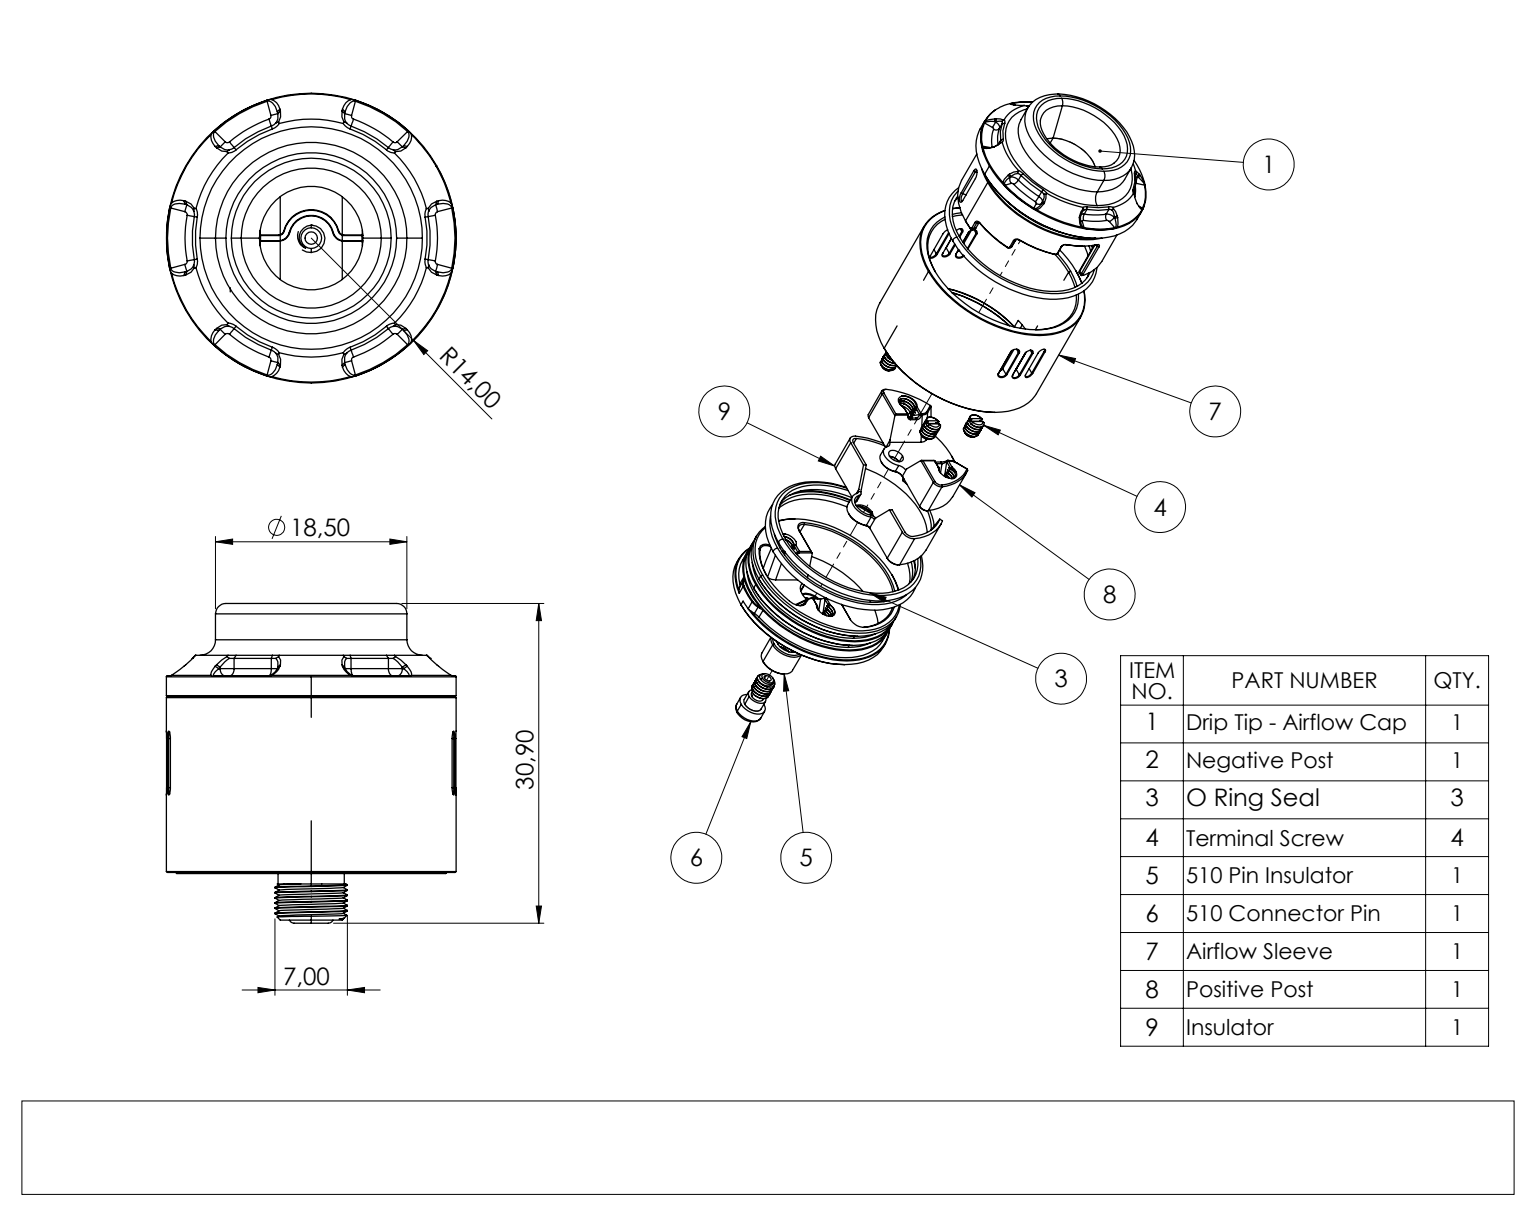
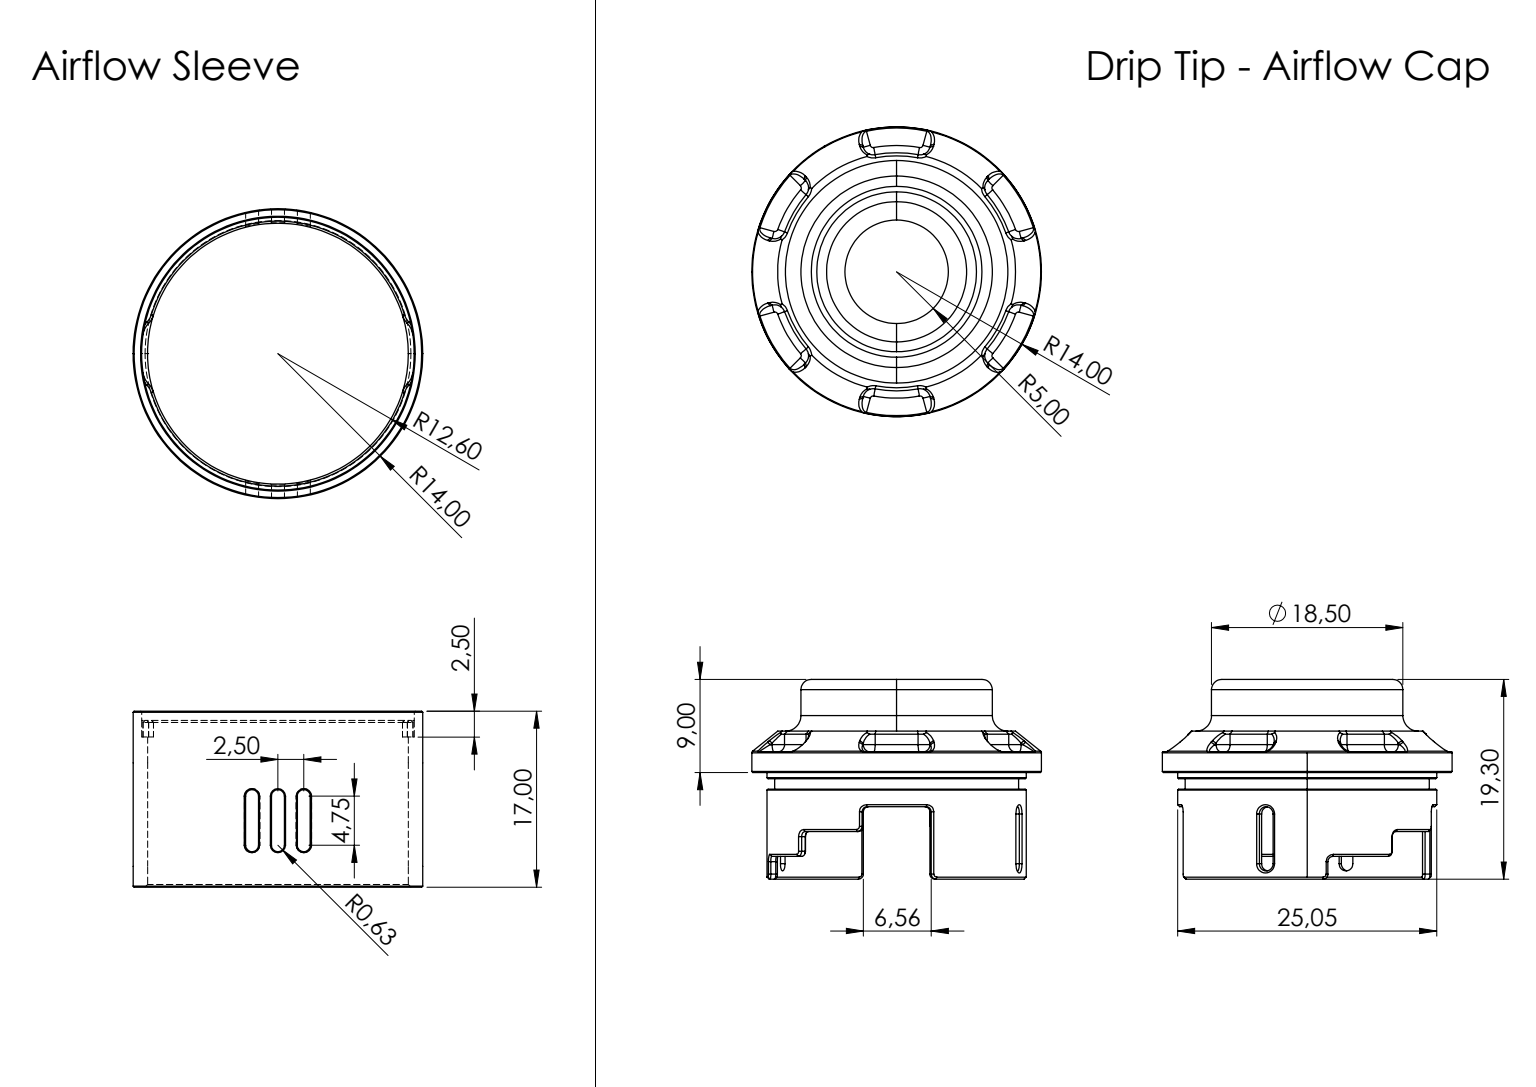
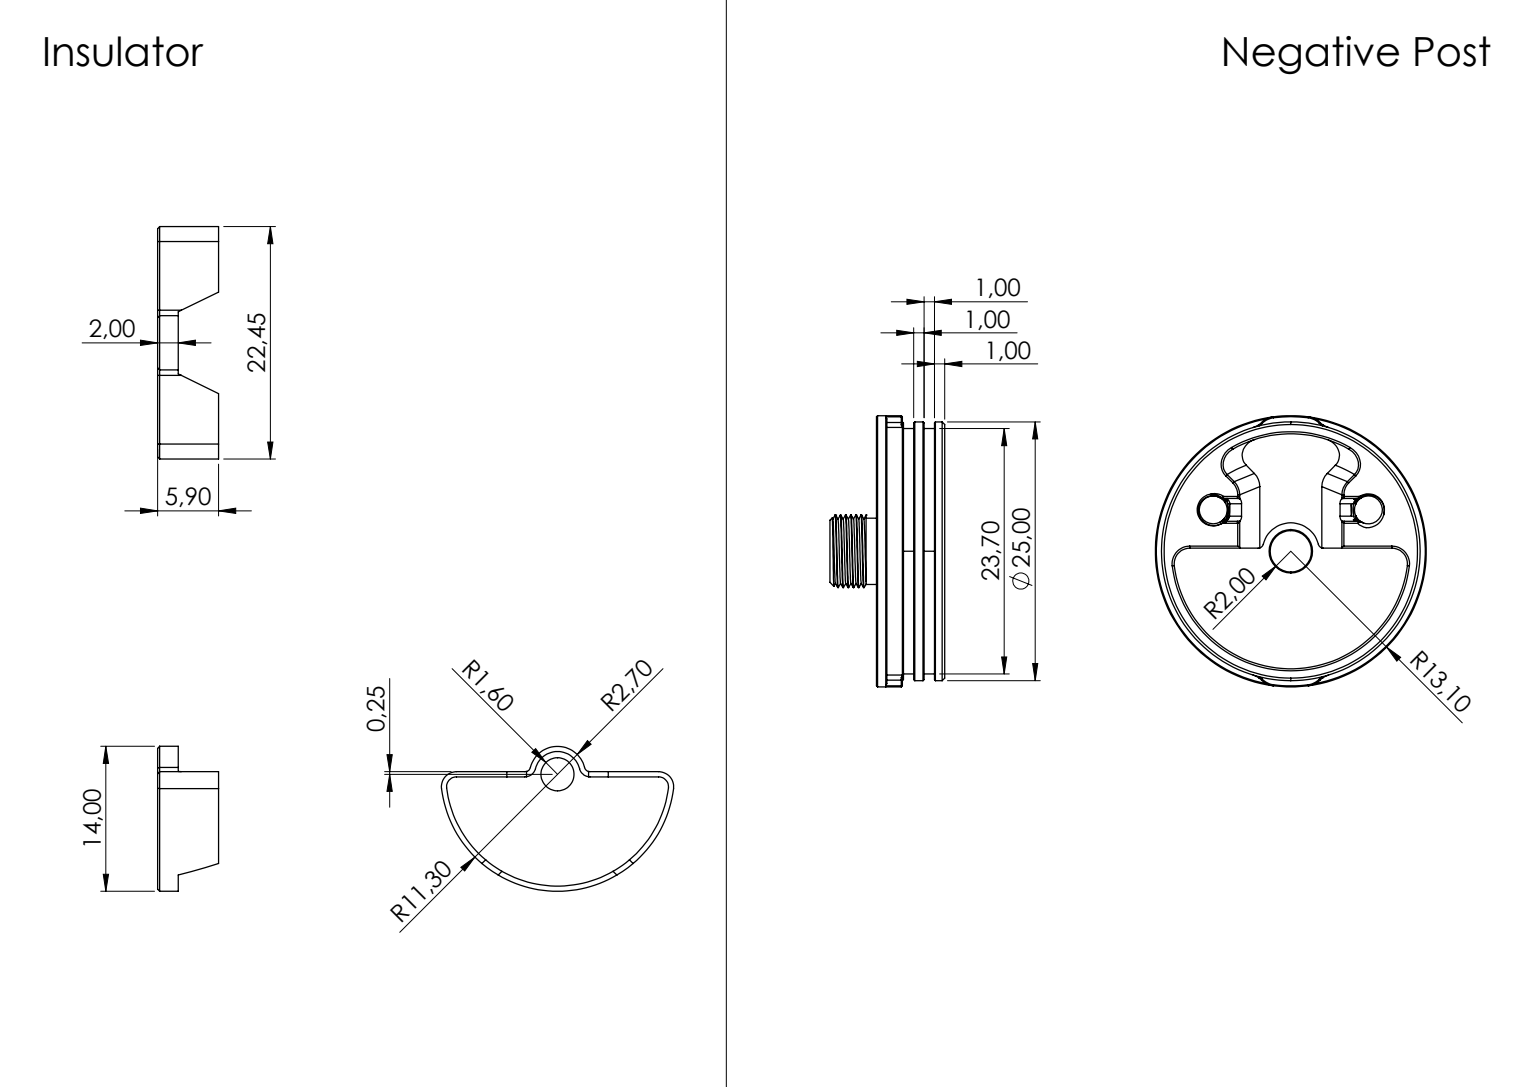
ISO-10303-21;
HEADER;
FILE_DESCRIPTION (('STEP AP214'),
    '1' );
FILE_NAME ('MAS-678',
    '2026-10-05T22:38:29',
    ( '' ),
    ( '' ),
    'SwSTEP 2.0',
    'SolidWorks 2020',
    '' );
FILE_SCHEMA (( 'AUTOMOTIVE_DESIGN' ));
ENDSEC;

DATA;
#1 = ORIENTED_EDGE ( 'NONE', *, *, #7882, .T. ) ;
#2 = CARTESIAN_POINT ( 'NONE',  ( 10.88210843320517007, 2.862311695598936723, 6.901605483505062644 ) ) ;
#3 = DIRECTION ( 'NONE',  ( 1.000000000000000000, 0.000000000000000000, 0.000000000000000000 ) ) ;
#4 = VERTEX_POINT ( 'NONE', #45504 ) ;
#5 = DIRECTION ( 'NONE',  ( 1.000000000000000000, 0.000000000000000000, 0.000000000000000000 ) ) ;
#6 = CARTESIAN_POINT ( 'NONE',  ( 11.11718313518939816, 3.377550038693600154, 6.712912394634500401 ) ) ;
#7 = CARTESIAN_POINT ( 'NONE',  ( 10.13049857835000012, 3.092060693447000297, 8.629378633793999498 ) ) ;
#8 = CARTESIAN_POINT ( 'NONE',  ( 10.70780830849999887, 5.157484706885999692, -6.267808298721999627 ) ) ;
#9 = CARTESIAN_POINT ( 'NONE',  ( 8.298061260823001106, 5.118905885020002877, 6.382684838875003486 ) ) ;
#10 = CARTESIAN_POINT ( 'NONE',  ( 9.778462793022999477, -5.743713977826000239, 7.748300060190000060 ) ) ;
#11 = CARTESIAN_POINT ( 'NONE',  ( 17.93538082550040613, 0.4959841406075952142, -12.68696163625449991 ) ) ;
#12 = CARTESIAN_POINT ( 'NONE',  ( 12.26368341514758420, 2.812488373142785214, -12.37327521544950670 ) ) ;
#13 = CARTESIAN_POINT ( 'NONE',  ( 11.38795122972049967, -3.601717549869600354, -6.578956058177199751 ) ) ;
#14 = CARTESIAN_POINT ( 'NONE',  ( 8.817635841231000526, 3.894644548817000285, 6.044465307984999924 ) ) ;
#15 = ORIENTED_EDGE ( 'NONE', *, *, #36574, .T. ) ;
#16 = ADVANCED_FACE ( 'NONE', ( #60887 ), #64896, .T. ) ;
#17 = FILL_AREA_STYLE_COLOUR ( '', #27665 ) ;
#18 = CARTESIAN_POINT ( 'NONE',  ( 11.09999999999999787, 2.363924005032890907, -6.981107664647397293 ) ) ;
#19 = CYLINDRICAL_SURFACE ( 'NONE', #27188, 3.500000000000000000 ) ;
#20 = CARTESIAN_POINT ( 'NONE',  ( 29.60000000000000142, 0.000000000000000000, 9.250000000000000000 ) ) ;
#21 = ADVANCED_FACE ( 'NONE', ( #67495 ), #4617, .T. ) ;
#22 = CARTESIAN_POINT ( 'NONE',  ( 18.07822721942927302, 2.978550302103497138, 12.24288824562991351 ) ) ;
#23 = CARTESIAN_POINT ( 'NONE',  ( 10.96871661479000082, 6.473054195915000086, 5.205103511516999681 ) ) ;
#24 = B_SPLINE_CURVE_WITH_KNOTS ( 'NONE', 3,
 ( #18393, #12452, #50546, #13155, #61715, #44967, #55102, #35164, #34485, #56132, #66271, #55449, #55796, #8240, #40068, #29927 ),
 .UNSPECIFIED., .F., .F.,
 ( 4, 2, 2, 1, 1, 2, 2, 2, 4 ),
 ( 0.000000000000000000, 0.2499999999999854561, 0.3749999999999792943, 0.4374999999999752420, 0.4687499999999756861, 0.4843749999999741873, 0.4999999999999726885, 0.7499999999999863443, 1.000000000000000000 ),
 .UNSPECIFIED. ) ;
#25 = CARTESIAN_POINT ( 'NONE',  ( 11.12426277055000057, 7.494722804685999940, 6.525523669353000322 ) ) ;
#26 = CARTESIAN_POINT ( 'NONE',  ( 9.239023565813489824, -2.669687318136871212, 7.269906695626100479 ) ) ;
#27 = CARTESIAN_POINT ( 'NONE',  ( 12.80505043854146940, -1.875000000000000444, 13.78631952119025605 ) ) ;
#28 = ORIENTED_EDGE ( 'NONE', *, *, #52791, .T. ) ;
#29 = FACE_OUTER_BOUND ( 'NONE', #10230, .T. ) ;
#30 = CARTESIAN_POINT ( 'NONE',  ( 10.08762143724499794, -3.241588663654300095, -6.646450532840099790 ) ) ;
#31 = CARTESIAN_POINT ( 'NONE',  ( 8.842811534616762614, 2.713269201112010087, -7.026666560124946947 ) ) ;
#32 = VECTOR ( 'NONE', #8697, 999.9999999999998863 ) ;
#33 = CARTESIAN_POINT ( 'NONE',  ( 8.330224159023998709, 2.898680183691999979, -6.607597200868999820 ) ) ;
#34 = CARTESIAN_POINT ( 'NONE',  ( 11.83872066707849946, -3.141388196630700236, 8.019361746728900897 ) ) ;
#35 = B_SPLINE_SURFACE_WITH_KNOTS ( 'NONE', 3, 3, ( 
 ( #2869, #65803, #50776, #34359 ),
 ( #29812, #34009, #40284, #7079 ),
 ( #23854, #61601, #66495, #55327 ),
 ( #7424, #28419, #39247, #8122 ),
 ( #61263, #39944, #28771, #60570 ),
 ( #24197, #50084, #1494, #45534 ),
 ( #13032, #2527, #23505, #44847 ),
 ( #22810, #49733, #13718, #17578 ),
 ( #55678, #56015, #66844, #65457 ),
 ( #50423, #38906, #18957, #35048 ),
 ( #1842, #60228, #7777, #56363 ),
 ( #23160, #12678, #66153, #18271 ) ),
 .UNSPECIFIED., .F., .F., .F.,
 ( 4, 1, 1, 1, 1, 1, 1, 1, 1, 4 ),
 ( 4, 4 ),
 ( 0.01095778183512000070, 0.05000000000000000278, 0.1000000000000000056, 0.1499999999999999944, 0.2000000000000000111, 0.2500000000000000000, 0.2999999999999999889, 0.3499999999999999778, 0.4000000000000000222, 0.4461465442842999507 ),
 ( -0.2706701497076000051, 1.270791666117000007 ),
 .UNSPECIFIED. ) ;
#36 = CARTESIAN_POINT ( 'NONE',  ( 10.55103166480599874, 2.999015536536000504, -7.570575893572789816 ) ) ;
#37 = CARTESIAN_POINT ( 'NONE',  ( 8.691343736187999269, 3.625767601089900261, 6.690658690097199823 ) ) ;
#38 = CARTESIAN_POINT ( 'NONE',  ( 11.59999999999999964, 3.116215992411100366, 7.174999999999999822 ) ) ;
#39 = CARTESIAN_POINT ( 'NONE',  ( 43.76123417800000226, 13.94845324556000143, -4.312847325879000770 ) ) ;
#40 = CARTESIAN_POINT ( 'NONE',  ( 12.29711362085063797, 1.966768764679983184, 12.44555721978031038 ) ) ;
#42 = CARTESIAN_POINT ( 'NONE',  ( 18.35676500243362952, -3.328522075972216498, -12.07468831868077963 ) ) ;
#41 = CARTESIAN_POINT ( 'NONE',  ( 9.125113844317997547, 4.288351516201100111, -6.395197822644999697 ) ) ;
#43 = CARTESIAN_POINT ( 'NONE',  ( 11.67918044953561996, 5.011483761127000669, -8.027436060358800418 ) ) ;
#44 = CARTESIAN_POINT ( 'NONE',  ( 7.733151861820001471, 2.920631402299000534, -6.523085346364998038 ) ) ;
#45 = CARTESIAN_POINT ( 'NONE',  ( 10.26693915877000052, 5.500023470133998948, -6.419501519420999891 ) ) ;
#46 = CARTESIAN_POINT ( 'NONE',  ( 8.568822372493999140, 3.671800173070400408, -8.573651380901999630 ) ) ;
#48 = CARTESIAN_POINT ( 'NONE',  ( 12.27854653041788957, 2.836954440259892962, 12.36664979425441580 ) ) ;
#47 = CARTESIAN_POINT ( 'NONE',  ( 15.36937411412500154, -8.827864207275998965, -7.821779713377999599 ) ) ;
#49 = CARTESIAN_POINT ( 'NONE',  ( 8.041787892231001322, 5.114458628598999468, -6.690862273930999748 ) ) ;
#50 = ORIENTED_EDGE ( 'NONE', *, *, #56829, .T. ) ;
#51 = CARTESIAN_POINT ( 'NONE',  ( 12.25734197670618641, 0.3012394090295977822, 12.69519438487549756 ) ) ;
#52 = DIRECTION ( 'NONE',  ( 0.000000000000000000, -1.000000000000000000, 0.000000000000000000 ) ) ;
#53 = DIRECTION ( 'NONE',  ( 1.000000000000000000, 0.000000000000000000, 0.000000000000000000 ) ) ;
#54 = CARTESIAN_POINT ( 'NONE',  ( 9.804975701332999449, 4.636077325177999420, 6.910836541441499392 ) ) ;
#55 = CARTESIAN_POINT ( 'NONE',  ( 12.37605701841387607, -2.954974367521621570, 13.56637846613975107 ) ) ;
#56 = CARTESIAN_POINT ( 'NONE',  ( 12.19373784185879472, 2.630112414937235688, 13.64494795218897671 ) ) ;
#57 = CARTESIAN_POINT ( 'NONE',  ( 8.674830025576039105, -2.649890579813208191, 7.499988935010342139 ) ) ;
#58 = ORIENTED_EDGE ( 'NONE', *, *, #5676, .F. ) ;
#59 = CARTESIAN_POINT ( 'NONE',  ( 4.808535432091000317, -0.4767679613171000308, 1.182990937922999919 ) ) ;
#60 = CARTESIAN_POINT ( 'NONE',  ( 9.554646554150998838, -3.380689388027600106, -8.619302797893999113 ) ) ;
#61 = CARTESIAN_POINT ( 'NONE',  ( 9.794101180193951706, -2.685368189354502721, -7.853409369710684373 ) ) ;
#62 = CYLINDRICAL_SURFACE ( 'NONE', #7615, 1.350000000000000089 ) ;
#63 = AXIS2_PLACEMENT_3D ( 'NONE', #33493, #16702, #6562 ) ;
#64 = CARTESIAN_POINT ( 'NONE',  ( 17.89568490471441820, 3.024116370425395939, -12.31388631808444600 ) ) ;
#65 = CARTESIAN_POINT ( 'NONE',  ( 9.833766445374623189, -5.249999999999997335, 7.659651991919251834 ) ) ;
#66 = DIRECTION ( 'NONE',  ( 0.000000000000000000, -1.000000000000000000, 0.000000000000000000 ) ) ;
#67 = CARTESIAN_POINT ( 'NONE',  ( 3.799999782336999754, 0.000000000000000000, -2.724999689663869962 ) ) ;
#68 = CARTESIAN_POINT ( 'NONE',  ( 24.30000000000000071, 8.810505093353000916, -8.810505093353000916 ) ) ;
#69 = CARTESIAN_POINT ( 'NONE',  ( 4.719609839682791907, -0.1963495408493605987, -1.500000000000000444 ) ) ;
#70 = B_SPLINE_CURVE_WITH_KNOTS ( 'NONE', 3,
 ( #4155, #68818, #63577, #63225, #63916, #25495, #46825, #36328, #9749, #31097, #4497, #25838, #47166, #15351, #10099, #27912 ),
 .UNSPECIFIED., .F., .F.,
 ( 4, 2, 2, 2, 2, 2, 2, 4 ),
 ( 0.000000000000000000, 0.06249999999999925060, 0.1249999999999985012, 0.2499999999999987232, 0.3749999999999989453, 0.4999999999999991118, 0.7499999999999995559, 1.000000000000000000 ),
 .UNSPECIFIED. ) ;
#71 = CARTESIAN_POINT ( 'NONE',  ( 11.09999763817999963, -1.407106875523000067, -11.46396985304999916 ) ) ;
#72 = CARTESIAN_POINT ( 'NONE',  ( 23.84129431493439455, 9.640979322668712825, -9.399448990175832463 ) ) ;
#73 = EDGE_CURVE ( 'NONE', #54965, #29508, #17176, .T. ) ;
#74 = CARTESIAN_POINT ( 'NONE',  ( 4.500000000000000000, -13.10000000000000142, 0.000000000000000000 ) ) ;
#75 = EDGE_CURVE ( 'NONE', #48923, #52150, #18017, .T. ) ;
#76 = CARTESIAN_POINT ( 'NONE',  ( 24.22109577643600176, 12.94658526084000094, -3.131939672619000081 ) ) ;
#77 = AXIS2_PLACEMENT_3D ( 'NONE', #39446, #28974, #49587 ) ;
#78 = B_SPLINE_CURVE_WITH_KNOTS ( 'NONE', 3,
 ( #47462, #68766, #250, #37651 ),
 .UNSPECIFIED., .F., .F.,
 ( 4, 4 ),
 ( 0.000000000000000000, 1.000000000000000000 ),
 .UNSPECIFIED. ) ;
#79 = VERTEX_POINT ( 'NONE', #50744 ) ;
#80 = CARTESIAN_POINT ( 'NONE',  ( 9.351420280414000530, 4.953415418491999844, -8.946479654552000227 ) ) ;
#81 = CARTESIAN_POINT ( 'NONE',  ( 11.88795122972049967, -3.601717549869600354, 8.421043941822800249 ) ) ;
#82 = ORIENTED_EDGE ( 'NONE', *, *, #59738, .T. ) ;
#83 = FACE_OUTER_BOUND ( 'NONE', #29738, .T. ) ;
#84 = CARTESIAN_POINT ( 'NONE',  ( 11.18687482311539938, -2.942322404451000128, -7.927326830586499007 ) ) ;
#85 = ORIENTED_EDGE ( 'NONE', *, *, #60976, .T. ) ;
#86 = CARTESIAN_POINT ( 'NONE',  ( 11.05435090131019926, 5.119447121461000449, 6.807613609764599616 ) ) ;
#87 = CARTESIAN_POINT ( 'NONE',  ( 23.84019513318622074, 3.320741495842120639, -13.05081507454588241 ) ) ;
#88 = CARTESIAN_POINT ( 'NONE',  ( 10.01835931248959888, -5.126777126172243015, -6.752018918849381102 ) ) ;
#89 = CARTESIAN_POINT ( 'NONE',  ( 14.46666666323366890, -9.471992681081616183, -8.194936219980965220 ) ) ;
#90 = CARTESIAN_POINT ( 'NONE',  ( 12.26246717640210626, 0.3103928943003824159, -13.89533876751735342 ) ) ;
#91 = CARTESIAN_POINT ( 'NONE',  ( 11.59999999999999964, -4.640264089079230381, -6.808168915892154338 ) ) ;
#92 = CARTESIAN_POINT ( 'NONE',  ( 13.73959992722299894, 11.36892293904000084, 2.362143082378000081 ) ) ;
#93 = VERTEX_POINT ( 'NONE', #24168 ) ;
#94 = CARTESIAN_POINT ( 'NONE',  ( 0.7000000000000000666, 0.000000000000000000, 0.000000000000000000 ) ) ;
#95 = VERTEX_POINT ( 'NONE', #41621 ) ;
#96 = CARTESIAN_POINT ( 'NONE',  ( 0.1199860357128856997, -1.197242505009922908, -2.894009422536151011 ) ) ;
#97 = EDGE_LOOP ( 'NONE', ( #29437, #64562 ) ) ;
#98 = CARTESIAN_POINT ( 'NONE',  ( 8.592138961223998450, 5.059894361919000438, 6.783753885003399375 ) ) ;
#99 = CARTESIAN_POINT ( 'NONE',  ( 18.17480529351248109, -2.583342416263718633, -12.43177882285068137 ) ) ;
#100 = EDGE_CURVE ( 'NONE', #6210, #57286, #54708, .T. ) ;
#101 = DIRECTION ( 'NONE',  ( 0.000000000000000000, 0.000000000000000000, -1.000000000000000000 ) ) ;
#102 = CARTESIAN_POINT ( 'NONE',  ( 20.10000000000000142, 11.84999999999999964, 0.000000000000000000 ) ) ;
#103 = CARTESIAN_POINT ( 'NONE',  ( 12.21303990359567848, -0.2014071429975183569, 13.89805485625563541 ) ) ;
#104 = EDGE_LOOP ( 'NONE', ( #11078, #29942, #13944, #17736 ) ) ;
#105 = CARTESIAN_POINT ( 'NONE',  ( 12.83944380997200163, 12.16696032571000075, -3.135189167188999537 ) ) ;
#106 = CARTESIAN_POINT ( 'NONE',  ( 18.29845715546600005, 11.81398323980999976, -3.695357857504999899 ) ) ;
#107 = B_SPLINE_CURVE_WITH_KNOTS ( 'NONE', 3,
 ( #46552, #47923, #10170, #41640 ),
 .UNSPECIFIED., .F., .F.,
 ( 4, 4 ),
 ( 0.000000000000000000, 1.000000000000000000 ),
 .UNSPECIFIED. ) ;
#108 = CARTESIAN_POINT ( 'NONE',  ( 9.860128811416625894, 4.869607263996035940, 7.403483289911290122 ) ) ;
#109 = CARTESIAN_POINT ( 'NONE',  ( 8.383148997457999130, -5.167567567567999731, 6.822293592207000934 ) ) ;
#110 = AXIS2_PLACEMENT_3D ( 'NONE', #3453, #51019, #35292 ) ;
#111 = CARTESIAN_POINT ( 'NONE',  ( 9.833904719592002408, 5.048004622677000341, -6.120508709481000231 ) ) ;
#112 = CARTESIAN_POINT ( 'NONE',  ( 18.47645006436894022, 11.77746884181073384, -4.263736182725015311 ) ) ;
#113 = CARTESIAN_POINT ( 'NONE',  ( 10.36950884864999978, -2.719121019997000399, -7.031782724641000293 ) ) ;
#114 = ORIENTED_EDGE ( 'NONE', *, *, #34124, .T. ) ;
#115 = VERTEX_POINT ( 'NONE', #31827 ) ;
#116 = AXIS2_PLACEMENT_3D ( 'NONE', #14745, #2874, #57380 ) ;
#117 = CARTESIAN_POINT ( 'NONE',  ( 10.17905590578999941, -2.899999999999999911, 6.571291218949999902 ) ) ;
#118 = LINE ( 'NONE', #6737, #27722 ) ;
#119 = CARTESIAN_POINT ( 'NONE',  ( 8.635274708161395196, -3.045105040003566632, -6.545565613752198253 ) ) ;
#120 = CARTESIAN_POINT ( 'NONE',  ( 12.27869449350093056, -2.837185661390559499, 13.59614283363490905 ) ) ;
#121 = CARTESIAN_POINT ( 'NONE',  ( 0.1499942179680000265, 2.749953718116143087, -0.3599680999394002101 ) ) ;
#122 = B_SPLINE_CURVE_WITH_KNOTS ( 'NONE', 3,
 ( #66091, #18210, #1783, #39886 ),
 .UNSPECIFIED., .F., .F.,
 ( 4, 4 ),
 ( 0.000000000000000000, 1.000000000000000000 ),
 .UNSPECIFIED. ) ;
#123 = B_SPLINE_CURVE_WITH_KNOTS ( 'NONE', 3,
 ( #913, #28170, #54387, #23268, #22568, #44612 ),
 .UNSPECIFIED., .F., .F.,
 ( 4, 2, 4 ),
 ( 0.000000000000000000, 0.5000000000000000000, 1.000000000000000000 ),
 .UNSPECIFIED. ) ;
#124 = CARTESIAN_POINT ( 'NONE',  ( 11.17901463001529905, 4.697110652903200290, -6.383488688482000128 ) ) ;
#125 = CARTESIAN_POINT ( 'NONE',  ( 8.927455549952998837, 4.674761969675400586, -6.955569812538500152 ) ) ;
#127 = CARTESIAN_POINT ( 'NONE',  ( 4.399793616306585164, -0.6172922141386431027, -0.9509182009922042544 ) ) ;
#126 = CARTESIAN_POINT ( 'NONE',  ( 9.549126402770998112, -2.931626221533000010, 7.902879529556599891 ) ) ;
#128 = DIRECTION ( 'NONE',  ( -0.3310054520069888873, 0.000000000000000000, -0.9436288416224086761 ) ) ;
#129 = VERTEX_POINT ( 'NONE', #36029 ) ;
#130 = CARTESIAN_POINT ( 'NONE',  ( 11.04749144726329924, -4.500836215462999945, -6.793273974143599681 ) ) ;
#131 = CIRCLE ( 'NONE', #66002, 11.65000000000000036 ) ;
#132 = CARTESIAN_POINT ( 'NONE',  ( 7.905017292225999803, -2.916160783733999562, 6.437838678341997856 ) ) ;
#133 = ADVANCED_FACE ( 'NONE', ( #9448 ), #52633, .T. ) ;
#134 = EDGE_CURVE ( 'NONE', #63154, #64134, #61396, .T. ) ;
#135 = CARTESIAN_POINT ( 'NONE',  ( 10.08963399569799790, 5.271405458160000279, 7.358888170452400068 ) ) ;
#136 = DIRECTION ( 'NONE',  ( 0.7071067617951957152, 0.000000000000000000, -0.7071068005778986532 ) ) ;
#137 = CARTESIAN_POINT ( 'NONE',  ( 9.215289122285998502, -4.861979632688999686, 8.938813901364000003 ) ) ;
#138 = CARTESIAN_POINT ( 'NONE',  ( 18.16648463825930548, 2.629536981073587132, -12.42046771373108172 ) ) ;
#139 = CARTESIAN_POINT ( 'NONE',  ( 16.13763077846600069, -3.625006537420000008, -11.03132468648999875 ) ) ;
#140 = CARTESIAN_POINT ( 'NONE',  ( 13.64331666222400052, -12.23490852752999913, -2.418322770048999981 ) ) ;
#141 = CARTESIAN_POINT ( 'NONE',  ( 7.083500347624626770, 5.272504913147756156, -6.972355927689905641 ) ) ;
#142 = CARTESIAN_POINT ( 'NONE',  ( 8.851468108405999402, -3.165798890946399879, -7.736255015838599647 ) ) ;
#143 = CARTESIAN_POINT ( 'NONE',  ( 5.807487603146999966, -1.101608967510000037, 0.4118716830840000176 ) ) ;
#144 = CARTESIAN_POINT ( 'NONE',  ( 15.39999999998900293, -9.471998555523999386, -8.194929586088999685 ) ) ;
#145 = CARTESIAN_POINT ( 'NONE',  ( 17.65093666542126272, 1.765655615500123954, 12.47567830514603671 ) ) ;
#146 = VERTEX_POINT ( 'NONE', #46530 ) ;
#147 = CARTESIAN_POINT ( 'NONE',  ( 12.18127380957210093, 0.04040257046694419041, -12.69991905489011685 ) ) ;
#148 = CARTESIAN_POINT ( 'NONE',  ( 10.87518447801629939, 4.865987311498500389, -7.480906371072489236 ) ) ;
#149 = CARTESIAN_POINT ( 'NONE',  ( 24.44496487975900223, 3.224879802562000464, -12.03535984693000138 ) ) ;
#150 = DIRECTION ( 'NONE',  ( -1.000000000000000000, 0.000000000000000000, 0.000000000000000000 ) ) ;
#151 = CARTESIAN_POINT ( 'NONE',  ( 10.13586576648993542, 5.314625264832240070, -7.853278872970742341 ) ) ;
#152 = EDGE_LOOP ( 'NONE', ( #38398, #58380, #48495, #62252 ) ) ;
#153 = CARTESIAN_POINT ( 'NONE',  ( 10.87751262143000019, 2.899999999999999911, 6.466455373849333554 ) ) ;
#154 = CONTEXT_DEPENDENT_SHAPE_REPRESENTATION ( #10108, #3848 ) ;
#155 = CARTESIAN_POINT ( 'NONE',  ( 10.85679632507500081, -3.509334349252600127, -8.409605917786398877 ) ) ;
#156 = EDGE_CURVE ( 'NONE', #45407, #3060, #52452, .T. ) ;
#157 = DIRECTION ( 'NONE',  ( 0.000000000000000000, -0.1333333333333049930, -0.9910712498212376209 ) ) ;
#158 = CYLINDRICAL_SURFACE ( 'NONE', #24280, 3.500000000000000000 ) ;
#159 = DIRECTION ( 'NONE',  ( 1.000000000000000000, -1.776356839337000228E-14, 0.000000000000000000 ) ) ;
#160 = CARTESIAN_POINT ( 'NONE',  ( 10.94501463001509833, 4.472480213525599879, -6.743262887067199784 ) ) ;
#161 = ORIENTED_EDGE ( 'NONE', *, *, #34361, .F. ) ;
#162 = EDGE_CURVE ( 'NONE', #21254, #36556, #58057, .T. ) ;
#163 = CARTESIAN_POINT ( 'NONE',  ( 10.00122642709000154, -2.274091010763000131, 7.851325450887000734 ) ) ;
#164 = CARTESIAN_POINT ( 'NONE',  ( 18.14041819333145966, 2.719953065120093161, -13.62436182279261132 ) ) ;
#165 = ORIENTED_EDGE ( 'NONE', *, *, #34097, .T. ) ;
#166 = DIRECTION ( 'NONE',  ( -1.000000000000000000, -0.000000000000000000, -0.000000000000000000 ) ) ;
#167 = CARTESIAN_POINT ( 'NONE',  ( 9.085769353209000698, -2.821866379289000193, 6.127148604720000336 ) ) ;
#168 = CARTESIAN_POINT ( 'NONE',  ( 10.32322128467999889, -3.399999874579999748, -4.621083553505000552 ) ) ;
#169 = ORIENTED_EDGE ( 'NONE', *, *, #59426, .T. ) ;
#170 = FACE_OUTER_BOUND ( 'NONE', #15935, .T. ) ;
#171 = CIRCLE ( 'NONE', #66048, 0.5000000000000000000 ) ;
#172 = CARTESIAN_POINT ( 'NONE',  ( 7.414760841225000121, 5.517512745430000365, -8.643112676966000052 ) ) ;
#173 = CARTESIAN_POINT ( 'NONE',  ( 9.593930206849998754, -2.750000000000000000, -7.500000000000000000 ) ) ;
#174 = CARTESIAN_POINT ( 'NONE',  ( 9.490131263588281740, 4.919273367466419522, 8.488493135541203216 ) ) ;
#175 = ORIENTED_EDGE ( 'NONE', *, *, #20604, .T. ) ;
#176 = CARTESIAN_POINT ( 'NONE',  ( 10.84168850528999961, -2.681008214828000114, 6.554752254946000889 ) ) ;
#177 = CARTESIAN_POINT ( 'NONE',  ( 25.19966795687700056, 11.70907786114999993, -2.905888020798000237 ) ) ;
#178 = CARTESIAN_POINT ( 'NONE',  ( 11.32299956498189886, 2.792989229543000107, -7.174999999999999822 ) ) ;
#179 = ORIENTED_EDGE ( 'NONE', *, *, #15611, .T. ) ;
#180 = CARTESIAN_POINT ( 'NONE',  ( 9.051300837857860770, 5.190117543293265356, -7.723566111296684689 ) ) ;
#181 = CARTESIAN_POINT ( 'NONE',  ( 10.65229194037999960, -4.944342461481999962, -8.478476072358999360 ) ) ;
#182 = ORIENTED_EDGE ( 'NONE', *, *, #30805, .F. ) ;
#183 = CARTESIAN_POINT ( 'NONE',  ( 10.90000000536000080, -2.899999999941999640, -5.157071284930999866 ) ) ;
#184 = CARTESIAN_POINT ( 'NONE',  ( 17.79602238657566105, -1.801771354310902185, -12.47051018296933833 ) ) ;
#185 = CARTESIAN_POINT ( 'NONE',  ( 4.658558767843999249, -0.5257635793736999963, -1.466092528140000129 ) ) ;
#186 = ADVANCED_FACE ( 'NONE', ( #41966 ), #57076, .T. ) ;
#187 = VECTOR ( 'NONE', #31580, 1000.000000000000000 ) ;
#188 = CARTESIAN_POINT ( 'NONE',  ( 11.59999999999999964, 4.695782097862117865, -6.595854147058993533 ) ) ;
#189 = CARTESIAN_POINT ( 'NONE',  ( 16.04647714749799903, 3.814092932148000159, 11.87318743920999964 ) ) ;
#190 = CARTESIAN_POINT ( 'NONE',  ( 7.117714276092232062, 5.069132632172260067, -8.338946761425976462 ) ) ;
#191 = CARTESIAN_POINT ( 'NONE',  ( 10.98768521492000083, -5.299565686336999981, -4.945211137252000455 ) ) ;
#192 = ORIENTED_EDGE ( 'NONE', *, *, #17294, .T. ) ;
#193 = CARTESIAN_POINT ( 'NONE',  ( 13.63045347340496072, -12.32568024774126414, -2.226002549929300134 ) ) ;
#194 = ORIENTED_EDGE ( 'NONE', *, *, #47268, .T. ) ;
#195 = CARTESIAN_POINT ( 'NONE',  ( 10.66951519566999806, 4.592673277375999952, 5.841403042559999648 ) ) ;
#196 = DIRECTION ( 'NONE',  ( 0.000000000000000000, -0.7577476854548028662, 0.6525476574074028369 ) ) ;
#197 = CARTESIAN_POINT ( 'NONE',  ( 25.60000000000000142, 2.258942858049999725, 12.29419282279000036 ) ) ;
#198 = CARTESIAN_POINT ( 'NONE',  ( 12.37517135966887061, 2.046199321548339611, -13.75929785978299158 ) ) ;
#199 = DIRECTION ( 'NONE',  ( 0.7071067811865462405, 0.7071067811865462405, -6.013987063531392487E-08 ) ) ;
#200 = CARTESIAN_POINT ( 'NONE',  ( 8.767881343006999728, -4.605543323398999966, -6.293427432547999523 ) ) ;
#201 = CARTESIAN_POINT ( 'NONE',  ( 17.81345962944524075, -0.5694488842926289651, 13.88429844810378277 ) ) ;
#202 = CARTESIAN_POINT ( 'NONE',  ( 9.492702081557240490, -3.384517283567192170, -9.168413593352800817 ) ) ;
#203 = ORIENTED_EDGE ( 'NONE', *, *, #51624, .T. ) ;
#204 = CARTESIAN_POINT ( 'NONE',  ( 4.599999999999999645, 0.7302158263239199032, -13.98094363220830871 ) ) ;
#205 = B_SPLINE_CURVE_WITH_KNOTS ( 'NONE', 3,
 ( #23649, #19782, #46008, #23996, #18761 ),
 .UNSPECIFIED., .F., .F.,
 ( 4, 1, 4 ),
 ( 0.8746094594482839435, 0.9935764648741313154, 1.000000000000000000 ),
 .UNSPECIFIED. ) ;
#206 = CARTESIAN_POINT ( 'NONE',  ( 11.21503032197930061, -3.256621462143499901, 8.539569492647999027 ) ) ;
#207 = CARTESIAN_POINT ( 'NONE',  ( 18.00676300522524897, -0.4321619634102875085, -13.89096157872279313 ) ) ;
#208 = CARTESIAN_POINT ( 'NONE',  ( 8.464254440379999522, -2.029110377978999846, 7.726994002375999315 ) ) ;
#210 = CARTESIAN_POINT ( 'NONE',  ( 11.09999999999999964, 4.000000000000000000, -7.500000000000000000 ) ) ;
#209 = CARTESIAN_POINT ( 'NONE',  ( 10.28314886242000092, 2.387776420306999992, 7.684265965147999644 ) ) ;
#211 = CARTESIAN_POINT ( 'NONE',  ( 10.47303166480599934, 2.862083839376000416, -7.580230465881790280 ) ) ;
#212 = VECTOR ( 'NONE', #46961, 1000.000000000000000 ) ;
#213 = CARTESIAN_POINT ( 'NONE',  ( 13.99999999379500082, -8.815218614167999789, -7.616697584347000394 ) ) ;
#214 = CARTESIAN_POINT ( 'NONE',  ( 9.577013376692997682, 3.227076647348800176, -7.107192877568799361 ) ) ;
#215 = ADVANCED_FACE ( 'NONE', ( #63962 ), #25886, .F. ) ;
#216 = EDGE_CURVE ( 'NONE', #67955, #28137, #42558, .T. ) ;
#217 = CARTESIAN_POINT ( 'NONE',  ( 18.17882706751078814, 0.04040257046694405857, 12.69991905489010442 ) ) ;
#218 = CARTESIAN_POINT ( 'NONE',  ( 6.627690453616000177, -1.117491691666000042, 0.8211442336051000268 ) ) ;
#219 = B_SPLINE_CURVE_WITH_KNOTS ( 'NONE', 3,
 ( #58732, #10838, #32180, #5585, #347, #21664, #49972, #33901, #17109, #28659 ),
 .UNSPECIFIED., .F., .F.,
 ( 4, 2, 2, 2, 4 ),
 ( 0.2126015446065814829, 0.4094511584549361261, 0.6063007723032907137, 0.8031503861516453568, 1.000000000000000000 ),
 .UNSPECIFIED. ) ;
#220 = CARTESIAN_POINT ( 'NONE',  ( 11.09999999999999964, -6.593648099371000271, -5.598803483715999896 ) ) ;
#221 = EDGE_LOOP ( 'NONE', ( #55907, #18470, #68764, #30688 ) ) ;
#222 = CARTESIAN_POINT ( 'NONE',  ( 8.764831853209999579, -5.808258301303999893, 7.446016267012000256 ) ) ;
#223 = CARTESIAN_POINT ( 'NONE',  ( 8.898558059623999483, -5.146736128384000075, 6.597417125647000447 ) ) ;
#224 = EDGE_CURVE ( 'NONE', #15130, #33857, #51488, .T. ) ;
#225 = CARTESIAN_POINT ( 'NONE',  ( 8.856851002545001350, 2.832432432432000269, -6.822293592207000934 ) ) ;
#226 = CARTESIAN_POINT ( 'NONE',  ( 0.7000000000000000666, 0.5773502691895999739, -1.000000000000000000 ) ) ;
#227 = VERTEX_POINT ( 'NONE', #53143 ) ;
#228 = AXIS2_PLACEMENT_3D ( 'NONE', #34366, #45196, #60235 ) ;
#229 = CARTESIAN_POINT ( 'NONE',  ( 0.9904415426042999515, 3.273731968234999901, -1.479853775367000246 ) ) ;
#230 = CARTESIAN_POINT ( 'NONE',  ( 10.29399293566599916, 4.546741702992100009, 6.829299525004299376 ) ) ;
#231 = AXIS2_PLACEMENT_3D ( 'NONE', #53437, #47852, #5532 ) ;
#232 = CARTESIAN_POINT ( 'NONE',  ( 10.95519834123000003, 3.860336562672999960, -6.147350406894000585 ) ) ;
#233 = EDGE_LOOP ( 'NONE', ( #37593, #40253, #39646, #55320, #24111 ) ) ;
#234 = CARTESIAN_POINT ( 'NONE',  ( 9.383499245234510511, 2.750003956825025853, -7.336369100805423038 ) ) ;
#235 = CARTESIAN_POINT ( 'NONE',  ( 9.928197172113101487, 5.125396288428318847, 6.749639981086157370 ) ) ;
#236 = CARTESIAN_POINT ( 'NONE',  ( 18.05312913029195698, 3.003720153666129100, -12.23674614497118718 ) ) ;
#237 = CARTESIAN_POINT ( 'NONE',  ( 2.300973465875999935, -3.500000000000000000, 0.000000000000000000 ) ) ;
#238 = CARTESIAN_POINT ( 'NONE',  ( 7.667607780408999929, 5.638704226117999596, 8.266404648244000342 ) ) ;
#239 = ORIENTED_EDGE ( 'NONE', *, *, #67496, .F. ) ;
#240 = CARTESIAN_POINT ( 'NONE',  ( 5.982073283530000118, -0.8842068839782000200, 1.351115652313999771 ) ) ;
#241 = CARTESIAN_POINT ( 'NONE',  ( 7.847520280408001092, 3.511256298105000173, -6.013302684100999329 ) ) ;
#242 = B_SPLINE_CURVE_WITH_KNOTS ( 'NONE', 3,
 ( #55856, #2711, #2367, #19824 ),
 .UNSPECIFIED., .F., .F.,
 ( 4, 4 ),
 ( 0.000000000000000000, 1.000000000000000000 ),
 .UNSPECIFIED. ) ;
#243 = CARTESIAN_POINT ( 'NONE',  ( 8.449835681852293945, -2.260412657429408334, 7.498936987450196767 ) ) ;
#244 = CARTESIAN_POINT ( 'NONE',  ( 11.79999999771000141, -12.39026187696000036, -1.832249219479999969 ) ) ;
#245 = ORIENTED_EDGE ( 'NONE', *, *, #68293, .F. ) ;
#246 = CARTESIAN_POINT ( 'NONE',  ( 2.959306799210166705, 3.058252359239905793, -1.762666431298143488 ) ) ;
#247 = CARTESIAN_POINT ( 'NONE',  ( 11.26443347348000046, 11.78677031080999882, 1.538950076482000107 ) ) ;
#248 = ORIENTED_EDGE ( 'NONE', *, *, #50052, .F. ) ;
#249 = DIRECTION ( 'NONE',  ( 1.000000000000000000, 0.000000000000000000, 0.000000000000000000 ) ) ;
#250 = CARTESIAN_POINT ( 'NONE',  ( 18.36662463489987474, -2.877217017167624125, 12.05304703251516507 ) ) ;
#251 = DIRECTION ( 'NONE',  ( 1.000000000000000000, 0.000000000000000000, 0.000000000000000000 ) ) ;
#252 = VERTEX_POINT ( 'NONE', #5244 ) ;
#253 = CARTESIAN_POINT ( 'NONE',  ( 15.71007343403957002, -8.769519461636603452, -7.669310999670508444 ) ) ;
#254 = CARTESIAN_POINT ( 'NONE',  ( 9.865041550948088656, -2.650034642413194419, -7.500002425457253707 ) ) ;
#255 = CARTESIAN_POINT ( 'NONE',  ( 10.94501463001509833, 4.472480213525599879, -6.743262887067199784 ) ) ;
#256 = CARTESIAN_POINT ( 'NONE',  ( 12.39106450428430328, 2.968342857027793880, -12.33004038639662525 ) ) ;
#257 = CARTESIAN_POINT ( 'NONE',  ( 10.64887885159599890, -2.730985436695000157, 7.651388779553199626 ) ) ;
#258 = ORIENTED_EDGE ( 'NONE', *, *, #890, .F. ) ;
#259 = CARTESIAN_POINT ( 'NONE',  ( 7.486426658771000220, 5.321913229613000063, 8.118244847118999630 ) ) ;
#260 = ORIENTED_EDGE ( 'NONE', *, *, #5436, .F. ) ;
#261 = CARTESIAN_POINT ( 'NONE',  ( 9.352250488097009651, -5.092274670905195144, -6.870455438679058169 ) ) ;
#262 = AXIS2_PLACEMENT_3D ( 'NONE', #53883, #16817, #11569 ) ;
#263 = CARTESIAN_POINT ( 'NONE',  ( 17.74546162999697074, 0.7003689475978067680, 12.58057160030229227 ) ) ;
#264 = CARTESIAN_POINT ( 'NONE',  ( 27.09999999999999787, 0.000000000000000000, 0.000000000000000000 ) ) ;
#265 = ORIENTED_EDGE ( 'NONE', *, *, #31744, .F. ) ;
#266 = CARTESIAN_POINT ( 'NONE',  ( 12.19523649643098295, -2.361571219431551238, -12.48275271858022073 ) ) ;
#267 = EDGE_CURVE ( 'NONE', #32166, #65266, #66403, .T. ) ;
#268 = CARTESIAN_POINT ( 'NONE',  ( 0.3804339246497162041, -3.380412643848677234, -0.4416305321314611398 ) ) ;
#269 = CARTESIAN_POINT ( 'NONE',  ( 23.56666365135700403, -9.069641144872004901, 7.556701426719000025 ) ) ;
#270 = CARTESIAN_POINT ( 'NONE',  ( 10.26685100253999927, 2.832432432432000269, 6.822293592207000934 ) ) ;
#271 = CARTESIAN_POINT ( 'NONE',  ( 12.33310466175879938, -1.963577280744732700, -13.86161695422964435 ) ) ;
#272 = ADVANCED_FACE ( 'NONE', ( #33201 ), #34811, .F. ) ;
#273 = CARTESIAN_POINT ( 'NONE',  ( 10.96949144726329806, -4.580206776679999869, -6.681274802424499448 ) ) ;
#274 = CARTESIAN_POINT ( 'NONE',  ( 18.22725926606490532, 3.461153921112412934, 12.03746648326613133 ) ) ;
#275 = CARTESIAN_POINT ( 'NONE',  ( 18.18412234634031677, -2.838955764657545178, 12.27602435542072001 ) ) ;
#276 = ORIENTED_EDGE ( 'NONE', *, *, #50855, .T. ) ;
#277 = CARTESIAN_POINT ( 'NONE',  ( 11.63611496860034933, -2.828587461987000395, -6.899705789500199415 ) ) ;
#278 = ORIENTED_EDGE ( 'NONE', *, *, #15421, .F. ) ;
#279 = CONICAL_SURFACE ( 'NONE', #19241, 5.886037960926999268, 0.3217505543965463732 ) ;
#280 = CARTESIAN_POINT ( 'NONE',  ( 11.44730853405000204, -12.38161968051000095, -1.492087993499999987 ) ) ;
#281 = CARTESIAN_POINT ( 'NONE',  ( 4.900006121741999898, 1.007237960741801164, 1.747572776708514297 ) ) ;
#282 = CARTESIAN_POINT ( 'NONE',  ( 10.98768521492000083, -5.299565686336999981, -4.945211137252000455 ) ) ;
#283 = LINE ( 'NONE', #64587, #6388 ) ;
#284 = CARTESIAN_POINT ( 'NONE',  ( 24.30000000000000071, 2.548720605937000006, 12.21654710926000220 ) ) ;
#285 = CARTESIAN_POINT ( 'NONE',  ( 24.02043810212400032, -12.55433174484000070, 3.484779853151999784 ) ) ;
#286 = CARTESIAN_POINT ( 'NONE',  ( 10.19255830160000009, 2.560287027313000063, 7.664549200117999561 ) ) ;
#287 = ORIENTED_EDGE ( 'NONE', *, *, #54615, .F. ) ;
#288 = LINE ( 'NONE', #16362, #21275 ) ;
#289 = CARTESIAN_POINT ( 'NONE',  ( 9.194604681486000075, 5.157771204918000230, 8.637848577075999401 ) ) ;
#290 = CARTESIAN_POINT ( 'NONE',  ( 2.071806799209333416, 3.408904368339104263, 0.9161175952574878156 ) ) ;
#291 = CARTESIAN_POINT ( 'NONE',  ( 11.06591429142999949, -3.980313504646230349, 8.533318907609000803 ) ) ;
#292 = CARTESIAN_POINT ( 'NONE',  ( 11.29999334531184552, -11.74553346643965490, -1.558194258341520699 ) ) ;
#293 = CARTESIAN_POINT ( 'NONE',  ( 11.14595257254739913, 3.168263696564200149, -7.741895249827200232 ) ) ;
#294 = CARTESIAN_POINT ( 'NONE',  ( 12.24435292127285457, -0.2761699508452415963, 12.69595998167824114 ) ) ;
#295 = CARTESIAN_POINT ( 'NONE',  ( 8.241841482360854343, 3.974357482335666436, -8.874747363613822770 ) ) ;
#296 = ADVANCED_FACE ( 'NONE', ( #16756 ), #38788, .T. ) ;
#297 = CARTESIAN_POINT ( 'NONE',  ( 9.814910518647794291, 2.650130971540564317, -7.499994893876710478 ) ) ;
#298 = B_SPLINE_SURFACE_WITH_KNOTS ( 'NONE', 1, 3, ( 
 ( #36914, #9639, #20138, #1143, #64749, #9988, #794, #31326, #57534, #6370, #16864, #59521, #32957, #54271, #27720, #57888, #22453, #65093, #20482, #63112, #9292, #51944, #4044, #25381, #52296, #62775, #14897, #4393, #15239, #52637, #4732, #26076, #47405, #68709, #1833, #12323, #28061, #7414, #23497, #39935, #7767, #45525, #50766, #66835, #61253, #28763, #39582, #7071, #28408, #13371, #17570, #39237, #38897, #60218, #33306, #59864, #8114, #17919, #23151, #49371, #23845, #50076, #49724, #34696, #11970, #18262, #44500, #1485, #60562, #33654, #18608, #56007, #65793, #24188, #18947, #29458, #12669, #2860, #33999, #54624, #55317, #6721, #2182, #22801, #65450, #44838, #54971, #44152, #66144, #60906 ),
 ( #29109, #13023, #34350, #55669, #50415, #2518, #45180, #66485, #25906, #31169, #47237, #41642, #61593, #9821, #57367, #30471, #51446, #52472, #29803, #67171, #13710, #15071, #51786, #19981, #25565, #35039, #4570, #62947, #20315, #4228, #51107, #8800, #61938, #3883, #35716, #8459, #14734, #14051, #68540, #36397, #40276, #67515, #41303, #57033, #19636, #46892, #56353, #3209, #24536, #3541, #46208, #62612, #40610, #30140, #45862, #57713, #19285, #35379, #36052, #9134, #14399, #46554, #56700, #9471, #24878, #40957, #62280, #25216, #67857, #30813, #68196, #52124, #20662, #41988, #52823, #26256, #53164, #64672, #63295, #53849, #54188, #15423, #5947, #5265, #36748, #31501, #714, #58069, #6287, #27634 ) ),
 .UNSPECIFIED., .F., .F., .F.,
 ( 2, 2 ),
 ( 4, 2, 2, 2, 2, 2, 2, 2, 2, 2, 2, 2, 2, 2, 2, 2, 2, 2, 2, 2, 2, 2, 2, 2, 2, 2, 2, 2, 2, 2, 2, 2, 2, 2, 2, 2, 2, 2, 2, 2, 2, 2, 2, 2, 4 ),
 ( 0.000000000000000000, 1.000000000000000000 ),
 ( 0.000000000000000000, 7.143002489358809843E-05, 0.0001428600497871761969, 0.0002142900746807642953, 0.0002857200995743523937, 0.0003214351120211464429, 0.0003571501244679404921, 0.0003928651369147345414, 0.0004285801493615285906, 0.0005000101742551166890, 0.0005357251867019107924, 0.0005714401991487047874, 0.0006071552115954987824, 0.0006428702240422928859, 0.0007143002489358809843, 0.0007857302738294690827, 0.0008214452862762631861, 0.0008571602987230571812, 0.0009285903236166452796, 0.001000020348510233378, 0.001071450373403821585, 0.001142880398297409575, 0.001214310423190997565, 0.001285740448084585772, 0.001321455460531379984, 0.001357170472978173979, 0.001428600497871761969, 0.001500030522765349959, 0.001535745535212143954, 0.001571460547658938165, 0.001607175560105732377, 0.001642890572552526372, 0.001714320597446114362, 0.001750035609892908357, 0.001785750622339702352, 0.001821465634786496347, 0.001857180647233290559, 0.001928610672126878766, 0.001964325684573672761, 0.002000040697020466756, 0.002035755709467261185, 0.002071470721914055180, 0.002142900746807643170, 0.002214330771701231160, 0.002285760796594819150 ),
 .UNSPECIFIED. ) ;
#299 = ORIENTED_EDGE ( 'NONE', *, *, #35075, .F. ) ;
#300 = FACE_OUTER_BOUND ( 'NONE', #44362, .T. ) ;
#301 = CARTESIAN_POINT ( 'NONE',  ( 6.928706320015000308, -0.2869491282519000541, -1.095445449434000018 ) ) ;
#302 = ADVANCED_FACE ( 'NONE', ( #33547 ), #22385, .T. ) ;
#303 = EDGE_CURVE ( 'NONE', #62021, #50139, #529, .T. ) ;
#304 = CARTESIAN_POINT ( 'NONE',  ( 18.12478797189196555, 2.757742546077707857, 13.61537068597721856 ) ) ;
#305 = APPLICATION_CONTEXT ( 'automotive_design' ) ;
#306 = CARTESIAN_POINT ( 'NONE',  ( 24.72544608131600086, 8.702416312035001766, -9.187185040898000921 ) ) ;
#307 = CARTESIAN_POINT ( 'NONE',  ( 10.94072200990529886, -5.077092948368999714, -7.124286150322599376 ) ) ;
#308 = ORIENTED_EDGE ( 'NONE', *, *, #5264, .T. ) ;
#309 = AXIS2_PLACEMENT_3D ( 'NONE', #43572, #37285, #64184 ) ;
#310 = DIRECTION ( 'NONE',  ( 1.000000000000000000, 0.000000000000000000, 0.000000000000000000 ) ) ;
#311 = CARTESIAN_POINT ( 'NONE',  ( 8.437857780412000963, 2.606995215518000286, 6.345762205468999717 ) ) ;
#314 = CARTESIAN_POINT ( 'NONE',  ( 17.55505043854144276, -0.6250000000000001110, -25.00000000000000000 ) ) ;
#313 = CARTESIAN_POINT ( 'NONE',  ( 9.152520280414000453, 4.102804347295999854, -5.770625657082999460 ) ) ;
#312 = PRODUCT_DEFINITION_CONTEXT ( 'detailed design', #15925, 'design' ) ;
#315 = DIRECTION ( 'NONE',  ( -1.000000000000000000, 0.000000000000000000, 0.000000000000000000 ) ) ;
#316 = ORIENTED_EDGE ( 'NONE', *, *, #45064, .F. ) ;
#317 = CARTESIAN_POINT ( 'NONE',  ( 9.444315208305999576, 2.927258006877999641, 8.897018628538001295 ) ) ;
#318 = CARTESIAN_POINT ( 'NONE',  ( 17.60327209889956279, -1.789008353514938809, -13.88522434179080101 ) ) ;
#319 = CARTESIAN_POINT ( 'NONE',  ( 10.29262282008599882, 4.451581486939200083, 6.771613406921599854 ) ) ;
#320 = CARTESIAN_POINT ( 'NONE',  ( 10.64872180584000105, -2.614778238704999591, 6.717279975758000177 ) ) ;
#321 = CARTESIAN_POINT ( 'NONE',  ( 7.127706853208000126, -4.698358408974000255, 8.789434435623999065 ) ) ;
#322 = ORIENTED_EDGE ( 'NONE', *, *, #42337, .T. ) ;
#323 = CARTESIAN_POINT ( 'NONE',  ( 8.829017219593000121, 5.290207928847999064, 8.768105151414001597 ) ) ;
#324 = EDGE_CURVE ( 'NONE', #49260, #51205, #2147, .T. ) ;
#326 = CARTESIAN_POINT ( 'NONE',  ( 10.41025564679000048, -4.690690303276999984, -6.142863315966000215 ) ) ;
#325 = CARTESIAN_POINT ( 'NONE',  ( 10.45222191436347714, 4.437430566769827500, -6.743201413565676816 ) ) ;
#327 = CARTESIAN_POINT ( 'NONE',  ( 7.869532996850215234, -3.050177706499410668, 8.968124616582409558 ) ) ;
#328 = VECTOR ( 'NONE', #55122, 1000.000000000000114 ) ;
#329 = CARTESIAN_POINT ( 'NONE',  ( 10.09196524370999981, -3.841385669346000231, 5.536421174581999338 ) ) ;
#330 = CARTESIAN_POINT ( 'NONE',  ( 24.15421034170099901, 3.593683958043000004, 12.72347868493999989 ) ) ;
#331 = ORIENTED_EDGE ( 'NONE', *, *, #21053, .T. ) ;
#332 = DIRECTION ( 'NONE',  ( 1.000000000000000000, 0.000000000000000000, 0.000000000000000000 ) ) ;
#333 = CARTESIAN_POINT ( 'NONE',  ( 10.87872469555899890, -3.497841151814999883, 8.368784980615899372 ) ) ;
#334 = CARTESIAN_POINT ( 'NONE',  ( 10.98579841651039857, 3.550031058388499972, 6.303820944768999901 ) ) ;
#335 = ORIENTED_EDGE ( 'NONE', *, *, #34880, .T. ) ;
#336 = CARTESIAN_POINT ( 'NONE',  ( 9.518314158773000244, 4.845406482350000488, -6.387189183984999907 ) ) ;
#337 = CARTESIAN_POINT ( 'NONE',  ( 12.50285324413422394, 1.826185914346435180, -12.46695919779662098 ) ) ;
#338 = CARTESIAN_POINT ( 'NONE',  ( 11.47124174884019965, -4.036194082918090231, 6.184229974648999928 ) ) ;
#339 = CARTESIAN_POINT ( 'NONE',  ( 7.951287431685589269, 4.953067615740292418, -6.432288716792883498 ) ) ;
#340 = CARTESIAN_POINT ( 'NONE',  ( 18.17508454104003945, 2.579277621789493047, -13.65633006993505205 ) ) ;
#341 = ORIENTED_EDGE ( 'NONE', *, *, #30199, .F. ) ;
#342 = CARTESIAN_POINT ( 'NONE',  ( 9.475279990687596410, 5.350441389720215213, 7.499985493516660107 ) ) ;
#343 = CARTESIAN_POINT ( 'NONE',  ( 5.752943173017458278, 1.199500263597271577, -0.9218200799623702535 ) ) ;
#344 = ORIENTED_EDGE ( 'NONE', *, *, #13743, .T. ) ;
#345 = CARTESIAN_POINT ( 'NONE',  ( 12.58137933218757887, -3.164643396295688138, -12.19610741112356678 ) ) ;
#346 = CARTESIAN_POINT ( 'NONE',  ( 10.74795391537419853, 4.830118059977199785, 6.936213817702099327 ) ) ;
#347 = CARTESIAN_POINT ( 'NONE',  ( 10.25036334590211773, 3.059888261081768590, -8.493457116339008905 ) ) ;
#348 = CARTESIAN_POINT ( 'NONE',  ( 11.05220172819000091, 2.768652217526999859, -4.974789451568000231 ) ) ;
#349 = CARTESIAN_POINT ( 'NONE',  ( 8.222961399606997901, 4.680050665548002087, 6.135920769709001021 ) ) ;
#350 = CARTESIAN_POINT ( 'NONE',  ( 10.92717634842000152, -5.023656093247000243, 8.718039182945998888 ) ) ;
#351 = CARTESIAN_POINT ( 'NONE',  ( 17.77734287254348544, -0.6847469513499682137, -12.58138041838080490 ) ) ;
#352 = B_SPLINE_CURVE_WITH_KNOTS ( 'NONE', 3,
 ( #56236, #18494, #65060, #55897 ),
 .UNSPECIFIED., .F., .F.,
 ( 4, 4 ),
 ( 0.000000000000000000, 0.5000000026798849806 ),
 .UNSPECIFIED. ) ;
#353 = EDGE_CURVE ( 'NONE', #93, #10401, #47217, .T. ) ;
#354 = CARTESIAN_POINT ( 'NONE',  ( 12.37651575364836098, 2.955073904862975720, -12.33383124654925567 ) ) ;
#355 = CARTESIAN_POINT ( 'NONE',  ( 10.55103166480599874, -5.000984463463999496, -7.570575893572789816 ) ) ;
#356 = CARTESIAN_POINT ( 'NONE',  ( 9.266948341230998309, 3.049618631524000367, 6.392542946894000266 ) ) ;
#357 = ORIENTED_EDGE ( 'NONE', *, *, #14220, .T. ) ;
#358 = CONICAL_SURFACE ( 'NONE', #32750, 12.71246950475999959, 0.8960553845711767273 ) ;
#359 = AXIS2_PLACEMENT_3D ( 'NONE', #39, #4584, #43386 ) ;
#360 =( LENGTH_UNIT ( ) NAMED_UNIT ( * ) SI_UNIT ( .MILLI., .METRE. ) );
#361 = DIRECTION ( 'NONE',  ( 0.000000000000000000, 1.000000000000000000, 0.000000000000000000 ) ) ;
#362 = DIRECTION ( 'NONE',  ( 0.000000000000000000, -1.000000000000000000, 0.000000000000000000 ) ) ;
#363 = CARTESIAN_POINT ( 'NONE',  ( 23.56665676678100141, -0.02078841289292433087, 13.98987519048835360 ) ) ;
#364 = PRODUCT_DEFINITION_SHAPE ( 'NONE', 'NONE',  #69206 ) ;
#365 = CARTESIAN_POINT ( 'NONE',  ( 18.17347573203822009, 2.104651709959050265, 12.42298141210392970 ) ) ;
#366 = DIRECTION ( 'NONE',  ( 0.000000000000000000, -0.7198977633594745296, 0.6940801180771755119 ) ) ;
#367 = CARTESIAN_POINT ( 'NONE',  ( 10.87889121877999976, 9.617170530054998778, 5.911408669357999912 ) ) ;
#368 = LINE ( 'NONE', #31851, #12349 ) ;
#369 = CARTESIAN_POINT ( 'NONE',  ( 10.08351354018237345, -2.750000000000000000, -7.663624617374468428 ) ) ;
#370 = ORIENTED_EDGE ( 'NONE', *, *, #4078, .T. ) ;
#371 = CARTESIAN_POINT ( 'NONE',  ( 12.27369669298503574, -2.970039040581493595, 12.24495604130071946 ) ) ;
#372 = CARTESIAN_POINT ( 'NONE',  ( 9.099784697134998268, -3.380386586585000241, -6.540930833646799947 ) ) ;
#373 = DIRECTION ( 'NONE',  ( 1.000000000000000000, 4.884985026250000111E-14, 0.000000000000000000 ) ) ;
#374 = CARTESIAN_POINT ( 'NONE',  ( 10.06844525594999951, -4.148609764890999863, 8.941457795715999524 ) ) ;
#375 = CARTESIAN_POINT ( 'NONE',  ( 11.19872335273220010, -3.650693637952500126, 6.559289673553299060 ) ) ;
#376 = CONICAL_SURFACE ( 'NONE', #56224, 0.9999998338055000602, 0.7853981908209605178 ) ;
#377 = CARTESIAN_POINT ( 'NONE',  ( 11.18687482311539938, 5.057677595549000316, -7.927326830586499007 ) ) ;
#378 = CARTESIAN_POINT ( 'NONE',  ( 12.61757266016683410, 0.6952251598378623720, 12.58080715426405938 ) ) ;
#379 = CARTESIAN_POINT ( 'NONE',  ( 8.717397846562217723, 3.754687009553119736, 6.659228100213050006 ) ) ;
#380 = CARTESIAN_POINT ( 'NONE',  ( 5.028782850970884510, 0.9602633891249825471, -0.7171280660100972648 ) ) ;
#381 = CARTESIAN_POINT ( 'NONE',  ( 12.58060354176263296, 1.796139714418076627, 12.47132288122299570 ) ) ;
#383 = PLANE ( 'NONE',  #54416 ) ;
#382 = CARTESIAN_POINT ( 'NONE',  ( 10.41690035061499842, 4.304339077956200299, -8.600505223349999895 ) ) ;
#384 = CARTESIAN_POINT ( 'NONE',  ( 10.84226088462129844, 4.002427228022017225, -6.359261544073000039 ) ) ;
#385 = CARTESIAN_POINT ( 'NONE',  ( 7.893560293058006216, 2.859109450078002546, -6.778905949012001386 ) ) ;
#386 = EDGE_CURVE ( 'NONE', #57373, #55782, #131, .T. ) ;
#387 = CARTESIAN_POINT ( 'NONE',  ( 17.60000000085000238, 12.11987927271999865, -3.159802730921999814 ) ) ;
#388 = CARTESIAN_POINT ( 'NONE',  ( 10.99999999997000089, 4.000000000000000000, 7.500000000000000000 ) ) ;
#390 = CARTESIAN_POINT ( 'NONE',  ( 18.16002653637816167, -0.1622975230824323101, 12.69869204565316601 ) ) ;
#389 = CARTESIAN_POINT ( 'NONE',  ( 7.826132327310000747, 5.086383815897999483, 6.522343373212003748 ) ) ;
#391 = FACE_OUTER_BOUND ( 'NONE', #34041, .T. ) ;
#392 = ORIENTED_EDGE ( 'NONE', *, *, #24053, .T. ) ;
#393 = CARTESIAN_POINT ( 'NONE',  ( 12.76469316422328859, 0.6249999999999994449, 12.67928922306548145 ) ) ;
#394 = DIRECTION ( 'NONE',  ( 0.000000000000000000, -0.7071067811865475727, -0.7071067811865475727 ) ) ;
#395 = CARTESIAN_POINT ( 'NONE',  ( 18.00086602808685754, -0.5750310236731011049, -12.58704914195511293 ) ) ;
#396 = CARTESIAN_POINT ( 'NONE',  ( 11.00000000000000000, 3.031410575668799900, 7.825000000000000178 ) ) ;
#397 = CARTESIAN_POINT ( 'NONE',  ( 12.21870270123690183, -2.283379404039359351, 13.71702370352176104 ) ) ;
#398 = CARTESIAN_POINT ( 'NONE',  ( 10.96083988456000036, 2.844674717313000034, 5.100114893396999527 ) ) ;
#399 = CARTESIAN_POINT ( 'NONE',  ( 10.99999975383417627, 2.937013229513552925, 7.633391978603163430 ) ) ;
#400 = EDGE_LOOP ( 'NONE', ( #33240, #49205, #31738, #46802 ) ) ;
#401 = ADVANCED_FACE ( 'NONE', ( #48505 ), #41881, .F. ) ;
#402 = CARTESIAN_POINT ( 'NONE',  ( 7.199141827028999963, 0.000000000000000000, 0.000000000000000000 ) ) ;
#403 = CARTESIAN_POINT ( 'NONE',  ( 11.16486084871730000, -2.792989229543000107, -7.174999999999999822 ) ) ;
#404 = VECTOR ( 'NONE', #30309, 1000.000000000000000 ) ;
#405 = CARTESIAN_POINT ( 'NONE',  ( 11.09999999999999964, 4.000000000000000000, 7.500000000000000000 ) ) ;
#406 = FACE_OUTER_BOUND ( 'NONE', #31055, .T. ) ;
#407 = ADVANCED_FACE ( 'NONE', ( #22962 ), #48160, .F. ) ;
#408 = CARTESIAN_POINT ( 'NONE',  ( 17.72806902343758040, 3.100663240735257897, -12.29112607895898890 ) ) ;
#409 = LINE ( 'NONE', #47627, #4203 ) ;
#410 = CARTESIAN_POINT ( 'NONE',  ( 11.04749144726329924, 3.499163784537000055, 8.206726025856399431 ) ) ;
#411 = B_SPLINE_CURVE_WITH_KNOTS ( 'NONE', 3,
 ( #32955, #65091, #6719, #11273 ),
 .UNSPECIFIED., .F., .F.,
 ( 4, 4 ),
 ( 0.000000000000000000, 1.000000000000000000 ),
 .UNSPECIFIED. ) ;
#412 = B_SPLINE_CURVE_WITH_KNOTS ( 'NONE', 3,
 ( #28021, #10975, #54929, #1442, #55625, #33954, #64101, #28714 ),
 .UNSPECIFIED., .F., .F.,
 ( 4, 1, 1, 1, 1, 4 ),
 ( 0.000000000000000000, 0.2000000000000000111, 0.4000000000000000222, 0.5999999999999999778, 0.8000000000000000444, 1.000000000000000000 ),
 .UNSPECIFIED. ) ;
#413 = CARTESIAN_POINT ( 'NONE',  ( 10.96029575260939204, -3.171266584307757874, 6.746534734305131842 ) ) ;
#414 = CARTESIAN_POINT ( 'NONE',  ( 10.10735564678999943, -4.293585439421999439, -8.994200998147999115 ) ) ;
#415 = CARTESIAN_POINT ( 'NONE',  ( 4.677943173015960632, -0.9218200799623716968, -1.199500263597270910 ) ) ;
#416 = CARTESIAN_POINT ( 'NONE',  ( 21.60000021221999944, -12.84999978760999895, -2.874109817690000262E-09 ) ) ;
#417 = DIRECTION ( 'NONE',  ( -0.000000000000000000, 0.6555644356537908557, 0.7551392392836745460 ) ) ;
#418 = DIRECTION ( 'NONE',  ( -1.000000000000000000, 0.000000000000000000, 0.000000000000000000 ) ) ;
#419 = ORIENTED_EDGE ( 'NONE', *, *, #22122, .T. ) ;
#420 = CARTESIAN_POINT ( 'NONE',  ( 9.401145280412999128, 3.927090956378999742, -9.230892435423001530 ) ) ;
#422 = CONICAL_SURFACE ( 'NONE', #39511, 13.04999999969999891, 0.7853981633972997312 ) ;
#421 = CARTESIAN_POINT ( 'NONE',  ( 10.80903300763299946, -3.402282662142699809, 6.873077781830399857 ) ) ;
#423 = EDGE_LOOP ( 'NONE', ( #35216, #41530, #64033, #16512, #37170, #10912, #48215, #947, #69122, #9098 ) ) ;
#424 = CARTESIAN_POINT ( 'NONE',  ( 17.57587793826700562, -3.124999446933518943, 13.52084426442465315 ) ) ;
#425 = CARTESIAN_POINT ( 'NONE',  ( 10.47303166480599934, -5.137916160623999140, -7.580230465881790280 ) ) ;
#426 = VERTEX_POINT ( 'NONE', #5845 ) ;
#427 = CARTESIAN_POINT ( 'NONE',  ( 10.43614141025499897, 4.549633050978300730, 6.521048559232099251 ) ) ;
#428 = CARTESIAN_POINT ( 'NONE',  ( 6.180771831090410728, 0.3343430079570269275, 1.082181004987261330 ) ) ;
#430 = DIRECTION ( 'NONE',  ( 0.9999999999999473754, 3.241492201312155981E-07, 2.435229255853115792E-09 ) ) ;
#429 = CIRCLE ( 'NONE', #68538, 2.000000000000001776 ) ;
#431 = CARTESIAN_POINT ( 'NONE',  ( 18.35295676019000055, -2.690485605734000085, 11.48482900035000043 ) ) ;
#432 = CARTESIAN_POINT ( 'NONE',  ( 11.27745123989519982, -3.589787500396900199, -8.292221125039500151 ) ) ;
#433 = CARTESIAN_POINT ( 'NONE',  ( 12.60522794377905775, 0.5937363472582638524, -13.88293910736286030 ) ) ;
#434 = CARTESIAN_POINT ( 'NONE',  ( 29.60000000000000142, 0.000000000000000000, 0.000000000000000000 ) ) ;
#435 = ADVANCED_FACE ( 'NONE', ( #64566 ), #48853, .T. ) ;
#436 = CARTESIAN_POINT ( 'NONE',  ( 10.52663358771999924, -4.933730002636999679, -6.506004698255999585 ) ) ;
#437 = CARTESIAN_POINT ( 'NONE',  ( 13.64504292973000332, 11.45087266113000091, 2.419799131125000002 ) ) ;
#438 = VERTEX_POINT ( 'NONE', #64909 ) ;
#439 = CARTESIAN_POINT ( 'NONE',  ( 7.614999999996999946, 5.349999999999999645, -7.500000000000000000 ) ) ;
#440 = ORIENTED_EDGE ( 'NONE', *, *, #23269, .T. ) ;
#441 = CARTESIAN_POINT ( 'NONE',  ( 9.934212804449000345, 5.120437537252000126, -8.883398686237999442 ) ) ;
#442 = ORIENTED_EDGE ( 'NONE', *, *, #23207, .F. ) ;
#443 = LINE ( 'NONE', #11611, #41449 ) ;
#444 = CARTESIAN_POINT ( 'NONE',  ( 18.09708155689165565, -2.811828937043457266, -12.37344130164188805 ) ) ;
#445 = CARTESIAN_POINT ( 'NONE',  ( 16.86666666157666583, 3.216308280197299752, 11.40341444503674850 ) ) ;
#446 = DIRECTION ( 'NONE',  ( 1.000000000000000000, 0.000000000000000000, 0.000000000000000000 ) ) ;
#447 = B_SPLINE_SURFACE_WITH_KNOTS ( 'NONE', 3, 3, ( 
 ( #68396, #63151, #9675, #42537, #51644, #8995, #69101, #31026, #41500, #35913, #63846, #15279, #3741, #52335, #46754, #36603, #4428, #15958, #9328 ),
 ( #51979, #4084, #31363, #47440, #68747, #16985, #54748, #5474, #65577, #11064, #16301, #38316, #32735, #38670, #42880, #54053, #58960, #32057, #53373 ),
 ( #32398, #6501, #53713, #576, #33085, #21887, #28183, #16646, #65227, #59644, #43222, #5808, #11742, #64527, #6847, #59293, #49499, #27150, #17340 ),
 ( #37972, #22926, #11397, #1609, #64874, #33431, #44277, #43574, #10710, #26810, #54399, #37289, #27846, #1265, #49153, #58608, #48123, #229, #43921 ) ),
 .UNSPECIFIED., .F., .F., .F.,
 ( 4, 4 ),
 ( 4, 1, 1, 1, 1, 1, 1, 1, 1, 1, 1, 1, 1, 1, 1, 1, 4 ),
 ( -0.1039370721279000015, 1.103937072127999963 ),
 ( 0.5600558712726999566, 0.5880915265348000132, 0.6161271817967999276, 0.6441628370587999530, 0.6721984923209000096, 0.7002341475828999240, 0.7282698028449000605, 0.7563054581070000060, 0.7843411133690000314, 0.8123767686310000569, 0.8404124238931000024, 0.8684480791551000278, 0.8964837344171000533, 0.9245193896790999677, 0.9525550449412000242, 0.9805907002032000497, 1.008626355465000124 ),
 .UNSPECIFIED. ) ;
#448 = CARTESIAN_POINT ( 'NONE',  ( 10.29378083128999855, -3.483628580733000302, 6.176326635498999629 ) ) ;
#449 = CARTESIAN_POINT ( 'NONE',  ( 12.18127378141864980, 0.04040202251154181162, 13.89992604541790477 ) ) ;
#450 = ORIENTED_EDGE ( 'NONE', *, *, #10251, .T. ) ;
#451 = CARTESIAN_POINT ( 'NONE',  ( 12.21268235885900033, 11.62758720635999765, -4.758865308234000224 ) ) ;
#452 = CARTESIAN_POINT ( 'NONE',  ( 18.19608105989800251, 11.86124369401000145, -3.532130569927999897 ) ) ;
#453 = CARTESIAN_POINT ( 'NONE',  ( 9.150912690312626552, 3.194792839887663938, 7.157693560935859622 ) ) ;
#454 = CARTESIAN_POINT ( 'NONE',  ( 4.446647932087000044, 1.441877299643999910, 0.3432711633658000472 ) ) ;
#455 = AXIS2_PLACEMENT_3D ( 'NONE', #28603, #17765, #7956 ) ;
#456 = CARTESIAN_POINT ( 'NONE',  ( 11.41486084871699802, 2.792989229543000107, 7.174999999999999822 ) ) ;
#457 = CARTESIAN_POINT ( 'NONE',  ( 17.98628609634500108, -3.388648274289000284, 11.90503202562999974 ) ) ;
#458 = CARTESIAN_POINT ( 'NONE',  ( 10.36629943602999937, -5.852732332139999549, -7.568014220767000033 ) ) ;
#459 = ORIENTED_EDGE ( 'NONE', *, *, #4248, .T. ) ;
#460 = ORIENTED_EDGE ( 'NONE', *, *, #48777, .T. ) ;
#461 = CARTESIAN_POINT ( 'NONE',  ( 8.821685841230998193, 2.633142096252999664, -7.791134854666999843 ) ) ;
#462 = CARTESIAN_POINT ( 'NONE',  ( 7.883148997456999929, 5.167567567567999731, 6.822293592207000934 ) ) ;
#463 = DIRECTION ( 'NONE',  ( -0.9486832980505238710, 8.389526310658208895E-10, -0.3162277660168079652 ) ) ;
#464 = CYLINDRICAL_SURFACE ( 'NONE', #11206, 1.500000000000000000 ) ;
#465 = CARTESIAN_POINT ( 'NONE',  ( 12.71012035425584763, 0.7146386402729469900, 12.57972080578532470 ) ) ;
#466 = EDGE_CURVE ( 'NONE', #45574, #28824, #50443, .T. ) ;
#467 = ADVANCED_FACE ( 'NONE', ( #50232 ), #38152, .T. ) ;
#468 = CARTESIAN_POINT ( 'NONE',  ( 11.63611496860034933, 5.171412538012999605, -6.899705789500199415 ) ) ;
#469 = CARTESIAN_POINT ( 'NONE',  ( 10.19190035061499877, 4.267716286314199969, -8.468075389605498771 ) ) ;
#471 = CARTESIAN_POINT ( 'NONE',  ( 23.60000000000000142, -9.305479840184000651, 8.315530346521999405 ) ) ;
#470 = CARTESIAN_POINT ( 'NONE',  ( 10.17832996542199986, -4.602191201513400109, 6.876242273533999416 ) ) ;
#472 = STYLED_ITEM ( 'NONE', ( #6780 ), #31992 ) ;
#473 = FACE_OUTER_BOUND ( 'NONE', #7500, .T. ) ;
#474 = ORIENTED_EDGE ( 'NONE', *, *, #22248, .F. ) ;
#475 = ADVANCED_FACE ( 'NONE', ( #66987 ), #44994, .T. ) ;
#476 = DIRECTION ( 'NONE',  ( 1.000000000000000000, 0.000000000000000000, 0.000000000000000000 ) ) ;
#477 = AXIS2_PLACEMENT_3D ( 'NONE', #56146, #39734, #50561 ) ;
#478 = CARTESIAN_POINT ( 'NONE',  ( 9.318721994369999706, -2.755032632138999737, 8.795122807847999269 ) ) ;
#479 = CARTESIAN_POINT ( 'NONE',  ( 9.758342523874999230, 2.871335344632000020, 7.672773098917999413 ) ) ;
#480 = CARTESIAN_POINT ( 'NONE',  ( 11.35394314717303388, -3.574441963229890717, 11.79291588350140252 ) ) ;
#481 = B_SPLINE_CURVE_WITH_KNOTS ( 'NONE', 3,
 ( #46917, #10879, #49, #58772, #15446 ),
 .UNSPECIFIED., .F., .F.,
 ( 4, 1, 4 ),
 ( 0.000000000000000000, 0.5000000000000000000, 1.000000000000000000 ),
 .UNSPECIFIED. ) ;
#482 = CARTESIAN_POINT ( 'NONE',  ( 9.504901164121001500, -3.934733502342999678, 5.704835336325999151 ) ) ;
#483 = CARTESIAN_POINT ( 'NONE',  ( 17.63847140754354470, 3.120744938278101177, -12.28504437646774328 ) ) ;
#484 = CARTESIAN_POINT ( 'NONE',  ( 9.780103651350286142, -2.899999999999999911, -6.453331515098025051 ) ) ;
#485 = EDGE_CURVE ( 'NONE', #31101, #42061, #40421, .T. ) ;
#486 = CARTESIAN_POINT ( 'NONE',  ( 10.16455864497999961, -3.101067942814400347, -8.204026508301600629 ) ) ;
#487 = B_SPLINE_CURVE_WITH_KNOTS ( 'NONE', 3,
 ( #56245, #40501, #34592, #24770, #50999, #23736, #61490, #8693, #13265, #40173, #7660, #28652, #18847, #3434, #19524, #62167 ),
 .UNSPECIFIED., .F., .F.,
 ( 4, 2, 2, 2, 2, 2, 2, 4 ),
 ( 0.000000000000000000, 0.2499999999999993339, 0.3749999999999994449, 0.4999999999999995559, 0.6249999999999996669, 0.7499999999999997780, 0.8749999999999998890, 1.000000000000000000 ),
 .UNSPECIFIED. ) ;
#488 = CARTESIAN_POINT ( 'NONE',  ( 5.375631947951000633, -0.1057711097905999903, -1.318062398728999884 ) ) ;
#489 = EDGE_CURVE ( 'NONE', #48158, #58325, #17998, .T. ) ;
#490 = CARTESIAN_POINT ( 'NONE',  ( 10.90299135172148226, -3.204747416617449218, 7.862853843651285146 ) ) ;
#491 = CARTESIAN_POINT ( 'NONE',  ( 11.49999672494999992, 5.885481364898664580, -10.12743717035875157 ) ) ;
#492 = EDGE_LOOP ( 'NONE', ( #43852, #65890, #15231, #61686 ) ) ;
#493 = CARTESIAN_POINT ( 'NONE',  ( 12.52804317529069955, 0.5603556898929429320, -12.68335562943301476 ) ) ;
#494 = CARTESIAN_POINT ( 'NONE',  ( 11.14595257254739913, 3.168263696564200149, -7.741895249827200232 ) ) ;
#495 = DIRECTION ( 'NONE',  ( 0.000000000000000000, -1.000000000000000000, 0.000000000000000000 ) ) ;
#496 = PLANE ( 'NONE',  #6664 ) ;
#497 = DIRECTION ( 'NONE',  ( 0.000000000000000000, -1.000000000000000000, 0.000000000000000000 ) ) ;
#498 = ORIENTED_EDGE ( 'NONE', *, *, #46740, .T. ) ;
#499 = CARTESIAN_POINT ( 'NONE',  ( 25.08881866225100410, -11.66016336090999950, -3.018804192941999975 ) ) ;
#500 = CARTESIAN_POINT ( 'NONE',  ( 11.10612378248509913, -4.482960757953799558, -6.586279795136899651 ) ) ;
#501 = CARTESIAN_POINT ( 'NONE',  ( 18.17180710799850374, 0.1030387083473175008, 12.69945707558845704 ) ) ;
#502 = DIRECTION ( 'NONE',  ( 0.000000000000000000, -1.000000000000000000, 0.000000000000000000 ) ) ;
#503 = CARTESIAN_POINT ( 'NONE',  ( 11.04664311227086415, 4.444039568019538144, -8.706333095531743282 ) ) ;
#504 = CARTESIAN_POINT ( 'NONE',  ( 10.56591429142999949, 4.019686495353769651, -6.466681092390999197 ) ) ;
#505 = ORIENTED_EDGE ( 'NONE', *, *, #36321, .F. ) ;
#506 = VECTOR ( 'NONE', #37555, 1000.000000000000000 ) ;
#507 = CARTESIAN_POINT ( 'NONE',  ( 10.18909467608999897, -5.907859813488999912, 7.801539220053999912 ) ) ;
#508 = CARTESIAN_POINT ( 'NONE',  ( 17.92121436125177070, 3.006915247989151219, -13.55278817016120740 ) ) ;
#509 = VERTEX_POINT ( 'NONE', #29617 ) ;
#510 = CARTESIAN_POINT ( 'NONE',  ( 4.599999999999999645, 1.875000000000000000, -13.78631952119025073 ) ) ;
#511 = DIRECTION ( 'NONE',  ( -0.7071052132515089905, -0.7071083491181088254, 2.836092545889034718E-08 ) ) ;
#512 = CARTESIAN_POINT ( 'NONE',  ( 15.35917414208899956, 8.811049802147000065, 7.563839685023999948 ) ) ;
#513 = ORIENTED_EDGE ( 'NONE', *, *, #37970, .T. ) ;
#514 = CARTESIAN_POINT ( 'NONE',  ( 10.90000000000000036, 0.2500000000000000000, 4.902439024389999567 ) ) ;
#515 = CARTESIAN_POINT ( 'NONE',  ( 7.762835841224000610, 4.574593532473000046, -5.689090339675999530 ) ) ;
#516 = CARTESIAN_POINT ( 'NONE',  ( 10.30226354018233437, -5.092232985442821658, -6.870476274536374994 ) ) ;
#517 = CARTESIAN_POINT ( 'NONE',  ( 7.198460030931516762, 4.679653997254563436, -8.679420697515526584 ) ) ;
#518 = VERTEX_POINT ( 'NONE', #61745 ) ;
#519 = CARTESIAN_POINT ( 'NONE',  ( 9.104016254283999743, -5.045864843302999780, 8.527867871227000407 ) ) ;
#520 = CARTESIAN_POINT ( 'NONE',  ( 24.48565841892600048, 12.12924569191000046, -3.164390090946999745 ) ) ;
#522 = CARTESIAN_POINT ( 'NONE',  ( 25.46372676430900128, 8.354609436172999892, -8.148458316574000548 ) ) ;
#521 = B_SPLINE_CURVE_WITH_KNOTS ( 'NONE', 3,
 ( #66809, #55639, #22770, #44121, #29079, #18920 ),
 .UNSPECIFIED., .F., .F.,
 ( 4, 2, 4 ),
 ( 0.000000000000000000, 0.5000000000000000000, 1.000000000000000000 ),
 .UNSPECIFIED. ) ;
#523 = VERTEX_POINT ( 'NONE', #44659 ) ;
#524 = AXIS2_PLACEMENT_3D ( 'NONE', #22459, #44507, #60569 ) ;
#525 = DIRECTION ( 'NONE',  ( 0.8987684456439055669, 0.000000000000000000, -0.4384236320214022764 ) ) ;
#526 = DIRECTION ( 'NONE',  ( 0.000000000000000000, 0.9553735099700838562, 0.2954005017724949944 ) ) ;
#527 = ORIENTED_EDGE ( 'NONE', *, *, #38514, .F. ) ;
#528 = CARTESIAN_POINT ( 'NONE',  ( 23.56664309646999911, -10.37807348783000094, 9.381504613656002078 ) ) ;
#529 = B_SPLINE_CURVE_WITH_KNOTS ( 'NONE', 3,
 ( #14964, #10403, #31745, #53061 ),
 .UNSPECIFIED., .F., .F.,
 ( 4, 4 ),
 ( 0.000000000000000000, 0.1253970409990855239 ),
 .UNSPECIFIED. ) ;
#530 = CARTESIAN_POINT ( 'NONE',  ( 17.97864539808068329, 0.4596704780454121120, -13.88977177191355139 ) ) ;
#531 = CARTESIAN_POINT ( 'NONE',  ( 5.332217238860999409, 0.4341136435772000035, 1.348325027692000022 ) ) ;
#532 = VECTOR ( 'NONE', #65504, 1000.000000000000114 ) ;
#533 = FACE_OUTER_BOUND ( 'NONE', #790, .T. ) ;
#534 = EDGE_CURVE ( 'NONE', #39090, #52961, #7578, .T. ) ;
#535 = CARTESIAN_POINT ( 'NONE',  ( 16.39944283128300029, 3.410739012457999930, 11.89826262991000050 ) ) ;
#536 = CARTESIAN_POINT ( 'NONE',  ( 7.243250223023721901, 3.136812440417415804, -8.580788443034522928 ) ) ;
#537 = CARTESIAN_POINT ( 'NONE',  ( 24.16219604515211117, 12.44497281315807413, 3.348778968579924520 ) ) ;
#538 = ADVANCED_FACE ( 'NONE', ( #39747 ), #65951, .T. ) ;
#539 = ORIENTED_EDGE ( 'NONE', *, *, #30229, .F. ) ;
#540 = CARTESIAN_POINT ( 'NONE',  ( 8.726787239609997471, 3.780467314030099946, -8.340498368324299250 ) ) ;
#541 = ORIENTED_EDGE ( 'NONE', *, *, #19877, .T. ) ;
#542 = CARTESIAN_POINT ( 'NONE',  ( 9.945533384955998812, 2.906048475816000121, 8.880389653997999844 ) ) ;
#543 = CARTESIAN_POINT ( 'NONE',  ( 4.587940964153251144, -1.500000000000001332, 0.3220548830679713093 ) ) ;
#544 = CIRCLE ( 'NONE', #61931, 0.5999999999999999778 ) ;
#545 = CARTESIAN_POINT ( 'NONE',  ( 18.38566024598074833, -11.99831085744367165, 3.595680291927078276 ) ) ;
#546 = CARTESIAN_POINT ( 'NONE',  ( 12.61254665343898651, 3.094705746550272529, -13.52917745889216228 ) ) ;
#547 = CARTESIAN_POINT ( 'NONE',  ( 11.09999999999999964, 4.000000000000000000, 7.500000000000000000 ) ) ;
#548 = CARTESIAN_POINT ( 'NONE',  ( 25.25778303248700141, 2.569631777580000165, 11.37091703377000051 ) ) ;
#549 = CARTESIAN_POINT ( 'NONE',  ( 17.65768761389442787, -0.6168528257048858654, 13.88157091029611045 ) ) ;
#550 = CARTESIAN_POINT ( 'NONE',  ( 10.90000000016000037, -2.832432432627000285, -6.822293591557000880 ) ) ;
#551 = B_SPLINE_CURVE_WITH_KNOTS ( 'NONE', 3,
 ( #46391, #63486, #3386, #19819 ),
 .UNSPECIFIED., .F., .F.,
 ( 4, 4 ),
 ( 0.000000000000000000, 1.000000000000000000 ),
 .UNSPECIFIED. ) ;
#552 = B_SPLINE_CURVE_WITH_KNOTS ( 'NONE', 3,
 ( #4825, #10765, #5523, #63558 ),
 .UNSPECIFIED., .F., .F.,
 ( 4, 4 ),
 ( 0.000000000000000000, 1.000000000000000000 ),
 .UNSPECIFIED. ) ;
#553 = ORIENTED_EDGE ( 'NONE', *, *, #2355, .F. ) ;
#554 = CARTESIAN_POINT ( 'NONE',  ( 12.53086501621864635, 0.5620205154750185228, 13.88470856849518675 ) ) ;
#555 = CARTESIAN_POINT ( 'NONE',  ( 11.23964560330029983, -3.608363763633400279, 8.716526793355999558 ) ) ;
#556 = PLANE ( 'NONE',  #3403 ) ;
#557 = CARTESIAN_POINT ( 'NONE',  ( 15.89994436294300151, 8.847904542234999781, 8.580301953175000662 ) ) ;
#558 = EDGE_CURVE ( 'NONE', #9109, #56864, #53026, .T. ) ;
#559 = ADVANCED_FACE ( 'NONE', ( #55130 ), #12482, .F. ) ;
#560 = CARTESIAN_POINT ( 'NONE',  ( 7.705394353206999725, -3.245532552444000185, 8.949627348471000943 ) ) ;
#562 = CARTESIAN_POINT ( 'NONE',  ( 7.851684996376999237, -4.710033951126000318, 6.351751497389999557 ) ) ;
#561 = CARTESIAN_POINT ( 'NONE',  ( 10.19255830160000009, 2.560287027313000063, 7.664549200117999561 ) ) ;
#563 = CARTESIAN_POINT ( 'NONE',  ( 10.49764694612699856, 2.940513484064000149, -7.922821994243300914 ) ) ;
#564 = EDGE_CURVE ( 'NONE', #28902, #67173, #57226, .T. ) ;
#565 = CARTESIAN_POINT ( 'NONE',  ( 24.60999195316300003, -8.752663949940000521, -9.057796881813999335 ) ) ;
#566 = PRODUCT_DEFINITION_FORMATION_WITH_SPECIFIED_SOURCE ( 'ANY', '', #18770, .NOT_KNOWN. ) ;
#567 = CARTESIAN_POINT ( 'NONE',  ( 8.969113844317998741, 4.218953675027299788, -6.661091642253600398 ) ) ;
#568 = CARTESIAN_POINT ( 'NONE',  ( 17.93538082550040613, -0.4959841406075954362, 12.68696163625449103 ) ) ;
#569 = CARTESIAN_POINT ( 'NONE',  ( 11.09999999999999787, -5.533462193136272411, 7.009885406647008210 ) ) ;
#570 = CARTESIAN_POINT ( 'NONE',  ( 17.97872601847819851, -3.578425380680470447, 12.00298730842247252 ) ) ;
#571 = ORIENTED_EDGE ( 'NONE', *, *, #6260, .F. ) ;
#572 = CARTESIAN_POINT ( 'NONE',  ( 9.406706853206999952, -3.705847642455000202, 9.096432253453999195 ) ) ;
#573 = CARTESIAN_POINT ( 'NONE',  ( 8.722714158775000115, 3.892978337449999771, -8.893414073324001023 ) ) ;
#574 = CARTESIAN_POINT ( 'NONE',  ( 8.599999952505998024, 4.000000000000000000, 7.500000000000000000 ) ) ;
#575 = CYLINDRICAL_SURFACE ( 'NONE', #60048, 0.5000000000000004441 ) ;
#576 = CARTESIAN_POINT ( 'NONE',  ( 0.3377116734105999885, 1.258511261458999941, -3.306246502378999974 ) ) ;
#577 = EDGE_CURVE ( 'NONE', #1541, #49491, #24675, .T. ) ;
#578 = AXIS2_PLACEMENT_3D ( 'NONE', #48457, #16634, #59282 ) ;
#579 = CARTESIAN_POINT ( 'NONE',  ( 10.40480513895999870, 4.779740423663599636, 7.933462475324499330 ) ) ;
#580 = CARTESIAN_POINT ( 'NONE',  ( 1.932518698273000046, 1.300495226975000085, -3.293006394410000315 ) ) ;
#581 = ORIENTED_EDGE ( 'NONE', *, *, #21347, .T. ) ;
#582 = CARTESIAN_POINT ( 'NONE',  ( 12.53842182639420244, -0.6689867242971878625, -12.58222862546947241 ) ) ;
#583 = CARTESIAN_POINT ( 'NONE',  ( 9.470944094206000585, -5.100000000000000533, 6.571291218949999902 ) ) ;
#584 = CARTESIAN_POINT ( 'NONE',  ( 17.81282484970910573, 3.152868460668829975, -12.19915726504404851 ) ) ;
#585 = CARTESIAN_POINT ( 'NONE',  ( 5.596495275685874127, 12.13697930370352296, 3.751366953416817029 ) ) ;
#586 = CARTESIAN_POINT ( 'NONE',  ( 8.026329719592000700, 5.601795057054999916, 7.176148573050999957 ) ) ;
#587 = ORIENTED_EDGE ( 'NONE', *, *, #5822, .F. ) ;
#588 = CARTESIAN_POINT ( 'NONE',  ( 5.629173046212000209, -1.056937757944000023, -1.220746830110999825 ) ) ;
#589 = CARTESIAN_POINT ( 'NONE',  ( 8.105004719587000750, 2.627120679234999923, -8.556648795244999661 ) ) ;
#590 = CARTESIAN_POINT ( 'NONE',  ( 8.432199894032919474, -2.299073235464944798, 7.876362923782135539 ) ) ;
#591 = CARTESIAN_POINT ( 'NONE',  ( 9.218784697134999817, -3.305825103746500293, 8.574479223074998657 ) ) ;
#592 = ORIENTED_EDGE ( 'NONE', *, *, #31679, .T. ) ;
#593 = CARTESIAN_POINT ( 'NONE',  ( 15.99022209853100129, -3.654801648850000362, -11.82543339652000114 ) ) ;
#594 = CARTESIAN_POINT ( 'NONE',  ( 11.71278712779700015, 11.72302084951000190, 1.966028253584000129 ) ) ;
#595 = ORIENTED_EDGE ( 'NONE', *, *, #47317, .T. ) ;
#596 = CARTESIAN_POINT ( 'NONE',  ( 11.10000000000000142, 2.402782103116360979, -8.046943094580276679 ) ) ;
#597 = CARTESIAN_POINT ( 'NONE',  ( 7.732053840042254045, -3.067861470021875814, 6.507875357840980257 ) ) ;
#598 = CARTESIAN_POINT ( 'NONE',  ( 17.81326568215976636, -0.5695321295966285779, -13.88429381145914299 ) ) ;
#599 = ORIENTED_EDGE ( 'NONE', *, *, #49645, .F. ) ;
#600 = CARTESIAN_POINT ( 'NONE',  ( 10.28566371494471632, -5.375939593780930892, -6.377587382198379728 ) ) ;
#601 = CARTESIAN_POINT ( 'NONE',  ( 9.079784991436001818, 7.881284392328999466, 5.316045437065000101 ) ) ;
#602 = CARTESIAN_POINT ( 'NONE',  ( 24.32158614469118518, -12.72716443521392016, 3.095238905934254880 ) ) ;
#603 = CARTESIAN_POINT ( 'NONE',  ( 9.004094043040858253, -2.621318921512024946, 6.376249635427098994 ) ) ;
#605 = AXIS2_PLACEMENT_3D ( 'NONE', #58152, #41390, #62024 ) ;
#604 = CARTESIAN_POINT ( 'NONE',  ( 11.19041504065829962, -2.975441626403999784, 8.263934892306599167 ) ) ;
#606 = VERTEX_POINT ( 'NONE', #23655 ) ;
#607 = CARTESIAN_POINT ( 'NONE',  ( 7.256079719589999755, 2.531201476950000195, 8.216704145297999418 ) ) ;
#608 = ORIENTED_EDGE ( 'NONE', *, *, #1012, .T. ) ;
#609 = CARTESIAN_POINT ( 'NONE',  ( 10.11094409420000062, 5.100000000000000533, -6.571291218949999902 ) ) ;
#610 = CARTESIAN_POINT ( 'NONE',  ( 15.39165415090800337, -9.395515400280999074, -8.199438574490999443 ) ) ;
#611 = CARTESIAN_POINT ( 'NONE',  ( 9.056630296855326279, -5.100000000000000533, 6.328714934328742103 ) ) ;
#612 = ORIENTED_EDGE ( 'NONE', *, *, #21132, .T. ) ;
#613 = B_SPLINE_SURFACE_WITH_KNOTS ( 'NONE', 3, 3, ( 
 ( #37486, #31912, #20724, #14796, #5326, #20038, #26668, #47984, #15137, #57429, #36115, #42052, #31566, #58467, #4984, #21069, #25628, #47300, #9888, #15820, #86, #25972, #51846, #42737, #36458, #9535, #25283, #4633, #64041, #41367, #47646, #16162, #46617, #58812, #4292 ),
 ( #30533, #3944, #30880, #26318, #52193, #36812, #46956, #68259, #41705, #63008, #57777, #31229, #52536, #68604, #63358, #15485, #58130, #10231, #54603, #43434, #6007, #17900, #33636, #38166, #48323, #49350, #65428, #49014, #11949, #59496, #54248, #27347, #32260, #53569, #427 ),
 ( #44483, #16844, #21743, #39217, #1121, #59843, #1812, #10916, #23132, #5664, #11594, #32593, #27005, #54952, #17551, #44130, #33288, #48669, #1465, #43075, #22780, #64382, #49703, #16503, #37830, #59153, #11255, #65774, #53907, #32938, #774, #22089, #22434, #64728, #6350 ),
 ( #27698, #43776, #6701, #65070, #38877, #17190, #60199, #38521, #28042, #12303, #7053, #28389, #50745, #23481, #14033, #50058, #56681, #35359, #45161, #18243, #44820, #2842, #61575, #19264, #13691, #51088, #55649, #8095, #39917, #24518, #8780, #55991, #12649, #3190, #66467 ) ),
 .UNSPECIFIED., .F., .F., .F.,
 ( 4, 4 ),
 ( 4, 1, 1, 1, 1, 1, 1, 1, 1, 1, 1, 1, 1, 1, 1, 1, 1, 1, 1, 1, 1, 1, 1, 1, 1, 1, 1, 1, 1, 1, 1, 1, 4 ),
 ( -0.02000000000000000042, 1.020000000000000018 ),
 ( 0.1633025096610999927, 0.1899619885200000136, 0.2166214673788000034, 0.2432809462376999965, 0.2699404250964999585, 0.2965999039553000038, 0.3232593828141999692, 0.3499188616730000145, 0.3765783405318000043, 0.4032378193906999697, 0.4298972982494999595, 0.4565567771083000048, 0.4832162559671999702, 0.5098757348260000155, 0.5365352136848999809, 0.5631946925437000262, 0.5898541714025000715, 0.6165136502614000369, 0.6431731291201999712, 0.6698326079790000165, 0.6964920868378999819, 0.7231515656967000272, 0.7498110445554999615, 0.7764705234143999268, 0.8031300022731999722, 0.8297894811320000175, 0.8564489599908999828, 0.8831084388497000282, 0.9097679177085999935, 0.9364273965674000388, 0.9630868754261999731, 0.9897463542851000495, 1.016405833144000015 ),
 .UNSPECIFIED. ) ;
#614 = CARTESIAN_POINT ( 'NONE',  ( 12.55381283423609418, -1.927626388171778116, -12.56664888159296112 ) ) ;
#615 = PRODUCT_DEFINITION_FORMATION_WITH_SPECIFIED_SOURCE ( 'ANY', '', #3696, .NOT_KNOWN. ) ;
#616 = LINE ( 'NONE', #53412, #60037 ) ;
#617 = FACE_OUTER_BOUND ( 'NONE', #1285, .T. ) ;
#618 = EDGE_CURVE ( 'NONE', #41936, #57550, #68288, .T. ) ;
#619 = CARTESIAN_POINT ( 'NONE',  ( 24.30001697352500045, -3.271769158411000245, -12.21048181092999840 ) ) ;
#620 = CARTESIAN_POINT ( 'NONE',  ( 12.15267534726965337, -2.198616041048526704, -13.82629894333309295 ) ) ;
#621 = ADVANCED_FACE ( 'NONE', ( #24348 ), #36555, .F. ) ;
#622 = CARTESIAN_POINT ( 'NONE',  ( 11.58071932425156980, -4.167269912168199753, -8.628410767520000135 ) ) ;
#623 = CARTESIAN_POINT ( 'NONE',  ( 10.40769129028899975, 3.110563525881361535, 6.586710612921465646 ) ) ;
#624 = CARTESIAN_POINT ( 'NONE',  ( 18.25535445515778576, -2.667446342172965501, 12.31441698789904393 ) ) ;
#625 = ORIENTED_EDGE ( 'NONE', *, *, #32487, .T. ) ;
#626 = CARTESIAN_POINT ( 'NONE',  ( 11.39189666366029918, -4.052152326617509459, -8.673729056199000809 ) ) ;
#627 = ORIENTED_EDGE ( 'NONE', *, *, #37110, .F. ) ;
#628 = CARTESIAN_POINT ( 'NONE',  ( 11.48828127163000268, -12.23964378314000001, -1.839251152677999990 ) ) ;
#629 = VECTOR ( 'NONE', #51467, 1000.000000000000000 ) ;
#630 = CARTESIAN_POINT ( 'NONE',  ( 11.97657389914466819, -4.648774973711785385, 6.404407512144051573 ) ) ;
#631 = B_SPLINE_CURVE_WITH_KNOTS ( 'NONE', 3,
 ( #60194, #12642, #28735, #50050, #49008, #43068, #64375, #6000, #44477, #65769, #33973, #59145, #27341, #22429, #767, #16838, #43428, #64722, #38160, #11587, #59837, #32931, #11942, #54241, #33282, #29083, #14027, #51081, #19609, #40929, #29778, #57008, #35013, #55983, #30117, #24162, #3184, #35692, #51758, #61911, #50393, #39910, #24512, #40585, #66117, #61569, #44814, #45833, #45154, #8432, #2493, #23475, #66812, #35352, #18237, #45498, #66461, #39558, #46181, #8775, #56675, #14373, #67488, #51420, #18583, #60882, #3515, #62251, #8089, #61229, #2836, #23817, #12998, #13345, #18923, #34322, #40248, #13684, #9108, #34670, #24853, #30446, #29432, #67145, #55642, #56328, #19258, #50738, #7741, #31476, #4202 ),
 .UNSPECIFIED., .F., .F.,
 ( 4, 1, 1, 1, 1, 1, 1, 1, 1, 1, 1, 1, 1, 1, 1, 1, 1, 1, 1, 1, 1, 1, 1, 1, 1, 1, 1, 1, 1, 1, 1, 1, 1, 1, 1, 1, 1, 1, 1, 1, 1, 1, 1, 1, 1, 1, 1, 1, 1, 1, 1, 1, 1, 1, 1, 1, 1, 1, 1, 1, 1, 1, 1, 1, 1, 1, 1, 1, 1, 1, 1, 1, 1, 1, 1, 1, 1, 1, 1, 1, 1, 1, 1, 1, 1, 1, 1, 1, 4 ),
 ( 0.000000000000000000, 0.004874450823355541522, 0.009661345194022003327, 0.01436103260279607101, 0.01897537103212419002, 0.02350775731914938119, 0.02796115294545339219, 0.03233656637161005237, 0.03663363768239984858, 0.04085119304253923694, 0.04498768735433079924, 0.04904154886712413369, 0.05301143935174792293, 0.05689644225696363633, 0.06069618962671503859, 0.06441093687713574101, 0.06804159303743011200, 0.07158970920874503652, 0.07498141635100204205, 0.08501006463908243604, 0.09841337508356413910, 0.1118176718332323377, 0.1187820131990808270, 0.1252437490255899066, 0.1404218166617251795, 0.1574035577456479040, 0.1761129495041070525, 0.1966414853897626713, 0.2019033837996370984, 0.2100638602301221347, 0.2234696548173721320, 0.2414626216399035907, 0.2502561337435587063, 0.2678629632046341524, 0.2752677410504689171, 0.2907998480710696776, 0.3002851497986598339, 0.3238876161481084592, 0.3442582269590512833, 0.3613588172231308460, 0.3751465592194264675, 0.3959010830434372408, 0.4196307664705191121, 0.4463514864640283908, 0.4514228443006744196, 0.4597736081350440318, 0.4670316664865736267, 0.4731994725281417624, 0.4907875272513019804, 0.4999891125105156986, 0.5206125037787298071, 0.5393828774126382397, 0.5563118703635043794, 0.5713334752878752587, 0.5782068158715422124, 0.5847575811334744245, 0.5906763917012011200, 0.5981799785644238421, 0.6175854672771887710, 0.6249630545279218907, 0.6409200020002955300, 0.6581577244971096308, 0.6766092828860079678, 0.6963689643179452604, 0.7014886240358610969, 0.7097912278688763843, 0.7168462699965328921, 0.7232171845259283138, 0.7405756818954355447, 0.7500085531557023621, 0.7700661893775517797, 0.7886464287371296455, 0.8057650030297832666, 0.8213545077432261587, 0.8410359930661466255, 0.8481241221261679453, 0.8668504199967879131, 0.8749138338875376286, 0.8911902668814143391, 0.9085325902296357281, 0.9268791062040830919, 0.9463236143299509351, 0.9513222611507794468, 0.9597458290560116900, 0.9666803444524524336, 0.9731718905766858496, 0.9852515542005497728, 0.9942041435450702513, 1.000000000000000000 ),
 .UNSPECIFIED. ) ;
#632 = CARTESIAN_POINT ( 'NONE',  ( 5.077371418665322267, -0.3835488334464972615, 1.315173458188629851 ) ) ;
#633 = CARTESIAN_POINT ( 'NONE',  ( 10.25166529434999951, -3.418639857622999934, -8.733652610425998830 ) ) ;
#634 = AXIS2_PLACEMENT_3D ( 'NONE', #59823, #28367, #23107 ) ;
#635 = CARTESIAN_POINT ( 'NONE',  ( 11.58810207955139937, -4.796537143354000499, 7.825000000000000178 ) ) ;
#636 = CARTESIAN_POINT ( 'NONE',  ( 23.86822025922500146, -13.28639123634000008, 3.449149526223000084 ) ) ;
#637 = CARTESIAN_POINT ( 'NONE',  ( 10.44079719460000000, 5.435719122931000236, 7.303631812894000319 ) ) ;
#638 = ORIENTED_EDGE ( 'NONE', *, *, #47754, .F. ) ;
#639 = CARTESIAN_POINT ( 'NONE',  ( 10.85646369190719973, -5.100000000000000533, 6.665341197380437066 ) ) ;
#640 = CARTESIAN_POINT ( 'NONE',  ( 10.93227693248999977, 2.539877577705000000, 6.453611809651000009 ) ) ;
#641 = PLANE ( 'NONE',  #30391 ) ;
#642 = CARTESIAN_POINT ( 'NONE',  ( 11.19057802013490033, -5.033226574983999946, 7.524052967375959966 ) ) ;
#643 = CARTESIAN_POINT ( 'NONE',  ( 17.60000001994400165, -11.53041320601000130, 4.891397783926000109 ) ) ;
#644 = CARTESIAN_POINT ( 'NONE',  ( 11.49056651104150006, 4.085456792591960706, -6.638028001068500217 ) ) ;
#645 = ADVANCED_FACE ( 'NONE', ( #36905 ), #41460, .T. ) ;
#646 = CARTESIAN_POINT ( 'NONE',  ( 7.100000000000154188, 5.265235852882342193, -6.934887023210864143 ) ) ;
#647 = FACE_OUTER_BOUND ( 'NONE', #28213, .T. ) ;
#648 = CARTESIAN_POINT ( 'NONE',  ( 23.52034043602500191, -10.38860555204000136, 9.575296714885999094 ) ) ;
#649 = ORIENTED_EDGE ( 'NONE', *, *, #42532, .T. ) ;
#650 = DIRECTION ( 'NONE',  ( 1.000000000000000000, 0.000000000000000000, -1.736057635220000058E-14 ) ) ;
#651 = CARTESIAN_POINT ( 'NONE',  ( 6.895498187670000334, -0.7063073661229000155, -0.8851390247125999755 ) ) ;
#652 = CARTESIAN_POINT ( 'NONE',  ( 18.08647318473500221, 2.829117779091812501, 13.59807435138920617 ) ) ;
#653 = CARTESIAN_POINT ( 'NONE',  ( 10.66922466734516739, 4.845815779105637766, 4.789865691387857893 ) ) ;
#654 = CARTESIAN_POINT ( 'NONE',  ( 10.34995525820099971, -4.107710726525199973, -6.364355462479999836 ) ) ;
#655 = ORIENTED_EDGE ( 'NONE', *, *, #20266, .T. ) ;
#656 =( GEOMETRIC_REPRESENTATION_CONTEXT ( 3 ) GLOBAL_UNCERTAINTY_ASSIGNED_CONTEXT ( ( #63933 ) ) GLOBAL_UNIT_ASSIGNED_CONTEXT ( ( #8267, #61410, #19098 ) ) REPRESENTATION_CONTEXT ( 'NONE', 'WORKASPACE' ) );
#657 = CARTESIAN_POINT ( 'NONE',  ( 9.099999886593998610, -3.819167204710999825E-14, 1.447156853930999928E-13 ) ) ;
#658 = CARTESIAN_POINT ( 'NONE',  ( 7.577017219590000074, 5.480308727866000318, 8.192324747680999053 ) ) ;
#659 = EDGE_CURVE ( 'NONE', #35912, #16031, #57879, .T. ) ;
#660 = VECTOR ( 'NONE', #36324, 1000.000000000000000 ) ;
#662 = CARTESIAN_POINT ( 'NONE',  ( 10.98937577273789046, -4.461177266722074819, -8.699885912910444219 ) ) ;
#661 = CARTESIAN_POINT ( 'NONE',  ( 9.608904719592000987, 4.946705552514000459, -6.253848946732999181 ) ) ;
#663 = CARTESIAN_POINT ( 'NONE',  ( 3.148789388360131447, -0.09951366136684100527, -3.256401652200602737 ) ) ;
#664 = VERTEX_POINT ( 'NONE', #9284 ) ;
#665 = CARTESIAN_POINT ( 'NONE',  ( 9.611387933856001098, 3.334846092635999959, 5.869117602953000556 ) ) ;
#666 = CARTESIAN_POINT ( 'NONE',  ( 18.27992102884633141, -2.544330805874861934, -13.76687901878135278 ) ) ;
#667 = CARTESIAN_POINT ( 'NONE',  ( 10.45257053952200010, 3.605640676136899980, 8.422730500489899796 ) ) ;
#668 = CARTESIAN_POINT ( 'NONE',  ( 10.98286725694000054, -3.998514182530999772, 9.091066422484001208 ) ) ;
#669 = CARTESIAN_POINT ( 'NONE',  ( 7.833769353207999941, -2.583664704444999849, 6.684748541034000624 ) ) ;
#670 = ORIENTED_EDGE ( 'NONE', *, *, #63025, .T. ) ;
#671 = CARTESIAN_POINT ( 'NONE',  ( 8.205992358809998777, -3.399999999999999911, 6.138278517058000538 ) ) ;
#673 = CARTESIAN_POINT ( 'NONE',  ( 10.29666814679000097, -2.755511079787000384, -6.622434938646999392 ) ) ;
#672 = CARTESIAN_POINT ( 'NONE',  ( 12.38412398422500083, -11.44428158143999852, 4.450268217599000486 ) ) ;
#674 = CARTESIAN_POINT ( 'NONE',  ( 7.771548168530000744, -5.066493862386956870, 8.873801325387214334 ) ) ;
#675 = CARTESIAN_POINT ( 'NONE',  ( 10.58844302970999962, -3.754658547780000521, 5.545362468768000319 ) ) ;
#677 = CARTESIAN_POINT ( 'NONE',  ( 11.46989666366029859, -4.058428102321880004, -8.814970315645998866 ) ) ;
#676 = CIRCLE ( 'NONE', #63137, 2.250000000000000000 ) ;
#678 = ORIENTED_EDGE ( 'NONE', *, *, #66237, .T. ) ;
#679 = CARTESIAN_POINT ( 'NONE',  ( 9.446013540182333301, 3.000416447002273834, -8.268183399968640046 ) ) ;
#680 = CARTESIAN_POINT ( 'NONE',  ( 11.34641504065830020, -3.195537720350400068, 8.099826052678000821 ) ) ;
#681 = VECTOR ( 'NONE', #12487, 1000.000000000000000 ) ;
#682 = CARTESIAN_POINT ( 'NONE',  ( 11.61759063708296047, 5.217265640542000149, 7.157757529645699890 ) ) ;
#683 = VERTEX_POINT ( 'NONE', #46710 ) ;
#684 = B_SPLINE_CURVE_WITH_KNOTS ( 'NONE', 3,
 ( #26074, #9986, #26422, #58569 ),
 .UNSPECIFIED., .F., .F.,
 ( 4, 4 ),
 ( 0.000000000000000000, 1.000000000000000000 ),
 .UNSPECIFIED. ) ;
#685 = CARTESIAN_POINT ( 'NONE',  ( 8.921614158776000281, 3.251172436837000301, -6.320036569851000152 ) ) ;
#686 = CARTESIAN_POINT ( 'NONE',  ( 12.15211780798802188, 2.166395227764201792, -12.41237995041120712 ) ) ;
#687 = CARTESIAN_POINT ( 'NONE',  ( 11.51790547754520055, -2.825704134258000266, 7.462730980357120458 ) ) ;
#688 = PLANE ( 'NONE',  #67510 ) ;
#689 = CARTESIAN_POINT ( 'NONE',  ( 18.07075314651731546, 2.853223032301765105, -13.59217294861458036 ) ) ;
#690 = ORIENTED_EDGE ( 'NONE', *, *, #61029, .F. ) ;
#691 = CARTESIAN_POINT ( 'NONE',  ( 8.946004440379999423, -5.458705123429999695, 7.456451825584000659 ) ) ;
#692 = CARTESIAN_POINT ( 'NONE',  ( 23.72390849569146454, 9.881471858020274723, 9.454770968183350277 ) ) ;
#693 = ORIENTED_EDGE ( 'NONE', *, *, #12418, .T. ) ;
#694 = CARTESIAN_POINT ( 'NONE',  ( 12.50326937753805190, -3.134539878383340472, -12.20388000700442355 ) ) ;
#695 = CARTESIAN_POINT ( 'NONE',  ( 11.31410538575739899, 4.975963290822400076, 7.733337754805098996 ) ) ;
#696 = CARTESIAN_POINT ( 'NONE',  ( 10.00637913184999839, 5.119263020957999899, 8.420380450036001108 ) ) ;
#697 = CARTESIAN_POINT ( 'NONE',  ( 10.01277517397999972, 3.440623091551000101, -9.267603345544999982 ) ) ;
#698 = EDGE_CURVE ( 'NONE', #53063, #51133, #31661, .T. ) ;
#699 = CARTESIAN_POINT ( 'NONE',  ( 9.140654977342494547, 5.049579698492543400, -6.802596805975135830 ) ) ;
#700 = CARTESIAN_POINT ( 'NONE',  ( 13.64731601457200050, 9.647116713587001513, 7.903424745186999445 ) ) ;
#701 = EDGE_CURVE ( 'NONE', #59694, #61758, #40523, .T. ) ;
#702 = CARTESIAN_POINT ( 'NONE',  ( 17.65049462686344128, -0.7131288892044901351, -12.57980326738671906 ) ) ;
#703 = LINE ( 'NONE', #27621, #24063 ) ;
#704 = CARTESIAN_POINT ( 'NONE',  ( 11.33456651104149948, -3.887457492043800311, -6.364824110469998963 ) ) ;
#705 = ADVANCED_FACE ( 'NONE', ( #26415 ), #52981, .T. ) ;
#706 = EDGE_CURVE ( 'NONE', #1057, #51230, #41392, .T. ) ;
#707 = CARTESIAN_POINT ( 'NONE',  ( 8.625073341231001223, 3.117378429069999957, 8.662179062556001341 ) ) ;
#708 = ORIENTED_EDGE ( 'NONE', *, *, #61590, .F. ) ;
#709 = CARTESIAN_POINT ( 'NONE',  ( 23.60205915885299888, -11.53346724329999873, 4.150849519444998137 ) ) ;
#710 = CARTESIAN_POINT ( 'NONE',  ( 9.266851002542999538, 2.832432432432000269, 6.822293592207000934 ) ) ;
#711 = CARTESIAN_POINT ( 'NONE',  ( 11.84785375340600133, 12.11644693747000012, 2.030267990277999868 ) ) ;
#712 = B_SPLINE_CURVE_WITH_KNOTS ( 'NONE', 3,
 ( #8653, #51640, #4081, #36251 ),
 .UNSPECIFIED., .F., .F.,
 ( 4, 4 ),
 ( 0.000000000000000000, 1.000000000000000000 ),
 .UNSPECIFIED. ) ;
#713 = CARTESIAN_POINT ( 'NONE',  ( 18.16391642019718944, 2.089583161048361060, 12.42552483951006614 ) ) ;
#714 = CARTESIAN_POINT ( 'NONE',  ( 12.70945613931266394, 1.793774045999471989, 13.88460948128834538 ) ) ;
#715 = CARTESIAN_POINT ( 'NONE',  ( 11.13250283087000092, 9.191281752207999034, 6.598833342203999308 ) ) ;
#716 = CARTESIAN_POINT ( 'NONE',  ( 10.46144540014562807, -3.652722274830687343, 8.303075619429563403 ) ) ;
#717 = CARTESIAN_POINT ( 'NONE',  ( 10.05226354018249779, -2.907767014557177898, -8.129523725463625894 ) ) ;
#718 = VERTEX_POINT ( 'NONE', #41118 ) ;
#719 = CARTESIAN_POINT ( 'NONE',  ( 12.63802361681261743, -3.180808137691513604, 12.19190235712762416 ) ) ;
#720 = CARTESIAN_POINT ( 'NONE',  ( 10.28824205624999877, -4.360201998293100623, -8.437601616732200327 ) ) ;
#721 = CARTESIAN_POINT ( 'NONE',  ( 9.959641781044998865, 5.406625910119999823, 7.700299649248999678 ) ) ;
#722 = EDGE_CURVE ( 'NONE', #61638, #23923, #32242, .T. ) ;
#723 = CARTESIAN_POINT ( 'NONE',  ( 10.31668414895000119, -3.819528725844000494, 6.062183754159999438 ) ) ;
#724 = AXIS2_PLACEMENT_3D ( 'NONE', #29766, #40575, #8080 ) ;
#725 = CARTESIAN_POINT ( 'NONE',  ( 11.06379841651039797, 3.598362324325699912, -8.567697191971999970 ) ) ;
#726 = CARTESIAN_POINT ( 'NONE',  ( 12.08617037725598031, 0.09400131084486976207, 12.59965472429368916 ) ) ;
#727 = CARTESIAN_POINT ( 'NONE',  ( 8.560885841230001958, 4.228291488957999888, 8.941375734143997889 ) ) ;
#728 = CARTESIAN_POINT ( 'NONE',  ( 4.759810628746807382, -0.7637421492518075006, 0.9236198983835054444 ) ) ;
#729 = CARTESIAN_POINT ( 'NONE',  ( 12.20420485406508782, 2.672372548754606836, 12.40973746665996025 ) ) ;
#730 = CARTESIAN_POINT ( 'NONE',  ( 18.15060209888356724, -3.510419631047395850, -12.02305644365783976 ) ) ;
#731 = CARTESIAN_POINT ( 'NONE',  ( 10.74379975933729980, 5.078682052940000524, -7.128873141726999485 ) ) ;
#732 = CARTESIAN_POINT ( 'NONE',  ( 12.21312755196900390, 11.61418968116140249, -4.689146002353034248 ) ) ;
#733 = CARTESIAN_POINT ( 'NONE',  ( 10.48598278040999965, 5.506034726153999692, -7.274787238512000265 ) ) ;
#734 = CARTESIAN_POINT ( 'NONE',  ( 17.55505043854143565, 1.875000000000000000, -13.78631952119025073 ) ) ;
#736 = CARTESIAN_POINT ( 'NONE',  ( 12.35392836371782188, 2.932699513109607192, 12.34015408322985863 ) ) ;
#735 = CARTESIAN_POINT ( 'NONE',  ( 7.948904172952001801, 4.897346594336003278, 6.290771953639007208 ) ) ;
#737 = DIRECTION ( 'NONE',  ( 0.8660254037844289376, 0.000000000000000000, -0.5000000000000169864 ) ) ;
#738 = ORIENTED_EDGE ( 'NONE', *, *, #19532, .T. ) ;
#739 = CARTESIAN_POINT ( 'NONE',  ( 12.38151466835624070, 0.4597251443544757565, 12.68880184500992137 ) ) ;
#740 = CARTESIAN_POINT ( 'NONE',  ( 8.765417767663000959, 5.029951493281999753, -6.097931603992000404 ) ) ;
#741 = EDGE_CURVE ( 'NONE', #62685, #5496, #3861, .T. ) ;
#742 = CARTESIAN_POINT ( 'NONE',  ( 12.25964841771344638, -11.59985379594602861, 4.724415456180611983 ) ) ;
#743 = CARTESIAN_POINT ( 'NONE',  ( 8.791809814040998816, 4.530359890157599878, 6.814123855771700100 ) ) ;
#744 = EDGE_CURVE ( 'NONE', #12348, #53120, #12170, .T. ) ;
#745 = CARTESIAN_POINT ( 'NONE',  ( 12.08613047971140020, -2.614761652440403150, 13.75367554324229680 ) ) ;
#746 = CARTESIAN_POINT ( 'NONE',  ( 11.13709883525000066, 2.663413669911999904, 5.177930968215000540 ) ) ;
#747 = CARTESIAN_POINT ( 'NONE',  ( 11.00000000000000000, 2.941427501403999667, 7.174999999999999822 ) ) ;
#748 = ORIENTED_EDGE ( 'NONE', *, *, #51140, .F. ) ;
#749 = CARTESIAN_POINT ( 'NONE',  ( 12.10000000004390586, 11.04996331189681946, -3.691231723793510167 ) ) ;
#750 = CARTESIAN_POINT ( 'NONE',  ( 11.37299956498129916, -5.207010770456999893, -7.174999999999999822 ) ) ;
#751 = VECTOR ( 'NONE', #15220, 1000.000000000000000 ) ;
#752 = CARTESIAN_POINT ( 'NONE',  ( 18.23980063401625173, -2.972525811573661692, 11.47315805793748389 ) ) ;
#753 = CARTESIAN_POINT ( 'NONE',  ( 10.14393020684899938, -2.750000000000000000, -7.500000000000000000 ) ) ;
#754 = CARTESIAN_POINT ( 'NONE',  ( 17.81575242098903544, 1.931873426913545355, -12.56596755615859884 ) ) ;
#755 = CARTESIAN_POINT ( 'NONE',  ( 10.45746213570999927, 5.100000000000000533, -6.571291218949999902 ) ) ;
#756 =( GEOMETRIC_REPRESENTATION_CONTEXT ( 3 ) GLOBAL_UNCERTAINTY_ASSIGNED_CONTEXT ( ( #28801 ) ) GLOBAL_UNIT_ASSIGNED_CONTEXT ( ( #13097, #2935, #24264 ) ) REPRESENTATION_CONTEXT ( 'NONE', 'WORKASPACE' ) );
#757 = CARTESIAN_POINT ( 'NONE',  ( 8.342859831669791504, 2.714084127472751629, -7.027014477893811950 ) ) ;
#758 = B_SPLINE_CURVE_WITH_KNOTS ( 'NONE', 3,
 ( #19058, #30584, #36168, #20089, #57480, #2978, #30932, #52242, #34810, #40383 ),
 .UNSPECIFIED., .F., .F.,
 ( 4, 2, 2, 2, 4 ),
 ( 0.1253179912170450105, 0.3126267435314338261, 0.4999354958458225862, 0.6872442481602113462, 0.8745530004746001618 ),
 .UNSPECIFIED. ) ;
#759 = CARTESIAN_POINT ( 'NONE',  ( 15.52628979459879588, 9.187490316955907232, 8.213190486479970076 ) ) ;
#760 = CARTESIAN_POINT ( 'NONE',  ( 10.09249435321000021, -2.841617206345000035, -8.724656239052000828 ) ) ;
#761 = AXIS2_PLACEMENT_3D ( 'NONE', #40490, #29334, #65681 ) ;
#762 = DIRECTION ( 'NONE',  ( -1.000000000000000000, 0.000000000000000000, 0.000000000000000000 ) ) ;
#763 = DIRECTION ( 'NONE',  ( -1.000000000000000000, 0.000000000000000000, 0.000000000000000000 ) ) ;
#764 = CARTESIAN_POINT ( 'NONE',  ( 24.14075320594848861, 9.153203792121958671, -9.127249519516993814 ) ) ;
#765 = DIRECTION ( 'NONE',  ( -0.7660444431190119863, -5.852582307674940185E-12, -0.6427876096864989508 ) ) ;
#766 = ORIENTED_EDGE ( 'NONE', *, *, #53572, .F. ) ;
#767 = CARTESIAN_POINT ( 'NONE',  ( 7.397780563817286215, 2.619533902629167965, 8.557926001834172069 ) ) ;
#768 = CARTESIAN_POINT ( 'NONE',  ( 11.69102897915239936, -3.743141152489600110, 6.529961657816500065 ) ) ;
#769 = ORIENTED_EDGE ( 'NONE', *, *, #2828, .T. ) ;
#770 = AXIS2_PLACEMENT_3D ( 'NONE', #37977, #27155, #33437 ) ;
#771 = CARTESIAN_POINT ( 'NONE',  ( 18.00577237252833385, -2.933105347812601238, 13.57200668515162434 ) ) ;
#772 = CARTESIAN_POINT ( 'NONE',  ( 10.71918447801630059, -2.859536135895000442, -7.474854604063350116 ) ) ;
#773 = ORIENTED_EDGE ( 'NONE', *, *, #61507, .T. ) ;
#774 = CARTESIAN_POINT ( 'NONE',  ( 10.48280513895999988, 4.903310631086600146, 8.002155910165599906 ) ) ;
#775 = CARTESIAN_POINT ( 'NONE',  ( 6.423150728792507813, -0.4364103388565075958, -1.045044225101665614 ) ) ;
#776 = CARTESIAN_POINT ( 'NONE',  ( 24.01910276523975796, 3.345607443898567457, -12.71185236705795418 ) ) ;
#777 = FACE_OUTER_BOUND ( 'NONE', #56163, .T. ) ;
#778 = FACE_OUTER_BOUND ( 'NONE', #54702, .T. ) ;
#779 = CARTESIAN_POINT ( 'NONE',  ( 9.841846873515665450, -4.999583552997724389, -6.731816600031354625 ) ) ;
#780 = CARTESIAN_POINT ( 'NONE',  ( 11.59999999999999964, -4.817420948848700313, -7.174999999999999822 ) ) ;
#781 = AXIS2_PLACEMENT_3D ( 'NONE', #36370, #52797, #57683 ) ;
#782 = CARTESIAN_POINT ( 'NONE',  ( 10.43283788151999936, -3.279327064383000145, -9.029275888523999427 ) ) ;
#783 = CYLINDRICAL_SURFACE ( 'NONE', #42949, 1.350000000000000533 ) ;
#784 = ORIENTED_EDGE ( 'NONE', *, *, #40961, .T. ) ;
#785 = ADVANCED_FACE ( 'NONE', ( #4383, #56855 ), #42154, .T. ) ;
#786 = EDGE_CURVE ( 'NONE', #29932, #48584, #62192, .T. ) ;
#787 = CARTESIAN_POINT ( 'NONE',  ( 8.830545280412000153, 3.207599814920999659, -6.150466394809999571 ) ) ;
#788 = ORIENTED_EDGE ( 'NONE', *, *, #41401, .T. ) ;
#789 = CARTESIAN_POINT ( 'NONE',  ( 15.90018573812399971, 8.493548356068000516, 8.263529029821000904 ) ) ;
#790 = EDGE_LOOP ( 'NONE', ( #8197, #43500, #53236, #46954 ) ) ;
#791 = CARTESIAN_POINT ( 'NONE',  ( 17.77739983953771841, -3.084473828682777974, -12.29598274197197760 ) ) ;
#792 = CARTESIAN_POINT ( 'NONE',  ( 25.09889915318881393, -8.522830760771270775, 8.212608576531337690 ) ) ;
#793 = DIRECTION ( 'NONE',  ( 0.000000000000000000, -0.7270098363383266094, 0.6866270442294852838 ) ) ;
#794 = CARTESIAN_POINT ( 'NONE',  ( 12.64146116164745060, 3.103558470340185504, 13.52669597090169695 ) ) ;
#795 = CARTESIAN_POINT ( 'NONE',  ( 9.423521818475000700, -4.993993578306000103, 8.578110568283999982 ) ) ;
#796 = CARTESIAN_POINT ( 'NONE',  ( 23.56666365135700403, -8.673757318230000735, -7.881093921673004488 ) ) ;
#797 = CARTESIAN_POINT ( 'NONE',  ( 12.30917092924265077, -0.3809766167652373636, 13.89298487834589402 ) ) ;
#798 = VERTEX_POINT ( 'NONE', #25717 ) ;
#799 = CARTESIAN_POINT ( 'NONE',  ( 6.886728317542999633, 3.037137096735000430, -6.379793420563999895 ) ) ;
#800 = CARTESIAN_POINT ( 'NONE',  ( 18.10540495109299997, 12.00990144118000025, -3.349639255392000248 ) ) ;
#801 = EDGE_CURVE ( 'NONE', #38352, #55375, #8952, .T. ) ;
#802 = CARTESIAN_POINT ( 'NONE',  ( 10.26539516633362759, 4.233208782175254647, 6.656705459454948404 ) ) ;
#803 = CARTESIAN_POINT ( 'NONE',  ( 4.686986683301000767, -0.8504805407472000311, 1.028515646795000071 ) ) ;
#804 = VECTOR ( 'NONE', #57381, 1000.000000000000000 ) ;
#805 = CARTESIAN_POINT ( 'NONE',  ( 9.155142860581458208, 2.899999999999999911, -6.163493177590811278 ) ) ;
#806 =( GEOMETRIC_REPRESENTATION_CONTEXT ( 3 ) GLOBAL_UNCERTAINTY_ASSIGNED_CONTEXT ( ( #18298 ) ) GLOBAL_UNIT_ASSIGNED_CONTEXT ( ( #13706, #60212, #45521 ) ) REPRESENTATION_CONTEXT ( 'NONE', 'WORKASPACE' ) );
#807 = CARTESIAN_POINT ( 'NONE',  ( 10.53706676393788300, 5.286158710546891015, -7.027080267280216397 ) ) ;
#808 = CARTESIAN_POINT ( 'NONE',  ( 10.19715077290999972, -4.982624057277000418, -6.124316828241999744 ) ) ;
#809 = ORIENTED_EDGE ( 'NONE', *, *, #32463, .T. ) ;
#810 = CARTESIAN_POINT ( 'NONE',  ( 30.60000000000000142, 0.000000000000000000, 0.000000000000000000 ) ) ;
#811 = CARTESIAN_POINT ( 'NONE',  ( 11.13729092125999998, 5.336331659174000208, -5.186744570729000969 ) ) ;
#812 = VECTOR ( 'NONE', #3122, 999.9999999999998863 ) ;
#813 = LINE ( 'NONE', #29124, #66788 ) ;
#814 = CARTESIAN_POINT ( 'NONE',  ( 17.55505043854147118, -3.248109929747637903, 13.61799478206225444 ) ) ;
#815 = FACE_OUTER_BOUND ( 'NONE', #8987, .T. ) ;
#816 = DIRECTION ( 'NONE',  ( -1.000000000000000000, 0.000000000000000000, 0.000000000000000000 ) ) ;
#817 = CARTESIAN_POINT ( 'NONE',  ( 11.14767835872009982, 3.125658946326500320, -6.948943352864199952 ) ) ;
#818 = CARTESIAN_POINT ( 'NONE',  ( 9.001430433046998303, 3.145249924879699677, -6.972511033848699746 ) ) ;
#820 = CARTESIAN_POINT ( 'NONE',  ( 4.399761055266754539, -0.1241639754006147178, -1.193569193835689379 ) ) ;
#819 = CARTESIAN_POINT ( 'NONE',  ( 9.621088727410999297, -4.863977618062000019, 7.427538838030949719 ) ) ;
#821 = DIRECTION ( 'NONE',  ( -0.4384236320214023319, 0.000000000000000000, -0.8987684456439056779 ) ) ;
#822 = ORIENTED_EDGE ( 'NONE', *, *, #22160, .T. ) ;
#823 = AXIS2_PLACEMENT_3D ( 'NONE', #45975, #56816, #14846 ) ;
#824 = CARTESIAN_POINT ( 'NONE',  ( 11.39700581613019992, 4.869652672166700391, 6.941573685175900010 ) ) ;
#825 = CARTESIAN_POINT ( 'NONE',  ( 10.02990552045999983, -2.506467134554999809, 6.215414506835998942 ) ) ;
#826 = CARTESIAN_POINT ( 'NONE',  ( 10.06229229006299875, 4.987433183662999703, 8.073332500201798823 ) ) ;
#827 = CARTESIAN_POINT ( 'NONE',  ( 5.568708401995168700, -12.91387459874235688, -2.616215378977960970 ) ) ;
#828 = AXIS2_PLACEMENT_3D ( 'NONE', #21507, #9987, #48429 ) ;
#829 = CARTESIAN_POINT ( 'NONE',  ( 9.442841440870999747, -2.691258483914000355, 6.269525829285999663 ) ) ;
#830 = EDGE_CURVE ( 'NONE', #13026, #36556, #49687, .T. ) ;
#831 = CARTESIAN_POINT ( 'NONE',  ( 23.56665657345700282, -13.31365812469000076, 4.296923216748999685 ) ) ;
#832 = CARTESIAN_POINT ( 'NONE',  ( 10.56059687351646481, 4.629523725463624118, 6.407767014557177454 ) ) ;
#833 = CARTESIAN_POINT ( 'NONE',  ( 9.128076168957999670, -4.509700402263200125, -8.365475476407400635 ) ) ;
#834 = B_SPLINE_CURVE_WITH_KNOTS ( 'NONE', 3,
 ( #1682, #43648, #12175, #38390, #60071, #63918 ),
 .UNSPECIFIED., .F., .F.,
 ( 4, 1, 1, 4 ),
 ( 0.000000000000000000, 0.1550125193758622177, 0.7488612380771151322, 1.000000000000000000 ),
 .UNSPECIFIED. ) ;
#835 = CARTESIAN_POINT ( 'NONE',  ( 6.686404257991999778, -0.8351886993729999986, 1.025064727650000007 ) ) ;
#836 = CARTESIAN_POINT ( 'NONE',  ( 10.95222191436348247, -3.562569433230172944, 8.256798586434323184 ) ) ;
#837 = CARTESIAN_POINT ( 'NONE',  ( 24.44496483130000186, -3.224879855413000040, 12.03535978074999946 ) ) ;
#838 = CARTESIAN_POINT ( 'NONE',  ( 12.66237550623657704, 0.6088395004560429591, -12.68034807294329980 ) ) ;
#839 = CARTESIAN_POINT ( 'NONE',  ( 23.59999999999999787, 11.54195020457962606, 7.798376075308690147 ) ) ;
#840 = CARTESIAN_POINT ( 'NONE',  ( 5.500000000000000000, 12.87590651766999983, 2.791353855799999728 ) ) ;
#841 = CARTESIAN_POINT ( 'NONE',  ( 8.331682176603999679, 5.101289360622999425, 6.607176324693000424 ) ) ;
#842 = DIRECTION ( 'NONE',  ( 1.000000000000000000, 0.000000000000000000, 0.000000000000000000 ) ) ;
#843 = EDGE_LOOP ( 'NONE', ( #8756, #37718, #39211, #61668 ) ) ;
#844 = CARTESIAN_POINT ( 'NONE',  ( 7.610826510211253115, -3.823093646280199653, 8.848653938445639966 ) ) ;
#845 = SHAPE_DEFINITION_REPRESENTATION ( #41120, #15732 ) ;
#846 = CARTESIAN_POINT ( 'NONE',  ( 10.98656920625009903, -3.967932847735990531, -6.608450613814399688 ) ) ;
#847 = CARTESIAN_POINT ( 'NONE',  ( 5.699999999836000697, -1.433333331105999919, -10.65401593570999950 ) ) ;
#848 = B_SPLINE_CURVE_WITH_KNOTS ( 'NONE', 3,
 ( #68295, #61336, #45608, #41038 ),
 .UNSPECIFIED., .F., .F.,
 ( 4, 4 ),
 ( 0.000000000000000000, 1.000000000000000000 ),
 .UNSPECIFIED. ) ;
#849 = CARTESIAN_POINT ( 'NONE',  ( 10.84920446231350155, -2.899999999999999911, -6.662590550579920112 ) ) ;
#850 = CYLINDRICAL_SURFACE ( 'NONE', #44076, 11.84999999999999964 ) ;
#851 = CARTESIAN_POINT ( 'NONE',  ( 10.44635971519499940, 4.459622816450200311, -6.735384833238199143 ) ) ;
#852 = VERTEX_POINT ( 'NONE', #14552 ) ;
#853 = CARTESIAN_POINT ( 'NONE',  ( 4.600001223043999943, 1.829647544581999737E-13, -13.09999975891967416 ) ) ;
#854 = CARTESIAN_POINT ( 'NONE',  ( 17.55505043854143565, 3.125000000000000000, -13.52084414783465505 ) ) ;
#855 = VERTEX_POINT ( 'NONE', #54700 ) ;
#856 = CARTESIAN_POINT ( 'NONE',  ( 8.087243290925727024, 5.285867343427418596, -7.027213786845273091 ) ) ;
#857 = LINE ( 'NONE', #11681, #59166 ) ;
#858 = CARTESIAN_POINT ( 'NONE',  ( 9.608904719592000987, 4.946705552514000459, -6.253848946732999181 ) ) ;
#859 = EDGE_LOOP ( 'NONE', ( #2403, #13429, #58338, #59065 ) ) ;
#860 = CARTESIAN_POINT ( 'NONE',  ( 23.60000648363190123, -13.25016151468667225, 4.189794345519016971 ) ) ;
#861 = CARTESIAN_POINT ( 'NONE',  ( 11.67766954483535891, -3.284117569315500251, -6.395429936871999566 ) ) ;
#862 = CARTESIAN_POINT ( 'NONE',  ( 18.11689826751305787, 0.2739464174175113564, -12.69602652205120208 ) ) ;
#863 = AXIS2_PLACEMENT_3D ( 'NONE', #9240, #47006, #61366 ) ;
#864 = CARTESIAN_POINT ( 'NONE',  ( 9.911640687501567015, -2.873222873816665413, -6.752018918868491149 ) ) ;
#865 = CARTESIAN_POINT ( 'NONE',  ( 7.136007566080033726, 5.350530049016002820, -7.853201045838831718 ) ) ;
#866 = VERTEX_POINT ( 'NONE', #6104 ) ;
#867 = CARTESIAN_POINT ( 'NONE',  ( 10.68904248846000016, -2.568964727443000307, 7.728094434513999467 ) ) ;
#868 = EDGE_CURVE ( 'NONE', #40899, #66838, #6329, .T. ) ;
#870 = EDGE_CURVE ( 'NONE', #57810, #22321, #17292, .T. ) ;
#869 = B_SPLINE_CURVE_WITH_KNOTS ( 'NONE', 3,
 ( #26263, #31, #15769, #62955 ),
 .UNSPECIFIED., .F., .F.,
 ( 4, 4 ),
 ( 0.000000000000000000, 0.1844766778621776404 ),
 .UNSPECIFIED. ) ;
#871 = CARTESIAN_POINT ( 'NONE',  ( 25.41802413019000184, 11.20519658595999957, -3.227494277392999766 ) ) ;
#872 =( LENGTH_UNIT ( ) NAMED_UNIT ( * ) SI_UNIT ( .MILLI., .METRE. ) );
#873 = VERTEX_POINT ( 'NONE', #6798 ) ;
#874 = AXIS2_PLACEMENT_3D ( 'NONE', #61387, #34827, #56139 ) ;
#875 = CARTESIAN_POINT ( 'NONE',  ( 27.64127793187000037, 13.87069231928999891, -4.225386915259999654 ) ) ;
#876 = FACE_OUTER_BOUND ( 'NONE', #24822, .T. ) ;
#877 = ORIENTED_EDGE ( 'NONE', *, *, #25501, .F. ) ;
#878 = CARTESIAN_POINT ( 'NONE',  ( 10.18988779216199880, 5.056118594996999782, 7.119137915499500480 ) ) ;
#879 = CARTESIAN_POINT ( 'NONE',  ( 18.13610176147147257, 0.2304125752724597853, -13.89743363615660776 ) ) ;
#880 = CARTESIAN_POINT ( 'NONE',  ( 4.795397656733999092, 1.527828479674999906, -0.3026462966785000153 ) ) ;
#881 = CARTESIAN_POINT ( 'NONE',  ( 7.841306432805004611, 5.081857837045995474, -6.476218562526999456 ) ) ;
#882 = B_SPLINE_CURVE_WITH_KNOTS ( 'NONE', 3,
 ( #55892, #6952, #65330, #54503, #12550, #23382, #29330, #18142, #17089, #17449, #39119, #1712, #11847, #33185, #6603, #65678, #27945, #28284, #60099, #12205, #17800, #33533, #60442, #54852, #49604, #23031, #55197, #7299, #28640, #49951, #2064 ),
 .UNSPECIFIED., .F., .F.,
 ( 4, 2, 2, 1, 1, 2, 2, 2, 1, 2, 2, 2, 2, 2, 2, 2, 4 ),
 ( 0.000000000000000000, 0.06250000000000358047, 0.09375000000000592582, 0.1093750000000056066, 0.1171875000000048711, 0.1210937500000059258, 0.1250000000000069666, 0.1875000000000131839, 0.2187500000000159872, 0.2343750000000168199, 0.2500000000000176525, 0.3750000000000245359, 0.4375000000000285882, 0.4687500000000288658, 0.5000000000000291989, 0.7500000000000146549, 1.000000000000000000 ),
 .UNSPECIFIED. ) ;
#883 = CARTESIAN_POINT ( 'NONE',  ( 24.81123823827553565, 11.68013870454559289, -3.194582531880967746 ) ) ;
#884 = DIRECTION ( 'NONE',  ( 0.000000000000000000, 0.000000000000000000, -1.000000000000000000 ) ) ;
#885 = B_SPLINE_SURFACE_WITH_KNOTS ( 'NONE', 3, 3, ( 
 ( #48955, #21008, #38108, #37089 ),
 ( #43015, #43373, #16440, #48609 ),
 ( #15762, #5600, #58404, #64319 ),
 ( #23, #59434, #21344, #37769 ),
 ( #42673, #59094, #32876, #11196 ),
 ( #32534, #28676, #23422, #13292 ),
 ( #23068, #34263, #17487, #44066 ),
 ( #44757, #8033, #12937, #50338 ),
 ( #49641, #66061, #43715, #65008 ) ),
 .UNSPECIFIED., .F., .F., .F.,
 ( 4, 1, 1, 1, 1, 1, 4 ),
 ( 4, 4 ),
 ( -0.01864526228370000024, 0.000000000000000000, 0.2500000000000000000, 0.5000000000000000000, 0.7500000000000000000, 1.000000000000000000, 1.019255357118999950 ),
 ( -0.2206650646280000072, 1.220665064628000174 ),
 .UNSPECIFIED. ) ;
#886 = CARTESIAN_POINT ( 'NONE',  ( 9.327383005933997495, -3.946161398296482048, 9.238824392371451921 ) ) ;
#887 = ORIENTED_EDGE ( 'NONE', *, *, #47584, .T. ) ;
#888 = CARTESIAN_POINT ( 'NONE',  ( 10.63461554336999981, 5.668731883089999535, 6.527253515312000154 ) ) ;
#889 = CARTESIAN_POINT ( 'NONE',  ( 9.900934992105000276, 4.883852641422000040, -9.070888919673000927 ) ) ;
#890 = EDGE_CURVE ( 'NONE', #26237, #27264, #13051, .T. ) ;
#891 = CARTESIAN_POINT ( 'NONE',  ( 18.47604564451473053, -11.77695503131875121, 4.265147058870558894 ) ) ;
#892 = CARTESIAN_POINT ( 'NONE',  ( 12.21987570834413006, 2.720459983100028012, -13.62424277487875024 ) ) ;
#893 = CARTESIAN_POINT ( 'NONE',  ( 9.972537864286000087, 2.899999999999999911, -6.571291218949999902 ) ) ;
#894 = EDGE_CURVE ( 'NONE', #28055, #27697, #3524, .T. ) ;
#895 = CARTESIAN_POINT ( 'NONE',  ( 9.305875415870998424, -4.945293979885000191, 9.077881967919999795 ) ) ;
#896 = CARTESIAN_POINT ( 'NONE',  ( 18.16408159376649323, -0.1418539764880170639, 13.89904537328360767 ) ) ;
#897 = CARTESIAN_POINT ( 'NONE',  ( 7.717206996518667594, -2.839603352907888123, 6.809939372030577864 ) ) ;
#898 = B_SPLINE_CURVE_WITH_KNOTS ( 'NONE', 3,
 ( #49158, #53718, #235, #33090 ),
 .UNSPECIFIED., .F., .F.,
 ( 4, 4 ),
 ( 0.000000000000000000, 1.000000000000000000 ),
 .UNSPECIFIED. ) ;
#899 = EDGE_LOOP ( 'NONE', ( #66916, #36286, #32294, #9509 ) ) ;
#900 = ORIENTED_EDGE ( 'NONE', *, *, #41275, .F. ) ;
#901 = CARTESIAN_POINT ( 'NONE',  ( 10.80168826891999956, 3.998196217194999846, 9.431555066626000183 ) ) ;
#902 = CARTESIAN_POINT ( 'NONE',  ( 12.24303834293817417, 0.2736100116213214806, 13.89637849652254609 ) ) ;
#903 = CARTESIAN_POINT ( 'NONE',  ( 12.32624190542397891, -0.4017285589307944549, -13.89218662323934339 ) ) ;
#904 = CARTESIAN_POINT ( 'NONE',  ( 9.199609130449999839, -2.551382302226000487, 7.536606162076999738 ) ) ;
#905 = CARTESIAN_POINT ( 'NONE',  ( 17.82908354277550700, -0.5620915422472464451, -13.88470483921558341 ) ) ;
#906 = CARTESIAN_POINT ( 'NONE',  ( 8.347269353210000631, -2.741638482234999952, 6.457327039244000311 ) ) ;
#907 = CARTESIAN_POINT ( 'NONE',  ( 5.100000000000000533, 0.1499999999999999944, 6.463315149415000072 ) ) ;
#909 = CARTESIAN_POINT ( 'NONE',  ( 12.09999922233642522, -11.66744139996562701, 3.971920075675145156 ) ) ;
#908 = CARTESIAN_POINT ( 'NONE',  ( 9.905747021776001304, -4.961496216383199709, 6.656252755052399550 ) ) ;
#910 = CARTESIAN_POINT ( 'NONE',  ( 10.56733863405299800, 4.788475529394700558, -8.505794571537999005 ) ) ;
#911 = CARTESIAN_POINT ( 'NONE',  ( 12.10000000000000142, -4.549997407263328242, 6.620235306175750623 ) ) ;
#912 = AXIS2_PLACEMENT_3D ( 'NONE', #56306, #8412, #34650 ) ;
#913 = CARTESIAN_POINT ( 'NONE',  ( 8.757697342472001267, 2.899999999999999911, -6.397101765418000241 ) ) ;
#914 = CARTESIAN_POINT ( 'NONE',  ( 18.17477462772146524, -0.08167875237853229609, 12.69965198491186342 ) ) ;
#915 = CARTESIAN_POINT ( 'NONE',  ( 11.07925595036916633, -5.279255950369167394, 6.503434303641999925 ) ) ;
#916 = MECHANICAL_DESIGN_GEOMETRIC_PRESENTATION_REPRESENTATION (  '', ( #29982 ), #21023 ) ;
#917 = CARTESIAN_POINT ( 'NONE',  ( 24.15346678657299861, 9.222906534045000271, 9.474494998088001552 ) ) ;
#918 = ORIENTED_EDGE ( 'NONE', *, *, #57966, .F. ) ;
#919 = FACE_OUTER_BOUND ( 'NONE', #48407, .T. ) ;
#920 = CARTESIAN_POINT ( 'NONE',  ( 8.834370559623998531, -4.141908960411000429, 6.047561724438000219 ) ) ;
#921 = DIRECTION ( 'NONE',  ( -1.000000000000000000, 0.000000000000000000, 0.000000000000000000 ) ) ;
#922 = CARTESIAN_POINT ( 'NONE',  ( 10.99328643597520738, 6.237225121672477002, 5.127881282518703898 ) ) ;
#923 = CONICAL_SURFACE ( 'NONE', #42201, 11.34994642770999818, 0.7853934433894341760 ) ;
#924 = CARTESIAN_POINT ( 'NONE',  ( 13.49980696792483137, -10.68794281923488931, -6.218617845733625416 ) ) ;
#925 = CARTESIAN_POINT ( 'NONE',  ( 11.44366954483529852, 4.485203148598100320, 8.248643701125299543 ) ) ;
#926 = CARTESIAN_POINT ( 'NONE',  ( 2.600065990445999731, 2.304586066898000052, 2.969387198930000249 ) ) ;
#927 = ORIENTED_EDGE ( 'NONE', *, *, #61621, .F. ) ;
#928 = ADVANCED_FACE ( 'NONE', ( #43869 ), #27800, .F. ) ;
#929 = CARTESIAN_POINT ( 'NONE',  ( 12.13954479299508904, 0.2856017019952032387, -12.59676745213710447 ) ) ;
#930 = CIRCLE ( 'NONE', #18804, 13.00000000000000178 ) ;
#931 = DIRECTION ( 'NONE',  ( -1.000000000000000000, 0.000000000000000000, 0.000000000000000000 ) ) ;
#932 = CARTESIAN_POINT ( 'NONE',  ( 10.19810941423799910, 4.946022705791000007, 8.359277272599898723 ) ) ;
#933 = CARTESIAN_POINT ( 'NONE',  ( 15.80279819343546599, -8.703657694420874336, -8.043987028914523663 ) ) ;
#934 = CARTESIAN_POINT ( 'NONE',  ( 9.053329719590999858, 5.618384167307999277, 7.727742442702000503 ) ) ;
#935 = ORIENTED_EDGE ( 'NONE', *, *, #21606, .T. ) ;
#936 = CARTESIAN_POINT ( 'NONE',  ( 5.751874906802000531, 1.422967556274000067, 0.3628923349178999613 ) ) ;
#937 = CARTESIAN_POINT ( 'NONE',  ( 7.110504719587999567, 2.557426065706999818, -8.459317650138999056 ) ) ;
#938 = CARTESIAN_POINT ( 'NONE',  ( 8.447423826815846581, -2.260942181570626541, 7.552185937853629127 ) ) ;
#939 = CARTESIAN_POINT ( 'NONE',  ( 10.99375810342578141, -3.998140074039970848, -6.625879789168364731 ) ) ;
#940 = ORIENTED_EDGE ( 'NONE', *, *, #36929, .F. ) ;
#941 = CYLINDRICAL_SURFACE ( 'NONE', #63297, 1.250000000000000222 ) ;
#942 = CARTESIAN_POINT ( 'NONE',  ( 6.115443173016667622, -1.500000000000000222, -0.1963495408493622085 ) ) ;
#943 = ORIENTED_EDGE ( 'NONE', *, *, #1738, .T. ) ;
#944 = CARTESIAN_POINT ( 'NONE',  ( 11.09999999999999964, 3.512324525112999751, -8.971282648301999174 ) ) ;
#945 = CARTESIAN_POINT ( 'NONE',  ( 12.80505043854146940, -3.166049082260463443, -13.55318600037536747 ) ) ;
#946 = CARTESIAN_POINT ( 'NONE',  ( 18.16373243908211776, -0.1422577892986764680, -13.89902525486550289 ) ) ;
#947 = ORIENTED_EDGE ( 'NONE', *, *, #10087, .F. ) ;
#948 = CARTESIAN_POINT ( 'NONE',  ( 10.77164068750950143, -2.873222873834234914, 6.752018918838221140 ) ) ;
#949 = CARTESIAN_POINT ( 'NONE',  ( 11.04783424078000031, -2.764605797469000148, 5.041477660832000218 ) ) ;
#950 = CARTESIAN_POINT ( 'NONE',  ( 10.98656920625009903, 4.032067152264009913, -6.608450613814399688 ) ) ;
#951 = DIRECTION ( 'NONE',  ( 0.000000000000000000, -1.000000000000000000, 0.000000000000000000 ) ) ;
#952 = CARTESIAN_POINT ( 'NONE',  ( 11.63349010443640097, -2.725546193138000284, 7.404690636538299842 ) ) ;
#953 = EDGE_LOOP ( 'NONE', ( #20511, #17436, #26609 ) ) ;
#954 = CARTESIAN_POINT ( 'NONE',  ( 7.769579719591000355, 2.431401017850999935, 7.958393275880999873 ) ) ;
#955 = EDGE_CURVE ( 'NONE', #66838, #16567, #68868, .T. ) ;
#956 = EDGE_CURVE ( 'NONE', #9091, #38701, #48076, .T. ) ;
#957 = CARTESIAN_POINT ( 'NONE',  ( 17.94049251029959535, -1.899108762321214394, 13.87060088084272458 ) ) ;
#958 = VERTEX_POINT ( 'NONE', #12051 ) ;
#959 = CARTESIAN_POINT ( 'NONE',  ( 9.196006702408608291, -3.000394487162607149, -6.731788826750699783 ) ) ;
#960 = EDGE_CURVE ( 'NONE', #28311, #4423, #4597, .T. ) ;
#961 = CARTESIAN_POINT ( 'NONE',  ( 11.59999999999999964, -4.000000000000000000, -7.500000000000000000 ) ) ;
#962 = CARTESIAN_POINT ( 'NONE',  ( 11.07126769815000067, 6.557511878246000236, -5.495874711259999934 ) ) ;
#963 = ORIENTED_EDGE ( 'NONE', *, *, #30747, .T. ) ;
#964 = CARTESIAN_POINT ( 'NONE',  ( 12.18778960455906635, -2.401422506651156752, -12.47398279053984282 ) ) ;
#965 = AXIS2_PLACEMENT_3D ( 'NONE', #37909, #1203, #48061 ) ;
#966 = CARTESIAN_POINT ( 'NONE',  ( 0.1423795961331161819, -1.074693865285089478, -3.000024710404201045 ) ) ;
#967 = CYLINDRICAL_SURFACE ( 'NONE', #19295, 1.350000000000000533 ) ;
#968 = FACE_OUTER_BOUND ( 'NONE', #9546, .T. ) ;
#969 = CARTESIAN_POINT ( 'NONE',  ( 12.30654613137385489, -1.987682873648405124, -13.85818111229402838 ) ) ;
#970 = CARTESIAN_POINT ( 'NONE',  ( 10.28026357027499849, -3.014700852776899698, -7.690095141806899903 ) ) ;
#971 = CARTESIAN_POINT ( 'NONE',  ( 5.846693173017501799, 1.310679582531385501, 0.7554284705563518720 ) ) ;
#972 = CARTESIAN_POINT ( 'NONE',  ( 17.81328364446397927, -1.807903055951888938, 12.46962321666120665 ) ) ;
#973 = ORIENTED_EDGE ( 'NONE', *, *, #67687, .F. ) ;
#974 = FACE_OUTER_BOUND ( 'NONE', #62452, .T. ) ;
#975 = EDGE_LOOP ( 'NONE', ( #66563, #2565, #7052, #21478 ) ) ;
#976 = CARTESIAN_POINT ( 'NONE',  ( 11.75750014570500035, -12.43407951582999971, -1.799970604841000021 ) ) ;
#977 = CARTESIAN_POINT ( 'NONE',  ( 9.436104719595000745, 5.619431609641999614, -8.115423117607999615 ) ) ;
#978 = CARTESIAN_POINT ( 'NONE',  ( 10.99480479316000014, 3.850613903518000036, -9.347963496621000345 ) ) ;
#979 = EDGE_CURVE ( 'NONE', #25079, #67571, #55510, .T. ) ;
#980 = CARTESIAN_POINT ( 'NONE',  ( 10.77434462036999818, -4.612888200890999713, -8.898797372219998891 ) ) ;
#981 = FACE_OUTER_BOUND ( 'NONE', #43868, .T. ) ;
#982 = CARTESIAN_POINT ( 'NONE',  ( 7.681993940831000067, 3.468925063633002903, -6.455929610676999886 ) ) ;
#983 = VECTOR ( 'NONE', #46111, 1000.000000000000227 ) ;
#984 = CARTESIAN_POINT ( 'NONE',  ( 18.00454058110402755, -1.908039605442538145, -12.45487753843153200 ) ) ;
#985 = ORIENTED_EDGE ( 'NONE', *, *, #39002, .F. ) ;
#986 = CARTESIAN_POINT ( 'NONE',  ( 1.977569202129666914, 2.124261041935755934, -2.802062795322278532 ) ) ;
#987 = CARTESIAN_POINT ( 'NONE',  ( 10.12550053024000007, 5.788811067708000024, 7.335561454339999621 ) ) ;
#988 = CARTESIAN_POINT ( 'NONE',  ( 23.60000000000000142, 9.305479840184000651, -8.315530346521999405 ) ) ;
#989 = CARTESIAN_POINT ( 'NONE',  ( 10.89969598649000027, -3.111999510220800236, 6.971269690999399415 ) ) ;
#990 = DIRECTION ( 'NONE',  ( 0.000000000000000000, 0.9835907196275001096, 0.1804142351995999538 ) ) ;
#991 = AXIS2_PLACEMENT_3D ( 'NONE', #2694, #50934, #24364 ) ;
#992 = CARTESIAN_POINT ( 'NONE',  ( 11.05286138047000222, 9.767097133436999812, -6.032307961834000309 ) ) ;
#993 = CARTESIAN_POINT ( 'NONE',  ( 11.09999999999999964, 2.649999999999999911, 7.500000000000000000 ) ) ;
#994 = CARTESIAN_POINT ( 'NONE',  ( 24.22107886057200332, -9.185649942997999418, -9.646111962386999750 ) ) ;
#995 = CARTESIAN_POINT ( 'NONE',  ( 11.48052502238429895, -2.954316262216015065, -7.824990984965952912 ) ) ;
#996 = DIRECTION ( 'NONE',  ( -0.7071067811865474617, -0.7071067811865474617, 1.013775886743067205E-08 ) ) ;
#997 = ORIENTED_EDGE ( 'NONE', *, *, #11789, .F. ) ;
#998 = FACE_OUTER_BOUND ( 'NONE', #6504, .T. ) ;
#999 = CARTESIAN_POINT ( 'NONE',  ( 7.327076482695999537, -0.8753148192162999441, 0.8932045635694000341 ) ) ;
#1000 = CARTESIAN_POINT ( 'NONE',  ( 18.18012160401607957, 2.482106737233722882, 13.67720576235794638 ) ) ;
#1001 = CARTESIAN_POINT ( 'NONE',  ( 10.59999999999999964, 4.599999999999999645, 4.756097560976000338 ) ) ;
#1002 = CARTESIAN_POINT ( 'NONE',  ( 11.33041235500449950, -4.942357465271699724, -6.636704692336500067 ) ) ;
#1003 = EDGE_LOOP ( 'NONE', ( #60883, #57791, #7358 ) ) ;
#1004 = CARTESIAN_POINT ( 'NONE',  ( 10.63789391302397647, -4.829717262113836895, -8.579596796881972409 ) ) ;
#1005 = CARTESIAN_POINT ( 'NONE',  ( 9.041948341230998665, 2.707986230053999854, 5.994446745591000436 ) ) ;
#1007 = CARTESIAN_POINT ( 'NONE',  ( 11.10391045180384140, -2.870950512581996961, -8.114538794791119614 ) ) ;
#1006 = CARTESIAN_POINT ( 'NONE',  ( 8.912754719595000097, 2.481540185810000132, -7.878707153279001396 ) ) ;
#1009 = B_SPLINE_CURVE_WITH_KNOTS ( 'NONE', 3,
 ( #13795, #60995, #55062, #45270 ),
 .UNSPECIFIED., .F., .F.,
 ( 4, 4 ),
 ( 0.000000000000000000, 1.000000000000000000 ),
 .UNSPECIFIED. ) ;
#1008 = CARTESIAN_POINT ( 'NONE',  ( 10.60689139207886988, 3.306467137587833172, 4.759459215648202957 ) ) ;
#1010 = ADVANCED_FACE ( 'NONE', ( #32688 ), #15657, .T. ) ;
#1011 = VERTEX_POINT ( 'NONE', #58142 ) ;
#1012 = EDGE_CURVE ( 'NONE', #60415, #6697, #5473, .T. ) ;
#1013 = CARTESIAN_POINT ( 'NONE',  ( 9.332933391271998502, 5.100349772922000646, 8.693467186193998941 ) ) ;
#1015 = CARTESIAN_POINT ( 'NONE',  ( 18.26357562437061688, -2.673039206754515007, -13.74245258260623714 ) ) ;
#1014 = VECTOR ( 'NONE', #43655, 1000.000000000000114 ) ;
#1016 = CARTESIAN_POINT ( 'NONE',  ( 11.43718179236249988, 3.790319673775199849, 8.481317998227099864 ) ) ;
#1017 = CARTESIAN_POINT ( 'NONE',  ( 10.18239901426000138, -2.607725299334000102, 7.783410967795999724 ) ) ;
#1018 = CARTESIAN_POINT ( 'NONE',  ( 8.770183059623999355, -3.049610585291000042, 6.392533570808999421 ) ) ;
#1019 = VERTEX_POINT ( 'NONE', #26331 ) ;
#1020 = DIRECTION ( 'NONE',  ( -1.000000000000000000, 0.000000000000000000, -3.472115270429000239E-14 ) ) ;
#1022 = CARTESIAN_POINT ( 'NONE',  ( 11.01605564679000082, -5.482859940357000639, -7.846409404949000077 ) ) ;
#1021 = CARTESIAN_POINT ( 'NONE',  ( 12.00339635128600158, -11.70009917314000170, 4.315816162729000816 ) ) ;
#1023 = CARTESIAN_POINT ( 'NONE',  ( 7.767789809242127141, -5.129599579532937881, 8.822844411293367273 ) ) ;
#1024 = DIRECTION ( 'NONE',  ( 0.8843050081471363066, -0.1786785918943075702, -0.4313683036160176343 ) ) ;
#1025 = CARTESIAN_POINT ( 'NONE',  ( 11.00284540370999942, 5.167376273215000815, 4.969475793453000279 ) ) ;
#1026 = ORIENTED_EDGE ( 'NONE', *, *, #43279, .F. ) ;
#1027 = CARTESIAN_POINT ( 'NONE',  ( 5.719609839683332808, -0.1963495408493605987, -1.500000000000000444 ) ) ;
#1028 = CARTESIAN_POINT ( 'NONE',  ( 12.19559063708295987, -2.913481137622000006, 7.194517870904999945 ) ) ;
#1029 = CARTESIAN_POINT ( 'NONE',  ( 17.92302462182508194, 1.881539600493004061, 13.87303898715941486 ) ) ;
#1030 = CARTESIAN_POINT ( 'NONE',  ( 11.10887482311539998, 5.184953745778000389, 7.021250586468399391 ) ) ;
#1031 = ORIENTED_EDGE ( 'NONE', *, *, #60303, .F. ) ;
#1032 = B_SPLINE_CURVE_WITH_KNOTS ( 'NONE', 3,
 ( #42511, #68372, #21179, #4744 ),
 .UNSPECIFIED., .F., .F.,
 ( 4, 4 ),
 ( 0.000000000000000000, 1.000000000000000000 ),
 .UNSPECIFIED. ) ;
#1033 = B_SPLINE_SURFACE_WITH_KNOTS ( 'NONE', 3, 3, ( 
 ( #27951, #38781, #17456, #33888 ),
 ( #10223, #42043, #25962, #54858 ),
 ( #17096, #52877, #23037, #44386 ),
 ( #20716, #60108, #58121, #4976 ),
 ( #38428, #49262, #12212, #10564 ),
 ( #43684, #47291, #63349, #28291 ),
 ( #59752, #31555, #33541, #39125 ),
 ( #6960, #47976, #26659, #49611 ),
 ( #21061, #65686, #1718, #76 ),
 ( #1372, #60450, #17809, #11854 ),
 ( #58458, #22690, #22347, #37141 ),
 ( #26309, #33193, #53216, #68594 ) ),
 .UNSPECIFIED., .F., .F., .F.,
 ( 4, 1, 1, 1, 1, 1, 1, 1, 1, 4 ),
 ( 4, 4 ),
 ( 0.5515699153562999557, 0.5999999999999999778, 0.6500000000000000222, 0.6999999999999999556, 0.7500000000000000000, 0.8000000000000000444, 0.8499999999999999778, 0.9000000000000000222, 0.9499999999999999556, 0.9893635532735000071 ),
 ( -0.2706691663378000268, 1.270787837442000079 ),
 .UNSPECIFIED. ) ;
#1034 = CARTESIAN_POINT ( 'NONE',  ( 9.418864158773999407, 3.210851187372000037, -6.346613542714999667 ) ) ;
#1035 = CARTESIAN_POINT ( 'NONE',  ( 12.80505043854143388, 1.874999999999999556, -12.57545641911172751 ) ) ;
#1036 = CARTESIAN_POINT ( 'NONE',  ( 12.05811496860034993, -2.954409148022000053, 8.035816473382100256 ) ) ;
#1037 = EDGE_CURVE ( 'NONE', #55115, #37404, #15830, .T. ) ;
#1038 = EDGE_LOOP ( 'NONE', ( #13976, #62077, #33921, #6620 ) ) ;
#1039 = FACE_OUTER_BOUND ( 'NONE', #39336, .T. ) ;
#1041 = EDGE_CURVE ( 'NONE', #38352, #51298, #47656, .T. ) ;
#1040 = DIRECTION ( 'NONE',  ( -0.7660444431190069903, 0.000000000000000000, -0.6427876096865049460 ) ) ;
#1042 = ORIENTED_EDGE ( 'NONE', *, *, #49334, .T. ) ;
#1043 = CARTESIAN_POINT ( 'NONE',  ( 9.395316940379000670, -5.146736128384000075, 6.597417125647000447 ) ) ;
#1044 = CARTESIAN_POINT ( 'NONE',  ( 23.71153137169101299, 9.910002971162056085, 9.457066138817401324 ) ) ;
#1045 = ORIENTED_EDGE ( 'NONE', *, *, #54865, .F. ) ;
#1046 = CARTESIAN_POINT ( 'NONE',  ( 10.00068357938802954, -3.239576832587917732, -9.078134629932138822 ) ) ;
#1047 = CARTESIAN_POINT ( 'NONE',  ( 11.01872200990539952, 3.052519557825900343, 7.830502140005199507 ) ) ;
#1048 = CARTESIAN_POINT ( 'NONE',  ( 23.56666365135700403, 2.009474831861002286, -11.63289034805000277 ) ) ;
#1049 = CARTESIAN_POINT ( 'NONE',  ( 11.13508722342999846, 2.662017522928000091, -5.085688471786000697 ) ) ;
#1050 = CARTESIAN_POINT ( 'NONE',  ( 8.361434368299004660, 5.126350915548002263, 6.365320234831002288 ) ) ;
#1051 = CARTESIAN_POINT ( 'NONE',  ( 12.79999999202000005, 11.41069016990000051, -4.623987642516999230 ) ) ;
#1052 = CARTESIAN_POINT ( 'NONE',  ( 11.09999233421999953, -1.199999999999999956, -11.47663049995799156 ) ) ;
#1053 = CARTESIAN_POINT ( 'NONE',  ( 17.95964167607823114, -0.4764818960106708690, -12.68796903437993606 ) ) ;
#1054 = SURFACE_STYLE_FILL_AREA ( #22016 ) ;
#1055 = CARTESIAN_POINT ( 'NONE',  ( 10.44841638348500013, -5.108333310975999630, -7.230023356477299323 ) ) ;
#1056 = CARTESIAN_POINT ( 'NONE',  ( 8.764829719592999169, 5.808262417891000062, 7.446016144116000213 ) ) ;
#1057 = VERTEX_POINT ( 'NONE', #21414 ) ;
#1058 = DIRECTION ( 'NONE',  ( -1.000000000000000000, 0.000000000000000000, 0.000000000000000000 ) ) ;
#1059 = B_SPLINE_CURVE_WITH_KNOTS ( 'NONE', 3,
 ( #43938, #50214, #65243, #60353 ),
 .UNSPECIFIED., .F., .F.,
 ( 4, 4 ),
 ( 0.000000000000000000, 1.000000000000000000 ),
 .UNSPECIFIED. ) ;
#1060 = CARTESIAN_POINT ( 'NONE',  ( 7.108390820783056618, 3.867390187372035548, 8.850036383993245437 ) ) ;
#1061 = CARTESIAN_POINT ( 'NONE',  ( 7.883148997456999929, 5.167567567567999731, 6.822293592207000934 ) ) ;
#1062 = EDGE_CURVE ( 'NONE', #36031, #28388, #27149, .T. ) ;
#1063 = CARTESIAN_POINT ( 'NONE',  ( 18.20581337561478108, 2.797825772877919004, 12.28545032770987078 ) ) ;
#1064 = LINE ( 'NONE', #22718, #65137 ) ;
#1065 = CARTESIAN_POINT ( 'NONE',  ( 10.99096914765000044, 9.108466108418001639, 6.431364469357999880 ) ) ;
#1066 = CARTESIAN_POINT ( 'NONE',  ( 9.752229279041625176, -3.908861085869333785, 6.629812682664218748 ) ) ;
#1067 = CARTESIAN_POINT ( 'NONE',  ( 4.574515983791000080E-07, 0.000000000000000000, 0.000000000000000000 ) ) ;
#1068 = EDGE_LOOP ( 'NONE', ( #44039, #31133, #6167, #22308 ) ) ;
#1069 = CARTESIAN_POINT ( 'NONE',  ( 12.15211780798805385, -2.166395227764209341, 12.41237995041120712 ) ) ;
#1070 = CARTESIAN_POINT ( 'NONE',  ( 8.897151519676997466, -3.975306837623020062, -8.641543873690000765 ) ) ;
#1071 = CARTESIAN_POINT ( 'NONE',  ( 0.2500098862125000321, 0.000000000000000000, -3.249989426617000188 ) ) ;
#1072 = CARTESIAN_POINT ( 'NONE',  ( 10.13050497920000126, -3.092053006542000215, 8.629388195475000245 ) ) ;
#1073 = CARTESIAN_POINT ( 'NONE',  ( 10.45257053952200010, 3.605640676136899980, -6.577269499510100204 ) ) ;
#1074 = CARTESIAN_POINT ( 'NONE',  ( 12.08961557973415779, -0.1170514037749869340, 12.59946170170351643 ) ) ;
#1075 = CARTESIAN_POINT ( 'NONE',  ( 9.304732780410999382, 5.284130523641000110, 6.489275570566000795 ) ) ;
#1076 = CARTESIAN_POINT ( 'NONE',  ( 9.285195242305000818, 5.269680202247999823, 8.747831873285999649 ) ) ;
#1077 = CARTESIAN_POINT ( 'NONE',  ( 12.18120961385783829, 2.543048387066358274, 12.44145101111442742 ) ) ;
#1078 = ORIENTED_EDGE ( 'NONE', *, *, #21219, .T. ) ;
#1079 = CARTESIAN_POINT ( 'NONE',  ( 21.10000000000000142, 12.35000000006999876, 0.000000000000000000 ) ) ;
#1080 = CARTESIAN_POINT ( 'NONE',  ( 11.70379573085659786, 5.106255642043000087, -7.691418046581699919 ) ) ;
#1081 = CARTESIAN_POINT ( 'NONE',  ( 18.22927867710214045, -0.2646961475753731308, 12.59722401988189411 ) ) ;
#1082 = DIRECTION ( 'NONE',  ( 0.000000000000000000, 1.000000000000000000, 0.000000000000000000 ) ) ;
#1084 = CARTESIAN_POINT ( 'NONE',  ( 17.69617877293821451, -0.6091736731909352942, 12.68032649603923545 ) ) ;
#1083 = PLANE ( 'NONE',  #43091 ) ;
#1085 = VECTOR ( 'NONE', #9254, 1000.000000000000000 ) ;
#1086 = CARTESIAN_POINT ( 'NONE',  ( 8.350387243830999395, 3.399999999999999911, 6.632262360512000576 ) ) ;
#1087 = EDGE_LOOP ( 'NONE', ( #13122, #64415, #41237, #26351 ) ) ;
#1088 = CARTESIAN_POINT ( 'NONE',  ( 1.882430528421999982, -0.1982148001128000159, 3.252998300308999724 ) ) ;
#1089 = CARTESIAN_POINT ( 'NONE',  ( 23.97709314544701442, -9.403781800835757210, -9.292205342148244895 ) ) ;
#1090 = CARTESIAN_POINT ( 'NONE',  ( 12.68562097720242576, -12.11848650044661291, 3.165127050490176064 ) ) ;
#1091 = CARTESIAN_POINT ( 'NONE',  ( 18.20209611037771325, 2.854851737536822753, -12.27307487513336959 ) ) ;
#1092 = EDGE_CURVE ( 'NONE', #65620, #63173, #16942, .T. ) ;
#1093 = EDGE_CURVE ( 'NONE', #17729, #50078, #52151, .T. ) ;
#1094 = B_SPLINE_CURVE_WITH_KNOTS ( 'NONE', 3,
 ( #11339, #860, #32680, #22177, #53993, #43517, #64815, #16925, #59583, #11684, #6438, #29526, #66895, #39303, #23909, #60282, #38965, #40334, #13436, #50143, #29171, #7139, #45590, #45246, #66552, #18670, #13086, #28477, #2581, #1548, #49793, #65861 ),
 .UNSPECIFIED., .F., .F.,
 ( 4, 2, 2, 2, 2, 2, 2, 2, 1, 2, 2, 2, 1, 1, 1, 2, 2, 4 ),
 ( 0.000000000000000000, 0.2499999999999824030, 0.3749999999999745759, 0.4374999999999704681, 0.4687499999999693578, 0.4999999999999682476, 0.6249999999999634737, 0.6874999999999632516, 0.7187499999999620304, 0.7343749999999621414, 0.7499999999999622524, 0.8124999999999668043, 0.8437499999999708011, 0.8593749999999727995, 0.8671874999999756861, 0.8710937499999781286, 0.8749999999999804601, 1.000000000000000000 ),
 .UNSPECIFIED. ) ;
#1095 = CARTESIAN_POINT ( 'NONE',  ( 12.21493840618619053, -2.942228658260931162, 13.68734401625692954 ) ) ;
#1096 = CARTESIAN_POINT ( 'NONE',  ( 11.03521345716899837, -3.075109701058799772, 6.659120737011199331 ) ) ;
#1097 = CARTESIAN_POINT ( 'NONE',  ( 24.63805276219900264, 3.694107246557000401, -12.29549514572999946 ) ) ;
#1098 = ORIENTED_EDGE ( 'NONE', *, *, #66211, .F. ) ;
#1099 = EDGE_CURVE ( 'NONE', #35088, #29684, #36309, .T. ) ;
#1100 = DIRECTION ( 'NONE',  ( 0.000000000000000000, 0.000000000000000000, -1.000000000000000000 ) ) ;
#1101 = CARTESIAN_POINT ( 'NONE',  ( 18.17745566902672394, -10.88889238843039209, 4.142628063310672459 ) ) ;
#1102 = CARTESIAN_POINT ( 'NONE',  ( 21.05000072320150295, 1.558041382508999773E-13, -6.372680161347999694E-14 ) ) ;
#1103 = CARTESIAN_POINT ( 'NONE',  ( 0.9374279487471000039, -2.315742118336999944, -2.746122198278999615 ) ) ;
#1104 = CARTESIAN_POINT ( 'NONE',  ( 18.50003594170800270, -2.686563649653999963, 11.33603604535000109 ) ) ;
#1105 = B_SPLINE_CURVE_WITH_KNOTS ( 'NONE', 3,
 ( #52305, #25741, #42173, #52649, #53688, #11036 ),
 .UNSPECIFIED., .F., .F.,
 ( 4, 2, 4 ),
 ( 0.000000000000000000, 0.5000000000000000000, 1.000000000000000000 ),
 .UNSPECIFIED. ) ;
#1106 = CARTESIAN_POINT ( 'NONE',  ( 18.00740283128405395, 2.068595914410284120, -12.54170588102538808 ) ) ;
#1107 = CARTESIAN_POINT ( 'NONE',  ( 9.841834235717474400, -4.999591705763746674, 8.268200207948643410 ) ) ;
#1108 = CARTESIAN_POINT ( 'NONE',  ( 10.60441638348510018, 3.158410350011299883, 7.705001100909899314 ) ) ;
#1109 = LINE ( 'NONE', #53890, #62457 ) ;
#1110 = CARTESIAN_POINT ( 'NONE',  ( 10.16821935321000048, -2.330398934821000356, -7.267462182607999921 ) ) ;
#1111 = CARTESIAN_POINT ( 'NONE',  ( 11.00000000000000000, -0.4000000000000000222, -7.331472342878999626 ) ) ;
#1112 = CARTESIAN_POINT ( 'NONE',  ( 6.587956561560666557, -1.500000000000001332, 0.3217608788839342315 ) ) ;
#1113 = CARTESIAN_POINT ( 'NONE',  ( 24.60320129348500018, 12.45517092796000114, 2.982541609212000289 ) ) ;
#1114 = DIRECTION ( 'NONE',  ( 0.4384236320214023319, 0.000000000000000000, -0.8987684456439056779 ) ) ;
#1115 = EDGE_LOOP ( 'NONE', ( #37361, #63353, #248, #26137, #18913 ) ) ;
#1116 = CARTESIAN_POINT ( 'NONE',  ( 9.292835841232999883, 5.200883864107000321, -6.027780766890000308 ) ) ;
#1117 = ORIENTED_EDGE ( 'NONE', *, *, #15075, .T. ) ;
#1118 = CARTESIAN_POINT ( 'NONE',  ( 17.84291783703838874, -3.054853729147657848, 13.53999333998545218 ) ) ;
#1119 = CARTESIAN_POINT ( 'NONE',  ( 10.09964828895399869, -2.878385131502000149, -8.112615456209400833 ) ) ;
#1120 = ORIENTED_EDGE ( 'NONE', *, *, #39328, .F. ) ;
#1121 = CARTESIAN_POINT ( 'NONE',  ( 11.56322412107030928, 4.054600656575539475, 8.532060764998998792 ) ) ;
#1122 = CARTESIAN_POINT ( 'NONE',  ( 6.229247610630833876, -0.3449401851437640110, 1.078764845586133392 ) ) ;
#1123 = CARTESIAN_POINT ( 'NONE',  ( 24.30000000000000071, -3.224868684338999980, 12.03537377768999939 ) ) ;
#1124 = CARTESIAN_POINT ( 'NONE',  ( 18.24051303026600124, -3.055556278716000218, 11.39470302754000031 ) ) ;
#1125 = CARTESIAN_POINT ( 'NONE',  ( 12.70654069053541768, -3.248070099070596850, -13.61800428248625572 ) ) ;
#1126 = DIRECTION ( 'NONE',  ( -1.000000000000000000, 0.000000000000000000, 0.000000000000000000 ) ) ;
#1127 = CARTESIAN_POINT ( 'NONE',  ( 13.99999999231800096, 8.833253877201999060, 7.896562762484000686 ) ) ;
#1128 = CARTESIAN_POINT ( 'NONE',  ( 10.98277446826000059, -2.518728855032000169, -8.314788219120000434 ) ) ;
#1129 = CARTESIAN_POINT ( 'NONE',  ( 11.73671932425159881, -4.127012898954600217, -8.356835045446798560 ) ) ;
#1130 = EDGE_LOOP ( 'NONE', ( #15241, #60982, #45864, #48062, #6883 ) ) ;
#1131 = CARTESIAN_POINT ( 'NONE',  ( 8.559020380274414919, 4.705862675926775651, 8.704770267039732445 ) ) ;
#1133 = ORIENTED_EDGE ( 'NONE', *, *, #68920, .T. ) ;
#1132 = B_SPLINE_CURVE_WITH_KNOTS ( 'NONE', 3,
 ( #7572, #7229, #2671, #65944 ),
 .UNSPECIFIED., .F., .F.,
 ( 4, 4 ),
 ( 0.000000000000000000, 1.000000000000000000 ),
 .UNSPECIFIED. ) ;
#1134 = VECTOR ( 'NONE', #25112, 1000.000000000000114 ) ;
#1135 = DIRECTION ( 'NONE',  ( 0.000000000000000000, 0.9048270524660052549, -0.4257792915651026910 ) ) ;
#1136 = ORIENTED_EDGE ( 'NONE', *, *, #47046, .F. ) ;
#1137 = CARTESIAN_POINT ( 'NONE',  ( 21.00000000000000000, 0.000000000000000000, 0.000000000000000000 ) ) ;
#1138 = CARTESIAN_POINT ( 'NONE',  ( 10.85067755245999876, -5.068636324353000155, 5.153848641568999689 ) ) ;
#1139 = ADVANCED_FACE ( 'NONE', ( #66480 ), #2857, .F. ) ;
#1140 = CARTESIAN_POINT ( 'NONE',  ( 10.55068303964747578, 3.428091289053144308, 8.161067340483363353 ) ) ;
#1141 = CARTESIAN_POINT ( 'NONE',  ( 10.26693802597399952, 3.334935831489500124, -6.407263051216999017 ) ) ;
#1142 = B_SPLINE_CURVE_WITH_KNOTS ( 'NONE', 3,
 ( #7494, #49808, #55750, #28491, #28141, #34774, #17656, #49454, #65874, #33737, #55052, #40018, #67853, #28849, #2261, #50495, #8191, #50158 ),
 .UNSPECIFIED., .F., .F.,
 ( 4, 2, 2, 2, 2, 2, 2, 2, 4 ),
 ( 0.000000000000000000, 0.1250000000000000000, 0.2500000000000000000, 0.3750000000000000000, 0.5000000000000000000, 0.6250000000000000000, 0.7500000000000000000, 0.8750000000000000000, 1.000000000000000000 ),
 .UNSPECIFIED. ) ;
#1143 = CARTESIAN_POINT ( 'NONE',  ( 12.72201428491563746, 3.119809216722633227, 13.52222099568140479 ) ) ;
#1144 = CARTESIAN_POINT ( 'NONE',  ( 17.57589479786111042, -1.875260891896569415, 12.57541370809468972 ) ) ;
#1145 = ADVANCED_FACE ( 'NONE', ( #44144 ), #38890, .T. ) ;
#1146 = CARTESIAN_POINT ( 'NONE',  ( 23.59999172348799945, -10.30759808834999980, 9.317726582648999667 ) ) ;
#1147 = CARTESIAN_POINT ( 'NONE',  ( 12.70241326318844877, 0.6168528257048850882, 13.88157091029611045 ) ) ;
#1148 = VERTEX_POINT ( 'NONE', #12661 ) ;
#1149 = CARTESIAN_POINT ( 'NONE',  ( 6.652728317542999648, 4.719833207100999850, -8.789699670502999496 ) ) ;
#1150 = DIRECTION ( 'NONE',  ( 1.000000000000000000, 0.000000000000000000, 0.000000000000000000 ) ) ;
#1151 = CARTESIAN_POINT ( 'NONE',  ( 10.01210369451062654, 3.801861024511436593, 8.352216648108843344 ) ) ;
#1152 = CARTESIAN_POINT ( 'NONE',  ( 4.740781127745999690, -1.306963758498000061, 0.2701982545766000166 ) ) ;
#1153 = CARTESIAN_POINT ( 'NONE',  ( 10.02394528041000044, 5.481267232667000222, -8.005061172455999241 ) ) ;
#1154 = DIRECTION ( 'NONE',  ( -1.000000000000000000, 0.000000000000000000, 0.000000000000000000 ) ) ;
#1155 = CARTESIAN_POINT ( 'NONE',  ( 9.973487588364999823, -4.344961837988999598, -9.321582626371998970 ) ) ;
#1156 = ORIENTED_EDGE ( 'NONE', *, *, #49731, .F. ) ;
#1157 = CARTESIAN_POINT ( 'NONE',  ( 11.09999965054999826, -2.398081733189999864E-14, 0.000000000000000000 ) ) ;
#1158 = CARTESIAN_POINT ( 'NONE',  ( 8.218666589540001510, -2.895314275791000203, 6.639800878566000542 ) ) ;
#1159 = CARTESIAN_POINT ( 'NONE',  ( 5.605026506349999771, -1.500000000000000000, 0.000000000000000000 ) ) ;
#1160 = DIRECTION ( 'NONE',  ( 0.000000000000000000, 0.000000000000000000, -1.000000000000000000 ) ) ;
#1161 = DIRECTION ( 'NONE',  ( 0.000000000000000000, -1.000000000000000000, 0.000000000000000000 ) ) ;
#1162 = CARTESIAN_POINT ( 'NONE',  ( 10.72702344389999851, 2.995605560827999891, -6.890449684422599752 ) ) ;
#1163 = CARTESIAN_POINT ( 'NONE',  ( 9.457355082327998375, 3.550486524676900402, -6.601790705997299114 ) ) ;
#1165 = CYLINDRICAL_SURFACE ( 'NONE', #35113, 3.500000000000000000 ) ;
#1164 = CARTESIAN_POINT ( 'NONE',  ( 10.65958376188599921, -4.731143729777899765, 7.034020612385399218 ) ) ;
#1166 = CARTESIAN_POINT ( 'NONE',  ( 11.25851354018298522, -3.836375382625526687, 8.749999999999996447 ) ) ;
#1167 = ORIENTED_EDGE ( 'NONE', *, *, #53745, .T. ) ;
#1168 = AXIS2_PLACEMENT_3D ( 'NONE', #5018, #52227, #25660 ) ;
#1169 = CARTESIAN_POINT ( 'NONE',  ( 10.85679632507500081, 4.490665650747399873, 6.590394082213600235 ) ) ;
#1170 = CARTESIAN_POINT ( 'NONE',  ( 9.967845797207999681, -2.034786297409000078, 7.636877353231999344 ) ) ;
#1171 = CARTESIAN_POINT ( 'NONE',  ( 9.429063610504998749, 4.468346739194200445, 6.458661544034999480 ) ) ;
#1172 = CARTESIAN_POINT ( 'NONE',  ( 5.700000000000001954, -13.02829083177932823, 1.966948496269156132 ) ) ;
#1173 = EDGE_CURVE ( 'NONE', #26310, #57892, #61331, .T. ) ;
#1174 = CARTESIAN_POINT ( 'NONE',  ( 11.02786767503999954, -5.596230239120999705, 7.209501483790000442 ) ) ;
#1175 = CARTESIAN_POINT ( 'NONE',  ( 12.80505043854146940, -1.787797342887047947, -13.88538010501570774 ) ) ;
#1176 = CARTESIAN_POINT ( 'NONE',  ( 11.53943995709000170, 3.847421095330999741, -11.95976051375000004 ) ) ;
#1177 = EDGE_CURVE ( 'NONE', #35879, #44670, #28401, .T. ) ;
#1178 = EDGE_CURVE ( 'NONE', #50051, #21433, #30369, .T. ) ;
#1179 = VECTOR ( 'NONE', #6236, 1000.000000000000000 ) ;
#1180 = CARTESIAN_POINT ( 'NONE',  ( 8.874784697134998623, -3.454948069423500190, -6.656340890368899643 ) ) ;
#1181 = B_SPLINE_CURVE_WITH_KNOTS ( 'NONE', 3,
 ( #36973, #31045, #4447, #15640 ),
 .UNSPECIFIED., .F., .F.,
 ( 4, 4 ),
 ( 0.000000000000000000, 1.000000000000000000 ),
 .UNSPECIFIED. ) ;
#1182 = DIRECTION ( 'NONE',  ( 0.000000000000000000, -1.000000000000000000, 0.000000000000000000 ) ) ;
#1183 = CARTESIAN_POINT ( 'NONE',  ( 6.506620200880000482, 0.8089969479913999839, 1.225571816066999942 ) ) ;
#1184 = B_SPLINE_SURFACE_WITH_KNOTS ( 'NONE', 3, 3, ( 
 ( #28833, #59584, #60627, #54337, #43518, #861, #38966, #1903, #55385, #22178, #33374, #50144, #59930, #39304, #64816, #1549, #33722, #44570, #11685, #65862, #7480, #2249, #23562, #12388, #16926, #44903, #27788, #18328, #33025, #6439, #12041, #49438, #22870, #44220, #65514 ),
 ( #17642, #60283, #24603, #7837, #56767, #8178, #40673, #34758, #55734, #29868, #24941, #29172, #56417, #29527, #14800, #9195, #41022, #19702, #8864, #50829, #35781, #67578, #51176, #45591, #25286, #50480, #2582, #13437, #30202, #62005, #62344, #3272, #51507, #23910, #66897 ),
 ( #2925, #24253, #66553, #56068, #18671, #30538, #14461, #45247, #57096, #67235, #3606, #40003, #8520, #45925, #19010, #61318, #51849, #40335, #3947, #46620, #61658, #67925, #13772, #35105, #19351, #14117, #46274, #20041, #41370, #62679, #35441, #52888, #15488, #31232, #4636 ),
 ( #25975, #58472, #42741, #36815, #27009, #21747, #68262, #58133, #37153, #432, #47304, #43080, #20383, #21073, #5668, #64386, #36119, #42057, #48327, #57434, #46960, #10576, #64045, #16165, #31916, #47987, #68608, #63011, #9892, #37490, #57780, #26674, #53230, #20728, #52539 ) ),
 .UNSPECIFIED., .F., .F., .F.,
 ( 4, 4 ),
 ( 4, 1, 1, 1, 1, 1, 1, 1, 1, 1, 1, 1, 1, 1, 1, 1, 1, 1, 1, 1, 1, 1, 1, 1, 1, 1, 1, 1, 1, 1, 1, 1, 4 ),
 ( -0.02000000000000000042, 1.020000000000000018 ),
 ( 0.1633025096610999927, 0.1899619885200000136, 0.2166214673788000034, 0.2432809462376999965, 0.2699404250964999585, 0.2965999039553000038, 0.3232593828141999692, 0.3499188616730000145, 0.3765783405318000043, 0.4032378193906999697, 0.4298972982494999595, 0.4565567771083000048, 0.4832162559671999702, 0.5098757348260000155, 0.5365352136848999809, 0.5631946925437000262, 0.5898541714025000715, 0.6165136502614000369, 0.6431731291201999712, 0.6698326079790000165, 0.6964920868378999819, 0.7231515656967000272, 0.7498110445554999615, 0.7764705234143999268, 0.8031300022731999722, 0.8297894811320000175, 0.8564489599908999828, 0.8831084388497000282, 0.9097679177085999935, 0.9364273965674000388, 0.9630868754261999731, 0.9897463542851000495, 1.016405833144000015 ),
 .UNSPECIFIED. ) ;
#1185 = CARTESIAN_POINT ( 'NONE',  ( 8.629721738021999045, -2.812225201737000635, -6.860033716225003353 ) ) ;
#1186 = DIRECTION ( 'NONE',  ( 0.000000000000000000, -1.000000000000000000, 0.000000000000000000 ) ) ;
#1187 = CARTESIAN_POINT ( 'NONE',  ( 11.89210538575740017, -3.157545584346100220, 7.701417844014099678 ) ) ;
#1188 = CARTESIAN_POINT ( 'NONE',  ( 11.02287616594229824, 3.738072157442200005, -6.674353346984900348 ) ) ;
#1189 = CARTESIAN_POINT ( 'NONE',  ( 12.72228957558485618, 1.874999999999999778, -13.78631905550013137 ) ) ;
#1190 = CARTESIAN_POINT ( 'NONE',  ( 25.27036502875199986, -8.566977734595999650, 7.889724197193000776 ) ) ;
#1191 = CARTESIAN_POINT ( 'NONE',  ( 5.568708408617618844, 12.91387460240243357, 2.616215362094806540 ) ) ;
#1192 = ORIENTED_EDGE ( 'NONE', *, *, #19050, .T. ) ;
#1193 = DIRECTION ( 'NONE',  ( 1.000000000000000000, 0.000000000000000000, 0.000000000000000000 ) ) ;
#1194 = APPLICATION_PROTOCOL_DEFINITION ( 'draft international standard', 'automotive_design', 1998, #54308 ) ;
#1195 = CARTESIAN_POINT ( 'NONE',  ( 10.29399293566599916, -3.453258297007899991, -8.170700474995699736 ) ) ;
#1196 = CARTESIAN_POINT ( 'NONE',  ( 18.09779212070452914, 0.3101159434603414367, 12.69490728026488569 ) ) ;
#1197 = EDGE_CURVE ( 'NONE', #5681, #47380, #25405, .T. ) ;
#1198 = CARTESIAN_POINT ( 'NONE',  ( 7.961731591766580074, -5.351349901897480166, 7.263035046629693348 ) ) ;
#1199 = CARTESIAN_POINT ( 'NONE',  ( 7.000000000000000888, 9.410344523941196471, 4.699947945108982061 ) ) ;
#1200 = CARTESIAN_POINT ( 'NONE',  ( 5.634824896760862067, 12.09997259267891678, -3.741298181620886343 ) ) ;
#1201 = VERTEX_POINT ( 'NONE', #39231 ) ;
#1202 = DIRECTION ( 'NONE',  ( -5.239392413525232509E-16, -0.6482718649732923666, -0.7614089499631913061 ) ) ;
#1203 = DIRECTION ( 'NONE',  ( -1.000000000000000000, 0.000000000000000000, 0.000000000000000000 ) ) ;
#1204 = ORIENTED_EDGE ( 'NONE', *, *, #33666, .T. ) ;
#1205 = CARTESIAN_POINT ( 'NONE',  ( 9.884624721933931824, -2.899999999999999911, 6.445686799102332110 ) ) ;
#1206 = CARTESIAN_POINT ( 'NONE',  ( 8.545870559624999530, -3.856773448568000084, 5.521258396339000285 ) ) ;
#1207 = CARTESIAN_POINT ( 'NONE',  ( 9.070789158774999805, 5.349936549139000519, -7.138437102151999447 ) ) ;
#1208 = DIRECTION ( 'NONE',  ( 0.000000000000000000, -0.1862490057674050514, -0.9825025739664263735 ) ) ;
#1209 = CARTESIAN_POINT ( 'NONE',  ( 8.771640687503264644, 2.873222873813474632, 6.752018918873988085 ) ) ;
#1210 = CARTESIAN_POINT ( 'NONE',  ( 6.826920280409000341, 5.346927244140000646, -8.589407719218000281 ) ) ;
#1211 = CARTESIAN_POINT ( 'NONE',  ( 16.39999999347100257, -3.345256695718999751, -11.86066175541999890 ) ) ;
#1212 = CARTESIAN_POINT ( 'NONE',  ( 4.877943173016666023, 0.9218200799623692543, 1.199500263597272687 ) ) ;
#1213 = ORIENTED_EDGE ( 'NONE', *, *, #58230, .F. ) ;
#1214 = CARTESIAN_POINT ( 'NONE',  ( 8.100000113405998903, 3.037570195374000164E-13, -12.39999890530004123 ) ) ;
#1215 = CARTESIAN_POINT ( 'NONE',  ( 17.71800267517521377, -3.104751769966808794, -13.52637079326617453 ) ) ;
#1216 = EDGE_LOOP ( 'NONE', ( #57811, #11201, #40238 ) ) ;
#1217 = CARTESIAN_POINT ( 'NONE',  ( 11.04752711762115780, 5.162390711389719833, 7.175009463222314032 ) ) ;
#1218 = CARTESIAN_POINT ( 'NONE',  ( 11.35905860703999970, -2.719090443614000208, -7.157642341559000698 ) ) ;
#1219 = VERTEX_POINT ( 'NONE', #59857 ) ;
#1220 = CARTESIAN_POINT ( 'NONE',  ( 9.229392757687000071, 4.677963304775400566, 6.758914271013199304 ) ) ;
#1221 = CARTESIAN_POINT ( 'NONE',  ( 18.10291897067260436, 0.3009486140249941211, -13.89561788111246621 ) ) ;
#1222 = CARTESIAN_POINT ( 'NONE',  ( 5.389233442565000587, -0.5479625777084999871, 1.274769677192999939 ) ) ;
#1223 = AXIS2_PLACEMENT_3D ( 'NONE', #19547, #14309, #13625 ) ;
#1224 = CARTESIAN_POINT ( 'NONE',  ( 11.60000000000000320, 4.988477031107066750, -6.852161599766356304 ) ) ;
#1225 = CARTESIAN_POINT ( 'NONE',  ( 16.29309513285500088, 3.300500509464999954, 11.83372189959999865 ) ) ;
#1226 = CARTESIAN_POINT ( 'NONE',  ( 7.297051343136737422, 2.650314471270581063, -7.803711873237447527 ) ) ;
#1227 = AXIS2_PLACEMENT_3D ( 'NONE', #62461, #20852, #62798 ) ;
#1228 = EDGE_CURVE ( 'NONE', #12996, #40006, #20300, .T. ) ;
#1229 = CARTESIAN_POINT ( 'NONE',  ( 9.535355082327999554, 3.611978631017199959, 8.275336934318801241 ) ) ;
#1230 = CARTESIAN_POINT ( 'NONE',  ( 12.80505043854144276, 0.6249999999999994449, 13.88107975066923316 ) ) ;
#1231 = VERTEX_POINT ( 'NONE', #55311 ) ;
#1232 = DIRECTION ( 'NONE',  ( 1.000000000000000000, 0.000000000000000000, 0.000000000000000000 ) ) ;
#1233 = CARTESIAN_POINT ( 'NONE',  ( 9.991525552923999243, 4.805950298207000593, -8.932431532051998246 ) ) ;
#1234 = CARTESIAN_POINT ( 'NONE',  ( 17.65734784985741967, -11.53038622195815144, 4.891402515914990090 ) ) ;
#1235 = CARTESIAN_POINT ( 'NONE',  ( 12.18088137079341671, 2.461818645006701445, -13.68150212747531214 ) ) ;
#1236 = CARTESIAN_POINT ( 'NONE',  ( 16.39999999485600313, -3.595156957901000094, -11.99794989424000136 ) ) ;
#1237 = CARTESIAN_POINT ( 'NONE',  ( 9.409308287954999628, -2.634700736117999931, 8.920302460802998823 ) ) ;
#1238 = CARTESIAN_POINT ( 'NONE',  ( 17.99694095195319221, -0.5793931417437904186, 13.98801390351337659 ) ) ;
#1239 = CARTESIAN_POINT ( 'NONE',  ( 17.89454199030562620, 0.5248377731126082635, 13.88666204734250620 ) ) ;
#1240 = EDGE_LOOP ( 'NONE', ( #37312, #27362, #1741, #18662 ) ) ;
#1241 = ORIENTED_EDGE ( 'NONE', *, *, #9940, .T. ) ;
#1242 = CARTESIAN_POINT ( 'NONE',  ( 24.30000000000000071, 8.756202924575998026, -7.455126447192999883 ) ) ;
#1243 = CARTESIAN_POINT ( 'NONE',  ( 12.76469414187607399, -0.6250000000000007772, 13.88107975724713761 ) ) ;
#1244 = CARTESIAN_POINT ( 'NONE',  ( 12.31443335387396054, -0.3873583148778746987, -13.89273910399192147 ) ) ;
#1245 = CARTESIAN_POINT ( 'NONE',  ( 24.30001696810800027, 12.21047201856000086, 3.271805692349999628 ) ) ;
#1246 = CARTESIAN_POINT ( 'NONE',  ( 17.72543224073729817, -0.6019432101965236370, -13.88245510388864012 ) ) ;
#1247 = CARTESIAN_POINT ( 'NONE',  ( 8.796581853210000190, -2.368260286481999710, 7.410200011629000549 ) ) ;
#1248 = DIRECTION ( 'NONE',  ( -1.000000000000000000, 0.000000000000000000, 0.000000000000000000 ) ) ;
#1250 = LINE ( 'NONE', #43208, #68567 ) ;
#1249 = CARTESIAN_POINT ( 'NONE',  ( 10.91891290906799838, -4.809406943772300380, 6.509421987543800192 ) ) ;
#1251 = PLANE ( 'NONE',  #9581 ) ;
#1252 = FACE_OUTER_BOUND ( 'NONE', #59376, .T. ) ;
#1253 = CARTESIAN_POINT ( 'NONE',  ( 1.850000260467999924, -1.625000260409000141, 4.909918417534999635E-10 ) ) ;
#1254 = CARTESIAN_POINT ( 'NONE',  ( 18.06292190248829499, -0.3644117276601269717, 12.69296657371243953 ) ) ;
#1255 = DIRECTION ( 'NONE',  ( -4.331025598861020273E-21, -3.276905820014099985E-06, 0.9999999999946310725 ) ) ;
#1256 = CARTESIAN_POINT ( 'NONE',  ( 17.59643454745107505, -3.124999999999999556, -12.28373095898681910 ) ) ;
#1257 = ORIENTED_EDGE ( 'NONE', *, *, #60141, .F. ) ;
#1259 = CARTESIAN_POINT ( 'NONE',  ( 17.74638838757299553, 10.78680295286436852, -4.401676307962380186 ) ) ;
#1258 = CARTESIAN_POINT ( 'NONE',  ( 8.353308059623998361, -2.800111029801999774, 9.079936276749000612 ) ) ;
#1260 = CARTESIAN_POINT ( 'NONE',  ( 9.003345280414000840, 2.319062457810000311, -7.919229449146000022 ) ) ;
#1261 = EDGE_CURVE ( 'NONE', #64636, #25798, #1264, .T. ) ;
#1262 = CARTESIAN_POINT ( 'NONE',  ( 44.24148000000000280, -11.77655473258999841, 4.190794510628000680 ) ) ;
#1263 = FACE_OUTER_BOUND ( 'NONE', #6963, .T. ) ;
#1264 = B_SPLINE_CURVE_WITH_KNOTS ( 'NONE', 3,
 ( #28756, #50411, #13017, #2177, #23492 ),
 .UNSPECIFIED., .F., .F.,
 ( 4, 1, 4 ),
 ( 0.000000000000000000, 0.5000000000000000000, 1.000000000000000000 ),
 .UNSPECIFIED. ) ;
#1265 = CARTESIAN_POINT ( 'NONE',  ( 0.8396236793818999677, -2.525007632204000263, -2.706826389191999915 ) ) ;
#1266 = CARTESIAN_POINT ( 'NONE',  ( 10.52946886766499901, 3.569835351907400423, 8.281567006984099422 ) ) ;
#1267 = CARTESIAN_POINT ( 'NONE',  ( 2.552384041004999826, 3.577765746644000266, 1.152375606624999937 ) ) ;
#1268 = VERTEX_POINT ( 'NONE', #2512 ) ;
#1269 = CARTESIAN_POINT ( 'NONE',  ( 12.13047558099394863, 0.2638285456865417933, -12.59724228039519822 ) ) ;
#1271 = CONICAL_SURFACE ( 'NONE', #33670, 2.100040596737999810, 0.7853981633972997312 ) ;
#1270 = CARTESIAN_POINT ( 'NONE',  ( 6.899999691988000450, 12.20988339176000004, -3.111064831549000154 ) ) ;
#1272 = CARTESIAN_POINT ( 'NONE',  ( 10.14887885159599890, 5.269014563305000287, 7.651388779553199626 ) ) ;
#1273 = DIRECTION ( 'NONE',  ( 0.000000000000000000, -1.000000000000000000, 0.000000000000000000 ) ) ;
#1274 = CARTESIAN_POINT ( 'NONE',  ( 8.373670280412000011, 2.202812441249000219, 7.706988150133999405 ) ) ;
#1275 = ORIENTED_EDGE ( 'NONE', *, *, #68206, .F. ) ;
#1276 = CARTESIAN_POINT ( 'NONE',  ( 6.284559201231999737, 1.526675769738000010, -0.5259243426933000176 ) ) ;
#1277 = CARTESIAN_POINT ( 'NONE',  ( 8.145870280407001118, 3.552539078410000162, -8.999639305067001160 ) ) ;
#1278 = EDGE_CURVE ( 'NONE', #11696, #53746, #2872, .T. ) ;
#1280 = CARTESIAN_POINT ( 'NONE',  ( 9.520797373037000355, 3.270552986600999912, 5.711478154812000163 ) ) ;
#1279 = CARTESIAN_POINT ( 'NONE',  ( 8.377276386243467599, -2.937594683383006888, 8.878994193280906444 ) ) ;
#1281 = CARTESIAN_POINT ( 'NONE',  ( 11.22056920625029974, 4.047312782235129802, -6.184582852561999466 ) ) ;
#1282 = VERTEX_POINT ( 'NONE', #24530 ) ;
#1283 = LINE ( 'NONE', #33448, #6506 ) ;
#1284 = CARTESIAN_POINT ( 'NONE',  ( 9.532671748231999587, -4.663050389319001177, 8.669823109968998409 ) ) ;
#1285 = EDGE_LOOP ( 'NONE', ( #36999, #35644, #17389, #40139 ) ) ;
#1286 = ADVANCED_FACE ( 'NONE', ( #29799 ), #3878, .T. ) ;
#1287 = CARTESIAN_POINT ( 'NONE',  ( 12.15658143857204898, 2.853298863252174744, -12.27345178217327160 ) ) ;
#1288 = CARTESIAN_POINT ( 'NONE',  ( 24.81126097005384779, -8.606648885476735344, -8.517984218207937275 ) ) ;
#1289 = CARTESIAN_POINT ( 'NONE',  ( 18.17902784157848473, -0.04113803725886195500, -13.89993798560270122 ) ) ;
#1290 = EDGE_LOOP ( 'NONE', ( #30271, #11363, #2119, #42884 ) ) ;
#1291 = CARTESIAN_POINT ( 'NONE',  ( 16.09586749610213374, -8.411110950737080927, -8.060864562931225663 ) ) ;
#1292 = FILL_AREA_STYLE ('',( #64556 ) ) ;
#1293 = CARTESIAN_POINT ( 'NONE',  ( 11.31900581613029821, 4.750686773407899466, -7.982035256002799173 ) ) ;
#1294 = CARTESIAN_POINT ( 'NONE',  ( 10.20000030442999872, 12.49999969551000056, -3.568568717444000015E-10 ) ) ;
#1295 = CARTESIAN_POINT ( 'NONE',  ( 11.70733594839949809, -3.159733897807000425, 8.462948211532999920 ) ) ;
#1296 = ORIENTED_EDGE ( 'NONE', *, *, #59364, .F. ) ;
#1297 = DIRECTION ( 'NONE',  ( -1.000000000000000000, 0.000000000000000000, 0.000000000000000000 ) ) ;
#1298 = CARTESIAN_POINT ( 'NONE',  ( 12.30950027206278818, -2.881007065227998876, -13.58518188446750230 ) ) ;
#1299 = CARTESIAN_POINT ( 'NONE',  ( 9.258504216683469679, -3.836370129433861020, -6.250027056024106464 ) ) ;
#1300 = CARTESIAN_POINT ( 'NONE',  ( 17.55505043854144631, 0.7192913403693005359, 12.57945229203838267 ) ) ;
#1301 = ORIENTED_EDGE ( 'NONE', *, *, #41104, .T. ) ;
#1302 = CARTESIAN_POINT ( 'NONE',  ( 12.61159012396490731, -1.905606515074950602, -12.57035430044310331 ) ) ;
#1303 = FACE_OUTER_BOUND ( 'NONE', #8010, .T. ) ;
#1304 = CARTESIAN_POINT ( 'NONE',  ( 8.404999999999999361, 5.190914425723000214, -8.768195054477999406 ) ) ;
#1305 = DIRECTION ( 'NONE',  ( 0.000000000000000000, 1.000000000000000000, 0.000000000000000000 ) ) ;
#1306 = DIRECTION ( 'NONE',  ( -1.000000000000000000, 0.000000000000000000, 0.000000000000000000 ) ) ;
#1307 = CARTESIAN_POINT ( 'NONE',  ( 10.37872469555899890, -3.497841151814999883, -6.631215019384099740 ) ) ;
#1308 = CARTESIAN_POINT ( 'NONE',  ( 12.80505043854146940, -3.199751711897561801, 12.18694338143115452 ) ) ;
#1309 = CARTESIAN_POINT ( 'NONE',  ( 17.75769270374273390, -3.091259753241552222, 12.29395838111495465 ) ) ;
#1310 = ORIENTED_EDGE ( 'NONE', *, *, #68127, .T. ) ;
#1311 = CARTESIAN_POINT ( 'NONE',  ( 10.59725056272499977, -2.683866746800999792, -7.519505747156228992 ) ) ;
#1312 = ORIENTED_EDGE ( 'NONE', *, *, #52096, .F. ) ;
#1313 = CARTESIAN_POINT ( 'NONE',  ( 11.53681706333000179, -12.46890164658000089, -1.535189833763999978 ) ) ;
#1314 = CARTESIAN_POINT ( 'NONE',  ( 10.01622971959000097, 4.325866256860000369, -9.125812605905000652 ) ) ;
#1315 = CARTESIAN_POINT ( 'NONE',  ( 3.418575286264000201, -1.583709913295999971, 2.797960796442000131 ) ) ;
#1316 = CARTESIAN_POINT ( 'NONE',  ( 10.65650106607000147, -5.448187878199999723, -7.015213573792999036 ) ) ;
#1317 = LINE ( 'NONE', #11119, #24965 ) ;
#1318 = CARTESIAN_POINT ( 'NONE',  ( 7.607791299150002295, 3.471796661068001999, -6.504286038290998384 ) ) ;
#1319 = DIRECTION ( 'NONE',  ( 1.000000000000000000, 0.000000000000000000, 0.000000000000000000 ) ) ;
#1320 = VECTOR ( 'NONE', #52571, 1000.000000000000000 ) ;
#1321 = ORIENTED_EDGE ( 'NONE', *, *, #14631, .T. ) ;
#1322 = DIRECTION ( 'NONE',  ( 0.4682208595142289265, -0.4682208595142289265, -0.7493586947727458591 ) ) ;
#1323 = CARTESIAN_POINT ( 'NONE',  ( 10.06344080699000010, 5.156228702401000952, 6.125219923432000613 ) ) ;
#1324 = FACE_BOUND ( 'NONE', #36148, .T. ) ;
#1325 = CARTESIAN_POINT ( 'NONE',  ( 9.615066448851507630, -5.349942704376990044, -7.499996115248991124 ) ) ;
#1326 = CARTESIAN_POINT ( 'NONE',  ( 18.49055856039300139, 2.949841519493000330, -11.23086453091999992 ) ) ;
#1327 = CARTESIAN_POINT ( 'NONE',  ( 10.33364828895399867, 4.760196147278000112, -7.915211961479200475 ) ) ;
#1328 = CARTESIAN_POINT ( 'NONE',  ( 10.12947109217999930, 5.100000000000000533, 6.152188490330000370 ) ) ;
#1329 = VECTOR ( 'NONE', #54963, 1000.000000000000000 ) ;
#1330 = CARTESIAN_POINT ( 'NONE',  ( 24.22093573973900149, -8.982850686176998778, -8.867479996275999810 ) ) ;
#1331 = CARTESIAN_POINT ( 'NONE',  ( 23.64072730899000163, -10.12004117118999957, 9.384740691128001799 ) ) ;
#1332 = CARTESIAN_POINT ( 'NONE',  ( 10.90000000000000036, -8.091320520030999219, -7.077643127633000297 ) ) ;
#1333 = ORIENTED_EDGE ( 'NONE', *, *, #47460, .F. ) ;
#1334 = CARTESIAN_POINT ( 'NONE',  ( 8.207504440379000954, -5.944572422272999646, 7.106845737860000511 ) ) ;
#1335 = CARTESIAN_POINT ( 'NONE',  ( 7.326949057234999785, 0.08117426202284000469, 1.366388098755000113 ) ) ;
#1336 = ADVANCED_FACE ( 'NONE', ( #69147 ), #52485, .F. ) ;
#1337 = ADVANCED_FACE ( 'NONE', ( #40605 ), #57360, .F. ) ;
#1338 = CARTESIAN_POINT ( 'NONE',  ( 17.94528078231815371, 2.988314720655957935, 13.55762497744564321 ) ) ;
#1339 = CYLINDRICAL_SURFACE ( 'NONE', #51118, 1.250000000000000222 ) ;
#1340 = CARTESIAN_POINT ( 'NONE',  ( 10.96118313518939935, -4.792748567750200195, -8.502430091786999711 ) ) ;
#1341 = B_SPLINE_CURVE_WITH_KNOTS ( 'NONE', 3,
 ( #64302, #54167, #38789, #32176, #38439, #5581, #1381, #6267, #54521, #59413, #16420, #37748, #26924, #343, #64988, #21660, #59761, #49619 ),
 .UNSPECIFIED., .F., .F.,
 ( 4, 2, 2, 2, 2, 2, 2, 2, 4 ),
 ( 0.000000000000000000, 0.1250000000000000000, 0.2500000000000000000, 0.3750000000000000000, 0.5000000000000000000, 0.6250000000000000000, 0.7500000000000000000, 0.8750000000000000000, 1.000000000000000000 ),
 .UNSPECIFIED. ) ;
#1342 = ORIENTED_EDGE ( 'NONE', *, *, #57044, .F. ) ;
#1343 = CARTESIAN_POINT ( 'NONE',  ( 24.85114803437500086, 3.384270252302000070, -11.84837700269999949 ) ) ;
#1344 = CARTESIAN_POINT ( 'NONE',  ( 9.208107780409999776, 5.057081813675999626, 8.967637988488998957 ) ) ;
#1346 = CARTESIAN_POINT ( 'NONE',  ( 10.67905590578999941, -2.899999999999999911, 6.571291218949999902 ) ) ;
#1345 = CARTESIAN_POINT ( 'NONE',  ( 9.807804719590000886, 3.988943694240999704, -8.966360307350999648 ) ) ;
#1347 = CARTESIAN_POINT ( 'NONE',  ( 2.897287607496109807, 0.1609468932050526768, 3.253943878959492331 ) ) ;
#1348 = ORIENTED_EDGE ( 'NONE', *, *, #39585, .T. ) ;
#1349 = CARTESIAN_POINT ( 'NONE',  ( 10.91307008594999850, 2.096286256021000050, 7.827189715349000210 ) ) ;
#1351 = CARTESIAN_POINT ( 'NONE',  ( 17.57920283571460374, -1.787797991197240366, -13.88537998700429910 ) ) ;
#1350 = B_SPLINE_CURVE_WITH_KNOTS ( 'NONE', 3,
 ( #42513, #41819, #30998, #32375, #5450, #42175 ),
 .UNSPECIFIED., .F., .F.,
 ( 4, 2, 4 ),
 ( 0.000000000000000000, 0.5000000000000000000, 1.000000000000000000 ),
 .UNSPECIFIED. ) ;
#1352 = CARTESIAN_POINT ( 'NONE',  ( 11.04333729122639873, 2.996877626170000308, 7.526388557597149642 ) ) ;
#1353 = CARTESIAN_POINT ( 'NONE',  ( 9.534903635507999908, -3.030945724184999968, 8.761987396837000119 ) ) ;
#1354 = CARTESIAN_POINT ( 'NONE',  ( 8.641808059624999316, -2.933824946949000090, 8.496487880080000110 ) ) ;
#1355 = ORIENTED_EDGE ( 'NONE', *, *, #39332, .T. ) ;
#1356 = CARTESIAN_POINT ( 'NONE',  ( 8.191498616105999275, -3.399962740672999750, 6.146646623957999545 ) ) ;
#1357 = DIRECTION ( 'NONE',  ( -1.000000000000000000, 0.000000000000000000, 0.000000000000000000 ) ) ;
#1359 = CARTESIAN_POINT ( 'NONE',  ( 10.62256935321000029, -2.471463903746000224, -8.210787855397999380 ) ) ;
#1358 = CARTESIAN_POINT ( 'NONE',  ( 12.83176788310500172, -11.93188535256000016, 3.261584788209999974 ) ) ;
#1360 = CARTESIAN_POINT ( 'NONE',  ( 7.755402176232501610, -5.324011115352642598, 8.627901512810892015 ) ) ;
#1361 = CARTESIAN_POINT ( 'NONE',  ( 9.967845797207999681, -2.034786297409000078, 7.636877353231999344 ) ) ;
#1362 = CARTESIAN_POINT ( 'NONE',  ( 11.55300581613033906, -2.892415530317000272, -8.211208432468300344 ) ) ;
#1363 = ORIENTED_EDGE ( 'NONE', *, *, #20264, .F. ) ;
#1365 = CARTESIAN_POINT ( 'NONE',  ( 24.72672761098415961, -11.76480477972923389, -3.190859381812851669 ) ) ;
#1364 = VECTOR ( 'NONE', #19089, 1000.000000000000114 ) ;
#1366 = CARTESIAN_POINT ( 'NONE',  ( 10.75149413291699929, -2.962184842772000337, 7.973529073237199505 ) ) ;
#1367 = EDGE_CURVE ( 'NONE', #27101, #12493, #24548, .T. ) ;
#1368 = CARTESIAN_POINT ( 'NONE',  ( 17.60000000532009423, 11.20144845259485678, -4.552734317499857575 ) ) ;
#1369 = CARTESIAN_POINT ( 'NONE',  ( 11.20733594839949809, 4.840266102192999575, 8.462948211532999920 ) ) ;
#1370 = ORIENTED_EDGE ( 'NONE', *, *, #801, .T. ) ;
#1371 = CARTESIAN_POINT ( 'NONE',  ( 9.161379719595000637, 5.511689883260999956, -7.095113581311000672 ) ) ;
#1372 = CARTESIAN_POINT ( 'NONE',  ( 24.13719010493599981, 12.33331563296999889, -3.394048515820999867 ) ) ;
#1373 = CARTESIAN_POINT ( 'NONE',  ( 12.54706542093073018, 3.153101027525006650, -12.19910009420586050 ) ) ;
#1374 = CARTESIAN_POINT ( 'NONE',  ( 10.98791429143000009, -3.983006558652820051, 8.391963954669400039 ) ) ;
#1375 = ORIENTED_EDGE ( 'NONE', *, *, #64062, .T. ) ;
#1376 = CARTESIAN_POINT ( 'NONE',  ( 8.158337970077000990E-06, 2.999989272562999965, 0.000000000000000000 ) ) ;
#1377 = AXIS2_PLACEMENT_3D ( 'NONE', #9487, #68209, #20329 ) ;
#1378 = CARTESIAN_POINT ( 'NONE',  ( 10.62309687351639020, 5.217465845835395299, -7.827184855449101697 ) ) ;
#1379 = VERTEX_POINT ( 'NONE', #56694 ) ;
#1380 = CARTESIAN_POINT ( 'NONE',  ( 9.517197013793715854, 5.205368702673863091, 8.206177812346076905 ) ) ;
#1381 = CARTESIAN_POINT ( 'NONE',  ( 5.638359839683665165, -0.7554284705563483193, -1.310679582531387721 ) ) ;
#1382 = ORIENTED_EDGE ( 'NONE', *, *, #4865, .F. ) ;
#1383 = DIRECTION ( 'NONE',  ( 0.000000000000000000, 0.6664713972124013397, -0.7455306007789014311 ) ) ;
#1384 = CARTESIAN_POINT ( 'NONE',  ( 10.92026088462129962, 4.002135146349410810, 8.503467136482999678 ) ) ;
#1385 = CONICAL_SURFACE ( 'NONE', #46000, 2.624999810206000372, 0.7853980665166908626 ) ;
#1386 = CARTESIAN_POINT ( 'NONE',  ( 23.89320776801300283, 3.288740538445000805, -12.20874841465999516 ) ) ;
#1387 = CARTESIAN_POINT ( 'NONE',  ( 10.28774346735000123, 5.077605961126000267, -5.991341245382999503 ) ) ;
#1388 = CARTESIAN_POINT ( 'NONE',  ( 18.48305742508500416, -12.00075408335000127, 3.715624526910999759 ) ) ;
#1389 = CARTESIAN_POINT ( 'NONE',  ( 8.736413463905998711, 4.084156314540369870, 6.617590440947399344 ) ) ;
#1390 = CARTESIAN_POINT ( 'NONE',  ( 7.982285464787000961, 4.608336336177999648, -6.267435635568999963 ) ) ;
#1391 = CARTESIAN_POINT ( 'NONE',  ( 18.17180462559269571, -0.1017072266180428924, -12.69945743039636099 ) ) ;
#1392 = CARTESIAN_POINT ( 'NONE',  ( 12.19259201841741813, 2.624586292379584851, -12.42169361725944832 ) ) ;
#1393 = CARTESIAN_POINT ( 'NONE',  ( 11.57656516821460890, -3.100463633631699967, -8.407828142327998577 ) ) ;
#1394 = CARTESIAN_POINT ( 'NONE',  ( 9.187739158772000536, 5.964723767581000757, 7.776480083716999836 ) ) ;
#1395 = EDGE_LOOP ( 'NONE', ( #37179, #57187, #32619, #49048, #36873 ) ) ;
#1396 = B_SPLINE_CURVE_WITH_KNOTS ( 'NONE', 3,
 ( #38125, #59801, #11903, #21699 ),
 .UNSPECIFIED., .F., .F.,
 ( 4, 4 ),
 ( 0.000000000000000000, 1.000000000000000000 ),
 .UNSPECIFIED. ) ;
#1397 = CARTESIAN_POINT ( 'NONE',  ( 9.114639751325487538, 5.184985712744430764, -7.959719964829115035 ) ) ;
#1398 = CARTESIAN_POINT ( 'NONE',  ( 8.475341021510232054, 5.350570349241480450, 7.499981640446101494 ) ) ;
#1399 = CARTESIAN_POINT ( 'NONE',  ( 11.31944011432000075, 12.15765269271000015, 1.759220518310000037 ) ) ;
#1400 = CARTESIAN_POINT ( 'NONE',  ( 18.20050923854813263, 2.808308534135711909, 12.28305809155435924 ) ) ;
#1401 = EDGE_CURVE ( 'NONE', #46460, #36450, #58715, .T. ) ;
#1402 = CARTESIAN_POINT ( 'NONE',  ( 9.475279990687596410, 5.350441389720215213, 7.499985493516660107 ) ) ;
#1403 = ADVANCED_FACE ( 'NONE', ( #48865 ), #37022, .F. ) ;
#1404 = CARTESIAN_POINT ( 'NONE',  ( 11.08492721656000057, 3.668390701878999849, 5.558148445539999649 ) ) ;
#1405 = CARTESIAN_POINT ( 'NONE',  ( 10.43611625296362710, -3.418844976054905782, 8.154057418782388211 ) ) ;
#1406 = CARTESIAN_POINT ( 'NONE',  ( 8.783078676347997771, 3.752732269140699906, 6.553315803938899897 ) ) ;
#1407 = ORIENTED_EDGE ( 'NONE', *, *, #43007, .F. ) ;
#1408 = CARTESIAN_POINT ( 'NONE',  ( 12.15953697780020093, -2.808329718129386254, 12.28305324893824313 ) ) ;
#1409 = CARTESIAN_POINT ( 'NONE',  ( 9.226430433046999724, -4.971677342931100085, -6.900352112302299723 ) ) ;
#1410 = DIRECTION ( 'NONE',  ( 0.7071090068939822615, 0.000000000000000000, -0.7071045554721071547 ) ) ;
#1411 = CARTESIAN_POINT ( 'NONE',  ( 9.289886373836322875, -3.999992178805580334, 6.560153657526066162 ) ) ;
#1412 = AXIS2_PLACEMENT_3D ( 'NONE', #13011, #55655, #7755 ) ;
#1413 = CARTESIAN_POINT ( 'NONE',  ( 10.52641638348499953, 3.025038519517300184, -7.262511127784999410 ) ) ;
#1414 = CARTESIAN_POINT ( 'NONE',  ( 12.08472055051101890, 0.08234928811776985602, 12.59973629603894096 ) ) ;
#1415 = CARTESIAN_POINT ( 'NONE',  ( 7.983198341228001205, 5.321913229613000063, 8.118244847118999630 ) ) ;
#1416 = B_SPLINE_CURVE_WITH_KNOTS ( 'NONE', 3,
 ( #37175, #68632, #53599, #456 ),
 .UNSPECIFIED., .F., .F.,
 ( 4, 4 ),
 ( 0.000000000000000000, 1.000000000000000000 ),
 .UNSPECIFIED. ) ;
#1417 = B_SPLINE_CURVE_WITH_KNOTS ( 'NONE', 3,
 ( #33485, #17394, #59349, #2010 ),
 .UNSPECIFIED., .F., .F.,
 ( 4, 4 ),
 ( 0.8745775486650082531, 1.000000000000000000 ),
 .UNSPECIFIED. ) ;
#1418 = CARTESIAN_POINT ( 'NONE',  ( 10.52638970730999901, 2.451081172664000274, 6.282749363171999946 ) ) ;
#1419 = CARTESIAN_POINT ( 'NONE',  ( 12.59749754106150554, 3.089553852145856983, 12.29445441479364831 ) ) ;
#1420 = ORIENTED_EDGE ( 'NONE', *, *, #9940, .F. ) ;
#1421 = CARTESIAN_POINT ( 'NONE',  ( 7.726448341228000061, 2.630487280353000390, 6.995957894972000268 ) ) ;
#1422 = CARTESIAN_POINT ( 'NONE',  ( 10.39918582084299992, 3.253651555277099927, -6.637298362509499228 ) ) ;
#1423 = ADVANCED_FACE ( 'NONE', ( #974 ), #63655, .F. ) ;
#1424 = CARTESIAN_POINT ( 'NONE',  ( 9.574741131514889148, 3.579783539280448679, 8.799459768377362323 ) ) ;
#1426 = CARTESIAN_POINT ( 'NONE',  ( 24.77780280611190378, 11.71374231672910504, 3.192708380903468868 ) ) ;
#1425 = CARTESIAN_POINT ( 'NONE',  ( 12.22262912535705937, 10.88886164601108675, -4.142707164787215568 ) ) ;
#1427 = CARTESIAN_POINT ( 'NONE',  ( 11.46595122972049907, -3.656201404350900130, -6.704952129760900270 ) ) ;
#1428 = CARTESIAN_POINT ( 'NONE',  ( 23.59999193302000364, -13.22318594659000013, 4.267778254689999606 ) ) ;
#1429 = ORIENTED_EDGE ( 'NONE', *, *, #56998, .F. ) ;
#1430 = CIRCLE ( 'NONE', #49428, 11.84999999999999964 ) ;
#1431 = EDGE_CURVE ( 'NONE', #59495, #14271, #42132, .T. ) ;
#1432 = CARTESIAN_POINT ( 'NONE',  ( 1.014608762361999927, 1.892658550137999995, 3.053125390820000007 ) ) ;
#1433 = CARTESIAN_POINT ( 'NONE',  ( 6.903516731156273067, -1.060941250248529810, 0.7957428194428121104 ) ) ;
#1434 = CARTESIAN_POINT ( 'NONE',  ( 17.92003806247919329, 0.6285461057906830407, -12.58436427553157166 ) ) ;
#1435 = CARTESIAN_POINT ( 'NONE',  ( 11.80000000000000071, -49.70447530208000586, -8.683202977359000485 ) ) ;
#1436 = CARTESIAN_POINT ( 'NONE',  ( 8.724507172011824352, 3.875764422069722492, -8.374507226493388856 ) ) ;
#1437 = CARTESIAN_POINT ( 'NONE',  ( 12.18685148345903890, -2.135865664097126526, 13.83612956354244083 ) ) ;
#1438 = CARTESIAN_POINT ( 'NONE',  ( 6.999999691988000095, 0.000000000000000000, 0.000000000000000000 ) ) ;
#1439 = CARTESIAN_POINT ( 'NONE',  ( 24.22079749817700289, 3.188112890658000076, -12.21338637798000093 ) ) ;
#1440 = CARTESIAN_POINT ( 'NONE',  ( 12.99403162610500040, -12.11619719077999946, -2.031914795679000019 ) ) ;
#1441 = VERTEX_POINT ( 'NONE', #57891 ) ;
#1442 = CARTESIAN_POINT ( 'NONE',  ( 8.370221971083998014, 8.037647819758998224, -4.982909524621000230 ) ) ;
#1443 = DIRECTION ( 'NONE',  ( 0.000000000000000000, 0.000000000000000000, -1.000000000000000000 ) ) ;
#1444 = CARTESIAN_POINT ( 'NONE',  ( 11.59999999999999964, -4.883784007588900522, -7.825000000000000178 ) ) ;
#1445 = CARTESIAN_POINT ( 'NONE',  ( 18.22968849645625511, -3.214251582956586528, -11.19784508593207484 ) ) ;
#1446 = CARTESIAN_POINT ( 'NONE',  ( 1.085247135132000107, 2.814509306356999918, 2.491368026013999870 ) ) ;
#1447 = CARTESIAN_POINT ( 'NONE',  ( 10.66714959199030410, 5.079709024444567511, -8.329714913667638498 ) ) ;
#1448 = B_SPLINE_CURVE_WITH_KNOTS ( 'NONE', 3,
 ( #31023, #3398, #41841, #19833, #40461, #62470, #46407, #52331, #35911, #61791 ),
 .UNSPECIFIED., .F., .F.,
 ( 4, 2, 2, 2, 4 ),
 ( 0.000000000000000000, 0.1250000000000001665, 0.2500000000000002776, 0.3750000000000004441, 0.5000000000000005551 ),
 .UNSPECIFIED. ) ;
#1449 = ADVANCED_FACE ( 'NONE', ( #9991 ), #58479, .F. ) ;
#1450 = CARTESIAN_POINT ( 'NONE',  ( 18.03475265876376810, 2.099231872491031936, -12.53598779768163318 ) ) ;
#1451 = CARTESIAN_POINT ( 'NONE',  ( 9.748087964304161801, -3.672831456759385382, 8.717422821756882101 ) ) ;
#1452 = CARTESIAN_POINT ( 'NONE',  ( 10.72749279009019929, 3.774717370312400178, 6.663611138821799784 ) ) ;
#1453 = CARTESIAN_POINT ( 'NONE',  ( 11.72005178064354780, -3.595543782890631146, 11.99782022136165871 ) ) ;
#1454 = CARTESIAN_POINT ( 'NONE',  ( 11.16750564679000135, -3.188702545307000147, -8.788667016604001958 ) ) ;
#1455 = DIRECTION ( 'NONE',  ( 0.000000000000000000, 0.000000000000000000, -1.000000000000000000 ) ) ;
#1456 = CARTESIAN_POINT ( 'NONE',  ( 24.46275371508600216, 12.39843049379000028, 3.098824767661999768 ) ) ;
#1457 = CARTESIAN_POINT ( 'NONE',  ( 9.408231868349719917, 5.323181814481385388, 7.228671914213086858 ) ) ;
#1458 = ORIENTED_EDGE ( 'NONE', *, *, #33084, .T. ) ;
#1459 = CARTESIAN_POINT ( 'NONE',  ( 8.994485841233000656, 3.854507394315999758, -9.394302886912999639 ) ) ;
#1460 = ORIENTED_EDGE ( 'NONE', *, *, #17637, .F. ) ;
#1461 = VECTOR ( 'NONE', #1082, 1000.000000000000000 ) ;
#1462 = CARTESIAN_POINT ( 'NONE',  ( 18.17918265292645685, -2.461360938835027934, 13.68159685767607137 ) ) ;
#1463 = CARTESIAN_POINT ( 'NONE',  ( 10.19810941423799910, -3.053977294209000437, -6.640722727400100389 ) ) ;
#1464 = EDGE_LOOP ( 'NONE', ( #38827, #63076, #36669, #30707 ) ) ;
#1465 = CARTESIAN_POINT ( 'NONE',  ( 10.98146005378009882, 4.911671201000399556, 7.986817550794899745 ) ) ;
#1466 = CARTESIAN_POINT ( 'NONE',  ( 27.64127793187000037, 2.399999999999999911, 6.571291218949999902 ) ) ;
#1467 = CARTESIAN_POINT ( 'NONE',  ( 8.396419424012371735, 5.286796060078585491, 7.027454876807467166 ) ) ;
#1468 = CARTESIAN_POINT ( 'NONE',  ( 10.83668832355999889, 4.288537082977999404, 9.448742031664000507 ) ) ;
#1469 = CARTESIAN_POINT ( 'NONE',  ( 24.30001694670299983, 8.938702829764999080, 8.938676122491999720 ) ) ;
#1470 = CARTESIAN_POINT ( 'NONE',  ( 11.09999999969000051, 8.475027130630000016, -6.745942718869000210 ) ) ;
#1471 = CARTESIAN_POINT ( 'NONE',  ( 11.31919037786000182, 3.456300244116000453, -11.37193521011000108 ) ) ;
#1472 = CARTESIAN_POINT ( 'NONE',  ( 11.15192313136999935, -2.359310578948000003, -6.636692315558000210 ) ) ;
#1473 = CARTESIAN_POINT ( 'NONE',  ( 11.49056651104150006, -3.914543207408039738, -6.638028001068500217 ) ) ;
#1474 = ORIENTED_EDGE ( 'NONE', *, *, #36051, .F. ) ;
#1475 = CYLINDRICAL_SURFACE ( 'NONE', #7670, 0.4999999999999998335 ) ;
#1476 = VERTEX_POINT ( 'NONE', #44240 ) ;
#1477 = VECTOR ( 'NONE', #32084, 1000.000000000000000 ) ;
#1478 = CARTESIAN_POINT ( 'NONE',  ( 8.857090631127384484, 4.619515535681817830, -6.695274228472994693 ) ) ;
#1479 = ORIENTED_EDGE ( 'NONE', *, *, #21563, .T. ) ;
#1480 = CARTESIAN_POINT ( 'NONE',  ( 17.79074592071068039, -3.210128306667220155, -13.62701119231860680 ) ) ;
#1481 = VECTOR ( 'NONE', #30903, 1000.000000000000000 ) ;
#1482 = CARTESIAN_POINT ( 'NONE',  ( 10.32769335537625111, -3.168316061382061566, 4.960153499376385611 ) ) ;
#1483 = CARTESIAN_POINT ( 'NONE',  ( 12.80505043854144276, 0.7192913403693015351, 12.57945229203838267 ) ) ;
#1484 = EDGE_CURVE ( 'NONE', #44214, #24573, #12032, .T. ) ;
#1485 = CARTESIAN_POINT ( 'NONE',  ( 12.39041931600610091, 2.032227219086496284, 13.76156428297225709 ) ) ;
#1486 = ADVANCED_FACE ( 'NONE', ( #33394 ), #6869, .T. ) ;
#1487 = CARTESIAN_POINT ( 'NONE',  ( 9.569799020577001158, -4.064052785562999759, 8.919253808370999792 ) ) ;
#1488 = CARTESIAN_POINT ( 'NONE',  ( 12.78475401282448942, 0.6249999999999995559, -12.67928921589118474 ) ) ;
#1489 = ADVANCED_FACE ( 'NONE', ( #54710 ), #63063, .F. ) ;
#1490 = CARTESIAN_POINT ( 'NONE',  ( 12.57146999070152837, 0.6916885356983997202, 13.98290438115173551 ) ) ;
#1491 = EDGE_LOOP ( 'NONE', ( #34098, #13524, #34844, #26152 ) ) ;
#1492 = CARTESIAN_POINT ( 'NONE',  ( 7.424590560819000373, 5.346164515353000191, -7.398308812559000636 ) ) ;
#1493 = DIRECTION ( 'NONE',  ( 0.000000000000000000, -0.8648648648648720183, 0.5020047465136825426 ) ) ;
#1494 = CARTESIAN_POINT ( 'NONE',  ( 23.85158989719599987, -3.519737302176999982, -13.16814931014999956 ) ) ;
#1495 = CARTESIAN_POINT ( 'NONE',  ( 4.550764323399000055, 1.072805779648999813, -0.5080389213338001309 ) ) ;
#1496 = B_SPLINE_CURVE_WITH_KNOTS ( 'NONE', 3,
 ( #53555, #757, #32921, #64363 ),
 .UNSPECIFIED., .F., .F.,
 ( 4, 4 ),
 ( 0.000000000000000000, 0.1253988501910747455 ),
 .UNSPECIFIED. ) ;
#1497 = CARTESIAN_POINT ( 'NONE',  ( 8.929995280412999392, 5.030502105212999453, -6.322203460290999999 ) ) ;
#1498 = CARTESIAN_POINT ( 'NONE',  ( 9.896013540183126622, 3.000416447002273834, -8.268183399968641822 ) ) ;
#1499 = CARTESIAN_POINT ( 'NONE',  ( 10.43283788151999936, -3.279327064383000145, -9.029275888523999427 ) ) ;
#1500 = DIRECTION ( 'NONE',  ( -1.000000000000000000, 0.000000000000000000, 0.000000000000000000 ) ) ;
#1501 = PLANE ( 'NONE',  #44912 ) ;
#1502 = LINE ( 'NONE', #17589, #63425 ) ;
#1503 = CARTESIAN_POINT ( 'NONE',  ( 5.000000000000000000, -0.2999999999999999889, -6.709430130811999682 ) ) ;
#1504 = FACE_OUTER_BOUND ( 'NONE', #31225, .T. ) ;
#1505 = FACE_OUTER_BOUND ( 'NONE', #35515, .T. ) ;
#1506 = CARTESIAN_POINT ( 'NONE',  ( 11.23078751119019891, 3.084247107206000038, -7.979095341142500075 ) ) ;
#1507 = CARTESIAN_POINT ( 'NONE',  ( 9.482684229509999341, 3.291972602441000095, -6.787581931282099745 ) ) ;
#1509 = CARTESIAN_POINT ( 'NONE',  ( 10.32941944301999904, -3.080527974829000204, 4.567383801607999949 ) ) ;
#1508 = CARTESIAN_POINT ( 'NONE',  ( 10.55826717315600050, -4.659895246859299789, 8.062357722167599050 ) ) ;
#1510 = CARTESIAN_POINT ( 'NONE',  ( 11.39393020684959978, -5.250000000000000000, 7.500000000000000000 ) ) ;
#1511 = ORIENTED_EDGE ( 'NONE', *, *, #59478, .F. ) ;
#1512 = CONICAL_SURFACE ( 'NONE', #11528, 11.34994642770999818, 0.7853934433896081480 ) ;
#1513 = CARTESIAN_POINT ( 'NONE',  ( 11.67403632436368888, 3.023821283238099955, 7.727966254184200245 ) ) ;
#1514 = CARTESIAN_POINT ( 'NONE',  ( 9.442841440870999747, -2.691258483914000355, 6.269525829285999663 ) ) ;
#1515 = CARTESIAN_POINT ( 'NONE',  ( 9.329759580229000093, 2.755835090116000696, 7.797385380423699885 ) ) ;
#1516 = CARTESIAN_POINT ( 'NONE',  ( 10.74809687351632448, -3.672815144550895194, -6.282534154164607365 ) ) ;
#1517 = CARTESIAN_POINT ( 'NONE',  ( 10.15903154954000165, -4.166415630773999901, 9.114167874391000623 ) ) ;
#1518 = CARTESIAN_POINT ( 'NONE',  ( 10.90453766415000025, -2.900310535872000273, -5.130381900875999435 ) ) ;
#1519 = CARTESIAN_POINT ( 'NONE',  ( 10.59184687351642751, 4.999583552997727054, 6.731816600031356401 ) ) ;
#1520 = ORIENTED_EDGE ( 'NONE', *, *, #12013, .F. ) ;
#1521 = CARTESIAN_POINT ( 'NONE',  ( 9.305380199233999505, -3.003429752324399793, -7.374740103075099640 ) ) ;
#1522 = CARTESIAN_POINT ( 'NONE',  ( 9.614763540183329127, -2.782534154164604256, -7.172815144550903632 ) ) ;
#1523 = CARTESIAN_POINT ( 'NONE',  ( 6.326836143768000298, 1.551976682437999910, -0.4457619964912000188 ) ) ;
#1524 = EDGE_CURVE ( 'NONE', #48385, #63935, #65393, .T. ) ;
#1525 = CARTESIAN_POINT ( 'NONE',  ( 8.666062080003996471, -2.822439486461001401, -6.845494810064998603 ) ) ;
#1526 = AXIS2_PLACEMENT_3D ( 'NONE', #10852, #31849, #11534 ) ;
#1527 = CARTESIAN_POINT ( 'NONE',  ( 25.59994555223599733, 8.527741194213000142, 7.260611644044000279 ) ) ;
#1528 = CARTESIAN_POINT ( 'NONE',  ( 11.84287482311539996, -3.196874704906699893, 7.175518335304800210 ) ) ;
#1529 = CARTESIAN_POINT ( 'NONE',  ( 10.48133997687999930, 4.184599793140999502, -6.653701289769800020 ) ) ;
#1530 = CARTESIAN_POINT ( 'NONE',  ( 6.899999691988000450, 12.43893545635000031, -2.828937028792000152 ) ) ;
#1531 = CARTESIAN_POINT ( 'NONE',  ( 24.87547543774200065, -8.587518678078000178, 8.379277945963000462 ) ) ;
#1532 = CARTESIAN_POINT ( 'NONE',  ( 12.80505043854143388, 1.760910691117811844, 12.47634535983622861 ) ) ;
#1533 = ORIENTED_EDGE ( 'NONE', *, *, #47663, .F. ) ;
#1534 = CARTESIAN_POINT ( 'NONE',  ( 7.548482128266483571, -4.828745666966125505, 8.579002673691162428 ) ) ;
#1535 = CARTESIAN_POINT ( 'NONE',  ( 12.12622056954395156, -0.2566959043864930345, -13.99765098363215365 ) ) ;
#1536 = CARTESIAN_POINT ( 'NONE',  ( 13.87289819560299975, -8.829573912736998764, -7.542332231507000273 ) ) ;
#1537 = CARTESIAN_POINT ( 'NONE',  ( 2.312398069789000310, -2.519008840803133698, -2.453290717214521077 ) ) ;
#1538 = CARTESIAN_POINT ( 'NONE',  ( 10.39393020684999946, -5.250000000000000000, -7.500000000000000000 ) ) ;
#1539 = DIRECTION ( 'NONE',  ( 0.000000000000000000, 0.000000000000000000, 1.000000000000000000 ) ) ;
#1540 = CARTESIAN_POINT ( 'NONE',  ( 10.26685100253999927, 2.832432432432000269, 6.822293592207000934 ) ) ;
#1541 = VERTEX_POINT ( 'NONE', #16267 ) ;
#1542 = CARTESIAN_POINT ( 'NONE',  ( 0.1274953728650994322, -0.5341933183653647665, -3.127475674304287967 ) ) ;
#1543 = CARTESIAN_POINT ( 'NONE',  ( 18.15689837892989544, 2.331154328543900700, -13.70782442673660384 ) ) ;
#1544 = ORIENTED_EDGE ( 'NONE', *, *, #22077, .T. ) ;
#1545 = FACE_OUTER_BOUND ( 'NONE', #6452, .T. ) ;
#1546 = CARTESIAN_POINT ( 'NONE',  ( 8.866808059624998961, -2.550589632307000088, 8.854674225901000284 ) ) ;
#1547 = CARTESIAN_POINT ( 'NONE',  ( 8.424364158774000799, 3.292387953886000140, -6.294868737226000377 ) ) ;
#1548 = CARTESIAN_POINT ( 'NONE',  ( 24.17206752463402708, -12.42860866793109231, 3.341570834813612390 ) ) ;
#1549 = CARTESIAN_POINT ( 'NONE',  ( 11.26212378248529866, -4.615095948180499619, -6.336291382830999908 ) ) ;
#1550 = CARTESIAN_POINT ( 'NONE',  ( 17.85612272126378031, 0.5477996803047007202, -12.68409554377638315 ) ) ;
#1551 = DIRECTION ( 'NONE',  ( -1.000000000000000000, 0.000000000000000000, 0.000000000000000000 ) ) ;
#1552 = ORIENTED_EDGE ( 'NONE', *, *, #16777, .F. ) ;
#1553 = CARTESIAN_POINT ( 'NONE',  ( 8.849204462305999996, 2.899999999999999911, -6.662590550603814776 ) ) ;
#1554 = AXIS2_PLACEMENT_3D ( 'NONE', #1589, #22905, #65555 ) ;
#1555 = CARTESIAN_POINT ( 'NONE',  ( 18.11165249910125752, -2.784436927218168378, -13.60895423192975073 ) ) ;
#1556 = CARTESIAN_POINT ( 'NONE',  ( 9.643864158774000828, 2.927176851028000293, -5.932007155957999878 ) ) ;
#1557 = VERTEX_POINT ( 'NONE', #58926 ) ;
#1558 = CARTESIAN_POINT ( 'NONE',  ( 10.64447074117000014, 5.073827170570999634, -8.340679549192000053 ) ) ;
#1559 = CARTESIAN_POINT ( 'NONE',  ( 9.284678295047999796, -4.000000000000000000, 7.500000000000000000 ) ) ;
#1560 = ORIENTED_EDGE ( 'NONE', *, *, #37783, .F. ) ;
#1561 = CARTESIAN_POINT ( 'NONE',  ( 9.406696787962999906, 4.172481380750499902, 8.489491017455099708 ) ) ;
#1562 = CARTESIAN_POINT ( 'NONE',  ( 17.95087979294698499, -3.083166700081136025, -12.21696069964854559 ) ) ;
#1563 = CARTESIAN_POINT ( 'NONE',  ( 23.50387503050299998, 3.769846058462999530E-06, -14.00000000000000000 ) ) ;
#1564 = CARTESIAN_POINT ( 'NONE',  ( 15.99022209853100129, 3.654801648850000362, 11.82543339652000114 ) ) ;
#1565 = CARTESIAN_POINT ( 'NONE',  ( 23.60205915885299888, 2.489696159930001595, 12.09604418630999945 ) ) ;
#1566 = EDGE_CURVE ( 'NONE', #852, #67663, #47083, .T. ) ;
#1567 = ADVANCED_FACE ( 'NONE', ( #23930 ), #45266, .F. ) ;
#1568 = CARTESIAN_POINT ( 'NONE',  ( 10.03992546752099990, 2.997990738918999920, 7.569424354486659290 ) ) ;
#1569 = ADVANCED_FACE ( 'NONE', ( #51195 ), #60302, .T. ) ;
#1570 = ADVANCED_FACE ( 'NONE', ( #39324 ), #59792, .F. ) ;
#1571 = CARTESIAN_POINT ( 'NONE',  ( 8.712501735000000025, 3.641148095589300304, -8.276078370613198842 ) ) ;
#1572 = ORIENTED_EDGE ( 'NONE', *, *, #63116, .F. ) ;
#1573 = CARTESIAN_POINT ( 'NONE',  ( 17.79999999998900151, -3.595165934733000057, -11.99793354950999991 ) ) ;
#1574 = CARTESIAN_POINT ( 'NONE',  ( 11.24323278040999874, 2.479734175328000223, -7.587230544849999703 ) ) ;
#1575 = CARTESIAN_POINT ( 'NONE',  ( 17.90362871669234579, -11.55108254360806264, 4.842339049571677378 ) ) ;
#1576 = CARTESIAN_POINT ( 'NONE',  ( 12.39110436774224588, 2.968713941934965295, -13.56281002627123122 ) ) ;
#1577 = CARTESIAN_POINT ( 'NONE',  ( 10.31759632033899976, -5.184381781355999586, -7.016653143730500197 ) ) ;
#1578 = CARTESIAN_POINT ( 'NONE',  ( 24.87547783684399860, 2.962907585147000145, 11.62664596340999879 ) ) ;
#1579 = CARTESIAN_POINT ( 'NONE',  ( 17.96724268330523344, 0.4699225802676941233, 13.88930950616752114 ) ) ;
#1580 = TOROIDAL_SURFACE ( 'NONE', #38402, 6.000000000000000000, 1.000000000000000000 ) ;
#1581 = CARTESIAN_POINT ( 'NONE',  ( 17.82908354283126329, 0.5620915422200578604, 13.88470483921787135 ) ) ;
#1582 = EDGE_LOOP ( 'NONE', ( #30528, #56779, #3834, #2096, #67818 ) ) ;
#1583 = ORIENTED_EDGE ( 'NONE', *, *, #45645, .F. ) ;
#1584 = CARTESIAN_POINT ( 'NONE',  ( 8.848264158775000610, 5.751585344281000545, -8.235867044345999588 ) ) ;
#1585 = CARTESIAN_POINT ( 'NONE',  ( 12.27345183621622837, -0.3288514424339070708, 13.89476819318031708 ) ) ;
#1586 = AXIS2_PLACEMENT_3D ( 'NONE', #15876, #57487, #64105 ) ;
#1587 = CARTESIAN_POINT ( 'NONE',  ( 12.70148458876750652, -0.6166668696418402540, -13.88158203759318887 ) ) ;
#1588 = CARTESIAN_POINT ( 'NONE',  ( 10.75110221171000013, -2.822135527917999820, 6.655890318096999714 ) ) ;
#1589 = CARTESIAN_POINT ( 'NONE',  ( 0.000000000000000000, 2.899999999999999911, 7.500000000000000000 ) ) ;
#1590 = EDGE_CURVE ( 'NONE', #12209, #11759, #18729, .T. ) ;
#1591 = DIRECTION ( 'NONE',  ( 1.000000000000000000, 0.000000000000000000, 0.000000000000000000 ) ) ;
#1592 = DIRECTION ( 'NONE',  ( 0.000000000000000000, -0.8350135785640888653, -0.5502293372890927348 ) ) ;
#1594 = CYLINDRICAL_SURFACE ( 'NONE', #31758, 0.6250000000000005551 ) ;
#1593 = CARTESIAN_POINT ( 'NONE',  ( 10.76693802597399952, -4.665064168510499876, 8.592736948783000983 ) ) ;
#1595 = CARTESIAN_POINT ( 'NONE',  ( 8.851049249631991245, -5.136676904523000076, -6.770570396461005558 ) ) ;
#1596 = CARTESIAN_POINT ( 'NONE',  ( 12.10000000000000142, -3.261098123302581531, 6.529275711103853297 ) ) ;
#1597 = CARTESIAN_POINT ( 'NONE',  ( 8.817138961223998095, 4.718363881473300658, -7.985449642667900250 ) ) ;
#1598 = CARTESIAN_POINT ( 'NONE',  ( 17.83205770179218774, 0.5603556898929425989, 12.68335562943300232 ) ) ;
#1599 = B_SPLINE_SURFACE_WITH_KNOTS ( 'NONE', 3, 3, ( 
 ( #37380, #15714, #30765, #37042, #58357, #20269, #42628, #36701, #58021, #26555, #46504, #9088, #52075, #57321, #10123, #4521, #10459, #14686, #25857, #4179, #3831, #25169, #9422, #25518, #47537, #46846, #41595, #41252, #62567, #68150, #19931, #31801, #31455, #15025, #62904, #52773, #36349, #47882, #31121, #69186, #57664, #53117, #21298, #4868, #5219, #63938, #9770, #26209, #16049, #30427, #15372, #51737, #67807, #68842, #36005, #20960, #42298, #63596, #52424, #47190, #68491, #20615, #41939, #63247, #54491, #319, #17433 ),
 ( #22669, #48563, #64277, #6592, #6936, #17788, #53465, #28271, #27933, #11834, #49591, #5897, #38061, #11152, #23018, #1016, #21635, #22324, #32826, #60087, #64963, #42970, #43666, #58702, #54142, #5558, #16394, #17076, #38762, #49242, #44366, #1352, #65665, #38409, #44012, #1698, #65317, #12193, #37721, #10805, #48908, #33521, #59733, #27582, #33174, #59385, #6240, #32149, #26900, #54840, #48212, #59050, #32486, #27239, #53800, #667, #21979, #43320, #64624, #16732, #11486, #56217, #49940, #55182, #24745, #3069, #28979 ),
 ( #13239, #50286, #8667, #23711, #18473, #61802, #7632, #45046, #61462, #45389, #46071, #67377, #29317, #7287, #24402, #39799, #2051, #66700, #28626, #23370, #66354, #55534, #56560, #13919, #34565, #18822, #61123, #44710, #34901, #55878, #30012, #24056, #18130, #51315, #60430, #39106, #35246, #7984, #40147, #50630, #3410, #12538, #33867, #66007, #2731, #2387, #39452, #45732, #13581, #60771, #8327, #29670, #50973, #67040, #12886, #19151, #34215, #40473, #47447, #30679, #53034, #47105, #68402, #36959, #56902, #47800, #62480 ),
 ( #20870, #26467, #5130, #9683, #9001, #4779, #20180, #51650, #25774, #35590, #30344, #25428, #35921, #58273, #63511, #14938, #20525, #41507, #3747, #15286, #4091, #10376, #4435, #67717, #31714, #40818, #19501, #15628, #57579, #41851, #46761, #62143, #14262, #25083, #46416, #68064, #51986, #19844, #52683, #31033, #41173, #62819, #9334, #63157, #36262, #14601, #26119, #57234, #68753, #42209, #52341, #36610, #57936, #10032, #31371, #37295, #29148, #42887, #48132, #932, #64535, #1272, #5480, #16652, #21551, #63852, #15965 ) ),
 .UNSPECIFIED., .F., .F., .F.,
 ( 4, 4 ),
 ( 4, 1, 1, 1, 1, 1, 1, 1, 1, 1, 1, 1, 1, 1, 1, 1, 1, 1, 1, 1, 1, 1, 1, 1, 1, 1, 1, 1, 1, 1, 1, 1, 1, 1, 1, 1, 1, 1, 1, 1, 1, 1, 1, 1, 1, 1, 1, 1, 1, 1, 1, 1, 1, 1, 1, 1, 1, 1, 1, 1, 1, 1, 1, 1, 4 ),
 ( -0.02000000000000000042, 1.020000000000000018 ),
 ( 0.008747244164287000176, 0.02453926110774999961, 0.04033127805120999970, 0.05612329499467000327, 0.07191531193812999989, 0.08770732888158999652, 0.1034993458251000087, 0.1192913627684999978, 0.1350833797120000179, 0.1508753966553999792, 0.1666674135988999994, 0.1824594305423999918, 0.1982514474858000086, 0.2140434644293000011, 0.2298354813727000179, 0.2456274983162000103, 0.2614195152596999749, 0.2772115322030999640, 0.2930035491465999842, 0.3087955660900000288, 0.3245875830334999934, 0.3403795999769999581, 0.3561716169204000026, 0.3719636338639000228, 0.3877556508073999875, 0.4035476677507999765, 0.4193396846942999967, 0.4351317016376999858, 0.4509237185811999504, 0.4667157355247000261, 0.4825077524681000152, 0.4982997694115999798, 0.5140917863550000799, 0.5298838032985000446, 0.5456758202420000092, 0.5614678371854000538, 0.5772598541289000185, 0.5930518710723000630, 0.6088438880158000277, 0.6246359049592999924, 0.6404279219027000369, 0.6562199388462000016, 0.6720119557896999662, 0.6878039727331000108, 0.7035959896765999755, 0.7193880066200000201, 0.7351800235634999847, 0.7509720405069999494, 0.7667640574504001050, 0.7825560743939000696, 0.7983480913373000032, 0.8141401082808000789, 0.8299321252243000435, 0.8457241421676999771, 0.8615161591112000528, 0.8773081760545999863, 0.8931001929981000620, 0.9088922099416000266, 0.9246842268849999602, 0.9404762438285000359, 0.9562682607720000005, 0.9720602777153999341, 0.9878522946589000098, 1.003644311601999961, 1.019436328545999970 ),
 .UNSPECIFIED. ) ;
#1600 = CARTESIAN_POINT ( 'NONE',  ( 10.31498017945871126, -2.650031506806249659, -7.499998780888571304 ) ) ;
#1601 = CARTESIAN_POINT ( 'NONE',  ( 18.16712151970202882, -2.626596269781440007, -12.42116978061999433 ) ) ;
#1602 = VERTEX_POINT ( 'NONE', #47322 ) ;
#1604 = CARTESIAN_POINT ( 'NONE',  ( 7.961495038489999843, 3.389986099490999827, -6.279439026173999849 ) ) ;
#1603 = CARTESIAN_POINT ( 'NONE',  ( 11.73627509987185746, -4.272452942476324012, 8.750000000000000000 ) ) ;
#1605 = CARTESIAN_POINT ( 'NONE',  ( 8.704995280412999747, 5.140767546012999567, -6.196177269779999719 ) ) ;
#1606 = CARTESIAN_POINT ( 'NONE',  ( 12.70155625791299947, -1.883284863834662648, 13.78507964965113963 ) ) ;
#1607 = CARTESIAN_POINT ( 'NONE',  ( 23.56665676678199972, -7.629452625224000015E-13, 2.908784324518000003E-13 ) ) ;
#1608 = VECTOR ( 'NONE', #56881, 1000.000000000000000 ) ;
#1609 = CARTESIAN_POINT ( 'NONE',  ( 0.4283022342298000162, 1.316872153397000034, -3.459566938009000392 ) ) ;
#1610 = B_SPLINE_SURFACE_WITH_KNOTS ( 'NONE', 3, 3, ( 
 ( #57043, #37102, #43030, #58760 ),
 ( #10864, #36760, #21357, #9833 ),
 ( #21694, #5276, #58081, #42355 ),
 ( #32210, #31860, #68551, #37 ) ),
 .UNSPECIFIED., .F., .F., .F.,
 ( 4, 4 ),
 ( 4, 4 ),
 ( -0.01349945606786999951, 0.08053609420915000539 ),
 ( -0.0005287450254680999126, 0.02696599629895000266 ),
 .UNSPECIFIED. ) ;
#1611 = EDGE_CURVE ( 'NONE', #23725, #4046, #18063, .T. ) ;
#1612 = CARTESIAN_POINT ( 'NONE',  ( 9.374036292344317900, 2.996224904950563150, 8.935525811917834460 ) ) ;
#1613 = CARTESIAN_POINT ( 'NONE',  ( 2.399791516557000293, -2.527095471400999660, 2.312705381146000327 ) ) ;
#1614 = ORIENTED_EDGE ( 'NONE', *, *, #62391, .F. ) ;
#1615 = CARTESIAN_POINT ( 'NONE',  ( 12.08146954708834997, 0.04649795050485474451, -12.59991969135870526 ) ) ;
#1616 = CARTESIAN_POINT ( 'NONE',  ( 11.00000000000000000, -2.920245322398999921, -7.825000000000000178 ) ) ;
#1617 = EDGE_CURVE ( 'NONE', #31379, #59008, #56247, .T. ) ;
#1618 = CARTESIAN_POINT ( 'NONE',  ( 23.79452366329859458, -13.02995649425213465, -3.714610742098415130 ) ) ;
#1619 = CARTESIAN_POINT ( 'NONE',  ( 7.705392219590000202, 3.245534453799999941, 8.949623695221001540 ) ) ;
#1620 = ORIENTED_EDGE ( 'NONE', *, *, #65212, .F. ) ;
#1621 = CARTESIAN_POINT ( 'NONE',  ( 6.435802160082999990, 0.003195320017092000316, 1.614721372341000105 ) ) ;
#1622 = CARTESIAN_POINT ( 'NONE',  ( 8.584535841227999953, 5.395910762051999932, -7.432402852051000153 ) ) ;
#1624 = DIRECTION ( 'NONE',  ( 1.000000000000000000, 0.000000000000000000, 0.000000000000000000 ) ) ;
#1623 = CARTESIAN_POINT ( 'NONE',  ( 23.56664676942400050, 2.935522432666999748, 13.67843419499999946 ) ) ;
#1625 =( GEOMETRIC_REPRESENTATION_CONTEXT ( 3 ) GLOBAL_UNCERTAINTY_ASSIGNED_CONTEXT ( ( #23190 ) ) GLOBAL_UNIT_ASSIGNED_CONTEXT ( ( #12731, #28118, #7829 ) ) REPRESENTATION_CONTEXT ( 'NONE', 'WORKASPACE' ) );
#1626 = CARTESIAN_POINT ( 'NONE',  ( 10.35376078907947495, -3.141705924399422312, -7.665591875800525479 ) ) ;
#1627 = ORIENTED_EDGE ( 'NONE', *, *, #25480, .F. ) ;
#1628 = CARTESIAN_POINT ( 'NONE',  ( 16.43164332880499856, -3.528999066054999467, -11.96046905204000055 ) ) ;
#1629 = FILL_AREA_STYLE_COLOUR ( '', #4910 ) ;
#1630 = ORIENTED_EDGE ( 'NONE', *, *, #46199, .T. ) ;
#1631 = CARTESIAN_POINT ( 'NONE',  ( 9.769471092180999960, -5.100000000000000533, -6.152188490330000370 ) ) ;
#1632 = CARTESIAN_POINT ( 'NONE',  ( 12.80505043854146763, -3.248147246781390329, -13.61798588129781074 ) ) ;
#1633 = CIRCLE ( 'NONE', #34034, 5.000000000000000000 ) ;
#1634 = CARTESIAN_POINT ( 'NONE',  ( 18.06311169547815254, -0.3645810575750400573, -13.89357890581303501 ) ) ;
#1635 = EDGE_LOOP ( 'NONE', ( #49943, #30620, #39046, #66215, #5952, #10313 ) ) ;
#1636 = CARTESIAN_POINT ( 'NONE',  ( 12.80505043854143388, 2.499999999999999556, -25.00000000000000000 ) ) ;
#1637 = CARTESIAN_POINT ( 'NONE',  ( 25.49996575949806044, -2.042068214647287938, -11.11386275109044774 ) ) ;
#1638 = CARTESIAN_POINT ( 'NONE',  ( 10.10434687351666661, -2.749999999999998224, 7.663624617374462211 ) ) ;
#1639 = DIRECTION ( 'NONE',  ( -0.9999999999999997780, 1.340566441529999910E-09, -2.196397022486999685E-08 ) ) ;
#1640 = LINE ( 'NONE', #12475, #26186 ) ;
#1641 = VERTEX_POINT ( 'NONE', #10250 ) ;
#1642 = CARTESIAN_POINT ( 'NONE',  ( 7.000002934099999408, 1.243449787579999883E-13, -12.49999584805017250 ) ) ;
#1643 = CARTESIAN_POINT ( 'NONE',  ( 12.60065541204594908, -3.091968277195503489, -13.52988132686527756 ) ) ;
#1644 = AXIS2_PLACEMENT_3D ( 'NONE', #1722, #44391, #17814 ) ;
#1645 = CARTESIAN_POINT ( 'NONE',  ( 9.927263540183332680, -4.629523725463626782, 6.407767014557179230 ) ) ;
#1646 = CARTESIAN_POINT ( 'NONE',  ( 18.27990737420073586, -0.1887961029072405539, 12.59999260960568535 ) ) ;
#1647 = ORIENTED_EDGE ( 'NONE', *, *, #46056, .F. ) ;
#1648 = PLANE ( 'NONE',  #5957 ) ;
#1649 = CARTESIAN_POINT ( 'NONE',  ( 10.83351354018309820, 2.750000000000000000, -7.336375382625529795 ) ) ;
#1650 = CARTESIAN_POINT ( 'NONE',  ( 8.087797165043788539, 2.143741258173240460, -7.557751568339210024 ) ) ;
#1651 = CARTESIAN_POINT ( 'NONE',  ( 5.000030787343000327, 1.679270695423619619, 1.290525307673962674 ) ) ;
#1652 = CARTESIAN_POINT ( 'NONE',  ( 25.59997125372800042, -2.856414944279999979, 11.13959160109000024 ) ) ;
#1653 = CARTESIAN_POINT ( 'NONE',  ( 10.37581074856900187, 2.827416853083249748, 6.999756549658378901 ) ) ;
#1654 = EDGE_CURVE ( 'NONE', #56837, #65371, #36476, .T. ) ;
#1656 = EDGE_CURVE ( 'NONE', #4626, #15819, #9908, .T. ) ;
#1655 = CARTESIAN_POINT ( 'NONE',  ( 17.67525416028805552, -1.770698066894643041, 12.47496018400917173 ) ) ;
#1657 = ORIENTED_EDGE ( 'NONE', *, *, #17610, .F. ) ;
#1658 = CARTESIAN_POINT ( 'NONE',  ( 11.17901463001529905, -3.302889347096799710, -6.383488688482000128 ) ) ;
#1659 = ORIENTED_EDGE ( 'NONE', *, *, #37399, .T. ) ;
#1660 = AXIS2_PLACEMENT_3D ( 'NONE', #51724, #24478, #3819 ) ;
#1661 = CARTESIAN_POINT ( 'NONE',  ( 11.80877518040099972, -12.11591042788000117, -2.033719807695000270 ) ) ;
#1662 = CARTESIAN_POINT ( 'NONE',  ( 9.643864158774000828, 2.927176851028000293, -5.932007155957999878 ) ) ;
#1663 = CARTESIAN_POINT ( 'NONE',  ( 3.341497993174000314, 3.378630897718999826, -0.07134658118214000366 ) ) ;
#1664 = CARTESIAN_POINT ( 'NONE',  ( 10.85290698989999925, -3.170384785323999921, -8.782188229854000383 ) ) ;
#1665 = CARTESIAN_POINT ( 'NONE',  ( 6.691040091391770694, -0.7154887884274937493, -1.338493503189307487 ) ) ;
#1666 = PRODUCT_DEFINITION_FORMATION_WITH_SPECIFIED_SOURCE ( 'ANY', '', #8728, .NOT_KNOWN. ) ;
#1667 = CARTESIAN_POINT ( 'NONE',  ( 24.51038902278400045, 12.36384862481999924, 3.075095933055000064 ) ) ;
#1668 = CARTESIAN_POINT ( 'NONE',  ( 11.36486084871759950, 2.792989229543000107, 7.174999999999999822 ) ) ;
#1669 = ORIENTED_EDGE ( 'NONE', *, *, #30622, .T. ) ;
#1670 = CARTESIAN_POINT ( 'NONE',  ( 1.954534975661666785, 1.236092914997090064, -3.291825510064176896 ) ) ;
#1671 = CARTESIAN_POINT ( 'NONE',  ( 11.02641638348499953, -4.974961480482700260, 7.737488872214999702 ) ) ;
#1672 = CARTESIAN_POINT ( 'NONE',  ( 10.71256887705999894, 5.951815279772000089, 7.233043586354999555 ) ) ;
#1673 = CARTESIAN_POINT ( 'NONE',  ( 18.50003594167399967, -2.686563651857999613, -11.33603604486000016 ) ) ;
#1674 = EDGE_CURVE ( 'NONE', #28639, #10089, #68734, .T. ) ;
#1675 = CARTESIAN_POINT ( 'NONE',  ( 12.09999999999999964, -4.000000000000000000, 7.500000000000000000 ) ) ;
#1676 = CARTESIAN_POINT ( 'NONE',  ( 9.180263857702785302, 2.858372283262407887, 8.226552109004314772 ) ) ;
#1677 = CARTESIAN_POINT ( 'NONE',  ( 10.70287750876920008, 3.530799696887600092, -8.228113772635300194 ) ) ;
#1678 = CARTESIAN_POINT ( 'NONE',  ( 11.01895424672824397, 5.424779607850673813, 7.028465765783779240 ) ) ;
#1679 = CARTESIAN_POINT ( 'NONE',  ( 9.277088727410998104, 2.862182806015999947, -7.595427884080399927 ) ) ;
#1680 = CARTESIAN_POINT ( 'NONE',  ( 24.38582845604300076, -8.886027874258999759, -8.989742048622000326 ) ) ;
#1681 = CARTESIAN_POINT ( 'NONE',  ( 23.73390405283800320, -9.844988621918998817, 9.786411380388001291 ) ) ;
#1682 = CARTESIAN_POINT ( 'NONE',  ( 24.53429011008099891, 3.614318944477000084, -12.31267538233000103 ) ) ;
#1683 = VERTEX_POINT ( 'NONE', #31586 ) ;
#1684 = CARTESIAN_POINT ( 'NONE',  ( 7.886566940378000545, -3.084082018960999871, 9.259837032825000591 ) ) ;
#1685 = CARTESIAN_POINT ( 'NONE',  ( 9.754318513071000396, -2.462132291381999849, -7.373611177161000008 ) ) ;
#1686 = CARTESIAN_POINT ( 'NONE',  ( 17.81289281796187751, 1.835117743393749334, 13.87920855489149297 ) ) ;
#1687 = CARTESIAN_POINT ( 'NONE',  ( 23.56666365135700403, -2.920993777334001340, 11.72568747145000145 ) ) ;
#1688 = CARTESIAN_POINT ( 'NONE',  ( 10.73964560330029983, -3.608363763633400279, -6.283473206644000442 ) ) ;
#1689 = ORIENTED_EDGE ( 'NONE', *, *, #47994, .F. ) ;
#1690 = CARTESIAN_POINT ( 'NONE',  ( 10.58580560302255336, -5.314991280552569641, -7.853445763305400007 ) ) ;
#1691 = CARTESIAN_POINT ( 'NONE',  ( 7.282482780409000434, 3.448180532882000104, 9.222462917385000125 ) ) ;
#1693 = CARTESIAN_POINT ( 'NONE',  ( 11.30367835872029936, 2.886444435522000251, 8.201822467543799178 ) ) ;
#1692 = CARTESIAN_POINT ( 'NONE',  ( 8.895035841232999729, 5.751585344281000545, -8.235867044345999588 ) ) ;
#1694 = LINE ( 'NONE', #40142, #5609 ) ;
#1695 = ORIENTED_EDGE ( 'NONE', *, *, #30611, .F. ) ;
#1696 = DIRECTION ( 'NONE',  ( 0.000000000000000000, 0.000000000000000000, -1.000000000000000000 ) ) ;
#1697 = CARTESIAN_POINT ( 'NONE',  ( 18.25518009351767645, -2.707823354518777759, -13.73564093574334422 ) ) ;
#1698 = CARTESIAN_POINT ( 'NONE',  ( 10.94487616594229884, 3.696562859151900415, 8.456491899811199531 ) ) ;
#1699 = EDGE_CURVE ( 'NONE', #35262, #29277, #52901, .T. ) ;
#1700 = CARTESIAN_POINT ( 'NONE',  ( 11.09424907396999949, -2.431867116603999790, 7.769513708858000633 ) ) ;
#1701 = CARTESIAN_POINT ( 'NONE',  ( 7.832795987768000678, 2.851255020980998811, 6.795938453665997692 ) ) ;
#1702 = EDGE_LOOP ( 'NONE', ( #43272, #25436, #49295, #17211 ) ) ;
#1703 = CARTESIAN_POINT ( 'NONE',  ( 24.36809152945900081, 12.06003563633000120, -3.271087558346000179 ) ) ;
#1705 = CARTESIAN_POINT ( 'NONE',  ( 10.09249435321000021, -2.841617206345000035, -8.724656239052000828 ) ) ;
#1704 = CARTESIAN_POINT ( 'NONE',  ( 12.13343030045100157, -11.60886806805999960, 4.031065632098000506 ) ) ;
#1706 = CARTESIAN_POINT ( 'NONE',  ( 8.093175425641877752, -4.412936408959972745, 5.810561453377049546 ) ) ;
#1707 = AXIS2_PLACEMENT_3D ( 'NONE', #13473, #45284, #49829 ) ;
#1708 = CARTESIAN_POINT ( 'NONE',  ( 24.60115016793161757, 12.20856116708383965, 3.061105478265555568 ) ) ;
#1709 = CARTESIAN_POINT ( 'NONE',  ( -15.86200481174999943, 5.599999999999999645, 6.571291218949999902 ) ) ;
#1710 = CARTESIAN_POINT ( 'NONE',  ( 9.324126402770998467, -3.060189502158800146, 7.854398824525599565 ) ) ;
#1711 = ORIENTED_EDGE ( 'NONE', *, *, #29031, .F. ) ;
#1712 = CARTESIAN_POINT ( 'NONE',  ( 24.11212158815197526, -9.194244891325380920, 9.158718484554565720 ) ) ;
#1713 = CARTESIAN_POINT ( 'NONE',  ( 11.02226222744799955, -4.880489021643899861, 6.774721295617600170 ) ) ;
#1714 = ORIENTED_EDGE ( 'NONE', *, *, #11784, .T. ) ;
#1715 = CARTESIAN_POINT ( 'NONE',  ( 17.92207321737432579, 3.154877352444517058, 13.63994794764266238 ) ) ;
#1716 = VERTEX_POINT ( 'NONE', #14133 ) ;
#1717 = CARTESIAN_POINT ( 'NONE',  ( 9.889535841229999846, 5.798263352390999437, -8.113145944980999502 ) ) ;
#1718 = CARTESIAN_POINT ( 'NONE',  ( 24.15441789255899963, 12.81544408666000123, -3.249376310703999682 ) ) ;
#1719 = CARTESIAN_POINT ( 'NONE',  ( 12.75668783919146954, 3.198551280946738018, -12.18725874734144021 ) ) ;
#1720 = CARTESIAN_POINT ( 'NONE',  ( 11.14902344389989963, -4.883530143601199747, 8.036199780531900316 ) ) ;
#1721 =( BOUNDED_SURFACE ( )  B_SPLINE_SURFACE ( 3, 3, ( 
 ( #15410, #32518, #53151, #43000, #4903, #48245, #43358, #63632, #22011 ),
 ( #1050, #47572, #9, #16081, #53834, #5931, #27273, #64659, #16763 ),
 ( #37413, #63280, #32862, #32182, #54175, #6273, #27614, #53497, #36736 ),
 ( #58734, #349, #68877, #20994, #42330, #15749, #60122, #45084, #23051 ) ),
 .UNSPECIFIED., .F., .F., .T. ) 
 B_SPLINE_SURFACE_WITH_KNOTS ( ( 4, 4 ),
 ( 4, 1, 1, 1, 1, 1, 4 ),
 ( 0.000000000000000000, 1.000000000000000000 ),
 ( -0.004644144098274999473, 0.000000000000000000, 0.03269534097185999855, 0.06255479614191999937, 0.08986301827557000022, 0.1148786485006000058, 0.1342276000085000087 ),
 .UNSPECIFIED. ) 
 GEOMETRIC_REPRESENTATION_ITEM ( )  RATIONAL_B_SPLINE_SURFACE ( (
 ( 1.157365337832999996, 1.157365337832999996, 1.157365337832999996, 1.157365337832999996, 1.157365337832999996, 1.157365337832999996, 1.157365337832999996, 1.157365337832999996, 1.157365337832999996),
 ( 0.9475448873890999213, 0.9475448873890999213, 0.9475448873890999213, 0.9475448873890999213, 0.9475448873890999213, 0.9475448873890999213, 0.9475448873890999213, 0.9475448873890999213, 0.9475448873890999213),
 ( 0.9475448873890999213, 0.9475448873890999213, 0.9475448873890999213, 0.9475448873890999213, 0.9475448873890999213, 0.9475448873890999213, 0.9475448873890999213, 0.9475448873890999213, 0.9475448873890999213),
 ( 1.157365337832999996, 1.157365337832999996, 1.157365337832999996, 1.157365337832999996, 1.157365337832999996, 1.157365337832999996, 1.157365337832999996, 1.157365337832999996, 1.157365337832999996) ) ) 
 REPRESENTATION_ITEM ( '' )  SURFACE ( )  );
#1722 = CARTESIAN_POINT ( 'NONE',  ( 11.09999965054999826, -3.730349362740999292E-14, -9.259260025373999922E-14 ) ) ;
#1723 = ORIENTED_EDGE ( 'NONE', *, *, #16134, .F. ) ;
#1724 = CARTESIAN_POINT ( 'NONE',  ( 27.64127793187000037, -2.399999999999999911, -6.571291218949999902 ) ) ;
#1725 = DIRECTION ( 'NONE',  ( -0.000000000000000000, 0.4815106998111243208, 0.8764402124317445253 ) ) ;
#1726 = ORIENTED_EDGE ( 'NONE', *, *, #31675, .F. ) ;
#1727 = CARTESIAN_POINT ( 'NONE',  ( 12.58710648703388912, -3.166459836794174088, -12.19563591444343054 ) ) ;
#1729 = CARTESIAN_POINT ( 'NONE',  ( 11.16225954179439839, 4.877394611789299894, 6.770980925167799036 ) ) ;
#1728 = AXIS2_PLACEMENT_3D ( 'NONE', #29476, #67188, #24555 ) ;
#1730 = CARTESIAN_POINT ( 'NONE',  ( 11.06205805961999999, -2.154403720901000518, -7.605897512385999981 ) ) ;
#1731 = CARTESIAN_POINT ( 'NONE',  ( 10.95203274796000059, 2.845888289962000162, -5.182718820692000961 ) ) ;
#1732 = CARTESIAN_POINT ( 'NONE',  ( 18.35381692023100086, -11.68079677495000013, 4.101394359672999812 ) ) ;
#1733 = DIRECTION ( 'NONE',  ( 1.000000000000000000, 0.000000000000000000, 0.000000000000000000 ) ) ;
#1734 = CARTESIAN_POINT ( 'NONE',  ( 12.76344776297779227, -3.123961325724114779, -13.52107359494106475 ) ) ;
#1735 = CARTESIAN_POINT ( 'NONE',  ( 18.15003166281171332, 0.1916424759571789538, -12.69805926625132919 ) ) ;
#1736 = PLANE ( 'NONE',  #51995 ) ;
#1737 = CARTESIAN_POINT ( 'NONE',  ( 10.30072469555899950, -3.429147315060100176, -6.512367818249299667 ) ) ;
#1738 = EDGE_CURVE ( 'NONE', #38790, #21989, #49551, .T. ) ;
#1740 = EDGE_CURVE ( 'NONE', #11416, #1441, #13785, .T. ) ;
#1739 = CARTESIAN_POINT ( 'NONE',  ( 7.930392219590000735, 3.164805384346000228, 9.104735843897000080 ) ) ;
#1741 = ORIENTED_EDGE ( 'NONE', *, *, #35469, .F. ) ;
#1742 = CARTESIAN_POINT ( 'NONE',  ( 23.60205915885299888, -11.56239291744999065, 3.974820703413998846 ) ) ;
#1743 = CARTESIAN_POINT ( 'NONE',  ( 7.139655177822382015, 3.361094247794269574, 8.696675791344738116 ) ) ;
#1744 = DIRECTION ( 'NONE',  ( -1.000000000000000000, 7.105427357347999651E-14, -1.243449787536000124E-13 ) ) ;
#1745 = CARTESIAN_POINT ( 'NONE',  ( 23.74333388532700084, -3.207902546252999976, 13.21027681470999937 ) ) ;
#1746 = CARTESIAN_POINT ( 'NONE',  ( 17.78706641053893378, 1.919568985577240872, 12.56801103569107703 ) ) ;
#1747 = B_SPLINE_CURVE_WITH_KNOTS ( 'NONE', 3,
 ( #45743, #46770, #56573, #68073, #51662, #20190, #14948, #8677, #30024, #5490, #15296, #21224, #5140, #64548, #246, #52350, #42897, #63861 ),
 .UNSPECIFIED., .F., .F.,
 ( 4, 2, 2, 2, 2, 2, 2, 2, 4 ),
 ( 0.000000000000000000, 0.1250000000000000278, 0.2500000000000000555, 0.3749999999999999445, 0.4999999999999999445, 0.6249999999999998890, 0.7499999999999998890, 0.8750000000000000000, 1.000000000000000000 ),
 .UNSPECIFIED. ) ;
#1748 = LINE ( 'NONE', #49993, #6009 ) ;
#1749 = CARTESIAN_POINT ( 'NONE',  ( 9.409314688805999083, 2.634692233435000031, 8.920311306029999443 ) ) ;
#1750 = CARTESIAN_POINT ( 'NONE',  ( 10.80371347217102773, -3.410708369063951029, 6.869346568680468224 ) ) ;
#1751 = CARTESIAN_POINT ( 'NONE',  ( 2.175038703101999982, 1.745712609554999961, -2.581970805235000110 ) ) ;
#1752 = ORIENTED_EDGE ( 'NONE', *, *, #5266, .T. ) ;
#1753 = CARTESIAN_POINT ( 'NONE',  ( 12.13935791461259583, -2.765884558748030742, 12.29268093925658079 ) ) ;
#1754 = CARTESIAN_POINT ( 'NONE',  ( 9.353076168957999315, -4.579425901182000658, -8.483869947211399420 ) ) ;
#1755 = CARTESIAN_POINT ( 'NONE',  ( 24.60320129348500018, -3.644628662557000354, -12.27776523668999786 ) ) ;
#1756 = ADVANCED_FACE ( 'NONE', ( #59868 ), #10064, .T. ) ;
#1757 = CARTESIAN_POINT ( 'NONE',  ( 9.323602683899247623, 2.780955253993290022, 7.819247029363189050 ) ) ;
#1758 = CIRCLE ( 'NONE', #38577, 6.772075922005999615 ) ;
#1759 = B_SPLINE_SURFACE_WITH_KNOTS ( 'NONE', 3, 3, ( 
 ( #46830, #36334, #57649, #20946, #35315, #31103, #8736, #51381, #35657, #3480, #40892, #56971, #30410, #51722, #3817, #25154, #67793, #19914, #10443 ),
 ( #6226, #32134, #69172, #11472, #1335, #27566, #53787, #38046, #33160, #49228, #22310, #32472, #54477, #21620, #54127, #48894, #17062, #26884, #21282 ),
 ( #5883, #43303, #999, #64610, #32812, #37363, #59034, #42955, #43651, #38394, #37708, #63582, #64947, #48199, #26539, #37028, #16378, #59719, #31783 ),
 ( #11819, #58340, #6578, #16033, #27918, #27222, #42279, #11137, #53447, #48547, #15697, #63922, #301, #651, #53101, #5199, #47865, #42612, #21964 ) ),
 .UNSPECIFIED., .F., .F., .F.,
 ( 4, 4 ),
 ( 4, 1, 1, 1, 1, 1, 1, 1, 1, 1, 1, 1, 1, 1, 1, 1, 4 ),
 ( 0.1425182627899000132, 1.026369452518000047 ),
 ( 0.6640607743075999103, 0.6854686661408999626, 0.7068765579742000149, 0.7282844498075999873, 0.7496923416409000396, 0.7711002334743000119, 0.7925081253075999532, 0.8139160171409000055, 0.8353239089742999779, 0.8567318008076000302, 0.8781396926410000026, 0.8995475844743000549, 0.9209554763077000272, 0.9423633681409999685, 0.9637712599743000208, 0.9851791518076999932, 1.006587043640999823 ),
 .UNSPECIFIED. ) ;
#1760 = EDGE_CURVE ( 'NONE', #63538, #8271, #19600, .T. ) ;
#1761 = CARTESIAN_POINT ( 'NONE',  ( 11.15810538575740019, 5.242981041160000188, -7.202822423614300362 ) ) ;
#1762 = ORIENTED_EDGE ( 'NONE', *, *, #66570, .T. ) ;
#1763 = CARTESIAN_POINT ( 'NONE',  ( 12.16000645811907255, -0.3284204639250598023, 12.59572022474404562 ) ) ;
#1764 = VECTOR ( 'NONE', #32559, 1000.000000000000000 ) ;
#1765 = CARTESIAN_POINT ( 'NONE',  ( 8.047385841228999581, 4.468366666325000125, 8.882140983065999862 ) ) ;
#1766 = CARTESIAN_POINT ( 'NONE',  ( 9.305881816721999655, 4.945299866898000829, 9.077891794505999812 ) ) ;
#1767 = CARTESIAN_POINT ( 'NONE',  ( 12.27327344217065175, 2.829024202110181907, 12.36880877243790700 ) ) ;
#1768 = ORIENTED_EDGE ( 'NONE', *, *, #64540, .F. ) ;
#1769 = CARTESIAN_POINT ( 'NONE',  ( 9.345514158774999913, 5.775964236216999836, -8.174909295649001706 ) ) ;
#1770 = CARTESIAN_POINT ( 'NONE',  ( 10.39503166480599994, 2.725152142215999884, -7.589885038193400213 ) ) ;
#1771 = DIRECTION ( 'NONE',  ( 0.000000000000000000, 0.000000000000000000, -1.000000000000000000 ) ) ;
#1773 = CARTESIAN_POINT ( 'NONE',  ( 10.39393020684999946, 2.750000000000000000, -7.500000000000000000 ) ) ;
#1772 = CARTESIAN_POINT ( 'NONE',  ( 7.621422090919002912, 4.588776658069999570, 6.481258258681996232 ) ) ;
#1774 = CARTESIAN_POINT ( 'NONE',  ( 9.579430433046999482, -4.737822807309499673, 7.955330044604899342 ) ) ;
#1775 = CARTESIAN_POINT ( 'NONE',  ( 11.21979841651039855, -4.304975143798100312, -8.310733465454200442 ) ) ;
#1776 = ORIENTED_EDGE ( 'NONE', *, *, #618, .T. ) ;
#1777 = CIRCLE ( 'NONE', #55376, 12.79999953825000070 ) ;
#1778 = CARTESIAN_POINT ( 'NONE',  ( 1.925339139801000021, 1.756325177964999984, 2.941112093452000309 ) ) ;
#1779 = CARTESIAN_POINT ( 'NONE',  ( 24.30001682246400208, -8.938702682732001747, -8.938676171235998780 ) ) ;
#1780 = VECTOR ( 'NONE', #63109, 1000.000000000000000 ) ;
#1781 = CARTESIAN_POINT ( 'NONE',  ( 12.79999998712400178, -11.53033693765999779, 4.891431908114999949 ) ) ;
#1782 = CARTESIAN_POINT ( 'NONE',  ( 17.92356899887492006, 1.853474162671549852, -12.46298541230188128 ) ) ;
#1783 = CARTESIAN_POINT ( 'NONE',  ( 16.86666666253433533, 3.351256455363717190, 11.15757949424526352 ) ) ;
#1784 = CARTESIAN_POINT ( 'NONE',  ( 12.78422499708368321, -3.124999410541265732, 13.52084427634422603 ) ) ;
#1785 = CARTESIAN_POINT ( 'NONE',  ( 11.04471440339000132, 2.754763222384000176, 5.184237568466999235 ) ) ;
#1786 = LINE ( 'NONE', #50719, #5342 ) ;
#1787 = CARTESIAN_POINT ( 'NONE',  ( 13.73682146000800053, -12.29517900649999973, -2.580790095973999776 ) ) ;
#1788 = EDGE_LOOP ( 'NONE', ( #20717, #67196, #12483, #48430, #46677, #49089, #64017, #27105, #14391, #50804, #27207, #17189, #26426, #33045, #29344, #30815, #67646, #42917, #24260, #20176, #39518, #17278, #7910, #28187, #35313, #8859 ) ) ;
#1789 = CARTESIAN_POINT ( 'NONE',  ( 7.614999999996999946, 5.349999999999999645, -7.500000000000000000 ) ) ;
#1790 = CARTESIAN_POINT ( 'NONE',  ( 9.643930206848999376, 5.250000000000000000, -7.500000000000000000 ) ) ;
#1791 = CARTESIAN_POINT ( 'NONE',  ( 11.25158531382729876, -3.727547057523674212, -6.249999999999998224 ) ) ;
#1792 = CARTESIAN_POINT ( 'NONE',  ( 9.721802827886399712, 2.874603711570469677, 6.749639981088244589 ) ) ;
#1793 = CARTESIAN_POINT ( 'NONE',  ( 1.609748578980999989, 1.927138280259999892, 3.227152792068999965 ) ) ;
#1794 = ORIENTED_EDGE ( 'NONE', *, *, #42391, .F. ) ;
#1795 = CARTESIAN_POINT ( 'NONE',  ( 10.76087777166980075, 3.646736399438096132, -8.814656132371421648 ) ) ;
#1796 = DIRECTION ( 'NONE',  ( 0.8987684456439055669, 0.000000000000000000, 0.4384236320214022764 ) ) ;
#1797 = CARTESIAN_POINT ( 'NONE',  ( 10.62793268324000096, 3.100586971929999880, 8.599896650316999569 ) ) ;
#1798 = CARTESIAN_POINT ( 'NONE',  ( 11.07210672858429845, 3.307795442047700263, 8.020722037455799480 ) ) ;
#1799 = EDGE_CURVE ( 'NONE', #57590, #42732, #8805, .T. ) ;
#1800 = ADVANCED_FACE ( 'NONE', ( #14738 ), #53780, .T. ) ;
#1801 = CARTESIAN_POINT ( 'NONE',  ( 7.115095033390245405, 5.350161709276040511, -7.499994210608702083 ) ) ;
#1802 = CARTESIAN_POINT ( 'NONE',  ( 11.01605564679000082, -5.482859940357000639, -7.846409404949000077 ) ) ;
#1803 = CARTESIAN_POINT ( 'NONE',  ( 11.29998658800000122, 3.824194713071000340, -11.71675648045999907 ) ) ;
#1804 = CARTESIAN_POINT ( 'NONE',  ( 12.48079089692552479, -10.80976533111302729, 4.345114765590690986 ) ) ;
#1805 = CARTESIAN_POINT ( 'NONE',  ( 12.54534433730547782, -3.068834427903050610, 12.30067458026101157 ) ) ;
#1806 = ORIENTED_EDGE ( 'NONE', *, *, #5814, .T. ) ;
#1807 = CARTESIAN_POINT ( 'NONE',  ( 9.392285841233000809, 5.775964236216999836, -8.174909295649001706 ) ) ;
#1808 = VERTEX_POINT ( 'NONE', #19640 ) ;
#1809 = CARTESIAN_POINT ( 'NONE',  ( 17.81506173200510190, -3.068442049787682979, 13.53632421860061008 ) ) ;
#1810 = CYLINDRICAL_SURFACE ( 'NONE', #28570, 1.050000000000000044 ) ;
#1811 = EDGE_LOOP ( 'NONE', ( #40604, #36803, #47897, #42745, #14625 ) ) ;
#1812 = CARTESIAN_POINT ( 'NONE',  ( 11.48011496860029901, 4.919769165942200040, 7.971338736265699332 ) ) ;
#1813 = CARTESIAN_POINT ( 'NONE',  ( 6.600895253773083837, 1.094225353004803170, 0.2934724196684175279 ) ) ;
#1814 = LINE ( 'NONE', #8440, #31130 ) ;
#1815 = VECTOR ( 'NONE', #20909, 1000.000000000000000 ) ;
#1816 = CARTESIAN_POINT ( 'NONE',  ( 10.77462860031000069, 5.575476001419000127, 8.682676628339999425 ) ) ;
#1817 = CARTESIAN_POINT ( 'NONE',  ( 12.70934146430499290, -1.792598170651241052, -13.88476440023862324 ) ) ;
#1818 = CARTESIAN_POINT ( 'NONE',  ( 10.72726354018266548, -3.370476274536371442, 8.592232985442818105 ) ) ;
#1819 = CARTESIAN_POINT ( 'NONE',  ( 17.78803358707871851, 0.6812425322175482689, -12.58157083403807341 ) ) ;
#1820 = CARTESIAN_POINT ( 'NONE',  ( 10.58996262057999971, -2.876743158681999812, -6.236533224899999617 ) ) ;
#1821 = CARTESIAN_POINT ( 'NONE',  ( 11.66287348028854964, -4.761955701524100526, -7.911973420841600380 ) ) ;
#1822 = EDGE_CURVE ( 'NONE', #61003, #58602, #36057, .T. ) ;
#1823 = EDGE_CURVE ( 'NONE', #15006, #18158, #54635, .T. ) ;
#1824 = ORIENTED_EDGE ( 'NONE', *, *, #13802, .T. ) ;
#1825 = B_SPLINE_CURVE_WITH_KNOTS ( 'NONE', 3,
 ( #51317, #24748, #46073, #67379 ),
 .UNSPECIFIED., .F., .F.,
 ( 4, 4 ),
 ( 0.000000000000000000, 1.000000000000000000 ),
 .UNSPECIFIED. ) ;
#1826 = DIRECTION ( 'NONE',  ( 1.000000000000000000, 0.000000000000000000, 0.000000000000000000 ) ) ;
#1827 = EDGE_CURVE ( 'NONE', #35905, #30122, #41502, .T. ) ;
#1828 = EDGE_LOOP ( 'NONE', ( #1310, #33184, #16721, #22187 ) ) ;
#1829 = CARTESIAN_POINT ( 'NONE',  ( 10.79967784386921359, 3.012248194717311645, -4.853501387253247756 ) ) ;
#1830 = CARTESIAN_POINT ( 'NONE',  ( 10.42019978113000001, -4.954695572289999461, 4.899689062414000595 ) ) ;
#1831 = CARTESIAN_POINT ( 'NONE',  ( 25.02478208083906708, -8.536665412330339819, 8.299458527514417483 ) ) ;
#1832 = CARTESIAN_POINT ( 'NONE',  ( 10.16562143724499911, 4.849675135054999586, -6.543738240676099771 ) ) ;
#1833 = CARTESIAN_POINT ( 'NONE',  ( 12.23130451870204460, 2.748081639521271935, 13.61765624098743821 ) ) ;
#1834 = CARTESIAN_POINT ( 'NONE',  ( 10.25888544622000076, -4.512389816463000081, 5.993697694029000544 ) ) ;
#1835 = ORIENTED_EDGE ( 'NONE', *, *, #52244, .T. ) ;
#1836 = B_SPLINE_CURVE_WITH_KNOTS ( 'NONE', 3,
 ( #53669, #27444, #27801, #5761 ),
 .UNSPECIFIED., .F., .F.,
 ( 4, 4 ),
 ( 0.000000000000000000, 1.000000000000000000 ),
 .UNSPECIFIED. ) ;
#1837 = CARTESIAN_POINT ( 'NONE',  ( 23.89320776801300283, -8.283889223751996767, -7.778387372934005839 ) ) ;
#1838 = CARTESIAN_POINT ( 'NONE',  ( 12.08961512266909999, 0.1188263301541283151, 13.99950072926553446 ) ) ;
#1839 = VERTEX_POINT ( 'NONE', #27292 ) ;
#1840 = CARTESIAN_POINT ( 'NONE',  ( 7.430271682458000626, 3.037137096735000430, -6.379793420563999895 ) ) ;
#1841 = CARTESIAN_POINT ( 'NONE',  ( 17.60677072361600182, 12.04986663410999981, -3.196654394853999825 ) ) ;
#1842 = CARTESIAN_POINT ( 'NONE',  ( 23.61707933771300105, -2.917569334758999933, -13.53508108455999981 ) ) ;
#1843 = CARTESIAN_POINT ( 'NONE',  ( 5.171136683305999071, -0.5839666677625000579, 1.090217988517000025 ) ) ;
#1844 = B_SPLINE_CURVE_WITH_KNOTS ( 'NONE', 3,
 ( #61692, #56452, #8558, #29905, #16201, #31264 ),
 .UNSPECIFIED., .F., .F.,
 ( 4, 2, 4 ),
 ( 0.000000000000000000, 0.5000000000000000000, 1.000000000000000000 ),
 .UNSPECIFIED. ) ;
#1845 = EDGE_CURVE ( 'NONE', #23021, #64952, #17865, .T. ) ;
#1846 = CARTESIAN_POINT ( 'NONE',  ( 9.485829719593997567, 4.953415418491999844, -8.946479654552000227 ) ) ;
#1847 = CARTESIAN_POINT ( 'NONE',  ( 4.099967492754000631, -2.049969825927307809, -8.734266014444028751E-09 ) ) ;
#1848 = CARTESIAN_POINT ( 'NONE',  ( 10.90421209872000041, -3.863781031729999871, -9.185081053980001187 ) ) ;
#1849 = DIRECTION ( 'NONE',  ( 0.000000000000000000, -1.000000000000000000, 0.000000000000000000 ) ) ;
#1850 = CARTESIAN_POINT ( 'NONE',  ( 23.66004879239100234, 3.393653897912999984, 13.50507458845999942 ) ) ;
#1851 = CARTESIAN_POINT ( 'NONE',  ( 4.529188755291665203, -1.439555872821473681, 0.4868043516139976545 ) ) ;
#1852 = CARTESIAN_POINT ( 'NONE',  ( 9.614739029020999084, -5.020908168068000776, -6.342951604057000203 ) ) ;
#1853 = CARTESIAN_POINT ( 'NONE',  ( 11.34287482311539996, 4.803125295093300551, -7.824481664695199790 ) ) ;
#1854 = CARTESIAN_POINT ( 'NONE',  ( 1.105140132542249631, 0.9161175952574701631, 3.408904368339106927 ) ) ;
#1855 = CARTESIAN_POINT ( 'NONE',  ( 10.35814141025499957, 4.483492689244800822, -8.361148840840000318 ) ) ;
#1856 = CARTESIAN_POINT ( 'NONE',  ( 9.584000818238999742, 3.111278474435999808, -7.967991827203400490 ) ) ;
#1858 = CARTESIAN_POINT ( 'NONE',  ( 7.000000000000000000, -9.735955015381000166, -5.735955015381000166 ) ) ;
#1857 = CARTESIAN_POINT ( 'NONE',  ( 10.35563399569799969, -3.138280386550500012, 7.404358731173799946 ) ) ;
#1859 = CARTESIAN_POINT ( 'NONE',  ( 11.37309687351627296, -5.217465845835394411, 7.827184855449101697 ) ) ;
#1860 = ORIENTED_EDGE ( 'NONE', *, *, #13240, .F. ) ;
#1861 = VECTOR ( 'NONE', #37919, 1000.000000000000000 ) ;
#1862 = CARTESIAN_POINT ( 'NONE',  ( 11.47500581613029880, 4.988618570924500339, 6.865182626353099948 ) ) ;
#1863 = CIRCLE ( 'NONE', #3003, 1.500000000000001332 ) ;
#1864 = CARTESIAN_POINT ( 'NONE',  ( 10.15402496696000156, -5.267980706381999667, 5.992344456606999437 ) ) ;
#1865 = CARTESIAN_POINT ( 'NONE',  ( 9.733013376692998264, 2.982096917914000223, 8.017308190024898806 ) ) ;
#1866 = CARTESIAN_POINT ( 'NONE',  ( 9.480191603681626944, 4.150249255682260774, -6.638050216028796413 ) ) ;
#1867 = CARTESIAN_POINT ( 'NONE',  ( 9.447848023450999833, -5.447470167531999863, 7.431328114251999573 ) ) ;
#1868 = CIRCLE ( 'NONE', #42088, 1.549999999999999156 ) ;
#1869 = DIRECTION ( 'NONE',  ( 0.000000000000000000, 1.000000000000000000, 0.000000000000000000 ) ) ;
#1870 = CARTESIAN_POINT ( 'NONE',  ( 5.477523075960999854, -12.82224764859999766, -2.276049205301000189 ) ) ;
#1871 = VERTEX_POINT ( 'NONE', #31504 ) ;
#1872 = B_SPLINE_CURVE_WITH_KNOTS ( 'NONE', 3,
 ( #57319, #67460, #19585, #62227 ),
 .UNSPECIFIED., .F., .F.,
 ( 4, 4 ),
 ( 0.000000000000000000, 1.000000000000000000 ),
 .UNSPECIFIED. ) ;
#1873 = CARTESIAN_POINT ( 'NONE',  ( 8.672151519676999598, -3.978278301382419890, -8.504175633905001419 ) ) ;
#1874 = CIRCLE ( 'NONE', #65486, 2.725000000000000089 ) ;
#1875 = CARTESIAN_POINT ( 'NONE',  ( 8.792630737453640322, 5.083486636429016770, -6.186355545360274100 ) ) ;
#1876 = CARTESIAN_POINT ( 'NONE',  ( 5.095019251604999688, -0.7389799844016000652, 1.268943043503000023 ) ) ;
#1877 = CARTESIAN_POINT ( 'NONE',  ( 7.000000000000000000, 10.29642145254486785, -4.279174610942646950 ) ) ;
#1878 = CARTESIAN_POINT ( 'NONE',  ( 24.46225079000999969, -3.515716880278999756, 12.28737560831000053 ) ) ;
#1879 = ADVANCED_FACE ( 'NONE', ( #43376 ), #33736, .F. ) ;
#1880 = EDGE_CURVE ( 'NONE', #56864, #16266, #33714, .T. ) ;
#1881 = CARTESIAN_POINT ( 'NONE',  ( 11.57210672858429845, -4.692204557952299737, 8.020722037455799480 ) ) ;
#1882 = CARTESIAN_POINT ( 'NONE',  ( 10.53057053952199951, 3.659587858614300249, -6.703496287302799672 ) ) ;
#1883 = CARTESIAN_POINT ( 'NONE',  ( 5.700000000000000178, 0.000000000000000000, 0.000000000000000000 ) ) ;
#1884 = CARTESIAN_POINT ( 'NONE',  ( 24.56666016946500264, -8.743959839545999202, 8.863853254959998651 ) ) ;
#1885 = CARTESIAN_POINT ( 'NONE',  ( 10.70271159698171992, 5.100000000000000533, 6.305985889763628727 ) ) ;
#1886 = ORIENTED_EDGE ( 'NONE', *, *, #26542, .T. ) ;
#1887 = CARTESIAN_POINT ( 'NONE',  ( 17.55505043854143565, 3.248109929747637903, -13.61799478206225444 ) ) ;
#1888 = CARTESIAN_POINT ( 'NONE',  ( 12.08146951720330087, -0.04720351400547519866, -13.99992551180917211 ) ) ;
#1889 = CARTESIAN_POINT ( 'NONE',  ( 21.00000012402669824, 12.42499880353999941, 0.000000000000000000 ) ) ;
#1890 = CARTESIAN_POINT ( 'NONE',  ( 25.25797159228700295, -8.562781201510999196, -7.910473564811001168 ) ) ;
#1891 = CARTESIAN_POINT ( 'NONE',  ( 13.00000000001300116, -11.52577654661000039, -1.696746661728000038 ) ) ;
#1892 = DIRECTION ( 'NONE',  ( 0.000000000000000000, 0.000000000000000000, -1.000000000000000000 ) ) ;
#1893 = CARTESIAN_POINT ( 'NONE',  ( 13.26944243593800010, 12.10482456369999937, 2.110592202804000284 ) ) ;
#1894 = ORIENTED_EDGE ( 'NONE', *, *, #26066, .T. ) ;
#1895 = CARTESIAN_POINT ( 'NONE',  ( 23.56666365135700403, 9.069641144917994779, 7.556701426681005529 ) ) ;
#1896 = CARTESIAN_POINT ( 'NONE',  ( 17.79021264935886748, 3.209040350003987463, -13.62725621160039324 ) ) ;
#1897 = ORIENTED_EDGE ( 'NONE', *, *, #20825, .T. ) ;
#1898 = CARTESIAN_POINT ( 'NONE',  ( 24.67921430886200085, -8.727631620858000261, -9.158313288899000426 ) ) ;
#1899 = CARTESIAN_POINT ( 'NONE',  ( 24.99831752671624585, 8.543272426953288701, -8.328706555083702057 ) ) ;
#1900 = CARTESIAN_POINT ( 'NONE',  ( 8.216604719590000272, 5.331510020787000315, -8.114341808290998159 ) ) ;
#1901 = CARTESIAN_POINT ( 'NONE',  ( 9.114639751325487538, 5.184985712744429875, 7.040280035170889406 ) ) ;
#1902 = B_SPLINE_CURVE_WITH_KNOTS ( 'NONE', 3,
 ( #39343, #11723, #23602, #6134, #59973, #44261 ),
 .UNSPECIFIED., .F., .F.,
 ( 4, 1, 1, 4 ),
 ( 0.000000000000000000, 0.3333333333333000081, 0.6666666666667000474, 1.000000000000000000 ),
 .UNSPECIFIED. ) ;
#1903 = CARTESIAN_POINT ( 'NONE',  ( 11.59456039236534330, -2.685288321999000249, -7.563984187103470092 ) ) ;
#1904 = FACE_OUTER_BOUND ( 'NONE', #31398, .T. ) ;
#1905 = CARTESIAN_POINT ( 'NONE',  ( 10.14393020684900115, -2.750000000000000000, 7.500000000000000000 ) ) ;
#1906 = EDGE_LOOP ( 'NONE', ( #68804, #41397, #34788, #67548, #39477, #23973, #37921, #1572, #51184, #50832 ) ) ;
#1907 = CARTESIAN_POINT ( 'NONE',  ( 9.820206362952999868, -3.883324525498000224, 6.055606607331999847 ) ) ;
#1908 = DIRECTION ( 'NONE',  ( 1.000000000000000000, 0.000000000000000000, 0.000000000000000000 ) ) ;
#1909 = CARTESIAN_POINT ( 'NONE',  ( 18.08703349542470917, -2.171337119009642436, 13.73770667395803358 ) ) ;
#1910 = VERTEX_POINT ( 'NONE', #11537 ) ;
#1911 = CIRCLE ( 'NONE', #8592, 14.00000000000000000 ) ;
#1912 = CARTESIAN_POINT ( 'NONE',  ( 10.57793656291999973, 4.393379542724999531, -6.024362243994999311 ) ) ;
#1913 = SURFACE_SIDE_STYLE ('',( #29879 ) ) ;
#1914 = EDGE_CURVE ( 'NONE', #57987, #6055, #56083, .T. ) ;
#1915 = ORIENTED_EDGE ( 'NONE', *, *, #46236, .F. ) ;
#1916 = CARTESIAN_POINT ( 'NONE',  ( 9.102747021775998704, 3.245052836381700168, 6.837506920432799618 ) ) ;
#1917 = CARTESIAN_POINT ( 'NONE',  ( 18.14595306053284318, -2.897894011715727025, -12.26224306838060585 ) ) ;
#1918 = CARTESIAN_POINT ( 'NONE',  ( 9.099999931440999390, 5.246365646610000155, 7.595250590283559866 ) ) ;
#1919 = CARTESIAN_POINT ( 'NONE',  ( 24.53429015151300163, -3.614318902553999902, -12.31267542782000035 ) ) ;
#1920 = CARTESIAN_POINT ( 'NONE',  ( 24.35365242081699932, 1.906711579079999552, 11.36048031428999572 ) ) ;
#1921 = COLOUR_RGB ( '', 0.08235294, 0.09019608, 0.10196078) ;
#1922 = CARTESIAN_POINT ( 'NONE',  ( 9.206076168957999073, 3.560025096655699883, 6.752918994396699404 ) ) ;
#1923 = CARTESIAN_POINT ( 'NONE',  ( 9.456118062523774626, -2.255366135290077345, 7.362790452840693334 ) ) ;
#1924 = ORIENTED_EDGE ( 'NONE', *, *, #13803, .F. ) ;
#1925 = CARTESIAN_POINT ( 'NONE',  ( 10.52323372634000087, 3.325642821414999784, 5.689987891230000372 ) ) ;
#1926 = CARTESIAN_POINT ( 'NONE',  ( 11.03905471959000018, 3.855072614532999875, -9.179480010827999692 ) ) ;
#1927 = CARTESIAN_POINT ( 'NONE',  ( 12.80505043854143388, 3.124999999999999556, -13.52084414783465505 ) ) ;
#1928 = CIRCLE ( 'NONE', #20935, 2.750000000000000000 ) ;
#1929 = CARTESIAN_POINT ( 'NONE',  ( 12.19536857401206831, 2.360987227094834218, -13.70197821715308706 ) ) ;
#1930 = CARTESIAN_POINT ( 'NONE',  ( 17.33333333161133538, -3.595161661652010565, -11.99793472338498646 ) ) ;
#1931 = CARTESIAN_POINT ( 'NONE',  ( 24.37846962615400059, 3.167532807711999965, 12.03742776834999972 ) ) ;
#1932 = EDGE_CURVE ( 'NONE', #26882, #57519, #6915, .T. ) ;
#1933 = CARTESIAN_POINT ( 'NONE',  ( 17.98979471028674126, 0.4491394412341184750, 13.89023495843590439 ) ) ;
#1934 = CARTESIAN_POINT ( 'NONE',  ( 17.92176811213217036, 0.5062908249625720503, 13.88759084002720989 ) ) ;
#1935 = ORIENTED_EDGE ( 'NONE', *, *, #53847, .F. ) ;
#1936 = ORIENTED_EDGE ( 'NONE', *, *, #20827, .T. ) ;
#1937 = CIRCLE ( 'NONE', #20890, 10.75000000000000533 ) ;
#1938 = CARTESIAN_POINT ( 'NONE',  ( 9.088029719595001055, 2.881930053949999682, -8.823338183322999129 ) ) ;
#1939 = CARTESIAN_POINT ( 'NONE',  ( 6.999999691988000095, -12.11716380430000051, -3.069905306952999791 ) ) ;
#1940 = CARTESIAN_POINT ( 'NONE',  ( 10.55041772631200026, -3.450375740502100275, 6.368647051112000135 ) ) ;
#1941 = CARTESIAN_POINT ( 'NONE',  ( 10.06844525594999951, -4.148609764890999863, 8.941457795715999524 ) ) ;
#1942 = CARTESIAN_POINT ( 'NONE',  ( 23.66004879239100234, 3.393652551760000247, -13.50507492672999987 ) ) ;
#1943 = CARTESIAN_POINT ( 'NONE',  ( 8.192495559623999668, -2.550228841911000188, 7.666975032000999946 ) ) ;
#1944 = CARTESIAN_POINT ( 'NONE',  ( 12.09999999999999964, -4.000000000000000000, 7.500000000000000000 ) ) ;
#1946 = CARTESIAN_POINT ( 'NONE',  ( 12.80505043854143388, 2.499999999999999556, -25.00000000000000000 ) ) ;
#1945 = CARTESIAN_POINT ( 'NONE',  ( 8.725348536223823004, 2.649439212887079620, 7.500023728975156345 ) ) ;
#1947 = CARTESIAN_POINT ( 'NONE',  ( 9.264867054676999558, -5.097279491198996482, -6.598518734304002820 ) ) ;
#1948 = LINE ( 'NONE', #66253, #10161 ) ;
#1949 = CARTESIAN_POINT ( 'NONE',  ( 8.724265421554999733, 3.837285628664199866, -8.341695632489900092 ) ) ;
#1950 = CARTESIAN_POINT ( 'NONE',  ( 17.56537431432192164, 0.6249999662751106744, 12.67928921590351798 ) ) ;
#1951 = CARTESIAN_POINT ( 'NONE',  ( 11.09999999999999964, -5.489445176276809057, 6.853104147731436946 ) ) ;
#1952 = CARTESIAN_POINT ( 'NONE',  ( 18.06413707771143606, -2.862722769407199053, -12.35962335206856544 ) ) ;
#1953 = ORIENTED_EDGE ( 'NONE', *, *, #35446, .T. ) ;
#1955 = CARTESIAN_POINT ( 'NONE',  ( 12.08078742596668675, -2.670354628853650603, -12.31525682383281506 ) ) ;
#1954 = LINE ( 'NONE', #50195, #11797 ) ;
#1956 = CARTESIAN_POINT ( 'NONE',  ( 8.506095280410999493, 2.305580295895999665, -7.860904109308999743 ) ) ;
#1957 = B_SPLINE_CURVE_WITH_KNOTS ( 'NONE', 3,
 ( #15570, #36898, #45511, #49442 ),
 .UNSPECIFIED., .F., .F.,
 ( 4, 4 ),
 ( 0.000000000000000000, 1.000000000000000000 ),
 .UNSPECIFIED. ) ;
#1958 = CARTESIAN_POINT ( 'NONE',  ( 11.09999999999999964, 4.000000000000000000, -7.500000000000000000 ) ) ;
#1959 = CARTESIAN_POINT ( 'NONE',  ( 18.18005043799233178, 2.500000011518615395, -12.45159158845316405 ) ) ;
#1960 = FACE_OUTER_BOUND ( 'NONE', #9425, .T. ) ;
#1961 = CARTESIAN_POINT ( 'NONE',  ( 18.29995268966800026, -2.861739928647000220, -11.98821236628000086 ) ) ;
#1962 = CARTESIAN_POINT ( 'NONE',  ( 2.304427617675000040, 1.234641978838000087, 3.195386953671000008 ) ) ;
#1963 = VERTEX_POINT ( 'NONE', #42677 ) ;
#1964 = ADVANCED_FACE ( 'NONE', ( #22378 ), #22582, .T. ) ;
#1965 = EDGE_CURVE ( 'NONE', #26060, #24715, #65012, .T. ) ;
#1966 = CARTESIAN_POINT ( 'NONE',  ( 12.23004733766516949, -0.4382646521645954252, -12.59237917444261434 ) ) ;
#1967 = CARTESIAN_POINT ( 'NONE',  ( 12.63917144501162326, -1.891830949829975461, -12.57269938248998642 ) ) ;
#1968 = DIRECTION ( 'NONE',  ( 0.000000000000000000, -0.9466492601157000530, 0.3222656952305000266 ) ) ;
#1970 = CARTESIAN_POINT ( 'NONE',  ( 7.924357780410000274, 2.432118421226999949, 6.597517552098000060 ) ) ;
#1969 = VECTOR ( 'NONE', #19314, 1000.000000000000114 ) ;
#1971 = VERTEX_POINT ( 'NONE', #17131 ) ;
#1972 = CARTESIAN_POINT ( 'NONE',  ( 5.846035669131000034, -1.131660731475000015, -0.3201946116248999830 ) ) ;
#1973 = EDGE_CURVE ( 'NONE', #57705, #2412, #32110, .T. ) ;
#1974 = EDGE_CURVE ( 'NONE', #63863, #13607, #32628, .T. ) ;
#1975 = CARTESIAN_POINT ( 'NONE',  ( 7.440860841227999956, 3.609683333014999995, -6.158094852492999927 ) ) ;
#1977 = CARTESIAN_POINT ( 'NONE',  ( 7.851683310611999644, 4.710036428759999616, 6.351753055261999847 ) ) ;
#1976 = CARTESIAN_POINT ( 'NONE',  ( 11.09999999999999964, -4.000000000000000000, 7.500000000000000000 ) ) ;
#1978 = CARTESIAN_POINT ( 'NONE',  ( 10.59991360228957191, -4.849288934224095904, -7.293123446196289272 ) ) ;
#1979 = ORIENTED_EDGE ( 'NONE', *, *, #63681, .F. ) ;
#1980 = CARTESIAN_POINT ( 'NONE',  ( 8.227533346876342080, 4.737976145808172390, 6.141445531819171855 ) ) ;
#1981 = ORIENTED_EDGE ( 'NONE', *, *, #34379, .F. ) ;
#1982 = CARTESIAN_POINT ( 'NONE',  ( 9.487500104632182740, -4.950335429809691767, 8.458601829922910653 ) ) ;
#1983 = CARTESIAN_POINT ( 'NONE',  ( 24.30001680106099826, 12.21047197645999915, -3.271805488357999891 ) ) ;
#1984 = CARTESIAN_POINT ( 'NONE',  ( 17.94354858665103336, -0.4896942981276207196, -13.88839019180475809 ) ) ;
#1985 = ORIENTED_EDGE ( 'NONE', *, *, #955, .T. ) ;
#1986 = CARTESIAN_POINT ( 'NONE',  ( 10.97494570512294132, 8.502725158598858357, -6.546417107134506530 ) ) ;
#1987 = CARTESIAN_POINT ( 'NONE',  ( 8.316694475082000437, 2.898380349184999982, 6.611503672649000407 ) ) ;
#1988 = LINE ( 'NONE', #3350, #1364 ) ;
#1989 = CARTESIAN_POINT ( 'NONE',  ( 8.769549439917666334, -5.100000000000000533, 6.459823844766666490 ) ) ;
#1990 = CARTESIAN_POINT ( 'NONE',  ( 18.16257472060389233, -2.647071732840386549, 12.41611113220489138 ) ) ;
#1991 = ORIENTED_EDGE ( 'NONE', *, *, #5864, .T. ) ;
#1992 = CARTESIAN_POINT ( 'NONE',  ( 8.513426658773999733, 5.040787533781999841, 8.522957620707000359 ) ) ;
#1993 = CARTESIAN_POINT ( 'NONE',  ( 24.22085262432600317, -12.94683699972000035, -3.132093620313999960 ) ) ;
#1994 = FACE_OUTER_BOUND ( 'NONE', #41081, .T. ) ;
#1995 = DIRECTION ( 'NONE',  ( -0.5000000000000150990, 0.08222066253632250021, -0.8621135439442261239 ) ) ;
#1996 = ORIENTED_EDGE ( 'NONE', *, *, #50585, .F. ) ;
#1997 = CARTESIAN_POINT ( 'NONE',  ( 10.67500447327561908, -2.650284540010996004, 7.500001951671615430 ) ) ;
#1998 = CARTESIAN_POINT ( 'NONE',  ( -2.444943969992999916E-05, -2.899969545325999931, 0.000000000000000000 ) ) ;
#1999 = CARTESIAN_POINT ( 'NONE',  ( 7.491097165042828188, 3.407826859982625578, -9.260216617036411080 ) ) ;
#2000 = CARTESIAN_POINT ( 'NONE',  ( 7.204898016025000018, -0.2500000000000000000, 3.099950251719000072 ) ) ;
#2001 = CARTESIAN_POINT ( 'NONE',  ( 24.34832162669904321, 8.810502600456597833, 8.810502600456597833 ) ) ;
#2002 = CARTESIAN_POINT ( 'NONE',  ( 8.205992358813000820, 3.399999999999999911, 6.138278517057000450 ) ) ;
#2003 = AXIS2_PLACEMENT_3D ( 'NONE', #35024, #19268, #45510 ) ;
#2004 = CARTESIAN_POINT ( 'NONE',  ( 17.60337015074825828, -1.762344248314565931, 12.47614295832086206 ) ) ;
#2005 = VERTEX_POINT ( 'NONE', #26607 ) ;
#2006 = CARTESIAN_POINT ( 'NONE',  ( 11.44366954483529852, -3.514796851401900124, -6.751356298874699569 ) ) ;
#2007 = B_SPLINE_CURVE_WITH_KNOTS ( 'NONE', 3,
 ( #39401, #49889, #44661, #18079 ),
 .UNSPECIFIED., .F., .F.,
 ( 4, 4 ),
 ( 0.000000000000000000, 1.000000000000000000 ),
 .UNSPECIFIED. ) ;
#2008 = EDGE_LOOP ( 'NONE', ( #58991, #6494, #23721, #13922 ) ) ;
#2009 = CARTESIAN_POINT ( 'NONE',  ( 0.1499942179679999987, -2.750000000000000000, 0.000000000000000000 ) ) ;
#2010 = CARTESIAN_POINT ( 'NONE',  ( 8.766851002546001581, -2.832432432432000269, 6.822293592207000934 ) ) ;
#2011 = CARTESIAN_POINT ( 'NONE',  ( 2.622152980194000005, -0.2193973046792999926, -3.207556849382000141 ) ) ;
#2012 = CARTESIAN_POINT ( 'NONE',  ( 9.870877370727999534, -2.904359058094999835, -8.563874348197000330 ) ) ;
#2013 = ADVANCED_FACE ( 'NONE', ( #10856 ), #5603, .T. ) ;
#2014 = AXIS2_PLACEMENT_3D ( 'NONE', #36960, #10377, #32406 ) ;
#2015 = CARTESIAN_POINT ( 'NONE',  ( 10.72422653164066730, 2.899999999999999911, -6.304440313833583609 ) ) ;
#2016 = CARTESIAN_POINT ( 'NONE',  ( 0.1500001228197999914, -2.250000122783999856, 5.253497258719000289E-10 ) ) ;
#2017 = DIRECTION ( 'NONE',  ( -1.000000000000000000, 0.000000000000000000, 0.000000000000000000 ) ) ;
#2018 = ORIENTED_EDGE ( 'NONE', *, *, #830, .T. ) ;
#2019 = EDGE_CURVE ( 'NONE', #25814, #56658, #66265, .T. ) ;
#2020 = COLOUR_RGB ( '', 0.66274510, 0.83137255, 0.94901961) ;
#2021 = CARTESIAN_POINT ( 'NONE',  ( 10.26537527815838580, 5.100000000000000533, 6.445686799303629755 ) ) ;
#2022 = CARTESIAN_POINT ( 'NONE',  ( 10.83364828895399867, -3.239803852721999888, 7.084788038520800413 ) ) ;
#2023 = CARTESIAN_POINT ( 'NONE',  ( 9.786671076420999427, 2.381202181614999525, 7.612749448318000489 ) ) ;
#2024 = CARTESIAN_POINT ( 'NONE',  ( 10.82336322479176083, -2.820284244472506252, -8.179952785015981220 ) ) ;
#2025 = DIRECTION ( 'NONE',  ( 0.8660254001570034665, -4.588230081904017516E-12, -0.5000000062829018654 ) ) ;
#2026 = CARTESIAN_POINT ( 'NONE',  ( 11.08333333333437842, 2.470076941866840237, 7.228155005602348915 ) ) ;
#2027 = AXIS2_PLACEMENT_3D ( 'NONE', #65321, #17437, #66358 ) ;
#2028 = CARTESIAN_POINT ( 'NONE',  ( 11.11718313518939816, 3.377550038693600154, -8.287087605365499599 ) ) ;
#2029 = CARTESIAN_POINT ( 'NONE',  ( 10.52052890781999928, 2.899999999999999911, 6.152188490330000370 ) ) ;
#2030 = CARTESIAN_POINT ( 'NONE',  ( 9.657025935145998830, 3.834207658792500251, -6.370288821165999593 ) ) ;
#2031 = B_SPLINE_CURVE_WITH_KNOTS ( 'NONE', 3,
 ( #28093, #50111, #59898, #43487, #23532, #22837, #23188, #12006, #49067, #44183, #44534, #7107, #66178, #11310, #28444, #32647, #53959, #22488, #43831, #60595, #6062, #65482, #17606, #65130 ),
 .UNSPECIFIED., .F., .F.,
 ( 4, 2, 2, 2, 2, 2, 2, 2, 2, 2, 2, 4 ),
 ( 0.000000000000000000, 0.06250000000000027756, 0.1250000000000005551, 0.1875000000000008327, 0.2500000000000011102, 0.3750000000000009992, 0.5000000000000008882, 0.6250000000000007772, 0.7500000000000006661, 0.8750000000000005551, 0.9375000000000002220, 1.000000000000000000 ),
 .UNSPECIFIED. ) ;
#2032 = CARTESIAN_POINT ( 'NONE',  ( 23.74223885472600060, -9.839017400655999168, 9.383841620339000045 ) ) ;
#2033 = CARTESIAN_POINT ( 'NONE',  ( 8.130886538030239308, 4.885509777356301875, -6.278165256758011736 ) ) ;
#2034 = CARTESIAN_POINT ( 'NONE',  ( 11.35906500789999996, 2.719101288111000159, -7.157645240044000268 ) ) ;
#2035 = ORIENTED_EDGE ( 'NONE', *, *, #57349, .F. ) ;
#2036 = CARTESIAN_POINT ( 'NONE',  ( 7.346668146792000087, -2.374041291348000016, 8.293390875797999939 ) ) ;
#2037 = CARTESIAN_POINT ( 'NONE',  ( 10.09166489801000033, -4.565692099013000771, -8.879633571423999783 ) ) ;
#2038 = CARTESIAN_POINT ( 'NONE',  ( 18.07920178076626883, 2.013390639430577167, 13.85446980737596157 ) ) ;
#2039 = CARTESIAN_POINT ( 'NONE',  ( 15.90000000000314451, -3.738168175168965046, -11.41174933108808176 ) ) ;
#2040 = CARTESIAN_POINT ( 'NONE',  ( 10.83810672858429847, -5.021298157087000114, -6.731711997412900494 ) ) ;
#2041 = VERTEX_POINT ( 'NONE', #60140 ) ;
#2042 = CARTESIAN_POINT ( 'NONE',  ( 24.78226642313899930, 3.612166370762999623, -12.07973911291999869 ) ) ;
#2043 = CARTESIAN_POINT ( 'NONE',  ( 17.76385332268500150, 3.526697956045000026, 11.96114712952999959 ) ) ;
#2045 = CARTESIAN_POINT ( 'NONE',  ( 11.17901463001529905, 4.697110652903200290, 8.616511311517999872 ) ) ;
#2044 = CARTESIAN_POINT ( 'NONE',  ( 10.33744474310099903, -3.228742141949900279, -7.874284411628199365 ) ) ;
#2046 = DIRECTION ( 'NONE',  ( 0.000000000000000000, -1.000000000000000000, 0.000000000000000000 ) ) ;
#2047 = ORIENTED_EDGE ( 'NONE', *, *, #59211, .T. ) ;
#2048 = EDGE_CURVE ( 'NONE', #14563, #36985, #42657, .T. ) ;
#2049 = CARTESIAN_POINT ( 'NONE',  ( 11.09647882763000126, 3.099775370665000196, 6.097099813297999660 ) ) ;
#2050 = CARTESIAN_POINT ( 'NONE',  ( 25.27001783331474627, 3.169702853053691260, -11.48327890507672144 ) ) ;
#2051 = CARTESIAN_POINT ( 'NONE',  ( 11.33456651104149948, 4.112542507956200133, 8.635175889530000148 ) ) ;
#2052 = CARTESIAN_POINT ( 'NONE',  ( 9.555699158955999195, -2.440755924888999839, 6.680881588809999272 ) ) ;
#2053 = CARTESIAN_POINT ( 'NONE',  ( 8.016657426769000949, 2.906672751340000804, 6.403732826568004910 ) ) ;
#2054 = VERTEX_POINT ( 'NONE', #61175 ) ;
#2055 = CARTESIAN_POINT ( 'NONE',  ( 8.455992358796999397, 2.899999999999999911, -6.571291218954000257 ) ) ;
#2056 = ADVANCED_FACE ( 'NONE', ( #29033 ), #38009, .F. ) ;
#2057 = EDGE_CURVE ( 'NONE', #28231, #31293, #31531, .T. ) ;
#2058 = CARTESIAN_POINT ( 'NONE',  ( 10.22094314679000071, -2.563075248996000255, -8.004105227364998854 ) ) ;
#2059 = CARTESIAN_POINT ( 'NONE',  ( 8.059803797423384708, -3.670685108766681193, 5.791771361350072311 ) ) ;
#2060 = CARTESIAN_POINT ( 'NONE',  ( 10.77962878203999963, -2.397503436487000261, 7.755423856053000442 ) ) ;
#2061 = CARTESIAN_POINT ( 'NONE',  ( 11.07745841296999778, 5.274854172210999614, 5.088889326835999150 ) ) ;
#2062 = CARTESIAN_POINT ( 'NONE',  ( 9.879355082327998971, -4.511005581663400044, 8.521081653687000212 ) ) ;
#2063 = ORIENTED_EDGE ( 'NONE', *, *, #25484, .T. ) ;
#2064 = CARTESIAN_POINT ( 'NONE',  ( 23.59999172348799945, -10.30759808834999980, 9.317726582648999667 ) ) ;
#2065 = CARTESIAN_POINT ( 'NONE',  ( 11.41610672858429965, -4.911600290708499905, 8.185766014210599906 ) ) ;
#2066 = ORIENTED_EDGE ( 'NONE', *, *, #34743, .F. ) ;
#2067 = DIRECTION ( 'NONE',  ( 2.801582883299285241E-16, -0.3352635608502960163, 0.9421243786071880066 ) ) ;
#2068 = VERTEX_POINT ( 'NONE', #44069 ) ;
#2069 = CARTESIAN_POINT ( 'NONE',  ( 9.102795280413999990, 3.071719032003000116, -6.037263251225000182 ) ) ;
#2070 = AXIS2_PLACEMENT_3D ( 'NONE', #15851, #52921, #10265 ) ;
#2071 = CARTESIAN_POINT ( 'NONE',  ( 8.188938565157450000, -2.652235273545322070, 7.263344527950025942 ) ) ;
#2072 = CARTESIAN_POINT ( 'NONE',  ( 24.30000000000000071, 8.756202924575998026, 7.455126447192999883 ) ) ;
#2073 = CARTESIAN_POINT ( 'NONE',  ( 12.61213290433100553, 1.905496177770260591, -12.57041190218061288 ) ) ;
#2074 = CARTESIAN_POINT ( 'NONE',  ( 11.61718313518939993, -4.622449961306399402, 6.712912394634500401 ) ) ;
#2075 = CARTESIAN_POINT ( 'NONE',  ( 11.81389666366019853, -4.045876550911099656, 6.467512203247999913 ) ) ;
#2076 = ADVANCED_FACE ( 'NONE', ( #17491 ), #1385, .T. ) ;
#2077 = ORIENTED_EDGE ( 'NONE', *, *, #61893, .T. ) ;
#2078 = DIRECTION ( 'NONE',  ( 1.000000000000000000, 0.000000000000000000, 0.000000000000000000 ) ) ;
#2079 = VECTOR ( 'NONE', #48036, 1000.000000000000114 ) ;
#2080 = VERTEX_POINT ( 'NONE', #23072 ) ;
#2081 = CARTESIAN_POINT ( 'NONE',  ( 7.464688980125999684, -4.351670788182000038, 8.977200644264000218 ) ) ;
#2082 = CARTESIAN_POINT ( 'NONE',  ( 17.65273365043483977, -0.7301396911442770143, 13.98094760870049136 ) ) ;
#2083 = ORIENTED_EDGE ( 'NONE', *, *, #54861, .T. ) ;
#2084 = CARTESIAN_POINT ( 'NONE',  ( 12.25620353052270595, -2.010025970016508623, -12.43864443381842833 ) ) ;
#2085 = CARTESIAN_POINT ( 'NONE',  ( 10.76841504065829902, 4.914510326623699576, 8.181880472491098288 ) ) ;
#2086 = CARTESIAN_POINT ( 'NONE',  ( 10.56984555961999916, -2.152868447761999704, -7.425101130468999777 ) ) ;
#2087 = CARTESIAN_POINT ( 'NONE',  ( 13.99999999379500082, 8.815218614167999789, 7.616697584347000394 ) ) ;
#2088 = AXIS2_PLACEMENT_3D ( 'NONE', #24785, #24101, #40861 ) ;
#2089 = CARTESIAN_POINT ( 'NONE',  ( 17.57251690949600231, -11.38899788448000017, 4.574196188622000392 ) ) ;
#2090 = CARTESIAN_POINT ( 'NONE',  ( 9.181310023244000362, 4.573021367100345458, -6.377665258770703005 ) ) ;
#2091 = CARTESIAN_POINT ( 'NONE',  ( 12.78422293702846524, -3.124999446934218383, -13.52078617650838943 ) ) ;
#2092 = CARTESIAN_POINT ( 'NONE',  ( 18.00459872918310822, -0.4343244881883122632, -12.69000555157927934 ) ) ;
#2093 = CARTESIAN_POINT ( 'NONE',  ( 12.18033843151448181, 2.521515055313179321, -12.44655896212864121 ) ) ;
#2094 = CARTESIAN_POINT ( 'NONE',  ( 10.32533997688000049, -3.756890902898200046, -6.385465081946999355 ) ) ;
#2095 = CARTESIAN_POINT ( 'NONE',  ( 8.251329719592000345, 5.773189794777000117, 7.141495931231999883 ) ) ;
#2096 = ORIENTED_EDGE ( 'NONE', *, *, #52477, .F. ) ;
#2097 = B_SPLINE_CURVE_WITH_KNOTS ( 'NONE', 3,
 ( #6932, #61798, #61458, #19147 ),
 .UNSPECIFIED., .F., .F.,
 ( 4, 4 ),
 ( 0.000000000000000000, 1.000000000000000000 ),
 .UNSPECIFIED. ) ;
#2098 = AXIS2_PLACEMENT_3D ( 'NONE', #41474, #4399, #42170 ) ;
#2099 = SHAPE_DEFINITION_REPRESENTATION ( #14325, #10823 ) ;
#2100 = CARTESIAN_POINT ( 'NONE',  ( 23.89320776801300283, -10.75689324691000337, 4.023240149132002230 ) ) ;
#2101 = CARTESIAN_POINT ( 'NONE',  ( 8.204580816340586225, 2.648164948733333635, 7.853008025112000468 ) ) ;
#2102 = CARTESIAN_POINT ( 'NONE',  ( 10.44806481732999792, 3.684980864017000091, -6.173120265414000052 ) ) ;
#2103 = CARTESIAN_POINT ( 'NONE',  ( 17.84319482158666048, 1.945290144093657192, 12.56363827966045932 ) ) ;
#2104 = CARTESIAN_POINT ( 'NONE',  ( 18.53493609108600282, 3.035043098171999798, -12.19104765307000093 ) ) ;
#2105 = CARTESIAN_POINT ( 'NONE',  ( 9.753142190738998352, 4.104977339646000090, 9.293283246364000050 ) ) ;
#2106 = ADVANCED_FACE ( 'NONE', ( #12247 ), #47478, .F. ) ;
#2107 = CARTESIAN_POINT ( 'NONE',  ( 10.00552075086462622, -4.127043264527912925, 8.365674464137100586 ) ) ;
#2108 = DIRECTION ( 'NONE',  ( 1.000000000000000000, 0.000000000000000000, 0.000000000000000000 ) ) ;
#2109 = VERTEX_POINT ( 'NONE', #10683 ) ;
#2110 = CARTESIAN_POINT ( 'NONE',  ( 12.60227161487513747, -1.908786995848724022, 12.56986146204938137 ) ) ;
#2111 = CARTESIAN_POINT ( 'NONE',  ( 9.097772138681998300, -4.373757805842100055, -6.567719246739500250 ) ) ;
#2112 = CARTESIAN_POINT ( 'NONE',  ( 9.514114512910998300, 4.887632373702999189, 8.462748516415999234 ) ) ;
#2113 = DIRECTION ( 'NONE',  ( 0.000000000000000000, 1.000000000000000000, 0.000000000000000000 ) ) ;
#2114 = CARTESIAN_POINT ( 'NONE',  ( 10.69456919669529960, 5.093991349577000172, -7.823222900359999343 ) ) ;
#2115 = CARTESIAN_POINT ( 'NONE',  ( 12.45211143562937650, -0.6284163952874709524, 12.58432055988358123 ) ) ;
#2116 = CARTESIAN_POINT ( 'NONE',  ( 8.625073341231001223, 3.117378429069999957, 8.662179062556001341 ) ) ;
#2117 = CARTESIAN_POINT ( 'NONE',  ( 9.781673028307999118, 5.464749740720999505, 8.817329433105999925 ) ) ;
#2118 = CARTESIAN_POINT ( 'NONE',  ( 12.39760546513563533, 2.025954772141363769, 12.54945441499613068 ) ) ;
#2119 = ORIENTED_EDGE ( 'NONE', *, *, #25190, .F. ) ;
#2120 = CARTESIAN_POINT ( 'NONE',  ( 25.41800012423099986, 8.397683232140998655, 8.090286078321000218 ) ) ;
#2121 = CARTESIAN_POINT ( 'NONE',  ( 10.34580110216399973, 2.909301855364999856, -6.833896451085399448 ) ) ;
#2122 = DIRECTION ( 'NONE',  ( 0.000000000000000000, 0.000000000000000000, -1.000000000000000000 ) ) ;
#2124 = CARTESIAN_POINT ( 'NONE',  ( 17.96217742534082618, -0.4744044027482017256, 12.68807559256817008 ) ) ;
#2123 = CARTESIAN_POINT ( 'NONE',  ( 8.753441940380000119, -2.876278577719999952, 6.568889245344999850 ) ) ;
#2125 = CARTESIAN_POINT ( 'NONE',  ( 10.48926717315599966, -4.764472860199700399, 8.151477970733999712 ) ) ;
#2126 = CARTESIAN_POINT ( 'NONE',  ( 11.53979707368350027, -4.430269712815499972, -6.748224392138099326 ) ) ;
#2127 = ORIENTED_EDGE ( 'NONE', *, *, #18147, .T. ) ;
#2128 = CARTESIAN_POINT ( 'NONE',  ( 1.310247135131999974, 2.440310627160000134, 2.160132089918000098 ) ) ;
#2129 = CARTESIAN_POINT ( 'NONE',  ( 24.12728729028544450, -9.172538159014450798, -9.141953683885004622 ) ) ;
#2130 = CARTESIAN_POINT ( 'NONE',  ( 11.09393020684900044, -2.750000000000000000, 7.500000000000000000 ) ) ;
#2131 = CARTESIAN_POINT ( 'NONE',  ( 18.10276869593483440, -2.801190086625830133, 13.60495303825237023 ) ) ;
#2132 = CARTESIAN_POINT ( 'NONE',  ( 7.720433623367209286, 2.879779284299745168, 6.726083774559347361 ) ) ;
#2133 = CARTESIAN_POINT ( 'NONE',  ( 12.09915596617140920, -2.684647274610782119, 13.74018952919733572 ) ) ;
#2134 = FACE_BOUND ( 'NONE', #12463, .T. ) ;
#2135 = DIRECTION ( 'NONE',  ( 0.7071067811865473507, 0.7071067811865473507, -2.044918114706133567E-08 ) ) ;
#2136 = CARTESIAN_POINT ( 'NONE',  ( 24.44496356232399847, -3.224881240379999792, -12.03535804424000055 ) ) ;
#2137 = ORIENTED_EDGE ( 'NONE', *, *, #3463, .T. ) ;
#2138 = CARTESIAN_POINT ( 'NONE',  ( 7.500416666664126097, 4.176714586764424197, -6.150000000000000355 ) ) ;
#2139 = EDGE_CURVE ( 'NONE', #67987, #8310, #21178, .T. ) ;
#2140 = EDGE_CURVE ( 'NONE', #22158, #29897, #58322, .T. ) ;
#2141 = DIRECTION ( 'NONE',  ( 0.000000000000000000, 0.9772984074130801613, 0.2118674653358960658 ) ) ;
#2142 = CARTESIAN_POINT ( 'NONE',  ( 17.63765675162811419, 1.874999999999999778, -13.78631904427533428 ) ) ;
#2143 = CARTESIAN_POINT ( 'NONE',  ( 18.30003129334700063, -2.732683817159999862, 11.53064095410000078 ) ) ;
#2144 = CARTESIAN_POINT ( 'NONE',  ( 1.657430528421999893, -0.2286091751511999948, 3.751814989407999956 ) ) ;
#2145 = ORIENTED_EDGE ( 'NONE', *, *, #32579, .T. ) ;
#2146 = DIRECTION ( 'NONE',  ( -1.000000000000000000, 0.000000000000000000, 0.000000000000000000 ) ) ;
#2147 = B_SPLINE_CURVE_WITH_KNOTS ( 'NONE', 3,
 ( #68432, #35946, #15315, #41878, #21242, #36639, #57260, #42570, #63185, #9360 ),
 .UNSPECIFIED., .F., .F.,
 ( 4, 2, 2, 2, 4 ),
 ( 0.000000000000000000, 0.2500000000000004441, 0.5000000000000008882, 0.7500000000000004441, 1.000000000000000000 ),
 .UNSPECIFIED. ) ;
#2148 = CARTESIAN_POINT ( 'NONE',  ( 21.59999953993000332, 7.283063041541000399E-14, -6.705747068735999778E-14 ) ) ;
#2149 = DIRECTION ( 'NONE',  ( 0.000000000000000000, -0.9466492601157001641, 0.3222656952305000266 ) ) ;
#2150 = CARTESIAN_POINT ( 'NONE',  ( 10.82179975933729921, 4.948878321068100661, 7.826467126457498757 ) ) ;
#2151 = B_SPLINE_CURVE_WITH_KNOTS ( 'NONE', 3,
 ( #29955, #3013, #8264, #35529 ),
 .UNSPECIFIED., .F., .F.,
 ( 4, 4 ),
 ( 0.000000000000000000, 1.000000000000000000 ),
 .UNSPECIFIED. ) ;
#2152 = CARTESIAN_POINT ( 'NONE',  ( 9.662398456552571346, -2.649938674317672049, 7.712117850346626113 ) ) ;
#2153 = CARTESIAN_POINT ( 'NONE',  ( 10.17270027370999941, -4.650151116117000605, -8.655526539784000661 ) ) ;
#2154 = CARTESIAN_POINT ( 'NONE',  ( 10.99385884816407888, -6.138431480138868856, 5.072166845528967016 ) ) ;
#2155 = CARTESIAN_POINT ( 'NONE',  ( 8.132072785282833394, 10.58563748539984850, 4.156721893235244103 ) ) ;
#2156 = CARTESIAN_POINT ( 'NONE',  ( 12.19483627255733893, -2.635236895375446586, 12.41905446230203758 ) ) ;
#2157 = EDGE_CURVE ( 'NONE', #61768, #27955, #21192, .T. ) ;
#2158 = VERTEX_POINT ( 'NONE', #53344 ) ;
#2159 = CARTESIAN_POINT ( 'NONE',  ( 9.342560841233000346, 5.835196551504000517, -7.008466539623000813 ) ) ;
#2160 = ORIENTED_EDGE ( 'NONE', *, *, #46879, .T. ) ;
#2161 = CARTESIAN_POINT ( 'NONE',  ( 18.07092639204462259, -2.147008627175521767, 13.74201915664823659 ) ) ;
#2162 = CARTESIAN_POINT ( 'NONE',  ( 11.23195122972050086, -3.492749840905900349, -6.326963915009999440 ) ) ;
#2163 = EDGE_LOOP ( 'NONE', ( #31496, #56603, #67810, #61087 ) ) ;
#2164 = ORIENTED_EDGE ( 'NONE', *, *, #36441, .F. ) ;
#2165 = ADVANCED_FACE ( 'NONE', ( #21860 ), #41558, .F. ) ;
#2166 = CARTESIAN_POINT ( 'NONE',  ( 24.97036958156635578, -2.963721569976427439, -11.58470578805197526 ) ) ;
#2167 = CARTESIAN_POINT ( 'NONE',  ( 5.000000000000000000, 0.6769230769231000533, -2.665384615385000266 ) ) ;
#2168 = CARTESIAN_POINT ( 'NONE',  ( 10.98768491210000064, -8.067891622241001315, 6.818837029638999958 ) ) ;
#2169 = CARTESIAN_POINT ( 'NONE',  ( 11.09999999999999964, -4.000000000000000000, -7.500000000000000000 ) ) ;
#2170 = CARTESIAN_POINT ( 'NONE',  ( 24.39664890157733268, -12.09373467336017960, 3.240506439202065270 ) ) ;
#2171 = DIRECTION ( 'NONE',  ( 1.000000000000000000, 0.000000000000000000, 0.000000000000000000 ) ) ;
#2172 = CARTESIAN_POINT ( 'NONE',  ( 0.7509734658760000015, -3.500000000000000000, 0.000000000000000000 ) ) ;
#2173 = CARTESIAN_POINT ( 'NONE',  ( 11.11264194660999927, -2.146089039267000231, -7.517188649391000510 ) ) ;
#2174 = DIRECTION ( 'NONE',  ( -0.7071067811865474617, 0.7071067811865474617, 1.196435574830078999E-09 ) ) ;
#2175 = CARTESIAN_POINT ( 'NONE',  ( 10.69836233406524606, -2.942435227297377498, -5.063088263990971782 ) ) ;
#2176 = ORIENTED_EDGE ( 'NONE', *, *, #18228, .F. ) ;
#2177 = CARTESIAN_POINT ( 'NONE',  ( 10.99828335019000214, -2.710349843344999954, -4.962170859942000689 ) ) ;
#2178 = CARTESIAN_POINT ( 'NONE',  ( 1.775000508673000077, 0.000000000000000000, -1.700000581162000035 ) ) ;
#2179 = CARTESIAN_POINT ( 'NONE',  ( 10.27122572358000063, -4.578406546873999616, 4.846540991051999647 ) ) ;
#2180 = DIRECTION ( 'NONE',  ( 0.000000000000000000, -0.8648648648648720183, -0.5020047465136826537 ) ) ;
#2181 = CARTESIAN_POINT ( 'NONE',  ( 10.31759632033899976, 2.815618218644000414, -7.016653143730500197 ) ) ;
#2182 = CARTESIAN_POINT ( 'NONE',  ( 12.61244651655885640, 1.905326457160023690, 13.78169738549997092 ) ) ;
#2183 = B_SPLINE_SURFACE_WITH_KNOTS ( 'NONE', 3, 3, ( 
 ( #41366, #56413, #51503, #3267, #66892, #19004, #51172, #24599, #51845, #67231, #35437, #30532, #56763, #30879, #8860, #62675, #14457, #30197, #19346, #57091, #3600, #9534, #24936, #46955, #46270, #14795, #24249, #67573, #3943, #45586, #57428, #25282, #40331, #61654, #46616, #8516, #29864, #67921, #13768, #35101, #19698, #41018, #62340, #35777, #49665, #24129, #12964, #17510, #13316, #28348, #45464, #1774, #66778, #33594, #3148, #12265, #18894, #50706, #54911, #29050, #65739, #38836, #39525, #24479, #60162, #34979, #7014 ),
 ( #55610, #60849, #66081, #44782, #2803, #34288, #23092, #50016, #7711, #28701, #29397, #18202, #2125, #50362, #40219, #34638, #45801, #56296, #2461, #60501, #61536, #13651, #23785, #33941, #8399, #44441, #45121, #17862, #39178, #66428, #12610, #29744, #51047, #23444, #55262, #7356, #18549, #55950, #61195, #39878, #8055, #44719, #28282, #18484, #50640, #44378, #56227, #34225, #54850, #55544, #66016, #24066, #28990, #6949, #7642, #55890, #49602, #50298, #1710, #2396, #2740, #39810, #8336, #61132, #29680, #23720, #34574 ),
 ( #34912, #39117, #66363, #50983, #7994, #45056, #18831, #40157, #13249, #65328, #17447, #29327, #61473, #45401, #66710, #13592, #22681, #44025, #23029, #38773, #18139, #60097, #12203, #33531, #65676, #17798, #60440, #12547, #33878, #55195, #7297, #28638, #49949, #2062, #23380, #39462, #60782, #12896, #24413, #20534, #61811, #9343, #10039, #57943, #62487, #40484, #57586, #3755, #35255, #41180, #52348, #30687, #56571, #19509, #41859, #47112, #67727, #51996, #25094, #8675, #68071, #4442, #13928, #19160, #14611, #4100, #40827 ),
 ( #51659, #30022, #3419, #45741, #3080, #63165, #30352, #35598, #51324, #25435, #35929, #46425, #19851, #57241, #9694, #46768, #24754, #56912, #20188, #14270, #14946, #41516, #9011, #62827, #36271, #31040, #31378, #15294, #25781, #46079, #68411, #36619, #67387, #67051, #62152, #5826, #11758, #22252, #53727, #5138, #58975, #63859, #26475, #32753, #43590, #37302, #11077, #53043, #42216, #64889, #16660, #53387, #48485, #43239, #54067, #32412, #591, #21900, #64545, #16316, #47808, #5488, #59311, #42551, #63521, #27163, #26823 ) ),
 .UNSPECIFIED., .F., .F., .F.,
 ( 4, 4 ),
 ( 4, 1, 1, 1, 1, 1, 1, 1, 1, 1, 1, 1, 1, 1, 1, 1, 1, 1, 1, 1, 1, 1, 1, 1, 1, 1, 1, 1, 1, 1, 1, 1, 1, 1, 1, 1, 1, 1, 1, 1, 1, 1, 1, 1, 1, 1, 1, 1, 1, 1, 1, 1, 1, 1, 1, 1, 1, 1, 1, 1, 1, 1, 1, 1, 4 ),
 ( -0.02000000000000000042, 1.020000000000000018 ),
 ( -0.02000000000000000042, -0.003749999999999999861, 0.01250000000000000069, 0.02875000000000000125, 0.04499999999999999833, 0.06124999999999999889, 0.07749999999999999944, 0.09375000000000000000, 0.1100000000000000006, 0.1262500000000000011, 0.1424999999999999878, 0.1587500000000000022, 0.1749999999999999889, 0.1912500000000000033, 0.2074999999999999900, 0.2237500000000000044, 0.2399999999999999911, 0.2562499999999999778, 0.2725000000000000200, 0.2887500000000000067, 0.3049999999999999933, 0.3212499999999999800, 0.3375000000000000222, 0.3537500000000000089, 0.3699999999999999956, 0.3862499999999999822, 0.4025000000000000244, 0.4187500000000000111, 0.4349999999999999978, 0.4512499999999999845, 0.4675000000000000266, 0.4837500000000000133, 0.5000000000000000000, 0.5162499999999999867, 0.5324999999999999734, 0.5487499999999999600, 0.5649999999999999467, 0.5812500000000000444, 0.5975000000000000311, 0.6137500000000000178, 0.6300000000000000044, 0.6462499999999999911, 0.6624999999999999778, 0.6787499999999999645, 0.6949999999999999512, 0.7112500000000000488, 0.7275000000000000355, 0.7437500000000000222, 0.7600000000000000089, 0.7762499999999999956, 0.7924999999999999822, 0.8087499999999999689, 0.8249999999999999556, 0.8412500000000000533, 0.8575000000000000400, 0.8737500000000000266, 0.8900000000000000133, 0.9062500000000000000, 0.9224999999999999867, 0.9387499999999999734, 0.9549999999999999600, 0.9712499999999999467, 0.9875000000000000444, 1.003749999999999920, 1.020000000000000018 ),
 .UNSPECIFIED. ) ;
#2184 = CARTESIAN_POINT ( 'NONE',  ( 10.64872180584000105, -2.614778238704999591, 6.717279975758000177 ) ) ;
#2185 = ORIENTED_EDGE ( 'NONE', *, *, #42796, .F. ) ;
#2186 = CARTESIAN_POINT ( 'NONE',  ( 23.60205915885299888, -9.230633470673003771, -8.204162215335996322 ) ) ;
#2187 = CARTESIAN_POINT ( 'NONE',  ( 12.57519714614618778, -0.5812901181791702010, 13.88363587338390381 ) ) ;
#2188 = ORIENTED_EDGE ( 'NONE', *, *, #14440, .T. ) ;
#2189 = CARTESIAN_POINT ( 'NONE',  ( 6.950909439180999350, 2.788803157567000035, -8.345558963038001821 ) ) ;
#2190 = CARTESIAN_POINT ( 'NONE',  ( 10.60689139212527898, 4.693532862563775332, -4.759459215670841736 ) ) ;
#2191 = AXIS2_PLACEMENT_3D ( 'NONE', #67985, #150, #5047 ) ;
#2192 = CARTESIAN_POINT ( 'NONE',  ( 8.751496707488000126, 4.081676005979390176, 6.643597378104299622 ) ) ;
#2193 = CARTESIAN_POINT ( 'NONE',  ( 4.170446217910000364, -0.9708739270978999913, -1.205883038339000235 ) ) ;
#2194 = B_SPLINE_CURVE_WITH_KNOTS ( 'NONE', 3,
 ( #31715, #22243, #53035, #49160, #15629, #43581, #54060, #26468, #27157, #21214 ),
 .UNSPECIFIED., .F., .F.,
 ( 4, 2, 2, 2, 4 ),
 ( 0.000000000000000000, 0.08334174874897928853, 0.1666834974979585771, 0.2500252462469378933, 0.3333669949959171541 ),
 .UNSPECIFIED. ) ;
#2195 = B_SPLINE_SURFACE_WITH_KNOTS ( 'NONE', 3, 3, ( 
 ( #6315, #53193, #52850, #4947, #37117, #26634, #58431, #10536, #47952, #42704, #37453, #23448, #12969, #39181, #2128, #49669, #44444, #44785, #18553, #17155, #59810, #34291, #11913, #38842, #22745, #55613, #1088, #17514, #50020, #65394, #50365, #61199, #12613, #38488, #55953 ),
 ( #13319, #22402, #34643, #43743, #66086, #29054, #60506, #33944, #44095, #29401, #54916, #18206, #12271, #33598, #7019, #60167, #33253, #7359, #55266, #39882, #7714, #8060, #28354, #2465, #23789, #1778, #23095, #28704, #65742, #65039, #39529, #54571, #6668, #17866, #60852 ),
 ( #45124, #49317, #28008, #66431, #1432, #30088, #14679, #14340, #2806, #56978, #3823, #25507, #35323, #8403, #13655, #50709, #8743, #40553, #9081, #51050, #18897, #24133, #30757, #51729, #62221, #29748, #68142, #20259, #46495, #66782, #67800, #30418, #56299, #40223, #9761 ),
 ( #40901, #19580, #3151, #45467, #56640, #25162, #61881, #13997, #51393, #24483, #61539, #19920, #35663, #41586, #57312, #62896, #67117, #52066, #62557, #3487, #24824, #41245, #46150, #15015, #35997, #34983, #45805, #67455, #19227, #9413, #4171, #46836, #36341, #57656, #21289 ) ),
 .UNSPECIFIED., .F., .F., .F.,
 ( 4, 4 ),
 ( 4, 1, 1, 1, 1, 1, 1, 1, 1, 1, 1, 1, 1, 1, 1, 1, 1, 1, 1, 1, 1, 1, 1, 1, 1, 1, 1, 1, 1, 1, 1, 1, 4 ),
 ( -0.1039370721279000015, 1.103937072127999963 ),
 ( -0.01999999999996000116, 0.01250000000003000100, 0.04500000000002999517, 0.07750000000003000322, 0.1100000000000000006, 0.1424999999999999878, 0.1749999999999999889, 0.2074999999999999900, 0.2399999999999999911, 0.2725000000000000200, 0.3049999999999999933, 0.3375000000000000222, 0.3699999999999999956, 0.4025000000000000244, 0.4349999999999999978, 0.4675000000000000266, 0.5000000000000000000, 0.5324999999999999734, 0.5649999999999999467, 0.5975000000000000311, 0.6300000000000000044, 0.6624999999999999778, 0.6949999999999999512, 0.7275000000000000355, 0.7600000000000000089, 0.7924999999999999822, 0.8249999999999999556, 0.8575000000000000400, 0.8900000000000000133, 0.9224999999999999867, 0.9549999999999999600, 0.9875000000000000444, 1.020000000000000018 ),
 .UNSPECIFIED. ) ;
#2196 = CARTESIAN_POINT ( 'NONE',  ( 9.079170280414000871, 4.815598936798999752, -8.835641302565999666 ) ) ;
#2197 = CARTESIAN_POINT ( 'NONE',  ( 17.76910169249500271, -3.411882384414000047, 11.89794055422999897 ) ) ;
#2198 = CARTESIAN_POINT ( 'NONE',  ( 25.59994555223600088, 10.09686240769173793, 5.033199831112243672 ) ) ;
#2199 = PRODUCT_DEFINITION ( 'UNKNOWN', '', #31816, #58350 ) ;
#2200 = DIRECTION ( 'NONE',  ( 0.000000000000000000, -1.000000000000000000, 0.000000000000000000 ) ) ;
#2201 = CARTESIAN_POINT ( 'NONE',  ( 0.000000000000000000, -2.899999999999999911, 7.500000000000000000 ) ) ;
#2202 = DIRECTION ( 'NONE',  ( 0.7071058580589949516, -0.7071077043128949358, 4.007459190705968920E-09 ) ) ;
#2203 = CARTESIAN_POINT ( 'NONE',  ( 9.658740731405000446, -5.476443305113000370, -7.051545409824000465 ) ) ;
#2204 = CARTESIAN_POINT ( 'NONE',  ( 10.40749413291699987, 4.788043169210699723, -7.140435631538599281 ) ) ;
#2205 = LINE ( 'NONE', #59883, #62835 ) ;
#2206 = CARTESIAN_POINT ( 'NONE',  ( 10.64391429142989765, 4.022379549362480766, -6.325326139450999641 ) ) ;
#2207 = CARTESIAN_POINT ( 'NONE',  ( 9.455342523874998406, 2.871335344632000020, -7.327226901081999699 ) ) ;
#2209 = DIRECTION ( 'NONE',  ( 0.000000000000000000, -1.000000000000000000, 0.000000000000000000 ) ) ;
#2208 = CARTESIAN_POINT ( 'NONE',  ( 15.48018231457700189, -8.819832297131000587, -7.692419064155999742 ) ) ;
#2210 = DIRECTION ( 'NONE',  ( 0.000000000000000000, 2.692747180787898834E-07, -0.9999999999999638067 ) ) ;
#2211 = ORIENTED_EDGE ( 'NONE', *, *, #64933, .T. ) ;
#2212 = CARTESIAN_POINT ( 'NONE',  ( 11.56322412107030928, 4.054600656575539475, 8.532060764998998792 ) ) ;
#2213 = CARTESIAN_POINT ( 'NONE',  ( 11.15982711745999900, -5.578228817597000955, 8.067792329320999656 ) ) ;
#2214 = CARTESIAN_POINT ( 'NONE',  ( 9.175772138681999479, 3.575113238066399912, 8.559813987224998755 ) ) ;
#2215 = CARTESIAN_POINT ( 'NONE',  ( 9.378875014952626543, 4.868116531169106587, -7.390885577342253931 ) ) ;
#2216 = CARTESIAN_POINT ( 'NONE',  ( 9.124702828701000357, -4.778665285493000070, 8.799745834808000211 ) ) ;
#2217 = CARTESIAN_POINT ( 'NONE',  ( 11.09999999999999964, 0.000000000000000000, 0.000000000000000000 ) ) ;
#2218 = UNCERTAINTY_MEASURE_WITH_UNIT (LENGTH_MEASURE( 1.000000000000000082E-05 ), #30891, 'distance_accuracy_value', 'NONE');
#2219 = ORIENTED_EDGE ( 'NONE', *, *, #66522, .T. ) ;
#2220 = EDGE_CURVE ( 'NONE', #22693, #7406, #5340, .T. ) ;
#2221 = EDGE_CURVE ( 'NONE', #8563, #48552, #29298, .T. ) ;
#2222 = CARTESIAN_POINT ( 'NONE',  ( 8.746126402770999064, -2.931626221533000010, -7.097120470443400109 ) ) ;
#2223 = DIRECTION ( 'NONE',  ( 0.000000000000000000, 1.000000000000000000, 0.000000000000000000 ) ) ;
#2224 = CARTESIAN_POINT ( 'NONE',  ( 6.002477004709999342, 0.8716839254852999375, 1.181818379215999970 ) ) ;
#2225 = CARTESIAN_POINT ( 'NONE',  ( 7.000000000000000000, 7.526486366024999874, 3.526486366024999874 ) ) ;
#2226 = DIRECTION ( 'NONE',  ( -1.000000000000000000, 0.000000000000000000, 0.000000000000000000 ) ) ;
#2227 = CARTESIAN_POINT ( 'NONE',  ( 11.78179573085659904, 4.973133828855400118, -7.668383662421899061 ) ) ;
#2228 = DIRECTION ( 'NONE',  ( 0.000000000000000000, 0.9565994702956989171, -0.2914059941558995170 ) ) ;
#2229 = CARTESIAN_POINT ( 'NONE',  ( 9.568154437819998748, -5.318469253323000245, -7.099528416287999910 ) ) ;
#2230 = CARTESIAN_POINT ( 'NONE',  ( 10.15293113568789352, -5.100000000000000533, -6.444141223401128826 ) ) ;
#2231 = VERTEX_POINT ( 'NONE', #10343 ) ;
#2232 = CARTESIAN_POINT ( 'NONE',  ( 7.400000000000000355, 0.000000000000000000, 0.000000000000000000 ) ) ;
#2233 = CARTESIAN_POINT ( 'NONE',  ( 12.63955452181609296, -0.7113363331415235580, -13.98191770012930135 ) ) ;
#2234 = CARTESIAN_POINT ( 'NONE',  ( 9.179055905797000037, -2.899999999999999911, 6.571291218949999902 ) ) ;
#2235 = CARTESIAN_POINT ( 'NONE',  ( 24.85106292538000261, -8.568916185850000033, -8.855133745165000292 ) ) ;
#2236 = VECTOR ( 'NONE', #24250, 999.9999999999998863 ) ;
#2237 = CARTESIAN_POINT ( 'NONE',  ( 4.900006121741999010, 1.007237960741798055, -1.747572776708516296 ) ) ;
#2238 = CARTESIAN_POINT ( 'NONE',  ( 7.000000000000000000, 10.24590114424279363, 4.325272293848827054 ) ) ;
#2239 = CARTESIAN_POINT ( 'NONE',  ( 13.36350100824700071, 12.09092425779999935, 2.196870506499999820 ) ) ;
#2240 = ORIENTED_EDGE ( 'NONE', *, *, #41188, .T. ) ;
#2241 = DIRECTION ( 'NONE',  ( 0.000000000000000000, 0.000000000000000000, -1.000000000000000000 ) ) ;
#2242 = CARTESIAN_POINT ( 'NONE',  ( 18.10320344748333454, 2.199570933858661981, -13.73260621368703660 ) ) ;
#2243 = VERTEX_POINT ( 'NONE', #15931 ) ;
#2244 = ADVANCED_FACE ( 'NONE', ( #5446 ), #32707, .F. ) ;
#2245 = CARTESIAN_POINT ( 'NONE',  ( 8.466090690305668076, 5.179931350395810874, 8.180989497825182255 ) ) ;
#2246 = CARTESIAN_POINT ( 'NONE',  ( 2.759306799211165728, -3.058252359239909346, 1.762666431298136605 ) ) ;
#2247 = CARTESIAN_POINT ( 'NONE',  ( 9.988985841228000595, 3.986577607995999806, -9.280166295424001177 ) ) ;
#2248 = CARTESIAN_POINT ( 'NONE',  ( 13.73886390325583484, -9.223149073484993465, -8.172668166918892751 ) ) ;
#2249 = CARTESIAN_POINT ( 'NONE',  ( 11.01279632507519857, -3.375091146194399983, -8.658468685623999406 ) ) ;
#2250 = CARTESIAN_POINT ( 'NONE',  ( 17.88362877544205176, 0.5317665474480599563, -12.68501283761906251 ) ) ;
#2251 = PLANE ( 'NONE',  #36256 ) ;
#2252 = ORIENTED_EDGE ( 'NONE', *, *, #59755, .T. ) ;
#2253 = LINE ( 'NONE', #23567, #59966 ) ;
#2254 = CARTESIAN_POINT ( 'NONE',  ( 18.05135021981381982, -2.880031268720636195, -13.58542674995411126 ) ) ;
#2255 = CARTESIAN_POINT ( 'NONE',  ( 17.72013721777323880, -1.891648809703187606, 13.78386988244476008 ) ) ;
#2256 = ORIENTED_EDGE ( 'NONE', *, *, #58583, .F. ) ;
#2257 = CARTESIAN_POINT ( 'NONE',  ( 10.02799997617999850, 3.452028386838999818, -6.074524158096999749 ) ) ;
#2258 = ORIENTED_EDGE ( 'NONE', *, *, #786, .F. ) ;
#2259 = CARTESIAN_POINT ( 'NONE',  ( 9.001430433046998303, 3.145249924879699677, 8.027488966151301142 ) ) ;
#2260 = CARTESIAN_POINT ( 'NONE',  ( 18.03534466112218482, -3.019381283786360282, -12.23288205540259099 ) ) ;
#2261 = CARTESIAN_POINT ( 'NONE',  ( 9.435596873515667227, 2.907767014557176566, 6.870476274536375882 ) ) ;
#2262 = CARTESIAN_POINT ( 'NONE',  ( 20.75138802851920161, 5.760487483753345295, -0.05108123232907756106 ) ) ;
#2263 = CARTESIAN_POINT ( 'NONE',  ( 11.06697824072435488, 2.733021759275644946, 6.467485083951054925 ) ) ;
#2264 = CARTESIAN_POINT ( 'NONE',  ( 8.978113844317999082, 4.218953675027299788, 8.338908357746399602 ) ) ;
#2265 = CARTESIAN_POINT ( 'NONE',  ( 7.642630378808000557, -9.064121401021999702, -5.575735562471000328 ) ) ;
#2266 = EDGE_LOOP ( 'NONE', ( #53785, #31479 ) ) ;
#2267 = CARTESIAN_POINT ( 'NONE',  ( 8.237893718522188991, -4.937145962667132792, 6.269524514844754037 ) ) ;
#2268 = CARTESIAN_POINT ( 'NONE',  ( 10.66042971959000063, 2.315663237570999566, -7.431702255173999738 ) ) ;
#2269 = CARTESIAN_POINT ( 'NONE',  ( 18.18005044388383240, -2.499999700414728743, -12.45156116530568902 ) ) ;
#2270 = CARTESIAN_POINT ( 'NONE',  ( 12.37945077454910781, 1.926407208811268257, -13.86683589633374147 ) ) ;
#2271 = CARTESIAN_POINT ( 'NONE',  ( 11.11476354018240364, -2.782534154164604256, 7.827184855449092815 ) ) ;
#2272 = CARTESIAN_POINT ( 'NONE',  ( 24.95408850090100117, 3.532265432305000008, 11.87004585020000036 ) ) ;
#2273 = CARTESIAN_POINT ( 'NONE',  ( 17.55505043854144276, 0.6250000000000001110, 13.88107975066923316 ) ) ;
#2274 = CARTESIAN_POINT ( 'NONE',  ( 25.34046477980565726, -8.480592698500919013, 7.990868443695373635 ) ) ;
#2275 = EDGE_CURVE ( 'NONE', #10113, #8792, #3596, .T. ) ;
#2276 = EDGE_CURVE ( 'NONE', #59370, #20699, #35967, .T. ) ;
#2277 = ORIENTED_EDGE ( 'NONE', *, *, #19880, .F. ) ;
#2278 = EDGE_LOOP ( 'NONE', ( #10024, #47177, #239, #5015 ) ) ;
#2279 = CARTESIAN_POINT ( 'NONE',  ( 9.386379719595000282, 5.673443217382001080, -7.051790060464000476 ) ) ;
#2280 = CARTESIAN_POINT ( 'NONE',  ( 12.41737190950597736, -0.4903666733423311941, 13.88835870178277965 ) ) ;
#2281 = CARTESIAN_POINT ( 'NONE',  ( 12.19329716804611508, -2.371658047293454530, 13.69984404025631441 ) ) ;
#2282 = DIRECTION ( 'NONE',  ( 0.8660254037844288266, -2.732564487855089756E-14, 0.5000000000000169864 ) ) ;
#2283 = CARTESIAN_POINT ( 'NONE',  ( 7.743183059623000020, -2.735207418315000361, 6.771977475428999860 ) ) ;
#2284 = CARTESIAN_POINT ( 'NONE',  ( 8.470944094208999076, -5.100000000000000533, 6.571291218949999902 ) ) ;
#2286 = LINE ( 'NONE', #22909, #50725 ) ;
#2285 = CARTESIAN_POINT ( 'NONE',  ( 10.74160887879199855, -4.289688213680199702, 8.745979585038000437 ) ) ;
#2287 = CARTESIAN_POINT ( 'NONE',  ( 10.19810941423799910, 4.946022705791000007, -6.640722727400100389 ) ) ;
#2288 = ORIENTED_EDGE ( 'NONE', *, *, #68127, .F. ) ;
#2289 = LINE ( 'NONE', #29911, #35859 ) ;
#2290 = CARTESIAN_POINT ( 'NONE',  ( 5.200000000000000178, 0.8000000000000000444, -3.149999999999999911 ) ) ;
#2291 = CARTESIAN_POINT ( 'NONE',  ( 11.09999999999999787, 5.503163505825636292, 6.850128801896341102 ) ) ;
#2292 = CARTESIAN_POINT ( 'NONE',  ( 12.33488707410255714, -0.4118223544696936744, 12.69101228723419261 ) ) ;
#2293 = CARTESIAN_POINT ( 'NONE',  ( 18.15140653325676467, -2.687261711676918630, -12.40596587103102522 ) ) ;
#2294 = EDGE_LOOP ( 'NONE', ( #17746, #39052 ) ) ;
#2296 = CARTESIAN_POINT ( 'NONE',  ( 10.89393020684959978, 2.750000000000000000, 7.500000000000000000 ) ) ;
#2295 = CARTESIAN_POINT ( 'NONE',  ( 8.160745559622998968, -5.944572422272999646, 7.106845737860000511 ) ) ;
#2297 = CARTESIAN_POINT ( 'NONE',  ( 9.450870280412999591, 2.928319778732999978, -8.861178115809998701 ) ) ;
#2298 = EDGE_CURVE ( 'NONE', #1148, #1871, #54939, .T. ) ;
#2299 = CARTESIAN_POINT ( 'NONE',  ( 25.29987667925500361, 10.83443035398000021, 3.855530949778000149 ) ) ;
#2300 = CARTESIAN_POINT ( 'NONE',  ( 10.59195391537400077, 5.057233422790000432, 6.781965272201699868 ) ) ;
#2301 = ADVANCED_FACE ( 'NONE', ( #64843 ), #49383, .T. ) ;
#2302 = PLANE ( 'NONE',  #6545 ) ;
#2303 = CARTESIAN_POINT ( 'NONE',  ( 8.198728570659000070, 3.399995396149000371, 6.142472185125999573 ) ) ;
#2304 = CARTESIAN_POINT ( 'NONE',  ( 3.453567742316999922, -1.715169620629000136, -3.156336854149000448 ) ) ;
#2305 = ORIENTED_EDGE ( 'NONE', *, *, #61446, .T. ) ;
#2306 = CARTESIAN_POINT ( 'NONE',  ( 12.33591545429644398, -0.5485298171727041039, -12.58805670501782004 ) ) ;
#2307 = CARTESIAN_POINT ( 'NONE',  ( 12.30490414479101524, -2.123060221858890095, -12.53148904351019866 ) ) ;
#2308 = CARTESIAN_POINT ( 'NONE',  ( 24.11240964069585146, -12.52839750956255571, -3.382904902698306682 ) ) ;
#2309 = CARTESIAN_POINT ( 'NONE',  ( 24.36809152945900081, 3.197172894633000251, -12.07984101077999917 ) ) ;
#2310 = ORIENTED_EDGE ( 'NONE', *, *, #13063, .T. ) ;
#2311 = CARTESIAN_POINT ( 'NONE',  ( 6.148521586833000541, 0.6981053669911999604, 0.9464826977047000600 ) ) ;
#2312 = CARTESIAN_POINT ( 'NONE',  ( 8.667410841228999629, 4.727211190310000255, -8.622645617656999661 ) ) ;
#2314 = CARTESIAN_POINT ( 'NONE',  ( 6.999998782146999332, -11.95749337870000062, 3.642574926947999892 ) ) ;
#2313 = CYLINDRICAL_SURFACE ( 'NONE', #26337, 1.000000000000000444 ) ;
#2315 = CARTESIAN_POINT ( 'NONE',  ( 10.68035971519489813, 4.678140486081599825, -6.371865185335000348 ) ) ;
#2316 = EDGE_LOOP ( 'NONE', ( #27031, #25592, #43397, #31222 ) ) ;
#2317 = CARTESIAN_POINT ( 'NONE',  ( 8.228368194308000483, 4.806758213781000322, 6.177034601037000527 ) ) ;
#2318 = ORIENTED_EDGE ( 'NONE', *, *, #22954, .F. ) ;
#2319 = EDGE_CURVE ( 'NONE', #52012, #63702, #47413, .T. ) ;
#2320 = CARTESIAN_POINT ( 'NONE',  ( 11.09999233421999953, 0.5000002011213999786, -9.776630298829998011 ) ) ;
#2322 = CARTESIAN_POINT ( 'NONE',  ( 16.20679720086500097, 3.450734216086000394, 11.08786462205999968 ) ) ;
#2321 = CIRCLE ( 'NONE', #7914, 11.84999999999999964 ) ;
#2323 = CARTESIAN_POINT ( 'NONE',  ( 17.99694095195319576, 0.5793931417437954146, -13.98801390351337837 ) ) ;
#2324 = VERTEX_POINT ( 'NONE', #20838 ) ;
#2325 = CARTESIAN_POINT ( 'NONE',  ( 10.95501454684088749, 9.026663460494706470, -6.403348769895080395 ) ) ;
#2326 = DIRECTION ( 'NONE',  ( 0.000000000000000000, -1.000000000000000000, -4.343197676503993465E-12 ) ) ;
#2327 = VECTOR ( 'NONE', #35567, 1000.000000000000114 ) ;
#2328 = CARTESIAN_POINT ( 'NONE',  ( 7.739689158769000876, 3.600418141940000094, -8.839175402873999943 ) ) ;
#2329 = CARTESIAN_POINT ( 'NONE',  ( 10.10478570706233370, 5.131706358131709500, 6.886599490775120458 ) ) ;
#2330 = CARTESIAN_POINT ( 'NONE',  ( 18.19991693152162426, -3.160411602603943049, 11.91446363486502413 ) ) ;
#2331 = VERTEX_POINT ( 'NONE', #64162 ) ;
#2332 = CARTESIAN_POINT ( 'NONE',  ( 24.67921580188599862, 3.567514645466999923, -12.13750897870000145 ) ) ;
#2333 = CARTESIAN_POINT ( 'NONE',  ( 24.56914242134000048, -12.57279260814000033, -2.966897477730999544 ) ) ;
#2335 = CONICAL_SURFACE ( 'NONE', #44768, 12.47499939740000130, 0.7853981102588313279 ) ;
#2334 = B_SPLINE_CURVE_WITH_KNOTS ( 'NONE', 3,
 ( #28072, #11982, #33320, #49046, #1498, #44164, #54985, #44850, #7082, #17932, #12681, #28776, #66157, #34363, #39596, #46905, #19993, #9146 ),
 .UNSPECIFIED., .F., .F.,
 ( 4, 2, 2, 2, 2, 2, 2, 2, 4 ),
 ( 0.000000000000000000, 0.1250000000000000000, 0.2500000000000000000, 0.3750000000000000000, 0.5000000000000000000, 0.6250000000000000000, 0.7500000000000000000, 0.8750000000000000000, 1.000000000000000000 ),
 .UNSPECIFIED. ) ;
#2336 = DIRECTION ( 'NONE',  ( 0.000000000000000000, -0.2437104726400046162, 0.9698480321811173699 ) ) ;
#2337 = CARTESIAN_POINT ( 'NONE',  ( 12.80505043854146940, -1.787816316115923287, 13.88537766212463076 ) ) ;
#2338 = ORIENTED_EDGE ( 'NONE', *, *, #27193, .F. ) ;
#2339 = DIRECTION ( 'NONE',  ( -1.000000000000000000, 0.000000000000000000, 0.000000000000000000 ) ) ;
#2340 = CARTESIAN_POINT ( 'NONE',  ( 8.896714042595458949, -4.136150106425177775, -6.453285899984953389 ) ) ;
#2341 = CARTESIAN_POINT ( 'NONE',  ( 4.699998537092440642, 13.17499999999999893, 0.000000000000000000 ) ) ;
#2342 = CARTESIAN_POINT ( 'NONE',  ( 10.02052890782000105, -2.899999999999999911, 6.152188490330000370 ) ) ;
#2343 = CARTESIAN_POINT ( 'NONE',  ( 24.44496488009700030, 8.810487470433001178, 8.810507756548000557 ) ) ;
#2344 = CARTESIAN_POINT ( 'NONE',  ( 12.27392385059252966, -0.3300666952397324216, -13.89473968862477449 ) ) ;
#2345 = CARTESIAN_POINT ( 'NONE',  ( 17.74784205817680061, -3.094544633123687660, 12.29297002796977800 ) ) ;
#2346 = ORIENTED_EDGE ( 'NONE', *, *, #26547, .T. ) ;
#2347 = CARTESIAN_POINT ( 'NONE',  ( 10.68546886766499959, -4.566506264294200257, -6.470713638631999665 ) ) ;
#2348 = ORIENTED_EDGE ( 'NONE', *, *, #9941, .T. ) ;
#2349 = DIRECTION ( 'NONE',  ( 0.000000000000000000, 0.2588190451024934835, 0.9659258262890757507 ) ) ;
#2350 = CARTESIAN_POINT ( 'NONE',  ( 9.476970280414001024, 5.511689883260999956, -7.095113581311000672 ) ) ;
#2351 = CARTESIAN_POINT ( 'NONE',  ( 2.957488688014000111, -2.712413859928999749, 1.726084346459000107 ) ) ;
#2352 = CARTESIAN_POINT ( 'NONE',  ( 10.98277446826000059, -2.518728855032000169, -8.314788219120000434 ) ) ;
#2353 = CARTESIAN_POINT ( 'NONE',  ( 6.764778664328501279, 0.6406565617180175476, -1.375763741981867794 ) ) ;
#2354 = DIRECTION ( 'NONE',  ( 1.000000000000000000, 0.000000000000000000, 0.000000000000000000 ) ) ;
#2355 = EDGE_CURVE ( 'NONE', #20484, #34155, #69072, .T. ) ;
#2357 = EDGE_CURVE ( 'NONE', #37496, #5290, #28185, .T. ) ;
#2356 = FACE_OUTER_BOUND ( 'NONE', #13486, .T. ) ;
#2358 = VERTEX_POINT ( 'NONE', #55760 ) ;
#2359 = CARTESIAN_POINT ( 'NONE',  ( 15.90000000000000036, 0.000000000000000000, 0.000000000000000000 ) ) ;
#2360 = EDGE_CURVE ( 'NONE', #41699, #50813, #19462, .T. ) ;
#2361 = CARTESIAN_POINT ( 'NONE',  ( 11.46949144726329983, -4.580206776679999869, 8.318725197575499664 ) ) ;
#2362 = CARTESIAN_POINT ( 'NONE',  ( 10.97864812944000157, 5.273131703456000352, 7.958028903907000462 ) ) ;
#2363 = DIRECTION ( 'NONE',  ( -1.000000000000000000, 0.000000000000000000, 0.000000000000000000 ) ) ;
#2364 = DIRECTION ( 'NONE',  ( 0.000000000000000000, 1.000000000000000000, 0.000000000000000000 ) ) ;
#2365 = CARTESIAN_POINT ( 'NONE',  ( 9.198965353459591654, 2.717767460002217916, 7.940252943362748894 ) ) ;
#2366 = CARTESIAN_POINT ( 'NONE',  ( 11.04749144726329924, 3.499163784537000055, -6.793273974143599681 ) ) ;
#2367 = CARTESIAN_POINT ( 'NONE',  ( 25.39409677104811891, -11.19592564009993474, -3.259886264983261839 ) ) ;
#2368 = CARTESIAN_POINT ( 'NONE',  ( 9.503038493598998215, 4.726907342723099426, -6.806856425099999441 ) ) ;
#2369 = CARTESIAN_POINT ( 'NONE',  ( 17.87583791501560526, -0.6451567829544473387, 12.58347320810647929 ) ) ;
#2370 = CARTESIAN_POINT ( 'NONE',  ( 24.25375554908000097, 3.234179890672000290, 12.21792844062999883 ) ) ;
#2371 = VECTOR ( 'NONE', #50412, 1000.000000000000114 ) ;
#2372 = CARTESIAN_POINT ( 'NONE',  ( 0.7962103212659377149, -2.967632330001188201, -1.897762364885174913 ) ) ;
#2373 = CARTESIAN_POINT ( 'NONE',  ( 10.91733584123000078, 3.256275267152000108, -6.361562334135999919 ) ) ;
#2374 = ORIENTED_EDGE ( 'NONE', *, *, #4327, .T. ) ;
#2375 = CARTESIAN_POINT ( 'NONE',  ( 8.335879440378999305, -4.310353212080000773, 9.459493062793997709 ) ) ;
#2376 = CARTESIAN_POINT ( 'NONE',  ( 18.21591247723851481, 2.819087736749464224, 13.71325046847544016 ) ) ;
#2377 = CARTESIAN_POINT ( 'NONE',  ( 23.66004879239100234, 3.393653897912999984, 13.50507458845999942 ) ) ;
#2378 = CARTESIAN_POINT ( 'NONE',  ( 10.20226357027499908, -2.879914860223000250, -7.716099591766099053 ) ) ;
#2379 = VERTEX_POINT ( 'NONE', #66236 ) ;
#2380 = CARTESIAN_POINT ( 'NONE',  ( 8.283079719592000956, 2.376526778640999815, 7.686980884243000745 ) ) ;
#2382 = CARTESIAN_POINT ( 'NONE',  ( 5.500000000000000000, 0.5415384615384001288, -2.132307692307999769 ) ) ;
#2381 = CARTESIAN_POINT ( 'NONE',  ( 8.497235841230001085, 3.789127741898000057, -9.388182174781999123 ) ) ;
#2383 = CARTESIAN_POINT ( 'NONE',  ( 16.32027728221806484, 3.351613101376117232, 11.15747237328652730 ) ) ;
#2384 = ORIENTED_EDGE ( 'NONE', *, *, #51224, .F. ) ;
#2385 = CARTESIAN_POINT ( 'NONE',  ( 10.89227882974000039, 3.998355201738000630, 9.261308739708001170 ) ) ;
#2386 = CARTESIAN_POINT ( 'NONE',  ( 18.08585342091144099, -3.015868411947693950, -13.67131429327874947 ) ) ;
#2387 = CARTESIAN_POINT ( 'NONE',  ( 10.62072335273219892, 4.397090433355999473, 6.430603299050000388 ) ) ;
#2388 = CARTESIAN_POINT ( 'NONE',  ( 10.78089914631999946, -5.735295708369000600, 7.801561210335000496 ) ) ;
#2389 = CARTESIAN_POINT ( 'NONE',  ( 7.939460911587998382, 2.865023798136999922, 6.766038833998996971 ) ) ;
#2390 = ORIENTED_EDGE ( 'NONE', *, *, #8541, .T. ) ;
#2391 = CARTESIAN_POINT ( 'NONE',  ( 11.44792571093000255, -3.801678398496999733, 11.87711516161999903 ) ) ;
#2392 = CARTESIAN_POINT ( 'NONE',  ( 1.480140132540750386, 3.408904368339106927, -0.9161175952574746040 ) ) ;
#2393 = CARTESIAN_POINT ( 'NONE',  ( 7.911796541810308447, -2.452069608993371119, 8.293693421916961128 ) ) ;
#2394 = CARTESIAN_POINT ( 'NONE',  ( 9.910792656537999790, -3.869344906782000049, 5.882544796414999944 ) ) ;
#2395 = CARTESIAN_POINT ( 'NONE',  ( 11.64122412107036908, -3.937930136014310190, -6.326756392227999015 ) ) ;
#2396 = CARTESIAN_POINT ( 'NONE',  ( 9.298797255587999189, -2.996487526130999779, 7.542485555928790220 ) ) ;
#2397 = ORIENTED_EDGE ( 'NONE', *, *, #34906, .F. ) ;
#2398 = DIRECTION ( 'NONE',  ( 0.000000000000000000, 1.000000000000000000, 0.000000000000000000 ) ) ;
#2399 = CARTESIAN_POINT ( 'NONE',  ( 12.07656516821461068, -3.100463633631699967, 6.592171857671999646 ) ) ;
#2400 = ORIENTED_EDGE ( 'NONE', *, *, #29004, .T. ) ;
#2401 = EDGE_CURVE ( 'NONE', #25841, #51664, #33749, .T. ) ;
#2402 = CARTESIAN_POINT ( 'NONE',  ( 6.999999691988000095, -11.00717859340000082, -1.432487142323000118 ) ) ;
#2403 = ORIENTED_EDGE ( 'NONE', *, *, #65572, .T. ) ;
#2404 = CARTESIAN_POINT ( 'NONE',  ( 9.751735624253999646, -3.361793157411000266, -5.915550373431999631 ) ) ;
#2405 = CARTESIAN_POINT ( 'NONE',  ( 8.555820280412000045, 2.414630869937000046, -6.801495146585999407 ) ) ;
#2406 = EDGE_CURVE ( 'NONE', #38892, #23870, #46951, .T. ) ;
#2407 = CARTESIAN_POINT ( 'NONE',  ( 9.406851002546000373, -2.832432432432000269, -6.822293592207000934 ) ) ;
#2408 = CYLINDRICAL_SURFACE ( 'NONE', #68991, 1.500000000000000000 ) ;
#2409 = CARTESIAN_POINT ( 'NONE',  ( 12.17614882354824068, 2.839252809666478861, -12.27595571488803650 ) ) ;
#2410 = CARTESIAN_POINT ( 'NONE',  ( 11.46949144726329983, -4.580206776679999869, 8.318725197575499664 ) ) ;
#2411 = CARTESIAN_POINT ( 'NONE',  ( 12.02166954483529970, -3.437903757373499847, 8.367285821793199574 ) ) ;
#2412 = VERTEX_POINT ( 'NONE', #50508 ) ;
#2413 = CYLINDRICAL_SURFACE ( 'NONE', #46311, 3.500000000000000000 ) ;
#2414 = ORIENTED_EDGE ( 'NONE', *, *, #57925, .F. ) ;
#2415 = CARTESIAN_POINT ( 'NONE',  ( 9.240543146793999796, -4.158911960977000000, 5.873536005760000123 ) ) ;
#2416 = CARTESIAN_POINT ( 'NONE',  ( 24.13791493634210994, 9.157217056292619617, 9.130314356011920651 ) ) ;
#2417 = EDGE_LOOP ( 'NONE', ( #49117, #33023, #2657, #42134 ) ) ;
#2418 = CARTESIAN_POINT ( 'NONE',  ( 12.33234491188480320, -1.934664193338951899, -12.45058764867823164 ) ) ;
#2419 = CARTESIAN_POINT ( 'NONE',  ( 11.38379707368349969, 3.433355370490100533, 8.490052513816499058 ) ) ;
#2420 = CARTESIAN_POINT ( 'NONE',  ( 10.19122055961999962, -3.990707710465999813, -5.651373900265999950 ) ) ;
#2421 = CARTESIAN_POINT ( 'NONE',  ( 6.513359839683332098, -1.310679582531389276, 0.7554284705563443225 ) ) ;
#2422 = CARTESIAN_POINT ( 'NONE',  ( 18.01908732848200145, -11.78185846591000008, 3.459210216787000025 ) ) ;
#2423 = CARTESIAN_POINT ( 'NONE',  ( 7.474316494907240482, -3.999963201012326053, 8.979508826873761507 ) ) ;
#2424 = CARTESIAN_POINT ( 'NONE',  ( 5.000000000000000000, 0.000000000000000000, 0.000000000000000000 ) ) ;
#2425 = CARTESIAN_POINT ( 'NONE',  ( 18.13994946422174337, 0.2205037192104047084, -12.69742880170240085 ) ) ;
#2426 = B_SPLINE_CURVE_WITH_KNOTS ( 'NONE', 3,
 ( #61022, #4256, #60674, #7885, #19054, #34468, #41669, #31196, #50876, #7527, #25934, #25594, #29219, #52501, #12788, #4598, #34117, #41330, #68223, #29574, #2973, #44953, #45640, #14762, #62975, #50531, #66943, #2292, #46919, #47263, #30841, #15100, #45294, #36424, #66257, #28882, #66601, #57739, #9850, #34805, #18719, #50192, #36080, #18378, #39700, #13484, #40053, #56115, #13139, #61364, #15786, #27662, #43399, #10882, #22052, #43044, #32561, #58774, #21710, #51, #64010, #10198, #37798, #21035, #64348, #53874, #59121, #48981, #11224, #26284, #58095, #42019, #739, #16466, #32228, #68919, #38134, #59462, #5974, #36773, #27314, #20690, #32903, #63321, #48639, #64698, #53540, #5631, #42368, #15449, #5293, #393, #31876 ),
 .UNSPECIFIED., .F., .F.,
 ( 4, 2, 2, 2, 2, 2, 2, 2, 2, 1, 1, 2, 2, 2, 2, 2, 2, 2, 2, 2, 2, 2, 2, 2, 2, 2, 2, 2, 2, 2, 2, 2, 2, 1, 1, 2, 2, 2, 2, 1, 2, 2, 2, 2, 2, 2, 2, 2, 4 ),
 ( 0.000000000000000000, 0.03124999999999071576, 0.06249999999998143152, 0.09374999999997214728, 0.1093749999999674982, 0.1249999999999628630, 0.1562499999999562850, 0.1718749999999529821, 0.1874999999999496791, 0.2031249999999463762, 0.2109374999999447109, 0.2148437499999447942, 0.2187499999999448774, 0.2499999999999507061, 0.2656249999999529265, 0.2734374999999541478, 0.2812499999999553135, 0.2968749999999561462, 0.3124999999999569789, 0.3437499999999587552, 0.3593749999999590883, 0.3749999999999593658, 0.4062499999999609757, 0.4374999999999625300, 0.4999999999999656941, 0.5312499999999672484, 0.5624999999999689138, 0.5937499999999704681, 0.6093749999999715783, 0.6249999999999726885, 0.6562499999999740208, 0.6718749999999746869, 0.6874999999999753530, 0.7031249999999760192, 0.7109374999999763522, 0.7148437499999772404, 0.7187499999999782396, 0.7499999999999861222, 0.7656249999999907851, 0.7734374999999930056, 0.7773437499999942268, 0.7812499999999953371, 0.7968749999999964473, 0.8124999999999974465, 0.8437499999999995559, 0.8593750000000005551, 0.8750000000000015543, 0.9375000000000007772, 1.000000000000000000 ),
 .UNSPECIFIED. ) ;
#2427 = AXIS2_PLACEMENT_3D ( 'NONE', #6372, #7417, #38191 ) ;
#2428 = DIRECTION ( 'NONE',  ( -1.000000000000000000, 0.000000000000000000, 0.000000000000000000 ) ) ;
#2429 = CARTESIAN_POINT ( 'NONE',  ( 7.775614158771000817, 4.636729845879000500, 9.378977473003999421 ) ) ;
#2430 = ORIENTED_EDGE ( 'NONE', *, *, #48721, .F. ) ;
#2431 = CARTESIAN_POINT ( 'NONE',  ( 8.099999999999999645, 0.000000000000000000, 0.000000000000000000 ) ) ;
#2432 = CYLINDRICAL_SURFACE ( 'NONE', #23842, 13.17499999999999893 ) ;
#2433 = CARTESIAN_POINT ( 'NONE',  ( 23.99192513437000329, -3.573328852826999746, 12.95691943739999985 ) ) ;
#2434 = CARTESIAN_POINT ( 'NONE',  ( 17.55505043854143565, 3.199698446519374073, 12.18695736643652516 ) ) ;
#2435 = AXIS2_PLACEMENT_3D ( 'NONE', #58659, #5519, #26859 ) ;
#2436 = CARTESIAN_POINT ( 'NONE',  ( 18.48724299199999876, 3.206939682244000167, -12.14698705996000072 ) ) ;
#2438 = EDGE_CURVE ( 'NONE', #59495, #227, #18014, .T. ) ;
#2437 = CARTESIAN_POINT ( 'NONE',  ( 9.815201913989998417, 2.813632032385000148, 8.848857341496000117 ) ) ;
#2439 = CARTESIAN_POINT ( 'NONE',  ( 5.500000000000000000, 0.000000000000000000, 0.000000000000000000 ) ) ;
#2440 = ADVANCED_FACE ( 'NONE', ( #49466 ), #64224, .F. ) ;
#2441 = CARTESIAN_POINT ( 'NONE',  ( 8.734997988989999129, 3.937347817007940343, 6.633566614602599998 ) ) ;
#2442 = EDGE_CURVE ( 'NONE', #19263, #35108, #66140, .T. ) ;
#2443 = EDGE_LOOP ( 'NONE', ( #13712, #30939, #31368, #19628 ) ) ;
#2444 = CARTESIAN_POINT ( 'NONE',  ( 12.30671156051923809, -2.122656121997153367, 12.53154589464477731 ) ) ;
#2445 = CARTESIAN_POINT ( 'NONE',  ( 9.956950584426998319, -3.655872208659600275, -6.704208565179699875 ) ) ;
#2446 = CARTESIAN_POINT ( 'NONE',  ( 10.51655086620999846, 4.930662802525000110, 8.573584269714999095 ) ) ;
#2447 = DIRECTION ( 'NONE',  ( 0.000000000000000000, -1.000000000000000000, 0.000000000000000000 ) ) ;
#2448 = B_SPLINE_CURVE_WITH_KNOTS ( 'NONE', 3,
 ( #68583, #16486, #37467, #47282 ),
 .UNSPECIFIED., .F., .F.,
 ( 4, 4 ),
 ( 0.000000000000000000, 0.1494581667962512628 ),
 .UNSPECIFIED. ) ;
#2449 = CARTESIAN_POINT ( 'NONE',  ( 10.52226222744799955, 3.119510978356100139, -8.225278704382400718 ) ) ;
#2450 = CARTESIAN_POINT ( 'NONE',  ( 12.76392908090536515, 0.6239794389693666954, 12.67935706666152740 ) ) ;
#2451 = CARTESIAN_POINT ( 'NONE',  ( 7.262114158771001193, 4.847807297114000491, 9.065373753110998578 ) ) ;
#2452 = CARTESIAN_POINT ( 'NONE',  ( 10.96080777006000062, 2.054568739078000306, 7.810084630238000258 ) ) ;
#2453 = CARTESIAN_POINT ( 'NONE',  ( 12.21847001913369191, 2.284010606415769029, 12.49926433191011377 ) ) ;
#2454 = ORIENTED_EDGE ( 'NONE', *, *, #55405, .T. ) ;
#2455 = CARTESIAN_POINT ( 'NONE',  ( 9.684729719592999331, 2.370176859044999862, -6.912649125838000508 ) ) ;
#2456 = CARTESIAN_POINT ( 'NONE',  ( 10.15303300763299887, 4.787165141710600480, -8.325626572044798834 ) ) ;
#2457 = EDGE_CURVE ( 'NONE', #40201, #63789, #28641, .T. ) ;
#2458 = CARTESIAN_POINT ( 'NONE',  ( 13.50000000000000178, 11.75776087185409402, 2.440894935389088527 ) ) ;
#2460 = CARTESIAN_POINT ( 'NONE',  ( 24.92848013445852828, 11.55907645929356775, 3.214033862752819992 ) ) ;
#2459 = CARTESIAN_POINT ( 'NONE',  ( 9.587879440377001572, -3.762710033898000184, 8.787827024292999667 ) ) ;
#2461 = CARTESIAN_POINT ( 'NONE',  ( 10.33729229006299910, -3.131390070940299974, 8.004340253666999416 ) ) ;
#2462 = CARTESIAN_POINT ( 'NONE',  ( 11.41672066707849886, -3.258843737379200078, -7.051685395375099752 ) ) ;
#2463 = ORIENTED_EDGE ( 'NONE', *, *, #6826, .F. ) ;
#2464 = AXIS2_PLACEMENT_3D ( 'NONE', #38344, #48498, #43251 ) ;
#2465 = CARTESIAN_POINT ( 'NONE',  ( 1.829975240918999990, 3.378571531507999826, -0.5657499728117999505 ) ) ;
#2466 = CARTESIAN_POINT ( 'NONE',  ( 18.04063798913343675, -0.3934994367753943956, -12.69179478357233748 ) ) ;
#2467 = CARTESIAN_POINT ( 'NONE',  ( 20.75138802851920161, -5.760713961201000544, 0.000000000000000000 ) ) ;
#2468 = CARTESIAN_POINT ( 'NONE',  ( 17.59634971247464819, -3.125000000000000444, 13.52084437902333391 ) ) ;
#2469 = CARTESIAN_POINT ( 'NONE',  ( 24.60999195273300089, -12.22061417745999989, 3.051130890667999918 ) ) ;
#2470 = CARTESIAN_POINT ( 'NONE',  ( 17.59662294266148663, -1.876036575741765189, -13.78611707749648119 ) ) ;
#2471 = LINE ( 'NONE', #35333, #23027 ) ;
#2472 = FACE_OUTER_BOUND ( 'NONE', #39066, .T. ) ;
#2473 = CARTESIAN_POINT ( 'NONE',  ( 10.06489140842196406, 5.349900232312646331, -7.500006335289779003 ) ) ;
#2474 = ORIENTED_EDGE ( 'NONE', *, *, #38115, .F. ) ;
#2475 = CARTESIAN_POINT ( 'NONE',  ( 9.587885841227999251, 3.762712042852999872, 8.787816121229999666 ) ) ;
#2476 = DIRECTION ( 'NONE',  ( 1.000000000000000000, -2.772811999483000412E-10, 2.750922296957000062E-11 ) ) ;
#2477 = LINE ( 'NONE', #56654, #64243 ) ;
#2478 = CONICAL_SURFACE ( 'NONE', #39314, 11.45000430352999921, 0.7853991313766258697 ) ;
#2479 = CARTESIAN_POINT ( 'NONE',  ( 7.800894438721999613, -3.218815632501999868, 6.398977300879999497 ) ) ;
#2480 = CARTESIAN_POINT ( 'NONE',  ( 0.7467001509839000795, -0.1589293563100999951, 3.588678346333000313 ) ) ;
#2481 = ORIENTED_EDGE ( 'NONE', *, *, #29770, .T. ) ;
#2482 = CARTESIAN_POINT ( 'NONE',  ( 17.60000000085000238, 12.11987927271999865, -3.159802730921999814 ) ) ;
#2483 = CARTESIAN_POINT ( 'NONE',  ( 10.79325778752896525, -5.089851028638672226, 5.099140771708407627 ) ) ;
#2484 = CARTESIAN_POINT ( 'NONE',  ( 10.07102359808000003, 4.042170458878000083, 8.920189456109998360 ) ) ;
#2485 = EDGE_CURVE ( 'NONE', #16376, #32335, #50301, .T. ) ;
#2486 = CARTESIAN_POINT ( 'NONE',  ( 10.60026222744819790, 3.225465054973100099, 6.861998062869400172 ) ) ;
#2487 = CARTESIAN_POINT ( 'NONE',  ( 7.100000000000000533, 5.326087788487999575, -7.247035225330000330 ) ) ;
#2488 = CARTESIAN_POINT ( 'NONE',  ( 10.87946694038000039, -2.817416132545000007, -6.828662897514999663 ) ) ;
#2489 = EDGE_CURVE ( 'NONE', #62373, #67945, #62785, .T. ) ;
#2490 = DIRECTION ( 'NONE',  ( 0.000000000000000000, -1.000000000000000000, 0.000000000000000000 ) ) ;
#2491 = CARTESIAN_POINT ( 'NONE',  ( 24.50549018585800098, 12.34681877080999968, 3.084981659446000002 ) ) ;
#2492 = CARTESIAN_POINT ( 'NONE',  ( 12.18009334795439003, -2.513081858656105450, 12.44854102044225463 ) ) ;
#2493 = CARTESIAN_POINT ( 'NONE',  ( 7.973714672046428475, 2.314332798270127167, 7.004429797696275273 ) ) ;
#2494 = VERTEX_POINT ( 'NONE', #37694 ) ;
#2495 = CARTESIAN_POINT ( 'NONE',  ( 18.22053876895019542, -2.807780685761766204, 13.71555663160087057 ) ) ;
#2496 = CARTESIAN_POINT ( 'NONE',  ( 11.13349010443639919, -2.725546193138000284, -7.595309363461700158 ) ) ;
#2497 = ORIENTED_EDGE ( 'NONE', *, *, #38767, .F. ) ;
#2498 = VERTEX_POINT ( 'NONE', #6564 ) ;
#2499 = CARTESIAN_POINT ( 'NONE',  ( 25.26127586260790281, -2.660441985988178715, -11.37584977663462205 ) ) ;
#2500 = CARTESIAN_POINT ( 'NONE',  ( 4.149992563291999836, 0.2617923565147994291, -1.999946284944287722 ) ) ;
#2501 = DIRECTION ( 'NONE',  ( 0.000000000000000000, 0.7158784314710772145, 0.6982249432342778617 ) ) ;
#2502 = CARTESIAN_POINT ( 'NONE',  ( 9.533434135307000901, 2.564753581125000181, 6.150586364588000343 ) ) ;
#2503 = B_SPLINE_CURVE_WITH_KNOTS ( 'NONE', 3,
 ( #58616, #12108, #11748, #54406 ),
 .UNSPECIFIED., .F., .F.,
 ( 4, 4 ),
 ( 0.000000000000000000, 1.000000000000000000 ),
 .UNSPECIFIED. ) ;
#2504 = CARTESIAN_POINT ( 'NONE',  ( 10.68375192593000023, 4.547306763790999184, -8.749120576764999768 ) ) ;
#2505 = CARTESIAN_POINT ( 'NONE',  ( 7.000000000000000000, -9.370210309074998634, -5.370210309075000410 ) ) ;
#2506 = CARTESIAN_POINT ( 'NONE',  ( 11.09999999999999964, 7.281355511280001025, -6.286510895624999762 ) ) ;
#2507 = CARTESIAN_POINT ( 'NONE',  ( 17.60275121352128025, 0.7181168112306527407, -12.57951960855069551 ) ) ;
#2508 = CARTESIAN_POINT ( 'NONE',  ( 10.09133114265999964, -2.216726401468000152, -8.007130485478999304 ) ) ;
#2509 = CARTESIAN_POINT ( 'NONE',  ( 10.98688827724838113, 5.367975154760830314, -6.994477628651915246 ) ) ;
#2510 = DIRECTION ( 'NONE',  ( -1.000000000000000000, 0.000000000000000000, 0.000000000000000000 ) ) ;
#2511 = VERTEX_POINT ( 'NONE', #988 ) ;
#2512 = CARTESIAN_POINT ( 'NONE',  ( 7.364999999998000035, 2.649999999999999911, -7.500000000000000000 ) ) ;
#2513 = VECTOR ( 'NONE', #53549, 1000.000000000000227 ) ;
#2514 =( NAMED_UNIT ( * ) SI_UNIT ( $, .STERADIAN. ) SOLID_ANGLE_UNIT ( ) );
#2515 = FACE_OUTER_BOUND ( 'NONE', #56149, .T. ) ;
#2516 = DIRECTION ( 'NONE',  ( 1.000000000000000000, 0.000000000000000000, 0.000000000000000000 ) ) ;
#2517 = CARTESIAN_POINT ( 'NONE',  ( 10.49490035061499782, 4.340961869598300105, -8.732935057095000175 ) ) ;
#2518 = CARTESIAN_POINT ( 'NONE',  ( 12.63832872341678204, 3.228981699441171305, 13.62254385108541754 ) ) ;
#2519 = CARTESIAN_POINT ( 'NONE',  ( 10.98286725694000054, -3.998514182530999772, 9.091066422484001208 ) ) ;
#2520 = VERTEX_POINT ( 'NONE', #59359 ) ;
#2521 = CARTESIAN_POINT ( 'NONE',  ( 12.60485626873164300, 0.5921620643864188294, -12.68141136813213166 ) ) ;
#2522 = CARTESIAN_POINT ( 'NONE',  ( 12.76393046405280174, -0.6239795106976188110, 13.88114172264461210 ) ) ;
#2523 = ADVANCED_FACE ( 'NONE', ( #26872, #11808 ), #641, .F. ) ;
#2524 = ORIENTED_EDGE ( 'NONE', *, *, #11348, .F. ) ;
#2525 = FACE_OUTER_BOUND ( 'NONE', #20210, .T. ) ;
#2526 = CARTESIAN_POINT ( 'NONE',  ( 13.50018479229300006, -11.60142623882999935, -2.415183939829000259 ) ) ;
#2527 = CARTESIAN_POINT ( 'NONE',  ( 23.73943898212699821, -3.322335461309999793, -13.28161925880999839 ) ) ;
#2528 = FACE_OUTER_BOUND ( 'NONE', #28917, .T. ) ;
#2529 = CARTESIAN_POINT ( 'NONE',  ( 8.383148997457999130, -5.167567567567999731, 6.822293592207000934 ) ) ;
#2530 = CARTESIAN_POINT ( 'NONE',  ( 11.07076166751999935, 7.299647376920999520, -6.238566460401999691 ) ) ;
#2531 = CARTESIAN_POINT ( 'NONE',  ( 0.3923104132283999901, -3.376221432737999795, -1.056438743269999980 ) ) ;
#2532 = FACE_OUTER_BOUND ( 'NONE', #25345, .T. ) ;
#2533 = CARTESIAN_POINT ( 'NONE',  ( 12.65065493613386138, 3.183300664725533746, 12.19125106909030798 ) ) ;
#2534 = CARTESIAN_POINT ( 'NONE',  ( 9.881332132140999036, -4.333399685216000385, -9.088699530815999239 ) ) ;
#2535 = CARTESIAN_POINT ( 'NONE',  ( 11.66287348028854964, 3.238044298475899918, -7.911973420841600380 ) ) ;
#2536 = FACE_OUTER_BOUND ( 'NONE', #1087, .T. ) ;
#2537 = CARTESIAN_POINT ( 'NONE',  ( 11.52677869730533011, 3.596497913043499750, -6.704332466833498927 ) ) ;
#2538 = EDGE_CURVE ( 'NONE', #56515, #56175, #27023, .T. ) ;
#2539 = CARTESIAN_POINT ( 'NONE',  ( 9.581988259785999773, 3.850604015305000072, -8.631996151823999597 ) ) ;
#2541 = CARTESIAN_POINT ( 'NONE',  ( 10.25832334068999963, -3.359820126011999974, 4.530776491823000462 ) ) ;
#2540 = CARTESIAN_POINT ( 'NONE',  ( 9.317138961223998095, -3.281636118526699786, 7.014550357332099750 ) ) ;
#2542 = CARTESIAN_POINT ( 'NONE',  ( 23.59299099590867499, -13.38589721419561407, 4.028864339703104314 ) ) ;
#2543 = VERTEX_POINT ( 'NONE', #33149 ) ;
#2544 = EDGE_CURVE ( 'NONE', #23293, #2626, #5810, .T. ) ;
#2545 = CARTESIAN_POINT ( 'NONE',  ( 18.29999330150736014, -11.02846243710336616, 3.754394858745019103 ) ) ;
#2546 = CARTESIAN_POINT ( 'NONE',  ( 11.11845396862999991, -5.767021056207999763, 7.178419201465000121 ) ) ;
#2547 = CARTESIAN_POINT ( 'NONE',  ( 9.806988259785999418, 3.868581654116200141, 6.504223158184999853 ) ) ;
#2548 = CARTESIAN_POINT ( 'NONE',  ( 10.16407857760462718, 3.262163830883630489, -7.970244675898661590 ) ) ;
#2549 = CARTESIAN_POINT ( 'NONE',  ( 23.56666365135700403, 11.07911597677999360, -4.076188921367005058 ) ) ;
#2550 = CYLINDRICAL_SURFACE ( 'NONE', #39808, 0.6250000000000005551 ) ;
#2551 = VERTEX_POINT ( 'NONE', #11127 ) ;
#2552 = CARTESIAN_POINT ( 'NONE',  ( 10.11188779216199940, -2.816792857868000155, -7.926693309523199282 ) ) ;
#2553 = AXIS2_PLACEMENT_3D ( 'NONE', #7891, #67894, #51816 ) ;
#2554 = DIRECTION ( 'NONE',  ( 1.000000000000000000, 0.000000000000000000, 0.000000000000000000 ) ) ;
#2555 = CARTESIAN_POINT ( 'NONE',  ( 5.044604931988000196, 0.1454693244516999939, 1.365796648849999961 ) ) ;
#2556 = PRODUCT_DEFINITION_SHAPE ( 'NONE', 'NONE',  #35119 ) ;
#2557 = CARTESIAN_POINT ( 'NONE',  ( 17.65148079338494824, 1.767134912084544318, -12.47546541983269286 ) ) ;
#2558 = CARTESIAN_POINT ( 'NONE',  ( 10.44728840309080020, 2.899999999999999911, 6.305985889617041984 ) ) ;
#2559 = DIRECTION ( 'NONE',  ( 0.000000000000000000, -1.000000000000000000, 0.000000000000000000 ) ) ;
#2560 = CARTESIAN_POINT ( 'NONE',  ( 10.55518582084299872, 3.433275964779900047, -6.844925608615599621 ) ) ;
#2561 = CARTESIAN_POINT ( 'NONE',  ( 3.500000000000000000, 0.000000000000000000, 0.000000000000000000 ) ) ;
#2562 = CARTESIAN_POINT ( 'NONE',  ( 9.612156140204000110, -5.332339947063000629, -7.851654145788001138 ) ) ;
#2563 = CARTESIAN_POINT ( 'NONE',  ( 25.47111570701200023, 11.11941859758999840, 3.299547261379999874 ) ) ;
#2564 = EDGE_CURVE ( 'NONE', #20189, #34088, #61198, .T. ) ;
#2565 = ORIENTED_EDGE ( 'NONE', *, *, #37644, .F. ) ;
#2566 = DIRECTION ( 'NONE',  ( 0.000000000000000000, 1.000000000000000000, 0.000000000000000000 ) ) ;
#2567 = CARTESIAN_POINT ( 'NONE',  ( 12.44165070291072261, -0.6323113780857178012, -13.98571806661953332 ) ) ;
#2568 = CARTESIAN_POINT ( 'NONE',  ( 8.241912900173000267, 4.599999999999999645, 6.117539782833000928 ) ) ;
#2569 = CARTESIAN_POINT ( 'NONE',  ( 25.20464492906199894, -8.548379336130999206, -7.995593105742999640 ) ) ;
#2570 = CARTESIAN_POINT ( 'NONE',  ( 13.09269116698435909, -11.52576810756808356, -1.696811579065486741 ) ) ;
#2571 = CARTESIAN_POINT ( 'NONE',  ( 23.59999445750599989, -13.22316420035999940, -4.267800004853000040 ) ) ;
#2573 = AXIS2_PLACEMENT_3D ( 'NONE', #66289, #18414, #39739 ) ;
#2572 = CARTESIAN_POINT ( 'NONE',  ( 4.599999999999999645, -1.760910691117812954, -12.47634535983622861 ) ) ;
#2574 = ORIENTED_EDGE ( 'NONE', *, *, #7850, .F. ) ;
#2575 = DIRECTION ( 'NONE',  ( 1.000000000000000000, 0.000000000000000000, 0.000000000000000000 ) ) ;
#2576 = CARTESIAN_POINT ( 'NONE',  ( 18.14815926393670154, 2.301857555364728913, -13.71350736626465405 ) ) ;
#2577 = ORIENTED_EDGE ( 'NONE', *, *, #23518, .T. ) ;
#2578 = CARTESIAN_POINT ( 'NONE',  ( 0.2500098862125000321, 0.000000000000000000, 0.000000000000000000 ) ) ;
#2579 = CARTESIAN_POINT ( 'NONE',  ( 24.74120093721589342, 3.111623860952520193, 11.77170576849003147 ) ) ;
#2580 = CARTESIAN_POINT ( 'NONE',  ( 9.061929719594999710, 4.092867382745001059, -5.937785237406000505 ) ) ;
#2581 = CARTESIAN_POINT ( 'NONE',  ( 24.13791496213264409, -12.48569266960873136, 3.365225404910305418 ) ) ;
#2582 = CARTESIAN_POINT ( 'NONE',  ( 10.72702344389999851, -5.004394439171999664, -6.890449684422599752 ) ) ;
#2583 = FACE_OUTER_BOUND ( 'NONE', #6984, .T. ) ;
#2584 = CARTESIAN_POINT ( 'NONE',  ( 10.91666666666863073, -5.385217356302812952, 7.523132604489776831 ) ) ;
#2585 = ORIENTED_EDGE ( 'NONE', *, *, #6064, .F. ) ;
#2586 = CARTESIAN_POINT ( 'NONE',  ( 8.642077642326000841, -2.899999999999999911, 6.463854830420999953 ) ) ;
#2587 = CARTESIAN_POINT ( 'NONE',  ( 5.600000001140999828, 0.000000000000000000, 0.000000000000000000 ) ) ;
#2588 = CARTESIAN_POINT ( 'NONE',  ( 9.544414158773999901, 2.173570076733999823, -8.023168429484000441 ) ) ;
#2589 = ORIENTED_EDGE ( 'NONE', *, *, #20575, .F. ) ;
#2590 = CARTESIAN_POINT ( 'NONE',  ( 10.72303311070000120, 3.890114357827999747, -8.859327677199999584 ) ) ;
#2591 = CARTESIAN_POINT ( 'NONE',  ( 25.39991778581708814, 10.74016754877895430, 3.821986718425039786 ) ) ;
#2592 = ORIENTED_EDGE ( 'NONE', *, *, #2620, .T. ) ;
#2593 = CARTESIAN_POINT ( 'NONE',  ( 9.126063610504999701, 4.468346739194200445, 6.458661544034999480 ) ) ;
#2594 = CARTESIAN_POINT ( 'NONE',  ( 18.27407156835994684, -2.576234207239483709, -12.33383912514346648 ) ) ;
#2595 = CARTESIAN_POINT ( 'NONE',  ( 10.98960529797957797, 5.570865012723525744, -4.946148922830412964 ) ) ;
#2596 = DIRECTION ( 'NONE',  ( 0.000000000000000000, 0.000000000000000000, -1.000000000000000000 ) ) ;
#2597 = FACE_OUTER_BOUND ( 'NONE', #58221, .T. ) ;
#2598 = CARTESIAN_POINT ( 'NONE',  ( 10.26788779216199821, 4.929030047862200448, 7.164969140522200242 ) ) ;
#2599 = EDGE_CURVE ( 'NONE', #35905, #43884, #68338, .T. ) ;
#2600 = CARTESIAN_POINT ( 'NONE',  ( 9.407593387382531702, -2.496308800233906222, 8.374379778997440127 ) ) ;
#2602 = EDGE_CURVE ( 'NONE', #12398, #46125, #32801, .T. ) ;
#2601 = B_SPLINE_CURVE_WITH_KNOTS ( 'NONE', 3,
 ( #29683, #67054, #20883, #26826 ),
 .UNSPECIFIED., .F., .F.,
 ( 4, 4 ),
 ( 0.000000000000000000, 1.000000000000000000 ),
 .UNSPECIFIED. ) ;
#2603 = ORIENTED_EDGE ( 'NONE', *, *, #7566, .T. ) ;
#2604 = CARTESIAN_POINT ( 'NONE',  ( 11.44571737393083133, 2.988799872700407700, 6.726238946114240669 ) ) ;
#2605 = CARTESIAN_POINT ( 'NONE',  ( 11.26847444708000090, 2.565620268983000329, -7.116623294300999270 ) ) ;
#2606 = CARTESIAN_POINT ( 'NONE',  ( 10.95262606961999907, -5.154900359228999918, -5.178689578204999755 ) ) ;
#2607 = CARTESIAN_POINT ( 'NONE',  ( 12.25852519399115614, 2.998253127629454617, -13.67519035003951267 ) ) ;
#2608 = CIRCLE ( 'NONE', #35015, 12.60000000000000142 ) ;
#2609 = CARTESIAN_POINT ( 'NONE',  ( 10.49490035061499782, -3.659038130401700339, -8.732935057095000175 ) ) ;
#2610 = CARTESIAN_POINT ( 'NONE',  ( 9.629020610622001541, -5.794331084664000819, 7.414872097535999629 ) ) ;
#2611 = CARTESIAN_POINT ( 'NONE',  ( 18.18333308066189247, -0.3651687365794509810, 13.99525266148724256 ) ) ;
#2612 = CARTESIAN_POINT ( 'NONE',  ( 18.17891623994083616, -2.457256301358912154, 12.46146663849685865 ) ) ;
#2613 = EDGE_LOOP ( 'NONE', ( #63715, #59921, #49367 ) ) ;
#2614 = ORIENTED_EDGE ( 'NONE', *, *, #19176, .T. ) ;
#2615 = CARTESIAN_POINT ( 'NONE',  ( 9.983079719591000156, 5.002683760508999988, -8.912673867568997821 ) ) ;
#2616 = CARTESIAN_POINT ( 'NONE',  ( 5.500000000000000000, 12.43893545635000031, 2.828937028792000152 ) ) ;
#2617 = CARTESIAN_POINT ( 'NONE',  ( 12.18408897593004347, -2.571470745484657261, 13.65804488218840618 ) ) ;
#2618 = DIRECTION ( 'NONE',  ( 0.7071074108314172602, 0.7071061515411172227, -4.731322706660111483E-09 ) ) ;
#2619 = CARTESIAN_POINT ( 'NONE',  ( 23.51521487668100008, 10.46906073003999893, -9.496281516038997950 ) ) ;
#2620 = EDGE_CURVE ( 'NONE', #53074, #40500, #38204, .T. ) ;
#2621 = CARTESIAN_POINT ( 'NONE',  ( 18.26242637978999994, -2.744390477411999818, -11.56740641610000075 ) ) ;
#2623 = CARTESIAN_POINT ( 'NONE',  ( 10.96256856629999987, -6.761408932091000246, 5.456131228213999762 ) ) ;
#2622 = CARTESIAN_POINT ( 'NONE',  ( 9.853076168957999315, -4.579425901182000658, 6.516130052788599691 ) ) ;
#2624 =( GEOMETRIC_REPRESENTATION_CONTEXT ( 3 ) GLOBAL_UNCERTAINTY_ASSIGNED_CONTEXT ( ( #31116 ) ) GLOBAL_UNIT_ASSIGNED_CONTEXT ( ( #41969, #4210, #20298 ) ) REPRESENTATION_CONTEXT ( 'NONE', 'WORKASPACE' ) );
#2625 = CARTESIAN_POINT ( 'NONE',  ( 12.09213512191444195, -4.803449168604846164, 7.825049263296810054 ) ) ;
#2626 = VERTEX_POINT ( 'NONE', #43639 ) ;
#2627 = ADVANCED_FACE ( 'NONE', ( #54464, #1324, #48188, #65291 ), #53088, .T. ) ;
#2628 = CARTESIAN_POINT ( 'NONE',  ( 10.89610713867999969, -2.705901429593000174, 4.900545273262999935 ) ) ;
#2629 = VECTOR ( 'NONE', #3454, 1000.000000000000000 ) ;
#2630 = DIRECTION ( 'NONE',  ( 1.000000000000000000, 0.000000000000000000, 0.000000000000000000 ) ) ;
#2631 = B_SPLINE_CURVE_WITH_KNOTS ( 'NONE', 3,
 ( #3979, #24641, #39692, #14155 ),
 .UNSPECIFIED., .F., .F.,
 ( 4, 4 ),
 ( 0.000000000000000000, 1.000000000000000000 ),
 .UNSPECIFIED. ) ;
#2632 = CARTESIAN_POINT ( 'NONE',  ( 17.66769993992418364, 0.6148490057825420907, 12.67995724530759816 ) ) ;
#2633 = DIRECTION ( 'NONE',  ( 0.000000000000000000, 1.000000000000000000, 0.000000000000000000 ) ) ;
#2634 = CARTESIAN_POINT ( 'NONE',  ( 4.149992563291999836, -1.999946284944288388, 0.2617923565147958764 ) ) ;
#2635 = ORIENTED_EDGE ( 'NONE', *, *, #64371, .T. ) ;
#2637 = CARTESIAN_POINT ( 'NONE',  ( 12.70687399449098365, -1.760978113263731881, -12.47633584387829941 ) ) ;
#2636 = CARTESIAN_POINT ( 'NONE',  ( 10.95375739185000086, -5.155102718910000270, 5.173734077849999835 ) ) ;
#2638 = CARTESIAN_POINT ( 'NONE',  ( 9.401145280412999128, 3.927090956378999742, -9.230892435423001530 ) ) ;
#2639 = CARTESIAN_POINT ( 'NONE',  ( 4.000000000000000000, -2.750000000000000000, 0.000000000000000000 ) ) ;
#2640 = CARTESIAN_POINT ( 'NONE',  ( 10.54272335273199879, 4.444874504667400750, 6.301916924546999255 ) ) ;
#2641 = CARTESIAN_POINT ( 'NONE',  ( 10.31905590579000176, 2.899999999999999911, -6.571291218949999902 ) ) ;
#2642 = CARTESIAN_POINT ( 'NONE',  ( 18.23777342769881926, -3.105166803968429257, -11.92942855515249967 ) ) ;
#2643 = CARTESIAN_POINT ( 'NONE',  ( 2.209063718793000231, 3.425644328890999901, 0.01271980431870000164 ) ) ;
#2644 = ORIENTED_EDGE ( 'NONE', *, *, #42100, .T. ) ;
#2645 = CARTESIAN_POINT ( 'NONE',  ( 12.38211335778635558, 0.5846869236304474970, -12.58643362292763612 ) ) ;
#2646 = CARTESIAN_POINT ( 'NONE',  ( 10.98768472639999949, 2.860900986606000007, -4.945212061661000469 ) ) ;
#2647 = CARTESIAN_POINT ( 'NONE',  ( 11.04968150330033438, -2.750318496699665438, -6.534572094925334085 ) ) ;
#2648 = CARTESIAN_POINT ( 'NONE',  ( 24.41456973790700147, 3.182129207855000086, -12.02370739584000070 ) ) ;
#2649 = SURFACE_STYLE_USAGE ( .BOTH. , #56826 ) ;
#2650 = ORIENTED_EDGE ( 'NONE', *, *, #12277, .F. ) ;
#2651 = CARTESIAN_POINT ( 'NONE',  ( 6.731620200880000127, 0.7284491026353999699, 1.103547660897999938 ) ) ;
#2652 = CARTESIAN_POINT ( 'NONE',  ( 10.90000004630000063, 9.856474695503001371, 5.627825000517000298 ) ) ;
#2654 = CARTESIAN_POINT ( 'NONE',  ( 10.56498513754044311, 5.349957030113837497, -7.500000808964303545 ) ) ;
#2653 = CARTESIAN_POINT ( 'NONE',  ( 8.574101921698924045, -3.981802517092035476, 5.760066862916072949 ) ) ;
#2655 = CARTESIAN_POINT ( 'NONE',  ( 7.804619354695629063, 2.996383457933911032, 6.547394516041353363 ) ) ;
#2656 = DIRECTION ( 'NONE',  ( 0.000000000000000000, 1.000000000000000000, 0.000000000000000000 ) ) ;
#2657 = ORIENTED_EDGE ( 'NONE', *, *, #16478, .F. ) ;
#2658 = AXIS2_PLACEMENT_3D ( 'NONE', #67437, #41568, #62877 ) ;
#2659 = DIRECTION ( 'NONE',  ( 0.000000000000000000, 0.8765967884314782577, -0.4812255921203881792 ) ) ;
#2660 = ORIENTED_EDGE ( 'NONE', *, *, #2599, .F. ) ;
#2661 = FACE_OUTER_BOUND ( 'NONE', #54085, .T. ) ;
#2662 = CARTESIAN_POINT ( 'NONE',  ( 7.464688980125999684, -4.351670788182000038, 8.977200644264000218 ) ) ;
#2663 = CARTESIAN_POINT ( 'NONE',  ( 18.14440149583523620, -0.4259565731506483321, -13.99353270933016979 ) ) ;
#2664 = EDGE_CURVE ( 'NONE', #64650, #54437, #48242, .T. ) ;
#2665 = EDGE_CURVE ( 'NONE', #30301, #35342, #42003, .T. ) ;
#2666 = ORIENTED_EDGE ( 'NONE', *, *, #6462, .F. ) ;
#2667 = CARTESIAN_POINT ( 'NONE',  ( 10.92122291580152371, 9.608538131000051052, -5.970078283598937219 ) ) ;
#2668 = CARTESIAN_POINT ( 'NONE',  ( 11.09999999999999964, -5.299999999999999822, 6.469505845987999493 ) ) ;
#2669 = CARTESIAN_POINT ( 'NONE',  ( 10.90000000000000036, 5.283926297003000094, 7.082827057608000132 ) ) ;
#2670 = DIRECTION ( 'NONE',  ( 0.000000000000000000, -1.000000000000000000, 0.000000000000000000 ) ) ;
#2671 = CARTESIAN_POINT ( 'NONE',  ( 8.609967445932001695, -4.707159105298062585, 5.915074581558068978 ) ) ;
#2672 = ORIENTED_EDGE ( 'NONE', *, *, #65261, .F. ) ;
#2673 = CARTESIAN_POINT ( 'NONE',  ( 9.524624721938954153, 2.899999999999999911, -6.445686799096955966 ) ) ;
#2674 = CARTESIAN_POINT ( 'NONE',  ( 23.74313545907000389, -13.04470672865000047, -3.827358778968999786 ) ) ;
#2675 = FACE_OUTER_BOUND ( 'NONE', #19705, .T. ) ;
#2676 = SURFACE_STYLE_USAGE ( .BOTH. , #55825 ) ;
#2677 = MECHANICAL_DESIGN_GEOMETRIC_PRESENTATION_REPRESENTATION (  '', ( #6002 ), #38399 ) ;
#2678 = CARTESIAN_POINT ( 'NONE',  ( 9.817462135711998883, -5.100000000000000533, 6.571291218949999902 ) ) ;
#2679 = ORIENTED_EDGE ( 'NONE', *, *, #61365, .T. ) ;
#2680 = CARTESIAN_POINT ( 'NONE',  ( 10.07314899745999881, -5.167567567567999731, -6.822293592207000934 ) ) ;
#2681 = AXIS2_PLACEMENT_3D ( 'NONE', #41221, #24456, #29722 ) ;
#2682 = CARTESIAN_POINT ( 'NONE',  ( 11.09999999999999964, 4.000000000000000000, -7.500000000000000000 ) ) ;
#2683 = CARTESIAN_POINT ( 'NONE',  ( 3.500000000000000444, 1.332139861897094546, 3.064909822328984568 ) ) ;
#2684 = CARTESIAN_POINT ( 'NONE',  ( 10.11094409420000062, 5.100000000000000533, -6.571291218949999902 ) ) ;
#2685 = CARTESIAN_POINT ( 'NONE',  ( 24.34833239419533513, 3.256146798601845749, 12.15210528928062494 ) ) ;
#2686 = AXIS2_PLACEMENT_3D ( 'NONE', #68665, #26379, #63067 ) ;
#2687 = CARTESIAN_POINT ( 'NONE',  ( 12.18006450918421812, 0.02080959496298997666, -13.89999914846831075 ) ) ;
#2688 = CARTESIAN_POINT ( 'NONE',  ( 17.98541303540595493, -2.046657644932490250, 12.54573712159721133 ) ) ;
#2689 = ORIENTED_EDGE ( 'NONE', *, *, #5232, .T. ) ;
#2690 = EDGE_CURVE ( 'NONE', #4735, #21492, #57171, .T. ) ;
#2691 = CARTESIAN_POINT ( 'NONE',  ( 11.39700581613019992, -3.130347327833300053, -8.058426314824099990 ) ) ;
#2692 = EDGE_CURVE ( 'NONE', #1683, #16661, #7828, .T. ) ;
#2693 = VERTEX_POINT ( 'NONE', #7952 ) ;
#2694 = CARTESIAN_POINT ( 'NONE',  ( 23.58333425412700279, 1.475264355121999897E-12, 7.429612480791998923E-13 ) ) ;
#2695 = CARTESIAN_POINT ( 'NONE',  ( 8.548770280408998445, 5.203550244299999683, -8.391678825488000371 ) ) ;
#2696 = ADVANCED_FACE ( 'NONE', ( #56190 ), #62753, .T. ) ;
#2697 = CARTESIAN_POINT ( 'NONE',  ( 2.922328358399999715, 1.841131904257000018, 2.833808463758999974 ) ) ;
#2698 = CARTESIAN_POINT ( 'NONE',  ( 10.43283788151999936, -3.279327064383000145, -9.029275888523999427 ) ) ;
#2699 = CARTESIAN_POINT ( 'NONE',  ( 13.00000000009400303, -11.69118001589999878, -1.923222888683999932 ) ) ;
#2700 = CARTESIAN_POINT ( 'NONE',  ( 9.061840010887420860, -4.635352338266921279, 8.712813424890676117 ) ) ;
#2701 = ORIENTED_EDGE ( 'NONE', *, *, #68552, .T. ) ;
#2702 = CARTESIAN_POINT ( 'NONE',  ( 11.93302763632549990, -5.035790660926999784, 7.977941233841399971 ) ) ;
#2703 = CARTESIAN_POINT ( 'NONE',  ( 10.22108913916999917, 2.983268757921999637, 8.764704075288999974 ) ) ;
#2704 = CARTESIAN_POINT ( 'NONE',  ( 10.68797807636034847, -4.829546767829381970, -8.579382731881592505 ) ) ;
#2705 = DIRECTION ( 'NONE',  ( -1.000000000000000000, 0.000000000000000000, 0.000000000000000000 ) ) ;
#2707 = CARTESIAN_POINT ( 'NONE',  ( 10.90000000000000036, 5.283926297003000094, 7.082827057608000132 ) ) ;
#2706 = CARTESIAN_POINT ( 'NONE',  ( 9.566963020987998334, 5.215925787220999865, 6.177726425586999248 ) ) ;
#2708 = VECTOR ( 'NONE', #49482, 1000.000000000000000 ) ;
#2709 = CARTESIAN_POINT ( 'NONE',  ( 10.48133997687999930, 4.184599793140999502, -6.653701289769800020 ) ) ;
#2710 = ADVANCED_FACE ( 'NONE', ( #39773 ), #24848, .T. ) ;
#2711 = CARTESIAN_POINT ( 'NONE',  ( 25.34046054230887179, -11.16058825301069746, -3.348982524390977655 ) ) ;
#2712 = CARTESIAN_POINT ( 'NONE',  ( 9.756329965421999262, 3.302375896175799852, -8.222608407156599242 ) ) ;
#2713 = CARTESIAN_POINT ( 'NONE',  ( 18.26375634269466275, -0.1521017209118873392, 12.59908727444663867 ) ) ;
#2714 = DIRECTION ( 'NONE',  ( 0.000000000000000000, 0.000000000000000000, -1.000000000000000000 ) ) ;
#2715 = DIRECTION ( 'NONE',  ( 0.000000000000000000, 0.000000000000000000, 1.000000000000000000 ) ) ;
#2716 = CARTESIAN_POINT ( 'NONE',  ( 10.84161084123000052, 2.641275823976000137, -7.444905437480000110 ) ) ;
#2717 = ORIENTED_EDGE ( 'NONE', *, *, #10477, .F. ) ;
#2718 = CARTESIAN_POINT ( 'NONE',  ( 7.373066940378000034, -3.394845988290999816, 9.388942682504000103 ) ) ;
#2719 = CARTESIAN_POINT ( 'NONE',  ( 18.26096953105663800, 2.684662952176594786, 13.74018646639511942 ) ) ;
#2720 = CARTESIAN_POINT ( 'NONE',  ( 12.09999999999999964, -4.000000000000000000, 7.500000000000000000 ) ) ;
#2721 = CARTESIAN_POINT ( 'NONE',  ( 10.24733997687999931, -3.727636250918499705, -6.251346978035999591 ) ) ;
#2722 = ORIENTED_EDGE ( 'NONE', *, *, #61872, .T. ) ;
#2723 = AXIS2_PLACEMENT_3D ( 'NONE', #2810, #24140, #45471 ) ;
#2724 = CARTESIAN_POINT ( 'NONE',  ( 7.550614158771000284, 4.468366666325000125, 8.882140983065999862 ) ) ;
#2726 = CARTESIAN_POINT ( 'NONE',  ( 0.6825985948785217028, -0.3204594736343227002, 3.524357824565985897 ) ) ;
#2725 = CARTESIAN_POINT ( 'NONE',  ( 9.442010841233001273, 5.045571591548999812, -9.086294919530001124 ) ) ;
#2727 = CARTESIAN_POINT ( 'NONE',  ( 10.30480165877000154, 5.828331171948000211, -7.226590957700000928 ) ) ;
#2728 = ORIENTED_EDGE ( 'NONE', *, *, #23207, .T. ) ;
#2729 = CARTESIAN_POINT ( 'NONE',  ( 11.02445190299000011, 3.404087387974999768, 5.822483872269000216 ) ) ;
#2730 = CARTESIAN_POINT ( 'NONE',  ( 18.20591985607871521, -2.840417715854227421, -13.70884684492145134 ) ) ;
#2731 = CARTESIAN_POINT ( 'NONE',  ( 10.64533863405319991, 4.703785194191100416, 6.602238051205399749 ) ) ;
#2732 = CARTESIAN_POINT ( 'NONE',  ( 10.66951732929000052, -4.592671928130000580, 5.841406818427000047 ) ) ;
#2733 = CARTESIAN_POINT ( 'NONE',  ( 17.60000000024299993, 11.86189249994999884, -3.298671769835999967 ) ) ;
#2734 = ORIENTED_EDGE ( 'NONE', *, *, #50915, .F. ) ;
#2735 = DIRECTION ( 'NONE',  ( 0.000000000000000000, -0.7071067811865475727, 0.7071067811865475727 ) ) ;
#2736 = CARTESIAN_POINT ( 'NONE',  ( 1.428056799207624739, 2.150913519912206695, -2.798833948393627313 ) ) ;
#2737 = CARTESIAN_POINT ( 'NONE',  ( 7.967003474473192348, -2.304381480019767725, 7.113056951929115357 ) ) ;
#2738 = CARTESIAN_POINT ( 'NONE',  ( 10.62197618263000010, -5.779779175739000685, 7.256573549370999743 ) ) ;
#2739 = CARTESIAN_POINT ( 'NONE',  ( 10.63880513895979973, -2.849548954067000039, -6.860457220153399760 ) ) ;
#2740 = CARTESIAN_POINT ( 'NONE',  ( 9.273468108405999999, -3.033597967472499768, 7.226304214866999587 ) ) ;
#2741 = ORIENTED_EDGE ( 'NONE', *, *, #67162, .T. ) ;
#2742 = CARTESIAN_POINT ( 'NONE',  ( 10.34612086457000046, -4.749262201179999643, -4.718566242310000547 ) ) ;
#2743 = CARTESIAN_POINT ( 'NONE',  ( 11.70733594839949809, -3.159733897807000425, 8.462948211532999920 ) ) ;
#2744 = ORIENTED_EDGE ( 'NONE', *, *, #13110, .T. ) ;
#2745 = DIRECTION ( 'NONE',  ( -1.000000000000000000, 0.000000000000000000, 0.000000000000000000 ) ) ;
#2746 = ORIENTED_EDGE ( 'NONE', *, *, #66997, .F. ) ;
#2747 = EDGE_CURVE ( 'NONE', #34308, #25967, #67870, .T. ) ;
#2748 = EDGE_CURVE ( 'NONE', #44042, #28231, #31973, .T. ) ;
#2749 = CARTESIAN_POINT ( 'NONE',  ( 11.09999999999999964, 3.512324525112999751, -8.971282648301999174 ) ) ;
#2750 = CARTESIAN_POINT ( 'NONE',  ( 8.506095280410999493, 2.305580295895999665, -7.860904109308999743 ) ) ;
#2751 = CARTESIAN_POINT ( 'NONE',  ( 23.58334011193800350, 0.000000000000000000, -3.819167204710999951E-13 ) ) ;
#2752 = DIRECTION ( 'NONE',  ( -1.000000000000000000, 0.000000000000000000, 0.000000000000000000 ) ) ;
#2753 = CARTESIAN_POINT ( 'NONE',  ( 12.21314472040064913, 2.700933736278044339, -12.40250870093142410 ) ) ;
#2754 = CARTESIAN_POINT ( 'NONE',  ( 11.49410672858429905, -4.801902424331299990, 8.103244025831999764 ) ) ;
#2755 = CARTESIAN_POINT ( 'NONE',  ( 11.11257802013489915, -4.891884252872400474, 7.520762592984879369 ) ) ;
#2756 = VERTEX_POINT ( 'NONE', #22990 ) ;
#2757 = CARTESIAN_POINT ( 'NONE',  ( 0.000000000000000000, 0.000000000000000000, 0.000000000000000000 ) ) ;
#2758 = CONICAL_SURFACE ( 'NONE', #6086, 12.71246950475999959, 0.8960553845711767273 ) ;
#2759 = ORIENTED_EDGE ( 'NONE', *, *, #62223, .F. ) ;
#2760 = CARTESIAN_POINT ( 'NONE',  ( 8.534480646793999981, -3.011617647609999615, 8.801438026873999121 ) ) ;
#2761 = CARTESIAN_POINT ( 'NONE',  ( 7.474999999999999645, -5.349999999999999645, 7.500000000000000000 ) ) ;
#2762 = ORIENTED_EDGE ( 'NONE', *, *, #33583, .T. ) ;
#2763 = B_SPLINE_SURFACE_WITH_KNOTS ( 'NONE', 3, 3, ( 
 ( #60568, #59870, #27726, #49376, #1840, #59526, #12676, #38904, #53931, #17576, #37856 ),
 ( #1492, #16872, #60226, #22458, #27372, #32962, #54276, #23158, #48699, #33314, #59181 ),
 ( #11975, #54630, #12329, #7421, #50082, #54979, #2189, #7077, #6377, #44506, #23503 ),
 ( #49040, #17222, #65800, #64754, #799, #11280, #66150, #6726, #1149, #32620, #22116 ) ),
 .UNSPECIFIED., .F., .F., .F.,
 ( 4, 4 ),
 ( 4, 1, 1, 1, 1, 1, 1, 1, 4 ),
 ( -0.1039370721279000015, 1.103937072127999963 ),
 ( 0.6999999999992999600, 0.7382352941170999827, 0.7764705882347999744, 0.8147058823525000770, 0.8529411764702999887, 0.8911764705879999804, 0.9294117647057000831, 0.9676470588234999948, 1.005882352940999924 ),
 .UNSPECIFIED. ) ;
#2764 = CARTESIAN_POINT ( 'NONE',  ( 12.08005347077625835, -2.506700685333587586, -12.34815832536655833 ) ) ;
#2765 = CARTESIAN_POINT ( 'NONE',  ( 11.30995122972050027, 4.452766304612699955, 8.547040013405998948 ) ) ;
#2766 = CARTESIAN_POINT ( 'NONE',  ( 10.69829435321000055, -2.534030585780999711, -6.667788699001999220 ) ) ;
#2767 = CARTESIAN_POINT ( 'NONE',  ( 6.724999999999962341, 5.339057002848987210, -8.130112396048081891 ) ) ;
#2768 = CARTESIAN_POINT ( 'NONE',  ( 18.35500032369700207, -2.879010252073999521, -12.03969535450000095 ) ) ;
#2769 = CARTESIAN_POINT ( 'NONE',  ( 24.46729256497600247, -8.826997888156999039, 8.952499470947000049 ) ) ;
#2770 = CARTESIAN_POINT ( 'NONE',  ( 12.80505043854146763, -3.125000000000000444, -13.52078605991414761 ) ) ;
#2771 = CARTESIAN_POINT ( 'NONE',  ( 5.342753212293000153, 1.434852097279999850, 0.6058508543602000307 ) ) ;
#2772 = CARTESIAN_POINT ( 'NONE',  ( 11.53979707368350027, -4.430269712815499972, -6.748224392138099326 ) ) ;
#2773 = CARTESIAN_POINT ( 'NONE',  ( 10.24733997687999931, -3.727636250918499705, -6.251346978035999591 ) ) ;
#2774 = DIRECTION ( 'NONE',  ( -1.000000000000000000, 0.000000000000000000, 0.000000000000000000 ) ) ;
#2775 = ORIENTED_EDGE ( 'NONE', *, *, #15396, .F. ) ;
#2776 = DIRECTION ( 'NONE',  ( 0.000000000000000000, 1.000000000000000000, 0.000000000000000000 ) ) ;
#2777 = CARTESIAN_POINT ( 'NONE',  ( 17.71800267521794936, 3.104751769958197016, 13.52637079326926539 ) ) ;
#2778 = EDGE_CURVE ( 'NONE', #26398, #63101, #12858, .T. ) ;
#2779 = CARTESIAN_POINT ( 'NONE',  ( 23.64145649527500126, -3.069298110642999955, 13.45466198155999926 ) ) ;
#2780 = AXIS2_PLACEMENT_3D ( 'NONE', #15144, #3275, #8180 ) ;
#2781 = CARTESIAN_POINT ( 'NONE',  ( 17.74512657133769622, 3.174942931788175216, 12.19343219266723821 ) ) ;
#2782 = DIRECTION ( 'NONE',  ( 1.000000000000000000, 0.000000000000000000, 0.000000000000000000 ) ) ;
#2783 = CARTESIAN_POINT ( 'NONE',  ( 11.13459739833729856, 3.176841881612200158, -7.825000000000000178 ) ) ;
#2784 = CARTESIAN_POINT ( 'NONE',  ( 9.650912690312628328, -4.805207160112336950, 7.157693560935859622 ) ) ;
#2785 = ORIENTED_EDGE ( 'NONE', *, *, #25253, .T. ) ;
#2786 = CARTESIAN_POINT ( 'NONE',  ( 12.17998194132763423, -2.482033040872618113, 12.45578191469033413 ) ) ;
#2787 = CARTESIAN_POINT ( 'NONE',  ( 10.33688779216199904, -3.198058499272899979, -7.789199634454999632 ) ) ;
#2788 = CARTESIAN_POINT ( 'NONE',  ( 11.12915085989000019, 3.083869275439000024, 8.585995236726001067 ) ) ;
#2789 = CONICAL_SURFACE ( 'NONE', #21735, 13.94999929345000211, 0.7853981072369679017 ) ;
#2790 = CARTESIAN_POINT ( 'NONE',  ( 12.17766954483535891, -3.284117569315500251, 8.604570063127999546 ) ) ;
#2791 = CARTESIAN_POINT ( 'NONE',  ( 11.50271932425157040, 3.812601581225100400, -8.764198628556998827 ) ) ;
#2792 = EDGE_CURVE ( 'NONE', #49108, #68077, #61771, .T. ) ;
#2793 = CARTESIAN_POINT ( 'NONE',  ( 12.23161381921988422, 0.2487950381773037789, 12.69672507751632118 ) ) ;
#2794 = CARTESIAN_POINT ( 'NONE',  ( 9.214142219592000416, 5.421534627450999899, 6.381126373995999579 ) ) ;
#2795 = CARTESIAN_POINT ( 'NONE',  ( 9.199602729599000384, 2.551394566582000145, 7.536605852160000119 ) ) ;
#2796 = CARTESIAN_POINT ( 'NONE',  ( 12.18110988575100251, 2.462234709496985197, 12.46028276222759068 ) ) ;
#2797 = ORIENTED_EDGE ( 'NONE', *, *, #54179, .F. ) ;
#2798 = CARTESIAN_POINT ( 'NONE',  ( 9.395239158775000377, 5.045571591548999812, -9.086294919530001124 ) ) ;
#2799 = CARTESIAN_POINT ( 'NONE',  ( 11.50271932425157040, 3.812601581225100400, -8.764198628556998827 ) ) ;
#2800 = CARTESIAN_POINT ( 'NONE',  ( 5.329623228227332810, 1.445318020077273724, 0.4634605740919916506 ) ) ;
#2802 = PLANE ( 'NONE',  #40727 ) ;
#2801 = CARTESIAN_POINT ( 'NONE',  ( 7.443293146792999693, -4.698358408974000255, 8.789434435623999065 ) ) ;
#2803 = CARTESIAN_POINT ( 'NONE',  ( 10.69190035061499877, -3.732283713685800031, 6.531924610394499453 ) ) ;
#2804 = CARTESIAN_POINT ( 'NONE',  ( 11.14179841651039915, -4.353306409735099969, -8.439215328713499886 ) ) ;
#2805 = ORIENTED_EDGE ( 'NONE', *, *, #68468, .T. ) ;
#2806 = CARTESIAN_POINT ( 'NONE',  ( 1.205336560124999901, -3.461062994654999780, -0.9617132324576000979 ) ) ;
#2807 = CARTESIAN_POINT ( 'NONE',  ( 17.91195086072671572, -0.5131995813064865741, -12.68604179104344531 ) ) ;
#2808 = CARTESIAN_POINT ( 'NONE',  ( 12.79999999824001122, 12.03389405692475300, -3.206111686008664918 ) ) ;
#2809 = CARTESIAN_POINT ( 'NONE',  ( 18.12459608108212805, -2.757432806210013521, 13.61548201701218197 ) ) ;
#2810 = CARTESIAN_POINT ( 'NONE',  ( 7.000000000000000000, 0.000000000000000000, 0.000000000000000000 ) ) ;
#2811 = CARTESIAN_POINT ( 'NONE',  ( 12.70947385406810604, -3.242135136469473267, 13.61941870117945186 ) ) ;
#2812 = CARTESIAN_POINT ( 'NONE',  ( 11.70596535229475776, -4.908912176279685013, 7.175015064079871330 ) ) ;
#2813 = CARTESIAN_POINT ( 'NONE',  ( 9.520528907821001141, 2.899999999999999911, 6.152188490330000370 ) ) ;
#2814 = CARTESIAN_POINT ( 'NONE',  ( 7.822379440378000481, -4.636725880537000855, 9.378965771357000492 ) ) ;
#2815 = ORIENTED_EDGE ( 'NONE', *, *, #35366, .F. ) ;
#2816 = CARTESIAN_POINT ( 'NONE',  ( 8.213545280409999094, 3.608525622520999843, 5.913376237674000002 ) ) ;
#2817 = CARTESIAN_POINT ( 'NONE',  ( 10.91620964606000044, 2.818413279081999789, -6.814156272943999504 ) ) ;
#2818 = CARTESIAN_POINT ( 'NONE',  ( 7.449893704810870432, -2.260907433923616150, 7.482160321753426935 ) ) ;
#2819 = LINE ( 'NONE', #30103, #37991 ) ;
#2820 = CARTESIAN_POINT ( 'NONE',  ( 1.700339139801000155, 1.841731729107999982, 3.084132442762999915 ) ) ;
#2821 = ORIENTED_EDGE ( 'NONE', *, *, #65016, .F. ) ;
#2822 = DIRECTION ( 'NONE',  ( 0.8660254038003750710, -1.114487574551968024E-07, -0.4999999999723849786 ) ) ;
#2823 = CARTESIAN_POINT ( 'NONE',  ( 11.08613868670750335, -2.236165381191161039, -7.580675004253683902 ) ) ;
#2824 = CARTESIAN_POINT ( 'NONE',  ( 9.479214860607999782, 4.071727169861000029, 9.089299483126000112 ) ) ;
#2825 = CIRCLE ( 'NONE', #13967, 0.5500000000000001554 ) ;
#2826 = CARTESIAN_POINT ( 'NONE',  ( 10.47718582084299932, 3.343463760027599818, 8.258888014436699621 ) ) ;
#2827 = EDGE_CURVE ( 'NONE', #12746, #20439, #6973, .T. ) ;
#2828 = EDGE_CURVE ( 'NONE', #56347, #4626, #55851, .T. ) ;
#2829 = CARTESIAN_POINT ( 'NONE',  ( 18.50001572531400029, -1.956586047027013553, 12.40985500578818090 ) ) ;
#2830 = CARTESIAN_POINT ( 'NONE',  ( 10.38725444037999956, -2.888666857901000196, -6.716331201355000502 ) ) ;
#2831 = CARTESIAN_POINT ( 'NONE',  ( 11.79999999684100054, 3.345264396959000130, -11.86064773189999855 ) ) ;
#2832 = EDGE_CURVE ( 'NONE', #60315, #18158, #48686, .T. ) ;
#2833 = EDGE_CURVE ( 'NONE', #17467, #8257, #41138, .T. ) ;
#2834 = CARTESIAN_POINT ( 'NONE',  ( 8.737760194560388882, -4.066145789045418013, -8.370465981241705933 ) ) ;
#2835 = CARTESIAN_POINT ( 'NONE',  ( 12.27931543957927119, -2.838108479055812872, 12.36635919027515307 ) ) ;
#2836 = CARTESIAN_POINT ( 'NONE',  ( 8.294817490939964344, 4.669395409018583187, 9.123971829385043364 ) ) ;
#2837 = ORIENTED_EDGE ( 'NONE', *, *, #6291, .T. ) ;
#2838 = CARTESIAN_POINT ( 'NONE',  ( 17.92019487611651485, -3.148838011673614101, 13.64129243465967356 ) ) ;
#2839 = CARTESIAN_POINT ( 'NONE',  ( 10.31746213571000048, -5.100000000000000533, 6.571291218949999902 ) ) ;
#2840 = ORIENTED_EDGE ( 'NONE', *, *, #46005, .T. ) ;
#2841 = ORIENTED_EDGE ( 'NONE', *, *, #64153, .F. ) ;
#2842 = CARTESIAN_POINT ( 'NONE',  ( 10.77879632507499785, 4.423544049216699747, 6.714825466131699727 ) ) ;
#2843 = CARTESIAN_POINT ( 'NONE',  ( 24.67921321731900264, -3.567517257907000250, -12.13750614118000115 ) ) ;
#2844 = CARTESIAN_POINT ( 'NONE',  ( 12.80505043854143388, 3.174834474598374090, -12.21921104873077013 ) ) ;
#2845 = CARTESIAN_POINT ( 'NONE',  ( 9.967852198058999136, 2.034774058634999605, 7.636878205663998997 ) ) ;
#2846 = CARTESIAN_POINT ( 'NONE',  ( 9.819565861057999001, 2.688248842995000221, -7.873038103423000145 ) ) ;
#2847 = CARTESIAN_POINT ( 'NONE',  ( 8.814947692958833514, 2.650138447187985413, -7.499997389691697158 ) ) ;
#2848 = CARTESIAN_POINT ( 'NONE',  ( 10.76010362286999822, -4.535387425205000156, 6.001717576299999024 ) ) ;
#2849 = CARTESIAN_POINT ( 'NONE',  ( 11.35562122949000141, 3.716778816705999855, -11.19591510979999960 ) ) ;
#2850 = DIRECTION ( 'NONE',  ( 0.000000000000000000, -0.9835907196275001096, -0.1804142351995999538 ) ) ;
#2851 = CARTESIAN_POINT ( 'NONE',  ( 10.28441772631199846, -3.627481539113199815, -8.266796319406900295 ) ) ;
#2852 = VECTOR ( 'NONE', #33316, 1000.000000000000000 ) ;
#2853 = DIRECTION ( 'NONE',  ( 1.000000000000000000, 0.000000000000000000, 0.000000000000000000 ) ) ;
#2854 = VERTEX_POINT ( 'NONE', #18794 ) ;
#2855 = EDGE_CURVE ( 'NONE', #16623, #2498, #14513, .T. ) ;
#2856 = VECTOR ( 'NONE', #61927, 1000.000000000000000 ) ;
#2857 = CYLINDRICAL_SURFACE ( 'NONE', #45952, 1.350000000000000533 ) ;
#2858 = DIRECTION ( 'NONE',  ( 0.000000000000000000, 0.7198977633594747516, -0.6940801180771756229 ) ) ;
#2859 = CARTESIAN_POINT ( 'NONE',  ( 9.177784697135001224, 4.694174896253500151, -6.425520776924999566 ) ) ;
#2860 = CARTESIAN_POINT ( 'NONE',  ( 12.54499921992989719, 1.931577877770959573, 13.77766407476416077 ) ) ;
#2861 = CARTESIAN_POINT ( 'NONE',  ( 10.53733998880999856, -2.992814141720000265, 8.731692578598000409 ) ) ;
#2862 = VERTEX_POINT ( 'NONE', #40446 ) ;
#2863 = CARTESIAN_POINT ( 'NONE',  ( 12.20957360716226248, -0.1900975198226042273, -12.69808960362384553 ) ) ;
#2864 = CARTESIAN_POINT ( 'NONE',  ( 12.75722769875344476, 0.7290248443971270031, 13.98100598729141097 ) ) ;
#2865 = ORIENTED_EDGE ( 'NONE', *, *, #21607, .T. ) ;
#2866 = DIRECTION ( 'NONE',  ( -1.000000000000000000, 0.000000000000000000, 0.000000000000000000 ) ) ;
#2867 = B_SPLINE_CURVE_WITH_KNOTS ( 'NONE', 3,
 ( #254, #27516, #31732, #58987, #63532, #53052, #16327, #11088 ),
 .UNSPECIFIED., .F., .F.,
 ( 4, 1, 1, 1, 1, 4 ),
 ( 0.2125974459517032678, 0.3245965717578418452, 0.5241428039294082630, 0.7236890361001979688, 0.9232352682709885627, 1.000000000000000000 ),
 .UNSPECIFIED. ) ;
#2868 = CARTESIAN_POINT ( 'NONE',  ( 10.52052890781999928, -2.899999999999999911, 6.152188490330000370 ) ) ;
#2869 = CARTESIAN_POINT ( 'NONE',  ( 24.25865791894600321, -3.167027296516999879, -12.13989236613999978 ) ) ;
#2870 = CARTESIAN_POINT ( 'NONE',  ( 23.59999443371599881, 2.915558930973999985, 13.58549620949000136 ) ) ;
#2871 = CIRCLE ( 'NONE', #17393, 1.699994593733000547 ) ;
#2872 = B_SPLINE_CURVE_WITH_KNOTS ( 'NONE', 3,
 ( #23840, #13365, #37335, #48172, #25211 ),
 .UNSPECIFIED., .F., .F.,
 ( 4, 1, 4 ),
 ( 0.000000000000000000, 0.3670466485305822757, 1.000000000000000000 ),
 .UNSPECIFIED. ) ;
#2873 = ADVANCED_FACE ( 'NONE', ( #41483 ), #46734, .F. ) ;
#2874 = DIRECTION ( 'NONE',  ( 1.000000000000000000, 0.000000000000000000, 0.000000000000000000 ) ) ;
#2875 = CARTESIAN_POINT ( 'NONE',  ( 24.67921580255100267, 8.727633792449999817, 9.158312800479000870 ) ) ;
#2876 = CARTESIAN_POINT ( 'NONE',  ( 25.55282635881618347, 11.13089659500204753, -3.116549873335771714 ) ) ;
#2877 = FACE_OUTER_BOUND ( 'NONE', #61126, .T. ) ;
#2878 = ADVANCED_FACE ( 'NONE', ( #51962 ), #15259, .F. ) ;
#2879 = CARTESIAN_POINT ( 'NONE',  ( 12.34734069910707710, 3.038294257956348776, 12.22819623478419260 ) ) ;
#2880 = CARTESIAN_POINT ( 'NONE',  ( 9.086718600414000591, -4.531444417037000072, -6.133284059228000018 ) ) ;
#2881 = CARTESIAN_POINT ( 'NONE',  ( 11.53979707368350027, 3.569730287184500472, -6.748224392138099326 ) ) ;
#2882 = LINE ( 'NONE', #8478, #57051 ) ;
#2883 = CARTESIAN_POINT ( 'NONE',  ( 10.32169598648999909, 4.766524664146899681, -7.956401575444799867 ) ) ;
#2884 = CARTESIAN_POINT ( 'NONE',  ( 9.860608878791998322, 3.741427262966100287, -6.387851364408000165 ) ) ;
#2886 = CARTESIAN_POINT ( 'NONE',  ( 9.290860954912000480, -3.902433532469449684, 6.578106533244199916 ) ) ;
#2885 = CARTESIAN_POINT ( 'NONE',  ( 9.443784697134999462, -3.529509552262100058, 8.228249052908999772 ) ) ;
#2887 = CARTESIAN_POINT ( 'NONE',  ( 23.56665657345700282, -13.31365812469000076, 4.296923216748999685 ) ) ;
#2888 = ORIENTED_EDGE ( 'NONE', *, *, #40786, .T. ) ;
#2889 = CARTESIAN_POINT ( 'NONE',  ( 1.700000000000000178, 0.000000000000000000, 0.000000000000000000 ) ) ;
#2890 = CARTESIAN_POINT ( 'NONE',  ( 10.80815535238000002, -2.937528991339000140, 8.948455587554001056 ) ) ;
#2891 = CARTESIAN_POINT ( 'NONE',  ( 9.477709346417000802, 4.907312911337299965, 7.930842873041400232 ) ) ;
#2892 = CARTESIAN_POINT ( 'NONE',  ( 9.657495633957626779, 3.225830943932614048, -7.907669647568630111 ) ) ;
#2893 = B_SPLINE_CURVE_WITH_KNOTS ( 'NONE', 3,
 ( #28176, #34120, #44272, #34472 ),
 .UNSPECIFIED., .F., .F.,
 ( 4, 4 ),
 ( 0.000000000000000000, 1.000000000000000000 ),
 .UNSPECIFIED. ) ;
#2894 = DIRECTION ( 'NONE',  ( 1.000000000000000000, 0.000000000000000000, 0.000000000000000000 ) ) ;
#2895 = CARTESIAN_POINT ( 'NONE',  ( 23.89320776801300283, 8.283889223723997830, -7.778387373039001851 ) ) ;
#2896 = ORIENTED_EDGE ( 'NONE', *, *, #27471, .T. ) ;
#2897 = CARTESIAN_POINT ( 'NONE',  ( 9.506000818238998562, -5.010295986746999830, -8.032011717116800398 ) ) ;
#2898 = CARTESIAN_POINT ( 'NONE',  ( 4.550000802215999229, 1.829647544581999737E-13, -13.04999934368000147 ) ) ;
#2899 = CARTESIAN_POINT ( 'NONE',  ( 18.28003019995797018, 2.460172313524571663, -12.35749544995779559 ) ) ;
#2900 = CARTESIAN_POINT ( 'NONE',  ( 10.96459579918999871, -2.848437942114999899, 5.071485159340999971 ) ) ;
#2901 = CIRCLE ( 'NONE', #48672, 13.98989063586000370 ) ;
#2902 = CARTESIAN_POINT ( 'NONE',  ( 5.440293061358000060, 12.88483958404999896, 2.133988467672999878 ) ) ;
#2903 = CARTESIAN_POINT ( 'NONE',  ( 6.055026506350000837, -1.500000000000000000, 0.000000000000000000 ) ) ;
#2904 = CARTESIAN_POINT ( 'NONE',  ( 9.883915020958999875, -5.811247906278000031, -7.978055797018001272 ) ) ;
#2905 = CARTESIAN_POINT ( 'NONE',  ( 8.150000662387999029, 3.037570195374000164E-13, -12.44999944941003989 ) ) ;
#2906 = VERTEX_POINT ( 'NONE', #36582 ) ;
#2907 = CARTESIAN_POINT ( 'NONE',  ( 24.48513962453899850, -12.12976302882999846, -3.164527203478999962 ) ) ;
#2908 = ADVANCED_FACE ( 'NONE', ( #9657 ), #54785, .F. ) ;
#2909 = CARTESIAN_POINT ( 'NONE',  ( 12.25919481816069734, -0.4811670829680815276, -13.99174107639406373 ) ) ;
#2910 = EDGE_CURVE ( 'NONE', #10029, #50859, #62792, .T. ) ;
#2911 = CARTESIAN_POINT ( 'NONE',  ( 13.99956681845000084, -8.827069132150999309, -7.822720559936999329 ) ) ;
#2912 = CARTESIAN_POINT ( 'NONE',  ( 21.72233714749290101, 4.999803429358669504, -0.04433585200820212152 ) ) ;
#2913 = CARTESIAN_POINT ( 'NONE',  ( 25.37646317443000044, -8.494765284640999781, -7.922174285211998956 ) ) ;
#2914 = CARTESIAN_POINT ( 'NONE',  ( 23.60000000000000497, -10.96673476284452775, -8.588459421149421402 ) ) ;
#2915 = CARTESIAN_POINT ( 'NONE',  ( 6.899999438051000133, 0.5526611926744998682, 1.394476821647000042 ) ) ;
#2916 = ORIENTED_EDGE ( 'NONE', *, *, #57098, .T. ) ;
#2917 = DIRECTION ( 'NONE',  ( -0.000000000000000000, 1.000000000000000000, 0.000000000000000000 ) ) ;
#2918 = CARTESIAN_POINT ( 'NONE',  ( 17.55505043854143565, 1.875000000000000000, -13.78631952119025250 ) ) ;
#2919 = VERTEX_POINT ( 'NONE', #41146 ) ;
#2920 = CARTESIAN_POINT ( 'NONE',  ( 10.90000000000000036, 0.000000000000000000, 0.000000000000000000 ) ) ;
#2921 = LINE ( 'NONE', #24600, #2236 ) ;
#2922 = CONICAL_SURFACE ( 'NONE', #52019, 13.94999929345000211, 0.7853981072369679017 ) ;
#2923 = CARTESIAN_POINT ( 'NONE',  ( 8.465229719592999302, 2.567871051582000241, -6.869011921437000012 ) ) ;
#2924 = CARTESIAN_POINT ( 'NONE',  ( 9.457462135716001583, 5.100000000000000533, -6.571291218949999902 ) ) ;
#2925 = CARTESIAN_POINT ( 'NONE',  ( 11.68788784977535933, -4.985985832792199979, -7.443657794094239222 ) ) ;
#2926 = CARTESIAN_POINT ( 'NONE',  ( 17.77470270344264947, 0.5852243768386650169, -12.68184418015340142 ) ) ;
#2927 = CARTESIAN_POINT ( 'NONE',  ( 11.07928131834999874, -7.977359646417001571, 6.935621157201000031 ) ) ;
#2928 = VERTEX_POINT ( 'NONE', #36235 ) ;
#2929 = CARTESIAN_POINT ( 'NONE',  ( 7.821752845075590876, 2.830873829569032107, -8.205201578233504378 ) ) ;
#2930 = CARTESIAN_POINT ( 'NONE',  ( 10.69809687351567362, -3.672815144550895639, 8.717465845835397076 ) ) ;
#2931 = CARTESIAN_POINT ( 'NONE',  ( 18.16451541384049051, -2.360124911643264323, 13.70214797745214241 ) ) ;
#2932 = ORIENTED_EDGE ( 'NONE', *, *, #1367, .F. ) ;
#2933 = ADVANCED_FACE ( 'NONE', ( #31003 ), #4409, .T. ) ;
#2934 = CARTESIAN_POINT ( 'NONE',  ( 10.22440590001000160, 5.317411003666999925, -8.272452263128000638 ) ) ;
#2935 =( NAMED_UNIT ( * ) PLANE_ANGLE_UNIT ( ) SI_UNIT ( $, .RADIAN. ) );
#2936 = ORIENTED_EDGE ( 'NONE', *, *, #2544, .T. ) ;
#2937 = CARTESIAN_POINT ( 'NONE',  ( 9.708633995697999453, 5.134843509922999871, 7.374045024026299799 ) ) ;
#2938 = CARTESIAN_POINT ( 'NONE',  ( 18.27884988594220772, -2.529462001843207464, -12.34351620764206814 ) ) ;
#2939 = CARTESIAN_POINT ( 'NONE',  ( 10.99328643597795896, 6.034724004534248287, -5.044002573406743295 ) ) ;
#2940 = CARTESIAN_POINT ( 'NONE',  ( 23.89320776801300283, 3.226867021103002831, 11.46303308828999867 ) ) ;
#2941 = CARTESIAN_POINT ( 'NONE',  ( 5.500000000000000000, 0.000000000000000000, 0.000000000000000000 ) ) ;
#2942 = CARTESIAN_POINT ( 'NONE',  ( 9.382165295667087790, -2.854056800879049671, 8.808963309177558543 ) ) ;
#2943 = ORIENTED_EDGE ( 'NONE', *, *, #46367, .F. ) ;
#2944 = CARTESIAN_POINT ( 'NONE',  ( 24.37808886069849379, 3.385972254890575961, -12.24452376059983827 ) ) ;
#2945 = CARTESIAN_POINT ( 'NONE',  ( 8.737804660583998739, 4.491756428607999396, -5.831236541471000123 ) ) ;
#2946 = CARTESIAN_POINT ( 'NONE',  ( 9.947724669985010593, -5.285954009497336514, 7.027653896126389022 ) ) ;
#2947 = CARTESIAN_POINT ( 'NONE',  ( 12.51458961313711171, 3.187047769811530706, -13.63241538057482671 ) ) ;
#2948 = CONICAL_SURFACE ( 'NONE', #63219, 11.74991359182999950, 0.7853990805437361944 ) ;
#2949 = CARTESIAN_POINT ( 'NONE',  ( 10.49288779216199785, -2.943881405003000218, -7.880862084500499520 ) ) ;
#2950 = CARTESIAN_POINT ( 'NONE',  ( 10.62197618263000010, -5.779779175739000685, 7.256573549370999743 ) ) ;
#2951 = CARTESIAN_POINT ( 'NONE',  ( 18.08442884140762175, 0.4994936913945440815, 13.99109680828866153 ) ) ;
#2952 = AXIS2_PLACEMENT_3D ( 'NONE', #21154, #64468, #1208 ) ;
#2953 = CARTESIAN_POINT ( 'NONE',  ( 7.100000000000000533, 0.000000000000000000, 0.000000000000000000 ) ) ;
#2954 = ORIENTED_EDGE ( 'NONE', *, *, #53131, .T. ) ;
#2955 = ORIENTED_EDGE ( 'NONE', *, *, #65162, .F. ) ;
#2956 = B_SPLINE_CURVE_WITH_KNOTS ( 'NONE', 3,
 ( #65821, #38217, #59546, #65120 ),
 .UNSPECIFIED., .F., .F.,
 ( 4, 4 ),
 ( 0.000000000000000000, 1.000000000000000000 ),
 .UNSPECIFIED. ) ;
#2957 = CARTESIAN_POINT ( 'NONE',  ( 10.01622971959000097, 4.325866256860000369, -9.125812605905000652 ) ) ;
#2958 = ADVANCED_FACE ( 'NONE', ( #38297 ), #52907, .T. ) ;
#2959 = CARTESIAN_POINT ( 'NONE',  ( 9.144252007565954798, 5.327746249399065270, 6.363126469476570790 ) ) ;
#2960 = CARTESIAN_POINT ( 'NONE',  ( 10.47253786429000044, 2.899999999999999911, -6.571291218949999902 ) ) ;
#2961 = LINE ( 'NONE', #55424, #17164 ) ;
#2963 = CARTESIAN_POINT ( 'NONE',  ( 23.58699436501100166, 10.27243565008999937, -9.419031392528999902 ) ) ;
#2962 =( REPRESENTATION_RELATIONSHIP ('NONE','NONE', #10823, #60729 ) REPRESENTATION_RELATIONSHIP_WITH_TRANSFORMATION ( #26389 )SHAPE_REPRESENTATION_RELATIONSHIP( ) );
#2964 = CARTESIAN_POINT ( 'NONE',  ( 17.96012107570599881, -3.168891391480999520, -11.45723209283999999 ) ) ;
#2966 = CARTESIAN_POINT ( 'NONE',  ( 11.07074860546000039, -5.433615603927000492, 5.078288009826000149 ) ) ;
#2965 = CARTESIAN_POINT ( 'NONE',  ( 10.48630484851599931, -2.961576783819000358, 7.025224608805800131 ) ) ;
#2967 = CARTESIAN_POINT ( 'NONE',  ( 9.082867883171827472, 4.782673203840020371, -8.474986547786114599 ) ) ;
#2968 = ORIENTED_EDGE ( 'NONE', *, *, #31098, .F. ) ;
#2969 = AXIS2_PLACEMENT_3D ( 'NONE', #1958, #39709, #33429 ) ;
#2970 = CARTESIAN_POINT ( 'NONE',  ( 12.43999839839561794, -0.6380582630144968626, 13.98550026811445157 ) ) ;
#2971 = CARTESIAN_POINT ( 'NONE',  ( 10.73883163666999963, -2.873420258502000113, -5.007713218437999991 ) ) ;
#2972 = CARTESIAN_POINT ( 'NONE',  ( 17.89428234746476676, 0.5250240499537031091, 12.68539034781188413 ) ) ;
#2973 = CARTESIAN_POINT ( 'NONE',  ( 12.41699802712859224, -0.4899468514546045372, 12.68727699266409203 ) ) ;
#2974 = DIRECTION ( 'NONE',  ( 1.000000000000000000, 0.000000000000000000, 0.000000000000000000 ) ) ;
#2975 = ORIENTED_EDGE ( 'NONE', *, *, #16779, .T. ) ;
#2977 = LINE ( 'NONE', #7889, #44094 ) ;
#2976 = CARTESIAN_POINT ( 'NONE',  ( 10.95899882946999959, -5.155721817611999214, 5.124270346052999692 ) ) ;
#2978 = CARTESIAN_POINT ( 'NONE',  ( 10.07963755961372776, 4.353097593134667598, 8.851823023821664194 ) ) ;
#2979 = CARTESIAN_POINT ( 'NONE',  ( 7.750036073563001615, -5.085252754069001568, 6.546627699621002883 ) ) ;
#2980 = DIRECTION ( 'NONE',  ( 0.000000000000000000, 0.7071067811865475727, -0.7071067811865475727 ) ) ;
#2981 = CARTESIAN_POINT ( 'NONE',  ( 0.3606221729291086975, -3.272802759155408747, 0.8804288485544362608 ) ) ;
#2982 = CARTESIAN_POINT ( 'NONE',  ( 3.501249691757999827, 0.3639092243019000361, -3.573579329690000250 ) ) ;
#2983 = VERTEX_POINT ( 'NONE', #15602 ) ;
#2984 = CARTESIAN_POINT ( 'NONE',  ( 12.50535913667519239, 0.6550687562476287251, -12.58296113213902423 ) ) ;
#2985 = CARTESIAN_POINT ( 'NONE',  ( 11.91544519387736578, -3.267573604823260869, 7.982107551664254785 ) ) ;
#2986 = CARTESIAN_POINT ( 'NONE',  ( 16.09997386696500143, 7.697446472043785626, 8.794756076490960695 ) ) ;
#2987 = CARTESIAN_POINT ( 'NONE',  ( 24.55996189763800075, 3.658601031398000192, -12.32999353876000015 ) ) ;
#2988 = CARTESIAN_POINT ( 'NONE',  ( 17.55505043854143565, 3.125000000000000000, 13.52078605991414939 ) ) ;
#2989 = ORIENTED_EDGE ( 'NONE', *, *, #56853, .T. ) ;
#2990 = CARTESIAN_POINT ( 'NONE',  ( 6.249350226066000324, -0.6943539861719999484, 0.9492381903959000722 ) ) ;
#2991 = EDGE_CURVE ( 'NONE', #64727, #56117, #39528, .T. ) ;
#2992 = EDGE_CURVE ( 'NONE', #5259, #36190, #47323, .T. ) ;
#2993 = CARTESIAN_POINT ( 'NONE',  ( 8.236460841226000085, 3.600418141940000094, -8.839175402873999943 ) ) ;
#2994 = CARTESIAN_POINT ( 'NONE',  ( 7.866260132094000213, 4.690793098693000651, 6.339956846641999988 ) ) ;
#2995 = CARTESIAN_POINT ( 'NONE',  ( 7.806090764269955962, 3.007686321021738607, 6.534914955162395955 ) ) ;
#2996 = CARTESIAN_POINT ( 'NONE',  ( 11.43345123989529810, 4.540230239159599890, -8.543317325199000223 ) ) ;
#2997 = ORIENTED_EDGE ( 'NONE', *, *, #61726, .F. ) ;
#2998 = AXIS2_PLACEMENT_3D ( 'NONE', #30155, #14412, #14748 ) ;
#2999 = CARTESIAN_POINT ( 'NONE',  ( 9.611390067472999732, -3.334847606888000193, 5.869121315726000709 ) ) ;
#3000 = EDGE_LOOP ( 'NONE', ( #68141, #29600, #65568, #23670, #1333 ) ) ;
#3001 = CARTESIAN_POINT ( 'NONE',  ( 16.03350391962053578, -3.653603504000225932, -11.13263026093549790 ) ) ;
#3002 = CARTESIAN_POINT ( 'NONE',  ( 8.534480646793999981, -3.011617647609999615, 8.801438026873999121 ) ) ;
#3003 = AXIS2_PLACEMENT_3D ( 'NONE', #26242, #5251, #11516 ) ;
#3004 = CARTESIAN_POINT ( 'NONE',  ( 17.99626221348004407, -0.5795518042670582126, -13.98800095993140857 ) ) ;
#3005 = VERTEX_POINT ( 'NONE', #21868 ) ;
#3006 = CARTESIAN_POINT ( 'NONE',  ( 6.831155956914999550, -9.270367636368000319, 5.219306890235999141 ) ) ;
#3007 = CARTESIAN_POINT ( 'NONE',  ( 23.73952317692686975, -9.827649483940422925, -9.725500440716153605 ) ) ;
#3008 = DIRECTION ( 'NONE',  ( 0.000000000000000000, -1.000000000000000000, 0.000000000000000000 ) ) ;
#3009 = CIRCLE ( 'NONE', #67719, 0.2999999999999999334 ) ;
#3010 = LINE ( 'NONE', #3352, #52098 ) ;
#3011 = CARTESIAN_POINT ( 'NONE',  ( 24.66807826193639031, 3.571100427759083651, 12.15100773348912178 ) ) ;
#3012 = ORIENTED_EDGE ( 'NONE', *, *, #50136, .F. ) ;
#3013 = CARTESIAN_POINT ( 'NONE',  ( 8.721802827889566956, -2.874603711571219744, 6.749639981086952290 ) ) ;
#3014 = CARTESIAN_POINT ( 'NONE',  ( 11.59999999999999964, 4.935123867447915202, 8.208828950335220753 ) ) ;
#3015 = CARTESIAN_POINT ( 'NONE',  ( 11.09999999999999964, -6.075667615221999718, -5.238593909383999048 ) ) ;
#3016 = EDGE_CURVE ( 'NONE', #38787, #35474, #57837, .T. ) ;
#3017 = CARTESIAN_POINT ( 'NONE',  ( 9.873096873515667227, 2.782534154164606921, 7.827184855449101697 ) ) ;
#3018 = AXIS2_PLACEMENT_3D ( 'NONE', #63932, #10799, #5892 ) ;
#3019 = DIRECTION ( 'NONE',  ( 0.000000000000000000, -1.000000000000000000, 0.000000000000000000 ) ) ;
#3020 = EDGE_LOOP ( 'NONE', ( #11322, #30908, #55815, #10074 ) ) ;
#3021 = CARTESIAN_POINT ( 'NONE',  ( 23.60000336012799593, 13.25014977213286471, -4.189788727593960260 ) ) ;
#3022 = ADVANCED_FACE ( 'NONE', ( #10691 ), #33063, .F. ) ;
#3023 = CARTESIAN_POINT ( 'NONE',  ( 0.09997256829956271962, -2.799974420760032334, -1.315021563105355128E-09 ) ) ;
#3024 = CARTESIAN_POINT ( 'NONE',  ( 7.043572165045040911, 2.453565085646790767, -8.528385632692831564 ) ) ;
#3025 = CARTESIAN_POINT ( 'NONE',  ( 24.14062753054661314, -3.327835720320030166, -12.49067376861903433 ) ) ;
#3026 = CARTESIAN_POINT ( 'NONE',  ( 11.09999999999999964, -1.300000000000000044, -9.662944685757000940 ) ) ;
#3027 = CARTESIAN_POINT ( 'NONE',  ( 12.70241326318844877, -0.6168528257048864205, -13.88157091029610157 ) ) ;
#3028 = CARTESIAN_POINT ( 'NONE',  ( 18.16584637247986933, -2.632875908479945348, 12.41964751440798409 ) ) ;
#3029 = ORIENTED_EDGE ( 'NONE', *, *, #2832, .F. ) ;
#3030 = CARTESIAN_POINT ( 'NONE',  ( 10.69057802013490033, -5.033226574983999946, -7.475947032624040034 ) ) ;
#3031 = ORIENTED_EDGE ( 'NONE', *, *, #23349, .F. ) ;
#3032 = CARTESIAN_POINT ( 'NONE',  ( 10.31457848836000046, 5.362142879234999882, 6.677781064327999339 ) ) ;
#3033 = CARTESIAN_POINT ( 'NONE',  ( 0.1499942179679999987, 1.384928887584813584, 2.402872127494069421 ) ) ;
#3034 = CARTESIAN_POINT ( 'NONE',  ( 10.11453584122999949, 5.322769172805999816, -7.951018786192998178 ) ) ;
#3035 = CARTESIAN_POINT ( 'NONE',  ( 2.977758589606999795, 3.090212625808999913, -2.049442917693999888 ) ) ;
#3036 = CARTESIAN_POINT ( 'NONE',  ( 9.922182479546000522, -3.489927462211000364, -9.111803974470001677 ) ) ;
#3037 = CARTESIAN_POINT ( 'NONE',  ( 24.30000000000000071, -8.756202924575998026, -7.455126447192999883 ) ) ;
#3038 = CARTESIAN_POINT ( 'NONE',  ( 23.58461259684199973, 13.39492983452999830, 4.041214499598000387 ) ) ;
#3039 = VERTEX_POINT ( 'NONE', #48107 ) ;
#3040 = CARTESIAN_POINT ( 'NONE',  ( 10.99764694612700033, -5.059486515935999407, 7.077178005756699974 ) ) ;
#3041 = CARTESIAN_POINT ( 'NONE',  ( 11.02786554143000153, 5.596226216413000110, 7.209502215883999199 ) ) ;
#3042 = CARTESIAN_POINT ( 'NONE',  ( 24.39664835772133600, -8.853227849050998799, -8.853227849050998799 ) ) ;
#3043 = CARTESIAN_POINT ( 'NONE',  ( 10.17500046684965120, 2.650307855385062972, 7.500001770945063484 ) ) ;
#3045 = CARTESIAN_POINT ( 'NONE',  ( 9.162715019320227583, 3.042330479684312472, 8.452182092981665562 ) ) ;
#3044 = CARTESIAN_POINT ( 'NONE',  ( 9.848730799670999403, 2.769737997918999994, 6.441853401936000090 ) ) ;
#3046 = CARTESIAN_POINT ( 'NONE',  ( 10.82179975933729921, 4.948878321068100661, -7.173532873542499466 ) ) ;
#3047 = CIRCLE ( 'NONE', #46627, 0.5000000000000004441 ) ;
#3048 = CARTESIAN_POINT ( 'NONE',  ( 24.30000000000000071, -2.524919604596999712, 12.12772056298999956 ) ) ;
#3049 = COLOUR_RGB ( '', 0.08235294, 0.09019608, 0.10196078) ;
#3050 = CARTESIAN_POINT ( 'NONE',  ( 9.300405316139999101, 3.786750623988900166, -8.481512610189300361 ) ) ;
#3051 = CARTESIAN_POINT ( 'NONE',  ( 17.81057016328025000, -0.6732419856523113033, 12.58200148172923960 ) ) ;
#3052 = CARTESIAN_POINT ( 'NONE',  ( 7.272653897099000453, -0.7925871808662000584, 0.8087861320687000921 ) ) ;
#3053 = CARTESIAN_POINT ( 'NONE',  ( 0.9681103717476999826, 3.205765437135000173, -1.404659375816999844 ) ) ;
#3054 = CARTESIAN_POINT ( 'NONE',  ( 23.61277708754100146, 10.15828648011000190, 9.482376091975998733 ) ) ;
#3055 = ORIENTED_EDGE ( 'NONE', *, *, #6336, .T. ) ;
#3056 = CARTESIAN_POINT ( 'NONE',  ( 7.550620559621999739, -4.468370631666999770, 8.882152684713000568 ) ) ;
#3057 = CARTESIAN_POINT ( 'NONE',  ( 18.27399547846086136, 2.614774648920893174, 13.75367307402544270 ) ) ;
#3058 = CARTESIAN_POINT ( 'NONE',  ( 8.550900948453382000, 5.350547267263451090, -7.263495630725214092 ) ) ;
#3059 = CARTESIAN_POINT ( 'NONE',  ( 10.01660887879199890, 3.803658216258800184, 8.344486736701099971 ) ) ;
#3060 = VERTEX_POINT ( 'NONE', #58939 ) ;
#3061 = AXIS2_PLACEMENT_3D ( 'NONE', #55633, #23467, #64713 ) ;
#3062 = CARTESIAN_POINT ( 'NONE',  ( 8.539829719592999524, 5.633477595780999714, 7.451234169193000412 ) ) ;
#3064 = CARTESIAN_POINT ( 'NONE',  ( 0.6708157676188386542, 0.2100481489804951751, 3.532047167415213629 ) ) ;
#3063 = CARTESIAN_POINT ( 'NONE',  ( 9.143660841233000269, 2.235961884443999459, -6.794506518623999902 ) ) ;
#3065 = CARTESIAN_POINT ( 'NONE',  ( 11.15264221959000146, 2.317063201199000222, -7.596564358366999947 ) ) ;
#3066 = ORIENTED_EDGE ( 'NONE', *, *, #64730, .F. ) ;
#3067 = CARTESIAN_POINT ( 'NONE',  ( 5.221693173016666023, 0.7554284705563509839, -1.310679582531386167 ) ) ;
#3068 = CARTESIAN_POINT ( 'NONE',  ( 17.78978190923680458, -3.208919636066283498, -13.62728338959921537 ) ) ;
#3069 = CARTESIAN_POINT ( 'NONE',  ( 10.21462282008599942, 4.523146351753199568, 6.656181553372300108 ) ) ;
#3070 = CARTESIAN_POINT ( 'NONE',  ( 9.743567407955000093, -5.287392049455999832, 8.939957179821000466 ) ) ;
#3071 = DIRECTION ( 'NONE',  ( -0.1522489054329967118, -0.9525130356996803771, -0.2637028396066944946 ) ) ;
#3072 = VERTEX_POINT ( 'NONE', #48451 ) ;
#3073 = CARTESIAN_POINT ( 'NONE',  ( 11.72754826524499983, -3.413272067235999963, 11.89753034518999897 ) ) ;
#3074 = EDGE_CURVE ( 'NONE', #42736, #40281, #29519, .T. ) ;
#3075 = ADVANCED_FACE ( 'NONE', ( #34106 ), #50517, .T. ) ;
#3076 = CARTESIAN_POINT ( 'NONE',  ( 11.10664194037999941, -5.324199331986000594, -7.809344861333999965 ) ) ;
#3077 = CARTESIAN_POINT ( 'NONE',  ( 7.966914046381088355, -2.303960697091592014, 7.114913321231458809 ) ) ;
#3078 = CARTESIAN_POINT ( 'NONE',  ( 9.848732933287999813, -2.769734897491000325, 6.441850735262000249 ) ) ;
#3079 = CARTESIAN_POINT ( 'NONE',  ( 11.72433327354039889, -4.983220429128399687, -6.856888818507299810 ) ) ;
#3080 = CARTESIAN_POINT ( 'NONE',  ( 10.53590035061499997, -3.659038130401700339, 6.267064942904999825 ) ) ;
#3081 = EDGE_LOOP ( 'NONE', ( #7939, #42566, #1511, #24982 ) ) ;
#3082 = CARTESIAN_POINT ( 'NONE',  ( 10.35353477906000030, -4.571505382416000351, -4.862086577461999681 ) ) ;
#3083 = CARTESIAN_POINT ( 'NONE',  ( 10.62426357027499968, -2.745128867668000350, 7.257895958275299542 ) ) ;
#3084 = EDGE_LOOP ( 'NONE', ( #18436, #5800, #47000, #44840, #64223 ) ) ;
#3085 = LINE ( 'NONE', #28995, #10507 ) ;
#3086 = ORIENTED_EDGE ( 'NONE', *, *, #37007, .F. ) ;
#3087 = CARTESIAN_POINT ( 'NONE',  ( 9.397139116365000433, -4.993413662858000812, -9.088148847710000311 ) ) ;
#3088 = CARTESIAN_POINT ( 'NONE',  ( 8.406645280410000254, 3.807713920470999991, -9.221758713517999695 ) ) ;
#3089 = B_SPLINE_CURVE_WITH_KNOTS ( 'NONE', 3,
 ( #30741, #29472, #50781, #62541 ),
 .UNSPECIFIED., .F., .F.,
 ( 4, 4 ),
 ( 0.000000000000000000, 1.000000000000000000 ),
 .UNSPECIFIED. ) ;
#3090 = FACE_OUTER_BOUND ( 'NONE', #60427, .T. ) ;
#3091 = DIRECTION ( 'NONE',  ( 1.000000000000000000, 0.000000000000000000, 0.000000000000000000 ) ) ;
#3092 = CARTESIAN_POINT ( 'NONE',  ( 12.32688384993702080, 2.902596799746486322, -12.34862005174977462 ) ) ;
#3093 = VECTOR ( 'NONE', #51941, 1000.000000000000227 ) ;
#3094 = CARTESIAN_POINT ( 'NONE',  ( 10.71462282008599942, -3.476853648246800432, 6.656181553372300108 ) ) ;
#3095 = CARTESIAN_POINT ( 'NONE',  ( 8.335885841230000537, 4.310355144869000732, 9.459505265942000918 ) ) ;
#3096 = ORIENTED_EDGE ( 'NONE', *, *, #37727, .T. ) ;
#3097 = CARTESIAN_POINT ( 'NONE',  ( 5.002606837613999602, -0.4199405305951999789, 1.440017343911000003 ) ) ;
#3098 = AXIS2_PLACEMENT_3D ( 'NONE', #5641, #36435, #58447 ) ;
#3099 = CARTESIAN_POINT ( 'NONE',  ( 9.176355646795000709, -2.935738482289000029, 6.259841087764999479 ) ) ;
#3100 = CARTESIAN_POINT ( 'NONE',  ( 17.92038287127229523, -0.6379138416578085113, 13.98550699733554303 ) ) ;
#3101 = ORIENTED_EDGE ( 'NONE', *, *, #20313, .T. ) ;
#3102 = CARTESIAN_POINT ( 'NONE',  ( 12.14402373937352841, -2.776896049134141009, -12.29021278449864774 ) ) ;
#3103 = EDGE_CURVE ( 'NONE', #64627, #19590, #12079, .T. ) ;
#3104 = CARTESIAN_POINT ( 'NONE',  ( 10.39918582084299992, 3.253651555277099927, 8.362701637490498996 ) ) ;
#3105 =( GEOMETRIC_REPRESENTATION_CONTEXT ( 3 ) GLOBAL_UNCERTAINTY_ASSIGNED_CONTEXT ( ( #34387 ) ) GLOBAL_UNIT_ASSIGNED_CONTEXT ( ( #25560, #9466, #41637 ) ) REPRESENTATION_CONTEXT ( 'NONE', 'WORKASPACE' ) );
#3106 = CARTESIAN_POINT ( 'NONE',  ( 11.09178064679000109, -4.578543110806999827, -8.908602356389000221 ) ) ;
#3107 = CARTESIAN_POINT ( 'NONE',  ( 6.440443173016666911, -0.1963495408493673156, 1.499999999999999556 ) ) ;
#3108 = CARTESIAN_POINT ( 'NONE',  ( 18.35168611684299833, -2.962034070680999776, -12.02052262816000017 ) ) ;
#3109 = CARTESIAN_POINT ( 'NONE',  ( 24.40777907856499951, -8.879621479695998687, 9.005112135669000040 ) ) ;
#3110 = DIRECTION ( 'NONE',  ( 0.000000000000000000, -1.000000000000000000, 0.000000000000000000 ) ) ;
#3111 = DIRECTION ( 'NONE',  ( -1.000000000000000000, 0.000000000000000000, 0.000000000000000000 ) ) ;
#3112 = VECTOR ( 'NONE', #42024, 1000.000000000000227 ) ;
#3113 = CARTESIAN_POINT ( 'NONE',  ( 11.63825819896753977, -4.851203879749700576, -7.660469764776300039 ) ) ;
#3114 = CARTESIAN_POINT ( 'NONE',  ( 11.10887482311539998, -2.815046254222000055, -7.978749413531599721 ) ) ;
#3115 = CARTESIAN_POINT ( 'NONE',  ( 8.560832189570803052, -5.056892070296432173, 6.275968648838331276 ) ) ;
#3116 = ORIENTED_EDGE ( 'NONE', *, *, #69052, .F. ) ;
#3117 = ORIENTED_EDGE ( 'NONE', *, *, #28669, .T. ) ;
#3118 = VECTOR ( 'NONE', #55368, 1000.000000000000227 ) ;
#3119 = CARTESIAN_POINT ( 'NONE',  ( 12.10000000004390408, -11.04996331180911717, 3.691231724050993979 ) ) ;
#3120 = CARTESIAN_POINT ( 'NONE',  ( 17.96842299895978101, 2.968890910958777773, 13.56270300417350860 ) ) ;
#3121 = CARTESIAN_POINT ( 'NONE',  ( 24.23279320724300234, -3.402312112046000259, 12.43077114457000043 ) ) ;
#3122 = DIRECTION ( 'NONE',  ( -0.9999999999999987788, -4.835299792554983623E-08, 1.472960222966996186E-08 ) ) ;
#3123 = CARTESIAN_POINT ( 'NONE',  ( 17.87877696946767614, 3.124133162484063586, 12.20654824865394517 ) ) ;
#3124 = CARTESIAN_POINT ( 'NONE',  ( 6.899999691988000450, 12.99045401563999924, -1.690592933733000125 ) ) ;
#3125 = CARTESIAN_POINT ( 'NONE',  ( 10.53138775541999905, 5.607751175212000838, 7.280102404048999887 ) ) ;
#3126 = AXIS2_PLACEMENT_3D ( 'NONE', #24427, #2752, #45413 ) ;
#3127 = CARTESIAN_POINT ( 'NONE',  ( 24.67921321731900264, -3.567517257907000250, -12.13750614118000115 ) ) ;
#3128 = ORIENTED_EDGE ( 'NONE', *, *, #16611, .F. ) ;
#3129 = CARTESIAN_POINT ( 'NONE',  ( 12.47240630447280907, -1.970775872724743749, 12.55927287175691731 ) ) ;
#3130 = CARTESIAN_POINT ( 'NONE',  ( 8.920468108405998464, -3.033597967472499768, -7.773695785133000413 ) ) ;
#3131 = B_SPLINE_CURVE_WITH_KNOTS ( 'NONE', 3,
 ( #49086, #43849, #1198, #27080 ),
 .UNSPECIFIED., .F., .F.,
 ( 4, 4 ),
 ( 0.000000000000000000, 0.1255288163819863745 ),
 .UNSPECIFIED. ) ;
#3132 = CARTESIAN_POINT ( 'NONE',  ( 9.423523952092001110, 4.993991073313000406, 8.578107851305000864 ) ) ;
#3133 = CARTESIAN_POINT ( 'NONE',  ( 11.68412378248529926, -4.549028353065900809, 8.538714411016998795 ) ) ;
#3134 = PRODUCT ( 'Terminal Screw 3', 'Terminal Screw 3', '', ( #25347 ) ) ;
#3135 = CARTESIAN_POINT ( 'NONE',  ( 10.27610941423800028, 4.844410192686099847, -6.733017893878099791 ) ) ;
#3136 = CARTESIAN_POINT ( 'NONE',  ( 12.18832871607760460, 0.1019009512359494996, 12.69945530929771493 ) ) ;
#3137 = EDGE_CURVE ( 'NONE', #26116, #66034, #2961, .T. ) ;
#3138 = EDGE_CURVE ( 'NONE', #57343, #27955, #66246, .T. ) ;
#3139 = CARTESIAN_POINT ( 'NONE',  ( 8.572267219592999865, 2.606995215518000286, 6.345762205468999717 ) ) ;
#3140 = CARTESIAN_POINT ( 'NONE',  ( 10.40726830891999910, 3.797905842462999892, 5.889914049998000500 ) ) ;
#3141 = CARTESIAN_POINT ( 'NONE',  ( 12.79462099885201454, 1.875000035136120236, 12.57541665307954837 ) ) ;
#3142 = ORIENTED_EDGE ( 'NONE', *, *, #54835, .T. ) ;
#3143 = CARTESIAN_POINT ( 'NONE',  ( 8.549914158773001205, 2.141799395716999843, -7.895788736628000848 ) ) ;
#3144 = CARTESIAN_POINT ( 'NONE',  ( 10.91195257254739914, 2.772832764353999835, -7.856899084262298771 ) ) ;
#3145 = CARTESIAN_POINT ( 'NONE',  ( 24.30000000000000071, -2.204728229456999866, 11.99913219504999873 ) ) ;
#3147 = DIRECTION ( 'NONE',  ( 0.000000000000000000, -0.7071067811865475727, -0.7071067811865475727 ) ) ;
#3146 = CARTESIAN_POINT ( 'NONE',  ( 7.764230646791999924, -4.628942671846000501, 5.991663889842000046 ) ) ;
#3148 = CARTESIAN_POINT ( 'NONE',  ( 9.503442991500000048, -4.054579081944059915, 8.365291319916600798 ) ) ;
#3149 = CARTESIAN_POINT ( 'NONE',  ( 11.01872200990539952, -4.947480442174099657, -7.169497859994799605 ) ) ;
#3150 = VERTEX_POINT ( 'NONE', #61011 ) ;
#3151 = CARTESIAN_POINT ( 'NONE',  ( 1.009835424300000062, 3.696170276785000208, -0.6823948523853999859 ) ) ;
#3152 = CARTESIAN_POINT ( 'NONE',  ( 12.09999922233642344, 11.66744139996707119, -3.971920075670921424 ) ) ;
#3154 = CARTESIAN_POINT ( 'NONE',  ( 11.42397234076999979, 3.432581932914000156, -11.79497283202000091 ) ) ;
#3153 = CARTESIAN_POINT ( 'NONE',  ( 11.07213888212999997, -2.731532893235999904, -5.080375744811999716 ) ) ;
#3155 = PLANE ( 'NONE',  #42507 ) ;
#3156 = B_SPLINE_CURVE_WITH_KNOTS ( 'NONE', 3,
 ( #43988, #42944, #22301, #16707, #42602, #11462 ),
 .UNSPECIFIED., .F., .F.,
 ( 4, 1, 1, 4 ),
 ( 0.000000000000000000, 0.3333333333333000081, 0.6666666666667000474, 1.000000000000000000 ),
 .UNSPECIFIED. ) ;
#3157 = B_SPLINE_CURVE_WITH_KNOTS ( 'NONE', 3,
 ( #38807, #33913, #39846, #50334 ),
 .UNSPECIFIED., .F., .F.,
 ( 4, 4 ),
 ( 0.8719585443747394082, 1.000000000000000000 ),
 .UNSPECIFIED. ) ;
#3158 = CARTESIAN_POINT ( 'NONE',  ( 5.699999999554000496, -0.3000000004460000036, 9.662944681662999358 ) ) ;
#3159 = FACE_OUTER_BOUND ( 'NONE', #12491, .T. ) ;
#3160 = DIRECTION ( 'NONE',  ( 0.000000000000000000, 1.000000000000000000, 0.000000000000000000 ) ) ;
#3161 = CARTESIAN_POINT ( 'NONE',  ( 18.49993212792200126, -2.908182645667999999, -12.18276646858999968 ) ) ;
#3162 = CARTESIAN_POINT ( 'NONE',  ( 9.298691940377999288, -5.159251056493999954, 9.109488373271000583 ) ) ;
#3163 = ORIENTED_EDGE ( 'NONE', *, *, #38453, .T. ) ;
#3164 = CARTESIAN_POINT ( 'NONE',  ( 9.523698341228998387, 4.852728889087999598, 8.683917172082999514 ) ) ;
#3165 = EDGE_CURVE ( 'NONE', #21223, #852, #54504, .T. ) ;
#3166 = CARTESIAN_POINT ( 'NONE',  ( 7.100000000000000533, 12.50865771883999855, 2.924687089724999911 ) ) ;
#3167 = CARTESIAN_POINT ( 'NONE',  ( 7.446475209053147637, -2.261386354369964824, 7.556112484256551909 ) ) ;
#3168 = CONICAL_SURFACE ( 'NONE', #51185, 12.44999944941000081, 0.7853981146832407223 ) ;
#3169 = CARTESIAN_POINT ( 'NONE',  ( 11.41486084871699802, 2.792989229543000107, -7.825000000000000178 ) ) ;
#3170 = CARTESIAN_POINT ( 'NONE',  ( 1.361792155651999847, -1.181558911493999942, 3.215390670984000554 ) ) ;
#3171 = VERTEX_POINT ( 'NONE', #23950 ) ;
#3172 = CARTESIAN_POINT ( 'NONE',  ( 1.858550344655261810, 1.693358345689038202, 2.835668913445299477 ) ) ;
#3173 = EDGE_CURVE ( 'NONE', #12996, #16254, #43901, .T. ) ;
#3174 = CARTESIAN_POINT ( 'NONE',  ( 12.35159063708299954, -3.174974693948799942, 7.268038553423699533 ) ) ;
#3175 = CYLINDRICAL_SURFACE ( 'NONE', #64330, 0.5000000000000000000 ) ;
#3176 = CARTESIAN_POINT ( 'NONE',  ( 9.757669403192000601, 4.489270656625000022, 5.986034819543999852 ) ) ;
#3177 = CARTESIAN_POINT ( 'NONE',  ( 11.09256785386839894, 3.167490253789400523, 6.939751505745099358 ) ) ;
#3178 = AXIS2_PLACEMENT_3D ( 'NONE', #56692, #19974, #15064 ) ;
#3179 = CARTESIAN_POINT ( 'NONE',  ( 9.612308556531111492, -3.034755127823582921, 8.468084591988906951 ) ) ;
#3180 = DIRECTION ( 'NONE',  ( 0.000000000000000000, -0.2461538461537955691, -0.9692307692307821076 ) ) ;
#3181 = CARTESIAN_POINT ( 'NONE',  ( 7.816481737960005560, -3.426408505174418195, 6.252170097456407838 ) ) ;
#3182 = CARTESIAN_POINT ( 'NONE',  ( 11.40010796094000334, -6.616929226765999876E-14, -1.143529715363999905E-14 ) ) ;
#3183 = CARTESIAN_POINT ( 'NONE',  ( 12.36790781771545689, -2.946786910879655608, 12.33618673617669970 ) ) ;
#3184 = CARTESIAN_POINT ( 'NONE',  ( 7.696932380987085764, 5.748606536197243599, 7.412610333444322741 ) ) ;
#3185 = ORIENTED_EDGE ( 'NONE', *, *, #62808, .T. ) ;
#3186 = CARTESIAN_POINT ( 'NONE',  ( 17.65136412466926075, -3.242045876614692013, 13.61943996000380430 ) ) ;
#3187 = DIRECTION ( 'NONE',  ( -1.000000000000000000, 0.000000000000000000, 0.000000000000000000 ) ) ;
#3188 = ORIENTED_EDGE ( 'NONE', *, *, #15214, .T. ) ;
#3189 = ORIENTED_EDGE ( 'NONE', *, *, #34206, .T. ) ;
#3190 = CARTESIAN_POINT ( 'NONE',  ( 10.29399293566599916, 4.546741702992100009, 6.829299525004299376 ) ) ;
#3191 = CARTESIAN_POINT ( 'NONE',  ( 9.729346873516670158, 3.836375382625535124, -6.249999999999999112 ) ) ;
#3192 = ADVANCED_FACE ( 'NONE', ( #7181 ), #6830, .T. ) ;
#3193 = FACE_OUTER_BOUND ( 'NONE', #20944, .T. ) ;
#3194 = CARTESIAN_POINT ( 'NONE',  ( 10.71756692516999898, 3.040224182812999665, 8.808452309630000698 ) ) ;
#3195 = CARTESIAN_POINT ( 'NONE',  ( 10.85290485628999946, 3.170386876061999537, -8.782184998573001167 ) ) ;
#3196 = CARTESIAN_POINT ( 'NONE',  ( 10.24006601915162484, -4.042412777185713679, -8.373918476712228554 ) ) ;
#3197 = CARTESIAN_POINT ( 'NONE',  ( 9.479212726990999371, -4.071727350623000063, 9.089303488377000306 ) ) ;
#3198 = CARTESIAN_POINT ( 'NONE',  ( 18.26841343935702255, 0.1288995356414767979, -12.59934597632939735 ) ) ;
#3199 = CARTESIAN_POINT ( 'NONE',  ( 10.68054891417000007, -2.768175152062000155, -6.114413274984999980 ) ) ;
#3200 = CARTESIAN_POINT ( 'NONE',  ( 10.80133863405319872, -3.465595476214000215, -8.181696703306599261 ) ) ;
#3201 = DIRECTION ( 'NONE',  ( 0.000000000000000000, 1.000000000000000000, 0.000000000000000000 ) ) ;
#3202 = ORIENTED_EDGE ( 'NONE', *, *, #10334, .T. ) ;
#3203 = CARTESIAN_POINT ( 'NONE',  ( 11.12486991174999851, -5.426792458777999428, -5.164830891052999640 ) ) ;
#3204 = SHAPE_REPRESENTATION_RELATIONSHIP ( 'NONE' , 'NONE' ,  #12958, #43565 ) ;
#3205 = CARTESIAN_POINT ( 'NONE',  ( 24.71768044457226665, 8.650200248279249493, 8.600992414847871359 ) ) ;
#3206 = AXIS2_PLACEMENT_3D ( 'NONE', #47649, #30883, #58815 ) ;
#3207 = CARTESIAN_POINT ( 'NONE',  ( 9.099999931440999390, 5.246365646610000155, 7.595250590283559866 ) ) ;
#3208 = CARTESIAN_POINT ( 'NONE',  ( 9.025809814041000578, 4.782507962695600412, -8.511961036725999463 ) ) ;
#3209 = CARTESIAN_POINT ( 'NONE',  ( 12.09560501594671500, 2.367229839359596522, 13.79841893036761213 ) ) ;
#3210 = CARTESIAN_POINT ( 'NONE',  ( 9.687876499438001332, -5.912252057206999645, 7.772299417761000306 ) ) ;
#3211 = ORIENTED_EDGE ( 'NONE', *, *, #45064, .T. ) ;
#3212 = AXIS2_PLACEMENT_3D ( 'NONE', #68224, #20342, #15102 ) ;
#3213 = CARTESIAN_POINT ( 'NONE',  ( 12.64392860536586127, 0.6042188441601874516, -12.68064732209416867 ) ) ;
#3214 = DIRECTION ( 'NONE',  ( -1.000000000000000000, 0.000000000000000000, 0.000000000000000000 ) ) ;
#3215 = B_SPLINE_CURVE_WITH_KNOTS ( 'NONE', 3,
 ( #63658, #48274, #21696, #43032 ),
 .UNSPECIFIED., .F., .F.,
 ( 4, 4 ),
 ( 0.000000000000000000, 1.000000000000000000 ),
 .UNSPECIFIED. ) ;
#3216 = ORIENTED_EDGE ( 'NONE', *, *, #19477, .F. ) ;
#3217 = CARTESIAN_POINT ( 'NONE',  ( 11.28192504596561996, -3.091022006579346115, -7.825000185715046186 ) ) ;
#3218 = CARTESIAN_POINT ( 'NONE',  ( 12.80505043854144276, -0.6878608935795337276, 12.61273126665598276 ) ) ;
#3219 = CARTESIAN_POINT ( 'NONE',  ( 10.61476354018240187, -2.782534154164604256, -7.172815144550903632 ) ) ;
#3220 = CARTESIAN_POINT ( 'NONE',  ( 4.582870291988999867, -1.595997307511999752, 0.3299522913273999492 ) ) ;
#3221 = CARTESIAN_POINT ( 'NONE',  ( 8.698544349573893442, 4.680090960897770103, -8.679957510353851546 ) ) ;
#3222 = ADVANCED_FACE ( 'NONE', ( #65205 ), #40779, .F. ) ;
#3223 = EDGE_CURVE ( 'NONE', #52567, #7034, #44259, .T. ) ;
#3224 = CARTESIAN_POINT ( 'NONE',  ( 0.09605912983313999454, 2.413895893032000028, 2.806361486493000434 ) ) ;
#3225 = DIRECTION ( 'NONE',  ( -2.154007395656495261E-21, 3.276905819395100166E-06, -0.9999999999946310725 ) ) ;
#3226 = DIRECTION ( 'NONE',  ( 0.000000000000000000, -0.2588190451024934835, -0.9659258262890757507 ) ) ;
#3227 = CARTESIAN_POINT ( 'NONE',  ( 9.174722005181999762, -5.536248950452999473, -7.355084988757000453 ) ) ;
#3228 = EDGE_CURVE ( 'NONE', #2494, #12730, #63524, .T. ) ;
#3229 = CARTESIAN_POINT ( 'NONE',  ( 11.24441369783139777, 3.956299011112040187, -8.365094684940499903 ) ) ;
#3230 = CARTESIAN_POINT ( 'NONE',  ( 8.493376396436000064, 2.902501347630999984, -6.607668289109998483 ) ) ;
#3231 = CARTESIAN_POINT ( 'NONE',  ( 10.79701415876999882, 5.792870175253000298, -7.049262931951000510 ) ) ;
#3232 = CARTESIAN_POINT ( 'NONE',  ( 9.404684229509999938, 3.195116560491999991, -6.690125258578699885 ) ) ;
#3234 = CARTESIAN_POINT ( 'NONE',  ( 9.241501215035999195, -4.228777700933000538, 6.624106355763400344 ) ) ;
#3233 = CARTESIAN_POINT ( 'NONE',  ( 15.72922381500400313, -8.763625284509998892, -7.896085856502000233 ) ) ;
#3235 = DIRECTION ( 'NONE',  ( 0.000000000000000000, -1.000000000000000000, 0.000000000000000000 ) ) ;
#3236 = ORIENTED_EDGE ( 'NONE', *, *, #33621, .T. ) ;
#3237 = B_SPLINE_CURVE_WITH_KNOTS ( 'NONE', 3,
 ( #26257, #2783, #44067, #65368, #17488, #33571 ),
 .UNSPECIFIED., .F., .F.,
 ( 4, 1, 1, 4 ),
 ( 0.000000000000000000, 0.3333333333333000081, 0.6666666666667000474, 1.000000000000000000 ),
 .UNSPECIFIED. ) ;
#3238 = CARTESIAN_POINT ( 'NONE',  ( 10.98656920625009903, 4.032067152264009913, 8.391549386185598536 ) ) ;
#3239 = CARTESIAN_POINT ( 'NONE',  ( 9.166075977534999808, -4.023333687735000552, 9.122281080215000060 ) ) ;
#3240 = CARTESIAN_POINT ( 'NONE',  ( 9.251759580228998914, 2.889471124893000287, 7.765443149353999708 ) ) ;
#3241 = CARTESIAN_POINT ( 'NONE',  ( 9.100254395947628083, 3.149024541069663563, -7.296596368717002790 ) ) ;
#3242 = CARTESIAN_POINT ( 'NONE',  ( 9.615066448851507630, -5.349942704376990044, -7.499996115248991124 ) ) ;
#3243 = DIRECTION ( 'NONE',  ( 1.000000000000000000, 0.000000000000000000, 0.000000000000000000 ) ) ;
#3244 = CARTESIAN_POINT ( 'NONE',  ( 23.56666365135700403, 8.694246338465996260, -8.392498551259993889 ) ) ;
#3245 = VERTEX_POINT ( 'NONE', #50865 ) ;
#3246 = CARTESIAN_POINT ( 'NONE',  ( 9.126063610504999701, -3.531653260805799999, -8.541338455964998744 ) ) ;
#3247 = CARTESIAN_POINT ( 'NONE',  ( 10.68287132187968602, -5.051222535738905783, -5.058047779293387336 ) ) ;
#3248 = CARTESIAN_POINT ( 'NONE',  ( 11.06080513895999928, -2.973119161490000106, 8.070849345005600028 ) ) ;
#3249 = CARTESIAN_POINT ( 'NONE',  ( 17.87931509819275888, 1.836668601340711193, -12.46541920085824451 ) ) ;
#3250 = CARTESIAN_POINT ( 'NONE',  ( 2.709306799209334038, -3.058252359239909790, 1.762666431298136382 ) ) ;
#3251 = DIRECTION ( 'NONE',  ( 0.000000000000000000, -0.1218274111675002047, 0.9925512993736015366 ) ) ;
#3252 = CARTESIAN_POINT ( 'NONE',  ( 12.18026105735517461, 2.480641341450430026, -13.67754910896964660 ) ) ;
#3253 = CARTESIAN_POINT ( 'NONE',  ( 8.996132306828998892, -4.474581801608000120, -6.279517683005999551 ) ) ;
#3254 = CARTESIAN_POINT ( 'NONE',  ( 9.036851812263130057, 5.286388725631042895, -7.027200320027173319 ) ) ;
#3255 = EDGE_LOOP ( 'NONE', ( #27597, #8885, #11706, #56447 ) ) ;
#3256 = CARTESIAN_POINT ( 'NONE',  ( 24.77999265559800079, -12.27030725872999817, -2.912406685646000248 ) ) ;
#3257 = CARTESIAN_POINT ( 'NONE',  ( 12.30932141792787604, 0.5329747956505024309, -13.98985355243729423 ) ) ;
#3258 = CARTESIAN_POINT ( 'NONE',  ( 10.73912476063878607, 2.651371201321757187, 7.263709536580951642 ) ) ;
#3259 = CARTESIAN_POINT ( 'NONE',  ( 10.03695705046682818, -5.286467410629250629, -7.027033154920563796 ) ) ;
#3260 = CARTESIAN_POINT ( 'NONE',  ( 18.18005044388380043, 2.499999700417821380, 12.45156116530496604 ) ) ;
#3261 = CARTESIAN_POINT ( 'NONE',  ( 23.60000000000000497, -12.52449491606653709, -6.096403221384886884 ) ) ;
#3262 = CARTESIAN_POINT ( 'NONE',  ( 11.89210538575740017, -3.157545584346100220, 7.701417844014099678 ) ) ;
#3263 = ORIENTED_EDGE ( 'NONE', *, *, #15874, .F. ) ;
#3264 = CARTESIAN_POINT ( 'NONE',  ( 4.000000000000000888, -2.149963194831999935, 0.2827069376517963306 ) ) ;
#3265 = CARTESIAN_POINT ( 'NONE',  ( 18.05244152647595257, 3.049274110449839092, -13.66389386579125897 ) ) ;
#3266 = ORIENTED_EDGE ( 'NONE', *, *, #45588, .F. ) ;
#3267 = CARTESIAN_POINT ( 'NONE',  ( 10.79522949779699914, -3.519000825516800379, 6.778648208007999720 ) ) ;
#3268 = CARTESIAN_POINT ( 'NONE',  ( 24.73253374366442969, 3.116078331550232505, 11.77909370293319036 ) ) ;
#3269 = ADVANCED_FACE ( 'NONE', ( #38647 ), #39001, .T. ) ;
#3270 = CARTESIAN_POINT ( 'NONE',  ( 8.233179719589999834, 5.203550244299999683, -8.391678825488000371 ) ) ;
#3271 = CARTESIAN_POINT ( 'NONE',  ( 10.06805547886711594, 2.257110507042949799, -7.995645982437191712 ) ) ;
#3272 = CARTESIAN_POINT ( 'NONE',  ( 10.51925056272499859, -2.825232917634000085, -7.517410630436119234 ) ) ;
#3273 = CARTESIAN_POINT ( 'NONE',  ( 13.63315305048521964, -12.20113081363247076, -2.519319003639654220 ) ) ;
#3274 = EDGE_CURVE ( 'NONE', #12955, #37266, #55075, .T. ) ;
#3275 = DIRECTION ( 'NONE',  ( 1.000000000000000000, 0.000000000000000000, 0.000000000000000000 ) ) ;
#3276 = ORIENTED_EDGE ( 'NONE', *, *, #54353, .F. ) ;
#3277 = CARTESIAN_POINT ( 'NONE',  ( 7.882561745187770974, 2.667458184526113829, -7.203446184243078143 ) ) ;
#3278 = CARTESIAN_POINT ( 'NONE',  ( 10.64601354018233081, -3.000416447002271170, 8.268183399968638270 ) ) ;
#3279 = CARTESIAN_POINT ( 'NONE',  ( 9.029445280412998542, 5.442817578555000146, -8.106149115450000053 ) ) ;
#3280 = ORIENTED_EDGE ( 'NONE', *, *, #41131, .T. ) ;
#3281 = CARTESIAN_POINT ( 'NONE',  ( 9.753031682810998859, 4.922927894835999574, -8.639534507509999628 ) ) ;
#3282 =( NAMED_UNIT ( * ) PLANE_ANGLE_UNIT ( ) SI_UNIT ( $, .RADIAN. ) );
#3283 = ORIENTED_EDGE ( 'NONE', *, *, #22917, .F. ) ;
#3284 = CARTESIAN_POINT ( 'NONE',  ( 9.759292290062999697, 4.987433183662999703, 8.073332500201798823 ) ) ;
#3285 = CARTESIAN_POINT ( 'NONE',  ( 17.63760627221314081, -1.880133632725761172, -12.57457483776005525 ) ) ;
#3286 = DIRECTION ( 'NONE',  ( -1.000000000000000000, 0.000000000000000000, 0.000000000000000000 ) ) ;
#3287 = CARTESIAN_POINT ( 'NONE',  ( 24.60320129348500018, -12.45517092796000114, -2.982541609212000289 ) ) ;
#3288 = DIRECTION ( 'NONE',  ( 0.000000000000000000, -0.6884191022827257367, 0.7253131321107084695 ) ) ;
#3289 = ORIENTED_EDGE ( 'NONE', *, *, #33539, .T. ) ;
#3290 = CARTESIAN_POINT ( 'NONE',  ( 11.59999999999999964, 3.801977891258315534, 6.428664210949555979 ) ) ;
#3291 = CARTESIAN_POINT ( 'NONE',  ( 5.500000000000000000, -11.00717859340000082, 1.432487142323000118 ) ) ;
#3292 = CARTESIAN_POINT ( 'NONE',  ( 9.099999931440999390, -4.000000000000000000, -7.500000000000000000 ) ) ;
#3293 = CARTESIAN_POINT ( 'NONE',  ( 12.36183802548525179, 3.095880799707793063, -13.65340897264974451 ) ) ;
#3294 = CARTESIAN_POINT ( 'NONE',  ( 9.405747021775999528, -4.961496216383199709, -8.343747244947598674 ) ) ;
#3295 = CARTESIAN_POINT ( 'NONE',  ( 18.23380192947725575, 0.2577288767859139962, 13.99764474128114600 ) ) ;
#3296 = DIRECTION ( 'NONE',  ( 1.000000000000000000, 0.000000000000000000, -6.069219200923000182E-14 ) ) ;
#3297 = EDGE_CURVE ( 'NONE', #44223, #44911, #24975, .T. ) ;
#3298 = ORIENTED_EDGE ( 'NONE', *, *, #16906, .F. ) ;
#3299 = ORIENTED_EDGE ( 'NONE', *, *, #45108, .T. ) ;
#3300 = CARTESIAN_POINT ( 'NONE',  ( 9.219485841232998524, 3.892978337449999771, -8.893414073324001023 ) ) ;
#3301 = CARTESIAN_POINT ( 'NONE',  ( 10.60113158428548097, 5.349785647439726510, -7.263300972600675642 ) ) ;
#3302 = EDGE_CURVE ( 'NONE', #35662, #64677, #11035, .T. ) ;
#3303 = ADVANCED_FACE ( 'NONE', ( #35813 ), #53629, .F. ) ;
#3304 = CARTESIAN_POINT ( 'NONE',  ( 7.465326089856205272, -5.349750919053078313, 7.322903698185732502 ) ) ;
#3305 = CARTESIAN_POINT ( 'NONE',  ( 24.08742125846098503, 3.338819417450129112, 12.58660453514891309 ) ) ;
#3306 = CARTESIAN_POINT ( 'NONE',  ( 23.62017846084600237, 10.21547452202000095, -9.339924903530999245 ) ) ;
#3307 = CARTESIAN_POINT ( 'NONE',  ( 17.76937411412500367, -3.251867979506000150, -11.33740618442000070 ) ) ;
#3309 = CARTESIAN_POINT ( 'NONE',  ( 8.953746459558937332, 2.251940015626868519, 7.420647187261359079 ) ) ;
#3308 = CARTESIAN_POINT ( 'NONE',  ( 10.84091290906799898, -4.722468360609500593, 6.615820196229499572 ) ) ;
#3310 = CARTESIAN_POINT ( 'NONE',  ( 9.065735834902588053, 4.411345979885467727, -8.662764376609992212 ) ) ;
#3311 = EDGE_LOOP ( 'NONE', ( #16784, #34463 ) ) ;
#3312 = DIRECTION ( 'NONE',  ( -1.000000000000000000, 0.000000000000000000, 0.000000000000000000 ) ) ;
#3313 = CARTESIAN_POINT ( 'NONE',  ( 24.35365242081700288, -10.90899669677000006, -3.315896191878997978 ) ) ;
#3314 = CARTESIAN_POINT ( 'NONE',  ( 9.888906509039999904, -2.890602650755999647, -6.682694598879999504 ) ) ;
#3315 = CARTESIAN_POINT ( 'NONE',  ( 12.80505043854143210, 3.248147246781388553, 13.61798588129781251 ) ) ;
#3316 = LINE ( 'NONE', #25674, #15394 ) ;
#3317 = CARTESIAN_POINT ( 'NONE',  ( 21.60000000000000142, -12.52500000000000036, 0.000000000000000000 ) ) ;
#3318 = CARTESIAN_POINT ( 'NONE',  ( 9.243110841233001196, 4.112741311853999271, -5.603466076760000192 ) ) ;
#3319 = EDGE_CURVE ( 'NONE', #37580, #53410, #13840, .T. ) ;
#3321 = VECTOR ( 'NONE', #68066, 999.9999999999998863 ) ;
#3320 = B_SPLINE_CURVE_WITH_KNOTS ( 'NONE', 3,
 ( #36846, #3976, #67958, #58164 ),
 .UNSPECIFIED., .F., .F.,
 ( 4, 4 ),
 ( 0.000000000000000000, 1.000000000000000000 ),
 .UNSPECIFIED. ) ;
#3322 = CARTESIAN_POINT ( 'NONE',  ( 10.51810807141099779, 4.059045408506610109, 6.223352037434000117 ) ) ;
#3323 = DIRECTION ( 'NONE',  ( 0.7071067388045961799, 0.7071068235684964121, -1.176037761303994353E-10 ) ) ;
#3324 = B_SPLINE_SURFACE_WITH_KNOTS ( 'NONE', 3, 3, ( 
 ( #31250, #5353, #53595, #20750 ),
 ( #37511, #37857, #52910, #26692 ),
 ( #15508, #47326, #53247, #68629 ),
 ( #5691, #5007, #9911, #26343 ),
 ( #59182, #10595, #47669, #68981 ),
 ( #10943, #48346, #42421, #21095 ),
 ( #27033, #16531, #63728, #52559 ),
 ( #15840, #64068, #37172, #58491 ),
 ( #48700, #42760, #31937, #48007 ),
 ( #58835, #21770, #106, #11282 ),
 ( #32621, #64407, #452, #21423 ),
 ( #43105, #800, #22117, #25995 ),
 ( #53932, #43462, #6035, #27373 ),
 ( #15159, #36479, #4655, #60227 ),
 ( #12330, #1841, #13031, #65801 ),
 ( #11976, #17928, #54980, #11623 ) ),
 .UNSPECIFIED., .F., .F., .F.,
 ( 4, 1, 1, 1, 1, 1, 1, 1, 1, 1, 1, 1, 1, 4 ),
 ( 4, 4 ),
 ( 0.01677647950063999860, 0.07692307692307999434, 0.1538461538461999845, 0.2307692307692000011, 0.3076923076922999933, 0.3846153846154000133, 0.4615384615385000333, 0.5384615384614999112, 0.6153846153845999867, 0.6923076923076999512, 0.7692307692308000266, 0.8461538461537999600, 0.9230769230769000355, 0.9705716827899999455 ),
 ( -0.1835260008786999963, 1.183623993927000129 ),
 .UNSPECIFIED. ) ;
#3325 = CARTESIAN_POINT ( 'NONE',  ( 0.2681673312783822150, 1.646699379977375699, 2.855331343420156376 ) ) ;
#3326 = CARTESIAN_POINT ( 'NONE',  ( 2.490382077375999703, -2.404207915413000052, 2.200243182853999890 ) ) ;
#3327 = EDGE_LOOP ( 'NONE', ( #15740, #25312, #25715, #3984 ) ) ;
#3328 = CARTESIAN_POINT ( 'NONE',  ( 12.70960625021945134, 0.7131288892044854721, -12.57980326738671906 ) ) ;
#3329 = DIRECTION ( 'NONE',  ( 1.000000000000000000, 0.000000000000000000, 0.000000000000000000 ) ) ;
#3330 = FACE_OUTER_BOUND ( 'NONE', #63610, .T. ) ;
#3331 = CARTESIAN_POINT ( 'NONE',  ( 8.770176658772999900, 3.049618631524000367, 6.392542946894000266 ) ) ;
#3332 = CARTESIAN_POINT ( 'NONE',  ( 18.06247470437139313, -3.164801830692922202, -11.41978211458705594 ) ) ;
#3333 = ORIENTED_EDGE ( 'NONE', *, *, #20575, .T. ) ;
#3334 = CARTESIAN_POINT ( 'NONE',  ( 6.479548602795000889, -0.7569293636342000475, -1.084220404132000048 ) ) ;
#3335 = APPLICATION_PROTOCOL_DEFINITION ( 'draft international standard', 'automotive_design', 1998, #37366 ) ;
#3336 = CARTESIAN_POINT ( 'NONE',  ( 0.6152921912379571978, 0.4809088339291435754, 3.497386196961711491 ) ) ;
#3337 = CARTESIAN_POINT ( 'NONE',  ( 8.745593092018999926, 5.100000000000000533, 6.404090157675000228 ) ) ;
#3338 = CARTESIAN_POINT ( 'NONE',  ( 10.32118582084299874, 3.163839350524900063, 8.466515260542900378 ) ) ;
#3339 = CARTESIAN_POINT ( 'NONE',  ( 10.81524174883999834, 3.971581146373189597, -8.533115712456000423 ) ) ;
#3340 = ORIENTED_EDGE ( 'NONE', *, *, #61926, .T. ) ;
#3341 = CARTESIAN_POINT ( 'NONE',  ( 9.534903635507999908, -3.030945724184999968, 8.761987396837000119 ) ) ;
#3342 = ORIENTED_EDGE ( 'NONE', *, *, #53039, .F. ) ;
#3343 = FACE_BOUND ( 'NONE', #40249, .T. ) ;
#3344 = CARTESIAN_POINT ( 'NONE',  ( 8.304129440378000382, -3.650411072918999800, 6.083135626079000602 ) ) ;
#3345 = CARTESIAN_POINT ( 'NONE',  ( 18.18884185737635661, -0.3547769576528466695, -13.99550803169339730 ) ) ;
#3346 = B_SPLINE_CURVE_WITH_KNOTS ( 'NONE', 3,
 ( #42390, #25618, #19689, #14449, #62332, #20369, #31220, #9183, #35429, #30523, #47636, #68250 ),
 .UNSPECIFIED., .F., .F.,
 ( 4, 1, 1, 1, 1, 1, 1, 1, 1, 4 ),
 ( 0.000000000000000000, 0.1111111114150000051, 0.2222222219940999943, 0.3333333325730999941, 0.4444444431521000216, 0.5555555537312000247, 0.6666666643101999412, 0.7777777748892999998, 0.8888888854682999163, 1.000000000000000000 ),
 .UNSPECIFIED. ) ;
#3347 = ORIENTED_EDGE ( 'NONE', *, *, #56436, .F. ) ;
#3348 = CARTESIAN_POINT ( 'NONE',  ( 10.95238143012640109, 9.081849699400036613, -6.376793985733890224 ) ) ;
#3349 = PLANE ( 'NONE',  #50592 ) ;
#3350 = CARTESIAN_POINT ( 'NONE',  ( 11.09999422944000003, -1.406550927767000081, 10.45582307705999980 ) ) ;
#3351 = EDGE_CURVE ( 'NONE', #51171, #61050, #53944, .T. ) ;
#3352 = CARTESIAN_POINT ( 'NONE',  ( 7.550000000000000711, 4.000000000000000000, 8.849999999999999645 ) ) ;
#3353 = CARTESIAN_POINT ( 'NONE',  ( 12.80505043854146940, -3.207073286498425269, 13.58561123731972131 ) ) ;
#3354 = EDGE_LOOP ( 'NONE', ( #67265, #60278, #29681, #40410 ) ) ;
#3355 = CARTESIAN_POINT ( 'NONE',  ( 10.89874164595999950, -2.834836218627000193, 9.088455567997000273 ) ) ;
#3356 = CARTESIAN_POINT ( 'NONE',  ( 12.19373784164274532, -2.630112413918074932, -13.64494795241839675 ) ) ;
#3357 = CARTESIAN_POINT ( 'NONE',  ( 11.09999999999999964, -5.556657014908000569, -5.124965748850000224 ) ) ;
#3358 = CARTESIAN_POINT ( 'NONE',  ( 10.99548912979983939, 5.205161879957274529, 6.659293853268957619 ) ) ;
#3359 = CARTESIAN_POINT ( 'NONE',  ( 12.43708913301322028, -1.881554942479412018, 13.87303690248389643 ) ) ;
#3360 = ORIENTED_EDGE ( 'NONE', *, *, #61566, .F. ) ;
#3361 = CARTESIAN_POINT ( 'NONE',  ( 17.91802112630374211, 0.5089014841412820012, -13.88746088749277874 ) ) ;
#3362 = CARTESIAN_POINT ( 'NONE',  ( 11.02452225494999993, -2.775477745048999800, -6.571291218949999902 ) ) ;
#3363 = CARTESIAN_POINT ( 'NONE',  ( 23.59999172237900211, -2.915589696762999949, -13.58550518520000061 ) ) ;
#3364 = CYLINDRICAL_SURFACE ( 'NONE', #9751, 2.250000000000000000 ) ;
#3365 = CARTESIAN_POINT ( 'NONE',  ( 12.18528724423033616, -0.08139021474669536071, -13.89968437038779925 ) ) ;
#3366 = CARTESIAN_POINT ( 'NONE',  ( 18.13036722553557567, -2.255582932783688488, 12.50519018731260878 ) ) ;
#3367 = ORIENTED_EDGE ( 'NONE', *, *, #57684, .T. ) ;
#3368 = CARTESIAN_POINT ( 'NONE',  ( 10.60235971519489873, -3.394698737128500010, -6.493038401303000029 ) ) ;
#3369 = EDGE_LOOP ( 'NONE', ( #61943, #44800, #6576, #9043 ) ) ;
#3370 = CARTESIAN_POINT ( 'NONE',  ( 9.625496329943999285, 3.134638325776999856, 8.626949804392001653 ) ) ;
#3371 = AXIS2_PLACEMENT_3D ( 'NONE', #67151, #13004, #45839 ) ;
#3372 = DIRECTION ( 'NONE',  ( 1.000000000000000000, 0.000000000000000000, 0.000000000000000000 ) ) ;
#3373 = CARTESIAN_POINT ( 'NONE',  ( 8.681370280410998674, 2.949305648881000330, -8.659807625323999503 ) ) ;
#3374 = CARTESIAN_POINT ( 'NONE',  ( 3.355011260902999837, -1.961156070315999811, -3.146982238240999763 ) ) ;
#3375 = CARTESIAN_POINT ( 'NONE',  ( 9.973487588364999823, -4.344961837988999598, -9.321582626371998970 ) ) ;
#3376 = CARTESIAN_POINT ( 'NONE',  ( -0.2999999999999999889, 0.5773502691895999739, 1.000000000000000000 ) ) ;
#3377 = CARTESIAN_POINT ( 'NONE',  ( 23.66465205395200044, 13.24762218775999933, 3.909563642290999397 ) ) ;
#3378 = ORIENTED_EDGE ( 'NONE', *, *, #63757, .T. ) ;
#3379 = ADVANCED_FACE ( 'NONE', ( #68995 ), #26706, .T. ) ;
#3380 = CARTESIAN_POINT ( 'NONE',  ( 10.92380110216399913, -4.973546009874400653, 8.094557215852098864 ) ) ;
#3381 = CARTESIAN_POINT ( 'NONE',  ( 9.385781899350000401, 4.980865465981000106, 6.433345686594999613 ) ) ;
#3382 = ADVANCED_FACE ( 'NONE', ( #21782 ), #32300, .T. ) ;
#3383 = CARTESIAN_POINT ( 'NONE',  ( 15.58628609634500073, 9.247881098673000011, 8.227358011109998870 ) ) ;
#3384 = FACE_OUTER_BOUND ( 'NONE', #65595, .T. ) ;
#3386 = CARTESIAN_POINT ( 'NONE',  ( 13.56663763856171734, 9.565814837444753138, 7.877123307579370071 ) ) ;
#3385 = CARTESIAN_POINT ( 'NONE',  ( 10.58844943056000076, 3.754657019866000311, 5.545350295858999523 ) ) ;
#3387 = CARTESIAN_POINT ( 'NONE',  ( 10.32949413291699869, 4.912929163218899831, -7.083453279150199400 ) ) ;
#3388 = CARTESIAN_POINT ( 'NONE',  ( 24.37899130486400168, -12.00803297839000017, 3.275428646162999780 ) ) ;
#3389 = CARTESIAN_POINT ( 'NONE',  ( 10.00962143724499853, 4.667147537636399335, -6.749162825004299648 ) ) ;
#3390 = CARTESIAN_POINT ( 'NONE',  ( 17.91761838490637615, -0.6233258800551685352, 12.58457734799055139 ) ) ;
#3391 = CARTESIAN_POINT ( 'NONE',  ( 24.41555930013399944, 3.181808913646000381, 12.02251225967000003 ) ) ;
#3392 = DIRECTION ( 'NONE',  ( 1.000000000000000000, 0.000000000000000000, 0.000000000000000000 ) ) ;
#3393 = CARTESIAN_POINT ( 'NONE',  ( 25.29989727901499919, -2.078227429405999693, -11.31065739696999906 ) ) ;
#3394 = ORIENTED_EDGE ( 'NONE', *, *, #26841, .F. ) ;
#3395 = CARTESIAN_POINT ( 'NONE',  ( 7.897956853208000005, -3.608524635952000459, 5.913372239166000632 ) ) ;
#3396 = DIRECTION ( 'NONE',  ( -1.000000000000000000, 0.000000000000000000, 0.000000000000000000 ) ) ;
#3397 = EDGE_CURVE ( 'NONE', #47471, #13866, #67900, .T. ) ;
#3398 = CARTESIAN_POINT ( 'NONE',  ( 5.000030787343001215, -2.099962892531005210, -0.2748844998327738542 ) ) ;
#3399 = DIRECTION ( 'NONE',  ( -1.000000000000000000, 0.000000000000000000, 0.000000000000000000 ) ) ;
#3400 = ORIENTED_EDGE ( 'NONE', *, *, #28809, .T. ) ;
#3401 = EDGE_CURVE ( 'NONE', #24359, #44723, #27760, .T. ) ;
#3402 = CARTESIAN_POINT ( 'NONE',  ( 17.77415039705200073, 3.297056071606000227, 11.83473721697999892 ) ) ;
#3403 = AXIS2_PLACEMENT_3D ( 'NONE', #49133, #21867, #43204 ) ;
#3405 = CARTESIAN_POINT ( 'NONE',  ( 11.14767835872009982, 3.125658946326500320, 8.051056647135798272 ) ) ;
#3404 = CARTESIAN_POINT ( 'NONE',  ( 8.775480666858998191, -3.710922827228400056, -8.317400147935998689 ) ) ;
#3406 = CARTESIAN_POINT ( 'NONE',  ( 11.00119221959000093, 4.640446572790000168, -9.059321223816999336 ) ) ;
#3407 = ORIENTED_EDGE ( 'NONE', *, *, #61529, .T. ) ;
#3408 = CARTESIAN_POINT ( 'NONE',  ( 1.405140132540666942, -0.9161175952574773795, -3.408904368339105595 ) ) ;
#3409 = CARTESIAN_POINT ( 'NONE',  ( 17.67416556365687441, -3.238622530711267267, -13.62025504818856270 ) ) ;
#3410 = CARTESIAN_POINT ( 'NONE',  ( 10.74379975933729980, 5.078682052940000524, 7.871126858273000515 ) ) ;
#3411 = LINE ( 'NONE', #67718, #6488 ) ;
#3412 = CARTESIAN_POINT ( 'NONE',  ( 10.90000004630000063, 9.856474695503001371, 5.627825000517000298 ) ) ;
#3413 = VERTEX_POINT ( 'NONE', #38212 ) ;
#3414 = CARTESIAN_POINT ( 'NONE',  ( 11.35641146476999985, -3.755935701663000170, 11.79446980948000068 ) ) ;
#3415 = DIRECTION ( 'NONE',  ( -1.000000000000000000, 0.000000000000000000, 0.000000000000000000 ) ) ;
#3416 = AXIS2_PLACEMENT_3D ( 'NONE', #21781, #49744, #64421 ) ;
#3417 = CARTESIAN_POINT ( 'NONE',  ( 8.227919288421315258, -5.628404604175369030, 8.112053306693633559 ) ) ;
#3418 = CARTESIAN_POINT ( 'NONE',  ( 10.51925056272499859, -2.825232917634000085, -7.517410630436119234 ) ) ;
#3419 = CARTESIAN_POINT ( 'NONE',  ( 10.58655864498000021, -2.992894514506000192, 6.711254117843599154 ) ) ;
#3420 = VERTEX_POINT ( 'NONE', #58850 ) ;
#3421 = CARTESIAN_POINT ( 'NONE',  ( 10.38053123589000037, -4.707947451838999875, -5.013008711266000006 ) ) ;
#3422 = FACE_OUTER_BOUND ( 'NONE', #52917, .T. ) ;
#3423 = ORIENTED_EDGE ( 'NONE', *, *, #38032, .T. ) ;
#3424 = CARTESIAN_POINT ( 'NONE',  ( 9.946013540182333301, -4.999583552997726166, 6.731816600031359066 ) ) ;
#3425 = ORIENTED_EDGE ( 'NONE', *, *, #46204, .T. ) ;
#3426 = FACE_OUTER_BOUND ( 'NONE', #12221, .T. ) ;
#3427 = FACE_OUTER_BOUND ( 'NONE', #47908, .T. ) ;
#3428 = CARTESIAN_POINT ( 'NONE',  ( 11.84388784977539899, 2.744254309011999737, -7.428242901739219306 ) ) ;
#3429 = CARTESIAN_POINT ( 'NONE',  ( 8.228673390747101024, 4.831902665061588387, 6.190044796983404041 ) ) ;
#3430 = CARTESIAN_POINT ( 'NONE',  ( 12.21993702172673757, 2.719929609653445546, -12.39763114037443970 ) ) ;
#3431 = CARTESIAN_POINT ( 'NONE',  ( 11.66225954179439839, -3.122605388210700106, 6.770980925167799036 ) ) ;
#3432 = CARTESIAN_POINT ( 'NONE',  ( 8.464260841230998977, 2.029098103856999735, 7.726995416028000108 ) ) ;
#3433 = ORIENTED_EDGE ( 'NONE', *, *, #13109, .T. ) ;
#3434 = CARTESIAN_POINT ( 'NONE',  ( 7.500005746562851350, 5.303016073863008550, 7.913359363012708592 ) ) ;
#3435 = CARTESIAN_POINT ( 'NONE',  ( 8.855418146794999501, -5.633481712366999794, 7.451234046297000368 ) ) ;
#3436 = CARTESIAN_POINT ( 'NONE',  ( 10.07309687351575178, 5.217465845835396188, 7.172815144550900968 ) ) ;
#3437 = ORIENTED_EDGE ( 'NONE', *, *, #43227, .T. ) ;
#3438 = CARTESIAN_POINT ( 'NONE',  ( 12.12868457208163520, -2.220738826795313869, -12.40275942113248142 ) ) ;
#3439 = CARTESIAN_POINT ( 'NONE',  ( 11.18272066707849888, 5.093522884867000222, 8.161456030935699602 ) ) ;
#3440 = CARTESIAN_POINT ( 'NONE',  ( 10.56170564679000101, -5.057490041178001050, -8.595713413570999606 ) ) ;
#3441 = CARTESIAN_POINT ( 'NONE',  ( 8.475341021510246264, -5.350570349241358770, 7.499981640446112152 ) ) ;
#3442 = CARTESIAN_POINT ( 'NONE',  ( 18.53936233968600078, -2.923364741758000207, -12.21823820824000073 ) ) ;
#3443 = CARTESIAN_POINT ( 'NONE',  ( 24.26733150070300127, -8.951944080097000267, 8.897842723392001218 ) ) ;
#3444 = CARTESIAN_POINT ( 'NONE',  ( 12.42225061842106903, -2.005837741177418199, -13.76588300560132438 ) ) ;
#3445 = CARTESIAN_POINT ( 'NONE',  ( 9.356851002546999752, 2.832432432432000269, -6.822293592207000934 ) ) ;
#3446 = CARTESIAN_POINT ( 'NONE',  ( 10.34580110216399973, -5.090698144635000588, -6.833896451085399448 ) ) ;
#3447 = AXIS2_PLACEMENT_3D ( 'NONE', #3901, #56025, #56722 ) ;
#3448 = CARTESIAN_POINT ( 'NONE',  ( 8.614144221484336228, -4.937690759611556679, 6.045737820659460304 ) ) ;
#3449 = ORIENTED_EDGE ( 'NONE', *, *, #51146, .T. ) ;
#3450 = ORIENTED_EDGE ( 'NONE', *, *, #39707, .T. ) ;
#3451 = CARTESIAN_POINT ( 'NONE',  ( 10.27669459503999860, -4.581840238100999940, 5.003918118598999598 ) ) ;
#3452 = PRESENTATION_STYLE_ASSIGNMENT (( #51695 ) ) ;
#3453 = CARTESIAN_POINT ( 'NONE',  ( 15.20000000000000107, -11.99088163391999906, 3.229229350024999778 ) ) ;
#3454 = DIRECTION ( 'NONE',  ( 1.000000000000000000, 0.000000000000000000, 0.000000000000000000 ) ) ;
#3455 = CARTESIAN_POINT ( 'NONE',  ( 10.69578011722000177, 5.505003832924999507, -7.759263776825999770 ) ) ;
#3456 = AXIS2_PLACEMENT_3D ( 'NONE', #4224, #16435, #15067 ) ;
#3457 = PLANE ( 'NONE',  #41636 ) ;
#3458 = CARTESIAN_POINT ( 'NONE',  ( 17.84326074309960575, 3.054675730970588532, 12.30486402137391977 ) ) ;
#3459 = CARTESIAN_POINT ( 'NONE',  ( 25.59997821859199973, 2.856411258734000036, -11.13959759756999901 ) ) ;
#3460 = CARTESIAN_POINT ( 'NONE',  ( 10.84168637167000071, 2.681011538858999899, 6.554754637093000547 ) ) ;
#3461 = AXIS2_PLACEMENT_3D ( 'NONE', #63406, #62717, #36854 ) ;
#3462 = CARTESIAN_POINT ( 'NONE',  ( 11.33810207955129812, 4.796537143354000499, 7.174999999999999822 ) ) ;
#3463 = EDGE_CURVE ( 'NONE', #7451, #11759, #19904, .T. ) ;
#3464 = EDGE_LOOP ( 'NONE', ( #48545, #53593, #31926, #6711 ) ) ;
#3465 = CARTESIAN_POINT ( 'NONE',  ( 12.57303446153997406, -1.919568987556539152, 12.56805043247348941 ) ) ;
#3466 = EDGE_CURVE ( 'NONE', #56100, #38413, #51889, .T. ) ;
#3467 = B_SPLINE_CURVE_WITH_KNOTS ( 'NONE', 3,
 ( #7363, #50023, #51052, #8406, #29056, #66434 ),
 .UNSPECIFIED., .F., .F.,
 ( 4, 2, 4 ),
 ( 0.000000000000000000, 0.5000000000000000000, 1.000000000000000000 ),
 .UNSPECIFIED. ) ;
#3468 = CARTESIAN_POINT ( 'NONE',  ( 23.63877154019659343, -10.04588656656894408, -9.676553435357190480 ) ) ;
#3469 = CARTESIAN_POINT ( 'NONE',  ( 10.64872393945999995, 2.614781729644000130, 6.717281948314999696 ) ) ;
#3470 = CARTESIAN_POINT ( 'NONE',  ( 10.94999293566599974, -3.279967330949900450, 6.616719557880299085 ) ) ;
#3471 = CARTESIAN_POINT ( 'NONE',  ( 8.441604719589999917, 5.473983809665999622, -8.180077404516000072 ) ) ;
#3472 = CARTESIAN_POINT ( 'NONE',  ( 10.76426088462129904, 4.002719309691810778, -6.221990224628999755 ) ) ;
#3473 = CARTESIAN_POINT ( 'NONE',  ( 12.19601995205470502, -0.1418569258565868241, 12.69895512164409368 ) ) ;
#3474 = CLOSED_SHELL ( 'NONE', ( #28195, #17438, #68773, #19112, #26004, #23320, #22416, #45394, #47214, #46509, #33819, #65301, #62948, #8663, #61282, #19216, #21792, #7686, #34104, #11873, #31846, #60807, #30869, #19196, #40315, #7528, #66177, #45704, #37950, #7274, #37336, #51691, #68046, #42924, #46259, #37998, #4392, #62477, #41735, #1286, #10192, #3075, #8153, #26939, #60158, #32528, #16986, #51991, #5002, #31962, #62475, #32851, #4389, #705, #29629, #2696, #5033, #19055, #47007, #9517, #44482, #37639, #5438, #49841, #34185, #14878, #37872, #1964, #42276, #4958, #41741, #6971, #47662, #1449, #56238, #64684, #68248, #25729, #39874, #20513, #22999, #66381, #12726, #35288, #36862, #48965, #22577, #67823, #61981, #58308, #36891, #10721, #13970, #32198, #22521, #56187, #66404, #61200, #56518, #61839, #16108, #13933, #66134, #48631, #30784, #1567, #17259, #48352, #302, #31888, #8607, #62503, #56292, #61239, #20149, #51905, #50451, #14528, #51147, #43049, #15659, #31407, #32284, #18974, #65905, #19736, #16479, #44457, #29627, #48218, #29286, #46735, #62228, #32526, #12533, #50756, #1570, #60692, #38053, #1336, #35669, #13339, #11957, #39272, #30332, #59835, #4556, #35587, #17858, #34417, #33337, #46180, #16356, #51270, #61749, #58614, #10519, #7575, #22722, #21936, #10866, #296, #28976, #38746, #69003, #67771, #18932, #16390, #62369, #65956, #6713, #50272, #19277, #66566, #12394, #61108, #16525, #50130, #52221, #55966 ) ) ;
#3475 = CARTESIAN_POINT ( 'NONE',  ( 8.636454719592999041, 3.869396554003000421, 5.695652484872999466 ) ) ;
#3476 = CARTESIAN_POINT ( 'NONE',  ( 11.05639637898999972, 5.030226177531999632, 6.028288223959999748 ) ) ;
#3477 = CARTESIAN_POINT ( 'NONE',  ( 12.73227166903752128, 1.879164230820285608, 12.57473389636349026 ) ) ;
#3478 = VERTEX_POINT ( 'NONE', #58504 ) ;
#3479 = CARTESIAN_POINT ( 'NONE',  ( 9.915635841230999503, 3.210851187372000037, -6.346613542714999667 ) ) ;
#3480 = CARTESIAN_POINT ( 'NONE',  ( 7.227197234740000198, 1.247817563501999905, -0.8087676081403000206 ) ) ;
#3481 = CARTESIAN_POINT ( 'NONE',  ( 10.64079374716282800, -5.301110017552429277, 6.316741276523229587 ) ) ;
#3483 = CARTESIAN_POINT ( 'NONE',  ( 9.593930206849998754, -2.750000000000000000, -7.500000000000000000 ) ) ;
#3482 = CARTESIAN_POINT ( 'NONE',  ( 7.464688980125999684, -4.351670788182000038, 8.977200644264000218 ) ) ;
#3484 = CARTESIAN_POINT ( 'NONE',  ( 12.09999999999999964, -4.672781865721786332, 8.148846660984084167 ) ) ;
#3485 = CARTESIAN_POINT ( 'NONE',  ( 10.99410672858429905, -4.801902424331299990, -6.896755974168000236 ) ) ;
#3486 = ORIENTED_EDGE ( 'NONE', *, *, #16665, .T. ) ;
#3487 = CARTESIAN_POINT ( 'NONE',  ( 1.820428564792999859, -3.146289470026999879, -2.056511572473000093 ) ) ;
#3488 = EDGE_CURVE ( 'NONE', #23313, #22584, #53266, .T. ) ;
#3489 = CARTESIAN_POINT ( 'NONE',  ( 18.01651533331883570, -0.4224082581076209486, -12.69056396411460774 ) ) ;
#3491 = CARTESIAN_POINT ( 'NONE',  ( 13.78326532032400031, -9.295717737520000412, -8.172239456948000580 ) ) ;
#3490 = CARTESIAN_POINT ( 'NONE',  ( 8.324914158772999784, 2.633142096252999664, -7.791134854666999843 ) ) ;
#3492 = CARTESIAN_POINT ( 'NONE',  ( 17.92097848891127398, -3.007049802558098062, 13.55275178750181020 ) ) ;
#3493 = CARTESIAN_POINT ( 'NONE',  ( 25.50731327284336558, -8.309743679583657894, 8.116427603517399447 ) ) ;
#3494 = CARTESIAN_POINT ( 'NONE',  ( 11.49978667957999967, -12.43119799159999950, -1.530013559959999991 ) ) ;
#3495 = DIRECTION ( 'NONE',  ( 0.000000000000000000, -0.9693731749023103417, 0.2455924424322025734 ) ) ;
#3496 = DIRECTION ( 'NONE',  ( 1.000000000000000000, 0.000000000000000000, 0.000000000000000000 ) ) ;
#3497 = CARTESIAN_POINT ( 'NONE',  ( 8.592629440379999650, -3.856773448568000084, 5.521258396339000285 ) ) ;
#3498 = EDGE_LOOP ( 'NONE', ( #1257, #5484, #49726, #46063, #29954 ) ) ;
#3499 = CARTESIAN_POINT ( 'NONE',  ( 9.433107780409999421, 4.954905351382000944, 8.825777580285999235 ) ) ;
#3500 = CARTESIAN_POINT ( 'NONE',  ( 13.50018479229300006, -11.60142623882999935, -2.415183939829000259 ) ) ;
#3501 = CARTESIAN_POINT ( 'NONE',  ( 7.441574459899483962, -2.267067028809165219, 7.663462709907783221 ) ) ;
#3502 = DIRECTION ( 'NONE',  ( 0.4384236320213994453, 0.6355252626312996034, 0.6355252626312994924 ) ) ;
#3503 = CARTESIAN_POINT ( 'NONE',  ( 1.314110206211000165, 0.8376700968564000371, 3.321615185007000370 ) ) ;
#3504 = ORIENTED_EDGE ( 'NONE', *, *, #66051, .F. ) ;
#3505 = CARTESIAN_POINT ( 'NONE',  ( 1.620140597451261044, -1.263880145926562948, -3.051407509797793516 ) ) ;
#3506 = CARTESIAN_POINT ( 'NONE',  ( 10.88287885159599888, -3.139900861731399928, 7.602606670248799325 ) ) ;
#3507 = DIRECTION ( 'NONE',  ( -0.8660254037844288266, 0.000000000000000000, 0.5000000000000169864 ) ) ;
#3508 = CARTESIAN_POINT ( 'NONE',  ( 10.92717848204000042, 5.023653513500000223, 8.718036113327999104 ) ) ;
#3509 = CARTESIAN_POINT ( 'NONE',  ( 11.58487348028854846, 3.117292544139400157, 7.022738645480499642 ) ) ;
#3510 = VECTOR ( 'NONE', #19141, 1000.000000000000000 ) ;
#3511 = CARTESIAN_POINT ( 'NONE',  ( 23.84019000122944831, -3.320739317830645021, 13.05082518065574426 ) ) ;
#3512 = CARTESIAN_POINT ( 'NONE',  ( 18.05145975767274891, 0.3802875570022087870, -13.89301034115781874 ) ) ;
#3513 = CARTESIAN_POINT ( 'NONE',  ( 8.576923877145999242, -3.399999999999999911, 5.924121105096999962 ) ) ;
#3514 = LINE ( 'NONE', #20635, #47695 ) ;
#3515 = CARTESIAN_POINT ( 'NONE',  ( 8.237473783029317431, 5.556797505346596999, 8.286080926133671198 ) ) ;
#3516 = ORIENTED_EDGE ( 'NONE', *, *, #30043, .T. ) ;
#3517 = CARTESIAN_POINT ( 'NONE',  ( 17.88894803995539817, -3.166162608671032608, 13.63728156593011498 ) ) ;
#3518 = PLANE ( 'NONE',  #29431 ) ;
#3519 = ORIENTED_EDGE ( 'NONE', *, *, #38934, .F. ) ;
#3520 = DIRECTION ( 'NONE',  ( 0.000000000000000000, 0.000000000000000000, -1.000000000000000000 ) ) ;
#3521 = CARTESIAN_POINT ( 'NONE',  ( 24.57710018668033669, -3.191964740936587663, -11.91258045713028224 ) ) ;
#3522 = CARTESIAN_POINT ( 'NONE',  ( 9.833513540183332680, 2.750000000000000000, -7.336375382625529795 ) ) ;
#3523 = FACE_OUTER_BOUND ( 'NONE', #68930, .T. ) ;
#3524 = CIRCLE ( 'NONE', #30339, 11.55000237494000537 ) ;
#3525 = EDGE_CURVE ( 'NONE', #60760, #68619, #6817, .T. ) ;
#3526 = CARTESIAN_POINT ( 'NONE',  ( 10.15902941591999920, 4.166415211384999040, 9.114163806478000396 ) ) ;
#3527 = EDGE_CURVE ( 'NONE', #51133, #46559, #29127, .T. ) ;
#3528 = CARTESIAN_POINT ( 'NONE',  ( 10.40878363256000050, 3.093886843363999883, -6.480781753756000185 ) ) ;
#3529 = CARTESIAN_POINT ( 'NONE',  ( 9.530849898046625412, -4.391573077584247642, -6.717566108970133953 ) ) ;
#3530 = CARTESIAN_POINT ( 'NONE',  ( 10.12670810574000058, -3.117521507207000386, 8.613544937223998943 ) ) ;
#3531 = CARTESIAN_POINT ( 'NONE',  ( 18.03319509584025937, 0.5408165383911073265, -12.58839068838662278 ) ) ;
#3532 = CARTESIAN_POINT ( 'NONE',  ( 25.50737144172638438, 11.18383546498688297, 3.138211644118512833 ) ) ;
#3533 = CARTESIAN_POINT ( 'NONE',  ( 10.92441504065829960, -3.305585767322499979, -6.982228367137699898 ) ) ;
#3534 = CARTESIAN_POINT ( 'NONE',  ( 7.726448341228000061, 2.630487280353000390, 6.995957894972000268 ) ) ;
#3535 = ORIENTED_EDGE ( 'NONE', *, *, #485, .F. ) ;
#3536 = CARTESIAN_POINT ( 'NONE',  ( 10.96504121510999852, -6.670435863508999752, -5.365570440722000178 ) ) ;
#3537 =( NAMED_UNIT ( * ) PLANE_ANGLE_UNIT ( ) SI_UNIT ( $, .RADIAN. ) );
#3538 = CARTESIAN_POINT ( 'NONE',  ( 11.27769289846838241, -5.045673698156681652, -7.824982657629016458 ) ) ;
#3539 = CARTESIAN_POINT ( 'NONE',  ( 17.60324462842604376, 1.762109595560071851, 12.47617631420775197 ) ) ;
#3540 = CARTESIAN_POINT ( 'NONE',  ( 9.684367640780997988, 4.603017491986999943, -6.371835875489000323 ) ) ;
#3541 = CARTESIAN_POINT ( 'NONE',  ( 12.10383213726155560, 2.332238815612523553, 13.80437617213671331 ) ) ;
#3542 = CARTESIAN_POINT ( 'NONE',  ( 11.09999999999999964, -4.000000000000000000, 7.500000000000000000 ) ) ;
#3543 = ORIENTED_EDGE ( 'NONE', *, *, #65361, .F. ) ;
#3544 = CARTESIAN_POINT ( 'NONE',  ( 12.29147016624624733, 0.3563519072876710769, -12.69327554148065573 ) ) ;
#3545 = CARTESIAN_POINT ( 'NONE',  ( 25.44994642811700203, 0.000000000000000000, 2.140509991476999645E-13 ) ) ;
#3546 = EDGE_CURVE ( 'NONE', #37562, #19987, #34446, .T. ) ;
#3547 = ORIENTED_EDGE ( 'NONE', *, *, #57600, .T. ) ;
#3548 = DIRECTION ( 'NONE',  ( -1.000000000000000000, 0.000000000000000000, 0.000000000000000000 ) ) ;
#3549 = ADVANCED_FACE ( 'NONE', ( #45201 ), #8157, .T. ) ;
#3550 = DIRECTION ( 'NONE',  ( 1.000000000000000000, 0.000000000000000000, 0.000000000000000000 ) ) ;
#3551 = CARTESIAN_POINT ( 'NONE',  ( 10.98768472625999948, -5.449702614167000192, -4.945212061590999575 ) ) ;
#3552 = CARTESIAN_POINT ( 'NONE',  ( 11.05518582084300050, -4.566724035220099509, 8.155074391384399490 ) ) ;
#3553 = AXIS2_PLACEMENT_3D ( 'NONE', #52541, #30884, #4638 ) ;
#3554 = EDGE_CURVE ( 'NONE', #16603, #54112, #7094, .T. ) ;
#3555 = CARTESIAN_POINT ( 'NONE',  ( 10.09393020685000053, -2.750000000000000000, 7.500000000000000000 ) ) ;
#3556 = CARTESIAN_POINT ( 'NONE',  ( 0.3017198524092000178, -3.532786812989999969, -1.105428934477000080 ) ) ;
#3557 = CARTESIAN_POINT ( 'NONE',  ( 11.11486084871780022, 5.207010770456999893, 7.825000000000000178 ) ) ;
#3558 = CARTESIAN_POINT ( 'NONE',  ( 12.68571266918094764, 3.190282694684578590, 12.18942654693561600 ) ) ;
#3559 = CARTESIAN_POINT ( 'NONE',  ( 8.571413182547999554, 4.599999999999999645, 5.927302706106000407 ) ) ;
#3560 = CARTESIAN_POINT ( 'NONE',  ( 11.56025819896753859, 3.013900664291200293, -7.685900384398899554 ) ) ;
#3561 = DIRECTION ( 'NONE',  ( 0.000000000000000000, 0.7577476854548028662, -0.6525476574074028369 ) ) ;
#3562 = CARTESIAN_POINT ( 'NONE',  ( 10.28014141025500017, 4.417352327511700594, -8.243346240911998635 ) ) ;
#3563 = CARTESIAN_POINT ( 'NONE',  ( 9.784621437244998887, 4.758411336345700349, -6.646450532840099790 ) ) ;
#3565 = CARTESIAN_POINT ( 'NONE',  ( 12.18582115250623055, 2.585797660597818570, 12.43116941330281300 ) ) ;
#3564 = CARTESIAN_POINT ( 'NONE',  ( 16.04382898362900178, -8.457859886528000359, -8.090718092504999959 ) ) ;
#3566 = CARTESIAN_POINT ( 'NONE',  ( 10.97807333593999957, -5.235090452703000885, -6.783100406990000053 ) ) ;
#3567 = EDGE_LOOP ( 'NONE', ( #50420, #59717, #47929, #9347, #26491 ) ) ;
#3568 = ADVANCED_FACE ( 'NONE', ( #22476, #1505 ), #50433, .F. ) ;
#3569 = DIRECTION ( 'NONE',  ( -1.000000000000000000, 0.000000000000000000, 0.000000000000000000 ) ) ;
#3570 = VECTOR ( 'NONE', #55413, 1000.000000000000000 ) ;
#3571 = CARTESIAN_POINT ( 'NONE',  ( 9.481330364773148389, 3.644056349852950127, -9.240156464735864716 ) ) ;
#3572 = CARTESIAN_POINT ( 'NONE',  ( 9.150442991499998513, 3.928121959910110483, 8.639547276484998761 ) ) ;
#3573 = DIRECTION ( 'NONE',  ( 0.000000000000000000, 1.000000000000000000, 0.000000000000000000 ) ) ;
#3574 = CARTESIAN_POINT ( 'NONE',  ( 24.35365242081699932, 10.79182034089001796, -4.028979492054000744 ) ) ;
#3575 = FACE_OUTER_BOUND ( 'NONE', #55151, .T. ) ;
#3576 = CARTESIAN_POINT ( 'NONE',  ( 7.077542425583873253, -1.465994342824544899E-06, -1.322443989608400816 ) ) ;
#3577 = VERTEX_POINT ( 'NONE', #50096 ) ;
#3578 = CARTESIAN_POINT ( 'NONE',  ( 9.202051052051999136, -2.879444846832000415, -7.719295683256799379 ) ) ;
#3579 = DIRECTION ( 'NONE',  ( 0.7071067811865712205, 0.1740570408699930738, -0.6853496527492721757 ) ) ;
#3580 = CARTESIAN_POINT ( 'NONE',  ( 11.77234208742519961, -4.554746427620499638, 6.627995351445298944 ) ) ;
#3581 = CARTESIAN_POINT ( 'NONE',  ( 18.23147373744589927, 2.220711592698080494, -12.40276429823313897 ) ) ;
#3582 = CARTESIAN_POINT ( 'NONE',  ( 8.887782330080007398, -3.105205165878999196, -6.157731156825001051 ) ) ;
#3583 = DIRECTION ( 'NONE',  ( -1.000000000000000000, 0.000000000000000000, 0.000000000000000000 ) ) ;
#3584 = CARTESIAN_POINT ( 'NONE',  ( 8.186785374738994037, 2.888678623336002005, 6.695956381329003726 ) ) ;
#3585 = CARTESIAN_POINT ( 'NONE',  ( 9.353311703536000721, -4.905858243509999106, -8.948175900338000588 ) ) ;
#3586 = FACE_OUTER_BOUND ( 'NONE', #23902, .T. ) ;
#3587 = DIRECTION ( 'NONE',  ( 1.000000000000000000, 0.000000000000000000, 0.000000000000000000 ) ) ;
#3588 = PLANE ( 'NONE',  #56553 ) ;
#3589 = CARTESIAN_POINT ( 'NONE',  ( 10.26195629121000152, -4.600000265269999389, 4.591198190832999515 ) ) ;
#3590 = FACE_OUTER_BOUND ( 'NONE', #60039, .T. ) ;
#3591 = CARTESIAN_POINT ( 'NONE',  ( 2.821806799211333594, -3.408904368339104263, -0.9161175952574813763 ) ) ;
#3592 = CARTESIAN_POINT ( 'NONE',  ( 9.717214158771000143, 3.990126737362999609, -8.809457313313998839 ) ) ;
#3593 = CARTESIAN_POINT ( 'NONE',  ( 12.08902763632552002, -4.786505910413500153, 7.862914650060299770 ) ) ;
#3594 = ORIENTED_EDGE ( 'NONE', *, *, #41270, .F. ) ;
#3595 = CIRCLE ( 'NONE', #19280, 0.9999999999999993339 ) ;
#3596 = B_SPLINE_CURVE_WITH_KNOTS ( 'NONE', 3,
 ( #68718, #31678, #16274, #893 ),
 .UNSPECIFIED., .F., .F.,
 ( 4, 4 ),
 ( 0.000000000000000000, 1.000000000000000000 ),
 .UNSPECIFIED. ) ;
#3597 = CARTESIAN_POINT ( 'NONE',  ( 9.156713723001384864, -5.179807657556271927, -8.179981299039964071 ) ) ;
#3598 = CARTESIAN_POINT ( 'NONE',  ( 18.15341532599038032, 2.105586285009647174, -13.84075898842493935 ) ) ;
#3599 = ORIENTED_EDGE ( 'NONE', *, *, #11468, .T. ) ;
#3600 = CARTESIAN_POINT ( 'NONE',  ( 10.36463399569800004, -3.138280386550500012, 7.404358731173799946 ) ) ;
#3601 = FACE_OUTER_BOUND ( 'NONE', #56676, .T. ) ;
#3602 = DIRECTION ( 'NONE',  ( 0.000000000000000000, 1.000000000000000000, 0.000000000000000000 ) ) ;
#3603 = ADVANCED_FACE ( 'NONE', ( #2536 ), #18284, .F. ) ;
#3604 = CARTESIAN_POINT ( 'NONE',  ( 9.733247726267846289, 4.120954015165996687, -8.873126350618022684 ) ) ;
#3605 = EDGE_CURVE ( 'NONE', #46374, #38378, #22664, .T. ) ;
#3606 = CARTESIAN_POINT ( 'NONE',  ( 11.31389666366019853, -4.045876550911099656, -8.532487796751999198 ) ) ;
#3607 = CARTESIAN_POINT ( 'NONE',  ( 11.59999999999999787, -3.165084187357963597, -6.701316188976606192 ) ) ;
#3608 = EDGE_CURVE ( 'NONE', #46752, #65197, #2205, .T. ) ;
#3609 = CARTESIAN_POINT ( 'NONE',  ( 8.905196823546312146, -3.391797362091467427, -8.372486832488423403 ) ) ;
#3610 = ORIENTED_EDGE ( 'NONE', *, *, #5918, .F. ) ;
#3611 = CARTESIAN_POINT ( 'NONE',  ( 21.60000012424471194, 13.89999856298999958, 0.000000000000000000 ) ) ;
#3612 = CARTESIAN_POINT ( 'NONE',  ( 7.744301850232000461, 3.130385018321999890, 6.467396599055999395 ) ) ;
#3613 = CARTESIAN_POINT ( 'NONE',  ( 10.02394528041000044, 5.481267232667000222, -8.005061172455999241 ) ) ;
#3614 = ORIENTED_EDGE ( 'NONE', *, *, #58389, .F. ) ;
#3615 = VECTOR ( 'NONE', #842, 1000.000000000000000 ) ;
#3616 = CARTESIAN_POINT ( 'NONE',  ( 10.58996475420000039, 2.876740601533999797, -6.236530348556999392 ) ) ;
#3617 = ORIENTED_EDGE ( 'NONE', *, *, #3525, .T. ) ;
#3618 = CARTESIAN_POINT ( 'NONE',  ( 8.577265421554999492, 3.785712956512099936, 6.391527115138999626 ) ) ;
#3619 = CARTESIAN_POINT ( 'NONE',  ( 17.84610786052058984, -3.139226446220204636, -12.20267444563224224 ) ) ;
#3620 = CARTESIAN_POINT ( 'NONE',  ( 17.79999999998900151, -3.595165934733000057, 11.99793354950999991 ) ) ;
#3621 = B_SPLINE_CURVE_WITH_KNOTS ( 'NONE', 3,
 ( #19156, #55540, #18480, #39804 ),
 .UNSPECIFIED., .F., .F.,
 ( 4, 4 ),
 ( 0.000000000000000000, 1.000000000000000000 ),
 .UNSPECIFIED. ) ;
#3622 = DIRECTION ( 'NONE',  ( 0.000000000000000000, 0.8648648648648720183, 0.5020047465136825426 ) ) ;
#3623 = CARTESIAN_POINT ( 'NONE',  ( 13.50007192468514106, -9.074936576711701619, -7.617865797329282707 ) ) ;
#3624 = EDGE_LOOP ( 'NONE', ( #5415, #61793, #18763, #56843 ) ) ;
#3625 = CARTESIAN_POINT ( 'NONE',  ( 11.09999999999999964, 2.649999999999999911, 7.500000000000000000 ) ) ;
#3626 = CARTESIAN_POINT ( 'NONE',  ( 11.18237334122999904, 4.516636732814999888, -8.757876389238999693 ) ) ;
#3627 = DIRECTION ( 'NONE',  ( -0.000000000000000000, -0.000000000000000000, 1.000000000000000000 ) ) ;
#3628 = CARTESIAN_POINT ( 'NONE',  ( 12.18865279333483720, 2.902449960337685653, -13.69583488376822800 ) ) ;
#3629 = EDGE_CURVE ( 'NONE', #15208, #67674, #35195, .T. ) ;
#3630 = CARTESIAN_POINT ( 'NONE',  ( 18.27886422513980591, 0.04806343339259133707, 13.99993753789458850 ) ) ;
#3631 = DIRECTION ( 'NONE',  ( 1.000000000000000000, -2.025400574418000070E-14, -2.893429392025000534E-14 ) ) ;
#3632 = CARTESIAN_POINT ( 'NONE',  ( 10.64447714202000128, -5.073836261934999925, -8.340686666652999293 ) ) ;
#3633 = EDGE_LOOP ( 'NONE', ( #18086, #32343, #38437, #61367, #66252, #67432, #51642, #5520, #4334, #36983, #15639, #15704, #18460, #55837, #60774 ) ) ;
#3634 = ORIENTED_EDGE ( 'NONE', *, *, #890, .T. ) ;
#3635 = CARTESIAN_POINT ( 'NONE',  ( 9.576420280414000175, 4.861259245430999520, -8.806664389576001284 ) ) ;
#3636 = CARTESIAN_POINT ( 'NONE',  ( 6.899999691988000450, 12.43893545635000031, 2.828937028792000152 ) ) ;
#3637 = CARTESIAN_POINT ( 'NONE',  ( 7.434063311431996723, -5.180700782550064609, 6.820069141833377202 ) ) ;
#3638 = CARTESIAN_POINT ( 'NONE',  ( 24.11240984803955456, 3.334517130192976353, 12.54136258879263544 ) ) ;
#3639 = CARTESIAN_POINT ( 'NONE',  ( 23.85292159917500143, 9.641972580453998631, -9.631818861864001491 ) ) ;
#3640 = CARTESIAN_POINT ( 'NONE',  ( 18.16715644869600155, -3.024463723863999753, -11.49930835314999911 ) ) ;
#3642 = CARTESIAN_POINT ( 'NONE',  ( 8.886504504762845258, 2.780594424960459499, 8.755326434349345988 ) ) ;
#3641 = CARTESIAN_POINT ( 'NONE',  ( 10.03038019923399915, -2.867101906753999785, 7.642395078236999595 ) ) ;
#3643 = CARTESIAN_POINT ( 'NONE',  ( 8.344928245395999866, -4.790498497136999489, -6.523246444533000954 ) ) ;
#3644 = ORIENTED_EDGE ( 'NONE', *, *, #64240, .T. ) ;
#3645 = AXIS2_PLACEMENT_3D ( 'NONE', #3145, #44779, #24476 ) ;
#3646 = CARTESIAN_POINT ( 'NONE',  ( 10.64393020684969926, 5.250000000000000000, 7.500000000000000000 ) ) ;
#3647 = EDGE_CURVE ( 'NONE', #3577, #11746, #24416, .T. ) ;
#3648 = CARTESIAN_POINT ( 'NONE',  ( 10.61390167354000091, -2.793204138329999697, -4.716480657362000173 ) ) ;
#3649 = CARTESIAN_POINT ( 'NONE',  ( 10.01832872737000102, -5.491975933468000726, -7.893788029530999673 ) ) ;
#3650 = LINE ( 'NONE', #24987, #6790 ) ;
#3651 = CARTESIAN_POINT ( 'NONE',  ( 9.884778143176074394, -2.675332436538061742, -7.165830604257146241 ) ) ;
#3652 = DIRECTION ( 'NONE',  ( -1.000000000000000000, 0.000000000000000000, 1.554312234491000161E-14 ) ) ;
#3653 = CARTESIAN_POINT ( 'NONE',  ( 6.999999691988000095, -12.36734761319999798, 2.759114534468000368 ) ) ;
#3654 = CARTESIAN_POINT ( 'NONE',  ( 7.966947972481352558, 2.969119817116051330, -6.520715660824929927 ) ) ;
#3655 = AXIS2_PLACEMENT_3D ( 'NONE', #56151, #12128, #54772 ) ;
#3656 = CARTESIAN_POINT ( 'NONE',  ( 6.210802160082999457, 0.002327316029692000007, 1.176084684120999979 ) ) ;
#3657 = DIRECTION ( 'NONE',  ( 0.000000000000000000, -1.000000000000000000, 0.000000000000000000 ) ) ;
#3658 = CARTESIAN_POINT ( 'NONE',  ( 3.067338808729000110, -0.7022537682570999529, -3.352858224555000266 ) ) ;
#3659 = VERTEX_POINT ( 'NONE', #8132 ) ;
#3660 = CARTESIAN_POINT ( 'NONE',  ( 12.76392908090536338, -0.6239794389693680277, -12.67935706666153450 ) ) ;
#3661 = CARTESIAN_POINT ( 'NONE',  ( 12.20324964192238326, -2.330992520672867219, -12.48933099340478492 ) ) ;
#3662 = CARTESIAN_POINT ( 'NONE',  ( 16.09997386696500143, 8.350085070477001992, 8.123950967096998710 ) ) ;
#3663 = CARTESIAN_POINT ( 'NONE',  ( 8.449239158774000558, 5.458692773671000253, 7.456452194274000078 ) ) ;
#3664 = PRESENTATION_STYLE_ASSIGNMENT (( #2649 ) ) ;
#3665 = ORIENTED_EDGE ( 'NONE', *, *, #53282, .T. ) ;
#3666 = LINE ( 'NONE', #63773, #40012 ) ;
#3667 = CARTESIAN_POINT ( 'NONE',  ( 0.000000000000000000, 0.000000000000000000, 0.000000000000000000 ) ) ;
#3668 = CARTESIAN_POINT ( 'NONE',  ( 10.99014425376339688, 7.742518842553854697, 6.423560035353997222 ) ) ;
#3669 = CARTESIAN_POINT ( 'NONE',  ( 13.25609597789999938, -11.48890257311000163, -1.688129671228999928 ) ) ;
#3670 = CARTESIAN_POINT ( 'NONE',  ( 7.795984407058476506, 2.673910249782932347, -7.823565946277482475 ) ) ;
#3671 = CARTESIAN_POINT ( 'NONE',  ( 11.26723293495529887, 2.826061044294000180, -7.452807962566580180 ) ) ;
#3672 = EDGE_LOOP ( 'NONE', ( #15756, #21183, #46185, #55962 ) ) ;
#3673 = CARTESIAN_POINT ( 'NONE',  ( 10.64872180584000105, -2.614778238704999591, 6.717279975758000177 ) ) ;
#3674 = ORIENTED_EDGE ( 'NONE', *, *, #7441, .T. ) ;
#3675 = CARTESIAN_POINT ( 'NONE',  ( -15.86200481174999943, -2.399999999999999911, 6.571291218949999902 ) ) ;
#3676 = CARTESIAN_POINT ( 'NONE',  ( 15.95266668291200141, 3.685671355860000276, 11.20570641515999988 ) ) ;
#3677 = CARTESIAN_POINT ( 'NONE',  ( 18.27538073532130980, -0.08359636179364166031, -13.99975542440154541 ) ) ;
#3678 = ADVANCED_FACE ( 'NONE', ( #18967 ), #62629, .F. ) ;
#3679 = ORIENTED_EDGE ( 'NONE', *, *, #46178, .T. ) ;
#3680 = CARTESIAN_POINT ( 'NONE',  ( 23.58602290021012493, 10.21078611479860854, 9.552280232028873996 ) ) ;
#3681 = ADVANCED_FACE ( 'NONE', ( #9152 ), #55156, .F. ) ;
#3682 = CARTESIAN_POINT ( 'NONE',  ( 5.200000000000000178, -1.376649746192999846, 11.21582968292000082 ) ) ;
#3683 = CARTESIAN_POINT ( 'NONE',  ( 7.283304719589999365, 4.462983737834999687, -8.994919855354998717 ) ) ;
#3684 = CARTESIAN_POINT ( 'NONE',  ( 18.29995268966800026, -2.861739928647000220, -11.98821236628000086 ) ) ;
#3685 = EDGE_CURVE ( 'NONE', #17499, #67326, #5208, .T. ) ;
#3686 = CARTESIAN_POINT ( 'NONE',  ( 17.75789140674246980, -3.091531401859648476, 12.29387995131532918 ) ) ;
#3687 = ORIENTED_EDGE ( 'NONE', *, *, #12236, .F. ) ;
#3688 = CARTESIAN_POINT ( 'NONE',  ( 11.20904026220999938, -5.937811873294999820, 7.147336919140999001 ) ) ;
#3689 = EDGE_CURVE ( 'NONE', #5290, #13996, #62965, .T. ) ;
#3690 = CARTESIAN_POINT ( 'NONE',  ( 11.59999999999999964, 4.420828903570659385, 8.516100029838437280 ) ) ;
#3691 = CYLINDRICAL_SURFACE ( 'NONE', #37238, 1.350000000000000533 ) ;
#3692 = CARTESIAN_POINT ( 'NONE',  ( 10.17310292480999934, -4.709171320598000143, -8.664883863910000983 ) ) ;
#3693 = CIRCLE ( 'NONE', #51712, 1.249999999999999778 ) ;
#3694 = CARTESIAN_POINT ( 'NONE',  ( -15.86200481174999943, 13.87069231928999891, 4.225386915259999654 ) ) ;
#3695 = EDGE_LOOP ( 'NONE', ( #8253, #34860, #29460, #42476 ) ) ;
#3696 = PRODUCT ( 'MAS-678', 'MAS-678', '', ( #41982 ) ) ;
#3697 = CARTESIAN_POINT ( 'NONE',  ( 24.01908949132420545, 12.68161222272001609, -3.458556830167235585 ) ) ;
#3698 = CARTESIAN_POINT ( 'NONE',  ( 5.188359839683666763, -0.7554284705563480973, -1.310679582531387277 ) ) ;
#3699 = CARTESIAN_POINT ( 'NONE',  ( 10.46166951222632591, -5.351570712698000776, 7.263306442112493322 ) ) ;
#3700 = DIRECTION ( 'NONE',  ( 0.000000000000000000, 1.000000000000000000, 0.000000000000000000 ) ) ;
#3701 = CARTESIAN_POINT ( 'NONE',  ( 12.19409625758322235, 0.1321590433901056461, -13.89915950722680016 ) ) ;
#3702 = CARTESIAN_POINT ( 'NONE',  ( 18.05208962242105741, -2.879457400869560146, 12.35505085550156501 ) ) ;
#3703 = ORIENTED_EDGE ( 'NONE', *, *, #25818, .T. ) ;
#3704 = CARTESIAN_POINT ( 'NONE',  ( 8.185765847591000011, -4.942196905450001232, 6.196983455206997782 ) ) ;
#3705 = ORIENTED_EDGE ( 'NONE', *, *, #23301, .T. ) ;
#3706 = CARTESIAN_POINT ( 'NONE',  ( 10.70441484796999987, 3.444517850837000239, 6.009055070331999815 ) ) ;
#3707 = EDGE_CURVE ( 'NONE', #65107, #43577, #17735, .T. ) ;
#3708 = AXIS2_PLACEMENT_3D ( 'NONE', #39749, #7581, #28930 ) ;
#3709 = CARTESIAN_POINT ( 'NONE',  ( 11.33810207955129812, -3.203462856645999945, -7.825000000000000178 ) ) ;
#3710 = CARTESIAN_POINT ( 'NONE',  ( 8.590779719591999708, 2.836879604150999601, -8.783908972046001296 ) ) ;
#3711 = CARTESIAN_POINT ( 'NONE',  ( 3.432088553994000257, 3.542926904065000215, -0.07481602154510001712 ) ) ;
#3712 = CARTESIAN_POINT ( 'NONE',  ( 10.51140025105000042, -2.326718149302000160, -7.741209600718000239 ) ) ;
#3713 = LINE ( 'NONE', #67343, #35066 ) ;
#3714 = AXIS2_PLACEMENT_3D ( 'NONE', #55751, #2596, #362 ) ;
#3715 = CARTESIAN_POINT ( 'NONE',  ( 9.001479836347179742, -5.278236052291213731, 7.933966972496419245 ) ) ;
#3716 = ORIENTED_EDGE ( 'NONE', *, *, #29201, .F. ) ;
#3717 = CARTESIAN_POINT ( 'NONE',  ( 12.03148876160955005, -4.790673964186999534, 6.677731919207799294 ) ) ;
#3718 = CYLINDRICAL_SURFACE ( 'NONE', #40984, 1.350000000000000533 ) ;
#3719 = CARTESIAN_POINT ( 'NONE',  ( 16.04495723965300158, 8.927588545536998765, 8.707532029612000457 ) ) ;
#3720 = B_SPLINE_CURVE_WITH_KNOTS ( 'NONE', 3,
 ( #27770, #59567, #37898, #32662, #65144, #11664, #43499, #16909, #17265, #60955, #56748, #13753, #40318, #34738, #13419, #29154, #8502, #29849 ),
 .UNSPECIFIED., .F., .F.,
 ( 4, 2, 2, 2, 2, 2, 2, 2, 4 ),
 ( 0.000000000000000000, 0.1250000000000000000, 0.2500000000000000000, 0.3750000000000000000, 0.5000000000000000000, 0.6250000000000000000, 0.7500000000000000000, 0.8750000000000000000, 1.000000000000000000 ),
 .UNSPECIFIED. ) ;
#3721 = CARTESIAN_POINT ( 'NONE',  ( 7.565629440376999248, -3.206365290996999740, 5.681739161071000410 ) ) ;
#3723 = LINE ( 'NONE', #41828, #11626 ) ;
#3722 = CARTESIAN_POINT ( 'NONE',  ( 9.662551629919999385, 4.094830335839000135, 9.119946295870999364 ) ) ;
#3724 = CARTESIAN_POINT ( 'NONE',  ( 10.79718447801629999, 5.003225587801999552, -7.477880487566260115 ) ) ;
#3725 = CARTESIAN_POINT ( 'NONE',  ( 24.63781072324900023, -11.77741428486000075, 3.228729438162000420 ) ) ;
#3726 = EDGE_CURVE ( 'NONE', #34076, #27484, #30245, .T. ) ;
#3727 = B_SPLINE_CURVE_WITH_KNOTS ( 'NONE', 3,
 ( #56755, #9876, #3933, #15475 ),
 .UNSPECIFIED., .F., .F.,
 ( 4, 4 ),
 ( 0.000000000000000000, 1.000000000000000000 ),
 .UNSPECIFIED. ) ;
#3728 = CARTESIAN_POINT ( 'NONE',  ( 9.021784697134998865, 4.545051930576500254, -6.656340890368899643 ) ) ;
#3729 = CARTESIAN_POINT ( 'NONE',  ( 18.25578817174763202, 0.1860047152749647326, 12.59864695008082336 ) ) ;
#3730 = DIRECTION ( 'NONE',  ( 0.000000000000000000, 0.7071067811865475727, 0.7071067811865475727 ) ) ;
#3731 = CARTESIAN_POINT ( 'NONE',  ( 4.574515983791000080E-07, 0.000000000000000000, 0.000000000000000000 ) ) ;
#3732 = EDGE_CURVE ( 'NONE', #41793, #8371, #52143, .T. ) ;
#3733 = CARTESIAN_POINT ( 'NONE',  ( 23.73689480596400259, 9.842602752810000410, 9.652213948273999478 ) ) ;
#3734 = ORIENTED_EDGE ( 'NONE', *, *, #1611, .T. ) ;
#3735 = CARTESIAN_POINT ( 'NONE',  ( 7.320269353207000229, -2.466384407480000096, 6.935560677555000275 ) ) ;
#3736 = CARTESIAN_POINT ( 'NONE',  ( 20.10000000000000142, 0.000000000000000000, 0.000000000000000000 ) ) ;
#3737 = CARTESIAN_POINT ( 'NONE',  ( 9.082867883171827472, 4.782673203840020371, 6.525013452213887177 ) ) ;
#3738 = CARTESIAN_POINT ( 'NONE',  ( 10.19810941423799910, -3.053977294209000437, -6.640722727400100389 ) ) ;
#3739 = ORIENTED_EDGE ( 'NONE', *, *, #36867, .F. ) ;
#3740 = CIRCLE ( 'NONE', #62925, 10.75000000000000533 ) ;
#3741 = CARTESIAN_POINT ( 'NONE',  ( 0.5267198524092000511, -3.063090672237000156, -0.9584583608479999572 ) ) ;
#3742 = CARTESIAN_POINT ( 'NONE',  ( 10.72702344389999851, 2.995605560827999891, 8.109550315577399360 ) ) ;
#3743 = CARTESIAN_POINT ( 'NONE',  ( 10.39539221959000059, 5.667182949051000840, -7.250689098107000241 ) ) ;
#3744 = ORIENTED_EDGE ( 'NONE', *, *, #65897, .T. ) ;
#3745 = CARTESIAN_POINT ( 'NONE',  ( 11.79999999550100220, 3.351258778187000242, -11.15757272551999968 ) ) ;
#3746 = CARTESIAN_POINT ( 'NONE',  ( 21.59999987243000064, 1.172395514003999961E-13, -2.486899575159999765E-14 ) ) ;
#3747 = CARTESIAN_POINT ( 'NONE',  ( 11.20733594839949809, 4.840266102192999575, 8.462948211532999920 ) ) ;
#3748 = CARTESIAN_POINT ( 'NONE',  ( 15.40000000001299973, 8.815237407733999220, 7.616696375847999967 ) ) ;
#3749 = FACE_OUTER_BOUND ( 'NONE', #51580, .T. ) ;
#3750 = VERTEX_POINT ( 'NONE', #19655 ) ;
#3751 = CARTESIAN_POINT ( 'NONE',  ( 11.60578299225600141, -3.447612089971000326, 11.88742905964999963 ) ) ;
#3752 = CARTESIAN_POINT ( 'NONE',  ( 8.353629719588999691, 5.354408404900999230, -6.419792067946000103 ) ) ;
#3753 = CARTESIAN_POINT ( 'NONE',  ( 8.119297623376104056, -4.926355840723960711, 6.024311677146462429 ) ) ;
#3754 = CIRCLE ( 'NONE', #50694, 0.2999999999999999334 ) ;
#3755 = CARTESIAN_POINT ( 'NONE',  ( 9.524747021775999301, -4.858221690000700477, 6.746879837742599584 ) ) ;
#3756 = ORIENTED_EDGE ( 'NONE', *, *, #27217, .T. ) ;
#3757 = CARTESIAN_POINT ( 'NONE',  ( 10.42469759965999998, -4.813117804065999650, -5.025876989183999832 ) ) ;
#3758 = CARTESIAN_POINT ( 'NONE',  ( 10.91964694612699915, -5.186980343482999523, 7.026297514493899499 ) ) ;
#3759 = ORIENTED_EDGE ( 'NONE', *, *, #23060, .T. ) ;
#3760 = CARTESIAN_POINT ( 'NONE',  ( 9.977263540182335078, -4.629523725463626782, 6.407767014557177454 ) ) ;
#3761 = CONICAL_SURFACE ( 'NONE', #55134, 1.949999999913999860, 0.7853981633972997312 ) ;
#3762 = ORIENTED_EDGE ( 'NONE', *, *, #58697, .T. ) ;
#3763 = LINE ( 'NONE', #37313, #50964 ) ;
#3764 = DIRECTION ( 'NONE',  ( -1.000000000000000000, 0.000000000000000000, 0.000000000000000000 ) ) ;
#3765 = CARTESIAN_POINT ( 'NONE',  ( 11.52166954483529793, 4.562096242626500597, -6.632714178206799538 ) ) ;
#3766 = CARTESIAN_POINT ( 'NONE',  ( 11.47124174884019965, -4.036194082918090231, 6.184229974648999928 ) ) ;
#3767 = CARTESIAN_POINT ( 'NONE',  ( 12.28024293382672028, 2.160546425968631556, -12.52422939561507675 ) ) ;
#3768 = EDGE_CURVE ( 'NONE', #35849, #24800, #24896, .T. ) ;
#3769 = CARTESIAN_POINT ( 'NONE',  ( 11.14533863405319991, -3.296214805808900028, 6.602238051205399749 ) ) ;
#3770 = CARTESIAN_POINT ( 'NONE',  ( 7.886573341228999112, 3.084076314893000159, 9.259847992573000397 ) ) ;
#3771 = ADVANCED_FACE ( 'NONE', ( #35396 ), #8817, .F. ) ;
#3772 = ORIENTED_EDGE ( 'NONE', *, *, #2221, .F. ) ;
#3773 = CARTESIAN_POINT ( 'NONE',  ( 11.09999999999999964, 2.649999999999999911, -7.500000000000000000 ) ) ;
#3774 = B_SPLINE_CURVE_WITH_KNOTS ( 'NONE', 3,
 ( #41596, #67463, #15373, #30766 ),
 .UNSPECIFIED., .F., .F.,
 ( 4, 4 ),
 ( 0.000000000000000000, 1.000000000000000000 ),
 .UNSPECIFIED. ) ;
#3775 = CARTESIAN_POINT ( 'NONE',  ( 7.968183059622999664, -2.280579276705999803, 6.510290672242000198 ) ) ;
#3776 = CARTESIAN_POINT ( 'NONE',  ( 15.89994436294300151, -8.847904542234999781, -8.580301953175000662 ) ) ;
#3777 = ORIENTED_EDGE ( 'NONE', *, *, #17925, .F. ) ;
#3778 = CARTESIAN_POINT ( 'NONE',  ( 12.41053097114618708, -2.984774150185583785, -12.32529705072536963 ) ) ;
#3779 = CARTESIAN_POINT ( 'NONE',  ( 10.47303166480599934, 2.862083839376000416, 7.419769534118209720 ) ) ;
#3780 = CARTESIAN_POINT ( 'NONE',  ( 10.33453064679000200, -3.295701412239999684, -6.149875347297999895 ) ) ;
#3781 = CARTESIAN_POINT ( 'NONE',  ( 6.981311842138000934, 10.82753206518999534, -3.400792444267003667 ) ) ;
#3782 = CARTESIAN_POINT ( 'NONE',  ( 17.61613042390700201, -12.05009377076000021, 3.195812565461000343 ) ) ;
#3783 = FACE_OUTER_BOUND ( 'NONE', #40083, .T. ) ;
#3784 = CARTESIAN_POINT ( 'NONE',  ( 12.41408225146707522, -2.012274740545227480, -13.76483611190084133 ) ) ;
#3785 = CARTESIAN_POINT ( 'NONE',  ( 11.58902763632552002, -4.786505910413500153, -7.137085349939700230 ) ) ;
#3786 = CARTESIAN_POINT ( 'NONE',  ( 11.20733594839949809, -3.159733897807000425, -6.537051788466999191 ) ) ;
#3787 = CARTESIAN_POINT ( 'NONE',  ( 11.09999999999999964, 4.000000000000000000, 7.500000000000000000 ) ) ;
#3788 = ORIENTED_EDGE ( 'NONE', *, *, #28518, .T. ) ;
#3789 = EDGE_LOOP ( 'NONE', ( #67150, #61530, #29888, #3276 ) ) ;
#3790 = DIRECTION ( 'NONE',  ( 0.7071062208423759543, -0.7071073415302749909, 1.056388098201964040E-09 ) ) ;
#3791 = EDGE_CURVE ( 'NONE', #45267, #47657, #2882, .T. ) ;
#3792 = AXIS2_PLACEMENT_3D ( 'NONE', #63666, #64345, #21368 ) ;
#3793 = CARTESIAN_POINT ( 'NONE',  ( 23.60001133530950668, -1.983597864821140026E-14, -13.89477126879791058 ) ) ;
#3794 = CARTESIAN_POINT ( 'NONE',  ( 18.17228756840857073, 2.598712620722948508, 13.65197972919175484 ) ) ;
#3795 = CARTESIAN_POINT ( 'NONE',  ( 10.06728116094000036, 4.192860729918999496, -5.985054792427000336 ) ) ;
#3796 = CARTESIAN_POINT ( 'NONE',  ( 5.500000000000000000, 0.000000000000000000, 0.000000000000000000 ) ) ;
#3797 = CARTESIAN_POINT ( 'NONE',  ( 18.00599872992918549, 2.932869382066923603, 12.34010572687589757 ) ) ;
#3798 = CARTESIAN_POINT ( 'NONE',  ( 17.79290994143500271, 3.413161104324000217, -11.89755508104000015 ) ) ;
#3799 = CARTESIAN_POINT ( 'NONE',  ( 9.013423559847998590, 4.933953210258000155, 8.417881984655998906 ) ) ;
#3800 = CARTESIAN_POINT ( 'NONE',  ( 10.13586576648898330, -5.314625264832349316, -7.853278872971151792 ) ) ;
#3801 = VERTEX_POINT ( 'NONE', #34713 ) ;
#3802 = CARTESIAN_POINT ( 'NONE',  ( 9.905792474809000936, 2.698958900805999761, 8.979236532123000103 ) ) ;
#3803 = CARTESIAN_POINT ( 'NONE',  ( 8.943784697134999462, -3.529509552262100058, -6.771750947090999340 ) ) ;
#3804 = CARTESIAN_POINT ( 'NONE',  ( 9.534905769125000319, 3.030948166328000237, 8.761984216465000586 ) ) ;
#3805 = CARTESIAN_POINT ( 'NONE',  ( 12.26588784977539959, -5.120865761890000201, 7.564049652083489228 ) ) ;
#3806 = CARTESIAN_POINT ( 'NONE',  ( 7.156776345353000224, 1.243223188895000053, 2.274921040069000118E-10 ) ) ;
#3807 = CARTESIAN_POINT ( 'NONE',  ( 24.87965768662300192, 8.586235434208999706, 8.375234271308000800 ) ) ;
#3808 = CARTESIAN_POINT ( 'NONE',  ( 12.18407639872240189, 0.07155418421575378274, 12.69973420405192144 ) ) ;
#3809 = CIRCLE ( 'NONE', #30631, 10.75000000000000000 ) ;
#3810 = CARTESIAN_POINT ( 'NONE',  ( 8.289114158772999730, 4.310355144869000732, 9.459505265942000918 ) ) ;
#3811 = CARTESIAN_POINT ( 'NONE',  ( 10.22108913916999917, 2.983268757921999637, 8.764704075288999974 ) ) ;
#3812 = DIRECTION ( 'NONE',  ( 0.000000000000000000, 1.000000000000000000, 0.000000000000000000 ) ) ;
#3813 = ADVANCED_FACE ( 'NONE', ( #24205 ), #40976, .T. ) ;
#3814 = VERTEX_POINT ( 'NONE', #45548 ) ;
#3815 = CIRCLE ( 'NONE', #47352, 0.7499999936418002555 ) ;
#3816 = CARTESIAN_POINT ( 'NONE',  ( 9.427245280414000561, 4.989193221215000307, -6.287302145481000082 ) ) ;
#3817 = CARTESIAN_POINT ( 'NONE',  ( 7.061156573014000237, -1.318960494382000137, -0.6866539737626000672 ) ) ;
#3818 = CARTESIAN_POINT ( 'NONE',  ( 17.81540764135917243, 1.931433452195108869, 13.77768866547343407 ) ) ;
#3819 = DIRECTION ( 'NONE',  ( 1.000000000000000000, 0.000000000000000000, 0.000000000000000000 ) ) ;
#3820 = DIRECTION ( 'NONE',  ( 0.000000000000000000, 1.000000000000000000, 0.000000000000000000 ) ) ;
#3821 = CARTESIAN_POINT ( 'NONE',  ( 10.96949144726329806, -4.580206776679999869, -6.681274802424499448 ) ) ;
#3822 = ORIENTED_EDGE ( 'NONE', *, *, #9776, .T. ) ;
#3823 = CARTESIAN_POINT ( 'NONE',  ( 1.300700459006000065, -0.3635854775007999473, -3.573745162754999871 ) ) ;
#3824 = CARTESIAN_POINT ( 'NONE',  ( 12.18965064077888627, 11.77436608085541536, -3.633175706307454345 ) ) ;
#3827 = UNCERTAINTY_MEASURE_WITH_UNIT (LENGTH_MEASURE( 1.000000000000000082E-05 ), #61246, 'distance_accuracy_value', 'NONE');
#3826 = FACE_OUTER_BOUND ( 'NONE', #14473, .T. ) ;
#3825 = CARTESIAN_POINT ( 'NONE',  ( 8.275189158773001097, 3.061731693614000438, -8.535706278603999664 ) ) ;
#3828 = CARTESIAN_POINT ( 'NONE',  ( 15.89979320884932967, 7.372865056442157616, 9.926947018133178702 ) ) ;
#3829 = CARTESIAN_POINT ( 'NONE',  ( 9.514114512910998300, 4.887632373702999189, 8.462748516415999234 ) ) ;
#3830 = CARTESIAN_POINT ( 'NONE',  ( 17.96975113184320350, -2.032288328865629268, -13.76155421333986340 ) ) ;
#3831 = CARTESIAN_POINT ( 'NONE',  ( 11.39210538575740017, 4.842454415653899780, 7.701417844014099678 ) ) ;
#3832 = CARTESIAN_POINT ( 'NONE',  ( 24.81129275592842021, -11.68008348722340273, 3.194587719868046349 ) ) ;
#3833 = CARTESIAN_POINT ( 'NONE',  ( 7.694004440376999376, -5.850279024084999335, 6.784181137144999596 ) ) ;
#3834 = ORIENTED_EDGE ( 'NONE', *, *, #49027, .F. ) ;
#3835 = CARTESIAN_POINT ( 'NONE',  ( 7.673642219589999591, 4.696238830159999544, 5.830273622963999536 ) ) ;
#3837 = CARTESIAN_POINT ( 'NONE',  ( 10.45625805961999966, -3.661873208228000109, -9.317463915629002003 ) ) ;
#3836 = CARTESIAN_POINT ( 'NONE',  ( 6.562102968646999379, -1.381912473529000041, 0.6877288610791999490 ) ) ;
#3838 = CARTESIAN_POINT ( 'NONE',  ( 7.458084730951140884, -2.267780973363890062, 7.308742852188579775 ) ) ;
#3839 = AXIS2_PLACEMENT_3D ( 'NONE', #61094, #50949, #67017 ) ;
#3840 = CARTESIAN_POINT ( 'NONE',  ( 17.95596346641302077, -0.4795055877513557108, 13.88886709645684547 ) ) ;
#3841 = CARTESIAN_POINT ( 'NONE',  ( 1.552519953415999909, -1.310877008326999826, -3.164872840607000359 ) ) ;
#3842 = VERTEX_POINT ( 'NONE', #67879 ) ;
#3843 = CARTESIAN_POINT ( 'NONE',  ( 2.001596192978043476, -3.143789697970717167, 1.012455472687556313 ) ) ;
#3844 = CARTESIAN_POINT ( 'NONE',  ( 11.05518582084300050, -4.566724035220099509, 8.155074391384399490 ) ) ;
#3845 = CARTESIAN_POINT ( 'NONE',  ( 11.07236672166249924, -2.278048615010975553, -7.888876361990175390 ) ) ;
#3846 = CARTESIAN_POINT ( 'NONE',  ( 10.50244247011999832, 2.268911387573000038, 7.824865741583000300 ) ) ;
#3847 = CARTESIAN_POINT ( 'NONE',  ( 11.30995122972050027, 4.452766304612699955, 8.547040013405998948 ) ) ;
#3848 = PRODUCT_DEFINITION_SHAPE ( 'NONE', 'NONE',  #69204 ) ;
#3849 = CARTESIAN_POINT ( 'NONE',  ( 9.629471092178999214, 5.100000000000000533, 6.152188490330000370 ) ) ;
#3850 = CARTESIAN_POINT ( 'NONE',  ( 9.709999999999999076, 4.496968146123999865, -8.755198255949000696 ) ) ;
#3851 = EDGE_CURVE ( 'NONE', #36962, #18749, #68215, .T. ) ;
#3852 = CARTESIAN_POINT ( 'NONE',  ( 24.14474107922869806, -3.678932646489693870, -12.80134524014008690 ) ) ;
#3853 = ADVANCED_FACE ( 'NONE', ( #66853 ), #49495, .F. ) ;
#3854 = CARTESIAN_POINT ( 'NONE',  ( 24.37847033660100138, -3.167532588666000404, -12.03742754479999988 ) ) ;
#3855 = CIRCLE ( 'NONE', #524, 1.799999999999999156 ) ;
#3856 = ORIENTED_EDGE ( 'NONE', *, *, #26270, .T. ) ;
#3857 = CARTESIAN_POINT ( 'NONE',  ( 17.78669369145618973, -1.919420387948956419, 13.77958849407365349 ) ) ;
#3858 = CARTESIAN_POINT ( 'NONE',  ( 8.737804660583998739, 4.491756428607999396, -5.831236541471000123 ) ) ;
#3859 = ORIENTED_EDGE ( 'NONE', *, *, #40205, .T. ) ;
#3860 = CARTESIAN_POINT ( 'NONE',  ( 8.941938785621264429, -5.237454815711724443, 6.943328879398332099 ) ) ;
#3861 = B_SPLINE_CURVE_WITH_KNOTS ( 'NONE', 3,
 ( #30628, #63103, #19791, #47051 ),
 .UNSPECIFIED., .F., .F.,
 ( 4, 4 ),
 ( 0.000000000000000000, 1.000000000000000000 ),
 .UNSPECIFIED. ) ;
#3862 = CARTESIAN_POINT ( 'NONE',  ( 23.58888753768338375, 10.33110938381009980, -9.338951014280834073 ) ) ;
#3863 = ORIENTED_EDGE ( 'NONE', *, *, #13383, .F. ) ;
#3864 = CARTESIAN_POINT ( 'NONE',  ( 10.56690934386000080, -5.170965040585000061, 4.739956486541999858 ) ) ;
#3866 = CARTESIAN_POINT ( 'NONE',  ( 11.29364426047339975, 4.466097552695299733, 6.769896129503799820 ) ) ;
#3865 = VECTOR ( 'NONE', #26408, 1000.000000000000000 ) ;
#3867 = CARTESIAN_POINT ( 'NONE',  ( 10.00138108374000012, 3.855364958793999985, 5.709478909302000638 ) ) ;
#3868 = CARTESIAN_POINT ( 'NONE',  ( 10.88015784977000067, 2.793131772868000073, -6.864962922767000819 ) ) ;
#3869 = CARTESIAN_POINT ( 'NONE',  ( 10.13874943042162613, -4.847937002157847175, -7.715719979441764131 ) ) ;
#3870 = CARTESIAN_POINT ( 'NONE',  ( 10.73930809942999964, -2.762991917822000154, 6.801028165221000066 ) ) ;
#3871 = CARTESIAN_POINT ( 'NONE',  ( 18.00565376249823046, 0.5635217852606941857, -12.58739276154098086 ) ) ;
#3872 = CARTESIAN_POINT ( 'NONE',  ( 18.49993212792200126, 2.908182645667999999, 12.18276646858999968 ) ) ;
#3873 = CARTESIAN_POINT ( 'NONE',  ( 10.53057053952199951, -4.340412141385700195, -6.703496287302799672 ) ) ;
#3874 = CARTESIAN_POINT ( 'NONE',  ( 8.330260465798849268, 5.101896243649416185, -8.673380106616962237 ) ) ;
#3875 = ORIENTED_EDGE ( 'NONE', *, *, #52731, .T. ) ;
#3876 = EDGE_CURVE ( 'NONE', #7451, #8271, #61935, .T. ) ;
#3877 = CIRCLE ( 'NONE', #40712, 11.84999999999999964 ) ;
#3878 = CYLINDRICAL_SURFACE ( 'NONE', #2435, 1.000000000000000000 ) ;
#3879 = CYLINDRICAL_SURFACE ( 'NONE', #33885, 1.350000000000000533 ) ;
#3880 = CARTESIAN_POINT ( 'NONE',  ( 23.59999468372399889, -2.915558691838999739, 13.58549495651999983 ) ) ;
#3881 = EDGE_CURVE ( 'NONE', #48209, #5914, #7697, .T. ) ;
#3882 = CARTESIAN_POINT ( 'NONE',  ( 7.557540957726994968, 10.72894448916999544, 3.699722378877996931 ) ) ;
#3883 = CARTESIAN_POINT ( 'NONE',  ( 12.14431428438022564, 2.818682143830020248, 13.71332026632872747 ) ) ;
#3884 = CARTESIAN_POINT ( 'NONE',  ( 10.52324012719000024, -3.325647021086999722, 5.689999163383999026 ) ) ;
#3885 = ORIENTED_EDGE ( 'NONE', *, *, #23279, .T. ) ;
#3886 = CARTESIAN_POINT ( 'NONE',  ( 12.53084372997124163, 0.5620101267580669413, -12.68326259364286202 ) ) ;
#3887 = CARTESIAN_POINT ( 'NONE',  ( 12.08965255773060221, -0.1190513140356090627, 13.99949878896183719 ) ) ;
#3888 = ORIENTED_EDGE ( 'NONE', *, *, #31740, .F. ) ;
#3889 = DIRECTION ( 'NONE',  ( 0.000000000000000000, 0.9999503185633161761, 0.009967968956736161443 ) ) ;
#3890 = CARTESIAN_POINT ( 'NONE',  ( 10.88269270164825997, 5.042464834414079888, -4.893996439828388390 ) ) ;
#3891 = CARTESIAN_POINT ( 'NONE',  ( 10.83351354018309998, -5.249999999999999112, -7.336375382625531572 ) ) ;
#3892 = DIRECTION ( 'NONE',  ( 1.000000000000000000, 0.000000000000000000, 0.000000000000000000 ) ) ;
#3893 = B_SPLINE_SURFACE_WITH_KNOTS ( 'NONE', 3, 3, ( 
 ( #27765, #3174, #45824, #27410, #33001, #54315, #59215, #33697, #23197, #6415, #12016, #17964, #16904, #33352, #38234, #17618, #59563, #49416, #12367, #56317, #1187, #7118, #1528, #32658, #65491, #11317, #28456, #65840, #60604, #11660, #6073, #39283, #49770, #1881, #43839, #48736, #12715, #8422, #29765, #9100, #30439, #19601, #62916, #41265, #47203, #4880, #4533, #15387, #14361, #68505, #9785, #67820, #51750, #36017, #3844, #58036, #52089, #14015, #67135, #56999, #68162, #3506, #62579, #40920, #35685, #62243, #41610 ),
 ( #30777, #19246, #4193, #20282, #41952, #25182, #24844, #30108, #40574, #46517, #19944, #25530, #67479, #15037, #9435, #36715, #25869, #20627, #14700, #31467, #52786, #8766, #57333, #46859, #26223, #36363, #63260, #57676, #31135, #10135, #46171, #52437, #61901, #35344, #56660, #51410, #48575, #64976, #63951, #680, #37737, #63612, #32499, #47551, #16745, #6254, #22340, #21312, #20974, #54155, #16406, #59062, #16062, #11499, #15728, #42982, #68854, #42310, #333, #64289, #5912, #43678, #17090, #53814, #21991, #26912, #11164 ),
 ( #37392, #1028, #48227, #32843, #37055, #58716, #27253, #43334, #27594, #64639, #53477, #58370, #26569, #21647, #6604, #38422, #10472, #59747, #31813, #38073, #48920, #59400, #11848, #33186, #32162, #54505, #53132, #5231, #47894, #59795, #42642, #10820, #5571, #2065, #17450, #66366, #44722, #23724, #55893, #49605, #61476, #28285, #13252, #50302, #55547, #49952, #39813, #34916, #39120, #1713, #7997, #17801, #56230, #44028, #60443, #23032, #45059, #12551, #18489, #65331, #1366, #33882, #44381, #27946, #50643, #18143, #29331 ),
 ( #24069, #45406, #34228, #2399, #7300, #39465, #12206, #55198, #54853, #61135, #28642, #34577, #33534, #38776, #49257, #22684, #66714, #65679, #2743, #60786, #23383, #66020, #18834, #40161, #7645, #6954, #60100, #12899, #13595, #28993, #67730, #46771, #13931, #14614, #9346, #31043, #46083, #19854, #40488, #35258, #61814, #46428, #56574, #40831, #25438, #8678, #50986, #24757, #25784, #52351, #3758, #67390, #19512, #62155, #4103, #41519, #36623, #62830, #25097, #68074, #9697, #30025, #3083, #9014, #51327, #14274, #24417 ) ),
 .UNSPECIFIED., .F., .F., .F.,
 ( 4, 4 ),
 ( 4, 1, 1, 1, 1, 1, 1, 1, 1, 1, 1, 1, 1, 1, 1, 1, 1, 1, 1, 1, 1, 1, 1, 1, 1, 1, 1, 1, 1, 1, 1, 1, 1, 1, 1, 1, 1, 1, 1, 1, 1, 1, 1, 1, 1, 1, 1, 1, 1, 1, 1, 1, 1, 1, 1, 1, 1, 1, 1, 1, 1, 1, 1, 1, 4 ),
 ( -0.02000000000000000042, 1.020000000000000018 ),
 ( 0.008747244164287000176, 0.02453926110774999961, 0.04033127805120999970, 0.05612329499467000327, 0.07191531193812999989, 0.08770732888158999652, 0.1034993458251000087, 0.1192913627684999978, 0.1350833797120000179, 0.1508753966553999792, 0.1666674135988999994, 0.1824594305423999918, 0.1982514474858000086, 0.2140434644293000011, 0.2298354813727000179, 0.2456274983162000103, 0.2614195152596999749, 0.2772115322030999640, 0.2930035491465999842, 0.3087955660900000288, 0.3245875830334999934, 0.3403795999769999581, 0.3561716169204000026, 0.3719636338639000228, 0.3877556508073999875, 0.4035476677507999765, 0.4193396846942999967, 0.4351317016376999858, 0.4509237185811999504, 0.4667157355247000261, 0.4825077524681000152, 0.4982997694115999798, 0.5140917863550000799, 0.5298838032985000446, 0.5456758202420000092, 0.5614678371854000538, 0.5772598541289000185, 0.5930518710723000630, 0.6088438880158000277, 0.6246359049592999924, 0.6404279219027000369, 0.6562199388462000016, 0.6720119557896999662, 0.6878039727331000108, 0.7035959896765999755, 0.7193880066200000201, 0.7351800235634999847, 0.7509720405069999494, 0.7667640574504001050, 0.7825560743939000696, 0.7983480913373000032, 0.8141401082808000789, 0.8299321252243000435, 0.8457241421676999771, 0.8615161591112000528, 0.8773081760545999863, 0.8931001929981000620, 0.9088922099416000266, 0.9246842268849999602, 0.9404762438285000359, 0.9562682607720000005, 0.9720602777153999341, 0.9878522946589000098, 1.003644311601999961, 1.019436328545999970 ),
 .UNSPECIFIED. ) ;
#3894 = CARTESIAN_POINT ( 'NONE',  ( 27.64127793187000037, -2.399999999999999911, -6.571291218949999902 ) ) ;
#3895 = PRODUCT_DEFINITION_FORMATION_WITH_SPECIFIED_SOURCE ( 'ANY', '', #50578, .NOT_KNOWN. ) ;
#3896 = DIRECTION ( 'NONE',  ( -1.000000000000000000, 0.000000000000000000, 0.000000000000000000 ) ) ;
#3897 = CARTESIAN_POINT ( 'NONE',  ( 11.00301147230000076, 2.832304442428000169, 4.969741576018000373 ) ) ;
#3898 = CARTESIAN_POINT ( 'NONE',  ( 12.08013217067790990, 2.460179751193587006, 12.35749396829501023 ) ) ;
#3899 = CARTESIAN_POINT ( 'NONE',  ( 9.957251191599000961, -4.686746084135999801, -9.174865097765998456 ) ) ;
#3900 = CARTESIAN_POINT ( 'NONE',  ( 11.53564291764652872, 3.004110626587600308, -7.376893506359599506 ) ) ;
#3901 = CARTESIAN_POINT ( 'NONE',  ( 11.09999999999999964, 4.000000000000000000, -7.500000000000000000 ) ) ;
#3902 = CARTESIAN_POINT ( 'NONE',  ( 10.52946886766499901, 3.569835351907400423, -6.718432993015899690 ) ) ;
#3903 = CARTESIAN_POINT ( 'NONE',  ( 8.972076168957999087, 3.350848599899200142, -8.602264418015000302 ) ) ;
#3905 = FACE_OUTER_BOUND ( 'NONE', #1582, .T. ) ;
#3904 = DIRECTION ( 'NONE',  ( 1.000000000000000000, 0.000000000000000000, 0.000000000000000000 ) ) ;
#3906 = CARTESIAN_POINT ( 'NONE',  ( 23.57471769411892737, -13.35750757171955527, 4.149007248513409074 ) ) ;
#3907 = ORIENTED_EDGE ( 'NONE', *, *, #62563, .F. ) ;
#3908 = CARTESIAN_POINT ( 'NONE',  ( 18.30000000000000071, -7.694584455362999620, 1.879999999999999893 ) ) ;
#3909 = AXIS2_PLACEMENT_3D ( 'NONE', #14813, #62691, #29884 ) ;
#3910 = DIRECTION ( 'NONE',  ( 1.000000000000000000, 0.000000000000000000, 0.000000000000000000 ) ) ;
#3911 = CARTESIAN_POINT ( 'NONE',  ( 9.501025935145998247, 3.874109063559000088, 8.357822485499299958 ) ) ;
#3912 = CARTESIAN_POINT ( 'NONE',  ( 8.998937807218627682, 3.944921334759000420, -6.626788336335921237 ) ) ;
#3913 = DIRECTION ( 'NONE',  ( 0.000000000000000000, 1.000000000000000000, 0.000000000000000000 ) ) ;
#3914 = CARTESIAN_POINT ( 'NONE',  ( 12.76347793713369505, -1.876036575608651447, 13.78616487348348052 ) ) ;
#3915 = CARTESIAN_POINT ( 'NONE',  ( 12.64199182499262619, 3.104696382830980372, 13.52638422211090408 ) ) ;
#3916 = CARTESIAN_POINT ( 'NONE',  ( 23.61813871572700307, 2.884258943580999990, -13.53885632044999987 ) ) ;
#3917 = ORIENTED_EDGE ( 'NONE', *, *, #27223, .T. ) ;
#3918 = CARTESIAN_POINT ( 'NONE',  ( 4.592741125323000162, 1.103414028882999887, 0.2634071631652999956 ) ) ;
#3919 = CARTESIAN_POINT ( 'NONE',  ( 9.909254614703000286, -5.239722547583999912, -7.815392442832299835 ) ) ;
#3920 = CARTESIAN_POINT ( 'NONE',  ( 8.856793857978997764, 5.100000000000000533, -6.339888365514000590 ) ) ;
#3921 = CARTESIAN_POINT ( 'NONE',  ( 11.48656920625009903, -3.967932847735990531, 8.391549386185598536 ) ) ;
#3922 = CARTESIAN_POINT ( 'NONE',  ( 18.00033872679588498, 1.911966235111669743, -12.45410047071287174 ) ) ;
#3923 = CARTESIAN_POINT ( 'NONE',  ( 10.86169145887000020, -2.934707142245000178, 5.180212859994000496 ) ) ;
#3924 = CARTESIAN_POINT ( 'NONE',  ( 18.07102077504459814, 2.852831731484589906, 12.36232801722215235 ) ) ;
#3925 = CARTESIAN_POINT ( 'NONE',  ( 12.18001976712812073, 2.492954602445635715, -13.67495394283574228 ) ) ;
#3926 = CARTESIAN_POINT ( 'NONE',  ( 10.96990540416000037, -2.852123108999999879, -5.029685703292000376 ) ) ;
#3927 = CARTESIAN_POINT ( 'NONE',  ( 10.64557055961999943, -2.988935764546999607, -5.952339209104000162 ) ) ;
#3928 = CARTESIAN_POINT ( 'NONE',  ( 8.911640687508834091, 2.873222873817929734, -6.752018918866312447 ) ) ;
#3929 = VECTOR ( 'NONE', #14484, 1000.000000000000227 ) ;
#3930 = CARTESIAN_POINT ( 'NONE',  ( 12.50552075632584170, 0.6654101994098731154, -13.98418081573738903 ) ) ;
#3931 = CARTESIAN_POINT ( 'NONE',  ( 9.073148997461000675, 5.167567567567999731, -6.822293592207000934 ) ) ;
#3932 = EDGE_CURVE ( 'NONE', #20142, #47790, #68600, .T. ) ;
#3933 = CARTESIAN_POINT ( 'NONE',  ( 24.34832118755700137, -8.810502277406902394, 8.810502277406998317 ) ) ;
#3934 = EDGE_CURVE ( 'NONE', #66816, #59953, #13552, .T. ) ;
#3935 = CARTESIAN_POINT ( 'NONE',  ( 2.998890132544666631, 2.798833948393634419, -2.150913519912196925 ) ) ;
#3936 = CARTESIAN_POINT ( 'NONE',  ( 9.608904719592000987, 4.946705552514000459, -6.253848946732999181 ) ) ;
#3937 = CARTESIAN_POINT ( 'NONE',  ( 6.569697510850818212, -1.499768286218591706, -0.2711207260315494083 ) ) ;
#3938 = ORIENTED_EDGE ( 'NONE', *, *, #63566, .F. ) ;
#3939 = ADVANCED_FACE ( 'NONE', ( #34546 ), #59289, .T. ) ;
#3940 = CARTESIAN_POINT ( 'NONE',  ( 9.135881449927612863, -5.314639390875580460, -7.853423517146890909 ) ) ;
#3941 = CARTESIAN_POINT ( 'NONE',  ( 18.06104743845536831, 3.040966990778155132, -13.66574534766771798 ) ) ;
#3942 = ORIENTED_EDGE ( 'NONE', *, *, #64210, .T. ) ;
#3943 = CARTESIAN_POINT ( 'NONE',  ( 10.16200081823899914, -4.767147064380999666, 7.096028062709999418 ) ) ;
#3944 = CARTESIAN_POINT ( 'NONE',  ( 11.75203632436369894, 2.890282938442000127, 7.759151359668400083 ) ) ;
#3945 = CARTESIAN_POINT ( 'NONE',  ( 8.944760841233000193, 4.990139824845000405, -9.121472988377998803 ) ) ;
#3946 = CARTESIAN_POINT ( 'NONE',  ( 13.86901036581968860, 9.187486520156699754, 8.213234632844541139 ) ) ;
#3947 = CARTESIAN_POINT ( 'NONE',  ( 10.98146005378009882, -3.088328798999600000, -7.013182449205100255 ) ) ;
#3948 = DIRECTION ( 'NONE',  ( -0.000000000000000000, -0.000000000000000000, 1.000000000000000000 ) ) ;
#3949 = CARTESIAN_POINT ( 'NONE',  ( 9.716851002543000604, -2.832432432432000269, 6.822293592207000934 ) ) ;
#3950 = EDGE_LOOP ( 'NONE', ( #15795, #10678, #37059, #68015, #13253, #23913, #23584, #30978, #63029, #47219, #26395, #50303, #62739, #26387, #67509 ) ) ;
#3951 = CARTESIAN_POINT ( 'NONE',  ( 25.29987261392200182, 8.756202924575998026, -7.455126447192999883 ) ) ;
#3952 =( BOUNDED_SURFACE ( )  B_SPLINE_SURFACE ( 3, 3, ( 
 ( #65004, #2100, #59089, #709 ),
 ( #28672, #33564, #43710, #1742 ),
 ( #16772, #32871, #17832, #54184 ),
 ( #54883, #17123, #6282, #66056 ) ),
 .UNSPECIFIED., .F., .F., .T. ) 
 B_SPLINE_SURFACE_WITH_KNOTS ( ( 4, 4 ),
 ( 4, 4 ),
 ( 0.000000000000000000, 1.000000000000000000 ),
 ( 0.000000000000000000, 1.000000000000000000 ),
 .UNSPECIFIED. ) 
 GEOMETRIC_REPRESENTATION_ITEM ( )  RATIONAL_B_SPLINE_SURFACE ( (
 ( 1.512182578520000042, 1.160176301760999840, 1.160176301760999840, 1.512182578520000042),
 ( 1.111288591041000196, 0.8526025270081000196, 0.8526025270081000196, 1.111288591041000196),
 ( 1.111288591041000196, 0.8526025270081000196, 0.8526025270081000196, 1.111288591041000196),
 ( 1.512182578520000042, 1.160176301760999840, 1.160176301760999840, 1.512182578520000042) ) ) 
 REPRESENTATION_ITEM ( '' )  SURFACE ( )  );
#3953 = CARTESIAN_POINT ( 'NONE',  ( 8.400739158770999637, 4.933589693325000525, -9.154576215408999573 ) ) ;
#3954 = ORIENTED_EDGE ( 'NONE', *, *, #53660, .F. ) ;
#3955 = CARTESIAN_POINT ( 'NONE',  ( 11.07336716268999943, 2.375546981533999791, -8.393546861057000541 ) ) ;
#3956 = ORIENTED_EDGE ( 'NONE', *, *, #56717, .F. ) ;
#3957 = CARTESIAN_POINT ( 'NONE',  ( 9.607317406968999052, 4.212364169857599983, 6.378110563671000044 ) ) ;
#3958 = CARTESIAN_POINT ( 'NONE',  ( 17.59659105803586954, -1.876041592512284195, -12.57524627323323863 ) ) ;
#3959 = EDGE_CURVE ( 'NONE', #16603, #11416, #48553, .T. ) ;
#3960 = CIRCLE ( 'NONE', #63140, 1.000000000000000222 ) ;
#3961 = CARTESIAN_POINT ( 'NONE',  ( 12.79999999202000005, 11.41069016990000051, -4.623987642516999230 ) ) ;
#3962 = FACE_OUTER_BOUND ( 'NONE', #7902, .T. ) ;
#3963 = CARTESIAN_POINT ( 'NONE',  ( 11.80671024775549682, -3.379344054882541304, 6.880623181275072220 ) ) ;
#3964 = VERTEX_POINT ( 'NONE', #38127 ) ;
#3965 = DIRECTION ( 'NONE',  ( 1.000000000000000000, -4.332706595949694629E-15, 1.401268137124204108E-14 ) ) ;
#3966 = CARTESIAN_POINT ( 'NONE',  ( 10.27367334122999942, 3.065551304793999510, -8.487910413489000661 ) ) ;
#3967 = CARTESIAN_POINT ( 'NONE',  ( 8.433148997460000018, -5.167567567567999731, 6.822293592207000934 ) ) ;
#3968 = FACE_OUTER_BOUND ( 'NONE', #68952, .T. ) ;
#3969 = CARTESIAN_POINT ( 'NONE',  ( 17.82168025737886197, 0.6791475903683997783, 13.98351814429473094 ) ) ;
#3970 = CARTESIAN_POINT ( 'NONE',  ( 10.31746213571000048, 5.100000000000000533, 6.571291218949999902 ) ) ;
#3971 = CARTESIAN_POINT ( 'NONE',  ( 9.831596185961002377, -3.539228349258999984, -8.956015611440999891 ) ) ;
#3972 = ORIENTED_EDGE ( 'NONE', *, *, #6609, .F. ) ;
#3973 = ORIENTED_EDGE ( 'NONE', *, *, #10138, .T. ) ;
#3974 = CARTESIAN_POINT ( 'NONE',  ( 9.725595280412999699, 2.495531372253999791, -7.930944806125000746 ) ) ;
#3975 = CARTESIAN_POINT ( 'NONE',  ( 21.00000012402669824, 1.558133232118999877E-13, -6.372680161347999694E-14 ) ) ;
#3976 = CARTESIAN_POINT ( 'NONE',  ( 1.433329478674677082, -2.750000000000000000, 3.881562544924731475E-10 ) ) ;
#3977 = CARTESIAN_POINT ( 'NONE',  ( 25.25776035775700024, 8.562683428954001030, -7.910855114518000164 ) ) ;
#3978 = CARTESIAN_POINT ( 'NONE',  ( 23.58549012003300049, 10.19447453086000088, -9.580977173348999898 ) ) ;
#3979 = CARTESIAN_POINT ( 'NONE',  ( 11.50001496185000249, 12.52500000000000036, 0.000000000000000000 ) ) ;
#3981 = CARTESIAN_POINT ( 'NONE',  ( 8.836073038665773538, 3.765130766121813188, 9.264018223852634293 ) ) ;
#3980 = CARTESIAN_POINT ( 'NONE',  ( 10.58762143724499971, -3.241588663654300095, 8.353549467159899322 ) ) ;
#3983 = PRESENTATION_LAYER_ASSIGNMENT (  '', '', ( #8453 ) ) ;
#3982 = DIRECTION ( 'NONE',  ( 0.000000000000000000, 0.000000000000000000, -1.000000000000000000 ) ) ;
#3984 = ORIENTED_EDGE ( 'NONE', *, *, #36802, .T. ) ;
#3985 = CARTESIAN_POINT ( 'NONE',  ( 9.696013540182335078, 4.999583552997727054, -6.731816600031361730 ) ) ;
#3986 = AXIS2_PLACEMENT_3D ( 'NONE', #21445, #47689, #31268 ) ;
#3987 = CARTESIAN_POINT ( 'NONE',  ( 7.722414202460995192, -2.834216095980001349, 6.826613447391997269 ) ) ;
#3988 = ADVANCED_FACE ( 'NONE', ( #19130 ), #49193, .T. ) ;
#3989 = EDGE_CURVE ( 'NONE', #42529, #68830, #33579, .T. ) ;
#3990 = CARTESIAN_POINT ( 'NONE',  ( 9.756901401888999459, -3.283392111224999965, -8.676955243274001361 ) ) ;
#3991 = CARTESIAN_POINT ( 'NONE',  ( 7.949325904507976936, 5.068739420852621080, 6.584571070534249948 ) ) ;
#3992 = CARTESIAN_POINT ( 'NONE',  ( 9.906851002540999929, -2.832432432432000269, -6.822293592207000934 ) ) ;
#3993 = CARTESIAN_POINT ( 'NONE',  ( 11.04626556088000022, -5.245434002695000153, 5.120146859325999777 ) ) ;
#3994 = CARTESIAN_POINT ( 'NONE',  ( 8.944760841233000193, 4.990139824845000405, -9.121472988377998803 ) ) ;
#3995 = CARTESIAN_POINT ( 'NONE',  ( 13.60249209530700121, 8.943624754334001281, 7.827978252961999672 ) ) ;
#3996 = CARTESIAN_POINT ( 'NONE',  ( 7.921841810112000282, 2.875629839593000003, -6.725486766668000271 ) ) ;
#3997 = VECTOR ( 'NONE', #8481, 1000.000000000000000 ) ;
#3998 = CARTESIAN_POINT ( 'NONE',  ( 6.311630799317000218, -1.121550593885000113, 0.3539842735925000095 ) ) ;
#3999 = VECTOR ( 'NONE', #69141, 1000.000000000000000 ) ;
#4000 = CARTESIAN_POINT ( 'NONE',  ( 18.50003594170800270, 2.686563649653999963, -11.33603604535000109 ) ) ;
#4001 = CARTESIAN_POINT ( 'NONE',  ( 18.50003594167399967, -2.686563651857999613, -11.33603604486000016 ) ) ;
#4002 = EDGE_LOOP ( 'NONE', ( #25993, #15744, #58189, #1192, #7301, #38673, #11330, #41577, #68191, #58539 ) ) ;
#4003 = CARTESIAN_POINT ( 'NONE',  ( 12.37030581721858447, -0.4491390935506887616, -12.68931154995402188 ) ) ;
#4004 = CARTESIAN_POINT ( 'NONE',  ( 12.42192081635679912, -3.001194947154673276, -12.32076077294284566 ) ) ;
#4005 = DIRECTION ( 'NONE',  ( 0.000000000000000000, 0.7455306007789014311, 0.6664713972124013397 ) ) ;
#4006 = DIRECTION ( 'NONE',  ( -1.000000000000000000, 0.000000000000000000, 0.000000000000000000 ) ) ;
#4007 = ORIENTED_EDGE ( 'NONE', *, *, #18487, .T. ) ;
#4008 = CARTESIAN_POINT ( 'NONE',  ( 5.745207029897000162, -0.6440133831468000114, 0.9840870706126000345 ) ) ;
#4009 = PRODUCT_CONTEXT ( 'NONE', #8793, 'mechanical' ) ;
#4010 = EDGE_CURVE ( 'NONE', #23656, #36822, #11896, .T. ) ;
#4011 = CARTESIAN_POINT ( 'NONE',  ( 10.90000000000000036, 2.778483479159999714, -6.925197956411000000 ) ) ;
#4012 = CARTESIAN_POINT ( 'NONE',  ( 9.610944094206999466, -5.100000000000000533, -6.571291218949999902 ) ) ;
#4013 = CARTESIAN_POINT ( 'NONE',  ( 7.806713606405746297, 3.013404723643958061, 6.528857899631486106 ) ) ;
#4014 = CARTESIAN_POINT ( 'NONE',  ( 11.23078751119019891, 3.084247107206000038, -7.979095341142500075 ) ) ;
#4015 = ORIENTED_EDGE ( 'NONE', *, *, #62507, .F. ) ;
#4016 = EDGE_CURVE ( 'NONE', #56617, #36930, #20191, .T. ) ;
#4017 = CARTESIAN_POINT ( 'NONE',  ( 10.70441271436000008, -3.444516450945999786, 6.009051312948000323 ) ) ;
#4018 = ORIENTED_EDGE ( 'NONE', *, *, #20354, .T. ) ;
#4019 = CARTESIAN_POINT ( 'NONE',  ( 9.432978986056474113, -5.350301812018463110, 7.637514618902952357 ) ) ;
#4020 = CARTESIAN_POINT ( 'NONE',  ( 8.085168146793000332, -2.431397064767999439, 7.958394431095000776 ) ) ;
#4021 = CARTESIAN_POINT ( 'NONE',  ( 16.13959992722299930, 8.325816698831998153, 8.094004264449001340 ) ) ;
#4022 = ORIENTED_EDGE ( 'NONE', *, *, #59036, .T. ) ;
#4023 = CARTESIAN_POINT ( 'NONE',  ( 8.613580616166148118, 2.319743054166865992, -6.990328426993228206 ) ) ;
#4024 = CARTESIAN_POINT ( 'NONE',  ( 8.199995020667000034, 2.894508905068999827, 6.645190348705000360 ) ) ;
#4025 = CARTESIAN_POINT ( 'NONE',  ( 7.920870280406000496, 3.504660014889999786, -9.160103207264000957 ) ) ;
#4026 = DIRECTION ( 'NONE',  ( -1.000000000000000000, 0.000000000000000000, 0.000000000000000000 ) ) ;
#4027 = CARTESIAN_POINT ( 'NONE',  ( 12.80505043854146940, -3.248109929747638347, 13.61799478206225444 ) ) ;
#4028 = VERTEX_POINT ( 'NONE', #61363 ) ;
#4029 = CARTESIAN_POINT ( 'NONE',  ( 2.136390132540208597, -0.4581489286485235790, 3.499999999999998224 ) ) ;
#4030 = CARTESIAN_POINT ( 'NONE',  ( 12.18521525456901777, -2.580824918023420622, -13.65593716523674317 ) ) ;
#4031 = CARTESIAN_POINT ( 'NONE',  ( 9.599999931441001166, -2.753634353389999845, 7.595250590283559866 ) ) ;
#4032 = ORIENTED_EDGE ( 'NONE', *, *, #5456, .T. ) ;
#4033 = CARTESIAN_POINT ( 'NONE',  ( 10.21238410957999854, -4.072568653311000375, -8.861841462475000597 ) ) ;
#4034 = CARTESIAN_POINT ( 'NONE',  ( 11.00000000000000000, 5.079754677601000523, 7.174999999999999822 ) ) ;
#4035 = B_SPLINE_CURVE_WITH_KNOTS ( 'NONE', 3,
 ( #6762, #33349, #34046, #28454, #55710, #38582, #49767, #28101, #43837, #65136 ),
 .UNSPECIFIED., .F., .F.,
 ( 4, 2, 2, 2, 4 ),
 ( 0.000000000000000000, 0.2500000000000000000, 0.5000000000000000000, 0.7500000000000000000, 1.000000000000000000 ),
 .UNSPECIFIED. ) ;
#4036 = B_SPLINE_CURVE_WITH_KNOTS ( 'NONE', 3,
 ( #34101, #13470, #2959, #55768, #57127, #50515, #35811, #14150, #51207, #8554, #61689, #40368, #67607, #29902 ),
 .UNSPECIFIED., .F., .F.,
 ( 4, 2, 2, 2, 2, 2, 4 ),
 ( 0.000000000000000000, 0.1249999999999998057, 0.2499999999999996114, 0.4999999999999991673, 0.7499999999999993339, 0.8749999999999997780, 1.000000000000000000 ),
 .UNSPECIFIED. ) ;
#4037 = ORIENTED_EDGE ( 'NONE', *, *, #60012, .F. ) ;
#4038 = CARTESIAN_POINT ( 'NONE',  ( 10.78969997251173929, 4.768152166674551218, 9.097113251175899862 ) ) ;
#4039 = EDGE_CURVE ( 'NONE', #64156, #1476, #52603, .T. ) ;
#4040 = CONICAL_SURFACE ( 'NONE', #35309, 3.186893810805000005, 0.7853950157668545540 ) ;
#4041 = CARTESIAN_POINT ( 'NONE',  ( 5.334193173017583334, 1.460959015002474048, -0.3926218265389178064 ) ) ;
#4042 = CARTESIAN_POINT ( 'NONE',  ( 11.50001258332000020, 11.56502147876000031, 1.404302031979000054 ) ) ;
#4043 = CARTESIAN_POINT ( 'NONE',  ( 5.000000000000000000, -1.199999999999999956, -9.776630298829998011 ) ) ;
#4044 = CARTESIAN_POINT ( 'NONE',  ( 12.36880880067034738, 2.947687262017097964, 13.56819815501604509 ) ) ;
#4045 = CARTESIAN_POINT ( 'NONE',  ( 17.97023714413482764, -2.032719534845758069, 12.54827100236067494 ) ) ;
#4046 = VERTEX_POINT ( 'NONE', #20085 ) ;
#4047 = CARTESIAN_POINT ( 'NONE',  ( 10.90346005378009941, -3.213042707518099839, -7.079777642108599167 ) ) ;
#4048 = ORIENTED_EDGE ( 'NONE', *, *, #54921, .F. ) ;
#4049 = CARTESIAN_POINT ( 'NONE',  ( 9.423523952092001110, 4.993991073313000406, 8.578107851305000864 ) ) ;
#4050 = B_SPLINE_CURVE_WITH_KNOTS ( 'NONE', 3,
 ( #57284, #986, #64932, #1670, #28241, #55152, #49558, #17405, #65289, #38730, #64593, #33146, #17759, #43982, #48186, #48879, #6211, #42940 ),
 .UNSPECIFIED., .F., .F.,
 ( 4, 2, 2, 2, 2, 2, 2, 2, 4 ),
 ( 0.000000000000000000, 0.1250000000000000000, 0.2500000000000000000, 0.3750000000000000000, 0.5000000000000000000, 0.6250000000000000000, 0.7500000000000000000, 0.8750000000000000000, 1.000000000000000000 ),
 .UNSPECIFIED. ) ;
#4051 = CARTESIAN_POINT ( 'NONE',  ( 11.16544712921906957, -4.732401051283384952, -7.982093405445620959 ) ) ;
#4052 = AXIS2_PLACEMENT_3D ( 'NONE', #52385, #30389, #51699 ) ;
#4053 = CARTESIAN_POINT ( 'NONE',  ( 12.64132288496826639, 1.896477787946245774, -13.78309086827116658 ) ) ;
#4054 = CARTESIAN_POINT ( 'NONE',  ( 2.426081430536000116, 3.527224658283000025, -0.3417833995711000439 ) ) ;
#4055 = CARTESIAN_POINT ( 'NONE',  ( 10.19715077290999972, -4.982624057277000418, -6.124316828241999744 ) ) ;
#4056 = CARTESIAN_POINT ( 'NONE',  ( 15.89994436294300151, -8.847904542234999781, -8.580301953175000662 ) ) ;
#4057 = CARTESIAN_POINT ( 'NONE',  ( 9.039803704978325527, -4.929474118734117560, 8.478877421443728579 ) ) ;
#4058 = ORIENTED_EDGE ( 'NONE', *, *, #39003, .T. ) ;
#4059 = CARTESIAN_POINT ( 'NONE',  ( 11.61302897915239818, -3.708003626182200030, 6.397263297997000109 ) ) ;
#4060 = CARTESIAN_POINT ( 'NONE',  ( 3.061390132544625775, 3.499999999999999112, 0.4581489286485193602 ) ) ;
#4061 = B_SPLINE_CURVE_WITH_KNOTS ( 'NONE', 3,
 ( #22470, #49388, #49741, #1158, #17234 ),
 .UNSPECIFIED., .F., .F.,
 ( 4, 1, 4 ),
 ( 0.000000000000000000, 0.5000000000000000000, 1.000000000000000000 ),
 .UNSPECIFIED. ) ;
#4062 = B_SPLINE_CURVE_WITH_KNOTS ( 'NONE', 3,
 ( #43964, #60033, #18082, #48511 ),
 .UNSPECIFIED., .F., .F.,
 ( 4, 4 ),
 ( 0.000000000000000000, 1.000000000000000000 ),
 .UNSPECIFIED. ) ;
#4063 = CARTESIAN_POINT ( 'NONE',  ( 15.95309301929700219, 8.865091978629999758, 8.639514276306002216 ) ) ;
#4064 = CARTESIAN_POINT ( 'NONE',  ( 18.29983863915590447, 1.925365965127968426, -12.21183828433472307 ) ) ;
#4066 = CARTESIAN_POINT ( 'NONE',  ( 23.56666365135700403, -2.920993777382001166, -11.72568747150000412 ) ) ;
#4065 = CARTESIAN_POINT ( 'NONE',  ( 10.83668832355999889, 4.288537082977999404, 9.448742031664000507 ) ) ;
#4067 = CARTESIAN_POINT ( 'NONE',  ( 11.38379707368349969, 3.433355370490100533, -6.509947486183500054 ) ) ;
#4068 = CARTESIAN_POINT ( 'NONE',  ( 10.76947109217999810, -5.100000000000000533, -6.152188490330000370 ) ) ;
#4069 = CARTESIAN_POINT ( 'NONE',  ( 10.26090035061499961, 4.231093494672100164, -8.335645555860798694 ) ) ;
#4070 = EDGE_CURVE ( 'NONE', #44229, #51258, #40720, .T. ) ;
#4071 = EDGE_CURVE ( 'NONE', #59692, #48385, #36506, .T. ) ;
#4072 = CARTESIAN_POINT ( 'NONE',  ( 17.99694387276892371, 0.5707228546306919448, 12.58707662888204304 ) ) ;
#4073 = CARTESIAN_POINT ( 'NONE',  ( 7.027657817496000270, 1.230545047785000179, 0.3267465519018999953 ) ) ;
#4074 = CARTESIAN_POINT ( 'NONE',  ( 11.76077869730539938, 3.404661623424200201, 8.673950353177000139 ) ) ;
#4075 = DIRECTION ( 'NONE',  ( 1.000000000000000000, 0.000000000000000000, 0.000000000000000000 ) ) ;
#4076 = ORIENTED_EDGE ( 'NONE', *, *, #57743, .T. ) ;
#4077 = CARTESIAN_POINT ( 'NONE',  ( 7.871558059623000148, -4.780993534312999671, 6.267212032957000467 ) ) ;
#4078 = EDGE_CURVE ( 'NONE', #45774, #15974, #26889, .T. ) ;
#4079 = EDGE_CURVE ( 'NONE', #56837, #129, #30249, .T. ) ;
#4080 = CARTESIAN_POINT ( 'NONE',  ( 17.72083032727074681, 3.229203862303413608, 13.62249117442681978 ) ) ;
#4081 = CARTESIAN_POINT ( 'NONE',  ( 8.666729817973333638, 2.899999999999999911, 6.535479089440332956 ) ) ;
#4082 = ORIENTED_EDGE ( 'NONE', *, *, #11426, .T. ) ;
#4083 = AXIS2_PLACEMENT_3D ( 'NONE', #52972, #46702, #5069 ) ;
#4084 = CARTESIAN_POINT ( 'NONE',  ( 0.1785675383994000109, -1.568133397559999809, -2.874292603119999789 ) ) ;
#4085 = AXIS2_PLACEMENT_3D ( 'NONE', #36814, #15140, #63010 ) ;
#4086 = CARTESIAN_POINT ( 'NONE',  ( 10.76346886766499900, 3.365322927604099679, 8.653146038559000885 ) ) ;
#4087 = CARTESIAN_POINT ( 'NONE',  ( 10.13035471959000056, 2.409325917207000511, -8.058043919563999680 ) ) ;
#4088 = ORIENTED_EDGE ( 'NONE', *, *, #51445, .F. ) ;
#4089 = CARTESIAN_POINT ( 'NONE',  ( 1.311390132540666498, -3.500000000000000888, -0.4581489286485119217 ) ) ;
#4090 = CARTESIAN_POINT ( 'NONE',  ( 9.210982939512550871, -5.015527360726283135, -6.211259001266990154 ) ) ;
#4091 = CARTESIAN_POINT ( 'NONE',  ( 11.15810538575740019, 5.242981041160000188, 7.797177576385699638 ) ) ;
#4092 = CARTESIAN_POINT ( 'NONE',  ( 7.954503319898948988, -5.004866943022359571, 6.489198313767416515 ) ) ;
#4094 = CARTESIAN_POINT ( 'NONE',  ( 10.90000000042000039, -0.3000000004212000082, -9.662944680462999258 ) ) ;
#4093 = AXIS2_PLACEMENT_3D ( 'NONE', #7811, #34049, #2228 ) ;
#4095 = ORIENTED_EDGE ( 'NONE', *, *, #40021, .T. ) ;
#4096 = CARTESIAN_POINT ( 'NONE',  ( 11.44731512799000228, -3.899625435828999898, 11.84583327264999930 ) ) ;
#4097 = CARTESIAN_POINT ( 'NONE',  ( 15.83979990366733048, 8.664995957719213493, 8.086229679809639137 ) ) ;
#4098 = CARTESIAN_POINT ( 'NONE',  ( 8.218406721992218777, -5.687944966856361972, 7.919044992995649679 ) ) ;
#4099 = AXIS2_PLACEMENT_3D ( 'NONE', #53786, #37027, #42954 ) ;
#4100 = CARTESIAN_POINT ( 'NONE',  ( 9.077265421554999492, -4.214287043487900064, 6.391527115138999626 ) ) ;
#4101 = ORIENTED_EDGE ( 'NONE', *, *, #32928, .T. ) ;
#4102 = CARTESIAN_POINT ( 'NONE',  ( 9.225602416349406809, -4.497379437544680947, 9.030677449726647765 ) ) ;
#4103 = CARTESIAN_POINT ( 'NONE',  ( 10.82118582084300051, -4.836160649475099937, 8.466515260542900378 ) ) ;
#4104 = VERTEX_POINT ( 'NONE', #35824 ) ;
#4105 = DIRECTION ( 'NONE',  ( 0.000000000000000000, 1.000000000000000000, 0.000000000000000000 ) ) ;
#4106 = ORIENTED_EDGE ( 'NONE', *, *, #23832, .F. ) ;
#4107 = CARTESIAN_POINT ( 'NONE',  ( 0.1869138731963999878, 0.000000000000000000, 0.000000000000000000 ) ) ;
#4108 = CARTESIAN_POINT ( 'NONE',  ( 9.269471092183000138, 5.100000000000000533, -6.152188490330000370 ) ) ;
#4109 = CARTESIAN_POINT ( 'NONE',  ( 10.60235971519489873, 4.605301262871499546, -6.493038401303000029 ) ) ;
#4110 = CARTESIAN_POINT ( 'NONE',  ( 12.14122412107036908, -3.937930136014310190, 8.673243607771999208 ) ) ;
#4111 = CARTESIAN_POINT ( 'NONE',  ( 12.19547854351943705, 2.361608046327442700, -12.48276200957625548 ) ) ;
#4112 = CARTESIAN_POINT ( 'NONE',  ( 11.56379841651039975, -4.401637675674300532, 6.432302808027999141 ) ) ;
#4113 = CARTESIAN_POINT ( 'NONE',  ( 7.731795280408999993, 4.580608786027000612, 9.213365309690999538 ) ) ;
#4114 = ORIENTED_EDGE ( 'NONE', *, *, #706, .T. ) ;
#4115 = CARTESIAN_POINT ( 'NONE',  ( 10.82894633243952498, 2.649868422364484388, -7.263390030261542840 ) ) ;
#4116 = CARTESIAN_POINT ( 'NONE',  ( 17.74278939942546174, -0.6963438834338713246, 12.58074676375308165 ) ) ;
#4117 = DIRECTION ( 'NONE',  ( 0.000000000000000000, 1.000000000000000000, 1.181194577550999990E-14 ) ) ;
#4118 = EDGE_LOOP ( 'NONE', ( #34580, #19431, #37509 ) ) ;
#4119 = CARTESIAN_POINT ( 'NONE',  ( 12.57326805540222914, -3.080523641713202476, -12.29716358636311213 ) ) ;
#4120 = CARTESIAN_POINT ( 'NONE',  ( 10.27610941423800028, 4.844410192686099847, 8.266982106121901097 ) ) ;
#4121 = EDGE_CURVE ( 'NONE', #54494, #17499, #32708, .T. ) ;
#4122 = CARTESIAN_POINT ( 'NONE',  ( 10.82674314678999927, -3.167157901876000103, -6.225148200207000215 ) ) ;
#4123 = CARTESIAN_POINT ( 'NONE',  ( 9.365000000002998704, -2.649999999999999911, -7.500000000000000000 ) ) ;
#4124 = CARTESIAN_POINT ( 'NONE',  ( 18.26122879894100137, -2.828234032943000020, -11.95647652451000020 ) ) ;
#4125 = CARTESIAN_POINT ( 'NONE',  ( 23.66004879239100234, -13.39256464007999980, -3.813546745462999876 ) ) ;
#4126 = CARTESIAN_POINT ( 'NONE',  ( 12.48178274919588482, -3.171647819517037892, -13.63600670097294021 ) ) ;
#4127 = ADVANCED_FACE ( 'NONE', ( #46666 ), #62627, .T. ) ;
#4128 = CARTESIAN_POINT ( 'NONE',  ( 10.38287885159599888, -3.139900861731399928, -7.397393329751199786 ) ) ;
#4129 = CARTESIAN_POINT ( 'NONE',  ( 11.09999999999999964, -0.5000000000000000000, -5.124965750789000296 ) ) ;
#4130 = CARTESIAN_POINT ( 'NONE',  ( 8.542969685731069518, -5.075224516770981076, 6.339907061512210618 ) ) ;
#4131 = ORIENTED_EDGE ( 'NONE', *, *, #59428, .T. ) ;
#4132 = ORIENTED_EDGE ( 'NONE', *, *, #55235, .F. ) ;
#4133 = CARTESIAN_POINT ( 'NONE',  ( 12.70736722663045448, -0.7301396911442795679, -13.98094760870049491 ) ) ;
#4134 = VECTOR ( 'NONE', #15601, 1000.000000000000000 ) ;
#4135 = CARTESIAN_POINT ( 'NONE',  ( 8.099999999999999645, 0.000000000000000000, 0.000000000000000000 ) ) ;
#4136 = CARTESIAN_POINT ( 'NONE',  ( 17.81484293442183997, 3.068795199393538287, 13.53617370486282923 ) ) ;
#4137 = CARTESIAN_POINT ( 'NONE',  ( 10.66852712374000056, 4.435471808682999395, -5.866466547508000673 ) ) ;
#4138 = CARTESIAN_POINT ( 'NONE',  ( 8.678237328909947479, 5.064959164704544214, 6.230262016040554407 ) ) ;
#4139 = STYLED_ITEM ( 'NONE', ( #51441 ), #43565 ) ;
#4140 = CARTESIAN_POINT ( 'NONE',  ( 18.17480529351244201, 2.583342416263719077, 12.43177882285067781 ) ) ;
#4141 = CARTESIAN_POINT ( 'NONE',  ( 18.23043922992600230, 3.518658233831999826, -12.06062508533999988 ) ) ;
#4142 = CARTESIAN_POINT ( 'NONE',  ( 9.385781899350000401, 4.980865465981000106, 6.433345686594999613 ) ) ;
#4143 = ORIENTED_EDGE ( 'NONE', *, *, #11505, .T. ) ;
#4144 = CIRCLE ( 'NONE', #37634, 12.50000000000000178 ) ;
#4145 = CARTESIAN_POINT ( 'NONE',  ( 9.045397103852565124, 2.494519796715142235, -8.441659411582618233 ) ) ;
#4146 = EDGE_LOOP ( 'NONE', ( #22610, #46769, #68896, #11093 ) ) ;
#4147 = CARTESIAN_POINT ( 'NONE',  ( 12.54002611783806387, -3.066051210233500690, 12.30150130090889427 ) ) ;
#4148 = CARTESIAN_POINT ( 'NONE',  ( 9.425038493598998812, -3.372531419565699906, -6.901676404381399621 ) ) ;
#4149 = CARTESIAN_POINT ( 'NONE',  ( 10.13339736671999880, 5.653645990693000556, 6.501823474484000442 ) ) ;
#4150 = CARTESIAN_POINT ( 'NONE',  ( 11.96989666366029859, -4.058428102321880004, 6.185029684353999357 ) ) ;
#4151 = CARTESIAN_POINT ( 'NONE',  ( 7.178932123752673533, 1.128209471082204374, 0.5373459335455109676 ) ) ;
#4152 = CARTESIAN_POINT ( 'NONE',  ( 10.96261281413999988, 7.423575154918000685, -6.118088960612000804 ) ) ;
#4153 = CARTESIAN_POINT ( 'NONE',  ( 10.81349144726329925, 3.261052100888700345, -6.457276458983999490 ) ) ;
#4154 = CARTESIAN_POINT ( 'NONE',  ( 12.75354487906747991, -0.6229596466635322072, 12.67942438339646571 ) ) ;
#4155 = CARTESIAN_POINT ( 'NONE',  ( 11.59999999999999964, 3.116215992411100366, -7.825000000000000178 ) ) ;
#4156 = EDGE_CURVE ( 'NONE', #62789, #21338, #9935, .T. ) ;
#4157 = CARTESIAN_POINT ( 'NONE',  ( 11.02786554143000153, 5.596226216413000110, 7.209502215883999199 ) ) ;
#4158 = AXIS2_PLACEMENT_3D ( 'NONE', #8165, #60009, #18995 ) ;
#4159 = CARTESIAN_POINT ( 'NONE',  ( 9.225036374688860619, -2.649952446100997339, 7.500002253091946791 ) ) ;
#4160 = VERTEX_POINT ( 'NONE', #42103 ) ;
#4161 = CARTESIAN_POINT ( 'NONE',  ( 8.780820280412001466, 2.567871051582000241, -6.869011921437000012 ) ) ;
#4162 = CARTESIAN_POINT ( 'NONE',  ( 10.98768491210000064, -8.067891622241001315, 6.818837029638999958 ) ) ;
#4163 = EDGE_CURVE ( 'NONE', #63599, #49185, #68654, .T. ) ;
#4164 = ADVANCED_FACE ( 'NONE', ( #56465 ), #15532, .T. ) ;
#4165 = DIRECTION ( 'NONE',  ( 0.000000000000000000, 1.000000000000000000, 0.000000000000000000 ) ) ;
#4166 = CARTESIAN_POINT ( 'NONE',  ( 17.55505043854143565, 1.760845406083394682, -12.47635457398814829 ) ) ;
#4167 = CARTESIAN_POINT ( 'NONE',  ( 5.555026506349999948, -1.500000000000000000, 0.000000000000000000 ) ) ;
#4168 = CARTESIAN_POINT ( 'NONE',  ( 10.74795391537419853, -3.169881940022800215, -8.063786182297898009 ) ) ;
#4169 = ORIENTED_EDGE ( 'NONE', *, *, #52791, .F. ) ;
#4170 = B_SPLINE_CURVE_WITH_KNOTS ( 'NONE', 3,
 ( #39781, #45374, #66334, #28608, #40132, #67024, #55164, #60414, #55860, #56542, #65647, #39089, #19133, #7966, #66681, #50268, #12519, #49920, #2033, #18114, #23351, #35230, #61445 ),
 .UNSPECIFIED., .F., .F.,
 ( 4, 2, 2, 2, 1, 2, 2, 2, 2, 2, 2, 4 ),
 ( 0.000000000000000000, 0.1250000000000140721, 0.1875000000000225653, 0.2187500000000262845, 0.2343750000000250355, 0.2421875000000237033, 0.2500000000000223710, 0.3750000000000177636, 0.4375000000000164313, 0.5000000000000150990, 0.7500000000000075495, 1.000000000000000000 ),
 .UNSPECIFIED. ) ;
#4171 = CARTESIAN_POINT ( 'NONE',  ( 2.344930008642999830, -2.375092696518000146, -2.913277015014000160 ) ) ;
#4172 = CARTESIAN_POINT ( 'NONE',  ( 7.373073341229000377, 3.394842219570000097, 9.388954446285000088 ) ) ;
#4174 = DIRECTION ( 'NONE',  ( -1.000000000000000000, 0.000000000000000000, 3.552713678903000467E-14 ) ) ;
#4173 = CARTESIAN_POINT ( 'NONE',  ( 8.225464158772000545, 3.844886277615000125, -8.888911790991000927 ) ) ;
#4175 = CARTESIAN_POINT ( 'NONE',  ( 18.13153191400934716, -2.741475808281053972, 13.61927240699122876 ) ) ;
#4176 = ORIENTED_EDGE ( 'NONE', *, *, #2665, .F. ) ;
#4177 = CARTESIAN_POINT ( 'NONE',  ( 0.7000000000000000666, 1.154700538379000108, 0.000000000000000000 ) ) ;
#4178 = CARTESIAN_POINT ( 'NONE',  ( 17.84240044433953543, -3.055120806185296800, -13.53986419860029322 ) ) ;
#4179 = CARTESIAN_POINT ( 'NONE',  ( 11.41672066707849886, 4.741156262620799922, 7.948314604624900248 ) ) ;
#4180 = CARTESIAN_POINT ( 'NONE',  ( 24.65661251414474009, -11.83370281768760002, 3.192273988792572403 ) ) ;
#4181 = CARTESIAN_POINT ( 'NONE',  ( 7.565629440376999248, -3.206365290996999740, 5.681739161071000410 ) ) ;
#4182 = VERTEX_POINT ( 'NONE', #30580 ) ;
#4183 = CARTESIAN_POINT ( 'NONE',  ( 8.545864158774001851, 3.856772556595000179, 5.521246073317000125 ) ) ;
#4184 = EDGE_CURVE ( 'NONE', #7152, #18020, #29174, .T. ) ;
#4186 = CARTESIAN_POINT ( 'NONE',  ( 24.63002439619599926, 0.000000000000000000, 0.000000000000000000 ) ) ;
#4185 = CARTESIAN_POINT ( 'NONE',  ( 10.52606775832647656, 3.656473597603909553, -6.696209471835564919 ) ) ;
#4187 = B_SPLINE_CURVE_WITH_KNOTS ( 'NONE', 3,
 ( #62360, #24274, #35797, #25644, #30550, #8883, #14479, #57447, #4310, #46637, #56784, #8536 ),
 .UNSPECIFIED., .F., .F.,
 ( 4, 2, 2, 2, 2, 4 ),
 ( 0.000000000000000000, 0.2500000000000000555, 0.3750000000000001110, 0.5000000000000001110, 0.7500000000000000000, 1.000000000000000000 ),
 .UNSPECIFIED. ) ;
#4188 = CARTESIAN_POINT ( 'NONE',  ( 7.526976851188666551, -3.029433660751889690, 6.048151158366446900 ) ) ;
#4189 = FACE_OUTER_BOUND ( 'NONE', #4146, .T. ) ;
#4190 = CARTESIAN_POINT ( 'NONE',  ( 1.414247443154999839, -3.006852806188000216, -1.965371480138999871 ) ) ;
#4191 = ORIENTED_EDGE ( 'NONE', *, *, #67942, .T. ) ;
#4192 = CARTESIAN_POINT ( 'NONE',  ( 2.049278142419042936, -3.167119488121065807, -0.9369383795961846451 ) ) ;
#4193 = CARTESIAN_POINT ( 'NONE',  ( 12.25718044953559982, -3.110233631466100324, 7.036033215662999218 ) ) ;
#4194 = CARTESIAN_POINT ( 'NONE',  ( 11.50962052873067520, 3.830320465062102109, 8.360247930805771333 ) ) ;
#4195 = CARTESIAN_POINT ( 'NONE',  ( 10.69030645188999884, 5.903031974240000146, 7.830710565751001440 ) ) ;
#4196 = PRESENTATION_LAYER_ASSIGNMENT (  '', '', ( #34362 ) ) ;
#4197 = CARTESIAN_POINT ( 'NONE',  ( 10.37872469555899890, 4.502158848185001006, 8.368784980615899372 ) ) ;
#4198 = CARTESIAN_POINT ( 'NONE',  ( 24.13557959378723794, -3.329020217945502846, 12.49973103956492082 ) ) ;
#4199 = AXIS2_PLACEMENT_3D ( 'NONE', #14506, #41415, #14844 ) ;
#4200 = CARTESIAN_POINT ( 'NONE',  ( 24.30000000000000071, 12.03537377768999939, -3.224868684338999980 ) ) ;
#4201 = CARTESIAN_POINT ( 'NONE',  ( 11.18220574173929904, 5.136173005413447790, -6.911917091190550089 ) ) ;
#4202 = CARTESIAN_POINT ( 'NONE',  ( 8.610875063856999745, 4.757997781751000410, 5.934102420827000124 ) ) ;
#4203 = VECTOR ( 'NONE', #68937, 1000.000000000000227 ) ;
#4204 = CARTESIAN_POINT ( 'NONE',  ( 24.63626627244600087, -12.49727471743999985, -2.949030056809999856 ) ) ;
#4205 = CARTESIAN_POINT ( 'NONE',  ( 17.55505043854144276, 0.6250000000000001110, 12.67928921589117586 ) ) ;
#4206 = ORIENTED_EDGE ( 'NONE', *, *, #24704, .T. ) ;
#4207 = CARTESIAN_POINT ( 'NONE',  ( 15.44552286930127494, -9.471974105402734878, -8.194957690431824204 ) ) ;
#4208 = DIRECTION ( 'NONE',  ( 1.000000000000000000, 0.000000000000000000, 0.000000000000000000 ) ) ;
#4209 = EDGE_LOOP ( 'NONE', ( #39408, #68302, #28412, #30210 ) ) ;
#4210 =( NAMED_UNIT ( * ) PLANE_ANGLE_UNIT ( ) SI_UNIT ( $, .RADIAN. ) );
#4211 = CARTESIAN_POINT ( 'NONE',  ( 10.70287750876920008, 3.530799696887600092, 6.771886227364699806 ) ) ;
#4212 = CARTESIAN_POINT ( 'NONE',  ( 9.290193290418001126, 2.377818438998999806, 7.540992072119000689 ) ) ;
#4213 = CARTESIAN_POINT ( 'NONE',  ( 9.988718791410999387, 2.842026940133999702, -6.504333051298999635 ) ) ;
#4214 = CARTESIAN_POINT ( 'NONE',  ( 10.16407857760462718, -4.737836169116369511, -7.970244675898661590 ) ) ;
#4215 = CARTESIAN_POINT ( 'NONE',  ( 9.532671748231999587, -4.663050389319001177, 8.669823109968998409 ) ) ;
#4216 = CARTESIAN_POINT ( 'NONE',  ( 18.25212943717077252, 0.1980440493285416381, -12.59844852634975254 ) ) ;
#4217 = CIRCLE ( 'NONE', #52224, 1.250000000000000000 ) ;
#4218 = EDGE_CURVE ( 'NONE', #44139, #60354, #12645, .T. ) ;
#4219 = CARTESIAN_POINT ( 'NONE',  ( 9.016029693782781962, 5.181541736818266131, 8.155019048524399849 ) ) ;
#4220 = CARTESIAN_POINT ( 'NONE',  ( 11.75718044953559804, -3.110233631466100324, -7.963966784336999005 ) ) ;
#4221 = CARTESIAN_POINT ( 'NONE',  ( 7.062379262093081422, 0.1858842090091465671, 1.343634368969766957 ) ) ;
#4222 = ORIENTED_EDGE ( 'NONE', *, *, #60750, .F. ) ;
#4223 = DIRECTION ( 'NONE',  ( 0.000000000000000000, -0.9659258262890756397, 0.2588190451024934280 ) ) ;
#4224 = CARTESIAN_POINT ( 'NONE',  ( 11.09999999999999964, -4.000000000000000000, -7.500000000000000000 ) ) ;
#4225 = CARTESIAN_POINT ( 'NONE',  ( 5.399999746777999654, 0.000000000000000000, 0.000000000000000000 ) ) ;
#4226 = CARTESIAN_POINT ( 'NONE',  ( 10.25851354018279160, -3.836375382625526687, -6.250000000000000888 ) ) ;
#4227 = CARTESIAN_POINT ( 'NONE',  ( 17.94097423839751926, 1.871151600931000081, 12.46029012432409289 ) ) ;
#4228 = CARTESIAN_POINT ( 'NONE',  ( 12.18844676753244727, 2.902714632704711750, 13.69578956119810442 ) ) ;
#4229 = CARTESIAN_POINT ( 'NONE',  ( 11.00366278039000001, -2.264082614160999984, 7.798350693290999835 ) ) ;
#4230 = ORIENTED_EDGE ( 'NONE', *, *, #43970, .T. ) ;
#4231 = CARTESIAN_POINT ( 'NONE',  ( 9.266851002542999538, -2.832432432432000269, 6.822293592207000934 ) ) ;
#4232 = CARTESIAN_POINT ( 'NONE',  ( 12.27567203567527621, -0.4994936913945440815, 13.99109680828866509 ) ) ;
#4233 = ORIENTED_EDGE ( 'NONE', *, *, #31453, .T. ) ;
#4234 = CARTESIAN_POINT ( 'NONE',  ( 24.44916829770000177, 8.894890565782000991, 9.199951775352998240 ) ) ;
#4235 = CARTESIAN_POINT ( 'NONE',  ( 24.30000000000000071, 50.50083396221999976, 14.25635100356000073 ) ) ;
#4236 = CARTESIAN_POINT ( 'NONE',  ( 9.910792656537999790, -3.869344906782000049, 5.882544796414999944 ) ) ;
#4237 = CARTESIAN_POINT ( 'NONE',  ( 9.307788144226000426, -3.909067355573210278, 6.546538158064899804 ) ) ;
#4238 = CARTESIAN_POINT ( 'NONE',  ( 11.86749010443640096, -3.136214309321499805, 7.435402237490909449 ) ) ;
#4239 = CARTESIAN_POINT ( 'NONE',  ( 24.34832116925733203, -12.03536991270508061, -3.224867648718668267 ) ) ;
#4240 = CARTESIAN_POINT ( 'NONE',  ( 0.4089629568059000020, 0.6171034757514999303, 3.149659041885999766 ) ) ;
#4241 = CARTESIAN_POINT ( 'NONE',  ( 9.599999931441001166, -2.753634353389999845, 7.595250590283559866 ) ) ;
#4242 = AXIS2_PLACEMENT_3D ( 'NONE', #44518, #28428, #48710 ) ;
#4243 = CARTESIAN_POINT ( 'NONE',  ( 12.11673986888014376, 2.253747544392081803, 12.39680392560332045 ) ) ;
#4244 = CARTESIAN_POINT ( 'NONE',  ( 11.09999999999999964, 2.700230688341999752, -5.136744347299999625 ) ) ;
#4245 = CARTESIAN_POINT ( 'NONE',  ( 11.43718179236249988, 3.790319673775199849, -6.518682001772900136 ) ) ;
#4246 = CARTESIAN_POINT ( 'NONE',  ( 17.55505043854144276, -0.6250000000000001110, 13.88107975066923494 ) ) ;
#4247 = EDGE_CURVE ( 'NONE', #10847, #13445, #3650, .T. ) ;
#4248 = EDGE_CURVE ( 'NONE', #11948, #21230, #53509, .T. ) ;
#4249 = CARTESIAN_POINT ( 'NONE',  ( 10.92546721959000067, 5.641524285727999910, -7.883474821562000301 ) ) ;
#4250 = CARTESIAN_POINT ( 'NONE',  ( 8.693455549952998851, 4.995562869655000071, -6.696732323226999739 ) ) ;
#4252 = CARTESIAN_POINT ( 'NONE',  ( 12.33152592722388796, 2.090072125033849204, 12.53771354783954983 ) ) ;
#4251 = CARTESIAN_POINT ( 'NONE',  ( 18.30000103245939158, -11.66744832144745203, 3.971921730545766138 ) ) ;
#4253 = CARTESIAN_POINT ( 'NONE',  ( 11.30000000000000071, -12.07633875558669345, -1.479860865542806714 ) ) ;
#4254 = ORIENTED_EDGE ( 'NONE', *, *, #58869, .F. ) ;
#4255 = AXIS2_PLACEMENT_3D ( 'NONE', #46942, #3587, #4279 ) ;
#4256 = CARTESIAN_POINT ( 'NONE',  ( 12.78475401288254432, -0.6250000000000006661, 12.67928921589117408 ) ) ;
#4257 = CARTESIAN_POINT ( 'NONE',  ( 9.129428851719998406, 5.099284414202999827, 6.151604790022999758 ) ) ;
#4258 = LINE ( 'NONE', #15104, #40753 ) ;
#4259 = CARTESIAN_POINT ( 'NONE',  ( 9.224417874593999755, 3.075647715286899953, 7.107043063332000088 ) ) ;
#4260 = CARTESIAN_POINT ( 'NONE',  ( 8.751496707488000126, 4.081676005979390176, -8.356402621895700378 ) ) ;
#4261 = CIRCLE ( 'NONE', #48889, 12.52500000000000036 ) ;
#4262 = CARTESIAN_POINT ( 'NONE',  ( 11.36663360327350070, 3.844887449686455572, -11.78015558627826920 ) ) ;
#4263 = CARTESIAN_POINT ( 'NONE',  ( 12.66212950609382126, -3.108785237067038576, 13.52531707329824684 ) ) ;
#4264 = CARTESIAN_POINT ( 'NONE',  ( 12.23606299695415878, 2.758663578173562669, 13.61513466668993466 ) ) ;
#4265 = CARTESIAN_POINT ( 'NONE',  ( 23.64080852780499953, 3.067619660802999970, -13.45636821867999977 ) ) ;
#4266 = VERTEX_POINT ( 'NONE', #67971 ) ;
#4267 = EDGE_CURVE ( 'NONE', #45407, #63209, #33449, .T. ) ;
#4268 = CARTESIAN_POINT ( 'NONE',  ( 5.116422932093001030, 1.142727098684000131, -0.5665245414306999683 ) ) ;
#4269 = CARTESIAN_POINT ( 'NONE',  ( 9.073392757686999488, -3.136549968260000210, -8.443842375698499936 ) ) ;
#4270 = CARTESIAN_POINT ( 'NONE',  ( 10.55878694030978338, -4.980312522622296179, -5.017513730241772052 ) ) ;
#4271 = CARTESIAN_POINT ( 'NONE',  ( 11.52812378248509795, -4.416893162838900544, 8.288725998710999576 ) ) ;
#4272 = ADVANCED_FACE ( 'NONE', ( #63753 ), #34760, .F. ) ;
#4273 = CARTESIAN_POINT ( 'NONE',  ( 18.17639191339633697, 2.431702999347771676, -12.46724561074273296 ) ) ;
#4274 = CARTESIAN_POINT ( 'NONE',  ( 2.678056799209334482, -2.150913519912214245, 2.798833948393621984 ) ) ;
#4275 = CARTESIAN_POINT ( 'NONE',  ( 18.13163533202872557, 2.741228481653361637, 12.39208274281023847 ) ) ;
#4276 = CARTESIAN_POINT ( 'NONE',  ( 12.72306420252682280, 3.125000000000000000, -13.52084465375510014 ) ) ;
#4277 = CARTESIAN_POINT ( 'NONE',  ( 4.600000207916445483, 2.033928581112999763E-13, 13.27499874715509698 ) ) ;
#4278 = CARTESIAN_POINT ( 'NONE',  ( 10.45625805961999966, -3.661873208228000109, -9.317463915629002003 ) ) ;
#4279 = DIRECTION ( 'NONE',  ( 0.000000000000000000, 1.000000000000000000, 0.000000000000000000 ) ) ;
#4280 = B_SPLINE_CURVE_WITH_KNOTS ( 'NONE', 3,
 ( #51771, #57698, #9808, #25203, #3196, #14721, #68527, #4214, #3869, #56340, #46538, #67503, #67844, #62597, #52459, #62263, #19620, #25895, #19966, #9121, #40942, #24523, #61580, #14384, #51432, #36036, #20303, #31157, #52111, #57352, #41629, #62935, #3529, #47224, #20649, #45848, #8785, #30129, #13696, #9456, #68185, #30459, #30798, #15059, #14038, #51093, #25552, #19269, #46877, #24864, #36382, #40598, #4554, #61923, #56686, #35704, #57021, #26244, #58055, #5253, #37077, #21666, #26591, #10158, #58388 ),
 .UNSPECIFIED., .F., .F.,
 ( 4, 1, 1, 1, 1, 1, 1, 1, 1, 1, 1, 1, 1, 1, 1, 1, 1, 1, 1, 1, 1, 1, 1, 1, 1, 1, 1, 1, 1, 1, 1, 1, 1, 1, 1, 1, 1, 1, 1, 1, 1, 1, 1, 1, 1, 1, 1, 1, 1, 1, 1, 1, 1, 1, 1, 1, 1, 1, 1, 1, 1, 1, 4 ),
 ( 0.000000000000000000, 0.01249986222369742044, 0.02874986775682986107, 0.04499987328996229996, 0.06124987882309473886, 0.07749988435622719163, 0.09374988988935963052, 0.1099998954224920694, 0.1262499009556244944, 0.1424999064887569333, 0.1587499120218893722, 0.1749999175550218111, 0.1912499230881542500, 0.2074999286212866889, 0.2237499341544191278, 0.2399999396875515667, 0.2562499452206840056, 0.2724999507538165000, 0.2887499562869489389, 0.3049999618200813778, 0.3212499673532137612, 0.3374999728863462556, 0.3537499784194786945, 0.3699999839526111334, 0.3862499894857435723, 0.4024999950188760112, 0.4187500005520084501, 0.4350000060851408890, 0.4512500116182733279, 0.4675000171514058223, 0.4837500226845382056, 0.5000000282176706445, 0.5162500337508030279, 0.5325000392839354113, 0.5487500448170679057, 0.5650000503502002891, 0.5812500558833328945, 0.5975000614164652779, 0.6137500669495976613, 0.6300000724827301557, 0.6462500780158625391, 0.6625000835489949225, 0.6787500890821274169, 0.6950000946152598003, 0.7112501001483924057, 0.7275001056815247891, 0.7437501112146571725, 0.7600001167477896669, 0.7762501222809220502, 0.7925001278140545447, 0.8087501333471869280, 0.8250001388803193114, 0.8412501444134519168, 0.8575001499465843002, 0.8737501554797167946, 0.8900001610128491780, 0.9062501665459815614, 0.9225001720791140558, 0.9387501776122464392, 0.9550001831453789336, 0.9712501886785113170, 0.9875001942116438114, 1.000000000000000000 ),
 .UNSPECIFIED. ) ;
#4281 = CARTESIAN_POINT ( 'NONE',  ( 12.17125901970652180, 0.3547769576528396196, -13.99550803169339908 ) ) ;
#4282 = CARTESIAN_POINT ( 'NONE',  ( 13.64750315638899991, -9.067203425066999500, -7.400836607049000371 ) ) ;
#4283 = CARTESIAN_POINT ( 'NONE',  ( 7.800894438721999613, -3.218815632501999868, 6.398977300879999497 ) ) ;
#4284 = CARTESIAN_POINT ( 'NONE',  ( 2.915556799211332706, -0.4581489286485083134, -3.500000000000000888 ) ) ;
#4285 = CARTESIAN_POINT ( 'NONE',  ( 8.216604719590000272, 5.331510020787000315, -8.114341808290998159 ) ) ;
#4286 = CARTESIAN_POINT ( 'NONE',  ( 12.18333460557258974, -3.837988184179999873, 6.509695444280099608 ) ) ;
#4287 = ORIENTED_EDGE ( 'NONE', *, *, #55091, .F. ) ;
#4288 = FACE_OUTER_BOUND ( 'NONE', #49751, .T. ) ;
#4289 = CARTESIAN_POINT ( 'NONE',  ( 18.17163261364642324, 2.902690589304655955, -13.69579465584391365 ) ) ;
#4290 = ORIENTED_EDGE ( 'NONE', *, *, #48322, .T. ) ;
#4291 = CARTESIAN_POINT ( 'NONE',  ( 8.674830025576062198, 2.649890579813255709, 7.499988935010339475 ) ) ;
#4292 = CARTESIAN_POINT ( 'NONE',  ( 10.51414141025500015, 4.615773412711500434, 6.403245959303999868 ) ) ;
#4293 = CARTESIAN_POINT ( 'NONE',  ( 4.149992563291999836, -0.2617923565147979859, -1.999946284944288166 ) ) ;
#4294 = VECTOR ( 'NONE', #38728, 1000.000000000000000 ) ;
#4295 = CARTESIAN_POINT ( 'NONE',  ( 11.01053724730969918, 3.051574408741400291, 7.825000000000000178 ) ) ;
#4296 = DIRECTION ( 'NONE',  ( 0.000000000000000000, 0.000000000000000000, -1.000000000000000000 ) ) ;
#4297 = LINE ( 'NONE', #19353, #52711 ) ;
#4298 = VECTOR ( 'NONE', #50442, 999.9999999999998863 ) ;
#4299 = CARTESIAN_POINT ( 'NONE',  ( 21.70000133425200062, 0.000000000000000000, 0.000000000000000000 ) ) ;
#4300 = ORIENTED_EDGE ( 'NONE', *, *, #20293, .T. ) ;
#4301 = CYLINDRICAL_SURFACE ( 'NONE', #15353, 1.999999999999999556 ) ;
#4302 = CARTESIAN_POINT ( 'NONE',  ( 9.377520280414000098, 4.092867382745001059, -5.937785237406000505 ) ) ;
#4303 = ORIENTED_EDGE ( 'NONE', *, *, #42774, .F. ) ;
#4304 = CIRCLE ( 'NONE', #63436, 0.9999997023190999590 ) ;
#4305 = CARTESIAN_POINT ( 'NONE',  ( 9.766125411066999717, 4.735428155407000794, -8.791393655830999521 ) ) ;
#4306 = ORIENTED_EDGE ( 'NONE', *, *, #2748, .F. ) ;
#4307 = CARTESIAN_POINT ( 'NONE',  ( 8.541480666858999982, 4.426512626096299918, 6.293984733123999753 ) ) ;
#4308 = CARTESIAN_POINT ( 'NONE',  ( 18.09858302120876772, -2.191289104517299080, -12.51814558466705840 ) ) ;
#4309 = DIRECTION ( 'NONE',  ( -1.000000000000000000, 0.000000000000000000, 0.000000000000000000 ) ) ;
#4310 = CARTESIAN_POINT ( 'NONE',  ( 4.400028935372505501, -1.270524258233924453, 0.06756676468397571078 ) ) ;
#4311 = CARTESIAN_POINT ( 'NONE',  ( 11.75962254157670017, -3.830327337663943510, 6.639751609450683212 ) ) ;
#4312 = ORIENTED_EDGE ( 'NONE', *, *, #36299, .F. ) ;
#4313 = CARTESIAN_POINT ( 'NONE',  ( 11.59999999999999964, 5.064318446328999634, 6.844464917182299324 ) ) ;
#4314 = CARTESIAN_POINT ( 'NONE',  ( 9.879728264518837122, -5.547209490050214242, -8.349578818441225181 ) ) ;
#4315 = AXIS2_PLACEMENT_3D ( 'NONE', #30724, #15330, #36658 ) ;
#4316 = CARTESIAN_POINT ( 'NONE',  ( 7.966460921982604582, -5.180256874905444064, 8.180071673469297977 ) ) ;
#4317 = LINE ( 'NONE', #9563, #1481 ) ;
#4318 = CARTESIAN_POINT ( 'NONE',  ( 17.99626221348004051, 0.5795518042670492198, 13.98800095993141390 ) ) ;
#4319 = CARTESIAN_POINT ( 'NONE',  ( 17.75917414208900169, 3.376094807733999836, 11.11072694497999969 ) ) ;
#4320 = CARTESIAN_POINT ( 'NONE',  ( 10.97075054419999951, -2.648517896406999750, -6.788869136079999755 ) ) ;
#4321 = ORIENTED_EDGE ( 'NONE', *, *, #19656, .T. ) ;
#4322 = VERTEX_POINT ( 'NONE', #5029 ) ;
#4323 = CARTESIAN_POINT ( 'NONE',  ( 8.548770280408998445, 5.203550244299999683, -8.391678825488000371 ) ) ;
#4324 = CARTESIAN_POINT ( 'NONE',  ( 10.47253786429000044, 2.899999999999999911, -6.571291218949999902 ) ) ;
#4325 = CARTESIAN_POINT ( 'NONE',  ( 12.24837323140831202, -2.784344744657781590, 13.60903177735235836 ) ) ;
#4326 = CARTESIAN_POINT ( 'NONE',  ( 23.81723299462928622, 3.309383924426469559, 13.09646026573576272 ) ) ;
#4327 = EDGE_CURVE ( 'NONE', #51766, #15157, #10279, .T. ) ;
#4328 = ADVANCED_FACE ( 'NONE', ( #21796 ), #64782, .T. ) ;
#4329 = CARTESIAN_POINT ( 'NONE',  ( 10.76346886766499900, 3.365322927604099679, -6.346853961441000003 ) ) ;
#4330 = CARTESIAN_POINT ( 'NONE',  ( 9.940621437244999470, 4.575883738927100097, -6.851875117168399143 ) ) ;
#4332 = DIRECTION ( 'NONE',  ( 1.000000000000000000, 0.000000000000000000, 0.000000000000000000 ) ) ;
#4331 = CARTESIAN_POINT ( 'NONE',  ( 10.18034252387499983, -4.992846242613000030, 7.651982363644999730 ) ) ;
#4333 = CARTESIAN_POINT ( 'NONE',  ( 4.659193173016666911, -0.3926218265389189721, -1.460959015002473604 ) ) ;
#4334 = ORIENTED_EDGE ( 'NONE', *, *, #47404, .T. ) ;
#4335 = CARTESIAN_POINT ( 'NONE',  ( 11.07245484343000008, -2.731907627704000419, 5.080881421444000345 ) ) ;
#4336 = B_SPLINE_CURVE_WITH_KNOTS ( 'NONE', 3,
 ( #5777, #1234, #6468, #11366, #48436, #17664, #1575, #32704, #32029, #12067, #22893, #891, #49120, #22204, #64841, #545, #53342, #16272, #44244, #26781, #65190, #37597, #17309, #58930, #11032, #21858 ),
 .UNSPECIFIED., .F., .F.,
 ( 4, 2, 2, 2, 2, 2, 2, 2, 2, 2, 2, 2, 4 ),
 ( 0.000000000000000000, 0.06250000000000215106, 0.09375000000000133227, 0.1250000000000005274, 0.2500000000000011102, 0.3750000000000016653, 0.5000000000000022204, 0.6250000000000028866, 0.7500000000000033307, 0.8125000000000039968, 0.8437500000000027756, 0.8750000000000014433, 1.000000000000000000 ),
 .UNSPECIFIED. ) ;
#4337 = CARTESIAN_POINT ( 'NONE',  ( 10.38593211929999960, -3.066808974315999858, -4.600377780681998985 ) ) ;
#4338 = CARTESIAN_POINT ( 'NONE',  ( 9.760355082327999199, 3.427502311996299955, 8.643954013369999245 ) ) ;
#4339 = CARTESIAN_POINT ( 'NONE',  ( 6.899999691988000450, -12.20988339176000004, -3.111064831550000243 ) ) ;
#4340 = AXIS2_PLACEMENT_3D ( 'NONE', #5806, #6148, #16983 ) ;
#4341 = PLANE ( 'NONE',  #4199 ) ;
#4342 = LINE ( 'NONE', #26720, #38599 ) ;
#4343 = CARTESIAN_POINT ( 'NONE',  ( 9.939260841229000221, 5.099602161831000124, -9.049221499261999924 ) ) ;
#4344 = DIRECTION ( 'NONE',  ( 0.000000000000000000, 1.000000000000000000, 0.000000000000000000 ) ) ;
#4345 = CARTESIAN_POINT ( 'NONE',  ( 7.961495038489999843, 3.389986099490999827, -6.279439026173999849 ) ) ;
#4346 = CARTESIAN_POINT ( 'NONE',  ( 6.513288077784000762, 0.7188269793800999841, -0.9308427218166001049 ) ) ;
#4347 = EDGE_CURVE ( 'NONE', #20297, #67708, #9285, .T. ) ;
#4348 = CARTESIAN_POINT ( 'NONE',  ( 11.58810207955139937, -4.796537143354000499, 7.825000000000000178 ) ) ;
#4349 = CARTESIAN_POINT ( 'NONE',  ( 17.92307254474012623, 3.107335109280919383, 12.21089239123578984 ) ) ;
#4350 = CARTESIAN_POINT ( 'NONE',  ( 3.444021066193000191, -0.7970639432754000886, 3.160059308709000092 ) ) ;
#4351 = ORIENTED_EDGE ( 'NONE', *, *, #17205, .F. ) ;
#4352 = CARTESIAN_POINT ( 'NONE',  ( 12.30864223534303648, 0.3802890292809097961, -12.69234946364261241 ) ) ;
#4353 = CARTESIAN_POINT ( 'NONE',  ( 12.23610050202371369, -2.758887154262256391, -12.38747357484177947 ) ) ;
#4354 = DIRECTION ( 'NONE',  ( 0.000000000000000000, 1.000000000000000000, 0.000000000000000000 ) ) ;
#4355 = CARTESIAN_POINT ( 'NONE',  ( 3.499644761404835158, -1.843447052673009123, -2.761503345702634782 ) ) ;
#4356 = CARTESIAN_POINT ( 'NONE',  ( 1.686390132541208509, -0.4581489286485234680, 3.499999999999998668 ) ) ;
#4357 = ORIENTED_EDGE ( 'NONE', *, *, #57711, .T. ) ;
#4358 = CARTESIAN_POINT ( 'NONE',  ( 5.241063833726999910, -0.5918267827669999592, 1.016258213757999851 ) ) ;
#4359 = SHAPE_DEFINITION_REPRESENTATION ( #39978, #55423 ) ;
#4360 = CARTESIAN_POINT ( 'NONE',  ( 17.98740632563133346, 0.4515327045973433484, 12.68919950483489067 ) ) ;
#4361 = CARTESIAN_POINT ( 'NONE',  ( 13.73712493497300180, -11.35980872612999804, -2.405726353896999736 ) ) ;
#4362 = DIRECTION ( 'NONE',  ( -0.000000000000000000, 0.9624505444715651947, 0.2714570858282905341 ) ) ;
#4363 = CARTESIAN_POINT ( 'NONE',  ( 11.60477869730532774, 3.532552483170099844, -6.578238193496799724 ) ) ;
#4364 = ORIENTED_EDGE ( 'NONE', *, *, #51382, .F. ) ;
#4365 = CARTESIAN_POINT ( 'NONE',  ( 9.351499161061999743, -4.821938821912000073, 8.950150764319998231 ) ) ;
#4366 = ORIENTED_EDGE ( 'NONE', *, *, #18176, .F. ) ;
#4367 = CARTESIAN_POINT ( 'NONE',  ( 11.89043504475232815, -5.070797187771876047, 6.797261353019674601 ) ) ;
#4368 = CARTESIAN_POINT ( 'NONE',  ( 8.251331853209000755, -5.773185758034999893, 7.141496747382000798 ) ) ;
#4369 = DIRECTION ( 'NONE',  ( 1.000000000000000000, 0.000000000000000000, 0.000000000000000000 ) ) ;
#4370 = ORIENTED_EDGE ( 'NONE', *, *, #11007, .T. ) ;
#4371 = CARTESIAN_POINT ( 'NONE',  ( 23.61227780979461954, 10.11764914276287541, 9.630145176663825524 ) ) ;
#4372 = LINE ( 'NONE', #19433, #56176 ) ;
#4373 = CARTESIAN_POINT ( 'NONE',  ( 6.612589158770999731, 5.292420046468999217, -7.844702366751000966 ) ) ;
#4374 = LINE ( 'NONE', #64132, #751 ) ;
#4375 = FACE_OUTER_BOUND ( 'NONE', #16806, .T. ) ;
#4376 = VERTEX_POINT ( 'NONE', #37533 ) ;
#4377 = CARTESIAN_POINT ( 'NONE',  ( 9.305875415870998424, -4.945293979885000191, 9.077881967919999795 ) ) ;
#4378 = CARTESIAN_POINT ( 'NONE',  ( 12.18808187647154817, -2.399650199032397069, -13.69418124938799330 ) ) ;
#4379 = CARTESIAN_POINT ( 'NONE',  ( 12.62563329236251519, 11.41733447966572434, -4.609296053777672597 ) ) ;
#4380 = EDGE_LOOP ( 'NONE', ( #66659, #68072 ) ) ;
#4381 = CARTESIAN_POINT ( 'NONE',  ( 10.77434462036999818, -4.612888200890999713, -8.898797372219998891 ) ) ;
#4382 = B_SPLINE_CURVE_WITH_KNOTS ( 'NONE', 3,
 ( #22265, #27874, #22609, #43952 ),
 .UNSPECIFIED., .F., .F.,
 ( 4, 4 ),
 ( 0.000000000000000000, 1.000000000000000000 ),
 .UNSPECIFIED. ) ;
#4383 = FACE_BOUND ( 'NONE', #9653, .T. ) ;
#4384 = ORIENTED_EDGE ( 'NONE', *, *, #8853, .T. ) ;
#4385 = CARTESIAN_POINT ( 'NONE',  ( 23.57382309776751583, -10.27665349734288291, 9.488812925140930332 ) ) ;
#4386 = CARTESIAN_POINT ( 'NONE',  ( 24.17201630339561902, 12.42869476374950821, -3.341605307461719576 ) ) ;
#4387 = LINE ( 'NONE', #68705, #43834 ) ;
#4388 = DIRECTION ( 'NONE',  ( 0.000000000000000000, -0.9999606858717338120, 0.008867170401640298016 ) ) ;
#4389 = ADVANCED_FACE ( 'NONE', ( #32309 ), #33609, .T. ) ;
#4390 = LINE ( 'NONE', #25724, #1780 ) ;
#4391 = CARTESIAN_POINT ( 'NONE',  ( 11.53159663546301417, 3.486713160384601107, -11.11613240504657796 ) ) ;
#4392 = ADVANCED_FACE ( 'NONE', ( #31612 ), #4587, .F. ) ;
#4393 = CARTESIAN_POINT ( 'NONE',  ( 12.30785086506343795, 2.879247442421004166, 13.58563033715520341 ) ) ;
#4394 = CARTESIAN_POINT ( 'NONE',  ( 5.200000000000000178, 1.600000000000000089, 0.000000000000000000 ) ) ;
#4395 = ORIENTED_EDGE ( 'NONE', *, *, #15057, .T. ) ;
#4396 = CARTESIAN_POINT ( 'NONE',  ( 3.401913944286333980, -1.050734239995861019, -3.384364968950117625 ) ) ;
#4397 = ORIENTED_EDGE ( 'NONE', *, *, #33873, .T. ) ;
#4398 = CARTESIAN_POINT ( 'NONE',  ( 11.12915085989000019, 3.083869275439000024, 8.585995236726001067 ) ) ;
#4399 = DIRECTION ( 'NONE',  ( 0.8480635683784220058, 0.000000000000000000, -0.5298945026977139872 ) ) ;
#4400 = CARTESIAN_POINT ( 'NONE',  ( 12.24277986057914980, 2.226901448799673666, -13.72760233995392731 ) ) ;
#4401 = CARTESIAN_POINT ( 'NONE',  ( 2.845251065309999827, 1.568303745132999749, -3.177790406895000253 ) ) ;
#4402 = CYLINDRICAL_SURFACE ( 'NONE', #23168, 1.350000000000000533 ) ;
#4403 = DIRECTION ( 'NONE',  ( 0.000000000000000000, 0.8648648648648717963, -0.5020047465136829867 ) ) ;
#4404 = CARTESIAN_POINT ( 'NONE',  ( 18.18005043824477696, -1.062925945863725942E-10, 13.90000000153292881 ) ) ;
#4405 = ORIENTED_EDGE ( 'NONE', *, *, #23795, .T. ) ;
#4406 = CARTESIAN_POINT ( 'NONE',  ( 24.30000000000000071, 8.810505093353000916, -8.810505093353000916 ) ) ;
#4407 = CARTESIAN_POINT ( 'NONE',  ( 11.43656785386840014, -5.060279460151999587, 6.786470850652599474 ) ) ;
#4408 = FACE_OUTER_BOUND ( 'NONE', #39180, .T. ) ;
#4409 = PLANE ( 'NONE',  #33782 ) ;
#4410 = EDGE_CURVE ( 'NONE', #46362, #27235, #21791, .T. ) ;
#4411 = CARTESIAN_POINT ( 'NONE',  ( 7.308879440377999970, -4.847802017252000439, 9.065364004483999594 ) ) ;
#4412 = VECTOR ( 'NONE', #32580, 1000.000000000000000 ) ;
#4414 = CARTESIAN_POINT ( 'NONE',  ( 11.09999999999999964, 5.299999999999999822, 6.469505845987999493 ) ) ;
#4413 = CARTESIAN_POINT ( 'NONE',  ( 10.77962664842000073, 2.397507474987000009, 7.755423212350999407 ) ) ;
#4415 = CARTESIAN_POINT ( 'NONE',  ( 11.45348876160960039, 3.114179898019400206, -8.421216112044099589 ) ) ;
#4416 = EDGE_CURVE ( 'NONE', #12823, #40899, #65123, .T. ) ;
#4417 = CARTESIAN_POINT ( 'NONE',  ( 14.93333333127366735, -8.815235367372471487, -7.616700428521845367 ) ) ;
#4418 = CARTESIAN_POINT ( 'NONE',  ( 8.844480666858999030, 4.334888990546500231, -8.446938520915798776 ) ) ;
#4419 = CARTESIAN_POINT ( 'NONE',  ( 17.63863136176617274, 0.7145943380091432928, 12.57972004139935152 ) ) ;
#4420 = CARTESIAN_POINT ( 'NONE',  ( 6.782661737893000087, -0.3582968336244000129, -1.367819579490999971 ) ) ;
#4421 = DIRECTION ( 'NONE',  ( 0.000000000000000000, 0.6482718649732923666, -0.7614089499631913061 ) ) ;
#4422 = CARTESIAN_POINT ( 'NONE',  ( 0.4021888528303215748, 2.957367267881657824, -1.739788196031706757 ) ) ;
#4423 = VERTEX_POINT ( 'NONE', #21118 ) ;
#4424 = CARTESIAN_POINT ( 'NONE',  ( 7.512831853207000421, -5.524126964933000927, 6.910359834012999691 ) ) ;
#4425 = CARTESIAN_POINT ( 'NONE',  ( 18.08585342091140546, 3.015868411947682404, 13.67131429327875125 ) ) ;
#4426 = LINE ( 'NONE', #19140, #27824 ) ;
#4427 = EDGE_LOOP ( 'NONE', ( #55944, #27432, #8692, #55742, #47714 ) ) ;
#4428 = CARTESIAN_POINT ( 'NONE',  ( 0.6912484304700000637, 2.302377811826000098, -2.236047032684999714 ) ) ;
#4429 = EDGE_CURVE ( 'NONE', #44304, #5638, #42444, .T. ) ;
#4430 = CARTESIAN_POINT ( 'NONE',  ( 11.05946005378019947, 5.036385109519999403, 8.053412743695298914 ) ) ;
#4431 = CARTESIAN_POINT ( 'NONE',  ( 10.50897971959000010, 4.485029564998000318, -9.114435267298000909 ) ) ;
#4432 = ORIENTED_EDGE ( 'NONE', *, *, #25440, .T. ) ;
#4433 = CARTESIAN_POINT ( 'NONE',  ( 1.478056799207333460, 2.150913519912206695, -2.798833948393626869 ) ) ;
#4434 = DIRECTION ( 'NONE',  ( 0.7071067811865475727, 0.7071067811865475727, 0.000000000000000000 ) ) ;
#4435 = CARTESIAN_POINT ( 'NONE',  ( 11.10887482311539998, 5.184953745778000389, 7.021250586468399391 ) ) ;
#4436 = CARTESIAN_POINT ( 'NONE',  ( 24.57937622057101379, 8.815984698512634665, -9.246564900184520042 ) ) ;
#4437 = CARTESIAN_POINT ( 'NONE',  ( 9.170323341230000480, 5.558938731259999599, 6.272977177425000050 ) ) ;
#4438 = ORIENTED_EDGE ( 'NONE', *, *, #8103, .F. ) ;
#4439 = CARTESIAN_POINT ( 'NONE',  ( 10.16000000000000014, 4.496968146123999865, -8.755198255949000696 ) ) ;
#4440 = CARTESIAN_POINT ( 'NONE',  ( 8.362489158770998188, 5.592690705327999723, -8.535639167491000379 ) ) ;
#4441 = CARTESIAN_POINT ( 'NONE',  ( 8.283766169413352642, -4.844672635244611669, 9.020389543242568919 ) ) ;
#4442 = CARTESIAN_POINT ( 'NONE',  ( 9.170138961223999630, -3.053949131563199693, 6.860686042446299204 ) ) ;
#4443 = VERTEX_POINT ( 'NONE', #21450 ) ;
#4444 = LINE ( 'NONE', #36621, #57812 ) ;
#4445 = CARTESIAN_POINT ( 'NONE',  ( 7.000000000000000000, -0.2392304845412999981, -3.000000000000000000 ) ) ;
#4446 = VERTEX_POINT ( 'NONE', #43129 ) ;
#4447 = CARTESIAN_POINT ( 'NONE',  ( 11.00009108335970609, 5.118893581675404647, -7.597657431955929574 ) ) ;
#4448 = CARTESIAN_POINT ( 'NONE',  ( 16.39999999308669842, -3.302282894619416265, -11.70823727156336425 ) ) ;
#4449 = ORIENTED_EDGE ( 'NONE', *, *, #19883, .F. ) ;
#4450 = DIRECTION ( 'NONE',  ( -1.000000000000000000, 0.000000000000000000, 0.000000000000000000 ) ) ;
#4451 = DIRECTION ( 'NONE',  ( 0.000000000000000000, -1.000000000000000000, 0.000000000000000000 ) ) ;
#4452 = CARTESIAN_POINT ( 'NONE',  ( 10.81013259637009938, 2.968328969579000276, -8.062151801142800167 ) ) ;
#4453 = CARTESIAN_POINT ( 'NONE',  ( 11.85034208742530026, -4.630634088820300143, 6.508707709313799050 ) ) ;
#4454 = CYLINDRICAL_SURFACE ( 'NONE', #8545, 1.250000000000000000 ) ;
#4455 = CARTESIAN_POINT ( 'NONE',  ( 12.12579573085663043, -2.760622544769000264, 7.285547569258399747 ) ) ;
#4456 = CARTESIAN_POINT ( 'NONE',  ( 7.373073341229000377, 3.394842219570000097, 9.388954446285000088 ) ) ;
#4457 = EDGE_LOOP ( 'NONE', ( #48790, #48754, #16300, #52974 ) ) ;
#4458 = CIRCLE ( 'NONE', #17911, 0.6999999999999992895 ) ;
#4459 = CARTESIAN_POINT ( 'NONE',  ( 6.899999438051000133, 0.5526611926744998682, 1.394476821647000042 ) ) ;
#4460 = CARTESIAN_POINT ( 'NONE',  ( 7.711433059622000208, -5.797088532631000213, 8.340479314546998424 ) ) ;
#4461 = CARTESIAN_POINT ( 'NONE',  ( 10.02101354018262569, 4.768183399968643599, 6.500416447002272946 ) ) ;
#4462 = ORIENTED_EDGE ( 'NONE', *, *, #55425, .T. ) ;
#4463 = CARTESIAN_POINT ( 'NONE',  ( 12.79295051314563203, -1.760910731560545450, -12.47634535177225068 ) ) ;
#4464 = CARTESIAN_POINT ( 'NONE',  ( 6.611566299282000791, 8.335736774492993106, -4.065895807218002034 ) ) ;
#4465 = CARTESIAN_POINT ( 'NONE',  ( 12.09999999999999964, -4.883784007588900522, 7.174999999999999822 ) ) ;
#4466 = EDGE_CURVE ( 'NONE', #36754, #29376, #5078, .T. ) ;
#4467 = CARTESIAN_POINT ( 'NONE',  ( 23.63971702668698072, -13.40694874527435410, -3.855832365366145265 ) ) ;
#4468 = CARTESIAN_POINT ( 'NONE',  ( 12.70873338277719711, -3.242082958893204303, -13.61943113270052486 ) ) ;
#4469 = EDGE_CURVE ( 'NONE', #24854, #47095, #59314, .T. ) ;
#4470 = CARTESIAN_POINT ( 'NONE',  ( 11.14179841651039915, -4.353306409735099969, -8.439215328713499886 ) ) ;
#4471 = ADVANCED_FACE ( 'NONE', ( #55349 ), #38929, .F. ) ;
#4472 = CARTESIAN_POINT ( 'NONE',  ( 11.41544519387737289, 4.732426395176744016, -7.017892448335746103 ) ) ;
#4473 = CARTESIAN_POINT ( 'NONE',  ( 18.27597346048322535, -2.401680171065127212, 12.36899652916222436 ) ) ;
#4474 = ORIENTED_EDGE ( 'NONE', *, *, #29547, .F. ) ;
#4475 = VERTEX_POINT ( 'NONE', #17604 ) ;
#4476 = FILL_AREA_STYLE_COLOUR ( '', #41883 ) ;
#4477 = CARTESIAN_POINT ( 'NONE',  ( 11.58810207955109917, -4.796537143354000499, -7.174999999999999822 ) ) ;
#4478 = DIRECTION ( 'NONE',  ( 1.000000000000000000, 0.000000000000000000, 0.000000000000000000 ) ) ;
#4479 = CARTESIAN_POINT ( 'NONE',  ( 9.701722306758000514, 4.253749110891999585, -8.839930742927998963 ) ) ;
#4480 = DIRECTION ( 'NONE',  ( 0.000000000000000000, 1.000000000000000000, 0.000000000000000000 ) ) ;
#4481 = CARTESIAN_POINT ( 'NONE',  ( 18.05239999627272951, 2.879049404332129747, 12.35514073459315476 ) ) ;
#4482 = CARTESIAN_POINT ( 'NONE',  ( 24.57010863793600208, -12.57173122536999976, 2.966538848022999719 ) ) ;
#4483 = CARTESIAN_POINT ( 'NONE',  ( 10.09696969267000100, 5.253376380222999131, 8.530663119653999260 ) ) ;
#4484 = B_SPLINE_CURVE_WITH_KNOTS ( 'NONE', 3,
 ( #60677, #22231, #49147, #60335, #12441, #19749 ),
 .UNSPECIFIED., .F., .F.,
 ( 4, 2, 4 ),
 ( 0.000000000000000000, 0.5000000000000000000, 1.000000000000000000 ),
 .UNSPECIFIED. ) ;
#4485 = ORIENTED_EDGE ( 'NONE', *, *, #67630, .T. ) ;
#4486 = CARTESIAN_POINT ( 'NONE',  ( 8.625477980836398828, -4.987582323328632938, -6.571819886621350193 ) ) ;
#4487 = EDGE_LOOP ( 'NONE', ( #36704, #63668, #24026, #18587 ) ) ;
#4488 = CARTESIAN_POINT ( 'NONE',  ( 9.285195242305000818, 5.269680202247999823, 8.747831873285999649 ) ) ;
#4489 = CARTESIAN_POINT ( 'NONE',  ( 9.627671671056999614, -4.855035690642299784, -7.643603315539799326 ) ) ;
#4490 = CARTESIAN_POINT ( 'NONE',  ( 10.83658792121999959, 5.133186143592999962, 8.848368005200001107 ) ) ;
#4491 = CARTESIAN_POINT ( 'NONE',  ( 10.97769598648999967, -2.990523684589000197, 6.898940957443399746 ) ) ;
#4492 = CARTESIAN_POINT ( 'NONE',  ( 8.722235841230000730, 3.844886277615000125, -8.888911790991000927 ) ) ;
#4493 = CARTESIAN_POINT ( 'NONE',  ( 11.01762739314999884, 7.862581927908000701, -6.520239972965000241 ) ) ;
#4494 = CARTESIAN_POINT ( 'NONE',  ( 10.27195525820100031, 3.879327850572200198, -6.227697122196000024 ) ) ;
#4495 = CIRCLE ( 'NONE', #68128, 11.50000000000000533 ) ;
#4496 = CARTESIAN_POINT ( 'NONE',  ( 10.87969287004431784, 5.549552169302327975, -8.346468143089040836 ) ) ;
#4497 = CARTESIAN_POINT ( 'NONE',  ( 11.59999999999999964, 3.801977891258315978, -8.571335789050444021 ) ) ;
#4498 = CARTESIAN_POINT ( 'NONE',  ( 9.509901345851000443, 5.077442745148000647, 8.469003100811999474 ) ) ;
#4499 = CARTESIAN_POINT ( 'NONE',  ( 9.208690252286228173, -2.678874286390015680, 7.777716411846479438 ) ) ;
#4500 = ORIENTED_EDGE ( 'NONE', *, *, #42230, .T. ) ;
#4501 = CARTESIAN_POINT ( 'NONE',  ( 8.929995280412999392, 5.030502105212999453, -6.322203460290999999 ) ) ;
#4502 = CARTESIAN_POINT ( 'NONE',  ( 18.18005043824377154, 1.329526366183796371E-10, 12.70000000088145420 ) ) ;
#4503 = CARTESIAN_POINT ( 'NONE',  ( 9.132625033077289345, 2.794592352500905541, 8.206332652464679356 ) ) ;
#4504 = CARTESIAN_POINT ( 'NONE',  ( 12.70917152008051154, -3.194951439751541944, -12.18820651941599387 ) ) ;
#4505 = CARTESIAN_POINT ( 'NONE',  ( 10.20851354018233437, 4.163624617374472869, -6.250000000000001776 ) ) ;
#4506 = AXIS2_PLACEMENT_3D ( 'NONE', #67448, #62887, #9755 ) ;
#4507 = CARTESIAN_POINT ( 'NONE',  ( 10.74379975933729980, -2.921317947059999920, -7.128873141726999485 ) ) ;
#4508 = ORIENTED_EDGE ( 'NONE', *, *, #44117, .T. ) ;
#4509 = B_SPLINE_CURVE_WITH_KNOTS ( 'NONE', 3,
 ( #36276, #9348, #56917, #41521 ),
 .UNSPECIFIED., .F., .F.,
 ( 4, 4 ),
 ( 0.000000000000000000, 1.000000000000000000 ),
 .UNSPECIFIED. ) ;
#4510 = DIRECTION ( 'NONE',  ( 0.000000000000000000, 0.8514543052404082157, -0.5244287998266055073 ) ) ;
#4511 = CARTESIAN_POINT ( 'NONE',  ( 7.886573341228999112, 3.084076314893000159, 9.259847992573000397 ) ) ;
#4512 = EDGE_CURVE ( 'NONE', #22792, #3413, #17600, .T. ) ;
#4515 = CARTESIAN_POINT ( 'NONE',  ( 10.90000053908999966, 0.000000000000000000, 0.000000000000000000 ) ) ;
#4514 = CARTESIAN_POINT ( 'NONE',  ( 9.667489158770999680, 4.808846957865000604, -8.639578604182998944 ) ) ;
#4513 = UNCERTAINTY_MEASURE_WITH_UNIT (LENGTH_MEASURE( 1.000000000000000082E-05 ), #12748, 'distance_accuracy_value', 'NONE');
#4516 = CARTESIAN_POINT ( 'NONE',  ( 17.79999999998900151, 3.595165934733000057, -11.99793354950999991 ) ) ;
#4517 = VERTEX_POINT ( 'NONE', #57064 ) ;
#4518 = CARTESIAN_POINT ( 'NONE',  ( 9.625496329943999285, 3.134638325776999856, 8.626949804392001653 ) ) ;
#4519 = EDGE_CURVE ( 'NONE', #51180, #39230, #15117, .T. ) ;
#4520 = CARTESIAN_POINT ( 'NONE',  ( 18.04548494004250969, -2.887558854919742846, -13.58353091070611107 ) ) ;
#4521 = CARTESIAN_POINT ( 'NONE',  ( 11.51518179236248862, 3.819003318705799899, 8.347076615013298451 ) ) ;
#4522 = CARTESIAN_POINT ( 'NONE',  ( 11.01895424672924584, -5.424779607849700369, 7.028465765784092767 ) ) ;
#4523 = CARTESIAN_POINT ( 'NONE',  ( 7.448644353207000357, -4.628942671846000501, 5.991663889842000046 ) ) ;
#4524 = EDGE_LOOP ( 'NONE', ( #54508, #68012, #15369, #18504 ) ) ;
#4525 = CARTESIAN_POINT ( 'NONE',  ( 8.058767219590999176, 2.432118421226999949, 6.597517552098000060 ) ) ;
#4527 = CARTESIAN_POINT ( 'NONE',  ( 10.64557055961999943, -2.988935764546999607, -5.952339209104000162 ) ) ;
#4526 = CARTESIAN_POINT ( 'NONE',  ( 10.12125395348325441, -3.646954034496651786, 8.849054885471268506 ) ) ;
#4528 = CARTESIAN_POINT ( 'NONE',  ( 7.594155103570124687, -4.422461687346440407, 5.812547095734072577 ) ) ;
#4529 = CARTESIAN_POINT ( 'NONE',  ( 18.17906596529827823, -0.04061643729585483892, 13.89993966956888372 ) ) ;
#4530 = CARTESIAN_POINT ( 'NONE',  ( 24.22025250524800200, 3.188360109827999889, 12.21446149360000000 ) ) ;
#4531 = ORIENTED_EDGE ( 'NONE', *, *, #25878, .F. ) ;
#4532 = CARTESIAN_POINT ( 'NONE',  ( 10.27427156480999848, -4.600000212792999754, 4.944156960788000710 ) ) ;
#4533 = CARTESIAN_POINT ( 'NONE',  ( 11.25210807141120029, -3.959980833595939664, 6.634727177901499573 ) ) ;
#4534 = CARTESIAN_POINT ( 'NONE',  ( 11.43114108301961629, 4.620688244309836712, 8.119401481368297979 ) ) ;
#4535 = CARTESIAN_POINT ( 'NONE',  ( 10.41103858098833790, 5.348820511807942601, 7.263526229479707830 ) ) ;
#4536 = CARTESIAN_POINT ( 'NONE',  ( 10.57149279008999798, 3.703313553258400059, 6.398515879103999993 ) ) ;
#4537 = VERTEX_POINT ( 'NONE', #51139 ) ;
#4538 = CARTESIAN_POINT ( 'NONE',  ( 24.30001680216799897, -3.271769318036999774, 12.21048166890999909 ) ) ;
#4539 = CARTESIAN_POINT ( 'NONE',  ( 12.08085380679222531, 2.436412096897879298, -12.36221874022169764 ) ) ;
#4540 = CARTESIAN_POINT ( 'NONE',  ( 10.98041052569057285, -5.205274417407212084, 6.713913193645853816 ) ) ;
#4542 = CARTESIAN_POINT ( 'NONE',  ( 24.34833250136633609, -8.895958538877664523, 8.895958538877664523 ) ) ;
#4541 = B_SPLINE_CURVE_WITH_KNOTS ( 'NONE', 3,
 ( #4001, #25338, #32915, #6326, #26031, #33613, #47706, #17529, #1445, #59472, #21129, #33958, #49683, #17168 ),
 .UNSPECIFIED., .F., .F.,
 ( 4, 2, 2, 2, 2, 2, 4 ),
 ( 0.000000000000000000, 0.1249999999999998890, 0.2499999999999997780, 0.4999999999999995559, 0.6249999999999994449, 0.7499999999999993339, 1.000000000000000000 ),
 .UNSPECIFIED. ) ;
#4543 = CARTESIAN_POINT ( 'NONE',  ( 17.84579744522524436, -1.849003904486296701, 13.87736309738764184 ) ) ;
#4544 = CARTESIAN_POINT ( 'NONE',  ( 18.16264250269799163, 2.646798803964871549, -13.64122832052404988 ) ) ;
#4545 = VERTEX_POINT ( 'NONE', #67544 ) ;
#4546 = DIRECTION ( 'NONE',  ( 0.000000000000000000, 0.000000000000000000, -1.000000000000000000 ) ) ;
#4547 = CARTESIAN_POINT ( 'NONE',  ( 9.110163692916374956, -2.765799910565780895, -7.245561603203542589 ) ) ;
#4549 = EDGE_LOOP ( 'NONE', ( #10593, #27962, #51852, #13002, #6695, #65973, #10325, #21314, #35450, #2497 ) ) ;
#4548 = AXIS2_PLACEMENT_3D ( 'NONE', #18686, #23239, #18345 ) ;
#4550 = DIRECTION ( 'NONE',  ( 0.7071060865237062121, -0.7071074758487063683, -8.142070991701072997E-10 ) ) ;
#4551 = CARTESIAN_POINT ( 'NONE',  ( 11.85159063708299954, 4.825025306051200502, 7.268038553423699533 ) ) ;
#4552 = CARTESIAN_POINT ( 'NONE',  ( 10.59344747867000081, 5.297752619853000944, 8.474195539311001113 ) ) ;
#4553 = CARTESIAN_POINT ( 'NONE',  ( 11.19121071698999970, 3.005389011699000079, -6.023544385387999966 ) ) ;
#4554 = CARTESIAN_POINT ( 'NONE',  ( 9.024266954400625096, -4.325581995510845879, -6.687886317613946474 ) ) ;
#4555 = CARTESIAN_POINT ( 'NONE',  ( 10.13340376756999994, -5.653635692335999607, 6.501829690795999817 ) ) ;
#4556 = ADVANCED_FACE ( 'NONE', ( #24568 ), #14640, .F. ) ;
#4557 = CARTESIAN_POINT ( 'NONE',  ( 18.24150829797650530, 0.2316996085786106607, -12.59787430930301433 ) ) ;
#4559 = AXIS2_PLACEMENT_3D ( 'NONE', #55432, #34800, #23267 ) ;
#4558 = B_SPLINE_CURVE_WITH_KNOTS ( 'NONE', 3,
 ( #26656, #37820, #20713, #36798 ),
 .UNSPECIFIED., .F., .F.,
 ( 4, 4 ),
 ( 0.000000000000000000, 1.000000000000000000 ),
 .UNSPECIFIED. ) ;
#4560 = CARTESIAN_POINT ( 'NONE',  ( 12.52707377838018132, 3.060156797977223508, -12.30326077405661778 ) ) ;
#4561 = CARTESIAN_POINT ( 'NONE',  ( 11.50687348028854906, -5.003459210197000573, -8.042549288197099244 ) ) ;
#4562 = ADVANCED_FACE ( 'NONE', ( #25598 ), #46924, .F. ) ;
#4563 = EDGE_CURVE ( 'NONE', #15006, #27711, #23564, .T. ) ;
#4564 = CARTESIAN_POINT ( 'NONE',  ( 7.555281674562000838, 4.314040636970999820, 8.819134391732999845 ) ) ;
#4565 = ORIENTED_EDGE ( 'NONE', *, *, #40188, .F. ) ;
#4566 = CARTESIAN_POINT ( 'NONE',  ( 24.71426445414105544, -3.125270931515957695, 11.79471460629179624 ) ) ;
#4567 = CARTESIAN_POINT ( 'NONE',  ( 11.03667431141999877, 5.223173388369999337, -5.023616880107000249 ) ) ;
#4568 = DIRECTION ( 'NONE',  ( 0.8843050095428930391, 0.1786786001429985227, 0.4313682973379965868 ) ) ;
#4569 = CARTESIAN_POINT ( 'NONE',  ( 8.008552228053002153, 8.952106511966999136, 5.726245348430995641 ) ) ;
#4570 = CARTESIAN_POINT ( 'NONE',  ( 12.25061842917684451, 2.988573241473608366, 13.67729937646034521 ) ) ;
#4571 = CARTESIAN_POINT ( 'NONE',  ( 10.80169466977000070, -3.998196228428999355, 9.431543037543999475 ) ) ;
#4572 = CARTESIAN_POINT ( 'NONE',  ( 12.80505043854144276, -0.6250000000000001110, -12.67928921589118652 ) ) ;
#4573 = CARTESIAN_POINT ( 'NONE',  ( 12.44248702983405153, -0.6327954766588973490, 13.98569611075749108 ) ) ;
#4574 = ORIENTED_EDGE ( 'NONE', *, *, #59530, .F. ) ;
#4575 = CARTESIAN_POINT ( 'NONE',  ( 12.56977253056427557, -1.799738463188393256, 12.47080370841241326 ) ) ;
#4576 = CARTESIAN_POINT ( 'NONE',  ( 10.23959632033899858, -5.057167065956000407, -7.068569539041399175 ) ) ;
#4577 = CARTESIAN_POINT ( 'NONE',  ( 5.500000000000000000, -12.78667792605000031, -2.345384795463000049 ) ) ;
#4578 = ADVANCED_FACE ( 'NONE', ( #46239 ), #11782, .F. ) ;
#4579 = CARTESIAN_POINT ( 'NONE',  ( 10.15903154954000165, -4.166415630773999901, 9.114167874391000623 ) ) ;
#4580 = CARTESIAN_POINT ( 'NONE',  ( 18.18005043824477696, -1.062925945863725942E-10, 13.90000000153292881 ) ) ;
#4581 = CARTESIAN_POINT ( 'NONE',  ( 12.18748876160954886, -4.600381688599499697, 6.875627981711399883 ) ) ;
#4582 = CARTESIAN_POINT ( 'NONE',  ( 12.16008153508536083, 0.3287229608534073533, 12.59571550161850695 ) ) ;
#4583 = CARTESIAN_POINT ( 'NONE',  ( 7.598073341229000022, 3.554857159507999853, 8.889479859586000288 ) ) ;
#4584 = DIRECTION ( 'NONE',  ( -1.000000000000000000, 0.000000000000000000, 0.000000000000000000 ) ) ;
#4585 = CARTESIAN_POINT ( 'NONE',  ( 12.30575661439779900, 1.958493781132642386, 12.44686177741867006 ) ) ;
#4586 = CARTESIAN_POINT ( 'NONE',  ( 9.795911616191999016, -5.239375073306999475, -6.095351682555999240 ) ) ;
#4587 = CONICAL_SURFACE ( 'NONE', #20220, 1.199999999294000030, 0.7853981633972997312 ) ;
#4588 = CARTESIAN_POINT ( 'NONE',  ( 10.42795525820099911, 3.905250696375530239, -6.501013802764199490 ) ) ;
#4589 = CARTESIAN_POINT ( 'NONE',  ( 7.802644552000999489, 3.157760251094000825, -6.317964942532003469 ) ) ;
#4590 = B_SPLINE_CURVE_WITH_KNOTS ( 'NONE', 3,
 ( #9352, #8683, #24762, #46776, #68081, #4797, #26140, #46088, #19517, #40837 ),
 .UNSPECIFIED., .F., .F.,
 ( 4, 1, 1, 1, 1, 1, 1, 4 ),
 ( 0.000000000000000000, 0.03621323782862000129, 0.1968444277449999946, 0.3574756176613000380, 0.5181068075775999704, 0.6787379974939999894, 0.8393691874102999773, 1.000000000000000000 ),
 .UNSPECIFIED. ) ;
#4591 = CARTESIAN_POINT ( 'NONE',  ( 10.94033278040999946, 5.142729166069000435, -6.493505370358000128 ) ) ;
#4592 = CARTESIAN_POINT ( 'NONE',  ( 9.048063610504998522, 4.524705472883399970, -8.666648427848999248 ) ) ;
#4594 = CARTESIAN_POINT ( 'NONE',  ( 12.42192081640602019, 3.001194947204297581, 12.32076077293008076 ) ) ;
#4593 = CARTESIAN_POINT ( 'NONE',  ( 15.46873602477000276, -8.828190495471000432, -7.821444125541998638 ) ) ;
#4595 = CARTESIAN_POINT ( 'NONE',  ( 11.04782425406999913, -5.235403588978999601, 5.041461677707999911 ) ) ;
#4596 = ORIENTED_EDGE ( 'NONE', *, *, #61266, .T. ) ;
#4597 = B_SPLINE_CURVE_WITH_KNOTS ( 'NONE', 3,
 ( #48767, #22530, #180, #33034, #21497, #37578, #22190, #42831, #37926, #49106 ),
 .UNSPECIFIED., .F., .F.,
 ( 4, 2, 2, 2, 4 ),
 ( 0.000000000000000000, 0.2500000000000000000, 0.5000000000000000000, 0.7500000000000000000, 1.000000000000000000 ),
 .UNSPECIFIED. ) ;
#4598 = CARTESIAN_POINT ( 'NONE',  ( 12.47604026688563117, -0.5315006617180365600, 12.68502792337811336 ) ) ;
#4599 = CARTESIAN_POINT ( 'NONE',  ( 24.30000000000000071, 9.517611874540000017, -8.103398312166000039 ) ) ;
#4600 = ADVANCED_FACE ( 'NONE', ( #34614 ), #54197, .T. ) ;
#4601 = CARTESIAN_POINT ( 'NONE',  ( 9.385788300200999856, -4.980873770300999759, 6.433336655958999728 ) ) ;
#4602 = CARTESIAN_POINT ( 'NONE',  ( 10.26090035061499961, 4.231093494672100164, 6.664354444139199529 ) ) ;
#4603 = AXIS2_PLACEMENT_3D ( 'NONE', #56350, #44834, #35035 ) ;
#4604 = DIRECTION ( 'NONE',  ( 1.000000000000000000, 0.000000000000000000, 0.000000000000000000 ) ) ;
#4605 = EDGE_CURVE ( 'NONE', #12182, #47849, #46821, .T. ) ;
#4606 = CARTESIAN_POINT ( 'NONE',  ( 12.30652006878824700, -2.122495540605185749, 13.74632343115108490 ) ) ;
#4607 = CARTESIAN_POINT ( 'NONE',  ( 12.80505043854143388, 1.875000000000000000, 13.78627172894481667 ) ) ;
#4608 = CARTESIAN_POINT ( 'NONE',  ( 24.30001683570900184, 3.271769286791000209, 12.21048169671000139 ) ) ;
#4609 = ORIENTED_EDGE ( 'NONE', *, *, #62889, .F. ) ;
#4610 = CARTESIAN_POINT ( 'NONE',  ( 4.763789736435000144, -0.8239865257563000478, 0.7797128048906999398 ) ) ;
#4611 = CARTESIAN_POINT ( 'NONE',  ( 9.326684229509998758, -4.901739481456999670, -6.592668585875199661 ) ) ;
#4612 = CARTESIAN_POINT ( 'NONE',  ( 9.804518107930274340, -2.650217341019555306, -7.676659142575331884 ) ) ;
#4613 = CARTESIAN_POINT ( 'NONE',  ( 11.48146005378009882, -3.088328798999600000, 7.986817550794899745 ) ) ;
#4614 = CARTESIAN_POINT ( 'NONE',  ( 18.17988829291487818, 2.482516021556980590, -12.45565317647434611 ) ) ;
#4615 = DIRECTION ( 'NONE',  ( -1.000000000000000000, 0.000000000000000000, 0.000000000000000000 ) ) ;
#4616 = CARTESIAN_POINT ( 'NONE',  ( 5.200000000000000178, 0.6646153846154000400, -2.616923076922999858 ) ) ;
#4617 = CONICAL_SURFACE ( 'NONE', #49237, 0.9346783463124002100, 0.7853981908209605178 ) ;
#4618 = CARTESIAN_POINT ( 'NONE',  ( 7.656866975822993915, 3.528150633380001899, 6.493493947281997691 ) ) ;
#4619 = CARTESIAN_POINT ( 'NONE',  ( 9.282558421712998609, -4.950980172046000050, -5.959730545597000884 ) ) ;
#4620 = CARTESIAN_POINT ( 'NONE',  ( 11.11478185320999934, -2.548220588762000194, -8.356740464335999263 ) ) ;
#4621 = CARTESIAN_POINT ( 'NONE',  ( 23.85399064179406281, 3.593187972531236341, -13.20264717798629306 ) ) ;
#4622 = CARTESIAN_POINT ( 'NONE',  ( 12.80505043854144276, 0.7302158263239216796, -13.98094363220831049 ) ) ;
#4623 = CARTESIAN_POINT ( 'NONE',  ( 10.76685100253999927, 2.832432432432000269, 6.822293592207000934 ) ) ;
#4624 = DIRECTION ( 'NONE',  ( 0.000000000000000000, 0.9905022095861402143, 0.1374968101629056305 ) ) ;
#4625 = CARTESIAN_POINT ( 'NONE',  ( 25.59997239626699894, -8.218962899087999929, 8.043524294852000267 ) ) ;
#4626 = VERTEX_POINT ( 'NONE', #32450 ) ;
#4627 = CARTESIAN_POINT ( 'NONE',  ( 9.102795280413999990, 3.071719032003000116, -6.037263251225000182 ) ) ;
#4628 = CARTESIAN_POINT ( 'NONE',  ( 11.07980110216399972, -4.739241740354600552, 7.951464549725199227 ) ) ;
#4629 = ORIENTED_EDGE ( 'NONE', *, *, #2275, .T. ) ;
#4630 = CARTESIAN_POINT ( 'NONE',  ( 18.40015514469800095, -2.331468351713000075E-14, -1.065814103639999827E-13 ) ) ;
#4631 = CARTESIAN_POINT ( 'NONE',  ( 17.92014050163761496, 1.886715056483305952, -13.87229028472749981 ) ) ;
#4632 = ORIENTED_EDGE ( 'NONE', *, *, #15141, .F. ) ;
#4633 = CARTESIAN_POINT ( 'NONE',  ( 10.76346886766499900, 3.365322927604099679, 8.653146038559000885 ) ) ;
#4634 = CARTESIAN_POINT ( 'NONE',  ( 9.342560841233000346, 5.835196551504000517, -7.008466539623000813 ) ) ;
#4635 = CARTESIAN_POINT ( 'NONE',  ( 6.999998782146999332, 1.243449787579999883E-13, -12.50000000000276756 ) ) ;
#4636 = CARTESIAN_POINT ( 'NONE',  ( 10.35814141025499957, -3.516507310755200066, -8.361148840840000318 ) ) ;
#4637 = CARTESIAN_POINT ( 'NONE',  ( 12.21279768068213656, 0.1999278272693495451, -13.89806912752725232 ) ) ;
#4638 = DIRECTION ( 'NONE',  ( 0.000000000000000000, -0.9772984074130801613, -0.2118674653358960658 ) ) ;
#4639 = DIRECTION ( 'NONE',  ( 1.000000000000000000, 0.000000000000000000, 0.000000000000000000 ) ) ;
#4640 = VERTEX_POINT ( 'NONE', #53766 ) ;
#4641 = CARTESIAN_POINT ( 'NONE',  ( 13.91137892731300063, 9.265832517555999459, 8.206449300197000696 ) ) ;
#4642 = EDGE_CURVE ( 'NONE', #7462, #146, #55985, .T. ) ;
#4643 = CARTESIAN_POINT ( 'NONE',  ( 9.336654719594999818, 5.095038542659000136, -6.157541456184000062 ) ) ;
#4644 = ORIENTED_EDGE ( 'NONE', *, *, #30786, .F. ) ;
#4645 = CARTESIAN_POINT ( 'NONE',  ( 10.94349541711000029, 3.081616890687000065, -8.919380927961000793 ) ) ;
#4646 = VERTEX_POINT ( 'NONE', #282 ) ;
#4647 = CARTESIAN_POINT ( 'NONE',  ( 9.428000818238999159, 2.868129552070000088, 6.903968392969799694 ) ) ;
#4648 = CARTESIAN_POINT ( 'NONE',  ( 18.14141836411850761, -2.283433982113741934, -12.49938471124205641 ) ) ;
#4649 = LINE ( 'NONE', #41383, #16191 ) ;
#4650 = TOROIDAL_SURFACE ( 'NONE', #22519, 8.250000000000000000, 1.000000000000000000 ) ;
#4651 = LINE ( 'NONE', #20745, #64778 ) ;
#4652 = CARTESIAN_POINT ( 'NONE',  ( 8.552563423645223040, 3.075208796447511439, 6.073673062848093274 ) ) ;
#4653 = VERTEX_POINT ( 'NONE', #5041 ) ;
#4654 = CARTESIAN_POINT ( 'NONE',  ( 12.79413755118400253, 11.93226572510000061, -3.260039893805000144 ) ) ;
#4655 = CARTESIAN_POINT ( 'NONE',  ( 17.70600070946500182, 11.93155574656999995, -3.263109129670000108 ) ) ;
#4656 = EDGE_CURVE ( 'NONE', #29163, #55276, #16869, .T. ) ;
#4657 = CARTESIAN_POINT ( 'NONE',  ( 8.008165174986327628, -4.679062738103563213, 8.679582621499569939 ) ) ;
#4658 = DIRECTION ( 'NONE',  ( 0.000000000000000000, 1.000000000000000000, 0.000000000000000000 ) ) ;
#4659 = CARTESIAN_POINT ( 'NONE',  ( 9.345514158774999913, 5.775964236216999836, -8.174909295649001706 ) ) ;
#4660 = CARTESIAN_POINT ( 'NONE',  ( 17.95534550153200115, -3.277905616156999713, 11.84067279748999901 ) ) ;
#4661 = CARTESIAN_POINT ( 'NONE',  ( 10.42081395746000005, -2.488448635474999726, -7.717895569088000229 ) ) ;
#4662 = ORIENTED_EDGE ( 'NONE', *, *, #29688, .F. ) ;
#4663 = ORIENTED_EDGE ( 'NONE', *, *, #6953, .T. ) ;
#4664 = CARTESIAN_POINT ( 'NONE',  ( 8.631645280409999899, 3.826300099041999747, -9.055335252254000267 ) ) ;
#4665 = CARTESIAN_POINT ( 'NONE',  ( 10.94076550314999885, -5.140765503144999471, -6.571291218949999902 ) ) ;
#4666 = CARTESIAN_POINT ( 'NONE',  ( 10.36409408021999923, -4.600000090830000943, -4.954046131267999087 ) ) ;
#4667 = CARTESIAN_POINT ( 'NONE',  ( 5.855026506350000659, 1.500000000000000000, 0.000000000000000000 ) ) ;
#4668 = CARTESIAN_POINT ( 'NONE',  ( 7.000000000000000000, 0.000000000000000000, 0.000000000000000000 ) ) ;
#4669 = CARTESIAN_POINT ( 'NONE',  ( 8.952784697134999803, 4.470490447737899942, -6.771750947090999340 ) ) ;
#4671 = PLANE ( 'NONE',  #20567 ) ;
#4670 = CARTESIAN_POINT ( 'NONE',  ( 10.53495058442699950, -3.601336184534900120, 8.421905343605699201 ) ) ;
#4672 = CARTESIAN_POINT ( 'NONE',  ( 7.861945368778997079, -2.855203060631998024, 6.787771340568003353 ) ) ;
#4673 = EDGE_LOOP ( 'NONE', ( #62440, #23823, #22596, #11693 ) ) ;
#4674 = CARTESIAN_POINT ( 'NONE',  ( 9.654346873515669003, 5.250000000000002665, -7.336375382625537789 ) ) ;
#4675 = LINE ( 'NONE', #51891, #31831 ) ;
#4676 = CARTESIAN_POINT ( 'NONE',  ( 9.836342523874998633, 2.735516931877000513, 7.693563834190999984 ) ) ;
#4677 = CARTESIAN_POINT ( 'NONE',  ( 12.80505043854143388, 3.166049082260463443, 13.55318600037536925 ) ) ;
#4678 = CARTESIAN_POINT ( 'NONE',  ( 10.55991645936999923, -5.094263939633999705, 6.075409946530999861 ) ) ;
#4679 = EDGE_CURVE ( 'NONE', #47743, #6658, #10511, .T. ) ;
#4680 = CARTESIAN_POINT ( 'NONE',  ( 17.92118024654437036, 3.006907963399584549, -12.31891425463943079 ) ) ;
#4681 = CARTESIAN_POINT ( 'NONE',  ( 15.86018463513499910, -3.716003765078999876, -11.29289727949000088 ) ) ;
#4682 = DIRECTION ( 'NONE',  ( -1.000000000000000000, 0.000000000000000000, 0.000000000000000000 ) ) ;
#4683 = CARTESIAN_POINT ( 'NONE',  ( 5.500000000000000000, 11.95749337870000062, 3.642574926947999892 ) ) ;
#4684 = CARTESIAN_POINT ( 'NONE',  ( 9.054101285863998427, -4.558267473659599389, -6.836640842107200022 ) ) ;
#4685 = CIRCLE ( 'NONE', #43789, 0.8000000000000000444 ) ;
#4686 = CARTESIAN_POINT ( 'NONE',  ( 6.664531036635000127, 0.6479012572794000668, 0.9815235057283998588 ) ) ;
#4687 = CARTESIAN_POINT ( 'NONE',  ( 11.32145113417867677, -3.276884167680957027, 7.008885863206549161 ) ) ;
#4688 = CARTESIAN_POINT ( 'NONE',  ( 8.748821772879614045, 4.302364887094737966, -8.374063393888503626 ) ) ;
#4689 = CARTESIAN_POINT ( 'NONE',  ( 2.585745976258000400, -2.924233445111000140, -1.438799925142999925 ) ) ;
#4690 = ORIENTED_EDGE ( 'NONE', *, *, #830, .F. ) ;
#4691 = CARTESIAN_POINT ( 'NONE',  ( 12.18006454708593544, -0.02081145935391386093, -12.69999906470294526 ) ) ;
#4692 = CARTESIAN_POINT ( 'NONE',  ( 12.35392836372401426, -2.932699513115810230, -12.34015408322826168 ) ) ;
#4693 = CARTESIAN_POINT ( 'NONE',  ( 23.60000000000000142, 11.77655473258999841, 4.190794510628000680 ) ) ;
#4694 = CARTESIAN_POINT ( 'NONE',  ( 10.90000000000000036, -5.283926297003000094, 7.082827057608000132 ) ) ;
#4695 = LINE ( 'NONE', #36878, #57212 ) ;
#4696 = ORIENTED_EDGE ( 'NONE', *, *, #39099, .T. ) ;
#4697 = CARTESIAN_POINT ( 'NONE',  ( 5.593964071046000797, 1.139611800844000156, 0.2906295266426999757 ) ) ;
#4698 = CARTESIAN_POINT ( 'NONE',  ( 11.47500581613029880, -3.011381429075500105, -8.134817373646898275 ) ) ;
#4699 = CARTESIAN_POINT ( 'NONE',  ( 10.97034794368816435, 8.644975688278298875, 6.526274310569194270 ) ) ;
#4700 = CARTESIAN_POINT ( 'NONE',  ( 12.99421883851900184, -11.64667883987999986, -1.861676925984000031 ) ) ;
#4701 = CARTESIAN_POINT ( 'NONE',  ( 5.699999999579000054, -0.3000000004212000082, -9.662944680462999258 ) ) ;
#4703 = VECTOR ( 'NONE', #64077, 1000.000000000000000 ) ;
#4702 = CARTESIAN_POINT ( 'NONE',  ( 10.48280513895999988, 4.903310631086600146, -6.997844089834400094 ) ) ;
#4704 = ORIENTED_EDGE ( 'NONE', *, *, #17398, .T. ) ;
#4705 = CARTESIAN_POINT ( 'NONE',  ( 11.02445830383999947, -3.404091099119999519, 5.822494319281999786 ) ) ;
#4706 = ORIENTED_EDGE ( 'NONE', *, *, #66046, .F. ) ;
#4707 = CARTESIAN_POINT ( 'NONE',  ( 11.87077408945317103, -5.183263708087437749, 7.086869749530762874 ) ) ;
#4708 = CARTESIAN_POINT ( 'NONE',  ( 7.518870559622000016, -3.206365290996999740, 5.681739161071000410 ) ) ;
#4709 = AXIS2_PLACEMENT_3D ( 'NONE', #58932, #21518, #53687 ) ;
#4710 = CARTESIAN_POINT ( 'NONE',  ( 16.00429364930199938, 8.559608311085998622, 7.983357056237001537 ) ) ;
#4711 = ORIENTED_EDGE ( 'NONE', *, *, #49497, .T. ) ;
#4712 = CARTESIAN_POINT ( 'NONE',  ( 23.66004879239100234, 9.998911746292000302, 9.691526727427998367 ) ) ;
#4713 = CARTESIAN_POINT ( 'NONE',  ( 7.382754719588999315, 2.727583171400000062, -8.411095346025000197 ) ) ;
#4714 = DIRECTION ( 'NONE',  ( 0.000000000000000000, 0.000000000000000000, 1.000000000000000000 ) ) ;
#4715 = CARTESIAN_POINT ( 'NONE',  ( 17.86968310087778278, -3.040418749906950158, 12.30910170914067514 ) ) ;
#4716 = VERTEX_POINT ( 'NONE', #41764 ) ;
#4717 = CARTESIAN_POINT ( 'NONE',  ( 10.62197618263000010, -5.779779175739000685, 7.256573549370999743 ) ) ;
#4718 = EDGE_CURVE ( 'NONE', #11189, #64219, #42799, .T. ) ;
#4719 = EDGE_CURVE ( 'NONE', #28231, #64377, #34325, .T. ) ;
#4720 = CARTESIAN_POINT ( 'NONE',  ( 25.37646601934299895, 11.10818569620999874, -3.395594564468000343 ) ) ;
#4722 = CARTESIAN_POINT ( 'NONE',  ( 12.45594992591494155, 11.44468663792899754, -4.547234112432383846 ) ) ;
#4721 = B_SPLINE_CURVE_WITH_KNOTS ( 'NONE', 3,
 ( #36185, #57159, #9957, #25691 ),
 .UNSPECIFIED., .F., .F.,
 ( 4, 4 ),
 ( 0.000000000000000000, 1.000000000000000000 ),
 .UNSPECIFIED. ) ;
#4723 = ORIENTED_EDGE ( 'NONE', *, *, #66656, .T. ) ;
#4724 = CARTESIAN_POINT ( 'NONE',  ( 9.022731225801246424, 2.899999999999999911, -6.450252854620909027 ) ) ;
#4725 = ORIENTED_EDGE ( 'NONE', *, *, #62270, .T. ) ;
#4726 = CARTESIAN_POINT ( 'NONE',  ( 4.953413393859332992, 0.4964519701263341855, 1.434320509598690840 ) ) ;
#4727 = CARTESIAN_POINT ( 'NONE',  ( 10.88582469064355784, 2.779316614152869569, 8.789661958747668535 ) ) ;
#4728 = CARTESIAN_POINT ( 'NONE',  ( 17.74668184667432413, -0.5949840079737200860, -12.68123264482376555 ) ) ;
#4729 = CYLINDRICAL_SURFACE ( 'NONE', #47769, 0.6250000000000005551 ) ;
#4730 = CARTESIAN_POINT ( 'NONE',  ( 3.999999173945999686, 0.000000000000000000, 0.000000000000000000 ) ) ;
#4731 = LINE ( 'NONE', #57887, #28798 ) ;
#4732 = CARTESIAN_POINT ( 'NONE',  ( 12.26307976823773949, 2.811936524129936998, 13.60229516772050573 ) ) ;
#4733 = ORIENTED_EDGE ( 'NONE', *, *, #11225, .F. ) ;
#4734 = CARTESIAN_POINT ( 'NONE',  ( 10.36325056272499978, -3.107965259299500183, -7.513220396995270001 ) ) ;
#4735 = VERTEX_POINT ( 'NONE', #37208 ) ;
#4736 = CARTESIAN_POINT ( 'NONE',  ( 11.09425120759000016, 2.431871068503000277, 7.769513029648000391 ) ) ;
#4737 = CARTESIAN_POINT ( 'NONE',  ( 11.06205165877000063, 2.154392227069000132, -7.605898171884000192 ) ) ;
#4738 = EDGE_CURVE ( 'NONE', #2693, #5374, #36789, .T. ) ;
#4739 = DIRECTION ( 'NONE',  ( 1.000000000000000000, 0.000000000000000000, 0.000000000000000000 ) ) ;
#4740 = CARTESIAN_POINT ( 'NONE',  ( 9.318935841232999451, 2.644017913812000131, -7.838184857420000817 ) ) ;
#4741 = AXIS2_PLACEMENT_3D ( 'NONE', #402, #38497, #1100 ) ;
#4742 = DIRECTION ( 'NONE',  ( 0.000000000000000000, -0.9999808993455937545, -0.006180691221632959691 ) ) ;
#4743 = EDGE_CURVE ( 'NONE', #38406, #14135, #52593, .T. ) ;
#4744 = CARTESIAN_POINT ( 'NONE',  ( 25.60000000000000142, -10.55163788719000095, -3.754896668835000284 ) ) ;
#4745 = CARTESIAN_POINT ( 'NONE',  ( 18.16373243908211776, 0.1422577892986753023, 13.89902525486551887 ) ) ;
#4746 = CARTESIAN_POINT ( 'NONE',  ( 9.350151960951233576, -5.734349002094055514, -7.726429600794550545 ) ) ;
#4747 = B_SPLINE_CURVE_WITH_KNOTS ( 'NONE', 3,
 ( #57548, #57900, #31337, #9651 ),
 .UNSPECIFIED., .F., .F.,
 ( 4, 4 ),
 ( 0.000000000000000000, 1.000000000000000000 ),
 .UNSPECIFIED. ) ;
#4748 = B_SPLINE_CURVE_WITH_KNOTS ( 'NONE', 3,
 ( #34337, #54957, #55305, #7059, #49710, #17905, #17556, #38882, #55654, #17196, #7402, #1818, #23137, #12655, #12308, #44488, #29096, #59849 ),
 .UNSPECIFIED., .F., .F.,
 ( 4, 2, 2, 2, 2, 2, 2, 2, 4 ),
 ( 0.000000000000000000, 0.1250000000000000000, 0.2500000000000000000, 0.3750000000000000000, 0.5000000000000000000, 0.6250000000000000000, 0.7500000000000000000, 0.8750000000000000000, 1.000000000000000000 ),
 .UNSPECIFIED. ) ;
#4749 = ORIENTED_EDGE ( 'NONE', *, *, #6953, .F. ) ;
#4750 = CARTESIAN_POINT ( 'NONE',  ( 12.68949153424100196, -11.39033517652999983, 4.571431300619999583 ) ) ;
#4751 = CARTESIAN_POINT ( 'NONE',  ( 11.80579707368350029, -4.634832087857400751, 8.609190966793999422 ) ) ;
#4752 = FACE_OUTER_BOUND ( 'NONE', #4871, .T. ) ;
#4753 = CARTESIAN_POINT ( 'NONE',  ( 15.77677363193000204, 9.321312496448001639, 8.284802892401000207 ) ) ;
#4754 = CARTESIAN_POINT ( 'NONE',  ( 7.475043146792000215, -3.276313010012999793, 5.841993238691999935 ) ) ;
#4756 = LINE ( 'NONE', #57211, #54052 ) ;
#4755 = CARTESIAN_POINT ( 'NONE',  ( 11.06923869026000062, 5.425682056982999768, 8.012911262916999178 ) ) ;
#4757 = CIRCLE ( 'NONE', #24839, 12.49999909015999577 ) ;
#4758 = CARTESIAN_POINT ( 'NONE',  ( 10.69456919669529960, 5.093991349577000172, -7.823222900359999343 ) ) ;
#4759 = CARTESIAN_POINT ( 'NONE',  ( 21.00000000000000000, -11.79499999999999993, 0.000000000000000000 ) ) ;
#4760 = CARTESIAN_POINT ( 'NONE',  ( 9.374380199233998567, 4.860242402105300563, -7.391875284387199763 ) ) ;
#4761 = CARTESIAN_POINT ( 'NONE',  ( 17.97798751929653704, 0.5846869236304546025, 12.58643362292763612 ) ) ;
#4762 = CARTESIAN_POINT ( 'NONE',  ( 7.068995775811000470, -1.403536588851999944, 0.5576917437232999930 ) ) ;
#4763 = CYLINDRICAL_SURFACE ( 'NONE', #36594, 2.700000000000000178 ) ;
#4764 = ORIENTED_EDGE ( 'NONE', *, *, #13690, .T. ) ;
#4765 = CARTESIAN_POINT ( 'NONE',  ( 7.454683059621999952, -2.138201851198999748, 6.814774777484000623 ) ) ;
#4766 = CARTESIAN_POINT ( 'NONE',  ( 9.807804719590000886, 3.988943694240999704, -8.966360307350999648 ) ) ;
#4767 = CARTESIAN_POINT ( 'NONE',  ( 17.97915611674147129, 3.110288500502087494, 13.65013405122916268 ) ) ;
#4768 = CARTESIAN_POINT ( 'NONE',  ( 1.000973465875999890, 3.500000000000000000, 0.000000000000000000 ) ) ;
#4769 = EDGE_LOOP ( 'NONE', ( #21350, #13848, #33094, #56494, #30396 ) ) ;
#4770 = B_SPLINE_CURVE_WITH_KNOTS ( 'NONE', 3,
 ( #65749, #50028, #44792, #61546, #23455, #12977, #45474, #34299, #40562, #29062 ),
 .UNSPECIFIED., .F., .F.,
 ( 4, 2, 2, 2, 4 ),
 ( 0.7033810150431129005, 0.7404583881627235797, 0.7775357612823343700, 0.8516905075215559506, 1.000000000000000000 ),
 .UNSPECIFIED. ) ;
#4771 = CARTESIAN_POINT ( 'NONE',  ( 18.04816728597000264, 3.610133590554000182, 12.03375048192000207 ) ) ;
#4772 = CARTESIAN_POINT ( 'NONE',  ( 10.43614141025499897, 4.549633050978300730, 6.521048559232099251 ) ) ;
#4773 = CARTESIAN_POINT ( 'NONE',  ( 11.12964528040999923, 3.869081149487999749, -9.017143166339000260 ) ) ;
#4774 = EDGE_CURVE ( 'NONE', #57892, #35475, #16465, .T. ) ;
#4775 = EDGE_LOOP ( 'NONE', ( #973, #997, #21904, #47816 ) ) ;
#4776 = ADVANCED_FACE ( 'NONE', ( #10631 ), #14853, .F. ) ;
#4777 = CARTESIAN_POINT ( 'NONE',  ( 12.44248249217650937, -0.6233258800551970680, -12.58457734799054784 ) ) ;
#4778 = CARTESIAN_POINT ( 'NONE',  ( 10.10478570706233370, 5.131706358131709500, -8.113400509224881318 ) ) ;
#4779 = CARTESIAN_POINT ( 'NONE',  ( 11.52733460557258915, 4.206337284815599986, 6.238754009183999472 ) ) ;
#4780 = CARTESIAN_POINT ( 'NONE',  ( 10.69031285273999821, -5.903020122789000013, 7.830708506196000229 ) ) ;
#4781 = DIRECTION ( 'NONE',  ( -0.7071067811866525998, 0.000000000000000000, -0.7071067811864425456 ) ) ;
#4782 = ORIENTED_EDGE ( 'NONE', *, *, #4863, .T. ) ;
#4783 = CARTESIAN_POINT ( 'NONE',  ( 11.53681523859000002, -3.897571790034000117, 11.94316735528000173 ) ) ;
#4784 = CARTESIAN_POINT ( 'NONE',  ( 7.914964158766999880, 4.624432025063999419, -9.294334464733999823 ) ) ;
#4785 = CARTESIAN_POINT ( 'NONE',  ( 8.254586106814789659, -5.344701609173532653, 8.603696000269675181 ) ) ;
#4786 = CARTESIAN_POINT ( 'NONE',  ( 11.04298866606778162, -4.505418116367177817, -6.786808489985508785 ) ) ;
#4787 = ORIENTED_EDGE ( 'NONE', *, *, #27139, .F. ) ;
#4789 = DIRECTION ( 'NONE',  ( -1.000000000000000000, 0.000000000000000000, 0.000000000000000000 ) ) ;
#4788 = AXIS2_PLACEMENT_3D ( 'NONE', #574, #11394, #26807 ) ;
#4790 = CARTESIAN_POINT ( 'NONE',  ( 11.53937873044000106, 11.52961813267000046, 1.376592384073999975 ) ) ;
#4791 = ORIENTED_EDGE ( 'NONE', *, *, #3685, .F. ) ;
#4792 = FACE_OUTER_BOUND ( 'NONE', #28827, .T. ) ;
#4793 = CARTESIAN_POINT ( 'NONE',  ( 20.75138802851920161, 5.760713961201000544, 0.000000000000000000 ) ) ;
#4794 = ORIENTED_EDGE ( 'NONE', *, *, #62529, .T. ) ;
#4795 = CARTESIAN_POINT ( 'NONE',  ( 8.020125753392001400, 4.498951069075999953, -6.245588651729999441 ) ) ;
#4796 = DIRECTION ( 'NONE',  ( 0.000000000000000000, 1.000000000000000000, 0.000000000000000000 ) ) ;
#4797 = CARTESIAN_POINT ( 'NONE',  ( 10.48419913891000022, -2.939341339380999507, -4.699609182310999778 ) ) ;
#4798 = CARTESIAN_POINT ( 'NONE',  ( 11.14256920625030034, 4.042230905578960254, -6.325872106312999676 ) ) ;
#4799 = CARTESIAN_POINT ( 'NONE',  ( 11.43479632507519916, -3.442212747724900268, 6.465962698293999722 ) ) ;
#4800 = CARTESIAN_POINT ( 'NONE',  ( 4.599999999999999645, 13.17499999999999893, 0.000000000000000000 ) ) ;
#4801 = CARTESIAN_POINT ( 'NONE',  ( 11.44072200990529886, -5.077092948368999714, 7.875713849677398848 ) ) ;
#4802 = CARTESIAN_POINT ( 'NONE',  ( 8.539829719592999524, 5.633477595780999714, 7.451234169193000412 ) ) ;
#4803 = EDGE_CURVE ( 'NONE', #31036, #56100, #53984, .T. ) ;
#4804 = EDGE_CURVE ( 'NONE', #9530, #53691, #50658, .T. ) ;
#4805 = ORIENTED_EDGE ( 'NONE', *, *, #19446, .T. ) ;
#4806 = CARTESIAN_POINT ( 'NONE',  ( 10.84289849785056603, 2.713620053740517957, -7.026897974086664611 ) ) ;
#4807 = AXIS2_PLACEMENT_3D ( 'NONE', #39918, #13352, #67498 ) ;
#4808 = EDGE_CURVE ( 'NONE', #8116, #2756, #12270, .T. ) ;
#4809 = CARTESIAN_POINT ( 'NONE',  ( 9.123558059623999128, -5.558929022707999046, 6.272984818914999927 ) ) ;
#4810 = LINE ( 'NONE', #19869, #56975 ) ;
#4811 = ORIENTED_EDGE ( 'NONE', *, *, #11700, .F. ) ;
#4812 = CARTESIAN_POINT ( 'NONE',  ( 12.59749754106154107, -3.089553852145857427, -12.29445441479364654 ) ) ;
#4813 = VECTOR ( 'NONE', #59778, 1000.000000000000000 ) ;
#4814 = CARTESIAN_POINT ( 'NONE',  ( 11.88107297659999340, 9.756593325465996003, -5.710004264910002014 ) ) ;
#4815 = CARTESIAN_POINT ( 'NONE',  ( 24.35365242081699932, -8.948887819865001703, 8.923422014301001681 ) ) ;
#4816 = DIRECTION ( 'NONE',  ( 0.000000000000000000, 0.000000000000000000, -1.000000000000000000 ) ) ;
#4817 = CARTESIAN_POINT ( 'NONE',  ( 12.51441652845170793, -3.187012454917765858, -13.63242365153888613 ) ) ;
#4818 = CARTESIAN_POINT ( 'NONE',  ( 11.06795257254739973, -4.963546614172099858, -7.780229861306499295 ) ) ;
#4819 = DIRECTION ( 'NONE',  ( 0.000000000000000000, 1.000000000000000000, 0.000000000000000000 ) ) ;
#4820 = CARTESIAN_POINT ( 'NONE',  ( 18.27887336143460928, -2.529852868668394539, 12.34343546511470890 ) ) ;
#4821 = VERTEX_POINT ( 'NONE', #54666 ) ;
#4822 = ORIENTED_EDGE ( 'NONE', *, *, #35989, .F. ) ;
#4823 = DIRECTION ( 'NONE',  ( 0.000000000000000000, 0.000000000000000000, 1.000000000000000000 ) ) ;
#4824 = CARTESIAN_POINT ( 'NONE',  ( 11.73424042080529617, -3.455907502640803042, 8.657883396625685180 ) ) ;
#4825 = CARTESIAN_POINT ( 'NONE',  ( 12.80505043854144098, -0.7302158263239267866, -13.98094363220830871 ) ) ;
#4826 = CARTESIAN_POINT ( 'NONE',  ( 9.780284676292000157, 3.021596928575999819, -8.450035627617001666 ) ) ;
#4827 = EDGE_CURVE ( 'NONE', #52918, #8614, #63138, .T. ) ;
#4828 = DIRECTION ( 'NONE',  ( -0.7070974425254246132, 0.000000000000000000, -0.7071161197243376328 ) ) ;
#4829 = CARTESIAN_POINT ( 'NONE',  ( 18.15011669908943048, 2.691369836981456487, 12.40492163541245674 ) ) ;
#4830 = CARTESIAN_POINT ( 'NONE',  ( 23.83547933438500266, -13.04069008200000113, 3.622007013137000353 ) ) ;
#4831 = CARTESIAN_POINT ( 'NONE',  ( 16.39999999485600313, 3.595156957901000094, 11.99794989424000136 ) ) ;
#4832 = VERTEX_POINT ( 'NONE', #54314 ) ;
#4833 = CARTESIAN_POINT ( 'NONE',  ( 10.32322128467999889, -4.600000125420001140, -4.621083553505000552 ) ) ;
#4834 = ORIENTED_EDGE ( 'NONE', *, *, #28863, .F. ) ;
#4835 = CARTESIAN_POINT ( 'NONE',  ( 12.32688384993705455, -2.902596799746487211, 12.34862005174977462 ) ) ;
#4836 = CARTESIAN_POINT ( 'NONE',  ( 9.121088727410999297, -4.863977618062000019, -7.572461161969050281 ) ) ;
#4837 = VECTOR ( 'NONE', #30973, 1000.000000000000000 ) ;
#4838 = CARTESIAN_POINT ( 'NONE',  ( 10.16829701902000060, 4.567214950372999738, 5.832525041908999341 ) ) ;
#4839 = CARTESIAN_POINT ( 'NONE',  ( 11.81900581613029999, -3.249313226592100534, 7.017964743997199939 ) ) ;
#4840 = CARTESIAN_POINT ( 'NONE',  ( 7.024999999999923084, 5.339057002848925926, -8.130112396048053469 ) ) ;
#4841 = AXIS2_PLACEMENT_3D ( 'NONE', #37703, #26879, #48195 ) ;
#4842 = CARTESIAN_POINT ( 'NONE',  ( 11.76133460557259980, 4.139849081322200419, -8.354833838171700222 ) ) ;
#4843 = CARTESIAN_POINT ( 'NONE',  ( 10.66579975933730040, 5.208485784810999775, -7.084213409908699965 ) ) ;
#4844 = CARTESIAN_POINT ( 'NONE',  ( 11.04498420206273224, 2.508453239880112928, -8.445281263845473063 ) ) ;
#4845 = CARTESIAN_POINT ( 'NONE',  ( 5.602673821509172036, -12.13104802960947914, -3.749633869517229101 ) ) ;
#4846 = DIRECTION ( 'NONE',  ( 1.000000000000000000, 0.000000000000000000, 0.000000000000000000 ) ) ;
#4847 = CARTESIAN_POINT ( 'NONE',  ( 9.167130263679302615, -2.992093955605813260, 8.398819266328139577 ) ) ;
#4848 = ORIENTED_EDGE ( 'NONE', *, *, #55092, .T. ) ;
#4849 = CARTESIAN_POINT ( 'NONE',  ( 10.07367028041000090, 4.905765359186999852, -8.776126235875999271 ) ) ;
#4850 = CARTESIAN_POINT ( 'NONE',  ( 1.700000000000000178, 0.000000000000000000, 0.000000000000000000 ) ) ;
#4851 = FACE_OUTER_BOUND ( 'NONE', #51598, .T. ) ;
#4852 = FACE_OUTER_BOUND ( 'NONE', #20720, .T. ) ;
#4853 = CARTESIAN_POINT ( 'NONE',  ( 12.10000000000000142, -4.569820763625129345, 8.269794803757207546 ) ) ;
#4854 = CARTESIAN_POINT ( 'NONE',  ( 10.64533863405319991, -3.296214805808900028, -8.397761948794601139 ) ) ;
#4855 = ORIENTED_EDGE ( 'NONE', *, *, #17354, .T. ) ;
#4856 = CONICAL_SURFACE ( 'NONE', #51728, 1.349999999648999971, 0.7853981633972997312 ) ;
#4857 = CARTESIAN_POINT ( 'NONE',  ( 5.629847151468639233, -12.10477468259465184, 3.742618271631878102 ) ) ;
#4858 = PLANE ( 'NONE',  #51220 ) ;
#4859 = AXIS2_PLACEMENT_3D ( 'NONE', #9053, #2782, #36313 ) ;
#4861 = CARTESIAN_POINT ( 'NONE',  ( 13.94794651623100101, -9.527030574842997979, -8.190375113092999371 ) ) ;
#4860 = CARTESIAN_POINT ( 'NONE',  ( 9.890475510420877470, 2.705325637622069124, 8.717411133782642096 ) ) ;
#4862 = DIRECTION ( 'NONE',  ( -1.000000000000000000, 0.000000000000000000, 0.000000000000000000 ) ) ;
#4863 = EDGE_CURVE ( 'NONE', #10153, #32857, #22845, .T. ) ;
#4864 = ORIENTED_EDGE ( 'NONE', *, *, #48779, .T. ) ;
#4865 = EDGE_CURVE ( 'NONE', #67307, #56244, #22790, .T. ) ;
#4866 = CARTESIAN_POINT ( 'NONE',  ( 10.53734212242000012, 2.992816679959000137, 8.731689474572998932 ) ) ;
#4867 = CARTESIAN_POINT ( 'NONE',  ( 18.15991033943444677, -2.341318227119850270, -13.70580147614464295 ) ) ;
#4868 = CARTESIAN_POINT ( 'NONE',  ( 10.82595391537419971, 4.716560378569699452, 7.013338090450799811 ) ) ;
#4869 = CARTESIAN_POINT ( 'NONE',  ( 24.87155164401192664, -11.61820474743187681, 3.203191883057006084 ) ) ;
#4870 = CARTESIAN_POINT ( 'NONE',  ( 8.989144353209001181, -5.284133759825000887, 6.489273023403000273 ) ) ;
#4871 = EDGE_LOOP ( 'NONE', ( #24194, #30693, #7713, #10149, #45409, #9140 ) ) ;
#4872 = CARTESIAN_POINT ( 'NONE',  ( 8.866801658774001282, 2.550580605805000012, 8.854682662413999594 ) ) ;
#4874 = CARTESIAN_POINT ( 'NONE',  ( 10.56984555961999916, -2.152868447761999704, -7.425101130468999777 ) ) ;
#4873 = FACE_OUTER_BOUND ( 'NONE', #32951, .T. ) ;
#4875 = CARTESIAN_POINT ( 'NONE',  ( 7.570875225191677771, -3.932046780718525980, 5.759964130382589254 ) ) ;
#4876 = DIRECTION ( 'NONE',  ( 0.000000000000000000, 0.9659258262890756397, -0.2588190451024934280 ) ) ;
#4877 = CARTESIAN_POINT ( 'NONE',  ( 7.400000000000000355, 0.000000000000000000, 0.000000000000000000 ) ) ;
#4878 = VERTEX_POINT ( 'NONE', #59560 ) ;
#4879 = CARTESIAN_POINT ( 'NONE',  ( 5.615443173016667622, -1.500000000000000222, -0.1963495408493622085 ) ) ;
#4880 = CARTESIAN_POINT ( 'NONE',  ( 11.27672335273219950, -3.698477709264200275, 6.687976048055599421 ) ) ;
#4881 = PLANE ( 'NONE',  #42001 ) ;
#4882 = CARTESIAN_POINT ( 'NONE',  ( 11.72001955157836406, 12.39031618367868148, 1.831854259322070133 ) ) ;
#4883 = CARTESIAN_POINT ( 'NONE',  ( 10.59610807141099897, 4.052703327804870526, 6.360477084256999980 ) ) ;
#4884 = ORIENTED_EDGE ( 'NONE', *, *, #19257, .F. ) ;
#4885 = B_SPLINE_SURFACE_WITH_KNOTS ( 'NONE', 3, 3, ( 
 ( #38024, #31417, #58666, #68450, #25820, #64242, #36661, #27203, #15333, #57982, #16357, #52733, #11118, #5180, #10767, #5525, #32451, #48524, #633, #21942, #28945, #43977, #60047, #28591, #12500, #13204, #61084, #65627, #43632, #60735, #6900, #38374, #33833, #22292, #64926 ),
 ( #18097, #28236, #17396, #44329, #39416, #1664, #27900, #980, #17042, #6557, #1316, #44675, #49209, #38725, #22633, #59698, #49552, #65283, #34178, #7250, #12157, #33488, #49903, #54801, #45013, #22981, #66318, #17752, #55496, #18441, #2012, #7596, #50250, #39072, #55147 ),
 ( #60395, #23334, #27545, #39766, #2352, #23675, #12849, #11800, #65969, #34532, #6203, #48872, #33139, #54455, #34864, #45356, #3712, #66665, #2698, #41477, #19809, #45698, #61429, #25049, #4055, #14907, #67007, #61765, #56871, #56180, #25390, #3036, #35213, #62786, #9304 ),
 ( #46036, #24022, #41139, #56525, #18784, #62108, #40115, #13545, #13883, #24367, #46728, #30645, #51280, #14227, #8630, #8291, #51616, #40438, #68034, #40783, #29636, #20150, #7945, #55841, #51954, #24712, #35554, #29978, #29282, #50596, #50939, #19116, #3375, #67341, #19463 ) ),
 .UNSPECIFIED., .F., .F., .F.,
 ( 4, 4 ),
 ( 4, 1, 1, 1, 1, 1, 1, 1, 1, 1, 1, 1, 1, 1, 1, 1, 1, 1, 1, 1, 1, 1, 1, 1, 1, 1, 1, 1, 1, 1, 1, 1, 4 ),
 ( -0.1039086239011999951, 1.103908623900999864 ),
 ( 0.1942321073450000157, 0.2199060843169000079, 0.2455800612886999967, 0.2712540382605999612, 0.2969280152323999777, 0.3226019922043000254, 0.3482759691761000420, 0.3739499461479999787, 0.3996239231197999953, 0.4252979000916999874, 0.4509718770635000040, 0.4766458540353999962, 0.5023198310072000128, 0.5279938079791000050, 0.5536677849509000771, 0.5793417619227999582, 0.6050157388945999193, 0.6306897158665000225, 0.6563636928382999836, 0.6820376698101999757, 0.7077116467820000478, 0.7333856237539000400, 0.7590596007256998901, 0.7847335776975999933, 0.8104075546693999543, 0.8360815316413000575, 0.8617555086131000186, 0.8874294855850000108, 0.9131034625568000829, 0.9387774395286999640, 0.9644514165004999251, 0.9901253934722999972, 1.015799370444000038 ),
 .UNSPECIFIED. ) ;
#4886 = CARTESIAN_POINT ( 'NONE',  ( 23.76527432394305706, -3.280151047146071974, 13.20034468938107608 ) ) ;
#4887 = B_SPLINE_CURVE_WITH_KNOTS ( 'NONE', 1,
 ( #36447, #9875 ),
 .UNSPECIFIED., .F., .F.,
 ( 2, 2 ),
 ( 0.000000000000000000, 1.000000000000000000 ),
 .UNSPECIFIED. ) ;
#4888 = CARTESIAN_POINT ( 'NONE',  ( 12.51375467530090191, 1.821335011922586844, -12.46766859972881392 ) ) ;
#4889 = CARTESIAN_POINT ( 'NONE',  ( 11.09725056272499977, -2.683866746800999792, 7.480494252843770120 ) ) ;
#4890 = CARTESIAN_POINT ( 'NONE',  ( 24.30001697071400457, -8.938702858184001343, 8.938676113071998941 ) ) ;
#4891 = AXIS2_PLACEMENT_3D ( 'NONE', #43633, #5526, #27901 ) ;
#4892 = CARTESIAN_POINT ( 'NONE',  ( 17.55505043854147118, -1.787816316115923509, 13.88537766212463254 ) ) ;
#4894 = ADVANCED_FACE ( 'NONE', ( #43138 ), #17616, .T. ) ;
#4893 = CARTESIAN_POINT ( 'NONE',  ( 18.10276869592869176, 2.801190086637412868, -13.60495303824969149 ) ) ;
#4895 = ORIENTED_EDGE ( 'NONE', *, *, #26187, .T. ) ;
#4896 = CARTESIAN_POINT ( 'NONE',  ( 10.93937577273821482, 3.538822733277925181, 6.300114087089554893 ) ) ;
#4897 = CARTESIAN_POINT ( 'NONE',  ( 13.12628980020838654, -12.15998242465562029, -2.000325904698448287 ) ) ;
#4898 = ORIENTED_EDGE ( 'NONE', *, *, #51983, .F. ) ;
#4899 = CARTESIAN_POINT ( 'NONE',  ( 8.571413182547999554, 4.599999999999999645, 5.927302706106000407 ) ) ;
#4900 = CARTESIAN_POINT ( 'NONE',  ( 11.26902897915239876, 4.221721321201099997, 6.662660017635100296 ) ) ;
#4901 = CARTESIAN_POINT ( 'NONE',  ( 10.31667774810000004, 3.819530253758000260, 6.062195927068000145 ) ) ;
#4902 = CARTESIAN_POINT ( 'NONE',  ( 10.57793656291999973, 4.393379542724999531, -6.024362243994999311 ) ) ;
#4903 = CARTESIAN_POINT ( 'NONE',  ( 8.200215090286000930, 5.110410283172001300, 6.692116316553004651 ) ) ;
#4904 = CARTESIAN_POINT ( 'NONE',  ( 9.834153701540001791, -5.173926576843999925, 8.813045240277000758 ) ) ;
#4905 = CARTESIAN_POINT ( 'NONE',  ( 18.06292190248829499, 0.3644117276601265831, -12.69296657371244841 ) ) ;
#4906 = CARTESIAN_POINT ( 'NONE',  ( 9.039804132582757390, 4.929468674194135147, 8.478882605368561087 ) ) ;
#4907 = CARTESIAN_POINT ( 'NONE',  ( 11.41256651104150066, -3.901000349726440053, -6.501426055769400136 ) ) ;
#4908 = CARTESIAN_POINT ( 'NONE',  ( 8.919607780412000864, 5.165497731316000873, 8.645531386060000045 ) ) ;
#4909 = ORIENTED_EDGE ( 'NONE', *, *, #18148, .F. ) ;
#4910 = COLOUR_RGB ( '', 0.40784314, 0.44705882, 0.49803922) ;
#4911 = SURFACE_STYLE_USAGE ( .BOTH. , #43709 ) ;
#4912 = CARTESIAN_POINT ( 'NONE',  ( 24.81123736889670184, -3.073480331628497542, 11.71258898044826324 ) ) ;
#4913 = CARTESIAN_POINT ( 'NONE',  ( 9.227928106276422682, 2.649889033192923016, 7.452433103127532377 ) ) ;
#4914 = CARTESIAN_POINT ( 'NONE',  ( 8.598411888655869362, 2.943885513252815667, -6.252349181257627286 ) ) ;
#4915 = B_SPLINE_CURVE_WITH_KNOTS ( 'NONE', 3,
 ( #4348, #68315, #59558, #6070, #42797, #53964, #5723, #64440, #21462, #53630, #31975, #26726, #4687, #16902, #27407, #32653, #16564, #42112, #21127, #5039, #26378, #5388, #26028, #52592, #48382, #63417, #11314, #836, #22151, #490, #68663, #37891, #15541, #31622, #48040 ),
 .UNSPECIFIED., .F., .F.,
 ( 4, 1, 1, 1, 1, 1, 1, 1, 1, 1, 1, 1, 1, 1, 1, 1, 1, 1, 1, 1, 1, 1, 1, 1, 1, 1, 1, 1, 1, 1, 1, 1, 4 ),
 ( 0.000000000000000000, 0.02634724210002143546, 0.05799096732718442282, 0.08963469255434740324, 0.1212784177813101688, 0.1529221430084731492, 0.1845658682354359148, 0.2162095934625989091, 0.2478533186897619034, 0.2794970439167246412, 0.3111407691438876633, 0.3427844943710506298, 0.3744282195980133676, 0.4060719448251763897, 0.4377156700521391275, 0.4693593952793021495, 0.5010031205064651161, 0.5326468457334281315, 0.5642905709605910980, 0.5959342961875536693, 0.6275780214147168579, 0.6592217466418798244, 0.6908654718688423957, 0.7225091970960055843, 0.7541529223229681556, 0.7857966475501313441, 0.8174403727772943107, 0.8490840980042568820, 0.8807278232314200705, 0.9123715484585830371, 0.9440152736855456084, 0.9756589989127087970, 1.000000000000000000 ),
 .UNSPECIFIED. ) ;
#4916 = EDGE_CURVE ( 'NONE', #52535, #31379, #56470, .T. ) ;
#4917 = VECTOR ( 'NONE', #23558, 1000.000000000000000 ) ;
#4918 = CARTESIAN_POINT ( 'NONE',  ( 10.90664291662000451, 8.258660472640997341, 7.032076946551004681 ) ) ;
#4919 = CARTESIAN_POINT ( 'NONE',  ( 11.29998578400000042, -3.824193979571000046, 11.71675423233000046 ) ) ;
#4920 = CARTESIAN_POINT ( 'NONE',  ( 11.12455253368000108, 7.320617754035000146, 6.383266958155999760 ) ) ;
#4921 = CARTESIAN_POINT ( 'NONE',  ( 12.44873997953563105, -0.5136077743616320745, -12.68601957541463676 ) ) ;
#4922 = VECTOR ( 'NONE', #51487, 1000.000000000000000 ) ;
#4923 = CARTESIAN_POINT ( 'NONE',  ( 21.72233714749290101, 0.000000000000000000, 0.000000000000000000 ) ) ;
#4924 = ORIENTED_EDGE ( 'NONE', *, *, #44537, .F. ) ;
#4925 = CARTESIAN_POINT ( 'NONE',  ( 12.51375467530093921, -1.821335011922595282, 12.46766859972881569 ) ) ;
#4926 = CARTESIAN_POINT ( 'NONE',  ( 9.735025935145998233, -4.185743043590700374, -6.234344474498000110 ) ) ;
#4927 = CARTESIAN_POINT ( 'NONE',  ( 11.10000000009000054, 5.300000000088999741, -6.571291220400000022 ) ) ;
#4928 = B_SPLINE_CURVE_WITH_KNOTS ( 'NONE', 3,
 ( #45444, #66757, #39504, #3462 ),
 .UNSPECIFIED., .F., .F.,
 ( 4, 4 ),
 ( 0.000000000000000000, 1.000000000000000000 ),
 .UNSPECIFIED. ) ;
#4929 = CARTESIAN_POINT ( 'NONE',  ( 9.848732933287999813, -2.769734897491000325, 6.441850735262000249 ) ) ;
#4930 = CARTESIAN_POINT ( 'NONE',  ( 11.47364560330029981, -3.734560974198899874, 8.324524538096799375 ) ) ;
#4931 = CARTESIAN_POINT ( 'NONE',  ( 12.09898038912534091, 0.1637242582067924557, 12.59894148523291157 ) ) ;
#4932 = CARTESIAN_POINT ( 'NONE',  ( 0.5240331185627999933, -2.301202007355999779, -2.466905145517999998 ) ) ;
#4933 = CARTESIAN_POINT ( 'NONE',  ( 5.136371739860884134, 0.9084939932534207285, 0.7817311076636899170 ) ) ;
#4934 = CARTESIAN_POINT ( 'NONE',  ( 12.09087492024910304, 2.355317862440506449, 12.37790828721919389 ) ) ;
#4935 = DIRECTION ( 'NONE',  ( 1.000000000000000000, 0.000000000000000000, 0.000000000000000000 ) ) ;
#4936 = CARTESIAN_POINT ( 'NONE',  ( 11.36333594839950045, 4.659759757475400832, -6.743912759487099784 ) ) ;
#4937 = CARTESIAN_POINT ( 'NONE',  ( 12.68583900965842481, 11.53041019655173294, -4.891346001956314637 ) ) ;
#4938 = B_SPLINE_CURVE_WITH_KNOTS ( 'NONE', 3,
 ( #41648, #20321, #10181, #20670 ),
 .UNSPECIFIED., .F., .F.,
 ( 4, 4 ),
 ( 0.000000000000000000, 1.000000000000000000 ),
 .UNSPECIFIED. ) ;
#4939 = B_SPLINE_CURVE_WITH_KNOTS ( 'NONE', 3,
 ( #1444, #48649, #58788, #26983 ),
 .UNSPECIFIED., .F., .F.,
 ( 4, 4 ),
 ( 0.000000000000000000, 1.000000000000000000 ),
 .UNSPECIFIED. ) ;
#4940 = CARTESIAN_POINT ( 'NONE',  ( 10.88760471959000142, 5.634847467408999222, -7.088990678556999825 ) ) ;
#4941 = CARTESIAN_POINT ( 'NONE',  ( 9.681292290062998518, 5.106256438265999620, -6.857675253263499471 ) ) ;
#4943 = CARTESIAN_POINT ( 'NONE',  ( 12.19364288186088352, 2.630035215285695394, 12.42031982010608182 ) ) ;
#4942 = CARTESIAN_POINT ( 'NONE',  ( 9.099999931440999390, -2.935682118448999844, -8.155535999783198875 ) ) ;
#4944 = DIRECTION ( 'NONE',  ( -1.000000000000000000, 0.000000000000000000, 0.000000000000000000 ) ) ;
#4945 = ORIENTED_EDGE ( 'NONE', *, *, #21994, .T. ) ;
#4946 = AXIS2_PLACEMENT_3D ( 'NONE', #5710, #64086, #53270 ) ;
#4947 = CARTESIAN_POINT ( 'NONE',  ( 0.7857456912831999318, 2.980225901380999964, 1.319047437492999908 ) ) ;
#4948 = LINE ( 'NONE', #26285, #17743 ) ;
#4949 = CARTESIAN_POINT ( 'NONE',  ( 9.448736632827984039, 4.355932816508206962, -9.239297493378444415 ) ) ;
#4950 = CARTESIAN_POINT ( 'NONE',  ( 8.996455549952997899, 4.781695603001899997, 8.130709350565298976 ) ) ;
#4951 = EDGE_CURVE ( 'NONE', #42349, #26060, #49594, .T. ) ;
#4952 = EDGE_CURVE ( 'NONE', #46692, #51958, #28455, .T. ) ;
#4953 = DIRECTION ( 'NONE',  ( 0.000000000000000000, -0.9979497300302145879, 0.06400262754467088422 ) ) ;
#4954 = CARTESIAN_POINT ( 'NONE',  ( 12.23531288305056819, -2.757742497410567317, 13.61542453244087270 ) ) ;
#4955 = CARTESIAN_POINT ( 'NONE',  ( 12.27940634384846064, 2.838250353088386468, 13.59582428664483267 ) ) ;
#4956 = CARTESIAN_POINT ( 'NONE',  ( 23.74236379950000142, 3.207225084832999951, -13.21247651630999975 ) ) ;
#4957 = ORIENTED_EDGE ( 'NONE', *, *, #32219, .F. ) ;
#4958 = ADVANCED_FACE ( 'NONE', ( #17258 ), #37892, .T. ) ;
#4959 = ADVANCED_FACE ( 'NONE', ( #32654 ), #9482, .F. ) ;
#4960 = CARTESIAN_POINT ( 'NONE',  ( 5.242725847550000040, -0.5733688592043999499, 0.9387623512300999895 ) ) ;
#4961 = AXIS2_PLACEMENT_3D ( 'NONE', #2587, #11691, #23917 ) ;
#4962 = CARTESIAN_POINT ( 'NONE',  ( 8.668126402770999661, -2.803062940908000122, -7.048639765412399782 ) ) ;
#4963 = CARTESIAN_POINT ( 'NONE',  ( 24.67921311619700120, 3.567517360056999820, 12.13750603036999998 ) ) ;
#4964 = DIRECTION ( 'NONE',  ( -1.000000000000000000, 0.000000000000000000, -2.609704304917999919E-14 ) ) ;
#4965 = CARTESIAN_POINT ( 'NONE',  ( 17.94557471909616098, 2.987998163485180214, -12.32438680867656444 ) ) ;
#4966 = CARTESIAN_POINT ( 'NONE',  ( 8.687922088694000067, 3.419384128876999718, -5.860036257779999147 ) ) ;
#4967 = CIRCLE ( 'NONE', #47400, 1.550000000000000044 ) ;
#4968 = CARTESIAN_POINT ( 'NONE',  ( 18.17221331277271190, 2.599179209401793589, 12.42790858716554858 ) ) ;
#4969 = CARTESIAN_POINT ( 'NONE',  ( 8.016657426769000949, 2.906672751340000804, 6.403732826568004910 ) ) ;
#4970 = CARTESIAN_POINT ( 'NONE',  ( 11.00000000000000000, 4.991767524623399233, 7.825000000000000178 ) ) ;
#4971 = CARTESIAN_POINT ( 'NONE',  ( 11.06205805961999999, -2.154403720901000518, -7.605897512385999981 ) ) ;
#4972 = CARTESIAN_POINT ( 'NONE',  ( 9.132625033077360399, -2.794592352501091170, 8.206332652464567445 ) ) ;
#4973 = CARTESIAN_POINT ( 'NONE',  ( 11.50001544675000353, -5.131800296024274566, 11.50030236634318115 ) ) ;
#4974 = CARTESIAN_POINT ( 'NONE',  ( 11.57299956498199833, -2.792989229543000107, 7.174999999999999822 ) ) ;
#4975 = CARTESIAN_POINT ( 'NONE',  ( 8.316694573732000606, -2.898380360490000029, 6.611503418275999522 ) ) ;
#4976 = CARTESIAN_POINT ( 'NONE',  ( 23.55780499550100160, 13.49844004384999963, -4.021617545008000505 ) ) ;
#4977 = EDGE_LOOP ( 'NONE', ( #460, #10966, #17291, #3407, #55069 ) ) ;
#4978 = CARTESIAN_POINT ( 'NONE',  ( 8.266329719591000824, 4.769017407621999993, -8.862909124839001507 ) ) ;
#4979 = CARTESIAN_POINT ( 'NONE',  ( 10.90749413291699987, -3.211956830789300277, 7.859564368461399830 ) ) ;
#4980 = ORIENTED_EDGE ( 'NONE', *, *, #19798, .T. ) ;
#4981 = CARTESIAN_POINT ( 'NONE',  ( 7.961778384057998537, 4.370833349752165198, -6.185172849432923670 ) ) ;
#4982 = CARTESIAN_POINT ( 'NONE',  ( 10.59610807141099897, -3.947296672195129918, -8.639522915742999132 ) ) ;
#4983 = EDGE_LOOP ( 'NONE', ( #14221, #32056, #15892, #8250 ) ) ;
#4984 = CARTESIAN_POINT ( 'NONE',  ( 11.30367835872029936, 2.886444435522000251, 8.201822467543799178 ) ) ;
#4985 = CARTESIAN_POINT ( 'NONE',  ( 7.100000000000000533, 0.000000000000000000, 0.000000000000000000 ) ) ;
#4986 = CARTESIAN_POINT ( 'NONE',  ( 17.88015371777900242, -3.314513509857999640, 11.22393657228000130 ) ) ;
#4987 = DIRECTION ( 'NONE',  ( 0.000000000000000000, 1.000000000000000000, 0.000000000000000000 ) ) ;
#4988 = CARTESIAN_POINT ( 'NONE',  ( 12.80505043854144276, 0.6249999999999994449, -13.88107975066922428 ) ) ;
#4989 = CARTESIAN_POINT ( 'NONE',  ( 7.167068301985500156, 0.5244239808134111280, 1.015631163775551515 ) ) ;
#4990 = CARTESIAN_POINT ( 'NONE',  ( 12.09999922233642344, 11.66744139996707119, -3.971920075670921424 ) ) ;
#4991 = ORIENTED_EDGE ( 'NONE', *, *, #52011, .F. ) ;
#4992 = CARTESIAN_POINT ( 'NONE',  ( 8.681370280410998674, 2.949305648881000330, -8.659807625323999503 ) ) ;
#4993 = VERTEX_POINT ( 'NONE', #24231 ) ;
#4994 = VECTOR ( 'NONE', #35659, 1000.000000000000000 ) ;
#4995 = CARTESIAN_POINT ( 'NONE',  ( 10.68559687351635112, 5.092232985442825210, -6.870476274536379435 ) ) ;
#4996 = EDGE_LOOP ( 'NONE', ( #6712, #64741 ) ) ;
#4997 = CARTESIAN_POINT ( 'NONE',  ( 9.579975701332999805, 4.938486452461599896, 6.630731591496600075 ) ) ;
#4998 = CARTESIAN_POINT ( 'NONE',  ( 18.11139879660522212, -2.784965558754640913, -12.38059455073776682 ) ) ;
#4999 = EDGE_CURVE ( 'NONE', #17060, #5259, #51834, .T. ) ;
#5000 = AXIS2_PLACEMENT_3D ( 'NONE', #26166, #32106, #31759 ) ;
#5001 = CARTESIAN_POINT ( 'NONE',  ( 8.849999778957998942, 4.000000000000000000, -7.500000000000000000 ) ) ;
#5002 = ADVANCED_FACE ( 'NONE', ( #50119 ), #39982, .F. ) ;
#5003 = CARTESIAN_POINT ( 'NONE',  ( 8.461732853997688153, -5.351516129092861895, 7.263730654262129605 ) ) ;
#5004 = DIRECTION ( 'NONE',  ( 1.000000000000000000, 0.000000000000000000, 0.000000000000000000 ) ) ;
#5005 = ORIENTED_EDGE ( 'NONE', *, *, #67862, .T. ) ;
#5006 = CARTESIAN_POINT ( 'NONE',  ( 12.83176788310500172, 11.93188535256000016, -3.261584788209999974 ) ) ;
#5007 = CARTESIAN_POINT ( 'NONE',  ( 17.93554207161599834, 11.52135921566999954, -4.763665720747999544 ) ) ;
#5008 = DIRECTION ( 'NONE',  ( 1.000000000000000000, 0.000000000000000000, 0.000000000000000000 ) ) ;
#5009 = CARTESIAN_POINT ( 'NONE',  ( 7.000000000000000000, -1.250000000000000000, 0.000000000000000000 ) ) ;
#5010 = CARTESIAN_POINT ( 'NONE',  ( 12.71442162208122539, -11.86191914805648118, 3.298674357357659126 ) ) ;
#5011 = CIRCLE ( 'NONE', #9501, 1.249999999999999778 ) ;
#5012 = CARTESIAN_POINT ( 'NONE',  ( 18.14341877109137968, 11.59808500082729843, -4.729434285192278153 ) ) ;
#5013 = CARTESIAN_POINT ( 'NONE',  ( 10.99693800072000016, -2.980603239157999962, -6.418614998350999912 ) ) ;
#5014 = VERTEX_POINT ( 'NONE', #7809 ) ;
#5015 = ORIENTED_EDGE ( 'NONE', *, *, #11738, .F. ) ;
#5016 = LINE ( 'NONE', #42769, #4703 ) ;
#5017 = DIRECTION ( 'NONE',  ( -1.000000000000000000, 0.000000000000000000, 0.000000000000000000 ) ) ;
#5018 = CARTESIAN_POINT ( 'NONE',  ( 18.90826270587400160, 11.15000000000000036, 4.842816425653999965E-11 ) ) ;
#5019 = CARTESIAN_POINT ( 'NONE',  ( 6.052943173016667622, -1.199500263597274685, 0.9218200799623673669 ) ) ;
#5020 = CARTESIAN_POINT ( 'NONE',  ( 10.88813259637009878, 2.844182332072999753, -8.129798612793599943 ) ) ;
#5021 = CARTESIAN_POINT ( 'NONE',  ( 9.003442991499998271, 3.945420918055940085, -6.634708680083400090 ) ) ;
#5023 = CARTESIAN_POINT ( 'NONE',  ( 10.27668195243999882, -3.417616861023999864, 5.003889090935000006 ) ) ;
#5022 = CARTESIAN_POINT ( 'NONE',  ( 9.648430433047000321, -4.854750075120300323, 8.027488966151301142 ) ) ;
#5024 = CARTESIAN_POINT ( 'NONE',  ( 7.684934563448005740, -2.928065616737000720, 6.508603912219004251 ) ) ;
#5025 = ORIENTED_EDGE ( 'NONE', *, *, #34586, .F. ) ;
#5026 = CARTESIAN_POINT ( 'NONE',  ( 5.500000000000000000, 12.22293095105000127, 3.800428736101999938 ) ) ;
#5027 = CARTESIAN_POINT ( 'NONE',  ( 10.41114191524999910, -3.147777059971999414, -4.883851472541000049 ) ) ;
#5028 = CARTESIAN_POINT ( 'NONE',  ( 9.492891187585001944, -4.474581801608000120, -6.279517683005999551 ) ) ;
#5029 = CARTESIAN_POINT ( 'NONE',  ( 25.29995422340600086, 2.596935224161999844, 11.35301931920000129 ) ) ;
#5030 = CARTESIAN_POINT ( 'NONE',  ( 10.89874164595999950, -2.834836218627000193, 9.088455567997000273 ) ) ;
#5031 = CARTESIAN_POINT ( 'NONE',  ( 17.86968310086820111, 3.040418749912511487, -12.30910170913888280 ) ) ;
#5032 = DIRECTION ( 'NONE',  ( 0.000000000000000000, 0.9565994702956989171, -0.2914059941558995170 ) ) ;
#5033 = ADVANCED_FACE ( 'NONE', ( #50809 ), #67213, .T. ) ;
#5034 = EDGE_CURVE ( 'NONE', #68681, #50848, #62325, .T. ) ;
#5035 = CARTESIAN_POINT ( 'NONE',  ( 15.40000000005200143, -9.187454762873001002, -8.213177997099000649 ) ) ;
#5036 = CARTESIAN_POINT ( 'NONE',  ( 7.995310464097279635, 3.151543199498028525, -6.329371383534729389 ) ) ;
#5037 = CARTESIAN_POINT ( 'NONE',  ( 9.510025935145998588, -4.125890936441000356, -6.642177514500700042 ) ) ;
#5038 = CARTESIAN_POINT ( 'NONE',  ( 11.09999999999999964, 5.350000000000000533, -7.500000000000000000 ) ) ;
#5039 = CARTESIAN_POINT ( 'NONE',  ( 11.14914416493166449, -4.811858819934198728, 7.176001761109866095 ) ) ;
#5040 = CARTESIAN_POINT ( 'NONE',  ( 8.330224159023998709, 2.898680183691999979, -6.607597200868999820 ) ) ;
#5041 = CARTESIAN_POINT ( 'NONE',  ( 11.09999999999999964, 5.299316147296000423, -5.124965750789000296 ) ) ;
#5042 = PLANE ( 'NONE',  #29236 ) ;
#5043 = ORIENTED_EDGE ( 'NONE', *, *, #44330, .F. ) ;
#5044 = CARTESIAN_POINT ( 'NONE',  ( 12.20412026884455692, -0.1720826094844762344, -12.69843621396829292 ) ) ;
#5045 = CARTESIAN_POINT ( 'NONE',  ( 10.16052890781999984, -2.899999999999999911, -6.152188490330000370 ) ) ;
#5046 = CARTESIAN_POINT ( 'NONE',  ( 9.461621083092298434, -5.351423275947231772, 7.263649724570567123 ) ) ;
#5047 = DIRECTION ( 'NONE',  ( 0.000000000000000000, -0.1333333333333049375, -0.9910712498212376209 ) ) ;
#5048 = CARTESIAN_POINT ( 'NONE',  ( 8.616332382228000242, -2.832433105983000132, -6.822293595522999077 ) ) ;
#5049 = ORIENTED_EDGE ( 'NONE', *, *, #4605, .F. ) ;
#5050 = CARTESIAN_POINT ( 'NONE',  ( 5.700000000000000178, 0.5292307692307999245, 2.083846153846000249 ) ) ;
#5051 = ITEM_DEFINED_TRANSFORMATION ( 'NONE', 'NONE', #68664,  #9676 ) ;
#5052 = CARTESIAN_POINT ( 'NONE',  ( 10.44635971519499940, -3.540377183549800133, -6.735384833238199143 ) ) ;
#5053 = DIRECTION ( 'NONE',  ( 0.000000000000000000, -0.9897433186107934544, -0.1428571428570991342 ) ) ;
#5054 = EDGE_CURVE ( 'NONE', #13504, #25295, #56395, .T. ) ;
#5055 = CARTESIAN_POINT ( 'NONE',  ( 18.90826270587400160, 0.000000000000000000, 0.000000000000000000 ) ) ;
#5056 = CARTESIAN_POINT ( 'NONE',  ( 7.686568289202588389, 4.059993974225437618, -8.863793664233034164 ) ) ;
#5057 = CARTESIAN_POINT ( 'NONE',  ( 11.52677869730533011, 3.596497913043499750, -6.704332466833498927 ) ) ;
#5058 = ORIENTED_EDGE ( 'NONE', *, *, #51471, .T. ) ;
#5059 = CARTESIAN_POINT ( 'NONE',  ( 9.465112865370999273, -2.290047720994000002, 6.601709978349000529 ) ) ;
#5060 = CARTESIAN_POINT ( 'NONE',  ( 18.11595230660369538, 2.775896237034515490, -13.61106543307219852 ) ) ;
#5061 = EDGE_LOOP ( 'NONE', ( #28240, #68949, #46639 ) ) ;
#5062 = DIRECTION ( 'NONE',  ( 0.000000000000000000, -1.000000000000000000, 0.000000000000000000 ) ) ;
#5063 = CARTESIAN_POINT ( 'NONE',  ( 9.149956853208999874, -4.175914961544999748, 5.699510287082000026 ) ) ;
#5064 = VECTOR ( 'NONE', #64420, 1000.000000000000114 ) ;
#5065 = CARTESIAN_POINT ( 'NONE',  ( 17.85458012075705270, -0.6654101994098823303, -13.98418081573739080 ) ) ;
#5066 = ORIENTED_EDGE ( 'NONE', *, *, #57541, .F. ) ;
#5067 = CARTESIAN_POINT ( 'NONE',  ( 23.58987130287489364, 10.19425842954025008, 9.567338712638951748 ) ) ;
#5068 = CARTESIAN_POINT ( 'NONE',  ( 7.134129719589999752, 5.287968704092000927, -6.611025344044000107 ) ) ;
#5069 = DIRECTION ( 'NONE',  ( 0.000000000000000000, 0.2098314828218890149, -0.9777375664342490280 ) ) ;
#5070 = CARTESIAN_POINT ( 'NONE',  ( 9.481858773912280824, 5.015405643915004319, 8.392875400259256935 ) ) ;
#5071 = EDGE_LOOP ( 'NONE', ( #57404, #46277, #23931, #54854 ) ) ;
#5072 = CARTESIAN_POINT ( 'NONE',  ( 9.318721994369999706, -2.755032632138999737, 8.795122807847999269 ) ) ;
#5073 = B_SPLINE_CURVE_WITH_KNOTS ( 'NONE', 3,
 ( #8062, #33600, #39184, #39531, #45469, #34294, #55616, #29404, #54918, #12615, #7716, #24136, #29750, #7021, #18900, #40225 ),
 .UNSPECIFIED., .F., .F.,
 ( 4, 2, 2, 2, 2, 2, 2, 4 ),
 ( 0.000000000000000000, 0.1249999999999994449, 0.2499999999999988898, 0.3749999999999983347, 0.4999999999999977796, 0.6249999999999980016, 0.7499999999999982236, 1.000000000000000000 ),
 .UNSPECIFIED. ) ;
#5074 = CARTESIAN_POINT ( 'NONE',  ( 11.60000000000000142, 3.327218134278213224, 8.148846660984084167 ) ) ;
#5075 = CARTESIAN_POINT ( 'NONE',  ( 5.427943173017375500, 0.9218200799623694763, 1.199500263597272465 ) ) ;
#5076 = ORIENTED_EDGE ( 'NONE', *, *, #37399, .F. ) ;
#5077 = CARTESIAN_POINT ( 'NONE',  ( 8.199995020667000034, 2.894508905068999827, 6.645190348705000360 ) ) ;
#5078 = B_SPLINE_CURVE_WITH_KNOTS ( 'NONE', 3,
 ( #53957, #6060, #45559, #44532 ),
 .UNSPECIFIED., .F., .F.,
 ( 4, 4 ),
 ( 0.000000000000000000, 1.000000000000000000 ),
 .UNSPECIFIED. ) ;
#5079 = ORIENTED_EDGE ( 'NONE', *, *, #46740, .F. ) ;
#5080 = CARTESIAN_POINT ( 'NONE',  ( 9.814967517147769271, -2.649990781018497721, -7.499998108648967765 ) ) ;
#5081 = CARTESIAN_POINT ( 'NONE',  ( 17.87873473849108308, -1.836456536727123279, -12.46545041361348716 ) ) ;
#5082 = CARTESIAN_POINT ( 'NONE',  ( 17.55505043854147118, -3.125000000000000000, -12.28373071562070074 ) ) ;
#5083 = CARTESIAN_POINT ( 'NONE',  ( 5.219609839683791996, -0.1963495408493605987, -1.500000000000000444 ) ) ;
#5084 = B_SPLINE_CURVE_WITH_KNOTS ( 'NONE', 3,
 ( #32160, #53812, #26911, #37054, #31812, #52785 ),
 .UNSPECIFIED., .F., .F.,
 ( 4, 2, 4 ),
 ( 0.000000000000000000, 0.5000000000000000000, 1.000000000000000000 ),
 .UNSPECIFIED. ) ;
#5085 = CYLINDRICAL_SURFACE ( 'NONE', #16290, 1.000000000000000666 ) ;
#5086 = CARTESIAN_POINT ( 'NONE',  ( 24.01967379662025692, 12.68055978488803781, 3.458368538996728248 ) ) ;
#5087 = EDGE_CURVE ( 'NONE', #1476, #19317, #59624, .T. ) ;
#5088 = ORIENTED_EDGE ( 'NONE', *, *, #13195, .T. ) ;
#5089 = CARTESIAN_POINT ( 'NONE',  ( 10.48791429142999831, -3.983006558652820051, -6.608036045330599961 ) ) ;
#5090 = EDGE_LOOP ( 'NONE', ( #26341, #45735, #52205, #23000 ) ) ;
#5091 = CARTESIAN_POINT ( 'NONE',  ( 10.00122429346999908, 2.274087081648999753, 7.851326250696001097 ) ) ;
#5092 = CARTESIAN_POINT ( 'NONE',  ( 8.731616107288068918, -3.999997736744774546, -8.381579007094499545 ) ) ;
#5093 = MECHANICAL_DESIGN_GEOMETRIC_PRESENTATION_REPRESENTATION (  '', ( #8453 ), #656 ) ;
#5094 = CARTESIAN_POINT ( 'NONE',  ( 17.55505043854144276, 0.7192913403693119712, -12.57945229203838267 ) ) ;
#5095 = CARTESIAN_POINT ( 'NONE',  ( 9.468110841233000841, 4.082930418187999955, -6.104944817728999773 ) ) ;
#5096 = DIRECTION ( 'NONE',  ( 0.000000000000000000, 0.2461538461537954858, 0.9692307692307821076 ) ) ;
#5097 = CARTESIAN_POINT ( 'NONE',  ( 8.348432779685110106, 2.904641401162685099, 6.526586896465118137 ) ) ;
#5098 = CARTESIAN_POINT ( 'NONE',  ( 17.77562957671592159, -0.5851376999905967269, 13.88342059653409066 ) ) ;
#5099 = AXIS2_PLACEMENT_3D ( 'NONE', #57391, #58093, #68565 ) ;
#5100 = CARTESIAN_POINT ( 'NONE',  ( 18.18005043854833147, 0.04052532553066783699, 13.90000015527369470 ) ) ;
#5101 = ORIENTED_EDGE ( 'NONE', *, *, #37255, .T. ) ;
#5102 = CARTESIAN_POINT ( 'NONE',  ( 12.58523710836478138, 0.5851630251601297461, 13.88341719038585076 ) ) ;
#5103 = CARTESIAN_POINT ( 'NONE',  ( 11.36272200990529946, -5.206705454565000224, 7.920925559347199219 ) ) ;
#5104 = DIRECTION ( 'NONE',  ( 0.000000000000000000, -0.9999606858717338120, 0.008867170401640298016 ) ) ;
#5105 = CARTESIAN_POINT ( 'NONE',  ( 17.63844293513428596, -0.6206536994987036371, -13.88134483103688765 ) ) ;
#5106 = CARTESIAN_POINT ( 'NONE',  ( 7.795980646793000624, -3.164807285701999984, 9.104732190648000767 ) ) ;
#5108 = CARTESIAN_POINT ( 'NONE',  ( 12.10004069261316495, -11.60802777289428533, 4.146429405019953940 ) ) ;
#5107 = CARTESIAN_POINT ( 'NONE',  ( 10.25461802485000007, 2.860644035673999941, 6.604613005744999654 ) ) ;
#5109 = CARTESIAN_POINT ( 'NONE',  ( 10.59610807141099897, 4.052703327804870526, -8.639522915742999132 ) ) ;
#5110 = DIRECTION ( 'NONE',  ( 0.000000000000000000, 0.000000000000000000, -1.000000000000000000 ) ) ;
#5111 = AXIS2_PLACEMENT_3D ( 'NONE', #54094, #22620, #54442 ) ;
#5112 = CARTESIAN_POINT ( 'NONE',  ( 8.945797255587999430, 5.003512473869000665, -7.457514444071220439 ) ) ;
#5113 = CARTESIAN_POINT ( 'NONE',  ( 18.27393049982691053, -0.09400131084487256539, 12.59965472429368916 ) ) ;
#5114 = CARTESIAN_POINT ( 'NONE',  ( 6.981910531964000910, 1.102261652484999965, 0.8856219692879000460 ) ) ;
#5115 = CARTESIAN_POINT ( 'NONE',  ( 12.80000000000000071, 10.78295181803999903, -4.410266442048000002 ) ) ;
#5116 = ORIENTED_EDGE ( 'NONE', *, *, #10605, .F. ) ;
#5117 = CARTESIAN_POINT ( 'NONE',  ( 7.802019353206999241, -5.638700495537999124, 8.266402903491000487 ) ) ;
#5118 = CARTESIAN_POINT ( 'NONE',  ( 9.518314158773000244, 4.845406482350000488, -6.387189183984999907 ) ) ;
#5119 = ADVANCED_FACE ( 'NONE', ( #40651 ), #29510, .T. ) ;
#5120 = ADVANCED_FACE ( 'NONE', ( #8842 ), #46256, .T. ) ;
#5121 = DIRECTION ( 'NONE',  ( 0.000000000000000000, 1.000000000000000000, 0.000000000000000000 ) ) ;
#5122 = CARTESIAN_POINT ( 'NONE',  ( 10.99107545325776059, 6.540855374579558124, 5.311061621516608433 ) ) ;
#5123 = VERTEX_POINT ( 'NONE', #29503 ) ;
#5124 = CARTESIAN_POINT ( 'NONE',  ( 18.06944243593800081, 3.222040310929999762, 11.85748006108999952 ) ) ;
#5125 = CARTESIAN_POINT ( 'NONE',  ( 11.19434208742519843, 3.521141233577200325, 6.747282993577999655 ) ) ;
#5126 = CARTESIAN_POINT ( 'NONE',  ( 10.31153584123000044, 2.716831823259000078, -7.950163994344000784 ) ) ;
#5127 = VERTEX_POINT ( 'NONE', #41000 ) ;
#5128 = CARTESIAN_POINT ( 'NONE',  ( 5.305026506349999948, 1.500000000000000000, 0.000000000000000000 ) ) ;
#5129 = CARTESIAN_POINT ( 'NONE',  ( 25.26997868831114147, -8.359964803326231930, 8.486741637760111701 ) ) ;
#5130 = CARTESIAN_POINT ( 'NONE',  ( 11.60118044953561878, 5.133201153721000054, 6.909094663619399945 ) ) ;
#5131 = CARTESIAN_POINT ( 'NONE',  ( 15.90018573812399971, -8.493548356068000516, -8.263529029821000904 ) ) ;
#5132 = CARTESIAN_POINT ( 'NONE',  ( 13.99999999379500082, -8.815218614167999789, -7.616697584347000394 ) ) ;
#5133 = ORIENTED_EDGE ( 'NONE', *, *, #15265, .T. ) ;
#5134 = CARTESIAN_POINT ( 'NONE',  ( 7.835154761361642350, -4.943139372678011512, 6.476578150245067000 ) ) ;
#5135 = CARTESIAN_POINT ( 'NONE',  ( 7.051920280410000075, 5.216734614776999734, -8.484106667489999865 ) ) ;
#5136 = EDGE_CURVE ( 'NONE', #54335, #61003, #56046, .T. ) ;
#5137 = CARTESIAN_POINT ( 'NONE',  ( 8.420824285387190855, -2.370222298025555840, 8.108356380490343795 ) ) ;
#5138 = CARTESIAN_POINT ( 'NONE',  ( 9.649380199234000699, -2.730774061183999901, 7.659530259549099718 ) ) ;
#5139 = EDGE_LOOP ( 'NONE', ( #25567, #14535, #4787, #24331, #23231, #13530 ) ) ;
#5140 = CARTESIAN_POINT ( 'NONE',  ( 2.928056799210041028, 2.150913519912206695, -2.798833948393627313 ) ) ;
#5141 = CARTESIAN_POINT ( 'NONE',  ( 11.80738107398800274, 11.64644714240999868, 1.863397721619000080 ) ) ;
#5142 = ORIENTED_EDGE ( 'NONE', *, *, #25704, .T. ) ;
#5143 = ADVANCED_FACE ( 'NONE', ( #61295 ), #9176, .T. ) ;
#5144 = CARTESIAN_POINT ( 'NONE',  ( 12.35552214745947275, 1.907986453762813284, -12.45488571128362487 ) ) ;
#5145 = CARTESIAN_POINT ( 'NONE',  ( 24.65660926167039690, -8.681443375485125458, -8.652152413449039514 ) ) ;
#5146 = CONICAL_SURFACE ( 'NONE', #44250, 12.72499970924999957, 0.7853981386146715593 ) ;
#5147 = CARTESIAN_POINT ( 'NONE',  ( 10.15000066238999921, -1.190159082397999942E-13, -1.213918169242000045E-13 ) ) ;
#5148 = ORIENTED_EDGE ( 'NONE', *, *, #23832, .T. ) ;
#5149 = FACE_OUTER_BOUND ( 'NONE', #66349, .T. ) ;
#5150 = CARTESIAN_POINT ( 'NONE',  ( 9.893930206848997599, -5.250000000000000000, -7.500000000000000000 ) ) ;
#5151 = CARTESIAN_POINT ( 'NONE',  ( 10.64391429142989765, 4.022379549362480766, -6.325326139450999641 ) ) ;
#5152 = B_SPLINE_CURVE_WITH_KNOTS ( 'NONE', 3,
 ( #27073, #54319, #49078, #59912, #28460, #49774, #12020, #65844, #33357, #53972, #38949, #64797, #59220, #54671, #33005, #1532 ),
 .UNSPECIFIED., .F., .F.,
 ( 4, 2, 2, 2, 2, 2, 2, 4 ),
 ( 0.000000000000000000, 0.06249999999999997224, 0.1249999999999999445, 0.2499999999999996669, 0.5000000000000002220, 0.7500000000000007772, 0.8750000000000003331, 1.000000000000000000 ),
 .UNSPECIFIED. ) ;
#5153 = CARTESIAN_POINT ( 'NONE',  ( 17.85668400807925238, 1.853912555516304739, -13.87670837816644287 ) ) ;
#5154 = CARTESIAN_POINT ( 'NONE',  ( 12.47244801656836799, 3.029249266520640305, -12.31238128988859692 ) ) ;
#5155 = CARTESIAN_POINT ( 'NONE',  ( 10.84580110216399973, -5.090698144635000588, 8.166103548914600552 ) ) ;
#5156 = ORIENTED_EDGE ( 'NONE', *, *, #7086, .F. ) ;
#5157 = CARTESIAN_POINT ( 'NONE',  ( 7.293864158771000028, 3.416213390569000197, 6.162512717529000206 ) ) ;
#5158 = ORIENTED_EDGE ( 'NONE', *, *, #23689, .T. ) ;
#5160 = CARTESIAN_POINT ( 'NONE',  ( 9.433148997456999751, 5.167567567567999731, 6.822293592207000934 ) ) ;
#5159 = B_SPLINE_CURVE_WITH_KNOTS ( 'NONE', 3,
 ( #43061, #1453, #5992, #16147, #59830, #33275 ),
 .UNSPECIFIED., .F., .F.,
 ( 4, 2, 4 ),
 ( 0.000000000000000000, 0.5000000000000000000, 1.000000000000000000 ),
 .UNSPECIFIED. ) ;
#5161 = CONICAL_SURFACE ( 'NONE', #36408, 13.94999927503000059, 0.7853981058017837080 ) ;
#5162 = CARTESIAN_POINT ( 'NONE',  ( 8.096558059622999792, -5.061720701958000390, 5.824087910811999613 ) ) ;
#5163 = CARTESIAN_POINT ( 'NONE',  ( 11.01812914314999858, 6.614778905590999791, -5.431520484943000326 ) ) ;
#5164 = VERTEX_POINT ( 'NONE', #23888 ) ;
#5165 = CARTESIAN_POINT ( 'NONE',  ( 12.51734955436001329, -3.054939157457061238, -12.30478592156021200 ) ) ;
#5166 = CARTESIAN_POINT ( 'NONE',  ( 17.80000000001300009, 3.351264566333000072, 11.15757590352999884 ) ) ;
#5167 = FACE_OUTER_BOUND ( 'NONE', #51693, .T. ) ;
#5168 = CARTESIAN_POINT ( 'NONE',  ( 10.89393020684959978, 2.750000000000000000, 7.500000000000000000 ) ) ;
#5169 = CARTESIAN_POINT ( 'NONE',  ( 12.36102515544325797, -1.940652449090411791, -13.86484480881332892 ) ) ;
#5170 = CARTESIAN_POINT ( 'NONE',  ( 11.63410404293056999, -4.442327784369100030, -8.400720262063998689 ) ) ;
#5171 = CARTESIAN_POINT ( 'NONE',  ( 13.69997185827399733, -10.91304490500501423, -4.183762365652779813 ) ) ;
#5172 = CARTESIAN_POINT ( 'NONE',  ( 18.20249588168630694, -2.156032850912788401, 12.41417075669994219 ) ) ;
#5173 = ORIENTED_EDGE ( 'NONE', *, *, #54441, .T. ) ;
#5174 = VERTEX_POINT ( 'NONE', #29846 ) ;
#5175 = CARTESIAN_POINT ( 'NONE',  ( 0.000000000000000000, 0.000000000000000000, 0.000000000000000000 ) ) ;
#5176 = DIRECTION ( 'NONE',  ( 1.000000000000000000, 0.000000000000000000, 0.000000000000000000 ) ) ;
#5177 = CARTESIAN_POINT ( 'NONE',  ( 11.93028911132391201, -5.144000659054666080, 6.940988051967041272 ) ) ;
#5178 = CARTESIAN_POINT ( 'NONE',  ( 11.19121071698999970, 3.005389011699000079, -6.023544385387999966 ) ) ;
#5179 = B_SPLINE_CURVE_WITH_KNOTS ( 'NONE', 3,
 ( #20510, #19483, #31018, #63145, #51973, #52327, #4422, #67360, #9321, #47090 ),
 .UNSPECIFIED., .F., .F.,
 ( 4, 2, 2, 2, 4 ),
 ( 0.2468845652704700078, 0.4351634239528525128, 0.6234422826352350455, 0.8117211413176175228, 1.000000000000000000 ),
 .UNSPECIFIED. ) ;
#5180 = CARTESIAN_POINT ( 'NONE',  ( 10.44807121817999906, -3.684978196963999864, -6.173109031625999776 ) ) ;
#5181 = CARTESIAN_POINT ( 'NONE',  ( 18.15916593608967133, 2.338515402758149619, -12.48776758577575308 ) ) ;
#5182 = PRODUCT_RELATED_PRODUCT_CATEGORY ( 'part', '', ( #56743 ) ) ;
#5183 = CARTESIAN_POINT ( 'NONE',  ( 8.436987556243993325, 2.901283824935000144, -6.624026488670998525 ) ) ;
#5184 = CARTESIAN_POINT ( 'NONE',  ( 8.797364180957998769, 3.929432544163579788, -8.475895758763700272 ) ) ;
#5185 = ORIENTED_EDGE ( 'NONE', *, *, #52574, .T. ) ;
#5186 = DIRECTION ( 'NONE',  ( 0.000000000000000000, -1.000000000000000000, 0.000000000000000000 ) ) ;
#5187 = CARTESIAN_POINT ( 'NONE',  ( 12.72186720215638189, -3.119790641632218975, 12.28533200497073885 ) ) ;
#5188 = CARTESIAN_POINT ( 'NONE',  ( 4.599999999999999645, 0.000000000000000000, 0.000000000000000000 ) ) ;
#5189 = CARTESIAN_POINT ( 'NONE',  ( 10.24477918374999952, 5.265206995764999398, 8.959504263949002123 ) ) ;
#5190 = CARTESIAN_POINT ( 'NONE',  ( 11.81389666366019853, -4.045876550911099656, 6.467512203247999913 ) ) ;
#5191 = CARTESIAN_POINT ( 'NONE',  ( 9.070310841232000598, 5.361622798585000460, -7.185294144754000634 ) ) ;
#5192 = CARTESIAN_POINT ( 'NONE',  ( 11.78594988689359901, 4.393436444036099786, -8.271690446953899212 ) ) ;
#5193 = CARTESIAN_POINT ( 'NONE',  ( 12.32802524195760085, -0.4039503557775031561, 12.69135589213615312 ) ) ;
#5194 = CARTESIAN_POINT ( 'NONE',  ( 5.600889858811719080, -12.13276343987879002, -3.750125071914726327 ) ) ;
#5195 = CARTESIAN_POINT ( 'NONE',  ( 9.571961069101000419, 4.084683332033999470, 8.946609345378000455 ) ) ;
#5196 = CARTESIAN_POINT ( 'NONE',  ( 4.074968078372999791, 0.000000000000000000, -2.074968475931999734 ) ) ;
#5197 = ORIENTED_EDGE ( 'NONE', *, *, #55257, .F. ) ;
#5198 = CARTESIAN_POINT ( 'NONE',  ( 8.821685841230998193, 2.633142096252999664, -7.791134854666999843 ) ) ;
#5199 = CARTESIAN_POINT ( 'NONE',  ( 6.829081922979999497, -1.130182777988000042, -0.07094392349790000496 ) ) ;
#5200 = EDGE_CURVE ( 'NONE', #51368, #5489, #20688, .T. ) ;
#5201 = EDGE_CURVE ( 'NONE', #8285, #32203, #55185, .T. ) ;
#5202 = CARTESIAN_POINT ( 'NONE',  ( 17.83426395974174383, 1.940453161589466458, 13.77628863228519407 ) ) ;
#5203 = CARTESIAN_POINT ( 'NONE',  ( 3.416991155292667504, 1.737579674229352333, -3.072309530587345794 ) ) ;
#5204 = CARTESIAN_POINT ( 'NONE',  ( 24.56046482271400322, 8.848342285916999117, -9.332993724188000328 ) ) ;
#5205 = CARTESIAN_POINT ( 'NONE',  ( 11.67918044953561996, -2.988516238873000219, -8.027436060358800418 ) ) ;
#5206 = ORIENTED_EDGE ( 'NONE', *, *, #20932, .T. ) ;
#5207 = CONICAL_SURFACE ( 'NONE', #27525, 0.9999998338055000602, 0.7853981908209605178 ) ;
#5208 = B_SPLINE_CURVE_WITH_KNOTS ( 'NONE', 3,
 ( #67190, #30490, #29478, #24557 ),
 .UNSPECIFIED., .F., .F.,
 ( 4, 4 ),
 ( 0.000000000000000000, 1.000000000000000000 ),
 .UNSPECIFIED. ) ;
#5209 = CARTESIAN_POINT ( 'NONE',  ( 11.14975833414749928, 3.203462856645999945, -7.825000000000000178 ) ) ;
#5210 = CARTESIAN_POINT ( 'NONE',  ( 13.70005190196300227, 9.005348107749998832, 7.391036106496999381 ) ) ;
#5213 = LINE ( 'NONE', #1346, #44356 ) ;
#5212 = CARTESIAN_POINT ( 'NONE',  ( 8.763579719593998618, 4.815598936798999752, -8.835641302565999666 ) ) ;
#5211 = UNCERTAINTY_MEASURE_WITH_UNIT (LENGTH_MEASURE( 1.000000000000000082E-05 ), #29365, 'distance_accuracy_value', 'NONE');
#5215 = B_SPLINE_CURVE_WITH_KNOTS ( 'NONE', 3,
 ( #65624, #60391, #12495, #39762, #34861, #29278, #3033, #23671, #18437, #56868, #18781, #34174, #50247, #55493, #56177, #67004, #7593, #2009 ),
 .UNSPECIFIED., .F., .F.,
 ( 4, 2, 2, 2, 2, 2, 2, 2, 4 ),
 ( 0.000000000000000000, 0.1249999999999998890, 0.2499999999999997780, 0.3749999999999997780, 0.4999999999999997780, 0.6249999999999998890, 0.7500000000000000000, 0.8750000000000000000, 1.000000000000000000 ),
 .UNSPECIFIED. ) ;
#5214 = CARTESIAN_POINT ( 'NONE',  ( 3.106872424883109662, -1.723087394956521745, -2.764963742037524153 ) ) ;
#5216 = ORIENTED_EDGE ( 'NONE', *, *, #7479, .T. ) ;
#5217 = CARTESIAN_POINT ( 'NONE',  ( 10.64872393945999995, 2.614781729644000130, 6.717281948314999696 ) ) ;
#5218 = CARTESIAN_POINT ( 'NONE',  ( 18.08802622730391008, -2.172927601657333785, -13.73737356033239010 ) ) ;
#5219 = CARTESIAN_POINT ( 'NONE',  ( 10.80133863405319872, 4.534404523786000674, 6.818303296693398963 ) ) ;
#5220 = CARTESIAN_POINT ( 'NONE',  ( 10.37026726325999881, -5.571557883540000589, 7.748386351620999868 ) ) ;
#5221 = CARTESIAN_POINT ( 'NONE',  ( 8.822980646795000936, -2.678334737187000325, 8.735278777293000729 ) ) ;
#5222 = ORIENTED_EDGE ( 'NONE', *, *, #4952, .F. ) ;
#5223 = CARTESIAN_POINT ( 'NONE',  ( 7.903989158771000056, 2.095715612964000218, 8.056490963156001328 ) ) ;
#5225 = CARTESIAN_POINT ( 'NONE',  ( 11.09992055961999924, -2.373397911211000189, -6.776606350776999577 ) ) ;
#5224 = CARTESIAN_POINT ( 'NONE',  ( 10.07963755961356611, -4.353097593134603649, 8.851823023821729919 ) ) ;
#5226 = CARTESIAN_POINT ( 'NONE',  ( 7.615409857907971869, -4.849756550714564796, 5.981625193514809702 ) ) ;
#5227 = CARTESIAN_POINT ( 'NONE',  ( 7.933148997457998952, -5.167567567567999731, 6.822293592207000934 ) ) ;
#5228 = CARTESIAN_POINT ( 'NONE',  ( 1.118609070385999882, -2.100966486736999705, -2.491430570518000209 ) ) ;
#5229 = ORIENTED_EDGE ( 'NONE', *, *, #49476, .F. ) ;
#5230 = DIRECTION ( 'NONE',  ( 0.000000000000000000, 0.5000000000000168754, 0.8660254037844288266 ) ) ;
#5231 = CARTESIAN_POINT ( 'NONE',  ( 11.56379841651039975, -4.401637675674300532, 6.432302808027999141 ) ) ;
#5232 = EDGE_CURVE ( 'NONE', #52415, #13624, #25039, .T. ) ;
#5233 = CARTESIAN_POINT ( 'NONE',  ( 10.07770645819999977, 4.622041375574999833, 5.671348593713000596 ) ) ;
#5234 = CARTESIAN_POINT ( 'NONE',  ( 11.06379841651039797, 3.598362324325699912, 6.432302808027999141 ) ) ;
#5235 = ORIENTED_EDGE ( 'NONE', *, *, #47710, .F. ) ;
#5236 = B_SPLINE_CURVE_WITH_KNOTS ( 'NONE', 3,
 ( #48986, #22059, #7025, #43407 ),
 .UNSPECIFIED., .F., .F.,
 ( 4, 4 ),
 ( 0.000000000000000000, 1.000000000000000000 ),
 .UNSPECIFIED. ) ;
#5237 = CARTESIAN_POINT ( 'NONE',  ( 8.713854719593998155, 5.442817578555000146, -8.106149115450000053 ) ) ;
#5238 = CARTESIAN_POINT ( 'NONE',  ( 12.11689977649198191, 2.253070615825692347, -12.39692697851452330 ) ) ;
#5239 = CARTESIAN_POINT ( 'NONE',  ( 11.10235971519489873, -3.394698737128500010, 8.506961598696999971 ) ) ;
#5240 = CARTESIAN_POINT ( 'NONE',  ( 24.44496350777200178, -12.03536639536000052, -3.224849854974999985 ) ) ;
#5241 = CIRCLE ( 'NONE', #14187, 1.500000000000000000 ) ;
#5242 = CARTESIAN_POINT ( 'NONE',  ( 24.44496264144000364, 8.810483598181999554, -8.810508341310001157 ) ) ;
#5243 = ORIENTED_EDGE ( 'NONE', *, *, #10951, .T. ) ;
#5244 = CARTESIAN_POINT ( 'NONE',  ( 12.79999998712400178, -11.53033693765999779, 4.891431908114999949 ) ) ;
#5245 = DIRECTION ( 'NONE',  ( 0.000000000000000000, -0.9999503185633161761, -0.009967968956736161443 ) ) ;
#5246 = VERTEX_POINT ( 'NONE', #13065 ) ;
#5247 = CARTESIAN_POINT ( 'NONE',  ( 9.458513540183334456, 3.836375382625530239, 6.250000000000000000 ) ) ;
#5248 = ADVANCED_BREP_SHAPE_REPRESENTATION ( '', ( #52451, #9676 ), #67824 ) ;
#5249 = CARTESIAN_POINT ( 'NONE',  ( 10.99410672858429905, 3.198097575668700010, 8.103244025831999764 ) ) ;
#5250 = STYLED_ITEM ( 'NONE', ( #43093 ), #64411 ) ;
#5251 = DIRECTION ( 'NONE',  ( -1.951617227613594778E-27, 1.000000000000000000, -3.745441456982000038E-14 ) ) ;
#5252 = CARTESIAN_POINT ( 'NONE',  ( 10.66852712374000056, 4.435471808682999395, -5.866466547508000673 ) ) ;
#5253 = CARTESIAN_POINT ( 'NONE',  ( 8.846962924124625260, -3.158163127838481188, -7.738417548727159812 ) ) ;
#5254 = CARTESIAN_POINT ( 'NONE',  ( 10.78089914631999946, -5.735295708369000600, 7.801561210335000496 ) ) ;
#5255 = CARTESIAN_POINT ( 'NONE',  ( 17.91892138177004412, 0.5082598251325838312, -12.68630931495243530 ) ) ;
#5256 = CARTESIAN_POINT ( 'NONE',  ( 12.43937386263551836, 3.007228867379230675, -12.31882001148154515 ) ) ;
#5257 = CARTESIAN_POINT ( 'NONE',  ( 11.43718179236249988, -4.209680326224799707, -6.518682001772900136 ) ) ;
#5258 = CARTESIAN_POINT ( 'NONE',  ( 9.240545280410998430, 4.158911560497999815, 5.873540104660999184 ) ) ;
#5259 = VERTEX_POINT ( 'NONE', #13750 ) ;
#5260 = CARTESIAN_POINT ( 'NONE',  ( 7.399999999999995026, 4.000000000000000000, 9.109807621135329825 ) ) ;
#5261 = CARTESIAN_POINT ( 'NONE',  ( 11.33810207955129812, 4.796537143354000499, 7.174999999999999822 ) ) ;
#5262 = CARTESIAN_POINT ( 'NONE',  ( 10.24809687351608289, -3.672815144550895194, -6.282534154164607365 ) ) ;
#5263 = CARTESIAN_POINT ( 'NONE',  ( 18.28023629128824012, 2.459623831379299297, 12.35762167929923017 ) ) ;
#5264 = EDGE_CURVE ( 'NONE', #67648, #39916, #49784, .T. ) ;
#5265 = CARTESIAN_POINT ( 'NONE',  ( 12.61605721975964478, 1.812633401299055480, 13.88216159563417662 ) ) ;
#5266 = EDGE_CURVE ( 'NONE', #47524, #41410, #51516, .T. ) ;
#5267 = CARTESIAN_POINT ( 'NONE',  ( 11.01356641589999974, 2.786433584103999994, 6.253463831328000211 ) ) ;
#5268 = CARTESIAN_POINT ( 'NONE',  ( 7.000000000000000000, 0.8000000000000000444, -3.149999999999999911 ) ) ;
#5269 = CARTESIAN_POINT ( 'NONE',  ( 9.948096873516250938, -4.327184855449103473, -8.717465845835395299 ) ) ;
#5270 = ORIENTED_EDGE ( 'NONE', *, *, #23663, .F. ) ;
#5271 = CARTESIAN_POINT ( 'NONE',  ( 12.25647171456043694, -2.009180677272478732, 12.43879158508227079 ) ) ;
#5272 = CARTESIAN_POINT ( 'NONE',  ( 9.177784697135001224, -3.305825103746500293, -6.425520776924999566 ) ) ;
#5273 = DIRECTION ( 'NONE',  ( 1.000000000000000000, 0.000000000000000000, 0.000000000000000000 ) ) ;
#5274 = CARTESIAN_POINT ( 'NONE',  ( 11.86486084871759950, -5.207010770456999893, 7.174999999999999822 ) ) ;
#5275 = CARTESIAN_POINT ( 'NONE',  ( 11.91256651104150066, -3.901000349726440053, 8.498573944230598087 ) ) ;
#5276 = CARTESIAN_POINT ( 'NONE',  ( 8.726967411678998587, 3.935557623441470643, 6.608809560686199625 ) ) ;
#5277 = CARTESIAN_POINT ( 'NONE',  ( 0.1621700897146000075, -0.4897778999537000244, -3.171902824723000336 ) ) ;
#5278 = CARTESIAN_POINT ( 'NONE',  ( 4.442561091537439388, -0.1847101713110425592, -1.159272428408197220 ) ) ;
#5279 = CARTESIAN_POINT ( 'NONE',  ( 12.25813800312568880, 2.953224329521587865, 12.24903309118795747 ) ) ;
#5281 = DIRECTION ( 'NONE',  ( 0.000000000000000000, -1.000000000000000000, 0.000000000000000000 ) ) ;
#5280 = CARTESIAN_POINT ( 'NONE',  ( 9.403734463322997783, 4.118936914955599882, -8.635600483553998785 ) ) ;
#5282 = CARTESIAN_POINT ( 'NONE',  ( 11.21149010443640037, 5.137564434800999891, -7.585072163144589652 ) ) ;
#5283 = CARTESIAN_POINT ( 'NONE',  ( 12.79999999914999975, 12.11987927271999865, -3.159802730921999814 ) ) ;
#5284 = EDGE_CURVE ( 'NONE', #59995, #19638, #64099, .T. ) ;
#5285 = CARTESIAN_POINT ( 'NONE',  ( 10.31966721959000033, 4.764593388688000530, -5.997651217580999727 ) ) ;
#5286 = CARTESIAN_POINT ( 'NONE',  ( 9.731950584426998674, 4.507735863714500191, -6.325866838823999139 ) ) ;
#5288 = CARTESIAN_POINT ( 'NONE',  ( 12.22547077881214506, 2.733971791169954813, 12.39396907918110813 ) ) ;
#5287 = CARTESIAN_POINT ( 'NONE',  ( 15.39421883851900219, -8.828753284254000633, -7.820747050108999510 ) ) ;
#5289 = CARTESIAN_POINT ( 'NONE',  ( 8.807788144226000426, 4.090932644426789722, 6.546538158064899804 ) ) ;
#5290 = VERTEX_POINT ( 'NONE', #4616 ) ;
#5291 = AXIS2_PLACEMENT_3D ( 'NONE', #29843, #35755, #40646 ) ;
#5292 = EDGE_CURVE ( 'NONE', #12138, #42349, #3815, .T. ) ;
#5293 = CARTESIAN_POINT ( 'NONE',  ( 12.72380912721855317, 0.6210782762490741904, 12.67955178808353445 ) ) ;
#5294 = CARTESIAN_POINT ( 'NONE',  ( 10.27934687351620724, 3.836375382625536012, 8.750000000000001776 ) ) ;
#5295 = CARTESIAN_POINT ( 'NONE',  ( 17.74546162998189658, -0.7003689476013792437, -12.58057160030211108 ) ) ;
#5296 = CARTESIAN_POINT ( 'NONE',  ( 8.844480666858999030, 4.334888990546500231, 6.553061479084200336 ) ) ;
#5298 = CARTESIAN_POINT ( 'NONE',  ( 12.20019055993962276, -2.341318142288553616, 13.70585175580906245 ) ) ;
#5297 = VECTOR ( 'NONE', #68800, 1000.000000000000000 ) ;
#5299 = DIRECTION ( 'NONE',  ( -0.9999999999848602217, 4.443944958194825790E-06, -3.245118987008870144E-06 ) ) ;
#5300 = CARTESIAN_POINT ( 'NONE',  ( 8.154280367422950704, 3.077394263664351648, 6.302239162262017302 ) ) ;
#5301 = VERTEX_POINT ( 'NONE', #64025 ) ;
#5302 = CARTESIAN_POINT ( 'NONE',  ( 4.695370291990000666, 0.05305521156200000005, 1.133177390024999953 ) ) ;
#5303 = CARTESIAN_POINT ( 'NONE',  ( 9.149380199233998923, -2.730774061183999901, -7.340469740450900282 ) ) ;
#5304 = CYLINDRICAL_SURFACE ( 'NONE', #19821, 0.5000000000000002220 ) ;
#5305 = CARTESIAN_POINT ( 'NONE',  ( 10.97863725587999895, 5.126101790820000836, -4.940798661402999947 ) ) ;
#5306 = EDGE_CURVE ( 'NONE', #15298, #52595, #1496, .T. ) ;
#5307 = CARTESIAN_POINT ( 'NONE',  ( 18.13036722553554370, 2.255582932783688044, -12.50519018731260168 ) ) ;
#5308 = DIRECTION ( 'NONE',  ( 0.9999999999995219380, 9.778750636281211500E-07, -5.518305718317118909E-11 ) ) ;
#5309 = CARTESIAN_POINT ( 'NONE',  ( 18.16243401547605885, 2.647653205692694911, 12.41593780989185092 ) ) ;
#5310 = CIRCLE ( 'NONE', #45515, 0.6999999999999992895 ) ;
#5311 = CARTESIAN_POINT ( 'NONE',  ( 10.39393020684899938, -5.250000000000000000, 7.500000000000000000 ) ) ;
#5312 = CARTESIAN_POINT ( 'NONE',  ( 10.07763305961999833, -2.169024213715999849, -7.244986319234999250 ) ) ;
#5313 = DIRECTION ( 'NONE',  ( 0.000000000000000000, 0.000000000000000000, -1.000000000000000000 ) ) ;
#5314 = B_SPLINE_SURFACE_WITH_KNOTS ( 'NONE', 3, 3, ( 
 ( #52484, #36407, #19645, #31180, #30824, #25916, #31858, #42354, #4581, #25227, #9832, #14743, #46563, #52832, #63654, #57378, #47247, #67869, #62291, #15771, #36759, #4238, #68550, #25578, #51795, #68902, #20672, #42000, #63305, #57724, #15432, #52136, #58080, #10183, #19992, #41313, #31511, #4930, #26265, #47595, #62621, #37100, #15082, #35726, #21018, #46904, #40968, #58414, #36062, #10518, #9481, #68205, #14409, #20324, #3552, #24887, #46218, #67524, #57042, #9144, #41651, #62958, #23681, #2022, #44337, #64329, #45018 ),
 ( #34186, #21692, #33494, #49909, #26615, #47934, #33839, #66323, #7258, #18103, #23340, #61089, #18445, #53173, #39423, #39771, #5275, #60741, #16450, #34, #63992, #55502, #21355, #13210, #42683, #12856, #7604, #54808, #65634, #32208, #16110, #6907, #37434, #58756, #2361, #10862, #60402, #28598, #28953, #44684, #53522, #5611, #26956, #50256, #48269, #375, #43027, #37779, #60058, #12163, #28242, #49560, #1671, #22988, #17761, #39079, #12506, #55153, #65976, #55847, #56530, #20154, #7950, #51960, #24027, #40790, #41481 ),
 ( #62112, #50600, #51620, #62790, #35559, #34536, #45361, #67011, #3717, #67690, #8634, #29289, #2702, #66669, #40119, #19120, #9308, #18791, #14231, #67348, #61433, #56875, #61769, #8974, #13553, #4059, #30313, #56188, #25055, #45702, #8295, #14574, #25396, #40444, #46386, #34870, #29641, #46732, #19813, #35217, #41144, #29983, #50944, #30649, #62453, #35890, #57205, #19467, #68038, #13890, #3040, #24373, #51284, #3380, #24716, #46041, #10690, #42857, #36580, #48449, #26440, #47076, #47770, #58244, #31001, #64168, #47418 ),
 ( #42178, #53006, #16282, #15937, #20844, #31341, #42516, #37268, #27129, #37607, #36932, #48106, #52655, #57906, #4751, #58590, #21866, #26790, #58938, #26093, #63481, #32037, #57551, #9655, #63825, #53693, #68725, #52315, #11043, #4407, #32378, #53351, #5103, #10349, #21185, #25746, #5454, #555, #206, #43203, #68377, #15600, #21526, #5786, #31685, #14911, #36233, #20498, #41822, #69079, #63130, #15257, #10004, #38645, #59272, #33410, #6478, #28160, #18024, #49827, #6828, #43552, #12077, #59625, #64852, #12427, #1940 ) ),
 .UNSPECIFIED., .F., .F., .F.,
 ( 4, 4 ),
 ( 4, 1, 1, 1, 1, 1, 1, 1, 1, 1, 1, 1, 1, 1, 1, 1, 1, 1, 1, 1, 1, 1, 1, 1, 1, 1, 1, 1, 1, 1, 1, 1, 1, 1, 1, 1, 1, 1, 1, 1, 1, 1, 1, 1, 1, 1, 1, 1, 1, 1, 1, 1, 1, 1, 1, 1, 1, 1, 1, 1, 1, 1, 1, 1, 4 ),
 ( -0.02000000000000000042, 1.020000000000000018 ),
 ( 0.008747244164287000176, 0.02453926110774999961, 0.04033127805120999970, 0.05612329499467000327, 0.07191531193812999989, 0.08770732888158999652, 0.1034993458251000087, 0.1192913627684999978, 0.1350833797120000179, 0.1508753966553999792, 0.1666674135988999994, 0.1824594305423999918, 0.1982514474858000086, 0.2140434644293000011, 0.2298354813727000179, 0.2456274983162000103, 0.2614195152596999749, 0.2772115322030999640, 0.2930035491465999842, 0.3087955660900000288, 0.3245875830334999934, 0.3403795999769999581, 0.3561716169204000026, 0.3719636338639000228, 0.3877556508073999875, 0.4035476677507999765, 0.4193396846942999967, 0.4351317016376999858, 0.4509237185811999504, 0.4667157355247000261, 0.4825077524681000152, 0.4982997694115999798, 0.5140917863550000799, 0.5298838032985000446, 0.5456758202420000092, 0.5614678371854000538, 0.5772598541289000185, 0.5930518710723000630, 0.6088438880158000277, 0.6246359049592999924, 0.6404279219027000369, 0.6562199388462000016, 0.6720119557896999662, 0.6878039727331000108, 0.7035959896765999755, 0.7193880066200000201, 0.7351800235634999847, 0.7509720405069999494, 0.7667640574504001050, 0.7825560743939000696, 0.7983480913373000032, 0.8141401082808000789, 0.8299321252243000435, 0.8457241421676999771, 0.8615161591112000528, 0.8773081760545999863, 0.8931001929981000620, 0.9088922099416000266, 0.9246842268849999602, 0.9404762438285000359, 0.9562682607720000005, 0.9720602777153999341, 0.9878522946589000098, 1.003644311601999961, 1.019436328545999970 ),
 .UNSPECIFIED. ) ;
#5315 = CARTESIAN_POINT ( 'NONE',  ( 24.30001694670299983, 8.938702829764999080, 8.938676122491999720 ) ) ;
#5316 = CARTESIAN_POINT ( 'NONE',  ( 24.00946830465457538, 9.351498316855998638, -9.262241387363053136 ) ) ;
#5317 = DIRECTION ( 'NONE',  ( -0.1570822244628920505, -0.9696804098390484628, 0.1872033053451904461 ) ) ;
#5318 = FACE_OUTER_BOUND ( 'NONE', #52978, .T. ) ;
#5319 = EDGE_LOOP ( 'NONE', ( #31789, #63161, #27500 ) ) ;
#5320 = CARTESIAN_POINT ( 'NONE',  ( 8.664129719593997692, 5.524776413195999325, -7.147585171405999915 ) ) ;
#5321 = CARTESIAN_POINT ( 'NONE',  ( 11.44903032197930060, -3.496160833528699996, 8.204588308639600314 ) ) ;
#5322 = ORIENTED_EDGE ( 'NONE', *, *, #50357, .T. ) ;
#5323 = CARTESIAN_POINT ( 'NONE',  ( 9.725191424783275806, 2.649754699899339538, 7.500009801425228773 ) ) ;
#5324 = CARTESIAN_POINT ( 'NONE',  ( 10.13662282008599824, -3.405288783432600219, -8.459250300176799797 ) ) ;
#5325 = ORIENTED_EDGE ( 'NONE', *, *, #3881, .T. ) ;
#5326 = CARTESIAN_POINT ( 'NONE',  ( 11.71922412107039868, 4.069539071394910223, 8.814426450544999625 ) ) ;
#5327 = CARTESIAN_POINT ( 'NONE',  ( 4.400000000000000355, -0.7080094843779000113, -0.8552562627201000245 ) ) ;
#5328 = CARTESIAN_POINT ( 'NONE',  ( 18.26001707275200303, -2.811958703674000137, 11.55267125806999928 ) ) ;
#5329 = CARTESIAN_POINT ( 'NONE',  ( 15.39999999998900293, -9.471998555523999386, -8.194929586088999685 ) ) ;
#5330 = CARTESIAN_POINT ( 'NONE',  ( 12.52211160825347136, 0.5573818238326222474, -13.88495700089724316 ) ) ;
#5331 = CARTESIAN_POINT ( 'NONE',  ( 7.233484566675572047, -0.4004848424655320094, 1.070581206862469159 ) ) ;
#5332 = DIRECTION ( 'NONE',  ( -1.000000000000000000, 0.000000000000000000, 0.000000000000000000 ) ) ;
#5333 = ORIENTED_EDGE ( 'NONE', *, *, #34423, .F. ) ;
#5334 = AXIS2_PLACEMENT_3D ( 'NONE', #68706, #15583, #14211 ) ;
#5335 = CARTESIAN_POINT ( 'NONE',  ( 9.070310841232000598, 5.361622798585000460, -7.185294144754000634 ) ) ;
#5336 = ORIENTED_EDGE ( 'NONE', *, *, #68958, .T. ) ;
#5337 = CARTESIAN_POINT ( 'NONE',  ( 10.65434687351636178, 5.250000000000002665, -7.336375382625537789 ) ) ;
#5338 = ORIENTED_EDGE ( 'NONE', *, *, #56125, .T. ) ;
#5339 = CARTESIAN_POINT ( 'NONE',  ( 9.225367640781000134, 4.603017491986999943, 8.628164124510998789 ) ) ;
#5340 = B_SPLINE_CURVE_WITH_KNOTS ( 'NONE', 3,
 ( #63817, #59265, #32032, #11034, #43543, #31335 ),
 .UNSPECIFIED., .F., .F.,
 ( 4, 1, 1, 4 ),
 ( 0.000000000000000000, 0.2305484662529838635, 0.8346924768898069669, 1.000000000000000000 ),
 .UNSPECIFIED. ) ;
#5341 = CARTESIAN_POINT ( 'NONE',  ( 17.84326074309963772, -3.054675730970588532, -12.30486402137391799 ) ) ;
#5342 = VECTOR ( 'NONE', #49677, 1000.000000000000000 ) ;
#5343 = CARTESIAN_POINT ( 'NONE',  ( 7.000000000000000000, 0.6769230769231000533, 2.665384615385000266 ) ) ;
#5344 = B_SPLINE_CURVE_WITH_KNOTS ( 'NONE', 3,
 ( #60380, #39751, #34519, #40424, #61415, #24697, #12485, #18428, #34852, #56167 ),
 .UNSPECIFIED., .F., .F.,
 ( 4, 2, 2, 2, 4 ),
 ( 0.000000000000000000, 0.2500000000000000000, 0.5000000000000000000, 0.7500000000000000000, 1.000000000000000000 ),
 .UNSPECIFIED. ) ;
#5345 = ADVANCED_FACE ( 'NONE', ( #43060 ), #31282, .F. ) ;
#5346 = ADVANCED_FACE ( 'NONE', ( #56140 ), #18747, .F. ) ;
#5347 = AXIS2_PLACEMENT_3D ( 'NONE', #53609, #25662, #46995 ) ;
#5348 = CARTESIAN_POINT ( 'NONE',  ( 18.10184514650583409, -2.186078922896901755, -12.51950284166921890 ) ) ;
#5349 = EDGE_CURVE ( 'NONE', #36055, #61826, #46342, .T. ) ;
#5350 = CARTESIAN_POINT ( 'NONE',  ( 12.29653044000528794, 0.3639325664385079095, 13.89360161040563035 ) ) ;
#5351 = ORIENTED_EDGE ( 'NONE', *, *, #32542, .F. ) ;
#5352 = CARTESIAN_POINT ( 'NONE',  ( 12.11132301796900101, 11.62873132690000055, -4.501748577889000735 ) ) ;
#5353 = CARTESIAN_POINT ( 'NONE',  ( 17.56428496274500262, 11.49803451072999927, -4.818043541624000170 ) ) ;
#5354 = CARTESIAN_POINT ( 'NONE',  ( 9.961445400145626294, 4.347277725169313989, 8.303075619429563403 ) ) ;
#5355 = VECTOR ( 'NONE', #66704, 1000.000000000000000 ) ;
#5356 = DIRECTION ( 'NONE',  ( -1.000000000000000000, -0.000000000000000000, -0.000000000000000000 ) ) ;
#5357 = CARTESIAN_POINT ( 'NONE',  ( 9.842764158772000727, 5.798263352390999437, -8.113145944980999502 ) ) ;
#5358 = CARTESIAN_POINT ( 'NONE',  ( 17.79408754209099897, -3.298114924730999764, 11.83441383768999877 ) ) ;
#5359 = CARTESIAN_POINT ( 'NONE',  ( 9.662447522843001124, -4.824180051339999942, -8.517611033492999084 ) ) ;
#5360 = B_SPLINE_CURVE_WITH_KNOTS ( 'NONE', 3,
 ( #28210, #16328, #10739, #58988, #602, #64557 ),
 .UNSPECIFIED., .F., .F.,
 ( 4, 2, 4 ),
 ( 0.000000000000000000, 0.5000000000000000000, 1.000000000000000000 ),
 .UNSPECIFIED. ) ;
#5361 = ORIENTED_EDGE ( 'NONE', *, *, #33227, .T. ) ;
#5362 = ORIENTED_EDGE ( 'NONE', *, *, #48233, .F. ) ;
#5363 = VECTOR ( 'NONE', #2822, 1000.000000000000227 ) ;
#5364 = CARTESIAN_POINT ( 'NONE',  ( 10.20920446230533507, -2.899999999999999911, 6.662590550568703307 ) ) ;
#5365 = DIRECTION ( 'NONE',  ( 0.000000000000000000, 0.000000000000000000, -1.000000000000000000 ) ) ;
#5366 = DIRECTION ( 'NONE',  ( 0.000000000000000000, 0.000000000000000000, -1.000000000000000000 ) ) ;
#5367 = CARTESIAN_POINT ( 'NONE',  ( 12.80505043854146940, -3.125000000000000000, 13.52084414783465860 ) ) ;
#5368 = DIRECTION ( 'NONE',  ( 0.000000000000000000, 0.7146936510990797853, 0.6994376205771799526 ) ) ;
#5369 = CARTESIAN_POINT ( 'NONE',  ( 10.97124174884019965, 3.963805917081910213, -8.815770025351000072 ) ) ;
#5370 = CARTESIAN_POINT ( 'NONE',  ( 10.11792546752099931, 3.135062625344399834, -7.440072690703440017 ) ) ;
#5372 = CARTESIAN_POINT ( 'NONE',  ( 10.26574321149000113, -3.424277613364000050, 4.689150231930001134 ) ) ;
#5371 = CARTESIAN_POINT ( 'NONE',  ( 10.40830484851599813, -3.086535948898899928, 7.082356937474298952 ) ) ;
#5373 = CARTESIAN_POINT ( 'NONE',  ( 8.335542453529990681, -2.897657451248000893, 6.653312621732999865 ) ) ;
#5374 = VERTEX_POINT ( 'NONE', #62410 ) ;
#5375 = VECTOR ( 'NONE', #6048, 1000.000000000000000 ) ;
#5376 = CARTESIAN_POINT ( 'NONE',  ( 11.71210404293059959, -4.381818659177399766, -8.277504409418298792 ) ) ;
#5377 = CARTESIAN_POINT ( 'NONE',  ( 8.212419626809003503, -3.104180672527999896, 6.104185052591001082 ) ) ;
#5378 = CARTESIAN_POINT ( 'NONE',  ( 9.887000818240000655, 2.868129552070000088, 6.903968392969799694 ) ) ;
#5379 = CARTESIAN_POINT ( 'NONE',  ( 5.644459972124513669, -12.96885562507462808, 2.321858007525494205 ) ) ;
#5380 = CARTESIAN_POINT ( 'NONE',  ( 10.77462219945999955, -5.575466189878000911, 8.682669263022999573 ) ) ;
#5381 = CARTESIAN_POINT ( 'NONE',  ( 10.90000037895999796, 0.2999996193951000034, 9.776630289319001577 ) ) ;
#5382 = CARTESIAN_POINT ( 'NONE',  ( 16.04649313145500145, -3.595593625533999749, -11.13765277391999931 ) ) ;
#5383 = CARTESIAN_POINT ( 'NONE',  ( 12.95870478550200211, -12.43384127863000010, -1.801469962976000039 ) ) ;
#5384 = CARTESIAN_POINT ( 'NONE',  ( 7.510833333330749539, 4.353359643885027275, -6.185136886497772934 ) ) ;
#5385 = CARTESIAN_POINT ( 'NONE',  ( 9.079430433046999482, -4.737822807309499673, -7.044669955395099770 ) ) ;
#5386 = CARTESIAN_POINT ( 'NONE',  ( 6.052891324326999722, 0.002905985354531999496, 1.468509142934999900 ) ) ;
#5387 = EDGE_CURVE ( 'NONE', #16312, #66190, #6429, .T. ) ;
#5388 = CARTESIAN_POINT ( 'NONE',  ( 11.09991360228957191, -4.849288934224095904, 7.706876553803710728 ) ) ;
#5389 = CARTESIAN_POINT ( 'NONE',  ( 0.1499942179680000542, -1.689975037551094017, -2.199046806507074958 ) ) ;
#5390 = ORIENTED_EDGE ( 'NONE', *, *, #57521, .F. ) ;
#5391 = CARTESIAN_POINT ( 'NONE',  ( 12.33468944037056048, 0.4116921281473236438, -12.69102089861180893 ) ) ;
#5392 = CARTESIAN_POINT ( 'NONE',  ( 11.26902897915239876, 4.221721321201099997, -8.337339982364900592 ) ) ;
#5393 = EDGE_CURVE ( 'NONE', #57153, #3039, #9782, .T. ) ;
#5394 = CYLINDRICAL_SURFACE ( 'NONE', #23070, 14.00000000000000000 ) ;
#5396 = CARTESIAN_POINT ( 'NONE',  ( 3.499617999551372094, -1.078410421222687265, -3.177282998230454680 ) ) ;
#5395 = AXIS2_PLACEMENT_3D ( 'NONE', #48369, #5713, #57920 ) ;
#5397 = CARTESIAN_POINT ( 'NONE',  ( 10.31298165360522212, 2.920330592986121854, -8.329669302950199139 ) ) ;
#5398 = ORIENTED_EDGE ( 'NONE', *, *, #48490, .F. ) ;
#5399 = CARTESIAN_POINT ( 'NONE',  ( 10.85502524286000003, 2.899999999999999911, 6.518873296399666728 ) ) ;
#5400 = CONTEXT_DEPENDENT_SHAPE_REPRESENTATION ( #40950, #14477 ) ;
#5401 = CARTESIAN_POINT ( 'NONE',  ( 11.48522412107029922, -3.952868550833580130, -6.609122077774299164 ) ) ;
#5402 = CARTESIAN_POINT ( 'NONE',  ( 18.04536347373271710, 0.3876168848508783626, 12.69203885981886870 ) ) ;
#5403 = CARTESIAN_POINT ( 'NONE',  ( 10.54184687351587613, -3.000416447002275611, 6.731816600031356401 ) ) ;
#5404 = CARTESIAN_POINT ( 'NONE',  ( 11.49999672495000169, -11.64999999999999858, 1.217117305822866591 ) ) ;
#5405 = AXIS2_PLACEMENT_3D ( 'NONE', #20116, #37229, #42137 ) ;
#5406 = CARTESIAN_POINT ( 'NONE',  ( 11.15278751119019773, 3.209519379020799867, -7.913556523549700294 ) ) ;
#5407 = EDGE_LOOP ( 'NONE', ( #4632, #53145, #11568, #53828, #57100, #64828 ) ) ;
#5408 = CARTESIAN_POINT ( 'NONE',  ( 9.260912867475999732, -4.901383038209000453, 9.090314591495999963 ) ) ;
#5409 = CARTESIAN_POINT ( 'NONE',  ( 17.77709566067061786, 3.084588255221574649, -13.53194174261899185 ) ) ;
#5410 = ORIENTED_EDGE ( 'NONE', *, *, #64730, .T. ) ;
#5411 = CARTESIAN_POINT ( 'NONE',  ( 8.101203251003541439, 5.350537603185198776, -7.263478961105667153 ) ) ;
#5412 = CARTESIAN_POINT ( 'NONE',  ( 8.727043146794999373, -3.882020254083999866, 5.870054788755000530 ) ) ;
#5413 = CARTESIAN_POINT ( 'NONE',  ( 17.91761384724884110, -0.6327954766588933522, -13.98569611075749464 ) ) ;
#5414 = CIRCLE ( 'NONE', #8770, 11.84999999999999964 ) ;
#5415 = ORIENTED_EDGE ( 'NONE', *, *, #57045, .T. ) ;
#5416 = CARTESIAN_POINT ( 'NONE',  ( 23.59999172237900211, -2.915589696762999949, -13.58550518520000061 ) ) ;
#5417 = CARTESIAN_POINT ( 'NONE',  ( 7.324170280405000177, 5.383759907926999766, -8.542359279933998906 ) ) ;
#5418 = CARTESIAN_POINT ( 'NONE',  ( 12.80505043854146940, -3.199698446519381179, -12.18695736643652516 ) ) ;
#5419 = CARTESIAN_POINT ( 'NONE',  ( 9.489492469587677448, 4.926922721015970730, 8.481275974749992841 ) ) ;
#5420 = ORIENTED_EDGE ( 'NONE', *, *, #26187, .F. ) ;
#5421 = CARTESIAN_POINT ( 'NONE',  ( 10.24961784311999935, -4.184221496660999406, 9.286877953065999947 ) ) ;
#5422 = CARTESIAN_POINT ( 'NONE',  ( 25.58980493882700458, 11.09071452174999806, -3.239363653489999884 ) ) ;
#5423 = DIRECTION ( 'NONE',  ( 0.000000000000000000, 0.9916377111174247139, 0.1290528957048031888 ) ) ;
#5424 = ORIENTED_EDGE ( 'NONE', *, *, #960, .T. ) ;
#5425 = AXIS2_PLACEMENT_3D ( 'NONE', #25816, #21258, #35962 ) ;
#5426 = CARTESIAN_POINT ( 'NONE',  ( 11.30000000000000071, -3.781170318299324595, 11.56421629219343394 ) ) ;
#5427 = CARTESIAN_POINT ( 'NONE',  ( 11.03091694037999915, -5.020463882420000523, -6.601194361798000010 ) ) ;
#5428 = ORIENTED_EDGE ( 'NONE', *, *, #3959, .F. ) ;
#5429 = DIRECTION ( 'NONE',  ( 1.000000000000000000, 0.000000000000000000, 0.000000000000000000 ) ) ;
#5430 = DIRECTION ( 'NONE',  ( 1.000000000000000000, 0.000000000000000000, 0.000000000000000000 ) ) ;
#5431 = CARTESIAN_POINT ( 'NONE',  ( 4.624349045621999998, -1.088952042328000136, -1.113569975696999892 ) ) ;
#5432 = CARTESIAN_POINT ( 'NONE',  ( 8.186785167650000972, 5.111321349790002522, -6.695956001718002426 ) ) ;
#5433 = DIRECTION ( 'NONE',  ( 0.000000000000000000, -0.9553735099700839672, 0.2954005017724949389 ) ) ;
#5434 = DIRECTION ( 'NONE',  ( 0.000000000000000000, 0.000000000000000000, -1.000000000000000000 ) ) ;
#5435 = CARTESIAN_POINT ( 'NONE',  ( 23.85847163005615812, 12.93463607130301618, 3.627669834457176279 ) ) ;
#5436 = EDGE_CURVE ( 'NONE', #28156, #22744, #39023, .T. ) ;
#5437 = EDGE_CURVE ( 'NONE', #23656, #46704, #58889, .T. ) ;
#5438 = ADVANCED_FACE ( 'NONE', ( #63081 ), #27081, .F. ) ;
#5439 = VERTEX_POINT ( 'NONE', #16233 ) ;
#5440 = CARTESIAN_POINT ( 'NONE',  ( 13.55676532395741063, -12.34669046015853766, -2.106274408588768132 ) ) ;
#5441 = ORIENTED_EDGE ( 'NONE', *, *, #38350, .F. ) ;
#5442 = CARTESIAN_POINT ( 'NONE',  ( 10.78089701270000056, 5.735299658853000082, 7.801561896854000366 ) ) ;
#5443 = CARTESIAN_POINT ( 'NONE',  ( 10.26693915877000052, 5.500023470133998948, -6.419501519420999891 ) ) ;
#5444 = CARTESIAN_POINT ( 'NONE',  ( 13.12628980020843450, 12.15998242465557233, 2.000325904699570057 ) ) ;
#5445 = CARTESIAN_POINT ( 'NONE',  ( 9.368660841232999914, 2.702406276695999754, -6.981052078638000147 ) ) ;
#5446 = FACE_OUTER_BOUND ( 'NONE', #63719, .T. ) ;
#5447 = SURFACE_SIDE_STYLE ('',( #37601 ) ) ;
#5448 = CARTESIAN_POINT ( 'NONE',  ( 18.14018103492323775, 0.2205930660282628131, 13.89766156610768277 ) ) ;
#5449 = AXIS2_PLACEMENT_3D ( 'NONE', #32598, #17904, #59501 ) ;
#5450 = CARTESIAN_POINT ( 'NONE',  ( 13.70003001321900449, -10.31266399190331384, -7.179884396236143829 ) ) ;
#5451 = ORIENTED_EDGE ( 'NONE', *, *, #27624, .F. ) ;
#5452 = AXIS2_PLACEMENT_3D ( 'NONE', #5632, #58432, #52 ) ;
#5453 = CARTESIAN_POINT ( 'NONE',  ( 12.64394750688183500, 0.6042238833753180716, 13.88232004407564801 ) ) ;
#5454 = CARTESIAN_POINT ( 'NONE',  ( 11.26426088462129904, -3.997280690308189666, 8.778009775371000245 ) ) ;
#5455 = CARTESIAN_POINT ( 'NONE',  ( 17.86525158946622938, -0.5426919696322294318, -13.88574006265329963 ) ) ;
#5456 = EDGE_CURVE ( 'NONE', #23313, #40162, #37557, .T. ) ;
#5457 = CARTESIAN_POINT ( 'NONE',  ( 9.079730646793999327, -5.421531391267000011, 6.381128921159999301 ) ) ;
#5459 = FACE_OUTER_BOUND ( 'NONE', #36713, .T. ) ;
#5458 = CARTESIAN_POINT ( 'NONE',  ( 10.22108913916999917, 2.983268757921999637, 8.764704075288999974 ) ) ;
#5460 = CARTESIAN_POINT ( 'NONE',  ( 10.91610672858429965, 3.088399709291500095, -6.814233985789400094 ) ) ;
#5461 = CARTESIAN_POINT ( 'NONE',  ( 11.39975833414730033, -3.203462856645999945, -7.174999999999999822 ) ) ;
#5462 = CARTESIAN_POINT ( 'NONE',  ( 9.627671671056999614, 3.144964309357700216, -7.643603315539799326 ) ) ;
#5463 = CARTESIAN_POINT ( 'NONE',  ( 18.17902769456078360, -0.04114048977874908142, 12.69993211551498469 ) ) ;
#5464 = B_SPLINE_SURFACE_WITH_KNOTS ( 'NONE', 3, 3, ( 
 ( #47089, #14923, #68051, #4074, #51972, #31354, #20165, #25411, #35572, #37881, #36246, #36593, #46746, #9320, #31016, #27054, #41835, #11303, #32642, #68389, #19828, #21793, #15269, #41493, #53952, #24729, #46055, #67359, #19482, #40803, #62125, #14244, #56888, #46400, #8985 ),
 ( #30327, #51635, #41159, #62465, #14585, #17246, #44867, #66172, #1862, #34033, #27750, #39611, #17601, #38221, #38926, #49401, #7442, #12350, #59549, #60248, #39267, #11645, #33682, #54299, #55000, #55346, #23180, #60937, #44529, #13052, #7101, #17949, #18292, #65823, #60590 ),
 ( #34380, #1513, #23526, #28439, #2212, #6056, #49753, #48722, #824, #12696, #27394, #28793, #50104, #22141, #43481, #64779, #32984, #16892, #22831, #6402, #49062, #1169, #22483, #43825, #44178, #65125, #38567, #59892, #12000, #33338, #65475, #54653, #6748, #28087, #8485 ),
 ( #29135, #30498, #23872, #9161, #56730, #24565, #29830, #35067, #13734, #40985, #51136, #56382, #66513, #46581, #45888, #67540, #3238, #66862, #67198, #19664, #51473, #41331, #25243, #19309, #29490, #35742, #30168, #61618, #57061, #55698, #20006, #40634, #61968, #18975, #62308 ) ),
 .UNSPECIFIED., .F., .F., .F.,
 ( 4, 4 ),
 ( 4, 1, 1, 1, 1, 1, 1, 1, 1, 1, 1, 1, 1, 1, 1, 1, 1, 1, 1, 1, 1, 1, 1, 1, 1, 1, 1, 1, 1, 1, 1, 1, 4 ),
 ( -0.02000000000000000042, 1.020000000000000018 ),
 ( 0.1633025096610999927, 0.1899619885200000136, 0.2166214673788000034, 0.2432809462376999965, 0.2699404250964999585, 0.2965999039553000038, 0.3232593828141999692, 0.3499188616730000145, 0.3765783405318000043, 0.4032378193906999697, 0.4298972982494999595, 0.4565567771083000048, 0.4832162559671999702, 0.5098757348260000155, 0.5365352136848999809, 0.5631946925437000262, 0.5898541714025000715, 0.6165136502614000369, 0.6431731291201999712, 0.6698326079790000165, 0.6964920868378999819, 0.7231515656967000272, 0.7498110445554999615, 0.7764705234143999268, 0.8031300022731999722, 0.8297894811320000175, 0.8564489599908999828, 0.8831084388497000282, 0.9097679177085999935, 0.9364273965674000388, 0.9630868754261999731, 0.9897463542851000495, 1.016405833144000015 ),
 .UNSPECIFIED. ) ;
#5465 = CARTESIAN_POINT ( 'NONE',  ( 6.882286134928000010, 1.186537294537999943, -0.7690490643353999900 ) ) ;
#5466 = CARTESIAN_POINT ( 'NONE',  ( 24.57010313871199969, 8.854968118029999502, 9.404173716609999900 ) ) ;
#5467 = VERTEX_POINT ( 'NONE', #25696 ) ;
#5468 = CARTESIAN_POINT ( 'NONE',  ( 8.406105646793999853, -5.342173944271999986, 8.432314172168000610 ) ) ;
#5469 = CARTESIAN_POINT ( 'NONE',  ( 9.209204462306566086, -2.899999999999999911, 6.662590550605525408 ) ) ;
#5470 = CARTESIAN_POINT ( 'NONE',  ( 24.63329087101742942, 8.756202933458791193, -7.455126436760659558 ) ) ;
#5471 = CARTESIAN_POINT ( 'NONE',  ( 11.09999965054999826, -12.24999851416000141, 0.000000000000000000 ) ) ;
#5472 = EDGE_LOOP ( 'NONE', ( #45140, #11863, #11674, #4351 ) ) ;
#5473 = B_SPLINE_CURVE_WITH_KNOTS ( 'NONE', 3,
 ( #37161, #21082, #32950, #789 ),
 .UNSPECIFIED., .F., .F.,
 ( 4, 4 ),
 ( 0.000000000000000000, 1.000000000000000000 ),
 .UNSPECIFIED. ) ;
#5474 = CARTESIAN_POINT ( 'NONE',  ( 0.4116496906523000043, 2.199938726422999924, 2.557617887446999916 ) ) ;
#5475 = CARTESIAN_POINT ( 'NONE',  ( 27.09999999999999787, 0.000000000000000000, -9.250000000000000000 ) ) ;
#5476 = CARTESIAN_POINT ( 'NONE',  ( 11.37168584123000059, 2.803494217761000495, -6.967881733280000489 ) ) ;
#5477 = ORIENTED_EDGE ( 'NONE', *, *, #38262, .F. ) ;
#5478 = CARTESIAN_POINT ( 'NONE',  ( 8.960616452296999768, 2.899999999999999911, 6.279946362737000243 ) ) ;
#5479 = CARTESIAN_POINT ( 'NONE',  ( 10.90000000000000036, 0.000000000000000000, 0.000000000000000000 ) ) ;
#5480 = CARTESIAN_POINT ( 'NONE',  ( 10.12426357027499790, 5.254871132332000094, 7.257895958275299542 ) ) ;
#5481 = EDGE_CURVE ( 'NONE', #29214, #15051, #32336, .T. ) ;
#5482 = CARTESIAN_POINT ( 'NONE',  ( 5.634466645576796218, 12.10031501007015819, 3.741403512701362732 ) ) ;
#5483 = CARTESIAN_POINT ( 'NONE',  ( 7.822385841228999048, 4.636729845879000500, 9.378977473003999421 ) ) ;
#5484 = ORIENTED_EDGE ( 'NONE', *, *, #21431, .F. ) ;
#5485 = LINE ( 'NONE', #15291, #54467 ) ;
#5486 = CARTESIAN_POINT ( 'NONE',  ( 7.955829719586001048, 5.418947913204000599, -8.493927145653000110 ) ) ;
#5487 = CARTESIAN_POINT ( 'NONE',  ( 8.542538633423246708, -3.328189143799264560, 5.895772191526457817 ) ) ;
#5488 = CARTESIAN_POINT ( 'NONE',  ( 9.092138961223998450, -2.940105638081000006, 6.783753885003399375 ) ) ;
#5489 = VERTEX_POINT ( 'NONE', #31989 ) ;
#5490 = CARTESIAN_POINT ( 'NONE',  ( 2.886390132543207976, 0.4581489286485156964, -3.499999999999998668 ) ) ;
#5491 = CARTESIAN_POINT ( 'NONE',  ( 6.344609839683333696, 1.500000000000000888, -0.1963495408493590444 ) ) ;
#5492 = ORIENTED_EDGE ( 'NONE', *, *, #68210, .T. ) ;
#5493 = CARTESIAN_POINT ( 'NONE',  ( 24.95274028248806886, 2.977348869105516105, -11.59849451147599808 ) ) ;
#5494 = CARTESIAN_POINT ( 'NONE',  ( 24.71427135204747216, -8.651883463778640149, -8.603915179283948333 ) ) ;
#5495 = CARTESIAN_POINT ( 'NONE',  ( 11.02452225494999993, -2.775477745048999800, -6.571291218949999902 ) ) ;
#5496 = VERTEX_POINT ( 'NONE', #26393 ) ;
#5497 = CARTESIAN_POINT ( 'NONE',  ( 10.49751479358649320, -3.288413547421944916, -9.126840212398633412 ) ) ;
#5498 = DIRECTION ( 'NONE',  ( 1.000000000000000000, 0.000000000000000000, 0.000000000000000000 ) ) ;
#5499 = CARTESIAN_POINT ( 'NONE',  ( 11.11123293495519881, 3.108594079907299967, -7.464165716332529676 ) ) ;
#5500 = CARTESIAN_POINT ( 'NONE',  ( 11.79999999471800010, 3.216299622513999701, -11.40340969442000052 ) ) ;
#5501 = CARTESIAN_POINT ( 'NONE',  ( 11.11656919669529842, -2.774362666861999838, 7.137881914002699446 ) ) ;
#5502 = ORIENTED_EDGE ( 'NONE', *, *, #19311, .T. ) ;
#5503 = CARTESIAN_POINT ( 'NONE',  ( 8.218892219592001780, 3.011620138462000273, 8.801434747080000065 ) ) ;
#5504 = ORIENTED_EDGE ( 'NONE', *, *, #22746, .F. ) ;
#5505 = CARTESIAN_POINT ( 'NONE',  ( 10.04184687351666661, -3.000416447002275611, 6.731816600031356401 ) ) ;
#5506 = CARTESIAN_POINT ( 'NONE',  ( 15.66944243593800046, -9.081775842407999733, -8.276637282895999093 ) ) ;
#5507 = CARTESIAN_POINT ( 'NONE',  ( 11.12440625316000009, 6.500244850899999705, -5.560228937576999542 ) ) ;
#5508 = ORIENTED_EDGE ( 'NONE', *, *, #40499, .T. ) ;
#5509 = CARTESIAN_POINT ( 'NONE',  ( 12.72194006826445545, -1.880463790526825552, -12.57452048663021671 ) ) ;
#5510 = CARTESIAN_POINT ( 'NONE',  ( 10.67726354018259904, 4.629523725463628558, -6.407767014557180119 ) ) ;
#5511 = CARTESIAN_POINT ( 'NONE',  ( 23.89320776801300283, -8.313844348326997036, 8.526065359053994541 ) ) ;
#5512 = DIRECTION ( 'NONE',  ( 0.000000000000000000, 0.9999606858717338120, -0.008867170401640424651 ) ) ;
#5513 = CARTESIAN_POINT ( 'NONE',  ( 12.13953890720640416, -2.807801093580551743, -13.71555245415304292 ) ) ;
#5514 = CARTESIAN_POINT ( 'NONE',  ( 10.70287750876920008, -4.469200303112399908, -8.228113772635300194 ) ) ;
#5515 = CARTESIAN_POINT ( 'NONE',  ( 7.123756830750108904, 1.021180222699791917, -0.7836994991100844077 ) ) ;
#5517 = ADVANCED_FACE ( 'NONE', ( #21476 ), #63778, .F. ) ;
#5516 = CARTESIAN_POINT ( 'NONE',  ( 18.10200918459799979, -2.953257374879731501, 12.24902512628088225 ) ) ;
#5518 = ORIENTED_EDGE ( 'NONE', *, *, #67769, .T. ) ;
#5519 = DIRECTION ( 'NONE',  ( 1.000000000000000000, 0.000000000000000000, 0.000000000000000000 ) ) ;
#5520 = ORIENTED_EDGE ( 'NONE', *, *, #57561, .F. ) ;
#5521 = CONICAL_SURFACE ( 'NONE', #11113, 0.9999998338055000602, 0.7853981908209605178 ) ;
#5522 = CARTESIAN_POINT ( 'NONE',  ( 10.43314899746000002, -5.167567567567999731, 6.822293592207000934 ) ) ;
#5523 = CARTESIAN_POINT ( 'NONE',  ( 12.80505043854144276, -0.6600719421079733751, -13.91436771118225302 ) ) ;
#5524 = CARTESIAN_POINT ( 'NONE',  ( 9.973493989215999278, 4.344963986309999804, -9.321593970653999861 ) ) ;
#5525 = CARTESIAN_POINT ( 'NONE',  ( 10.36950884864999978, -2.719121019997000399, -7.031782724641000293 ) ) ;
#5526 = DIRECTION ( 'NONE',  ( -1.000000000000000000, 0.000000000000000000, 0.000000000000000000 ) ) ;
#5527 = CARTESIAN_POINT ( 'NONE',  ( 23.58475003573600048, -13.39488253062000211, 4.040730013063999593 ) ) ;
#5528 = CARTESIAN_POINT ( 'NONE',  ( 8.741501215035997419, 3.771222299067000350, -8.375893644236599656 ) ) ;
#5529 = ORIENTED_EDGE ( 'NONE', *, *, #36574, .F. ) ;
#5530 = CARTESIAN_POINT ( 'NONE',  ( 11.47822875044625945, -3.830319670899316353, -6.639682804525812720 ) ) ;
#5531 = CARTESIAN_POINT ( 'NONE',  ( 9.629022744239000176, 5.794335169544999609, 7.414871903737999759 ) ) ;
#5532 = DIRECTION ( 'NONE',  ( 0.000000000000000000, -0.9048270524743471377, 0.4257792915473756490 ) ) ;
#5533 = EDGE_CURVE ( 'NONE', #60622, #60101, #35090, .T. ) ;
#5534 = CARTESIAN_POINT ( 'NONE',  ( 11.14902344389989963, -4.883530143601199747, 8.036199780531900316 ) ) ;
#5535 = CARTESIAN_POINT ( 'NONE',  ( 17.85726930274100255, 3.190143309604999811, -11.45065656613999927 ) ) ;
#5536 = CARTESIAN_POINT ( 'NONE',  ( 11.46595122972049907, 4.343798595649099425, -6.704952129760900270 ) ) ;
#5537 = EDGE_CURVE ( 'NONE', #37649, #17729, #61555, .T. ) ;
#5538 = CARTESIAN_POINT ( 'NONE',  ( 12.58454787187813295, -0.5848996845204778028, 12.68186405703078812 ) ) ;
#5539 = CARTESIAN_POINT ( 'NONE',  ( 5.596495275684807424, -12.13697930370502753, -3.751366953416414685 ) ) ;
#5540 = FACE_OUTER_BOUND ( 'NONE', #56381, .T. ) ;
#5541 = FILL_AREA_STYLE_COLOUR ( '', #2020 ) ;
#5542 = ORIENTED_EDGE ( 'NONE', *, *, #62589, .F. ) ;
#5543 = FACE_OUTER_BOUND ( 'NONE', #36453, .T. ) ;
#5544 = CARTESIAN_POINT ( 'NONE',  ( 9.910492310842998975, -4.686746084135999801, -9.174865097765998456 ) ) ;
#5545 = CARTESIAN_POINT ( 'NONE',  ( 17.75741541229203335, 3.091422763980662403, 13.53001720626202520 ) ) ;
#5546 = CARTESIAN_POINT ( 'NONE',  ( -0.2999999999999999889, -1.154700538379000108, 0.000000000000000000 ) ) ;
#5547 = CARTESIAN_POINT ( 'NONE',  ( 11.65456516821461008, -3.197083038490000195, -8.310318115935698913 ) ) ;
#5548 = B_SPLINE_CURVE_WITH_KNOTS ( 'NONE', 3,
 ( #60115, #54868, #48589, #28298, #22697, #1044, #692, #6968, #43352, #21324, #63963, #64652, #38086, #43694, #17105, #6622, #16075, #27961, #37406, #58728, #18506, #28655, #61492, #56248, #12566, #40504, #24087, #8354, #2416, #61829, #56591, #33896 ),
 .UNSPECIFIED., .F., .F.,
 ( 4, 2, 2, 2, 2, 2, 2, 2, 1, 2, 2, 2, 1, 1, 1, 2, 2, 4 ),
 ( 0.000000000000000000, 0.2500000000000310862, 0.3750000000000450751, 0.4375000000000534017, 0.4687500000000560663, 0.5000000000000587308, 0.6250000000000562883, 0.6875000000000531797, 0.7187500000000527356, 0.7343750000000519584, 0.7500000000000512923, 0.8125000000000498490, 0.8437500000000496270, 0.8593750000000495159, 0.8671875000000479616, 0.8710937500000468514, 0.8750000000000456302, 1.000000000000000000 ),
 .UNSPECIFIED. ) ;
#5549 = ORIENTED_EDGE ( 'NONE', *, *, #42841, .T. ) ;
#5550 = CARTESIAN_POINT ( 'NONE',  ( 16.03314433152361218, -8.943717616153330496, -8.673217039016838825 ) ) ;
#5551 = CARTESIAN_POINT ( 'NONE',  ( 10.12947109217999930, -5.100000000000000533, 6.152188490330000370 ) ) ;
#5553 = CARTESIAN_POINT ( 'NONE',  ( 11.04664311227086593, -3.555960431980462300, -8.706333095531745059 ) ) ;
#5552 = CARTESIAN_POINT ( 'NONE',  ( 8.126014158770999529, 5.189036231907000030, -8.048606212067999977 ) ) ;
#5554 = CARTESIAN_POINT ( 'NONE',  ( 2.687702790109109952, 1.441822626232357685, -2.921506834555485099 ) ) ;
#5555 = ORIENTED_EDGE ( 'NONE', *, *, #62176, .T. ) ;
#5556 = CARTESIAN_POINT ( 'NONE',  ( 10.14750576281000072, 2.602962605360999770, 6.738577830910999822 ) ) ;
#5557 = CARTESIAN_POINT ( 'NONE',  ( 17.59651852071655753, -3.123961849275329161, -13.52107344427228597 ) ) ;
#5558 = CARTESIAN_POINT ( 'NONE',  ( 11.19102897915239936, 4.256858847510399890, 6.529961657816500065 ) ) ;
#5559 = CARTESIAN_POINT ( 'NONE',  ( 10.03612181215999932, -3.011786236723999810, 8.746965724352000038 ) ) ;
#5560 = CARTESIAN_POINT ( 'NONE',  ( 7.256081853207000165, -2.531197775378000170, 8.216705951490000714 ) ) ;
#5561 = ORIENTED_EDGE ( 'NONE', *, *, #62115, .F. ) ;
#5562 = CARTESIAN_POINT ( 'NONE',  ( 8.122954719591000128, 3.566637212418000136, 5.743604853744000316 ) ) ;
#5564 = CARTESIAN_POINT ( 'NONE',  ( 11.16750564679000135, -3.188702545307000147, -8.788667016604001958 ) ) ;
#5563 = CARTESIAN_POINT ( 'NONE',  ( 10.59991360228957191, 3.150711065775904984, -7.293123446196289272 ) ) ;
#5565 = CIRCLE ( 'NONE', #43557, 11.35000000000000142 ) ;
#5566 = CARTESIAN_POINT ( 'NONE',  ( 7.806944751142499861, -4.387688527371611968, 9.195859951489477879 ) ) ;
#5567 = CARTESIAN_POINT ( 'NONE',  ( 10.31167756636999933, -2.874479384703000129, 8.900026329558999194 ) ) ;
#5568 = CARTESIAN_POINT ( 'NONE',  ( 2.024566109761000376, -3.102129433205000009, 0.9990388109167002151 ) ) ;
#5569 = VERTEX_POINT ( 'NONE', #59226 ) ;
#5570 = CARTESIAN_POINT ( 'NONE',  ( 5.709193173016666734, -0.3926218265389190276, -1.460959015002473826 ) ) ;
#5571 = CARTESIAN_POINT ( 'NONE',  ( 11.44072200990529886, -5.077092948368999714, 7.875713849677398848 ) ) ;
#5572 = CARTESIAN_POINT ( 'NONE',  ( 11.52733460557258915, 4.206337284815599986, 6.238754009183999472 ) ) ;
#5573 = VERTEX_POINT ( 'NONE', #58200 ) ;
#5574 = CARTESIAN_POINT ( 'NONE',  ( 8.772439158776000667, 3.098073081301000009, -8.567513114264999174 ) ) ;
#5575 = CARTESIAN_POINT ( 'NONE',  ( 12.41909388474793019, 1.871095411850174139, -12.46029856231474930 ) ) ;
#5576 = CARTESIAN_POINT ( 'NONE',  ( 11.06080513895999928, -2.973119161490000106, 8.070849345005600028 ) ) ;
#5577 = CARTESIAN_POINT ( 'NONE',  ( 7.946887679546887462, 4.820318833187246632, -6.338152156212514932 ) ) ;
#5578 = CARTESIAN_POINT ( 'NONE',  ( 18.11804139222710219, 2.771758052454487142, -13.61206300403527436 ) ) ;
#5579 = ORIENTED_EDGE ( 'NONE', *, *, #9211, .T. ) ;
#5580 = CARTESIAN_POINT ( 'NONE',  ( 8.897673733342999824, -5.117431802241999783, -6.704256657961999544 ) ) ;
#5581 = CARTESIAN_POINT ( 'NONE',  ( 5.627943173016957346, -0.9218200799623714747, -1.199500263597270466 ) ) ;
#5582 = ORIENTED_EDGE ( 'NONE', *, *, #59360, .T. ) ;
#5583 = CARTESIAN_POINT ( 'NONE',  ( 12.38044747764044651, -3.063579277862365391, -12.22188755179955955 ) ) ;
#5584 = CARTESIAN_POINT ( 'NONE',  ( 11.65871932425156920, 3.852858594438699935, 6.507377093516500288 ) ) ;
#5585 = CARTESIAN_POINT ( 'NONE',  ( 10.26328274790922812, 2.909659596545209670, -8.325272347294529141 ) ) ;
#5586 = CARTESIAN_POINT ( 'NONE',  ( 10.74708949327000163, 5.603142351927999698, -6.963341971584000589 ) ) ;
#5587 = DIRECTION ( 'NONE',  ( 0.000000000000000000, -0.5000000000000168754, -0.8660254037844288266 ) ) ;
#5588 = CARTESIAN_POINT ( 'NONE',  ( 11.09648096125000016, -3.099777420064000033, 6.097103007060000301 ) ) ;
#5589 = CARTESIAN_POINT ( 'NONE',  ( 17.94753454920341795, 0.4864235087029692428, -12.68745975172791240 ) ) ;
#5590 = CARTESIAN_POINT ( 'NONE',  ( 12.80505043854144276, 0.7302158263239216796, -13.98094363220830871 ) ) ;
#5591 = CARTESIAN_POINT ( 'NONE',  ( 10.57564694612699974, -4.931992688388300294, -7.871941502982999772 ) ) ;
#5592 = EDGE_CURVE ( 'NONE', #54751, #23033, #37274, .T. ) ;
#5594 = EDGE_CURVE ( 'NONE', #47991, #50185, #52938, .T. ) ;
#5593 = CARTESIAN_POINT ( 'NONE',  ( 9.331135841230999262, 4.141907758973999876, 6.047574021139999978 ) ) ;
#5595 = EDGE_LOOP ( 'NONE', ( #31424, #2185, #56487, #65731, #52234, #3665 ) ) ;
#5596 = CARTESIAN_POINT ( 'NONE',  ( 11.04664311227086415, 4.444039568019538144, 6.293666904468256718 ) ) ;
#5597 = DIRECTION ( 'NONE',  ( 0.000000000000000000, -1.000000000000000000, 0.000000000000000000 ) ) ;
#5598 = DIRECTION ( 'NONE',  ( 0.000000000000000000, 1.000000000000000000, 0.000000000000000000 ) ) ;
#5599 = CARTESIAN_POINT ( 'NONE',  ( 18.26225755805769424, 2.321011060851990493, 12.38438709824086814 ) ) ;
#5600 = CARTESIAN_POINT ( 'NONE',  ( 11.01817350255000072, 6.612266912192000134, 5.428976045567000419 ) ) ;
#5601 = CARTESIAN_POINT ( 'NONE',  ( 11.12486389849000012, 7.229950150994000069, 6.290773257298000409 ) ) ;
#5602 = DIRECTION ( 'NONE',  ( 0.000000000000000000, 0.000000000000000000, -1.000000000000000000 ) ) ;
#5603 = CYLINDRICAL_SURFACE ( 'NONE', #34878, 0.4999999999999998335 ) ;
#5604 = ORIENTED_EDGE ( 'NONE', *, *, #46115, .F. ) ;
#5605 = CARTESIAN_POINT ( 'NONE',  ( 24.25374608244500152, 8.963954835242001096, 8.909854536156000648 ) ) ;
#5606 = CARTESIAN_POINT ( 'NONE',  ( 10.13626717315599990, -4.764472860199700399, -6.848522029265999400 ) ) ;
#5607 = CARTESIAN_POINT ( 'NONE',  ( 13.70009528508592211, -8.955766972928978831, -7.451364690503297084 ) ) ;
#5608 = ADVANCED_FACE ( 'NONE', ( #55029 ), #2789, .T. ) ;
#5609 = VECTOR ( 'NONE', #54834, 1000.000000000000000 ) ;
#5610 = FACE_OUTER_BOUND ( 'NONE', #36601, .T. ) ;
#5611 = CARTESIAN_POINT ( 'NONE',  ( 11.29718447801629999, -2.996774412198000448, 7.522119512433738997 ) ) ;
#5612 = B_SPLINE_SURFACE_WITH_KNOTS ( 'NONE', 3, 3, ( 
 ( #10396, #57956, #14283, #31735, #62498, #30362, #51670, #30697, #46436, #53054, #57598, #47124, #31390, #25446, #15646, #24765, #56923, #46779, #25794, #58291, #35940, #46090, #3766, #9705, #63535, #67398, #19519, #57253, #36980, #35610, #9354, #68425, #40839, #20548, #52007 ),
 ( #36282, #67738, #52705, #19861, #4110, #68774, #41193, #10054, #14621, #20199, #52361, #4453, #68083, #15307, #63178, #20892, #42228, #31051, #41526, #36632, #62839, #4799, #26143, #14958, #47468, #25607, #15116, #51150, #67553, #30855, #3248, #36436, #15463, #57072, #61980 ),
 ( #24914, #19675, #58108, #20019, #35417, #51483, #56742, #57409, #68237, #8839, #24576, #3580, #42032, #67902, #45900, #46247, #46596, #62987, #4613, #14436, #40997, #62656, #25947, #14090, #20359, #30178, #9865, #41343, #57754, #30511, #47280, #36788, #62321, #25258, #41683 ),
 ( #67210, #14776, #68581, #19322, #31209, #52513, #40647, #20703, #35756, #63335, #36094, #10210, #9513, #9172, #51823, #4271, #3921, #52171, #46935, #43757, #48651, #31543, #22066, #43057, #10550, #59474, #59826, #58791, #6328, #47964, #64710, #68935, #26985, #59133, #11236 ) ),
 .UNSPECIFIED., .F., .F., .F.,
 ( 4, 4 ),
 ( 4, 1, 1, 1, 1, 1, 1, 1, 1, 1, 1, 1, 1, 1, 1, 1, 1, 1, 1, 1, 1, 1, 1, 1, 1, 1, 1, 1, 1, 1, 1, 1, 4 ),
 ( -0.02000000000000000042, 1.020000000000000018 ),
 ( 0.1633025096610999927, 0.1899619885200000136, 0.2166214673788000034, 0.2432809462376999965, 0.2699404250964999585, 0.2965999039553000038, 0.3232593828141999692, 0.3499188616730000145, 0.3765783405318000043, 0.4032378193906999697, 0.4298972982494999595, 0.4565567771083000048, 0.4832162559671999702, 0.5098757348260000155, 0.5365352136848999809, 0.5631946925437000262, 0.5898541714025000715, 0.6165136502614000369, 0.6431731291201999712, 0.6698326079790000165, 0.6964920868378999819, 0.7231515656967000272, 0.7498110445554999615, 0.7764705234143999268, 0.8031300022731999722, 0.8297894811320000175, 0.8564489599908999828, 0.8831084388497000282, 0.9097679177085999935, 0.9364273965674000388, 0.9630868754261999731, 0.9897463542851000495, 1.016405833144000015 ),
 .UNSPECIFIED. ) ;
#5613 = EDGE_CURVE ( 'NONE', #6251, #67640, #57468, .T. ) ;
#5614 = CARTESIAN_POINT ( 'NONE',  ( 11.35918179236250047, 3.761636028845500412, -6.384440618559000136 ) ) ;
#5615 = CARTESIAN_POINT ( 'NONE',  ( 12.51647491292534475, 0.6599616342124019486, 12.58270523616455705 ) ) ;
#5616 = CARTESIAN_POINT ( 'NONE',  ( 0.7791522574427000025, 2.971343835407000089, -0.7711576440234000351 ) ) ;
#5617 = B_SPLINE_CURVE_WITH_KNOTS ( 'NONE', 3,
 ( #60049, #7251, #33834, #56181 ),
 .UNSPECIFIED., .F., .F.,
 ( 4, 4 ),
 ( 0.000000000000000000, 1.000000000000000000 ),
 .UNSPECIFIED. ) ;
#5618 = B_SPLINE_CURVE_WITH_KNOTS ( 'NONE', 3,
 ( #51782, #9129, #50497, #65876 ),
 .UNSPECIFIED., .F., .F.,
 ( 4, 4 ),
 ( 0.000000000000000000, 1.000000000000000000 ),
 .UNSPECIFIED. ) ;
#5619 = CARTESIAN_POINT ( 'NONE',  ( 9.793983440715679833, 2.684660541979530635, -7.853435705109036213 ) ) ;
#5620 = CARTESIAN_POINT ( 'NONE',  ( 12.67305101672400269, 1.772831636685040957, 12.47465725448102170 ) ) ;
#5622 = CARTESIAN_POINT ( 'NONE',  ( 7.983198341228001205, 5.321913229613000063, 8.118244847118999630 ) ) ;
#5621 = CARTESIAN_POINT ( 'NONE',  ( 9.023797255587998833, 5.140789995332999851, -7.451702546394010085 ) ) ;
#5623 = CARTESIAN_POINT ( 'NONE',  ( 11.45764291764649911, 2.867875922590999771, -7.360052904210999891 ) ) ;
#5624 = CARTESIAN_POINT ( 'NONE',  ( 8.227131012390005438, 3.380163391545999207, -6.126525137394006393 ) ) ;
#5625 = CARTESIAN_POINT ( 'NONE',  ( 11.17788388625999829, 2.412139249855000056, -7.075601348558000048 ) ) ;
#5626 = CARTESIAN_POINT ( 'NONE',  ( 11.22823073745748168, 3.830325957789608715, 6.639671036489041001 ) ) ;
#5628 = LINE ( 'NONE', #42016, #42879 ) ;
#5627 = CARTESIAN_POINT ( 'NONE',  ( 12.73341336140044611, 10.78295181804158354, -4.410266442043442758 ) ) ;
#5629 = FACE_OUTER_BOUND ( 'NONE', #56136, .T. ) ;
#5630 = ORIENTED_EDGE ( 'NONE', *, *, #16251, .F. ) ;
#5631 = CARTESIAN_POINT ( 'NONE',  ( 12.55586324463467918, 0.5732756864902116556, 12.68257855878055906 ) ) ;
#5632 = CARTESIAN_POINT ( 'NONE',  ( 11.09999999999999964, 0.000000000000000000, 0.000000000000000000 ) ) ;
#5633 = FACE_OUTER_BOUND ( 'NONE', #9412, .T. ) ;
#5634 = CYLINDRICAL_SURFACE ( 'NONE', #68139, 1.350000000000000089 ) ;
#5635 = CARTESIAN_POINT ( 'NONE',  ( 12.54527475442097995, -3.068547466015818070, 13.53629565290702352 ) ) ;
#5636 = CARTESIAN_POINT ( 'NONE',  ( 12.21323965715487603, 2.701097325876321786, 13.62869820427204814 ) ) ;
#5637 = CARTESIAN_POINT ( 'NONE',  ( 9.048601287889788125, -3.999999532294070459, -8.698595322193611423 ) ) ;
#5638 = VERTEX_POINT ( 'NONE', #7129 ) ;
#5639 = FACE_OUTER_BOUND ( 'NONE', #26848, .T. ) ;
#5640 = CARTESIAN_POINT ( 'NONE',  ( 11.23424042080529794, -3.455907502640803042, -6.342116603374310380 ) ) ;
#5641 = CARTESIAN_POINT ( 'NONE',  ( 27.09999999999999787, 0.000000000000000000, 0.000000000000000000 ) ) ;
#5642 = CARTESIAN_POINT ( 'NONE',  ( 18.15531827657417097, -3.266808065250859983, 11.18265383028970206 ) ) ;
#5643 = VECTOR ( 'NONE', #1154, 1000.000000000000000 ) ;
#5644 = CARTESIAN_POINT ( 'NONE',  ( 18.17584245753825911, 2.573100139072833414, -12.43426722069302137 ) ) ;
#5645 = CARTESIAN_POINT ( 'NONE',  ( 8.631025703289717299, 3.780324811990126488, -5.892885401209013274 ) ) ;
#5646 = CARTESIAN_POINT ( 'NONE',  ( 11.63825819896753977, 3.148796120250299868, 7.339530235223699073 ) ) ;
#5647 = ADVANCED_FACE ( 'NONE', ( #60617 ), #65852, .T. ) ;
#5648 = EDGE_CURVE ( 'NONE', #39123, #11589, #544, .T. ) ;
#5649 = CARTESIAN_POINT ( 'NONE',  ( 4.599999999999999645, -1.875000000000000000, -13.78627172894481667 ) ) ;
#5650 = CARTESIAN_POINT ( 'NONE',  ( 10.97819314679000158, -5.476828481365000556, -7.128717489481000591 ) ) ;
#5651 = CARTESIAN_POINT ( 'NONE',  ( 4.740443173016209322, 0.1963495408493638184, -1.499999999999999778 ) ) ;
#5652 = CARTESIAN_POINT ( 'NONE',  ( 5.500000000000000000, -12.43893545635000031, -2.828937028792000152 ) ) ;
#5653 = CARTESIAN_POINT ( 'NONE',  ( 24.30001685126999789, 8.938702716825000394, -8.938676159935001309 ) ) ;
#5654 = CARTESIAN_POINT ( 'NONE',  ( 27.64127793187000037, 3.399999999999999911, 4.505338571134999803 ) ) ;
#5656 = AXIS2_PLACEMENT_3D ( 'NONE', #64708, #6680, #68666 ) ;
#5655 = B_SPLINE_CURVE_WITH_KNOTS ( 'NONE', 3,
 ( #1328, #22303, #32806, #38039, #16709, #55161, #64940, #59365, #64601, #22646, #12171, #39086, #33501, #22994, #6218, #27911, #11812, #12514, #43991, #43644, #27558, #6914, #49916, #2029 ),
 .UNSPECIFIED., .F., .F.,
 ( 4, 2, 2, 1, 2, 2, 2, 2, 2, 2, 1, 2, 4 ),
 ( 0.000000000000000000, 0.1250000000000000000, 0.1875000000000000278, 0.2500000000000000555, 0.3125000000000001110, 0.3750000000000001110, 0.5000000000000001110, 0.6250000000000001110, 0.7500000000000001110, 0.8125000000000001110, 0.8750000000000001110, 0.9375000000000001110, 1.000000000000000000 ),
 .UNSPECIFIED. ) ;
#5657 = VERTEX_POINT ( 'NONE', #39641 ) ;
#5658 = CARTESIAN_POINT ( 'NONE',  ( 9.003345280414000840, 2.319062457810000311, -7.919229449146000022 ) ) ;
#5659 = CARTESIAN_POINT ( 'NONE',  ( 11.30133863405320049, -3.465595476214000215, 6.818303296693398963 ) ) ;
#5660 = VERTEX_POINT ( 'NONE', #60273 ) ;
#5661 = DIRECTION ( 'NONE',  ( 0.000000000000000000, 1.000000000000000000, 0.000000000000000000 ) ) ;
#5662 = CARTESIAN_POINT ( 'NONE',  ( 11.52733460557258915, -3.793662715184400014, -8.761245990815998752 ) ) ;
#5663 = EDGE_LOOP ( 'NONE', ( #57772, #37739, #6022, #16331 ) ) ;
#5664 = CARTESIAN_POINT ( 'NONE',  ( 11.35545123989519922, 4.475221369382300196, 6.582230774881299595 ) ) ;
#5665 = CARTESIAN_POINT ( 'NONE',  ( 6.213089017450689866, -0.1141077043353598275, 1.127819592361385848 ) ) ;
#5666 = CARTESIAN_POINT ( 'NONE',  ( 23.91427437024694669, 3.339324960032359346, -12.90828973773218635 ) ) ;
#5667 = CARTESIAN_POINT ( 'NONE',  ( 0.7000000000000000666, 0.5773502691895999739, 1.000000000000000000 ) ) ;
#5668 = CARTESIAN_POINT ( 'NONE',  ( 11.06967835872019812, -4.754733798270200928, -7.024326263066900111 ) ) ;
#5669 = CARTESIAN_POINT ( 'NONE',  ( 12.39828470357503321, 0.4745495851175757784, -13.88909655036762913 ) ) ;
#5670 = CARTESIAN_POINT ( 'NONE',  ( 7.034235772605498482, 0.9591814253079407049, -0.6216893316854109619 ) ) ;
#5671 = FACE_OUTER_BOUND ( 'NONE', #53490, .T. ) ;
#5672 = CARTESIAN_POINT ( 'NONE',  ( 13.16012107570600342, 11.71981102724999957, 1.988987020038000209 ) ) ;
#5673 = ORIENTED_EDGE ( 'NONE', *, *, #4156, .F. ) ;
#5674 = ADVANCED_FACE ( 'NONE', ( #50133 ), #850, .F. ) ;
#5676 = EDGE_CURVE ( 'NONE', #44476, #61826, #45710, .T. ) ;
#5675 = CARTESIAN_POINT ( 'NONE',  ( 8.622785841227999626, 5.189036231907000030, -8.048606212067999977 ) ) ;
#5677 = ORIENTED_EDGE ( 'NONE', *, *, #48403, .F. ) ;
#5678 = CARTESIAN_POINT ( 'NONE',  ( 0.4268955145921133343, -1.033550240898596373, 3.083630227088956399 ) ) ;
#5679 = FILL_AREA_STYLE ('',( #53585 ) ) ;
#5680 = EDGE_CURVE ( 'NONE', #5660, #64040, #3877, .T. ) ;
#5681 = VERTEX_POINT ( 'NONE', #22857 ) ;
#5682 = CARTESIAN_POINT ( 'NONE',  ( 12.80505043854143388, 3.124999999999999556, -25.00000000000000000 ) ) ;
#5683 = CARTESIAN_POINT ( 'NONE',  ( 18.16381471383438395, -2.642962562933662607, -12.41712880859051893 ) ) ;
#5684 = CARTESIAN_POINT ( 'NONE',  ( 24.83136307050961022, -8.598812902131761859, 8.498673240716678734 ) ) ;
#5685 = CARTESIAN_POINT ( 'NONE',  ( 10.39393020684999946, 2.750000000000000000, -7.500000000000000000 ) ) ;
#5686 = CARTESIAN_POINT ( 'NONE',  ( 11.12914445903999905, -3.083861519183999977, 8.586004431109000024 ) ) ;
#5687 = CARTESIAN_POINT ( 'NONE',  ( 18.18000379063077787, -2.491959044355968711, -12.45343158201009359 ) ) ;
#5688 = CARTESIAN_POINT ( 'NONE',  ( 12.18832812670981092, -0.1018973686818604313, 13.89950237059086291 ) ) ;
#5689 = ORIENTED_EDGE ( 'NONE', *, *, #29167, .T. ) ;
#5690 = CARTESIAN_POINT ( 'NONE',  ( 12.03709034744600181, 11.69601057336999972, -4.586677359659000253 ) ) ;
#5691 = CARTESIAN_POINT ( 'NONE',  ( 17.97171023854900085, 11.57811841779999895, -4.879106015068000346 ) ) ;
#5692 = CARTESIAN_POINT ( 'NONE',  ( 9.176241837494625742, 3.342362352854908458, 6.922899494040819945 ) ) ;
#5693 = CARTESIAN_POINT ( 'NONE',  ( 4.823209043203000590, 0.3714911358654000018, -1.434864438388000041 ) ) ;
#5694 = AXIS2_PLACEMENT_3D ( 'NONE', #2431, #67086, #40520 ) ;
#5695 = EDGE_CURVE ( 'NONE', #53272, #13468, #54864, .T. ) ;
#5696 = CARTESIAN_POINT ( 'NONE',  ( 12.09997738314682891, -11.69706276465794126, 3.884924152325089697 ) ) ;
#5697 = CARTESIAN_POINT ( 'NONE',  ( 10.55101852147976871, 5.350099180695919721, -7.263329207706104462 ) ) ;
#5698 = CARTESIAN_POINT ( 'NONE',  ( 10.64126772939999910, -2.258710642251000156, -6.863482599505999815 ) ) ;
#5699 = EDGE_LOOP ( 'NONE', ( #50550, #18380, #44001, #64838 ) ) ;
#5700 = EDGE_LOOP ( 'NONE', ( #21842, #2888, #35871, #30193 ) ) ;
#5701 = CIRCLE ( 'NONE', #4559, 0.5000000000000000000 ) ;
#5702 = CARTESIAN_POINT ( 'NONE',  ( 10.95213788436999991, 5.154141894912999788, -5.181730563652999777 ) ) ;
#5703 = CARTESIAN_POINT ( 'NONE',  ( 7.910784822165987329, 5.348998117051813495, 7.262899563230552857 ) ) ;
#5704 = CARTESIAN_POINT ( 'NONE',  ( 17.74675502951912520, -3.228624035270135639, 13.62268076943954753 ) ) ;
#5705 = CARTESIAN_POINT ( 'NONE',  ( 23.60000000000000142, -2.548720605937000006, 12.21654710926000220 ) ) ;
#5706 = DIRECTION ( 'NONE',  ( -1.000000000000000000, 0.000000000000000000, 0.000000000000000000 ) ) ;
#5707 = CARTESIAN_POINT ( 'NONE',  ( 11.09999999999999964, 5.299999999999999822, -6.571291218949999902 ) ) ;
#5708 = CARTESIAN_POINT ( 'NONE',  ( 9.889963142879999225, 4.848366390061300102, -7.321163726496699553 ) ) ;
#5710 = CARTESIAN_POINT ( 'NONE',  ( 11.59999999999999964, 4.000000000000000000, 7.500000000000000000 ) ) ;
#5709 = CARTESIAN_POINT ( 'NONE',  ( 10.20365911260399905, -4.376739491155700712, 6.719118894894999805 ) ) ;
#5711 = CARTESIAN_POINT ( 'NONE',  ( 4.596693173016666023, -1.310679582531386389, -0.7554284705563492075 ) ) ;
#5712 = ORIENTED_EDGE ( 'NONE', *, *, #17839, .T. ) ;
#5713 = DIRECTION ( 'NONE',  ( 1.000000000000000000, 0.000000000000000000, 0.000000000000000000 ) ) ;
#5714 = CARTESIAN_POINT ( 'NONE',  ( 9.471368011205999693, -2.030678448189000118, 7.549764202121000523 ) ) ;
#5715 = CARTESIAN_POINT ( 'NONE',  ( 9.279101285863998072, 3.176316400316700150, 8.478738839062499366 ) ) ;
#5716 = CARTESIAN_POINT ( 'NONE',  ( 11.09999999999999964, 5.771037996939999637, -5.145626010725000476 ) ) ;
#5717 = CARTESIAN_POINT ( 'NONE',  ( 10.02990552045999983, -2.506467134554999809, 6.215414506835998942 ) ) ;
#5718 = CARTESIAN_POINT ( 'NONE',  ( 18.18005043799233178, 2.500000011518615395, -12.45159158845316405 ) ) ;
#5719 = CARTESIAN_POINT ( 'NONE',  ( 16.27289819560299833, -3.403267206945999934, -11.10251878130000058 ) ) ;
#5720 = CARTESIAN_POINT ( 'NONE',  ( 17.55505043854143565, 3.125000000000000000, -13.52084414783465682 ) ) ;
#5721 = CARTESIAN_POINT ( 'NONE',  ( 9.862621437244998290, -3.332852462363599777, -6.749162825004299648 ) ) ;
#5722 = CARTESIAN_POINT ( 'NONE',  ( 5.728532185269999744, -1.238562288345000040, 0.4630760545261999872 ) ) ;
#5723 = CARTESIAN_POINT ( 'NONE',  ( 11.46914282210477687, -3.732132604854249802, 8.332067702129235087 ) ) ;
#5724 = CARTESIAN_POINT ( 'NONE',  ( 17.60407896980289522, 1.760945483361004538, 12.47634044926096308 ) ) ;
#5725 = ORIENTED_EDGE ( 'NONE', *, *, #32832, .F. ) ;
#5726 = EDGE_CURVE ( 'NONE', #34183, #66927, #26512, .T. ) ;
#5727 = ADVANCED_FACE ( 'NONE', ( #40325 ), #43617, .T. ) ;
#5728 = CARTESIAN_POINT ( 'NONE',  ( 12.51886017880454816, 0.5557204214162397848, -12.68363025601217231 ) ) ;
#5729 = CARTESIAN_POINT ( 'NONE',  ( 11.24441369783139777, 3.956299011112040187, -8.365094684940499903 ) ) ;
#5730 = CARTESIAN_POINT ( 'NONE',  ( 9.475279990687656806, -5.350441389720279162, 7.499985493516659218 ) ) ;
#5731 = CARTESIAN_POINT ( 'NONE',  ( 24.98214528072500329, -8.515982190356998771, 8.483938328266001250 ) ) ;
#5732 = LINE ( 'NONE', #6077, #6965 ) ;
#5733 = VERTEX_POINT ( 'NONE', #16497 ) ;
#5734 = CARTESIAN_POINT ( 'NONE',  ( 25.29577264028900174, -11.38513750862999885, -3.114196631034000351 ) ) ;
#5735 = CONTEXT_DEPENDENT_SHAPE_REPRESENTATION ( #48092, #56886 ) ;
#5736 = CARTESIAN_POINT ( 'NONE',  ( 10.57102344389999971, -4.762665848028800220, -7.037150754511299233 ) ) ;
#5737 = CARTESIAN_POINT ( 'NONE',  ( 7.000000000000000000, 0.8000000000000000444, 3.149999999999999911 ) ) ;
#5738 = CARTESIAN_POINT ( 'NONE',  ( 25.59994555223600088, -1.356777910713382829, -11.13814279612294911 ) ) ;
#5739 = CARTESIAN_POINT ( 'NONE',  ( 11.30000000000000071, 0.000000000000000000, 0.000000000000000000 ) ) ;
#5740 = CARTESIAN_POINT ( 'NONE',  ( 10.48791429142999831, 4.016993441347180394, -6.608036045330599961 ) ) ;
#5741 = ORIENTED_EDGE ( 'NONE', *, *, #13743, .F. ) ;
#5742 = CARTESIAN_POINT ( 'NONE',  ( 10.72520823780999955, -5.521647200017000934, 6.612992938078999572 ) ) ;
#5743 = CARTESIAN_POINT ( 'NONE',  ( 18.00577237252829832, 2.933105347812601238, -13.57200668515162612 ) ) ;
#5744 = EDGE_LOOP ( 'NONE', ( #37231, #47503, #60698, #46344, #65796, #13780, #14925, #14592, #30451, #42264, #12133, #27894 ) ) ;
#5745 = CARTESIAN_POINT ( 'NONE',  ( 4.599999999999999645, 3.199698446519375850, 12.18695736643652694 ) ) ;
#5746 = CARTESIAN_POINT ( 'NONE',  ( 7.416894353206999746, -3.448181789123000218, 9.222458996124998976 ) ) ;
#5747 = CARTESIAN_POINT ( 'NONE',  ( 15.39421883851900219, 8.828753284254000633, 7.820747050108999510 ) ) ;
#5748 = VERTEX_POINT ( 'NONE', #28037 ) ;
#5749 = DIRECTION ( 'NONE',  ( 0.000000000000000000, 0.8648648648648720183, 0.5020047465136825426 ) ) ;
#5750 = VECTOR ( 'NONE', #54885, 1000.000000000000000 ) ;
#5751 = CARTESIAN_POINT ( 'NONE',  ( 7.125270280406000190, 3.516145570366999706, -5.836512876186000121 ) ) ;
#5752 = B_SPLINE_CURVE_WITH_KNOTS ( 'NONE', 3,
 ( #2568, #55025, #39637, #28111 ),
 .UNSPECIFIED., .F., .F.,
 ( 4, 4 ),
 ( 0.000000000000000000, 1.000000000000000000 ),
 .UNSPECIFIED. ) ;
#5753 = CARTESIAN_POINT ( 'NONE',  ( 10.10434687351566474, -2.749999999999998224, -7.336375382625535124 ) ) ;
#5754 = FACE_OUTER_BOUND ( 'NONE', #33608, .T. ) ;
#5755 = ORIENTED_EDGE ( 'NONE', *, *, #26356, .F. ) ;
#5756 = CARTESIAN_POINT ( 'NONE',  ( 9.691080333872001518, -5.335644368206000188, 8.701217921043999937 ) ) ;
#5757 = CARTESIAN_POINT ( 'NONE',  ( 11.59999999999999787, 3.244119941477264124, 8.017883087166149281 ) ) ;
#5758 = FILL_AREA_STYLE ('',( #6447 ) ) ;
#5759 = ORIENTED_EDGE ( 'NONE', *, *, #54309, .T. ) ;
#5760 = CARTESIAN_POINT ( 'NONE',  ( 6.284193173016666911, 1.460959015002474493, -0.3926218265389176953 ) ) ;
#5761 = CARTESIAN_POINT ( 'NONE',  ( 11.50029455687000102, 11.65000000000000036, 0.000000000000000000 ) ) ;
#5762 = EDGE_CURVE ( 'NONE', #58951, #32339, #48176, .T. ) ;
#5763 = ORIENTED_EDGE ( 'NONE', *, *, #20514, .T. ) ;
#5764 = CARTESIAN_POINT ( 'NONE',  ( 4.599999999999999645, 14.00000000000000000, 0.000000000000000000 ) ) ;
#5765 = CARTESIAN_POINT ( 'NONE',  ( 11.87299956498129916, -5.207010770456999893, 7.825000000000000178 ) ) ;
#5766 = CARTESIAN_POINT ( 'NONE',  ( 4.521719878954000293, -1.371967559285000027, 0.7372657696301000430 ) ) ;
#5767 = VECTOR ( 'NONE', #41307, 1000.000000000000000 ) ;
#5768 = CARTESIAN_POINT ( 'NONE',  ( 5.199999999919999283, -1.376649745807000169, 11.21582968289000171 ) ) ;
#5769 = CARTESIAN_POINT ( 'NONE',  ( 16.13854985688900001, 3.352851047014000052, 11.81842075147999971 ) ) ;
#5770 = CARTESIAN_POINT ( 'NONE',  ( 11.18220574173929904, 5.136173005413447790, 8.088082908809449023 ) ) ;
#5771 = CARTESIAN_POINT ( 'NONE',  ( 3.250973465878000290, -3.500000000000000000, 0.000000000000000000 ) ) ;
#5772 = ORIENTED_EDGE ( 'NONE', *, *, #2406, .T. ) ;
#5773 = CARTESIAN_POINT ( 'NONE',  ( 13.68260097612285264, -12.30227370000369369, -2.353106563162954856 ) ) ;
#5774 = EDGE_LOOP ( 'NONE', ( #62241, #18788, #62914, #11173, #11266, #8511, #43070, #55165 ) ) ;
#5775 = CARTESIAN_POINT ( 'NONE',  ( 10.35616100078999935, 2.777276096020000029, 8.995275123087999702 ) ) ;
#5776 = FACE_OUTER_BOUND ( 'NONE', #38008, .T. ) ;
#5777 = CARTESIAN_POINT ( 'NONE',  ( 17.60000001994400165, -11.53041320601000130, 4.891397783926000109 ) ) ;
#5778 = CARTESIAN_POINT ( 'NONE',  ( 12.31461592258503046, 2.887558836668429052, -13.58358613427759209 ) ) ;
#5779 = CARTESIAN_POINT ( 'NONE',  ( 9.179055905797000037, 2.899999999999999911, 6.571291218949999902 ) ) ;
#5780 = CARTESIAN_POINT ( 'NONE',  ( 8.938754677014808081, -4.205681946487742628, -6.150054534049018251 ) ) ;
#5781 = EDGE_CURVE ( 'NONE', #21446, #46265, #19822, .T. ) ;
#5782 = DIRECTION ( 'NONE',  ( -1.000000000000000000, 0.000000000000000000, 0.000000000000000000 ) ) ;
#5783 = CARTESIAN_POINT ( 'NONE',  ( 9.425619671860273385, -4.846212772418011738, -9.064231341663099073 ) ) ;
#5784 = ORIENTED_EDGE ( 'NONE', *, *, #9101, .F. ) ;
#5785 = CARTESIAN_POINT ( 'NONE',  ( 12.33489288317251820, 0.4118289862746073449, 13.89178842664828295 ) ) ;
#5786 = CARTESIAN_POINT ( 'NONE',  ( 11.09195391537400077, -2.942766577210000012, 6.781965272201699868 ) ) ;
#5787 = CARTESIAN_POINT ( 'NONE',  ( 17.55505043854144276, -0.6250000000000001110, -25.00000000000000000 ) ) ;
#5788 = CARTESIAN_POINT ( 'NONE',  ( 17.88363324753128580, -0.5317637309696081616, -13.88630818040599202 ) ) ;
#5789 = CARTESIAN_POINT ( 'NONE',  ( 8.630418146794999856, -5.808258301303999893, 7.446016267012000256 ) ) ;
#5790 = B_SPLINE_CURVE_WITH_KNOTS ( 'NONE', 3,
 ( #65452, #23500, #28064, #18265 ),
 .UNSPECIFIED., .F., .F.,
 ( 4, 4 ),
 ( 0.000000000000000000, 1.000000000000000000 ),
 .UNSPECIFIED. ) ;
#5792 = CARTESIAN_POINT ( 'NONE',  ( 10.09999999999999964, 0.000000000000000000, 0.000000000000000000 ) ) ;
#5791 = CARTESIAN_POINT ( 'NONE',  ( 9.137543006348998631, 2.995704926864999784, 8.544754656710999541 ) ) ;
#5793 = CARTESIAN_POINT ( 'NONE',  ( 10.20226357027499908, 5.120085139777000194, -7.716099591766099053 ) ) ;
#5794 = CONICAL_SURFACE ( 'NONE', #31512, 11.34994642770999818, 0.7853934433896081480 ) ;
#5795 = CARTESIAN_POINT ( 'NONE',  ( 7.450407011341527053, 4.176709736710048304, -6.150651269157633827 ) ) ;
#5796 = CARTESIAN_POINT ( 'NONE',  ( 17.68520301169487752, 11.41062399034242425, -4.624005385410825397 ) ) ;
#5797 = CARTESIAN_POINT ( 'NONE',  ( 17.65692019170432303, -0.6169782284476043044, 12.67981870385669652 ) ) ;
#5798 = CARTESIAN_POINT ( 'NONE',  ( 6.670498187669999801, -0.9697342503638000100, -1.215263594530000102 ) ) ;
#5799 = DIRECTION ( 'NONE',  ( 0.000000000000000000, -1.000000000000000000, 0.000000000000000000 ) ) ;
#5800 = ORIENTED_EDGE ( 'NONE', *, *, #15501, .T. ) ;
#5801 = CARTESIAN_POINT ( 'NONE',  ( 9.385311019873999072, -4.135077143711000325, 9.175520401071999288 ) ) ;
#5802 = CARTESIAN_POINT ( 'NONE',  ( 9.700639158771000581, 4.262870449202000422, -8.811513791423999820 ) ) ;
#5803 = B_SPLINE_CURVE_WITH_KNOTS ( 'NONE', 3,
 ( #19029, #40356, #61678, #4314, #13794, #35125, #32288, #42074, #57803, #31589 ),
 .UNSPECIFIED., .F., .F.,
 ( 4, 2, 2, 2, 4 ),
 ( 0.000000000000000000, 0.2500000000000000000, 0.5000000000000000000, 0.7500000000000000000, 1.000000000000000000 ),
 .UNSPECIFIED. ) ;
#5804 = B_SPLINE_CURVE_WITH_KNOTS ( 'NONE', 3,
 ( #53262, #44169, #33326, #59881, #17236, #119, #48357, #32298, #64767, #6046, #21437, #54287 ),
 .UNSPECIFIED., .F., .F.,
 ( 4, 2, 2, 2, 2, 4 ),
 ( 0.000000000000000000, 0.2499999999999962252, 0.3749999999999931721, 0.4374999999999933942, 0.4999999999999935607, 1.000000000000000000 ),
 .UNSPECIFIED. ) ;
#5805 = DIRECTION ( 'NONE',  ( -3.667724557042155543E-10, -0.9466472399347399813, 0.3222716294121134584 ) ) ;
#5806 = CARTESIAN_POINT ( 'NONE',  ( 5.000000000000000000, 0.2999999999999999889, -11.34603454956999791 ) ) ;
#5807 = AXIS2_PLACEMENT_3D ( 'NONE', #43470, #38208, #52919 ) ;
#5808 = CARTESIAN_POINT ( 'NONE',  ( 0.6667688295322999892, -3.457229061792999936, 0.7500022461462000356 ) ) ;
#5809 = CARTESIAN_POINT ( 'NONE',  ( 17.55505043854143565, 3.125000000000000000, -12.28374638332999602 ) ) ;
#5810 = CIRCLE ( 'NONE', #231, 1.350000000000000311 ) ;
#5811 = CARTESIAN_POINT ( 'NONE',  ( 10.23581084123000018, 3.621841509808999771, -8.806208131805998818 ) ) ;
#5812 = ORIENTED_EDGE ( 'NONE', *, *, #50129, .T. ) ;
#5813 = EDGE_CURVE ( 'NONE', #32611, #22269, #631, .T. ) ;
#5814 = EDGE_CURVE ( 'NONE', #46546, #57489, #13881, .T. ) ;
#5815 = CARTESIAN_POINT ( 'NONE',  ( 23.59999172237900211, -2.915589696762999949, -13.58550518520000061 ) ) ;
#5816 = LINE ( 'NONE', #54058, #24182 ) ;
#5817 = CARTESIAN_POINT ( 'NONE',  ( 17.70945903195347171, 3.183352579998539156, -12.19123751323113325 ) ) ;
#5818 = CARTESIAN_POINT ( 'NONE',  ( 15.83979990366733048, -8.664995957719217046, -8.086229679809637361 ) ) ;
#5819 = CARTESIAN_POINT ( 'NONE',  ( 7.886573341228999112, 3.084076314893000159, 9.259847992573000397 ) ) ;
#5820 = VERTEX_POINT ( 'NONE', #52798 ) ;
#5821 = CARTESIAN_POINT ( 'NONE',  ( 5.953532185270000276, -1.375515609181000132, 0.5142804259680000545 ) ) ;
#5822 = EDGE_CURVE ( 'NONE', #42736, #2331, #38891, .T. ) ;
#5823 = EDGE_CURVE ( 'NONE', #15298, #12624, #27250, .T. ) ;
#5824 = CARTESIAN_POINT ( 'NONE',  ( 7.657479719584999955, 2.267583043933999676, -7.494013172964999470 ) ) ;
#5825 = CARTESIAN_POINT ( 'NONE',  ( 8.409821582311559851, -2.468534350186054382, 8.326276327825025803 ) ) ;
#5826 = CARTESIAN_POINT ( 'NONE',  ( 9.750696787962999323, -3.780328739572700325, 8.760209873321999297 ) ) ;
#5827 = ORIENTED_EDGE ( 'NONE', *, *, #55658, .F. ) ;
#5828 = CARTESIAN_POINT ( 'NONE',  ( 16.20650642310300071, -3.719849042574000286, -12.00042637259999978 ) ) ;
#5829 = CARTESIAN_POINT ( 'NONE',  ( 11.83156678923300120, 11.57054462408999917, 1.756438942007999993 ) ) ;
#5830 = ORIENTED_EDGE ( 'NONE', *, *, #50623, .F. ) ;
#5831 = CARTESIAN_POINT ( 'NONE',  ( 12.15578049617548650, 2.108731457858032066, -12.42302753736613852 ) ) ;
#5832 = DIRECTION ( 'NONE',  ( -1.000000000000000000, 0.000000000000000000, 0.000000000000000000 ) ) ;
#5833 = CARTESIAN_POINT ( 'NONE',  ( 17.69685691690358809, -0.6090406077983145927, -13.88203505342130661 ) ) ;
#5834 = B_SPLINE_CURVE_WITH_KNOTS ( 'NONE', 3,
 ( #29587, #65582, #60687, #23975 ),
 .UNSPECIFIED., .F., .F.,
 ( 4, 4 ),
 ( 0.000000000000000000, 1.000000000000000000 ),
 .UNSPECIFIED. ) ;
#5835 = ORIENTED_EDGE ( 'NONE', *, *, #10138, .F. ) ;
#5836 = CARTESIAN_POINT ( 'NONE',  ( 13.50003721581400029, 9.159934378815998812, 7.517910889891000537 ) ) ;
#5837 = CARTESIAN_POINT ( 'NONE',  ( 11.02812378248509795, 3.583106837161099900, -6.711274001288999536 ) ) ;
#5838 = DIRECTION ( 'NONE',  ( -1.000000000000000000, 0.000000000000000000, 0.000000000000000000 ) ) ;
#5839 = CARTESIAN_POINT ( 'NONE',  ( 11.68272066707849888, -2.906477115133000222, 8.161456030935699602 ) ) ;
#5840 = VERTEX_POINT ( 'NONE', #52097 ) ;
#5841 = CARTESIAN_POINT ( 'NONE',  ( 8.951357780412001475, 2.821863697211000055, 6.127145479358000024 ) ) ;
#5842 = EDGE_CURVE ( 'NONE', #18715, #59008, #18422, .T. ) ;
#5843 = ORIENTED_EDGE ( 'NONE', *, *, #44982, .T. ) ;
#5844 = LINE ( 'NONE', #21921, #55246 ) ;
#5845 = CARTESIAN_POINT ( 'NONE',  ( 3.400000000000000355, 1.500000000000000000, 0.000000000000000000 ) ) ;
#5846 = CARTESIAN_POINT ( 'NONE',  ( 8.970944094206998898, -5.100000000000000533, 6.571291218949999902 ) ) ;
#5847 = ORIENTED_EDGE ( 'NONE', *, *, #13972, .F. ) ;
#5848 = CARTESIAN_POINT ( 'NONE',  ( 12.57288091590949897, -1.919630123611445693, -12.56800073041603305 ) ) ;
#5849 = CARTESIAN_POINT ( 'NONE',  ( 0.4002456762477398788, -2.971400501378169245, -1.711618823381010790 ) ) ;
#5850 = CARTESIAN_POINT ( 'NONE',  ( 25.46372676430900128, 8.354609436172999892, -8.148458316574000548 ) ) ;
#5851 = FACE_OUTER_BOUND ( 'NONE', #58259, .T. ) ;
#5852 = CARTESIAN_POINT ( 'NONE',  ( 12.14271297744737232, -2.220151667091626813, -13.82285866607422520 ) ) ;
#5853 = CARTESIAN_POINT ( 'NONE',  ( 11.60533460557258323, -3.815825449682300086, -8.625775273268001087 ) ) ;
#5854 = CARTESIAN_POINT ( 'NONE',  ( 13.69997185827400088, -11.21472423003502072, -3.290649947225299243 ) ) ;
#5855 = CARTESIAN_POINT ( 'NONE',  ( 17.84599613952814678, -3.139413506986239888, 12.20262697555082632 ) ) ;
#5856 = ORIENTED_EDGE ( 'NONE', *, *, #156, .F. ) ;
#5857 = CARTESIAN_POINT ( 'NONE',  ( 11.55811496860034815, -2.954409148022000053, -6.964183526617899744 ) ) ;
#5858 = EDGE_LOOP ( 'NONE', ( #30264, #4082, #21481, #58613 ) ) ;
#5859 = AXIS2_PLACEMENT_3D ( 'NONE', #65495, #17622, #55021 ) ;
#5860 = CARTESIAN_POINT ( 'NONE',  ( 11.40162633574000139, -12.25609765133000018, -1.727435033673999865 ) ) ;
#5861 = CARTESIAN_POINT ( 'NONE',  ( 12.06914347478616811, -3.251273819902354312, 6.470125748842364466 ) ) ;
#5862 = CARTESIAN_POINT ( 'NONE',  ( 5.227606837614000135, -0.3108367803229999948, 1.065889863396000115 ) ) ;
#5863 = CARTESIAN_POINT ( 'NONE',  ( 10.38314899745999931, 5.167567567567999731, 6.822293592207000934 ) ) ;
#5864 = EDGE_CURVE ( 'NONE', #50878, #22693, #46442, .T. ) ;
#5865 = CARTESIAN_POINT ( 'NONE',  ( 24.30001696810800027, 12.21047201856000086, 3.271805692349999628 ) ) ;
#5866 = FACE_OUTER_BOUND ( 'NONE', #10133, .T. ) ;
#5867 = CARTESIAN_POINT ( 'NONE',  ( 2.800973465877999669, -3.500000000000000000, 0.000000000000000000 ) ) ;
#5868 = VERTEX_POINT ( 'NONE', #47211 ) ;
#5869 = ADVANCED_FACE ( 'NONE', ( #41278 ), #26231, .F. ) ;
#5870 = CARTESIAN_POINT ( 'NONE',  ( 18.44382898362900036, 2.795331802377000407, 11.36579223931000016 ) ) ;
#5871 = CARTESIAN_POINT ( 'NONE',  ( 9.691082467489000152, 5.335647408863999352, 8.701220655673999715 ) ) ;
#5872 = CARTESIAN_POINT ( 'NONE',  ( 2.290556799209333860, -3.500000000000002220, 0.4581489286484968781 ) ) ;
#5873 = CARTESIAN_POINT ( 'NONE',  ( 12.14633327354034797, -4.864904118400500188, 8.065722083251399610 ) ) ;
#5874 = CARTESIAN_POINT ( 'NONE',  ( 18.26001707275200303, 2.811958703674000137, -11.55267125806999928 ) ) ;
#5875 = CARTESIAN_POINT ( 'NONE',  ( 10.91982473337999870, 9.073386231760999010, -6.344452675278001053 ) ) ;
#5876 = CARTESIAN_POINT ( 'NONE',  ( 24.37816192507718327, -12.29708154334037928, -3.190021095768833082 ) ) ;
#5877 = CARTESIAN_POINT ( 'NONE',  ( 6.703785368954362944, -0.9921252471994713718, 0.7441235177248552990 ) ) ;
#5878 = LINE ( 'NONE', #58681, #31660 ) ;
#5879 = CARTESIAN_POINT ( 'NONE',  ( 23.60000000000000497, -11.54188282345546490, 7.798337198497422129 ) ) ;
#5880 = B_SPLINE_SURFACE_WITH_KNOTS ( 'NONE', 3, 3, ( 
 ( #13761, #29517, #14452, #35432, #50820, #35772, #51840, #45581, #57424, #56758, #40326, #8855, #3593, #67916, #20032, #61647, #39993, #8510, #29859, #51167, #3262, #37144, #53564, #21398, #59146, #42731, #11250, #10568, #16156, #43069, #64035, #58806, #31224, #64376, #63003, #52531, #46949, #42395, #5321, #52880, #47641, #25622, #37825, #27000, #5659, #37480, #15132, #42046, #25966, #48316, #20374, #41697, #15814, #4628, #36452, #10911, #57771, #31560, #26663, #68951, #4979, #16498, #21064, #32255, #421, #15480, #10226 ),
 ( #68254, #21738, #9882, #31906, #32588, #4286, #63701, #47295, #68598, #26312, #20719, #58461, #63352, #53220, #36805, #58125, #47979, #81, #50311, #13262, #7656, #38161, #50654, #56242, #64723, #768, #23733, #34587, #2074, #8348, #61144, #16839, #39824, #2754, #2410, #22084, #12909, #18499, #34925, #24078, #40497, #45415, #61824, #55902, #66724, #24429, #18844, #40170, #11588, #45753, #43429, #32932, #27342, #45071, #8006, #34237, #29002, #6001, #19174, #29694, #50995, #61486, #59489, #23392, #6344, #3094, #54242 ),
 ( #13604, #27693, #67063, #49009, #13942, #44732, #53901, #48664, #66029, #18153, #39474, #66375, #60796, #55556, #29342, #20894, #56585, #52707, #24767, #41528, #42231, #63537, #25449, #3431, #20550, #35942, #67400, #4112, #15310, #62841, #19521, #51672, #4801, #10056, #30700, #14960, #57255, #40841, #31053, #36634, #46093, #51337, #46781, #36284, #3769, #25106, #57958, #62164, #14623, #14286, #35612, #8688, #35268, #26145, #62500, #67740, #56925, #68427, #68085, #46438, #31392, #30035, #57601, #9024, #30364, #9707, #19864 ),
 ( #4455, #20201, #41195, #9356, #41874, #52009, #52363, #25796, #47126, #63180, #47470, #68776, #37318, #49184, #27177, #47820, #48500, #58990, #1295, #5839, #53056, #952, #16330, #69129, #53742, #64903, #21916, #21234, #32087, #33115, #59675, #11092, #43253, #37659, #42565, #11427, #17016, #26490, #31737, #604, #64559, #53403, #5501, #38347, #63873, #64215, #15987, #58637, #58293, #15648, #54430, #42910, #48154, #5155, #48847, #16674, #26838, #11772, #36982, #38000, #10741, #257, #59326, #21572, #43605, #6531, #32426 ) ),
 .UNSPECIFIED., .F., .F., .F.,
 ( 4, 4 ),
 ( 4, 1, 1, 1, 1, 1, 1, 1, 1, 1, 1, 1, 1, 1, 1, 1, 1, 1, 1, 1, 1, 1, 1, 1, 1, 1, 1, 1, 1, 1, 1, 1, 1, 1, 1, 1, 1, 1, 1, 1, 1, 1, 1, 1, 1, 1, 1, 1, 1, 1, 1, 1, 1, 1, 1, 1, 1, 1, 1, 1, 1, 1, 1, 1, 4 ),
 ( -0.02000000000000000042, 1.020000000000000018 ),
 ( 0.008747244164287000176, 0.02453926110774999961, 0.04033127805120999970, 0.05612329499467000327, 0.07191531193812999989, 0.08770732888158999652, 0.1034993458251000087, 0.1192913627684999978, 0.1350833797120000179, 0.1508753966553999792, 0.1666674135988999994, 0.1824594305423999918, 0.1982514474858000086, 0.2140434644293000011, 0.2298354813727000179, 0.2456274983162000103, 0.2614195152596999749, 0.2772115322030999640, 0.2930035491465999842, 0.3087955660900000288, 0.3245875830334999934, 0.3403795999769999581, 0.3561716169204000026, 0.3719636338639000228, 0.3877556508073999875, 0.4035476677507999765, 0.4193396846942999967, 0.4351317016376999858, 0.4509237185811999504, 0.4667157355247000261, 0.4825077524681000152, 0.4982997694115999798, 0.5140917863550000799, 0.5298838032985000446, 0.5456758202420000092, 0.5614678371854000538, 0.5772598541289000185, 0.5930518710723000630, 0.6088438880158000277, 0.6246359049592999924, 0.6404279219027000369, 0.6562199388462000016, 0.6720119557896999662, 0.6878039727331000108, 0.7035959896765999755, 0.7193880066200000201, 0.7351800235634999847, 0.7509720405069999494, 0.7667640574504001050, 0.7825560743939000696, 0.7983480913373000032, 0.8141401082808000789, 0.8299321252243000435, 0.8457241421676999771, 0.8615161591112000528, 0.8773081760545999863, 0.8931001929981000620, 0.9088922099416000266, 0.9246842268849999602, 0.9404762438285000359, 0.9562682607720000005, 0.9720602777153999341, 0.9878522946589000098, 1.003644311601999961, 1.019436328545999970 ),
 .UNSPECIFIED. ) ;
#5881 = EDGE_LOOP ( 'NONE', ( #68785, #2160, #1312, #17723 ) ) ;
#5882 = CARTESIAN_POINT ( 'NONE',  ( 6.900000172107000118, -1.065814103639999922E-14, 1.505462421391999793E-13 ) ) ;
#5883 = CARTESIAN_POINT ( 'NONE',  ( 7.360284615040999512, -1.128968895613000178, 0.4485929593892000189 ) ) ;
#5884 = CARTESIAN_POINT ( 'NONE',  ( 18.14139820495726241, 2.283379482803411076, 13.71697381851087805 ) ) ;
#5885 = DIRECTION ( 'NONE',  ( -0.000000000000000000, 1.000000000000000000, 0.000000000000000000 ) ) ;
#5886 = CARTESIAN_POINT ( 'NONE',  ( 10.37457053952199892, -4.448306506338299826, -6.451042711717000167 ) ) ;
#5887 = ORIENTED_EDGE ( 'NONE', *, *, #37167, .F. ) ;
#5888 = CONICAL_SURFACE ( 'NONE', #68413, 0.9999998338055000602, 0.7853981908209605178 ) ;
#5889 = FACE_OUTER_BOUND ( 'NONE', #42644, .T. ) ;
#5890 = CARTESIAN_POINT ( 'NONE',  ( 7.641204719590000138, 4.524487726177000013, 9.047753146378999745 ) ) ;
#5892 = DIRECTION ( 'NONE',  ( 0.000000000000000000, 0.000000000000000000, 1.000000000000000000 ) ) ;
#5891 = CARTESIAN_POINT ( 'NONE',  ( 8.365779719592000063, 2.949305648881000330, -8.659807625323999503 ) ) ;
#5893 = CARTESIAN_POINT ( 'NONE',  ( 2.603868863154109370, -1.826195839757124739, -2.697973947297320763 ) ) ;
#5894 = ORIENTED_EDGE ( 'NONE', *, *, #43878, .F. ) ;
#5895 = CARTESIAN_POINT ( 'NONE',  ( 9.555697025339000561, 2.440752375194999768, 6.680879724048000234 ) ) ;
#5896 = CARTESIAN_POINT ( 'NONE',  ( 18.11095118117833636, -2.049130080444088620, -13.84922935676121902 ) ) ;
#5897 = CARTESIAN_POINT ( 'NONE',  ( 11.53564291764652872, 3.004110626587600308, 7.623106493640399606 ) ) ;
#5898 = CARTESIAN_POINT ( 'NONE',  ( 10.85068991645999859, -4.478102922274999287, 6.162028334171000488 ) ) ;
#5899 = CARTESIAN_POINT ( 'NONE',  ( 7.512831853207000421, -5.524126964933000927, 6.910359834012999691 ) ) ;
#5900 = VERTEX_POINT ( 'NONE', #25191 ) ;
#5901 = CARTESIAN_POINT ( 'NONE',  ( 8.203567189027999973, -3.399999998438999693, 6.139678690022999596 ) ) ;
#5902 = ADVANCED_FACE ( 'NONE', ( #15044 ), #64790, .F. ) ;
#5903 = EDGE_CURVE ( 'NONE', #57590, #69130, #63878, .T. ) ;
#5905 = CARTESIAN_POINT ( 'NONE',  ( 10.88760685321000032, -5.634843745609000365, -7.088991614236999972 ) ) ;
#5904 = CARTESIAN_POINT ( 'NONE',  ( 12.17512857912400115, -11.55078329699999884, 4.188961560869000067 ) ) ;
#5906 = CARTESIAN_POINT ( 'NONE',  ( 7.876919724916979781, -2.918260083478235067, 8.873651148443707726 ) ) ;
#5907 = VECTOR ( 'NONE', #65601, 1000.000000000000000 ) ;
#5908 = CARTESIAN_POINT ( 'NONE',  ( 10.02990552045999983, -2.506467134554999809, 6.215414506835998942 ) ) ;
#5909 = CARTESIAN_POINT ( 'NONE',  ( 23.95204559793199905, 3.419365875930000076, 12.89885794585999967 ) ) ;
#5910 = ORIENTED_EDGE ( 'NONE', *, *, #9605, .F. ) ;
#5911 = CARTESIAN_POINT ( 'NONE',  ( 5.844609839683332808, 1.500000000000000888, -0.1963495408493590444 ) ) ;
#5912 = CARTESIAN_POINT ( 'NONE',  ( 10.82949413291699869, -3.087070836781100169, 7.916546720849799712 ) ) ;
#5913 = CARTESIAN_POINT ( 'NONE',  ( 11.47810404293059960, 3.436653965247300047, 6.352848032645000309 ) ) ;
#5914 = VERTEX_POINT ( 'NONE', #60456 ) ;
#5915 = CARTESIAN_POINT ( 'NONE',  ( 9.617764158771999305, 5.322769172805999816, -7.951018786192998178 ) ) ;
#5916 = CARTESIAN_POINT ( 'NONE',  ( 12.18347802452934658, 2.109676230065139269, -12.42212916133884981 ) ) ;
#5917 = CARTESIAN_POINT ( 'NONE',  ( 11.80878751119029957, -5.041025164610000608, 6.955365841266999638 ) ) ;
#5918 = EDGE_CURVE ( 'NONE', #39559, #49026, #27261, .T. ) ;
#5919 = VERTEX_POINT ( 'NONE', #39129 ) ;
#5920 = B_SPLINE_CURVE_WITH_KNOTS ( 'NONE', 3,
 ( #56004, #61249, #18944, #8111, #29454, #50763, #61934, #40273, #51103, #3205, #24532, #19281, #40606, #14047, #36394, #26601, #63978, #51783, #15069, #58402, #57710, #47234 ),
 .UNSPECIFIED., .F., .F.,
 ( 4, 2, 2, 1, 1, 2, 2, 2, 2, 2, 2, 4 ),
 ( 0.000000000000000000, 0.1249999999999412137, 0.1874999999999118205, 0.2187499999999014677, 0.2343749999999007738, 0.2421874999999004130, 0.2499999999999000799, 0.3749999999999177325, 0.4374999999999291123, 0.4687499999999334421, 0.4999999999999377165, 1.000000000000000000 ),
 .UNSPECIFIED. ) ;
#5921 = CARTESIAN_POINT ( 'NONE',  ( 9.231494046297843425, 3.294621473794871580, -8.705007087319614811 ) ) ;
#5922 = CARTESIAN_POINT ( 'NONE',  ( 9.143927823787141307, -2.750011555256801188, -7.499999844943244121 ) ) ;
#5923 = ORIENTED_EDGE ( 'NONE', *, *, #1012, .F. ) ;
#5924 = CARTESIAN_POINT ( 'NONE',  ( 8.689254440380000943, -2.550228841911000188, 7.666975032000999946 ) ) ;
#5925 = CARTESIAN_POINT ( 'NONE',  ( 17.33333333119166753, 3.345268056437870730, 11.86064107241928411 ) ) ;
#5926 = ORIENTED_EDGE ( 'NONE', *, *, #2620, .F. ) ;
#5927 = DIRECTION ( 'NONE',  ( 0.000000000000000000, 0.000000000000000000, -1.000000000000000000 ) ) ;
#5928 = CARTESIAN_POINT ( 'NONE',  ( 11.70794988689359961, 4.455786710255300598, 6.606015074393400077 ) ) ;
#5929 = CARTESIAN_POINT ( 'NONE',  ( 10.25461802485000007, 2.860644035673999941, 6.604613005744999654 ) ) ;
#5930 = CARTESIAN_POINT ( 'NONE',  ( 11.13731690826999809, 2.663709268392000062, -5.187964601092999395 ) ) ;
#5931 = CARTESIAN_POINT ( 'NONE',  ( 7.935109315130008056, 5.090269470254001227, 6.488511505667004187 ) ) ;
#5932 = CARTESIAN_POINT ( 'NONE',  ( 10.50244460374000077, -2.268915328469999881, 7.824865002012999504 ) ) ;
#5933 = CARTESIAN_POINT ( 'NONE',  ( 13.73854985688900143, 9.171197327466000360, 8.173482659384999849 ) ) ;
#5934 = CARTESIAN_POINT ( 'NONE',  ( 17.81315952985430329, 0.5693054069933394246, -12.68281928773557787 ) ) ;
#5935 = CARTESIAN_POINT ( 'NONE',  ( 12.22109980851669953, 2.722998852138081016, -12.39684006587159892 ) ) ;
#5936 = CARTESIAN_POINT ( 'NONE',  ( 11.36333594839950045, -3.340240242524600056, -6.743912759487099784 ) ) ;
#5937 = CARTESIAN_POINT ( 'NONE',  ( 8.341920280410999311, 5.601795057054999916, 7.176148573050999957 ) ) ;
#5938 = ORIENTED_EDGE ( 'NONE', *, *, #33539, .F. ) ;
#5939 = AXIS2_PLACEMENT_3D ( 'NONE', #29957, #54164, #22352 ) ;
#5940 = AXIS2_PLACEMENT_3D ( 'NONE', #9837, #10522, #33586 ) ;
#5941 = SURFACE_SIDE_STYLE ('',( #59776 ) ) ;
#5942 = DIRECTION ( 'NONE',  ( 0.000000000000000000, -0.9048270524660053660, 0.4257792915651026910 ) ) ;
#5943 = CARTESIAN_POINT ( 'NONE',  ( 11.07758455333000036, 5.275003855962000721, -5.089091206712999416 ) ) ;
#5944 = CARTESIAN_POINT ( 'NONE',  ( 11.44438160092000167, 12.37754422778999874, 1.524124373512000030 ) ) ;
#5945 = CARTESIAN_POINT ( 'NONE',  ( 18.23116755655858867, 2.220104646260180559, 12.40287289761280576 ) ) ;
#5946 = B_SPLINE_CURVE_WITH_KNOTS ( 'NONE', 3,
 ( #42380, #21385, #53552, #5305, #15800 ),
 .UNSPECIFIED., .F., .F.,
 ( 4, 1, 4 ),
 ( 0.000000000000000000, 0.5000000000000000000, 1.000000000000000000 ),
 .UNSPECIFIED. ) ;
#5947 = CARTESIAN_POINT ( 'NONE',  ( 12.58164121395688007, 1.823227133926375698, 13.88077287699123197 ) ) ;
#5948 = CARTESIAN_POINT ( 'NONE',  ( 11.04954357929999986, 9.924925438703999347, 5.808563670758999820 ) ) ;
#5949 = ADVANCED_FACE ( 'NONE', ( #53485 ), #688, .T. ) ;
#5950 = DIRECTION ( 'NONE',  ( -1.000000000000000000, 0.000000000000000000, 0.000000000000000000 ) ) ;
#5951 = CARTESIAN_POINT ( 'NONE',  ( 25.50723805854519100, -2.874178715285141905, 11.25475534034192471 ) ) ;
#5952 = ORIENTED_EDGE ( 'NONE', *, *, #50358, .F. ) ;
#5953 = CARTESIAN_POINT ( 'NONE',  ( 12.54706542093076038, -3.153101027525017752, 12.19910009420584984 ) ) ;
#5954 = CARTESIAN_POINT ( 'NONE',  ( 9.125113844317997547, -3.711648483798899889, -6.395197822644999697 ) ) ;
#5955 = CARTESIAN_POINT ( 'NONE',  ( 24.25375554908000097, -3.234179890672000290, -12.21792844062999883 ) ) ;
#5956 = CARTESIAN_POINT ( 'NONE',  ( 10.87522165821000009, -4.831071966430999787, 6.312786525516999703 ) ) ;
#5957 = AXIS2_PLACEMENT_3D ( 'NONE', #23319, #24008, #34518 ) ;
#5958 = B_SPLINE_CURVE_WITH_KNOTS ( 'NONE', 1,
 ( #4205, #36027 ),
 .UNSPECIFIED., .F., .F.,
 ( 2, 2 ),
 ( 0.000000000000000000, 1.000000000000000000 ),
 .UNSPECIFIED. ) ;
#5959 = CARTESIAN_POINT ( 'NONE',  ( 11.13764426047339917, 4.613828180779599997, -8.461511872390000022 ) ) ;
#5960 = CARTESIAN_POINT ( 'NONE',  ( 12.27567264278500581, 0.4920215530101147428, 12.59040071882420797 ) ) ;
#5961 = B_SPLINE_CURVE_WITH_KNOTS ( 'NONE', 3,
 ( #16802, #44438, #49311, #1424, #38129, #32556, #38833, #60159, #11219, #54908 ),
 .UNSPECIFIED., .F., .F.,
 ( 4, 2, 2, 2, 4 ),
 ( 0.000000000000000000, 0.1954776249890681494, 0.3909552499781366319, 0.5864328749672050867, 0.7819104999562735969 ),
 .UNSPECIFIED. ) ;
#5962 = CARTESIAN_POINT ( 'NONE',  ( 8.727045280411999784, 3.882020551409000042, 5.870058896428999695 ) ) ;
#5963 = CARTESIAN_POINT ( 'NONE',  ( 5.184649729920792538, 0.2901060309370289136, 1.137486352124640776 ) ) ;
#5964 = CARTESIAN_POINT ( 'NONE',  ( 12.42670498308433658, 2.997500030636911728, 12.32161918487003405 ) ) ;
#5965 = CARTESIAN_POINT ( 'NONE',  ( 7.555281674562000838, 4.314040636970999820, 8.819134391732999845 ) ) ;
#5966 = CARTESIAN_POINT ( 'NONE',  ( 10.25149413291699929, 5.037815157227999663, -7.026470926762800495 ) ) ;
#5967 = CARTESIAN_POINT ( 'NONE',  ( 12.08097595789114642, 12.02669421650328019, -3.498808775432329377 ) ) ;
#5968 = CARTESIAN_POINT ( 'NONE',  ( 10.80374834123000127, 2.766954612461999918, -8.073381085840999560 ) ) ;
#5969 = CARTESIAN_POINT ( 'NONE',  ( 8.490822372493999737, 3.632306086542600010, -8.702849744394999476 ) ) ;
#5971 = CARTESIAN_POINT ( 'NONE',  ( 12.19705744689154692, 2.644897762231630534, 12.41662195483983488 ) ) ;
#5970 = CARTESIAN_POINT ( 'NONE',  ( 7.613778970466999141, 4.858908887722000358, 6.437635593844006188 ) ) ;
#5972 = CARTESIAN_POINT ( 'NONE',  ( 5.500000000000000000, 0.000000000000000000, 0.000000000000000000 ) ) ;
#5973 = ORIENTED_EDGE ( 'NONE', *, *, #31205, .F. ) ;
#5974 = CARTESIAN_POINT ( 'NONE',  ( 12.41737000022668269, 0.4903651763005736353, 12.68725775796289312 ) ) ;
#5975 = CARTESIAN_POINT ( 'NONE',  ( 23.60000337037311979, -10.25353992318573759, -9.380071257702633503 ) ) ;
#5976 = CARTESIAN_POINT ( 'NONE',  ( 11.92303154622437411, -11.77792023318479586, 4.262523390541344881 ) ) ;
#5977 = CARTESIAN_POINT ( 'NONE',  ( 17.55505043854143565, 1.760845406083394682, -12.47635457398814829 ) ) ;
#5978 = CARTESIAN_POINT ( 'NONE',  ( 12.08002994951554498, -2.497059486053643695, 13.77553160571068247 ) ) ;
#5979 = CARTESIAN_POINT ( 'NONE',  ( 10.85956136387000015, 2.936952989063999819, 5.179223561060999792 ) ) ;
#5980 = DIRECTION ( 'NONE',  ( 1.000000000000000000, 0.000000000000000000, 0.000000000000000000 ) ) ;
#5981 = VERTEX_POINT ( 'NONE', #16414 ) ;
#5982 = EDGE_CURVE ( 'NONE', #66075, #14790, #60556, .T. ) ;
#5983 = ADVANCED_FACE ( 'NONE', ( #1039 ), #43690, .T. ) ;
#5984 = CARTESIAN_POINT ( 'NONE',  ( 12.48078237941917301, 11.21561491925777432, -3.152940285276780941 ) ) ;
#5985 = FACE_OUTER_BOUND ( 'NONE', #30719, .T. ) ;
#5986 = VECTOR ( 'NONE', #56872, 1000.000000000000000 ) ;
#5987 = CARTESIAN_POINT ( 'NONE',  ( 9.669098047358048120, -4.353250594943018470, -8.814528502301756774 ) ) ;
#5988 = LINE ( 'NONE', #753, #45560 ) ;
#5989 = CARTESIAN_POINT ( 'NONE',  ( 17.63816080826976673, 1.880463790428644533, -12.57456020225082582 ) ) ;
#5990 = CARTESIAN_POINT ( 'NONE',  ( 8.680115641897847567, 4.300161509225400636, -5.864543311939105941 ) ) ;
#5991 = CARTESIAN_POINT ( 'NONE',  ( 11.19518313518939934, 3.462699341914400097, 6.820583637845799352 ) ) ;
#5992 = CARTESIAN_POINT ( 'NONE',  ( 11.64452043831720829, -3.625675755376928766, 11.98888621914706398 ) ) ;
#5993 = CARTESIAN_POINT ( 'NONE',  ( 11.09178064679000109, -4.578543110806999827, -8.908602356389000221 ) ) ;
#5994 = CARTESIAN_POINT ( 'NONE',  ( 12.43754357095653518, 3.154646014582549896, 13.64000194806622090 ) ) ;
#5995 = CARTESIAN_POINT ( 'NONE',  ( 24.30001129780202263, 8.895961348536667757, 8.895961348536667757 ) ) ;
#5996 = CARTESIAN_POINT ( 'NONE',  ( 11.36301932002747961, -5.250000000000001776, 7.200148911387369566 ) ) ;
#5997 = CARTESIAN_POINT ( 'NONE',  ( 9.383148997457999130, 5.167567567567999731, 6.822293592207000934 ) ) ;
#5998 = EDGE_CURVE ( 'NONE', #64677, #62083, #54736, .T. ) ;
#5999 = ORIENTED_EDGE ( 'NONE', *, *, #11208, .T. ) ;
#6000 = CARTESIAN_POINT ( 'NONE',  ( 7.360904521458606631, 3.242717731377448676, 9.067081841172152323 ) ) ;
#6002 = STYLED_ITEM ( 'NONE', ( #3664 ), #31079 ) ;
#6001 = CARTESIAN_POINT ( 'NONE',  ( 10.90333997687999990, -3.786145554879500441, 8.480416814141699788 ) ) ;
#6003 = VERTEX_POINT ( 'NONE', #33545 ) ;
#6004 = CARTESIAN_POINT ( 'NONE',  ( 17.69878333211500987, -3.108595074582393369, 13.52536937155546681 ) ) ;
#6005 = CARTESIAN_POINT ( 'NONE',  ( 10.49764694612699856, -5.059486515935999407, -7.922821994243300914 ) ) ;
#6006 = ORIENTED_EDGE ( 'NONE', *, *, #19479, .T. ) ;
#6007 = CARTESIAN_POINT ( 'NONE',  ( 10.97635090131019986, 4.999207052587699707, 6.881982988766500497 ) ) ;
#6008 = CARTESIAN_POINT ( 'NONE',  ( 5.599062476606316174, 1.099716160431485346, 0.2739963443920760966 ) ) ;
#6010 = CARTESIAN_POINT ( 'NONE',  ( 23.60000330292420045, 2.996599131394091842, -13.56986852407293753 ) ) ;
#6009 = VECTOR ( 'NONE', #17127, 1000.000000000000000 ) ;
#6011 = CARTESIAN_POINT ( 'NONE',  ( 18.44721083353000068, -2.702837639295000205, 11.38762126772000016 ) ) ;
#6012 = CARTESIAN_POINT ( 'NONE',  ( 12.35751123590698519, -3.100314578187023162, -13.65257769754496842 ) ) ;
#6013 = CARTESIAN_POINT ( 'NONE',  ( 12.53102142834153376, 0.5618070542492630270, -13.88471645277093103 ) ) ;
#6014 = FACE_OUTER_BOUND ( 'NONE', #31853, .T. ) ;
#6015 = CARTESIAN_POINT ( 'NONE',  ( 10.11858840337999865, -3.393395892949000014, -5.921999462319999630 ) ) ;
#6016 = VECTOR ( 'NONE', #159, 1000.000000000000000 ) ;
#6017 = FACE_OUTER_BOUND ( 'NONE', #51748, .T. ) ;
#6018 = VERTEX_POINT ( 'NONE', #17101 ) ;
#6019 = CARTESIAN_POINT ( 'NONE',  ( 9.169760841232999837, 4.728328492779000136, -8.692725459657999920 ) ) ;
#6020 = EDGE_LOOP ( 'NONE', ( #18374, #56308, #11960, #10569, #42336, #27068 ) ) ;
#6021 = CARTESIAN_POINT ( 'NONE',  ( 24.67921580316900076, -12.29514843751999997, 2.979196179828000002 ) ) ;
#6022 = ORIENTED_EDGE ( 'NONE', *, *, #28601, .T. ) ;
#6023 = FACE_OUTER_BOUND ( 'NONE', #21736, .T. ) ;
#6024 = CARTESIAN_POINT ( 'NONE',  ( 17.96133816917720338, -2.975035784927402283, -12.32810058309830836 ) ) ;
#6025 = CARTESIAN_POINT ( 'NONE',  ( 10.48744998751060997, -3.030310408214976992, 5.007827882781265671 ) ) ;
#6026 = CARTESIAN_POINT ( 'NONE',  ( 18.28126625413079154, 11.72532252228423744, -3.796277944706968110 ) ) ;
#6027 = CARTESIAN_POINT ( 'NONE',  ( 9.602263540182329749, -2.907767014557176566, -8.129523725463620565 ) ) ;
#6028 = B_SPLINE_SURFACE_WITH_KNOTS ( 'NONE', 3, 3, ( 
 ( #59391, #64631, #1358, #17082 ),
 ( #21984, #38415, #11491, #32492 ),
 ( #16737, #32836, #38768, #54148 ),
 ( #44020, #27587, #65671, #22331 ),
 ( #6944, #65323, #39111, #12198 ),
 ( #27938, #33526, #44373, #54845 ),
 ( #43326, #12542, #59740, #6245 ),
 ( #11841, #49249, #43671, #33179 ),
 ( #60435, #49597, #28276, #1704 ),
 ( #48913, #1021, #23023, #5904 ),
 ( #54497, #64968, #48568, #17793 ),
 ( #6597, #22675, #59055, #672 ),
 ( #11157, #53805, #21184, #63480 ),
 ( #43202, #48105, #11041, #4750 ),
 ( #63824, #15256, #15936, #26438 ),
 ( #58589, #36579, #37267, #16281 ) ),
 .UNSPECIFIED., .F., .F., .F.,
 ( 4, 1, 1, 1, 1, 1, 1, 1, 1, 1, 1, 1, 1, 4 ),
 ( 4, 4 ),
 ( 0.02931725585745000029, 0.07692307692307999434, 0.1538461538461999845, 0.2307692307692000011, 0.3076923076922999933, 0.3846153846154000133, 0.4615384615385000333, 0.5384615384614999112, 0.6153846153845999867, 0.6923076923076999512, 0.7692307692308000266, 0.8461538461537999600, 0.9230769230769000355, 0.9830414450855999853 ),
 ( -0.1835260008786999963, 1.183623993927000129 ),
 .UNSPECIFIED. ) ;
#6029 = CARTESIAN_POINT ( 'NONE',  ( 10.96207173348999930, -5.399846879528999999, 7.743266618618998898 ) ) ;
#6030 = ADVANCED_BREP_SHAPE_REPRESENTATION ( '', ( #30272, #9676 ), #58898 ) ;
#6031 = CARTESIAN_POINT ( 'NONE',  ( 18.17992876607769048, -2.487411392606218463, -12.45448399073205437 ) ) ;
#6032 = CARTESIAN_POINT ( 'NONE',  ( 12.26373570557222514, -0.3125842563278225517, 13.89527356689843884 ) ) ;
#6033 = ORIENTED_EDGE ( 'NONE', *, *, #21940, .T. ) ;
#6034 = CARTESIAN_POINT ( 'NONE',  ( 12.83523642498299999, 11.49802605210000195, -4.818062943702999590 ) ) ;
#6035 = CARTESIAN_POINT ( 'NONE',  ( 17.87004618316199966, 11.92229088141000126, -3.300664210127000064 ) ) ;
#6036 = CARTESIAN_POINT ( 'NONE',  ( 9.100254395947628083, 3.149024541069663563, 7.703403631282998099 ) ) ;
#6037 = CARTESIAN_POINT ( 'NONE',  ( 4.496969878954000244, 0.5190299378403000485, -1.067582673698000084 ) ) ;
#6038 = CIRCLE ( 'NONE', #27262, 1.775000326287000219 ) ;
#6039 = CARTESIAN_POINT ( 'NONE',  ( 9.395239158775000377, 5.045571591548999812, -9.086294919530001124 ) ) ;
#6040 = CARTESIAN_POINT ( 'NONE',  ( 18.48724299199999876, -3.206939682244000167, 12.14698705996000072 ) ) ;
#6041 = CARTESIAN_POINT ( 'NONE',  ( 10.09133114265999964, -2.216726401468000152, -8.007130485478999304 ) ) ;
#6042 = EDGE_CURVE ( 'NONE', #7868, #15904, #51391, .T. ) ;
#6043 = EDGE_LOOP ( 'NONE', ( #34858, #55821, #22919, #31302 ) ) ;
#6044 = FACE_OUTER_BOUND ( 'NONE', #14930, .T. ) ;
#6045 = LINE ( 'NONE', #59190, #25463 ) ;
#6046 = CARTESIAN_POINT ( 'NONE',  ( 8.672328646360149662, -3.200842352561755533, -6.403885667220094113 ) ) ;
#6047 = CARTESIAN_POINT ( 'NONE',  ( 9.319055905798999007, 2.899999999999999911, -6.571291218949999902 ) ) ;
#6048 = DIRECTION ( 'NONE',  ( 0.000000000000000000, -1.000000000000000000, 0.000000000000000000 ) ) ;
#6049 = CARTESIAN_POINT ( 'NONE',  ( 11.31389666366019853, 3.954123449088899900, -8.532487796751999198 ) ) ;
#6050 = CARTESIAN_POINT ( 'NONE',  ( 9.026759580228999269, 3.023107159668900312, -7.266499081715599218 ) ) ;
#6052 = CARTESIAN_POINT ( 'NONE',  ( 8.384356144328393157, 5.054963279901980577, -6.361519316970982274 ) ) ;
#6051 = CARTESIAN_POINT ( 'NONE',  ( 10.45695058442700009, -3.655872208659600275, 8.295791434820300125 ) ) ;
#6053 = CONICAL_SURFACE ( 'NONE', #38454, 11.75015521449999945, 0.7854113701714536822 ) ;
#6054 = CARTESIAN_POINT ( 'NONE',  ( 6.899999691988000450, 0.000000000000000000, 0.000000000000000000 ) ) ;
#6055 = VERTEX_POINT ( 'NONE', #1376 ) ;
#6056 = CARTESIAN_POINT ( 'NONE',  ( 11.52166954483529793, 4.562096242626500597, 8.367285821793199574 ) ) ;
#6057 = CIRCLE ( 'NONE', #27287, 12.32509977859000827 ) ;
#6058 = CARTESIAN_POINT ( 'NONE',  ( 9.595487457706001422, -3.928425191288000384, 5.531324308465000783 ) ) ;
#6059 = CARTESIAN_POINT ( 'NONE',  ( 9.203113844318000503, 4.323050436788100193, 8.737749087159000894 ) ) ;
#6060 = CARTESIAN_POINT ( 'NONE',  ( 17.60000005322544681, -11.49057892309719264, 4.802228223496430637 ) ) ;
#6061 = CARTESIAN_POINT ( 'NONE',  ( 10.71256247620999957, -5.951803124515000043, 7.233045248871000865 ) ) ;
#6062 = CARTESIAN_POINT ( 'NONE',  ( 9.987419771736607998, -2.445504403440184937, 6.696380856873024534 ) ) ;
#6063 = CARTESIAN_POINT ( 'NONE',  ( 16.29314246895800267, -3.193172571147000038, -11.44978050968999916 ) ) ;
#6064 = EDGE_CURVE ( 'NONE', #59855, #55474, #6118, .T. ) ;
#6066 = EDGE_CURVE ( 'NONE', #14453, #17504, #41857, .T. ) ;
#6065 = B_SPLINE_CURVE_WITH_KNOTS ( 'NONE', 3,
 ( #31153, #37072, #41285, #52455, #3864, #15052, #58384, #9804, #25548, #47220 ),
 .UNSPECIFIED., .F., .F.,
 ( 4, 1, 1, 1, 1, 1, 1, 4 ),
 ( 0.000000000000000000, 0.02409300149743000274, 0.1867443091173000003, 0.3493956167372000432, 0.5120469243570999751, 0.6746982319770000736, 0.8373495395968999500, 1.000000000000000000 ),
 .UNSPECIFIED. ) ;
#6067 = CARTESIAN_POINT ( 'NONE',  ( 10.13922949779699856, -3.366547096154099972, -8.449985803660998940 ) ) ;
#6068 = EDGE_CURVE ( 'NONE', #48015, #15478, #487, .T. ) ;
#6069 = CARTESIAN_POINT ( 'NONE',  ( 5.605830324680001198, 1.139611800844000156, 0.2906295266426999757 ) ) ;
#6070 = CARTESIAN_POINT ( 'NONE',  ( 11.54298866606777629, -4.505418116367177817, 8.213191510014491215 ) ) ;
#6071 = CARTESIAN_POINT ( 'NONE',  ( 24.55996189763800075, -3.658601031398000192, 12.32999353876000015 ) ) ;
#6072 = B_SPLINE_CURVE_WITH_KNOTS ( 'NONE', 3,
 ( #40112, #66313, #13201, #35210, #14223, #7942, #60732, #49900, #61426, #29632, #34529, #18091, #23331, #50593 ),
 .UNSPECIFIED., .F., .F.,
 ( 4, 2, 2, 2, 2, 2, 4 ),
 ( 0.000000000000000000, 0.2494049090185054274, 0.3741073635277598064, 0.4052829771550735538, 0.4364585907823873012, 0.4676342044097009931, 0.4988098180370147405 ),
 .UNSPECIFIED. ) ;
#6073 = CARTESIAN_POINT ( 'NONE',  ( 11.64595257254739913, -4.831736303435800295, 7.258104750172799768 ) ) ;
#6074 = CARTESIAN_POINT ( 'NONE',  ( 11.12133729122639991, 3.134101783108900197, -7.477221318588949117 ) ) ;
#6075 = DIRECTION ( 'NONE',  ( 0.000000000000000000, 0.3146293386371170064, -0.9492146118074512584 ) ) ;
#6076 = CARTESIAN_POINT ( 'NONE',  ( 25.19548496669100146, -8.372909214912999332, 8.693259092873001137 ) ) ;
#6077 = CARTESIAN_POINT ( 'NONE',  ( 5.699999772733999492, 12.03770622561999915, 3.722046322334000124 ) ) ;
#6078 = VERTEX_POINT ( 'NONE', #29007 ) ;
#6079 = CARTESIAN_POINT ( 'NONE',  ( 24.74074828464900122, -11.86918666989000037, -3.111331014755999824 ) ) ;
#6080 = SHAPE_DEFINITION_REPRESENTATION ( #40536, #53976 ) ;
#6081 = CARTESIAN_POINT ( 'NONE',  ( 11.40211496860029783, -3.206052520092899982, -7.093139000852099585 ) ) ;
#6082 = CARTESIAN_POINT ( 'NONE',  ( 18.14037995568667583, 0.2193687868415796216, 12.69745523515037711 ) ) ;
#6083 = CARTESIAN_POINT ( 'NONE',  ( 10.55880524123913666, 4.703942329535922617, 8.703471051125569957 ) ) ;
#6084 = CARTESIAN_POINT ( 'NONE',  ( 12.99284288850700086, 12.22216846288000092, 1.954503247608000205 ) ) ;
#6085 = ORIENTED_EDGE ( 'NONE', *, *, #11505, .F. ) ;
#6086 = AXIS2_PLACEMENT_3D ( 'NONE', #4186, #25524, #36011 ) ;
#6087 = DIRECTION ( 'NONE',  ( 1.000000000000000000, 0.000000000000000000, 0.000000000000000000 ) ) ;
#6088 = CARTESIAN_POINT ( 'NONE',  ( 8.727215710425999973, -4.373963964882100264, -8.308760775591800041 ) ) ;
#6089 = EDGE_LOOP ( 'NONE', ( #41646, #5579, #10126, #53743 ) ) ;
#6090 = EDGE_CURVE ( 'NONE', #23499, #23570, #60834, .T. ) ;
#6091 = CARTESIAN_POINT ( 'NONE',  ( 9.832537864288001472, -2.899999999999999911, 6.571291218949999902 ) ) ;
#6092 = CARTESIAN_POINT ( 'NONE',  ( 18.28832092538753074, 2.855728056445007823, 11.50255606616314630 ) ) ;
#6093 = CARTESIAN_POINT ( 'NONE',  ( 9.807804719590000886, 3.988943694240999704, -8.966360307350999648 ) ) ;
#6094 = ORIENTED_EDGE ( 'NONE', *, *, #65735, .T. ) ;
#6095 = DIRECTION ( 'NONE',  ( 0.000000000000000000, 0.000000000000000000, -1.000000000000000000 ) ) ;
#6096 = CARTESIAN_POINT ( 'NONE',  ( 7.215860841226000133, 3.469376689055999829, -5.675721888027999817 ) ) ;
#6097 = PLANE ( 'NONE',  #10778 ) ;
#6098 = CARTESIAN_POINT ( 'NONE',  ( 8.191498616105999275, -3.399962740672999750, 6.146646623957999545 ) ) ;
#6099 = VERTEX_POINT ( 'NONE', #23396 ) ;
#6100 = CARTESIAN_POINT ( 'NONE',  ( 10.31668414895000119, -3.819528725844000494, 6.062183754159999438 ) ) ;
#6101 = CARTESIAN_POINT ( 'NONE',  ( 25.20468521070600332, 11.19853207827999952, -3.405347367087999899 ) ) ;
#6102 = ORIENTED_EDGE ( 'NONE', *, *, #8215, .T. ) ;
#6103 = AXIS2_PLACEMENT_3D ( 'NONE', #34008, #1150, #27727 ) ;
#6104 = CARTESIAN_POINT ( 'NONE',  ( 10.33253786428999987, 2.899999999999999911, 6.571291218949999902 ) ) ;
#6105 = CARTESIAN_POINT ( 'NONE',  ( 10.06949314679000018, -4.910373174915999783, -8.649593977693999847 ) ) ;
#6106 = VERTEX_POINT ( 'NONE', #7310 ) ;
#6107 = CARTESIAN_POINT ( 'NONE',  ( 8.697480666858998788, 4.334888990546500231, 6.553061479084200336 ) ) ;
#6108 = CARTESIAN_POINT ( 'NONE',  ( 18.06139357112843058, 0.3666408745733568675, -13.89349736880774877 ) ) ;
#6109 = CARTESIAN_POINT ( 'NONE',  ( 5.321681265427999463, -0.6446507492830000352, 1.055470389442999979 ) ) ;
#6110 = VECTOR ( 'NONE', #68345, 1000.000000000000000 ) ;
#6111 = CARTESIAN_POINT ( 'NONE',  ( 11.59999999999999964, 3.205140046301732326, -7.075514291626551433 ) ) ;
#6112 = CARTESIAN_POINT ( 'NONE',  ( 24.71426486868732653, 11.77715745911889123, -3.190793282506284800 ) ) ;
#6113 = CARTESIAN_POINT ( 'NONE',  ( 7.144614836148978299, 4.730263389345491731, -8.645049034184477676 ) ) ;
#6114 = CARTESIAN_POINT ( 'NONE',  ( 13.04552286951900619, -12.39025300375189964, -1.832281502500274772 ) ) ;
#6115 = ORIENTED_EDGE ( 'NONE', *, *, #62966, .T. ) ;
#6116 = CARTESIAN_POINT ( 'NONE',  ( 11.00366064676999933, 2.264078662261999941, 7.798351372501000078 ) ) ;
#6117 = CARTESIAN_POINT ( 'NONE',  ( 24.30000000000000071, 0.000000000000000000, 0.000000000000000000 ) ) ;
#6118 = CIRCLE ( 'NONE', #1644, 12.24999851416000141 ) ;
#6119 = CARTESIAN_POINT ( 'NONE',  ( 25.30000327618300204, -0.7080256801165881742, 11.56241914337144294 ) ) ;
#6120 = CARTESIAN_POINT ( 'NONE',  ( 12.23531288305053621, 2.757742497410567317, -13.61542453244087092 ) ) ;
#6121 = CARTESIAN_POINT ( 'NONE',  ( 24.30000000000000071, 2.204728229456999866, 11.99913219504999873 ) ) ;
#6122 = CARTESIAN_POINT ( 'NONE',  ( 10.46432358320999967, -2.042767395367000027, 7.723698102088000006 ) ) ;
#6123 = CARTESIAN_POINT ( 'NONE',  ( 18.17882709566423216, -0.04040202251154500351, 13.89992604541790477 ) ) ;
#6124 = DIRECTION ( 'NONE',  ( 1.000000000000000000, 0.000000000000000000, 0.000000000000000000 ) ) ;
#6125 = EDGE_CURVE ( 'NONE', #66054, #37252, #8058, .T. ) ;
#6126 = EDGE_CURVE ( 'NONE', #46886, #146, #18093, .T. ) ;
#6127 = ORIENTED_EDGE ( 'NONE', *, *, #60927, .F. ) ;
#6128 = ORIENTED_EDGE ( 'NONE', *, *, #12355, .T. ) ;
#6129 = CARTESIAN_POINT ( 'NONE',  ( 12.22418139215586486, -0.2308705899090618963, 13.89742331311339818 ) ) ;
#6130 = CARTESIAN_POINT ( 'NONE',  ( 12.39787770614147355, -0.4743614816433503467, -13.88910774395701608 ) ) ;
#6131 = CARTESIAN_POINT ( 'NONE',  ( 9.625409048293999348, -2.899999999999999911, -6.226580113766999602 ) ) ;
#6132 = CARTESIAN_POINT ( 'NONE',  ( 18.18005043824477696, 1.062919176435095297E-10, -13.90000000153291637 ) ) ;
#6133 = CARTESIAN_POINT ( 'NONE',  ( 8.181105646794000208, -5.485781663882000281, 8.532068390166999805 ) ) ;
#6134 = CARTESIAN_POINT ( 'NONE',  ( 11.56049777433069892, -4.851452298509800087, 7.825000000000000178 ) ) ;
#6136 = CARTESIAN_POINT ( 'NONE',  ( 9.702862956260233318, 2.713451880140764327, 7.026479373626208336 ) ) ;
#6135 = CARTESIAN_POINT ( 'NONE',  ( 9.931076168958000494, -4.649151400100800302, 6.397735581984999698 ) ) ;
#6137 = CARTESIAN_POINT ( 'NONE',  ( 10.64118447801629941, 5.277702140407999565, -7.471828720557429193 ) ) ;
#6138 = CARTESIAN_POINT ( 'NONE',  ( 12.10000000000000142, -3.075975407729481415, 6.664392815890119337 ) ) ;
#6139 = STYLED_ITEM ( 'NONE', ( #3452 ), #46907 ) ;
#6140 = CARTESIAN_POINT ( 'NONE',  ( 17.78490268980527134, -0.5812897767837150731, 12.68208758371477352 ) ) ;
#6141 = CARTESIAN_POINT ( 'NONE',  ( 6.770122584706000701, 0.8499847235081999797, -1.301835277045000128 ) ) ;
#6142 = FACE_OUTER_BOUND ( 'NONE', #58373, .T. ) ;
#6143 = ORIENTED_EDGE ( 'NONE', *, *, #34995, .T. ) ;
#6144 = CARTESIAN_POINT ( 'NONE',  ( 7.673644353206999114, -4.696237245142999228, 5.830277424166999900 ) ) ;
#6145 = CARTESIAN_POINT ( 'NONE',  ( 8.324914158772999784, 2.633142096252999664, -7.791134854666999843 ) ) ;
#6146 = ADVANCED_FACE ( 'NONE', ( #66379 ), #22840, .F. ) ;
#6147 = CYLINDRICAL_SURFACE ( 'NONE', #21517, 12.50000000000000000 ) ;
#6148 = DIRECTION ( 'NONE',  ( -0.000000000000000000, 1.000000000000000000, 0.000000000000000000 ) ) ;
#6149 = ADVANCED_FACE ( 'NONE', ( #29345 ), #2413, .T. ) ;
#6150 = DIRECTION ( 'NONE',  ( 1.000000000000000000, 0.000000000000000000, 0.000000000000000000 ) ) ;
#6151 = CARTESIAN_POINT ( 'NONE',  ( 10.44125056272499918, 5.033400911533000510, 7.484684486284700178 ) ) ;
#6152 = CARTESIAN_POINT ( 'NONE',  ( 10.76588584123000025, 3.166544027818999574, -8.574484964885998650 ) ) ;
#6153 = ORIENTED_EDGE ( 'NONE', *, *, #16948, .T. ) ;
#6154 = CARTESIAN_POINT ( 'NONE',  ( 12.09857507241188657, 0.1632583333441771367, -12.59896334813831409 ) ) ;
#6155 = CARTESIAN_POINT ( 'NONE',  ( 10.90000000000000036, 0.000000000000000000, 0.000000000000000000 ) ) ;
#6156 = CARTESIAN_POINT ( 'NONE',  ( 17.74426251268373633, 3.174930969421378091, -12.19343357469032085 ) ) ;
#6157 = CARTESIAN_POINT ( 'NONE',  ( 7.955265382045282330, -4.958437936411385749, 6.436898865497720834 ) ) ;
#6158 = CARTESIAN_POINT ( 'NONE',  ( 8.758795280412000395, 3.977267228909999730, 9.308925224542001331 ) ) ;
#6159 = ORIENTED_EDGE ( 'NONE', *, *, #19091, .F. ) ;
#6160 = CARTESIAN_POINT ( 'NONE',  ( 5.802289226419000023, 0.9320062393831999303, 1.134853260389000029 ) ) ;
#6161 = CARTESIAN_POINT ( 'NONE',  ( 8.493945280408999210, 5.563172860439999923, -7.424303164651000486 ) ) ;
#6162 = CARTESIAN_POINT ( 'NONE',  ( 8.414809249528957480, -2.419867401190203715, 8.226612844550492909 ) ) ;
#6163 = CARTESIAN_POINT ( 'NONE',  ( 13.69999628573842543, 9.617752440245856960, 8.023770515523496627 ) ) ;
#6164 = ORIENTED_EDGE ( 'NONE', *, *, #36840, .F. ) ;
#6165 = DIRECTION ( 'NONE',  ( -1.000000000000000000, -5.329070518371000199E-14, 3.552713678914000343E-14 ) ) ;
#6166 = CARTESIAN_POINT ( 'NONE',  ( 6.177943173016666734, -0.9218200799623716968, -1.199500263597270910 ) ) ;
#6167 = ORIENTED_EDGE ( 'NONE', *, *, #63478, .F. ) ;
#6168 = EDGE_CURVE ( 'NONE', #18734, #46559, #28878, .T. ) ;
#6169 = CARTESIAN_POINT ( 'NONE',  ( 24.87152056774154119, 3.035077187909910545, -11.66328149024612237 ) ) ;
#6170 = CARTESIAN_POINT ( 'NONE',  ( 16.43176826122700263, 3.316188843241000050, 11.22344245815999919 ) ) ;
#6171 = CARTESIAN_POINT ( 'NONE',  ( 17.55505043854143921, 0.7302158263239216796, -13.98094363220831049 ) ) ;
#6172 = ORIENTED_EDGE ( 'NONE', *, *, #51709, .F. ) ;
#6173 = CYLINDRICAL_SURFACE ( 'NONE', #15235, 0.6250000000000005551 ) ;
#6174 = CARTESIAN_POINT ( 'NONE',  ( 8.871554213457001126, -3.399999843100999897, -6.206435837692999336 ) ) ;
#6175 = CARTESIAN_POINT ( 'NONE',  ( 10.61257802013489737, 3.108115747127599970, -7.479237407015119743 ) ) ;
#6176 = CARTESIAN_POINT ( 'NONE',  ( 23.58333425578799947, 1.192379528446999839E-13, -4.982680934517999418E-13 ) ) ;
#6178 = AXIS2_PLACEMENT_3D ( 'NONE', #8543, #66576, #24627 ) ;
#6177 = DIRECTION ( 'NONE',  ( 0.000000000000000000, 0.000000000000000000, -1.000000000000000000 ) ) ;
#6179 = ORIENTED_EDGE ( 'NONE', *, *, #60720, .T. ) ;
#6180 = CARTESIAN_POINT ( 'NONE',  ( 8.989142219592000771, 5.284130523641000110, 6.489275570566000795 ) ) ;
#6181 = CYLINDRICAL_SURFACE ( 'NONE', #37353, 1.350000000000000533 ) ;
#6182 = ORIENTED_EDGE ( 'NONE', *, *, #19479, .F. ) ;
#6183 = CARTESIAN_POINT ( 'NONE',  ( 9.227255459545913752, -3.370461114521380530, -6.407745725917161295 ) ) ;
#6184 = CARTESIAN_POINT ( 'NONE',  ( 15.48701341325400094, -9.525963125313998248, -8.191611664426000416 ) ) ;
#6185 = CARTESIAN_POINT ( 'NONE',  ( 10.96255546505999945, 5.431632148000000271, -4.905443575133999978 ) ) ;
#6186 = ORIENTED_EDGE ( 'NONE', *, *, #12938, .T. ) ;
#6187 = B_SPLINE_SURFACE_WITH_KNOTS ( 'NONE', 3, 3, ( 
 ( #56156, #4377, #14204, #25028, #45334, #8948, #40094, #57520, #46012, #66982, #66644, #14882, #30621, #51933, #19785, #61740, #25368, #46705, #56501, #30289, #36204, #18764, #13525, #45677, #50914, #19094, #13860, #3355, #35188, #67320, #51592, #19438, #3688, #41112, #62425 ),
 ( #14546, #32348, #42148, #5072, #64135, #31312, #63098, #47044, #15224, #5756, #58907, #15573, #10660, #26410, #48072, #68697, #52624, #36549, #5421, #68347, #26061, #9976, #32007, #42827, #4717, #20465, #47390, #16597, #42486, #41794, #20811, #21159, #37572, #48413, #58216 ),
 ( #519, #57875, #16249, #63451, #53663, #15905, #11011, #63796, #36901, #10320, #31653, #52975, #47737, #21836, #27098, #53998, #43167, #37237, #21493, #37922, #32685, #64473, #58554, #69051, #59241, #53321, #11347, #25712, #26759, #176, #38265, #65518, #7145, #34073, #28482 ),
 ( #43865, #11690, #33030, #65866, #60631, #16932, #44908, #49800, #12743, #6793, #66210, #60979, #59589, #28130, #1907, #39656, #17288, #13091, #54342, #60288, #18332, #34426, #6100, #38615, #27439, #6445, #59935, #48761, #867, #39308, #23228, #22183, #12046, #54694, #43523 ) ),
 .UNSPECIFIED., .F., .F., .F.,
 ( 4, 4 ),
 ( 4, 1, 1, 1, 1, 1, 1, 1, 1, 1, 1, 1, 1, 1, 1, 1, 1, 1, 1, 1, 1, 1, 1, 1, 1, 1, 1, 1, 1, 1, 1, 1, 4 ),
 ( -0.1039086239011999951, 1.103908623900999864 ),
 ( -0.01933701211302999920, 0.01208563257065999909, 0.04350827725433999843, 0.07493092193802000645, 0.1063535666217000075, 0.1377762113054000204, 0.1691988559891000055, 0.2006215006727000150, 0.2320441453564000001, 0.2634667900400999851, 0.2948894347238000258, 0.3263120794074999553, 0.3577347240911999959, 0.3891573687748000054, 0.4205800134584999905, 0.4520026581421999756, 0.4834253028259000162, 0.5148479475096000568, 0.5462705921932000663, 0.5776932368768999959, 0.6091158815606000365, 0.6405385262443000771, 0.6719611709280000067, 0.7033838156117000473, 0.7348064602953000568, 0.7662291049789999864, 0.7976517496627000270, 0.8290743943464000676, 0.8604970390300999972, 0.8919196837138000378, 0.9233423283974000473, 0.9547649730810999769, 0.9861876177648000175 ),
 .UNSPECIFIED. ) ;
#6188 = CARTESIAN_POINT ( 'NONE',  ( 12.24703709751431724, -2.218305284339070482, -12.51274264014588411 ) ) ;
#6189 = PLANE ( 'NONE',  #15377 ) ;
#6190 = CARTESIAN_POINT ( 'NONE',  ( 8.187247165044786001, 3.359395650746410222, -5.756825428974689629 ) ) ;
#6191 = DIRECTION ( 'NONE',  ( 1.000000000000000000, 0.000000000000000000, 0.000000000000000000 ) ) ;
#6192 = CARTESIAN_POINT ( 'NONE',  ( 12.08550557360782562, -2.425787521189701756, -13.78826042901831528 ) ) ;
#6193 = CARTESIAN_POINT ( 'NONE',  ( 10.50180110216399854, -4.856393875115199599, -6.976989117212499814 ) ) ;
#6194 = CARTESIAN_POINT ( 'NONE',  ( 12.70675980919359205, -3.199682200194524651, 12.18696163212649886 ) ) ;
#6195 = CARTESIAN_POINT ( 'NONE',  ( 17.63759097916654994, -3.119868145639166812, 12.28530842955781921 ) ) ;
#6196 = EDGE_LOOP ( 'NONE', ( #34226, #35721, #40011 ) ) ;
#6197 = CARTESIAN_POINT ( 'NONE',  ( 11.10101463001529964, -3.377766160221900016, -6.503413421344399481 ) ) ;
#6198 = ORIENTED_EDGE ( 'NONE', *, *, #4070, .T. ) ;
#6199 = CARTESIAN_POINT ( 'NONE',  ( 11.31944011432000075, -12.15765269271000015, -1.759220518310000037 ) ) ;
#6200 = CONICAL_SURFACE ( 'NONE', #26330, 0.4377388725247000623, 0.7853981633972997312 ) ;
#6201 = CARTESIAN_POINT ( 'NONE',  ( 9.485829719593997567, 4.953415418491999844, -8.946479654552000227 ) ) ;
#6202 = CARTESIAN_POINT ( 'NONE',  ( 11.15192953222999961, 2.359300361215999953, -6.636686939130999718 ) ) ;
#6203 = CARTESIAN_POINT ( 'NONE',  ( 10.74708735964999917, -5.603138702306000418, -6.963343193308999979 ) ) ;
#6204 = VECTOR ( 'NONE', #17868, 1000.000000000000000 ) ;
#6205 = DIRECTION ( 'NONE',  ( 0.000000000000000000, -1.000000000000000000, 0.000000000000000000 ) ) ;
#6206 = CARTESIAN_POINT ( 'NONE',  ( 7.577053541547003945, 3.182130936862002102, -6.424376193309997873 ) ) ;
#6207 = EDGE_CURVE ( 'NONE', #65266, #63941, #62292, .T. ) ;
#6209 = EDGE_CURVE ( 'NONE', #15006, #39410, #13925, .T. ) ;
#6208 = CARTESIAN_POINT ( 'NONE',  ( 17.60407896982588127, -1.760945483361028074, -12.47634044926095420 ) ) ;
#6210 = VERTEX_POINT ( 'NONE', #36287 ) ;
#6211 = CARTESIAN_POINT ( 'NONE',  ( 1.808651541364333371, -3.500000000000000000, -0.3376993977123543544 ) ) ;
#6212 = EDGE_CURVE ( 'NONE', #48015, #16312, #30587, .T. ) ;
#6213 = CARTESIAN_POINT ( 'NONE',  ( 9.662551629919999385, 4.094830335839000135, 9.119946295870999364 ) ) ;
#6214 = DIRECTION ( 'NONE',  ( 1.000000000000000000, -1.845552235241999991E-09, 8.866463766873999729E-13 ) ) ;
#6215 = CARTESIAN_POINT ( 'NONE',  ( 12.10477869730532774, -4.467447516829900600, 8.421761806503198500 ) ) ;
#6216 = CARTESIAN_POINT ( 'NONE',  ( 17.76930066282600151, 3.251864118589000263, -11.33740735155000046 ) ) ;
#6217 = CARTESIAN_POINT ( 'NONE',  ( 10.85408070804999880, 9.831992037111000116, -5.581278437649000779 ) ) ;
#6218 = CARTESIAN_POINT ( 'NONE',  ( 10.39055228715993451, 2.705487803219565279, 8.717536521744987610 ) ) ;
#6219 = CARTESIAN_POINT ( 'NONE',  ( 23.55777338189700032, -10.23214251361999949, -9.679131332715998681 ) ) ;
#6220 = B_SPLINE_CURVE_WITH_KNOTS ( 'NONE', 3,
 ( #49148, #26196, #1259, #12096, #54744, #6843, #28177, #20255, #47521, #36337 ),
 .UNSPECIFIED., .F., .F.,
 ( 4, 2, 2, 2, 4 ),
 ( 0.000000000000000000, 0.1249999999532679651, 0.2499999999065359302, 0.3749999998598039230, 0.4999999998130718604 ),
 .UNSPECIFIED. ) ;
#6221 = B_SPLINE_CURVE_WITH_KNOTS ( 'NONE', 3,
 ( #8097, #2844, #45164, #17902 ),
 .UNSPECIFIED., .F., .F.,
 ( 4, 4 ),
 ( 0.000000000000000000, 1.000000000000000000 ),
 .UNSPECIFIED. ) ;
#6222 = CARTESIAN_POINT ( 'NONE',  ( 25.44993329535400051, 2.258942858049999725, 12.29419282279000036 ) ) ;
#6223 = CARTESIAN_POINT ( 'NONE',  ( 20.75138802851920161, 0.000000000000000000, 0.000000000000000000 ) ) ;
#6224 = ORIENTED_EDGE ( 'NONE', *, *, #1914, .T. ) ;
#6225 = LINE ( 'NONE', #64262, #59903 ) ;
#6226 = CARTESIAN_POINT ( 'NONE',  ( 7.426573454271000685, -1.235669854462000172, 0.4909903177977000266 ) ) ;
#6227 = CARTESIAN_POINT ( 'NONE',  ( 18.02623320712467603, 2.911124530445448499, 13.57757619639374269 ) ) ;
#6228 = CARTESIAN_POINT ( 'NONE',  ( 24.44917776433500123, 8.894882193901999301, -9.199943407630001957 ) ) ;
#6229 = CARTESIAN_POINT ( 'NONE',  ( 11.61759063708296047, -2.782734359457999851, -7.842242470354300110 ) ) ;
#6230 = ORIENTED_EDGE ( 'NONE', *, *, #7477, .F. ) ;
#6231 = CARTESIAN_POINT ( 'NONE',  ( 24.30001131380927148, -8.895961354869664106, 8.895961354869664106 ) ) ;
#6232 = CARTESIAN_POINT ( 'NONE',  ( 9.106135841230999617, 4.192919163547999872, 5.525472271700999194 ) ) ;
#6233 = CIRCLE ( 'NONE', #28574, 13.92493900951001073 ) ;
#6235 = CARTESIAN_POINT ( 'NONE',  ( 18.29995268966800026, 2.861739928647000220, 11.98821236628000086 ) ) ;
#6234 = CARTESIAN_POINT ( 'NONE',  ( 9.791229719590001324, 4.294368353031000396, -8.968663198664000191 ) ) ;
#6236 = DIRECTION ( 'NONE',  ( -0.000000000000000000, -0.000000000000000000, 1.000000000000000000 ) ) ;
#6237 = VERTEX_POINT ( 'NONE', #15314 ) ;
#6238 = CARTESIAN_POINT ( 'NONE',  ( 10.51655086620999846, 4.930662802525000110, 8.573584269714999095 ) ) ;
#6239 = CARTESIAN_POINT ( 'NONE',  ( 18.20725128760098244, -2.198916822427667395, -13.82623906782133005 ) ) ;
#6240 = CARTESIAN_POINT ( 'NONE',  ( 10.67410807141119911, 4.046361247106100123, 6.497602131078999754 ) ) ;
#6241 = CARTESIAN_POINT ( 'NONE',  ( 10.46085355684000007, -5.403406918566000527, 7.721809917403000156 ) ) ;
#6242 = CARTESIAN_POINT ( 'NONE',  ( 8.449245559625000013, -5.458705123429999695, 7.456451825584000659 ) ) ;
#6243 = VERTEX_POINT ( 'NONE', #4459 ) ;
#6244 = CARTESIAN_POINT ( 'NONE',  ( 24.36453968238300050, 12.29068757677999990, -3.201420012754999878 ) ) ;
#6246 = CARTESIAN_POINT ( 'NONE',  ( 11.00119435320999983, -4.640445114785999969, -9.059317673956000405 ) ) ;
#6245 = CARTESIAN_POINT ( 'NONE',  ( 12.18592533278400047, -11.71489335541000010, 3.703722432179000101 ) ) ;
#6247 = CARTESIAN_POINT ( 'NONE',  ( 7.817505239956299867, -4.153452198738197154, 9.248890255915149794 ) ) ;
#6248 = CARTESIAN_POINT ( 'NONE',  ( 10.46432358320999967, -2.042767395367000027, 7.723698102088000006 ) ) ;
#6250 = CARTESIAN_POINT ( 'NONE',  ( 11.09999999999999964, 5.299311513382999550, 5.124965750789000296 ) ) ;
#6249 = AXIS2_PLACEMENT_3D ( 'NONE', #49323, #17872, #16475 ) ;
#6251 = VERTEX_POINT ( 'NONE', #20206 ) ;
#6252 = CARTESIAN_POINT ( 'NONE',  ( 11.09999999999999964, 2.700000000000000178, 5.160242713806000303 ) ) ;
#6253 = B_SPLINE_CURVE_WITH_KNOTS ( 'NONE', 3,
 ( #37212, #48388, #32660, #58529 ),
 .UNSPECIFIED., .F., .F.,
 ( 4, 4 ),
 ( 0.000000000000000000, 1.000000000000000000 ),
 .UNSPECIFIED. ) ;
#6254 = CARTESIAN_POINT ( 'NONE',  ( 11.19872335273220010, -3.650693637952500126, 6.559289673553299060 ) ) ;
#6255 = EDGE_CURVE ( 'NONE', #40006, #16502, #24005, .T. ) ;
#6256 = CARTESIAN_POINT ( 'NONE',  ( 9.525000000000000355, 4.417172942406000224, 8.783926296998000538 ) ) ;
#6257 = CARTESIAN_POINT ( 'NONE',  ( 11.08425954179440076, 4.982976321082899673, 6.683254058608399717 ) ) ;
#6258 = ORIENTED_EDGE ( 'NONE', *, *, #33730, .T. ) ;
#6259 = CARTESIAN_POINT ( 'NONE',  ( 8.474089158773999486, 4.131080973160000447, -6.108642999115999395 ) ) ;
#6260 = EDGE_CURVE ( 'NONE', #7747, #43855, #7187, .T. ) ;
#6261 = CARTESIAN_POINT ( 'NONE',  ( 12.49755103297837167, 3.131894283645451971, -12.20455838002552973 ) ) ;
#6262 = CARTESIAN_POINT ( 'NONE',  ( 11.76212378248530044, -4.615095948180499619, 8.663708617168998316 ) ) ;
#6263 = CARTESIAN_POINT ( 'NONE',  ( 7.963341518233496785, 5.029799759091138966, -6.519028237967030570 ) ) ;
#6264 = DIRECTION ( 'NONE',  ( -1.000000000000000000, 0.000000000000000000, 0.000000000000000000 ) ) ;
#6265 = ORIENTED_EDGE ( 'NONE', *, *, #48657, .F. ) ;
#6266 = CARTESIAN_POINT ( 'NONE',  ( 8.625066940379999991, -3.117370956513999758, 8.662188901935000018 ) ) ;
#6267 = CARTESIAN_POINT ( 'NONE',  ( 5.659193173017082579, -0.3926218265389189721, -1.460959015002473604 ) ) ;
#6268 = VERTEX_POINT ( 'NONE', #62844 ) ;
#6269 = CARTESIAN_POINT ( 'NONE',  ( 10.16052890781999984, -2.899999999999999911, -6.152188490330000370 ) ) ;
#6270 = CARTESIAN_POINT ( 'NONE',  ( 10.35826357027499789, 4.850513154668600002, 7.335909308151700614 ) ) ;
#6271 = CARTESIAN_POINT ( 'NONE',  ( 10.75109581085999899, 2.822145500011000063, 6.655897464539000552 ) ) ;
#6272 = CARTESIAN_POINT ( 'NONE',  ( 11.12916633214000051, 2.728377425829000114, -4.814907997079999724 ) ) ;
#6273 = CARTESIAN_POINT ( 'NONE',  ( 7.822787301102997581, 4.879242518472000967, 6.344068876191006012 ) ) ;
#6274 = CARTESIAN_POINT ( 'NONE',  ( 25.29987931604000195, 11.77655473258999841, -4.190794510628000680 ) ) ;
#6275 = CARTESIAN_POINT ( 'NONE',  ( 11.59999999999999964, 4.000000000000000000, -7.500000000000000000 ) ) ;
#6276 = CARTESIAN_POINT ( 'NONE',  ( 17.84384701673186058, -0.6598665579122044988, -12.58271022457860155 ) ) ;
#6277 = CARTESIAN_POINT ( 'NONE',  ( 12.20883946519827390, 2.687526094442107993, -12.40592204487018790 ) ) ;
#6278 = CARTESIAN_POINT ( 'NONE',  ( 10.71918447801630059, -2.859536135895000442, -7.474854604063350116 ) ) ;
#6279 = CARTESIAN_POINT ( 'NONE',  ( 9.074385841230999006, 3.981661882377999895, 8.959227447876999761 ) ) ;
#6280 = ORIENTED_EDGE ( 'NONE', *, *, #55027, .F. ) ;
#6281 = B_SPLINE_CURVE_WITH_KNOTS ( 'NONE', 3,
 ( #34595, #45759, #66384, #12915, #13269, #13610, #23399, #55563, #45078, #65694, #35274, #44395, #3100, #55909, #2082, #24434 ),
 .UNSPECIFIED., .F., .F.,
 ( 4, 2, 2, 2, 2, 2, 2, 4 ),
 ( 0.000000000000000000, 0.06249999999999893141, 0.1249999999999978628, 0.2499999999999999445, 0.5000000000000009992, 0.7500000000000019984, 0.8750000000000009992, 1.000000000000000000 ),
 .UNSPECIFIED. ) ;
#6282 = CARTESIAN_POINT ( 'NONE',  ( 23.56666365135700403, -12.07812737763999955, 3.551569042617998662 ) ) ;
#6283 = CARTESIAN_POINT ( 'NONE',  ( 7.272528695240493946, 2.858096677246901418, 6.733923262973229740 ) ) ;
#6284 = CARTESIAN_POINT ( 'NONE',  ( 11.80727443316700231, 12.22191286342000005, 1.956148154176999832 ) ) ;
#6285 = VECTOR ( 'NONE', #38365, 1000.000000000000114 ) ;
#6286 = CARTESIAN_POINT ( 'NONE',  ( 18.27884988594217219, 2.529462001843210128, 12.34351620764206814 ) ) ;
#6287 = CARTESIAN_POINT ( 'NONE',  ( 12.78089695109145119, 1.787798027819076596, 13.88537998392835249 ) ) ;
#6289 = EDGE_CURVE ( 'NONE', #17232, #958, #57961, .T. ) ;
#6288 = CARTESIAN_POINT ( 'NONE',  ( 11.04766396148000140, 10.00030925724000141, 5.674005852106000169 ) ) ;
#6290 = CARTESIAN_POINT ( 'NONE',  ( 10.30947051705162743, -3.358100414793015354, 6.905443702049931964 ) ) ;
#6291 = EDGE_CURVE ( 'NONE', #16920, #47459, #31743, .T. ) ;
#6292 = CARTESIAN_POINT ( 'NONE',  ( 9.854346873516623972, -5.250000000000000000, -7.663624617374463099 ) ) ;
#6293 = EDGE_CURVE ( 'NONE', #10305, #48780, #52248, .T. ) ;
#6294 = ORIENTED_EDGE ( 'NONE', *, *, #29067, .T. ) ;
#6295 = CARTESIAN_POINT ( 'NONE',  ( 12.32471554566195238, -3.019419751198730850, 12.23287256106958232 ) ) ;
#6296 = CARTESIAN_POINT ( 'NONE',  ( 9.806988259785999418, -4.131418345883800747, -8.495776841814999258 ) ) ;
#6297 = CARTESIAN_POINT ( 'NONE',  ( 10.46085995768999943, 5.403395036974999677, 7.721808039505000387 ) ) ;
#6298 = CARTESIAN_POINT ( 'NONE',  ( 9.323728576950999880, -3.947350124452999598, 6.051857392047999440 ) ) ;
#6299 = CARTESIAN_POINT ( 'NONE',  ( 11.03918313518939875, 3.292400735470800033, -8.394758848575399668 ) ) ;
#6300 = CARTESIAN_POINT ( 'NONE',  ( 12.12622238209133840, -0.2528603812084252445, 12.59746735456353051 ) ) ;
#6301 = CARTESIAN_POINT ( 'NONE',  ( 9.047982780412000992, 2.806082850903000026, 8.615880516515998622 ) ) ;
#6302 = CARTESIAN_POINT ( 'NONE',  ( 9.753142190738998352, 4.104977339646000090, 9.293283246364000050 ) ) ;
#6303 = CARTESIAN_POINT ( 'NONE',  ( 12.18425839594605442, 2.573099938722084978, 12.43423733299713341 ) ) ;
#6304 = ORIENTED_EDGE ( 'NONE', *, *, #57227, .T. ) ;
#6305 = FACE_OUTER_BOUND ( 'NONE', #29626, .T. ) ;
#6306 = CARTESIAN_POINT ( 'NONE',  ( 10.62072335273219892, 4.397090433355999473, -8.569396700949999612 ) ) ;
#6307 = CARTESIAN_POINT ( 'NONE',  ( 18.20534100106117137, -0.3182341284860664143, 12.59598505207571861 ) ) ;
#6308 = CARTESIAN_POINT ( 'NONE',  ( 10.42512334122999995, 3.371064118627999928, -6.294343971198999910 ) ) ;
#6309 = EDGE_CURVE ( 'NONE', #44124, #7173, #53060, .T. ) ;
#6310 = CARTESIAN_POINT ( 'NONE',  ( 8.566809814040999171, 4.782507962695600412, -8.511961036725999463 ) ) ;
#6312 = CARTESIAN_POINT ( 'NONE',  ( 17.90980607979504313, -0.5146431973202493237, 12.68596244101487791 ) ) ;
#6311 = CARTESIAN_POINT ( 'NONE',  ( 8.200215090286000930, 5.110410283172001300, 6.692116316553004651 ) ) ;
#6313 = CARTESIAN_POINT ( 'NONE',  ( 17.84552287012693128, 3.595130221969103701, 11.99794414424705025 ) ) ;
#6314 = VERTEX_POINT ( 'NONE', #25452 ) ;
#6315 = CARTESIAN_POINT ( 'NONE',  ( 0.6903817924015999141, 2.178673723483000035, -2.162625512369000358 ) ) ;
#6316 = CARTESIAN_POINT ( 'NONE',  ( 24.04053975777259566, -9.302302187229880559, -9.232450872209369663 ) ) ;
#6317 = DIRECTION ( 'NONE',  ( -1.000000000000000000, 0.000000000000000000, 0.000000000000000000 ) ) ;
#6318 = CARTESIAN_POINT ( 'NONE',  ( 8.867797255587998251, 4.866234952405400271, 7.536673658251589636 ) ) ;
#6319 = CARTESIAN_POINT ( 'NONE',  ( 12.36046591005678685, -1.940744226335692879, 13.86483863263027594 ) ) ;
#6320 = DIRECTION ( 'NONE',  ( 0.000000000000000000, 1.000000000000000000, 0.000000000000000000 ) ) ;
#6321 = CARTESIAN_POINT ( 'NONE',  ( 24.33723043407100306, 3.364332162536999959, -12.26583136334000024 ) ) ;
#6322 = EDGE_LOOP ( 'NONE', ( #54620, #48317, #36401, #65758, #58729, #54153, #38076 ) ) ;
#6323 = CARTESIAN_POINT ( 'NONE',  ( 24.30000000000000071, 0.000000000000000000, 0.000000000000000000 ) ) ;
#6324 = CARTESIAN_POINT ( 'NONE',  ( 3.000973465876999757, 3.500000000000000000, 0.000000000000000000 ) ) ;
#6325 = VECTOR ( 'NONE', #15902, 1000.000000000000000 ) ;
#6326 = CARTESIAN_POINT ( 'NONE',  ( 18.47905117804076269, -2.854821129073351837, -11.29488031137822901 ) ) ;
#6327 = CARTESIAN_POINT ( 'NONE',  ( 1.228292983454999820, -3.060375075103999976, 2.182311086106999642 ) ) ;
#6328 = CARTESIAN_POINT ( 'NONE',  ( 10.98791429143000009, -3.983006558652820051, 8.391963954669400039 ) ) ;
#6329 = B_SPLINE_CURVE_WITH_KNOTS ( 'NONE', 3,
 ( #63800, #5426, #65175, #43527 ),
 .UNSPECIFIED., .F., .F.,
 ( 4, 4 ),
 ( 0.000000000000000000, 1.000000000000000000 ),
 .UNSPECIFIED. ) ;
#6330 = CARTESIAN_POINT ( 'NONE',  ( 17.65865034516101773, 1.883559157718814880, -12.57405095325165512 ) ) ;
#6331 = CARTESIAN_POINT ( 'NONE',  ( 11.01776904286000125, 4.914120883409999863, 8.587704221454000475 ) ) ;
#6332 = AXIS2_PLACEMENT_3D ( 'NONE', #1559, #22881, #44231 ) ;
#6333 = CARTESIAN_POINT ( 'NONE',  ( 11.12133729122639991, 3.134101783108900197, 7.522778681411049995 ) ) ;
#6334 = CARTESIAN_POINT ( 'NONE',  ( 24.30000000000000071, 12.03537377768999939, 3.224868684338999980 ) ) ;
#6335 = CARTESIAN_POINT ( 'NONE',  ( 10.73615685320999980, -3.078046833211999900, -6.088743704655001032 ) ) ;
#6336 = EDGE_CURVE ( 'NONE', #36464, #43600, #21415, .T. ) ;
#6337 = VECTOR ( 'NONE', #31980, 1000.000000000000227 ) ;
#6338 = CARTESIAN_POINT ( 'NONE',  ( 25.44994642811700203, 3.641531520771000022E-14, 3.907985046680999726E-14 ) ) ;
#6339 = CARTESIAN_POINT ( 'NONE',  ( 8.679055905797000037, -2.899999999999999911, 6.571291218949999902 ) ) ;
#6340 = CARTESIAN_POINT ( 'NONE',  ( 11.42028665956053501, -4.742415037725373317, 6.450604656432373574 ) ) ;
#6341 = DIRECTION ( 'NONE',  ( -1.000000000000000000, 0.000000000000000000, 0.000000000000000000 ) ) ;
#6342 = EDGE_LOOP ( 'NONE', ( #38603, #35784 ) ) ;
#6343 = CARTESIAN_POINT ( 'NONE',  ( 8.497235841230001085, 3.789127741898000057, -9.388182174781999123 ) ) ;
#6344 = CARTESIAN_POINT ( 'NONE',  ( 10.73103300763300005, -3.307558760216100069, 6.773725604892799623 ) ) ;
#6345 = EDGE_LOOP ( 'NONE', ( #44573, #51982, #18928, #37899 ) ) ;
#6346 = CONICAL_SURFACE ( 'NONE', #18696, 12.44999944941000081, 0.7853981146832407223 ) ;
#6347 = CARTESIAN_POINT ( 'NONE',  ( 18.03303331148768862, -2.902815211882732616, 13.57973159350535752 ) ) ;
#6348 = CARTESIAN_POINT ( 'NONE',  ( 10.94072200990529886, -5.077092948368999714, -7.124286150322599376 ) ) ;
#6349 = ORIENTED_EDGE ( 'NONE', *, *, #10001, .T. ) ;
#6350 = CARTESIAN_POINT ( 'NONE',  ( 10.35814141025499957, 4.483492689244800822, 6.638851159159999682 ) ) ;
#6351 = CARTESIAN_POINT ( 'NONE',  ( 5.825282781127412157, -1.130605421812246769, 0.06802564610632597097 ) ) ;
#6352 = CARTESIAN_POINT ( 'NONE',  ( 23.77343880546692034, 3.285534861686421060, -13.18386822430981553 ) ) ;
#6353 = CARTESIAN_POINT ( 'NONE',  ( 18.05609597790000009, -3.343430715100999873, 11.12052764821000039 ) ) ;
#6354 = CARTESIAN_POINT ( 'NONE',  ( 8.457129882803000598, 5.100036551512999949, -6.571411952062999440 ) ) ;
#6355 = DIRECTION ( 'NONE',  ( 1.000000000000000000, 0.000000000000000000, 0.000000000000000000 ) ) ;
#6356 = B_SPLINE_CURVE_WITH_KNOTS ( 'NONE', 3,
 ( #20419, #20079, #30571, #45964, #15175, #57820, #30919, #35144, #63049, #29908, #67274, #51886, #3981, #41408, #9929, #3642, #31267, #25321, #61695, #3309, #19046, #24644, #19389, #35484 ),
 .UNSPECIFIED., .F., .F.,
 ( 4, 2, 1, 2, 2, 2, 2, 2, 2, 1, 2, 2, 4 ),
 ( 0.000000000000000000, 0.06249999999999997224, 0.1249999999999999445, 0.1874999999999999167, 0.2499999999999998890, 0.3749999999999998335, 0.4999999999999997780, 0.6249999999999997780, 0.6874999999999997780, 0.7499999999999998890, 0.8125000000000000000, 0.8750000000000000000, 1.000000000000000000 ),
 .UNSPECIFIED. ) ;
#6357 = CARTESIAN_POINT ( 'NONE',  ( 11.59999999999999964, -4.672781865721786332, -6.851153339015914057 ) ) ;
#6358 = AXIS2_PLACEMENT_3D ( 'NONE', #36105, #30868, #58120 ) ;
#6359 = CARTESIAN_POINT ( 'NONE',  ( 10.46009514222999925, -2.565650894080999667, -6.975682682930000489 ) ) ;
#6360 = CARTESIAN_POINT ( 'NONE',  ( 11.78594988689359901, -3.606563555963900214, -8.271690446953899212 ) ) ;
#6361 = ORIENTED_EDGE ( 'NONE', *, *, #34016, .F. ) ;
#6362 = CARTESIAN_POINT ( 'NONE',  ( 8.725348536223823004, 2.649439212887079620, 7.500023728975156345 ) ) ;
#6363 = ORIENTED_EDGE ( 'NONE', *, *, #19592, .T. ) ;
#6364 = CARTESIAN_POINT ( 'NONE',  ( 10.01277517397999972, 3.440623091551000101, -9.267603345544999982 ) ) ;
#6365 = VERTEX_POINT ( 'NONE', #46441 ) ;
#6366 = LINE ( 'NONE', #48337, #51523 ) ;
#6367 = SURFACE_SIDE_STYLE ('',( #32953 ) ) ;
#6368 = CARTESIAN_POINT ( 'NONE',  ( 3.800000448357999883, 0.000000000000000000, -1.625000000000000000 ) ) ;
#6369 = CARTESIAN_POINT ( 'NONE',  ( 10.38351354018329253, 2.750000000000000000, -7.336375382625530683 ) ) ;
#6370 = CARTESIAN_POINT ( 'NONE',  ( 12.55449126378680980, 3.072671109762265651, 13.53512077903586075 ) ) ;
#6371 = CARTESIAN_POINT ( 'NONE',  ( 9.625489929093001606, -3.134630999349000025, 8.626959345509000343 ) ) ;
#6372 = CARTESIAN_POINT ( 'NONE',  ( 5.500000000000000000, 13.94845324556000143, 4.312847325879000770 ) ) ;
#6373 = ADVANCED_FACE ( 'NONE', ( #63542 ), #28448, .F. ) ;
#6374 = CARTESIAN_POINT ( 'NONE',  ( 12.80505043854144098, 0.6249999999999996669, 13.88107975066923316 ) ) ;
#6375 = EDGE_CURVE ( 'NONE', #7391, #62696, #33070, .T. ) ;
#6376 = EDGE_LOOP ( 'NONE', ( #24682, #15427, #61392, #7338 ) ) ;
#6377 = CARTESIAN_POINT ( 'NONE',  ( 6.833909439180999357, 4.719833207100999850, -8.789699670502999496 ) ) ;
#6378 = CARTESIAN_POINT ( 'NONE',  ( 13.69997185827400266, -11.40547114375999982, -2.374390024598000082 ) ) ;
#6379 = PLANE ( 'NONE',  #28515 ) ;
#6380 = CARTESIAN_POINT ( 'NONE',  ( 4.959431403105000413, 0.2984107933419999914, 1.602071312762000099 ) ) ;
#6381 = VECTOR ( 'NONE', #59106, 1000.000000000000000 ) ;
#6382 = CARTESIAN_POINT ( 'NONE',  ( 8.731095280410999138, 2.469361196073999842, -7.826019481986000059 ) ) ;
#6383 = FACE_OUTER_BOUND ( 'NONE', #7063, .T. ) ;
#6384 = CARTESIAN_POINT ( 'NONE',  ( 10.94349328348999961, -3.081618981425999770, -8.919377696680001577 ) ) ;
#6385 = EDGE_LOOP ( 'NONE', ( #7270, #38058, #26788, #67346, #28623 ) ) ;
#6386 = CARTESIAN_POINT ( 'NONE',  ( 11.57299956498156845, 5.207010770456999893, -7.825000000000000178 ) ) ;
#6387 = CARTESIAN_POINT ( 'NONE',  ( 11.59999999999999964, 4.000000000000000000, 7.500000000000000000 ) ) ;
#6388 = VECTOR ( 'NONE', #42591, 1000.000000000000000 ) ;
#6389 = CARTESIAN_POINT ( 'NONE',  ( 9.099999931440999390, 5.250000000000000000, -7.500000000000000000 ) ) ;
#6390 = FACE_OUTER_BOUND ( 'NONE', #41480, .T. ) ;
#6391 = CARTESIAN_POINT ( 'NONE',  ( 11.78594988689359901, 4.393436444036099786, -8.271690446953899212 ) ) ;
#6392 = CARTESIAN_POINT ( 'NONE',  ( 1.284778323729000017E-07, 0.000000000000000000, 0.000000000000000000 ) ) ;
#6393 = CARTESIAN_POINT ( 'NONE',  ( 11.26723293495529887, 2.826061044294000180, -7.452807962566580180 ) ) ;
#6394 = EDGE_CURVE ( 'NONE', #61732, #60041, #22613, .T. ) ;
#6395 = CARTESIAN_POINT ( 'NONE',  ( 9.887950584426999256, 4.398663815465100768, -6.578094656394299911 ) ) ;
#6397 = CARTESIAN_POINT ( 'NONE',  ( 8.457129882803000598, 5.100036551512999949, -6.571411952062999440 ) ) ;
#6396 = CARTESIAN_POINT ( 'NONE',  ( 10.53293802597399953, -4.450760089576400347, 8.240623579255899500 ) ) ;
#6398 = FACE_OUTER_BOUND ( 'NONE', #57113, .T. ) ;
#6399 = ORIENTED_EDGE ( 'NONE', *, *, #68326, .F. ) ;
#6400 = VECTOR ( 'NONE', #52943, 1000.000000000000227 ) ;
#6401 = EDGE_CURVE ( 'NONE', #27251, #32166, #43259, .T. ) ;
#6402 = CARTESIAN_POINT ( 'NONE',  ( 10.93990547754509812, 5.032986398992000510, 7.467215766047949899 ) ) ;
#6403 = CARTESIAN_POINT ( 'NONE',  ( 17.55505043854143565, 3.199751711897561801, -12.18694338143115452 ) ) ;
#6404 = CARTESIAN_POINT ( 'NONE',  ( 9.152455549953000258, 4.995562869655000071, 8.303267676773000261 ) ) ;
#6405 = CARTESIAN_POINT ( 'NONE',  ( 5.579147253214326696, -12.92151814423300316, 2.574492151368334536 ) ) ;
#6406 = AXIS2_PLACEMENT_3D ( 'NONE', #28934, #22970, #34522 ) ;
#6407 = CARTESIAN_POINT ( 'NONE',  ( 11.15982711745999900, -5.578228817597000955, 8.067792329320999656 ) ) ;
#6408 = CARTESIAN_POINT ( 'NONE',  ( 24.53429014209899961, 12.47024915613999951, 3.026245713505000268 ) ) ;
#6409 = CARTESIAN_POINT ( 'NONE',  ( 11.40162633574000139, 3.633188743968999823, -11.83198634993999931 ) ) ;
#6410 = CARTESIAN_POINT ( 'NONE',  ( 9.938608878791999501, -4.227457260387500249, -6.521682313853199631 ) ) ;
#6411 = DIRECTION ( 'NONE',  ( 2.257582933432000069E-09, -1.000000000000000000, 1.101251388955000073E-09 ) ) ;
#6412 = CARTESIAN_POINT ( 'NONE',  ( 5.476460587185000506, 1.226089021931999978, -0.4951583500558000006 ) ) ;
#6413 = CARTESIAN_POINT ( 'NONE',  ( 10.90453766415000025, -2.900310535872000273, -5.130381900875999435 ) ) ;
#6414 = CARTESIAN_POINT ( 'NONE',  ( 11.49999672494999814, 8.721203281753671988, -7.819494091976955552 ) ) ;
#6415 = CARTESIAN_POINT ( 'NONE',  ( 12.16287348028854964, -4.761955701524100526, 7.088026579158399620 ) ) ;
#6416 = CARTESIAN_POINT ( 'NONE',  ( 10.92441504065829960, 4.694414232677499577, -6.982228367137699898 ) ) ;
#6417 = CARTESIAN_POINT ( 'NONE',  ( 11.09999999999999964, 4.000000000000000000, 7.500000000000000000 ) ) ;
#6418 = CARTESIAN_POINT ( 'NONE',  ( 24.63408956130300353, -8.686807539907999143, 8.587991764679999918 ) ) ;
#6419 = CARTESIAN_POINT ( 'NONE',  ( 8.225195096046189036, -2.649880853682571313, 7.500010424662522546 ) ) ;
#6420 = ORIENTED_EDGE ( 'NONE', *, *, #54469, .F. ) ;
#6421 = CARTESIAN_POINT ( 'NONE',  ( 7.474999999999999645, -5.349999999999999645, 7.500000000000000000 ) ) ;
#6422 = CARTESIAN_POINT ( 'NONE',  ( 10.32169598648999909, -3.233475335853099875, -7.956401575444799867 ) ) ;
#6423 = CARTESIAN_POINT ( 'NONE',  ( 24.37897525340100202, -8.840625649873999237, -8.761552777197998410 ) ) ;
#6424 = CARTESIAN_POINT ( 'NONE',  ( 5.399998535875000449, -12.99045401563999924, -1.690592933733000125 ) ) ;
#6425 = CARTESIAN_POINT ( 'NONE',  ( 12.09999999999999964, -4.000000000000000000, 7.500000000000000000 ) ) ;
#6426 = CARTESIAN_POINT ( 'NONE',  ( 5.602978689604023010, 12.13075210502077184, -3.749558893019930839 ) ) ;
#6427 = ORIENTED_EDGE ( 'NONE', *, *, #26542, .F. ) ;
#6428 = VECTOR ( 'NONE', #44718, 1000.000000000000000 ) ;
#6429 = B_SPLINE_CURVE_WITH_KNOTS ( 'NONE', 3,
 ( #13509, #56835, #41438, #57500, #9609, #8589, #2655, #50899, #2995, #14531, #30602, #4013, #25011, #35847, #56485 ),
 .UNSPECIFIED., .F., .F.,
 ( 4, 2, 2, 2, 1, 2, 2, 4 ),
 ( 0.000000000000000000, 0.2500000000000239808, 0.3750000000000371370, 0.4375000000000440203, 0.4687500000000439648, 0.4843750000000439648, 0.5000000000000439648, 1.000000000000000000 ),
 .UNSPECIFIED. ) ;
#6430 = CARTESIAN_POINT ( 'NONE',  ( 23.56666365135700403, 8.673757318230000735, 7.881093921673004488 ) ) ;
#6431 = CARTESIAN_POINT ( 'NONE',  ( 17.86097767714751328, 3.045104419577886912, -13.54261379197757087 ) ) ;
#6432 = ORIENTED_EDGE ( 'NONE', *, *, #37865, .T. ) ;
#6433 = CARTESIAN_POINT ( 'NONE',  ( 14.39999999570800249, 11.53036813819577411, -4.891445144093894193 ) ) ;
#6434 = CARTESIAN_POINT ( 'NONE',  ( 18.30003129332100187, 2.732683818840999646, 11.53064095373000164 ) ) ;
#6435 = AXIS2_PLACEMENT_3D ( 'NONE', #19039, #40707, #62033 ) ;
#6436 = CARTESIAN_POINT ( 'NONE',  ( 9.360279719594000625, 3.031907308384000022, -8.729608011560001657 ) ) ;
#6437 = ORIENTED_EDGE ( 'NONE', *, *, #42579, .T. ) ;
#6438 = CARTESIAN_POINT ( 'NONE',  ( 23.77345858638861031, -13.06030404894205077, 3.746546544767070497 ) ) ;
#6439 = CARTESIAN_POINT ( 'NONE',  ( 10.68035971519489813, -3.321859513918399731, -6.371865185335000348 ) ) ;
#6440 = CARTESIAN_POINT ( 'NONE',  ( 7.514210841224999271, 3.394203523730999539, -9.300711568980998933 ) ) ;
#6441 = VECTOR ( 'NONE', #36777, 1000.000000000000000 ) ;
#6442 = CARTESIAN_POINT ( 'NONE',  ( 10.16684687351567185, -3.231816600031351516, -6.500416447002278275 ) ) ;
#6443 = CARTESIAN_POINT ( 'NONE',  ( 4.805026506350000837, 1.500000000000000000, 0.000000000000000000 ) ) ;
#6444 = ORIENTED_EDGE ( 'NONE', *, *, #4951, .F. ) ;
#6445 = CARTESIAN_POINT ( 'NONE',  ( 10.50286331871000023, -5.158900740613000302, 8.369962360110999811 ) ) ;
#6446 = CARTESIAN_POINT ( 'NONE',  ( 17.99248396118099080, -2.946503669276440363, -13.56850299727616260 ) ) ;
#6447 = FILL_AREA_STYLE_COLOUR ( '', #67940 ) ;
#6448 = ORIENTED_EDGE ( 'NONE', *, *, #28203, .F. ) ;
#6449 = AXIS2_PLACEMENT_3D ( 'NONE', #5055, #43507, #64803 ) ;
#6450 = CARTESIAN_POINT ( 'NONE',  ( 11.09999607187999970, 1.243449787579999883E-13, 0.000000000000000000 ) ) ;
#6451 = CARTESIAN_POINT ( 'NONE',  ( 8.020125753392001400, 4.498951069075999953, -6.245588651729999441 ) ) ;
#6452 = EDGE_LOOP ( 'NONE', ( #7048, #12548, #9766, #4508 ) ) ;
#6453 = CARTESIAN_POINT ( 'NONE',  ( 9.961925467520998723, 2.860918852493000486, 7.578921399676699089 ) ) ;
#6454 = CARTESIAN_POINT ( 'NONE',  ( 17.77313190797698539, -1.794191980291848676, -12.47160287655520428 ) ) ;
#6455 = CARTESIAN_POINT ( 'NONE',  ( 4.682232516634000419, 1.148342943587000065, -0.8292968885249999422 ) ) ;
#6456 = CARTESIAN_POINT ( 'NONE',  ( 11.59999999999999787, 4.363617849674654714, -6.469788275435901959 ) ) ;
#6457 = CARTESIAN_POINT ( 'NONE',  ( 24.44496482743900145, 12.03536723905999928, -3.224852005146999989 ) ) ;
#6458 = DIRECTION ( 'NONE',  ( 0.000000000000000000, 0.000000000000000000, -1.000000000000000000 ) ) ;
#6459 = VECTOR ( 'NONE', #41872, 1000.000000000000114 ) ;
#6460 = B_SPLINE_SURFACE_WITH_KNOTS ( 'NONE', 1, 3, ( 
 ( #17387, #38717, #29968, #66994, #3027, #35204, #45001, #46024, #14559, #55833, #56171, #8281, #19106, #67332, #62097, #50928, #28937, #50240, #61076, #34523, #8620, #2344, #13193, #7937, #35877, #23664, #46371, #18432, #56513, #57192, #66308, #40428, #51271, #13873, #29624, #3365, #67672, #29273, #24701, #18776, #50587, #2687, #39757, #19452, #61754, #45689, #14215, #3701, #24357, #40772, #35544, #56862, #8959, #45347, #66657, #51604, #19800, #30299, #40105, #25040, #24013, #61419, #41125, #62438, #13537, #34856, #60958, #28110, #6772, #8163, #50465, #17971, #66192, #39290, #44204, #13422, #13073, #34403, #55720, #50127, #65498, #39636, #38591, #17626, #33705, #55024 ),
 ( #45231, #38952, #50815, #28818, #49422, #2233, #60612, #7816, #60269, #12374, #56052, #2567, #29157, #61303, #44555, #23548, #66536, #23896, #2909, #29511, #24238, #18656, #59915, #45576, #17268, #12723, #12024, #33360, #1535, #7125, #54674, #34741, #44888, #18313, #39989, #22853, #28463, #49777, #1888, #23205, #65847, #34054, #55369, #7464, #62330, #35091, #41354, #19332, #52524, #41691, #31218, #24925, #67911, #14446, #46257, #4281, #9874, #36446, #20027, #15126, #45909, #51835, #56752, #24586, #3257, #61640, #62664, #30521, #35765, #52180, #62997, #57081, #14784, #9181, #3930, #46606, #14102, #35427, #20367, #57763, #25267, #8849, #36103, #40321, #66882, #4622 ) ),
 .UNSPECIFIED., .F., .F., .F.,
 ( 2, 2 ),
 ( 4, 2, 2, 2, 2, 2, 2, 2, 2, 2, 2, 2, 2, 2, 2, 2, 2, 2, 2, 2, 2, 2, 2, 2, 2, 2, 2, 2, 2, 2, 2, 2, 2, 2, 2, 2, 2, 2, 2, 2, 2, 2, 4 ),
 ( 0.000000000000000000, 1.000000000000000000 ),
 ( 0.000000000000000000, 7.083094307561114554E-05, 0.0001416618861512222911, 0.0002124928292268334366, 0.0002833237723024445822, 0.0003541547153780557006, 0.0004249856584536668733, 0.0004958166015292780459, 0.0005666475446048891643, 0.0006374784876805002828, 0.0007083094307561114012, 0.0007791403738317225196, 0.0008145558453695280789, 0.0008499713169073337465, 0.0008853867884451394141, 0.0009208022599829449734, 0.0009916332030585560918, 0.001027048674596361651, 0.001062464146134167210, 0.001097879617671972769, 0.001133295089209778329, 0.001204126032285389447, 0.001239541503823195006, 0.001274956975361000566, 0.001310372446898806125, 0.001345787918436611684, 0.001416618861512222802, 0.001487449804587833921, 0.001522865276125639480, 0.001558280747663445039, 0.001629111690739056158, 0.001699942633814667493, 0.001735358105352473052, 0.001770773576890278828, 0.001806189048428084388, 0.001841604519965889947, 0.001912435463041501065, 0.001983266406117112184, 0.002018681877654917960, 0.002054097349192723302, 0.002124928292268334420, 0.002195759235343945539, 0.002266590178419556657 ),
 .UNSPECIFIED. ) ;
#6461 = CARTESIAN_POINT ( 'NONE',  ( 9.282063610504998508, 4.355629271815800507, 6.709281487801199262 ) ) ;
#6462 = EDGE_CURVE ( 'NONE', #45774, #38751, #64220, .T. ) ;
#6463 = CARTESIAN_POINT ( 'NONE',  ( 8.705449068729999240, 3.636021264089499994, -8.287166017043100297 ) ) ;
#6464 = EDGE_CURVE ( 'NONE', #6746, #61459, #17208, .T. ) ;
#6465 = ORIENTED_EDGE ( 'NONE', *, *, #23404, .F. ) ;
#6466 = CARTESIAN_POINT ( 'NONE',  ( 24.30000000000000071, 50.08530474119000075, -49.09535524753000146 ) ) ;
#6467 = CARTESIAN_POINT ( 'NONE',  ( 10.56170778040999991, 5.057487376164999660, -8.595710652231000282 ) ) ;
#6468 = CARTESIAN_POINT ( 'NONE',  ( 17.71367434320026035, -11.53249064895033271, 4.886450710725981139 ) ) ;
#6469 = CARTESIAN_POINT ( 'NONE',  ( 12.61514273204568859, 1.812907417374174379, -13.88212581052983197 ) ) ;
#6470 = CARTESIAN_POINT ( 'NONE',  ( 11.20851354018270207, -3.836375382625528019, 8.749999999999996447 ) ) ;
#6471 = CARTESIAN_POINT ( 'NONE',  ( 10.77462219945999955, -5.575466189878000911, 8.682669263022999573 ) ) ;
#6472 = CARTESIAN_POINT ( 'NONE',  ( 18.21574553171933886, -0.3008963210924971987, 13.99677033988233354 ) ) ;
#6473 = CARTESIAN_POINT ( 'NONE',  ( 24.74446781360200021, -3.238412344267999732, 11.83115098604999993 ) ) ;
#6474 = ORIENTED_EDGE ( 'NONE', *, *, #60714, .F. ) ;
#6475 = ORIENTED_EDGE ( 'NONE', *, *, #17460, .F. ) ;
#6476 = CARTESIAN_POINT ( 'NONE',  ( 11.00588826681000043, 3.012760565655999923, 5.961496895743000124 ) ) ;
#6477 = CARTESIAN_POINT ( 'NONE',  ( 12.44245189050256073, -0.5091685952834601459, 13.88744776337617282 ) ) ;
#6478 = CARTESIAN_POINT ( 'NONE',  ( 10.77195525820100031, -4.120672149427799802, 8.772302877803999976 ) ) ;
#6479 = FACE_OUTER_BOUND ( 'NONE', #21033, .T. ) ;
#6480 = DIRECTION ( 'NONE',  ( 0.000000000000000000, 0.000000000000000000, -1.000000000000000000 ) ) ;
#6481 = CARTESIAN_POINT ( 'NONE',  ( 9.099999999999999645, 11.84999999999999964, 0.000000000000000000 ) ) ;
#6482 = CARTESIAN_POINT ( 'NONE',  ( 0.07500030076246999577, 0.000000000000000000, 0.000000000000000000 ) ) ;
#6484 = FACE_OUTER_BOUND ( 'NONE', #53085, .T. ) ;
#6483 = CARTESIAN_POINT ( 'NONE',  ( 10.96957120343300041, -4.062009413492949861, 6.222291352336999815 ) ) ;
#6485 = CARTESIAN_POINT ( 'NONE',  ( 10.12426357027499790, 5.254871132332000094, -7.742104041724699570 ) ) ;
#6486 = EDGE_CURVE ( 'NONE', #38535, #39410, #7233, .T. ) ;
#6487 = CARTESIAN_POINT ( 'NONE',  ( 24.44916829770000177, -8.894890565782000991, -9.199951775352998240 ) ) ;
#6488 = VECTOR ( 'NONE', #31372, 1000.000000000000000 ) ;
#6489 = CARTESIAN_POINT ( 'NONE',  ( 23.56681878841384403, 10.34114842139075563, -9.422272710775716931 ) ) ;
#6490 = CARTESIAN_POINT ( 'NONE',  ( 17.71666921258853122, -0.6040886362899380302, 12.68065483099174884 ) ) ;
#6491 = CARTESIAN_POINT ( 'NONE',  ( 8.969356963619999235, -5.119357025014000584, -7.499999999914821025 ) ) ;
#6492 = PRESENTATION_LAYER_ASSIGNMENT (  '', '', ( #28835 ) ) ;
#6493 = CARTESIAN_POINT ( 'NONE',  ( 18.04518119038796442, -2.887943935952099306, -12.35267345331065414 ) ) ;
#6494 = ORIENTED_EDGE ( 'NONE', *, *, #37135, .T. ) ;
#6496 = CARTESIAN_POINT ( 'NONE',  ( 17.55505043854143565, 1.875000000000000000, -12.57545641911172751 ) ) ;
#6495 = CARTESIAN_POINT ( 'NONE',  ( 8.674245559624999657, -5.983034890242000081, 7.440798487724999966 ) ) ;
#6497 = CARTESIAN_POINT ( 'NONE',  ( 9.881820280408998514, 4.325866256860000369, -9.125812605905000652 ) ) ;
#6498 = DIRECTION ( 'NONE',  ( 0.000000000000000000, 0.000000000000000000, -1.000000000000000000 ) ) ;
#6499 = CARTESIAN_POINT ( 'NONE',  ( 6.998282674564999972, -1.401716800305999877, -2.564925509195000141E-10 ) ) ;
#6500 = CIRCLE ( 'NONE', #23232, 2.250000000000000000 ) ;
#6501 = CARTESIAN_POINT ( 'NONE',  ( 0.2691580992186000110, -1.644388561977000007, -3.014063655381999940 ) ) ;
#6502 = CARTESIAN_POINT ( 'NONE',  ( 10.56591429142999949, 4.019686495353769651, 8.533318907609000803 ) ) ;
#6503 = CARTESIAN_POINT ( 'NONE',  ( 11.33382334123000135, 2.642405149457999869, -7.577896731332000257 ) ) ;
#6504 = EDGE_LOOP ( 'NONE', ( #24749, #45634, #33512, #60016, #12943, #18412, #32841, #42428, #61785, #47821, #14978, #38719, #41181, #45076, #20857, #49528, #12153, #33659, #6667 ) ) ;
#6505 = CARTESIAN_POINT ( 'NONE',  ( 12.09168743772586296, -0.1288995356414814608, -12.59934597632939735 ) ) ;
#6506 = VECTOR ( 'NONE', #60355, 1000.000000000000000 ) ;
#6507 = CARTESIAN_POINT ( 'NONE',  ( 11.05391045180431675, -2.870950512581995628, -8.114538794791121390 ) ) ;
#6508 = CARTESIAN_POINT ( 'NONE',  ( 18.27038927661324053, 2.598921547761769091, -12.32906097307314219 ) ) ;
#6509 = CARTESIAN_POINT ( 'NONE',  ( 15.52913652543167089, -8.833284221180715434, -7.896593172538426408 ) ) ;
#6510 = CARTESIAN_POINT ( 'NONE',  ( 7.320267219589999819, 2.466388272391000225, 6.935562100014999842 ) ) ;
#6511 = ORIENTED_EDGE ( 'NONE', *, *, #52700, .F. ) ;
#6512 = CARTESIAN_POINT ( 'NONE',  ( 6.810575618758000438, 0.8089969479913999839, 1.225571816066999942 ) ) ;
#6513 = CARTESIAN_POINT ( 'NONE',  ( 8.593395280410000225, 4.529523339102000890, -8.867457431226998921 ) ) ;
#6515 = CARTESIAN_POINT ( 'NONE',  ( 9.242342830452999536, 5.206708472530999998, 8.808826521083998884 ) ) ;
#6514 = CARTESIAN_POINT ( 'NONE',  ( 8.449745872479532238, -2.260409384866206128, 7.500964401359662581 ) ) ;
#6516 = CARTESIAN_POINT ( 'NONE',  ( 11.46989666366029859, 3.941571897678119996, -8.814970315645998866 ) ) ;
#6517 = ORIENTED_EDGE ( 'NONE', *, *, #42251, .T. ) ;
#6518 = CARTESIAN_POINT ( 'NONE',  ( 16.39932787941000214, -3.295363098100999810, -11.83520513879000013 ) ) ;
#6519 = CARTESIAN_POINT ( 'NONE',  ( 9.569799020577001158, -4.064052785562999759, 8.919253808370999792 ) ) ;
#6520 = ORIENTED_EDGE ( 'NONE', *, *, #50264, .T. ) ;
#6521 = CARTESIAN_POINT ( 'NONE',  ( 24.71429018881659445, 3.125258109923432670, -11.79469236763018181 ) ) ;
#6522 = DIRECTION ( 'NONE',  ( 1.000000000000000000, 0.000000000000000000, 0.000000000000000000 ) ) ;
#6523 = CARTESIAN_POINT ( 'NONE',  ( 18.10142235202799199, -0.3036576181174172051, -13.89554011873102546 ) ) ;
#6524 = EDGE_CURVE ( 'NONE', #64614, #21925, #42237, .T. ) ;
#6525 = EDGE_CURVE ( 'NONE', #21901, #8000, #33468, .T. ) ;
#6526 = VERTEX_POINT ( 'NONE', #37664 ) ;
#6527 = CARTESIAN_POINT ( 'NONE',  ( 10.35084866221912137, -5.758574906236493263, -7.748452900945333788 ) ) ;
#6528 = CARTESIAN_POINT ( 'NONE',  ( 17.60000001947600268, -11.86186880240999919, 3.298627760718999991 ) ) ;
#6529 = CARTESIAN_POINT ( 'NONE',  ( 10.11476354018332913, -2.782534154164604256, 7.827184855449092815 ) ) ;
#6530 = CARTESIAN_POINT ( 'NONE',  ( 8.961955453702401542, -2.270851131865847528, 7.235821414696904874 ) ) ;
#6531 = CARTESIAN_POINT ( 'NONE',  ( 10.55862282008599884, -3.333723918618700210, 6.425317846273999933 ) ) ;
#6532 = ORIENTED_EDGE ( 'NONE', *, *, #22160, .F. ) ;
#6533 = DIRECTION ( 'NONE',  ( 1.000000000000000000, 0.000000000000000000, 0.000000000000000000 ) ) ;
#6534 = CARTESIAN_POINT ( 'NONE',  ( 24.25866698968500401, -12.09695184427999948, -3.327214749306000030 ) ) ;
#6535 = APPLICATION_CONTEXT ( 'automotive_design' ) ;
#6536 = CARTESIAN_POINT ( 'NONE',  ( 8.404999999999999361, 5.190914425723000214, -8.768195054477999406 ) ) ;
#6537 = CARTESIAN_POINT ( 'NONE',  ( 15.77677363193000204, -9.321312496448001639, -8.284802892401000207 ) ) ;
#6538 = ORIENTED_EDGE ( 'NONE', *, *, #68170, .F. ) ;
#6539 = CARTESIAN_POINT ( 'NONE',  ( 12.54434846374639001, -1.931873423426546443, -12.56592826555433362 ) ) ;
#6540 = VECTOR ( 'NONE', #54111, 1000.000000000000114 ) ;
#6541 = DIRECTION ( 'NONE',  ( 0.000000000000000000, 0.000000000000000000, 1.000000000000000000 ) ) ;
#6542 = CARTESIAN_POINT ( 'NONE',  ( 10.20000099824999928, 0.000000000000000000, 0.000000000000000000 ) ) ;
#6543 = CARTESIAN_POINT ( 'NONE',  ( 12.09999999999999964, -2.820501972398000046, 7.825000000000000178 ) ) ;
#6544 = CARTESIAN_POINT ( 'NONE',  ( 12.08884934673722711, -2.402320636441741541, -13.79236805980801073 ) ) ;
#6545 = AXIS2_PLACEMENT_3D ( 'NONE', #7893, #2980, #18387 ) ;
#6546 = CARTESIAN_POINT ( 'NONE',  ( 10.92026088462129962, -3.997864853650589634, -6.496532863517000322 ) ) ;
#6547 = CARTESIAN_POINT ( 'NONE',  ( 7.143568539511687909, 1.224060264657293562, -0.3280695054382070097 ) ) ;
#6548 = CARTESIAN_POINT ( 'NONE',  ( 17.57923549477752090, -1.761145725279483987, 12.47631219955854043 ) ) ;
#6549 = VERTEX_POINT ( 'NONE', #58994 ) ;
#6550 = CARTESIAN_POINT ( 'NONE',  ( 10.97635090131019986, -3.000792947412299849, -8.118017011233499503 ) ) ;
#6551 = EDGE_CURVE ( 'NONE', #24471, #16376, #14273, .T. ) ;
#6552 = ORIENTED_EDGE ( 'NONE', *, *, #11840, .F. ) ;
#6553 = CARTESIAN_POINT ( 'NONE',  ( 11.82330164685100193, -12.43416923969000010, -1.799281280950999928 ) ) ;
#6554 = CARTESIAN_POINT ( 'NONE',  ( 8.897989158775001073, 4.990139824845000405, -9.121472988377998803 ) ) ;
#6555 = EDGE_CURVE ( 'NONE', #63357, #64129, #5844, .T. ) ;
#6556 = CARTESIAN_POINT ( 'NONE',  ( 10.47212119989999835, 2.640756834784999896, -8.505248851866998194 ) ) ;
#6557 = CARTESIAN_POINT ( 'NONE',  ( 10.69578225082999978, -5.505007625740000243, -7.759264430206000540 ) ) ;
#6558 = DIRECTION ( 'NONE',  ( 0.8480635683783692702, 0.3746919961710865610, 0.3746919961710865610 ) ) ;
#6559 = LINE ( 'NONE', #12159, #28336 ) ;
#6560 = DIRECTION ( 'NONE',  ( 0.000000000000000000, 1.000000000000000000, 0.000000000000000000 ) ) ;
#6561 = ORIENTED_EDGE ( 'NONE', *, *, #16171, .F. ) ;
#6562 = DIRECTION ( 'NONE',  ( 0.000000000000000000, 1.000000000000000000, 0.000000000000000000 ) ) ;
#6563 = CARTESIAN_POINT ( 'NONE',  ( 10.83668832355999889, 4.288537082977999404, 9.448742031664000507 ) ) ;
#6564 = CARTESIAN_POINT ( 'NONE',  ( 11.09999999999999964, -2.274006712557999688, -7.281956340829000673 ) ) ;
#6565 = CARTESIAN_POINT ( 'NONE',  ( 10.86325056272499978, -3.107965259299500183, 7.486779603004729111 ) ) ;
#6566 = DIRECTION ( 'NONE',  ( -0.5000000000000150990, -0.08222066253632250021, 0.8621135439442261239 ) ) ;
#6567 = CIRCLE ( 'NONE', #32238, 13.00000000000000178 ) ;
#6568 = CARTESIAN_POINT ( 'NONE',  ( 10.94903032197929882, 4.503839166471300004, -6.795411691360399686 ) ) ;
#6569 = B_SPLINE_CURVE_WITH_KNOTS ( 'NONE', 3,
 ( #49973, #2767, #40181, #30046 ),
 .UNSPECIFIED., .F., .F.,
 ( 4, 4 ),
 ( 0.000000000000000000, 1.000000000000000000 ),
 .UNSPECIFIED. ) ;
#6570 = MANIFOLD_SOLID_BREP ( 'Stock-MAS-678-1', #59319 ) ;
#6571 = EDGE_CURVE ( 'NONE', #64727, #58276, #54244, .T. ) ;
#6572 = CARTESIAN_POINT ( 'NONE',  ( 11.05947712336470623, 5.538520942943965686, 7.349130516419430492 ) ) ;
#6573 = CARTESIAN_POINT ( 'NONE',  ( 23.74079507723600102, -9.838286271853998954, -9.517717110099001232 ) ) ;
#6574 = CARTESIAN_POINT ( 'NONE',  ( 23.85161546330200011, -9.644042618899000274, 9.632248201521999675 ) ) ;
#6575 = PRESENTATION_STYLE_ASSIGNMENT (( #48196 ) ) ;
#6576 = ORIENTED_EDGE ( 'NONE', *, *, #28951, .T. ) ;
#6577 = CARTESIAN_POINT ( 'NONE',  ( 9.842711596872401714, 5.100000000000000533, -6.305985889525932642 ) ) ;
#6578 = CARTESIAN_POINT ( 'NONE',  ( 7.260787643466000141, -0.7925871808662000584, 0.8087861320687000921 ) ) ;
#6579 = CARTESIAN_POINT ( 'NONE',  ( 18.05171780850496788, 2.879539315883434369, 13.58554773987827602 ) ) ;
#6580 = CARTESIAN_POINT ( 'NONE',  ( 10.71434555353880924, 4.907414883814396944, 4.811875879775000975 ) ) ;
#6581 = CARTESIAN_POINT ( 'NONE',  ( 11.42887348028849992, -5.124210964533999935, -8.107837221875000111 ) ) ;
#6582 = ORIENTED_EDGE ( 'NONE', *, *, #62650, .F. ) ;
#6583 = CARTESIAN_POINT ( 'NONE',  ( 24.63780974963800219, 3.092545797709000066, -11.81390549036999893 ) ) ;
#6584 = CARTESIAN_POINT ( 'NONE',  ( 9.015545280411000562, 4.175915362023999933, 5.699506188181000077 ) ) ;
#6586 = CARTESIAN_POINT ( 'NONE',  ( 11.39975833414730033, 4.796537143354000499, 7.825000000000000178 ) ) ;
#6585 = CARTESIAN_POINT ( 'NONE',  ( 9.251970280414001380, 5.673443217382001080, -7.051790060464000476 ) ) ;
#6587 = CARTESIAN_POINT ( 'NONE',  ( 10.88269269398620764, 2.957535174095307529, 4.893996436090802149 ) ) ;
#6588 = ORIENTED_EDGE ( 'NONE', *, *, #3223, .T. ) ;
#6589 = CARTESIAN_POINT ( 'NONE',  ( 11.05935155529000014, 2.480238120735000162, 6.610075178640000715 ) ) ;
#6591 = CARTESIAN_POINT ( 'NONE',  ( 17.77689708618911268, -3.084393760937525375, -13.53193451522998103 ) ) ;
#6590 = AXIS2_PLACEMENT_3D ( 'NONE', #31361, #52674, #53370 ) ;
#6592 = CARTESIAN_POINT ( 'NONE',  ( 11.73256516821459883, 4.706297556651700020, 6.787191910456499500 ) ) ;
#6593 = CARTESIAN_POINT ( 'NONE',  ( 10.14750362918999826, -2.602959084636999876, 6.738575912023000214 ) ) ;
#6594 = CARTESIAN_POINT ( 'NONE',  ( 7.528515907654997896, 3.227039430994999236, 6.419564954296006931 ) ) ;
#6595 = ORIENTED_EDGE ( 'NONE', *, *, #52955, .T. ) ;
#6596 = CARTESIAN_POINT ( 'NONE',  ( 24.62774583285499830, 12.19917312477000060, -3.045379866085000220 ) ) ;
#6598 = CARTESIAN_POINT ( 'NONE',  ( 10.31966935320999923, -4.764591648058999596, -5.997654637741999473 ) ) ;
#6597 = CARTESIAN_POINT ( 'NONE',  ( 12.21268235885900033, -11.62758720635999765, 4.758865308234000224 ) ) ;
#6599 = CARTESIAN_POINT ( 'NONE',  ( 7.744183139975749697, -5.475625709055735868, 8.421281122564774790 ) ) ;
#6600 = CARTESIAN_POINT ( 'NONE',  ( 9.843726350706999639, -4.115123626494000320, 9.466607949400000166 ) ) ;
#6601 = CARTESIAN_POINT ( 'NONE',  ( 11.09999999999999964, 5.350000000000000533, 7.500000000000000000 ) ) ;
#6602 = ORIENTED_EDGE ( 'NONE', *, *, #18008, .T. ) ;
#6603 = CARTESIAN_POINT ( 'NONE',  ( 24.03543920757945074, -9.310452318425328500, 9.237282073437325991 ) ) ;
#6604 = CARTESIAN_POINT ( 'NONE',  ( 11.88379707368349969, -4.566644629509899467, 8.490052513816499058 ) ) ;
#6605 = CARTESIAN_POINT ( 'NONE',  ( 7.762706781754004304, 3.200128145701000904, 6.302820412756005020 ) ) ;
#6606 = CARTESIAN_POINT ( 'NONE',  ( 11.37964291764649971, 2.731641218595000087, 7.656787697937099679 ) ) ;
#6607 = ORIENTED_EDGE ( 'NONE', *, *, #16658, .F. ) ;
#6608 = EDGE_CURVE ( 'NONE', #59297, #4993, #36807, .T. ) ;
#6609 = EDGE_CURVE ( 'NONE', #58398, #16938, #40825, .T. ) ;
#6610 = B_SPLINE_SURFACE_WITH_KNOTS ( 'NONE', 3, 3, ( 
 ( #43840, #43496, #21134, #16905, #10634, #53291, #48387, #16223, #65141, #10982, #53634, #27766, #42802, #32321, #27411, #32659, #12017, #59909, #64444, #38235, #38585, #64794, #59564, #53969, #63768, #5392, #5729, #21466, #22497, #49075, #494, #6074, #27070, #26730, #11661, #1188, #21809, #16569, #48046, #6416, #17262, #148, #69020, #64108, #43143, #37895, #33353, #59216, #48737, #50120, #44881, #23889, #65492, #18306, #2560, #1882, #55363, #1529, #13066, #50459, #60263, #49417, #12368, #23198, #65841, #34396, #28811 ),
 ( #2227, #12716, #44548, #33698, #23542, #55714, #38945, #45224, #66186, #39630, #55018, #60952, #66530, #7810, #29151, #18649, #39983, #13416, #61296, #17965, #60605, #34048, #49771, #34735, #54668, #6765, #28104, #39284, #22847, #7119, #7458, #44198, #28457, #17619, #59793, #54899, #59104, #7000, #11544, #27645, #27994, #63993, #11210, #43029, #65023, #17139, #47936, #54198, #11897, #32546, #64331, #36, #1413, #38120, #49301, #1073, #33235, #16792, #48964, #27298, #22035, #21356, #12253, #22729, #44079, #54555, #37436 ),
 ( #42685, #16451, #22386, #26957, #58759, #38472, #10863, #16111, #33581, #6651, #37780, #53524, #65377, #17498, #32209, #5614, #38821, #60147, #43725, #48271, #53859, #48622, #377, #21693, #5959, #59447, #43382, #725, #6299, #32888, #64682, #29039, #39167, #19211, #18535, #40208, #50349, #39512, #66416, #61524, #24117, #23774, #2114, #44770, #23431, #39864, #66070, #8041, #18190, #2449, #34277, #61861, #55939, #45107, #55597, #50003, #29384, #34965, #7345, #3135, #50695, #45451, #60836, #34626, #45790, #66765, #18880 ),
 ( #12949, #7698, #28333, #56624, #61184, #28690, #2791, #13304, #29730, #33927, #13639, #56282, #8388, #51035, #67103, #24465, #40537, #13982, #35307, #49653, #1761, #23080, #44427, #65725, #17849, #60489, #12599, #55248, #41231, #47510, #30742, #25146, #41914, #46134, #4153, #8729, #3472, #52050, #25493, #36326, #4843, #26184, #15000, #51374, #24809, #57641, #68816, #31095, #63222, #47164, #15688, #68465, #14326, #67439, #30071, #19562, #4494, #40884, #36677, #20938, #42271, #25834, #62205, #20588, #35650, #56962, #46822 ) ),
 .UNSPECIFIED., .F., .F., .F.,
 ( 4, 4 ),
 ( 4, 1, 1, 1, 1, 1, 1, 1, 1, 1, 1, 1, 1, 1, 1, 1, 1, 1, 1, 1, 1, 1, 1, 1, 1, 1, 1, 1, 1, 1, 1, 1, 1, 1, 1, 1, 1, 1, 1, 1, 1, 1, 1, 1, 1, 1, 1, 1, 1, 1, 1, 1, 1, 1, 1, 1, 1, 1, 1, 1, 1, 1, 1, 1, 4 ),
 ( -0.02000000000000000042, 1.020000000000000018 ),
 ( 0.008747244164287000176, 0.02453926110774999961, 0.04033127805120999970, 0.05612329499467000327, 0.07191531193812999989, 0.08770732888158999652, 0.1034993458251000087, 0.1192913627684999978, 0.1350833797120000179, 0.1508753966553999792, 0.1666674135988999994, 0.1824594305423999918, 0.1982514474858000086, 0.2140434644293000011, 0.2298354813727000179, 0.2456274983162000103, 0.2614195152596999749, 0.2772115322030999640, 0.2930035491465999842, 0.3087955660900000288, 0.3245875830334999934, 0.3403795999769999581, 0.3561716169204000026, 0.3719636338639000228, 0.3877556508073999875, 0.4035476677507999765, 0.4193396846942999967, 0.4351317016376999858, 0.4509237185811999504, 0.4667157355247000261, 0.4825077524681000152, 0.4982997694115999798, 0.5140917863550000799, 0.5298838032985000446, 0.5456758202420000092, 0.5614678371854000538, 0.5772598541289000185, 0.5930518710723000630, 0.6088438880158000277, 0.6246359049592999924, 0.6404279219027000369, 0.6562199388462000016, 0.6720119557896999662, 0.6878039727331000108, 0.7035959896765999755, 0.7193880066200000201, 0.7351800235634999847, 0.7509720405069999494, 0.7667640574504001050, 0.7825560743939000696, 0.7983480913373000032, 0.8141401082808000789, 0.8299321252243000435, 0.8457241421676999771, 0.8615161591112000528, 0.8773081760545999863, 0.8931001929981000620, 0.9088922099416000266, 0.9246842268849999602, 0.9404762438285000359, 0.9562682607720000005, 0.9720602777153999341, 0.9878522946589000098, 1.003644311601999961, 1.019436328545999970 ),
 .UNSPECIFIED. ) ;
#6611 = CARTESIAN_POINT ( 'NONE',  ( 9.758079719591000512, 4.905765359186999852, -8.776126235875999271 ) ) ;
#6612 = CARTESIAN_POINT ( 'NONE',  ( 10.02052890782000105, 2.899999999999999911, 6.152188490330000370 ) ) ;
#6613 = EDGE_CURVE ( 'NONE', #21433, #24707, #55131, .T. ) ;
#6614 = CARTESIAN_POINT ( 'NONE',  ( 12.08596835297189287, 2.576236330983344036, -12.33383868535373296 ) ) ;
#6615 = CARTESIAN_POINT ( 'NONE',  ( 11.93856039236529831, -2.967715280237000375, 7.449760924956519759 ) ) ;
#6616 =( BOUNDED_SURFACE ( )  B_SPLINE_SURFACE ( 3, 3, ( 
 ( #52553, #42756, #42070, #13027 ),
 ( #60565, #1837, #796, #33309 ),
 ( #55321, #55673, #54627, #2186 ),
 ( #12673, #64751, #22804, #27369 ) ),
 .UNSPECIFIED., .F., .F., .T. ) 
 B_SPLINE_SURFACE_WITH_KNOTS ( ( 4, 4 ),
 ( 4, 4 ),
 ( 0.000000000000000000, 1.000000000000000000 ),
 ( 0.000000000000000000, 1.000000000000000000 ),
 .UNSPECIFIED. ) 
 GEOMETRIC_REPRESENTATION_ITEM ( )  RATIONAL_B_SPLINE_SURFACE ( (
 ( 1.512182578520000042, 1.160176301760999840, 1.160176301760999840, 1.512182578520000042),
 ( 1.111288591041000196, 0.8526025270081000196, 0.8526025270081000196, 1.111288591041000196),
 ( 1.111288591041000196, 0.8526025270081000196, 0.8526025270081000196, 1.111288591041000196),
 ( 1.512182578520000042, 1.160176301760999840, 1.160176301760999840, 1.512182578520000042) ) ) 
 REPRESENTATION_ITEM ( '' )  SURFACE ( )  );
#6617 = ORIENTED_EDGE ( 'NONE', *, *, #744, .F. ) ;
#6618 = DIRECTION ( 'NONE',  ( -0.7071070951631277524, 0.7071064672098279491, 3.067185053825119010E-10 ) ) ;
#6619 = DIRECTION ( 'NONE',  ( -1.000000000000000000, 0.000000000000000000, 0.000000000000000000 ) ) ;
#6620 = ORIENTED_EDGE ( 'NONE', *, *, #15554, .T. ) ;
#6621 = CARTESIAN_POINT ( 'NONE',  ( 24.35365242081699932, 12.20235406300999514, 3.288253180468997172 ) ) ;
#6622 = CARTESIAN_POINT ( 'NONE',  ( 23.94498321860814727, 9.457022807326861624, 9.320427756281231879 ) ) ;
#6623 = VERTEX_POINT ( 'NONE', #66647 ) ;
#6624 = B_SPLINE_SURFACE_WITH_KNOTS ( 'NONE', 3, 3, ( 
 ( #67074, #40182, #62853, #30376 ),
 ( #8361, #51684, #25120, #46452 ),
 ( #29707, #34939, #14635, #56939 ),
 ( #35953, #35281, #19876, #51008 ),
 ( #40510, #20215, #46792, #67412 ),
 ( #57614, #57267, #14298, #40855 ),
 ( #31064, #56597, #25460, #56254 ),
 ( #18855, #46106, #3108, #24779 ),
 ( #3442, #8704, #2768, #9367 ),
 ( #30047, #51350, #52023, #4124 ) ),
 .UNSPECIFIED., .F., .F., .F.,
 ( 4, 1, 1, 1, 1, 1, 1, 4 ),
 ( 4, 4 ),
 ( 0.07203983506773999068, 0.1428571428570999946, 0.2857142857143000203, 0.4285714285713999594, 0.5714285714286000406, 0.7142857142856999797, 0.8571428571429000609, 0.9589780836993999635 ),
 ( -0.1900620218102000158, 1.190128522698000069 ),
 .UNSPECIFIED. ) ;
#6625 = CARTESIAN_POINT ( 'NONE',  ( 12.70928935905668489, -3.193791526923299706, -12.18850694772984333 ) ) ;
#6626 = CARTESIAN_POINT ( 'NONE',  ( 11.73256516821459883, 4.706297556651700020, 6.787191910456499500 ) ) ;
#6627 = CARTESIAN_POINT ( 'NONE',  ( 10.72129555961999792, -4.673507771948999689, -5.778404201896999659 ) ) ;
#6628 = CARTESIAN_POINT ( 'NONE',  ( 10.66684687351590277, 4.768183399968648040, 8.499583552997725278 ) ) ;
#6629 = CARTESIAN_POINT ( 'NONE',  ( 18.19189882637400046, -12.11510371750999937, 3.327574861395000028 ) ) ;
#6630 = DIRECTION ( 'NONE',  ( 0.000000000000000000, -0.6460255221484837440, 0.7633158093035797842 ) ) ;
#6631 = DIRECTION ( 'NONE',  ( 0.000000000000000000, -0.9905022095861402143, 0.1374968101629056305 ) ) ;
#6632 = CARTESIAN_POINT ( 'NONE',  ( 17.85930819889520649, -0.5460377805369022175, -12.68419612078312220 ) ) ;
#6633 = CARTESIAN_POINT ( 'NONE',  ( 12.21329150906689343, 2.701250044071452194, -12.40242623238894559 ) ) ;
#6634 = CARTESIAN_POINT ( 'NONE',  ( 11.60118044953561878, -2.866798846279000390, -8.090905336380599167 ) ) ;
#6635 = CARTESIAN_POINT ( 'NONE',  ( 8.995176658772999545, 2.707986230053999854, 5.994446745591000436 ) ) ;
#6636 = ORIENTED_EDGE ( 'NONE', *, *, #14550, .T. ) ;
#6637 = DIRECTION ( 'NONE',  ( 0.000000000000000000, -0.4257792915651026910, -0.9048270524660053660 ) ) ;
#6638 = CARTESIAN_POINT ( 'NONE',  ( 9.610944094206999466, 5.100000000000000533, -6.571291218949999902 ) ) ;
#6639 = CARTESIAN_POINT ( 'NONE',  ( 16.39999999347100257, 3.345256695718999751, 11.86066175541999890 ) ) ;
#6640 = CARTESIAN_POINT ( 'NONE',  ( 18.08635919897130151, 2.970004615628405897, 12.24496439055023700 ) ) ;
#6641 = CARTESIAN_POINT ( 'NONE',  ( 10.86180282788866691, 2.874603711589708066, -6.749639981055100435 ) ) ;
#6642 = DIRECTION ( 'NONE',  ( 0.000000000000000000, 0.000000000000000000, -1.000000000000000000 ) ) ;
#6643 = CARTESIAN_POINT ( 'NONE',  ( 12.80505043854144276, -0.7302158263239078018, 13.98094363220830871 ) ) ;
#6644 = DIRECTION ( 'NONE',  ( 1.000000000000000000, 0.000000000000000000, 0.000000000000000000 ) ) ;
#6645 = ORIENTED_EDGE ( 'NONE', *, *, #26350, .F. ) ;
#6646 = CARTESIAN_POINT ( 'NONE',  ( 12.12887591290038536, -2.220077349933753830, 12.40287778440552380 ) ) ;
#6647 = CARTESIAN_POINT ( 'NONE',  ( 8.922480666858998433, -3.619299191678599925, -8.576476893896000320 ) ) ;
#6648 = DIRECTION ( 'NONE',  ( 0.8660254037831510709, 1.247809965406074354E-13, -0.5000000000022299940 ) ) ;
#6649 = CARTESIAN_POINT ( 'NONE',  ( 8.276217158405398067, 2.979004627675164940, -6.354038587687713679 ) ) ;
#6650 = B_SPLINE_CURVE_WITH_KNOTS ( 'NONE', 1,
 ( #42538, #37290 ),
 .UNSPECIFIED., .F., .F.,
 ( 2, 2 ),
 ( 0.000000000000000000, 1.000000000000000000 ),
 .UNSPECIFIED. ) ;
#6651 = CARTESIAN_POINT ( 'NONE',  ( 11.50687348028854906, 2.996540789803000315, -8.042549288197099244 ) ) ;
#6652 = ADVANCED_FACE ( 'NONE', ( #1994 ), #23316, .F. ) ;
#6653 = CARTESIAN_POINT ( 'NONE',  ( 12.08233499759481155, -0.05827135643915358487, 12.59987075990256677 ) ) ;
#6654 = CARTESIAN_POINT ( 'NONE',  ( 9.475899447075999404, 4.122021000979000149, 9.013569734175000292 ) ) ;
#6655 = LINE ( 'NONE', #22733, #67368 ) ;
#6656 = EDGE_CURVE ( 'NONE', #2626, #53063, #68715, .T. ) ;
#6657 = CARTESIAN_POINT ( 'NONE',  ( 12.52646068131086210, 3.059569037265597480, 12.30341205401442473 ) ) ;
#6658 = VERTEX_POINT ( 'NONE', #50574 ) ;
#6659 = CARTESIAN_POINT ( 'NONE',  ( 7.100000000000000533, 0.000000000000000000, 0.000000000000000000 ) ) ;
#6660 = CARTESIAN_POINT ( 'NONE',  ( 10.91610672858429965, 3.088399709291500095, -6.814233985789400094 ) ) ;
#6661 = DIRECTION ( 'NONE',  ( 0.000000000000000000, 0.000000000000000000, 1.000000000000000000 ) ) ;
#6663 = CARTESIAN_POINT ( 'NONE',  ( 25.29995873461299993, 11.13046969959000165, 3.427501705020000067 ) ) ;
#6662 = CARTESIAN_POINT ( 'NONE',  ( 12.10941530405103173, 10.98038939432486849, -3.892884064768170838 ) ) ;
#6664 = AXIS2_PLACEMENT_3D ( 'NONE', #59911, #38948, #53636 ) ;
#6665 = CARTESIAN_POINT ( 'NONE',  ( 11.12133729122639991, -4.865898216891100247, -7.477221318588949117 ) ) ;
#6666 = DIRECTION ( 'NONE',  ( -0.000000000000000000, -0.000000000000000000, 1.000000000000000000 ) ) ;
#6667 = ORIENTED_EDGE ( 'NONE', *, *, #61977, .F. ) ;
#6668 = CARTESIAN_POINT ( 'NONE',  ( 2.259112785886000285, 1.685541059001999908, -2.982097634516000184 ) ) ;
#6669 = CARTESIAN_POINT ( 'NONE',  ( 10.98768472567999943, 6.720753181080999283, 5.471698459870999898 ) ) ;
#6670 = CARTESIAN_POINT ( 'NONE',  ( 12.36003207187220809, -11.57530800953469630, 4.784147006776684918 ) ) ;
#6671 = CARTESIAN_POINT ( 'NONE',  ( 8.842468108405999061, 4.834201109053600121, 7.263744984161399465 ) ) ;
#6672 = CARTESIAN_POINT ( 'NONE',  ( 9.174642513462206495, -2.649442673322992103, 7.499981897072125925 ) ) ;
#6673 = CARTESIAN_POINT ( 'NONE',  ( 12.25852519399118634, -2.998253127629475046, 13.67519035003951267 ) ) ;
#6674 = FACE_OUTER_BOUND ( 'NONE', #43139, .T. ) ;
#6675 = FACE_OUTER_BOUND ( 'NONE', #57989, .T. ) ;
#6676 = CARTESIAN_POINT ( 'NONE',  ( 13.08701341325400236, -12.43401476831999908, -1.800486563913999971 ) ) ;
#6677 = ORIENTED_EDGE ( 'NONE', *, *, #61176, .T. ) ;
#6678 = CARTESIAN_POINT ( 'NONE',  ( 10.99999648468999958, -1.199999999999999956, -9.776630298829998011 ) ) ;
#6679 = CARTESIAN_POINT ( 'NONE',  ( 11.09999999999999964, -5.350000000000000533, 7.500000000000000000 ) ) ;
#6680 = DIRECTION ( 'NONE',  ( -1.000000000000000000, 0.000000000000000000, 0.000000000000000000 ) ) ;
#6681 = CARTESIAN_POINT ( 'NONE',  ( 1.037565185690999980, 3.729267013836000011, 0.4700476753697999666 ) ) ;
#6682 = CARTESIAN_POINT ( 'NONE',  ( 5.599965786763100084, 11.06886219213000011, 1.536526853569999851 ) ) ;
#6683 = CARTESIAN_POINT ( 'NONE',  ( 17.74851076052200938, 1.905606517475760597, -12.57039381402181633 ) ) ;
#6684 = CARTESIAN_POINT ( 'NONE',  ( 9.099999931440999390, -2.753634353389999845, -7.404749409716440134 ) ) ;
#6685 = CARTESIAN_POINT ( 'NONE',  ( 10.94903032197929882, 4.503839166471300004, 8.204588308639600314 ) ) ;
#6686 = EDGE_CURVE ( 'NONE', #37678, #62414, #9282, .T. ) ;
#6687 = EDGE_CURVE ( 'NONE', #41893, #52150, #1758, .T. ) ;
#6688 = DIRECTION ( 'NONE',  ( 0.000000000000000000, 0.000000000000000000, -1.000000000000000000 ) ) ;
#6689 = CARTESIAN_POINT ( 'NONE',  ( 10.58470685321000104, -2.966812129551000154, -8.831977776575000050 ) ) ;
#6690 = CARTESIAN_POINT ( 'NONE',  ( 12.80505043854143388, 1.787797342887042840, 13.88538010501570774 ) ) ;
#6691 = EDGE_CURVE ( 'NONE', #21149, #66718, #57185, .T. ) ;
#6692 = EDGE_CURVE ( 'NONE', #2379, #61768, #18488, .T. ) ;
#6693 = CARTESIAN_POINT ( 'NONE',  ( 24.40777907822999993, 12.23846661367000088, 3.187421709680999804 ) ) ;
#6694 = CARTESIAN_POINT ( 'NONE',  ( 9.398026887492090253, 5.281042804537088742, 7.060559036506083075 ) ) ;
#6695 = ORIENTED_EDGE ( 'NONE', *, *, #37469, .T. ) ;
#6696 = CARTESIAN_POINT ( 'NONE',  ( 9.491735841231999871, 3.920043641733999884, -9.398198753036000497 ) ) ;
#6697 = VERTEX_POINT ( 'NONE', #48329 ) ;
#6698 = CARTESIAN_POINT ( 'NONE',  ( 18.17999014114401035, -2.522019970189117277, 13.66878426939143587 ) ) ;
#6699 = CARTESIAN_POINT ( 'NONE',  ( 10.24733997687999931, -3.727636250918499705, -6.251346978035999591 ) ) ;
#6700 = ORIENTED_EDGE ( 'NONE', *, *, #27085, .F. ) ;
#6701 = CARTESIAN_POINT ( 'NONE',  ( 11.56833327354034857, 3.253412192327699959, 7.988332985010599963 ) ) ;
#6702 = CARTESIAN_POINT ( 'NONE',  ( 6.762481185574685583, -0.7530625793056462403, 0.8466959786579407732 ) ) ;
#6703 = CARTESIAN_POINT ( 'NONE',  ( 23.98815239557806223, 3.345691041822517864, -12.76938554867816400 ) ) ;
#6704 = DIRECTION ( 'NONE',  ( 0.000000000000000000, -1.000000000000000000, -0.000000000000000000 ) ) ;
#6705 = B_SPLINE_CURVE_WITH_KNOTS ( 'NONE', 3,
 ( #43927, #16308, #28189, #10715, #64534, #48821, #32062, #16651, #6507, #63851 ),
 .UNSPECIFIED., .F., .F.,
 ( 4, 2, 2, 2, 4 ),
 ( 0.000000000000000000, 0.2500000000000000000, 0.5000000000000000000, 0.7500000000000000000, 1.000000000000000000 ),
 .UNSPECIFIED. ) ;
#6706 = CARTESIAN_POINT ( 'NONE',  ( 9.099999999999999645, 0.000000000000000000, 0.000000000000000000 ) ) ;
#6707 = CARTESIAN_POINT ( 'NONE',  ( 11.09999999569000018, 9.179538081559000418, -6.556854281509999716 ) ) ;
#6708 = CARTESIAN_POINT ( 'NONE',  ( 17.82167905068868663, 0.6689867242971743178, -12.58222862546947418 ) ) ;
#6709 = CARTESIAN_POINT ( 'NONE',  ( 10.04002603384999937, -2.348908096685999869, -7.136751747961000092 ) ) ;
#6710 = CARTESIAN_POINT ( 'NONE',  ( 11.81056516821459823, -3.390321848206700128, -8.115298063151199059 ) ) ;
#6711 = ORIENTED_EDGE ( 'NONE', *, *, #979, .T. ) ;
#6712 = ORIENTED_EDGE ( 'NONE', *, *, #13587, .T. ) ;
#6713 = ADVANCED_FACE ( 'NONE', ( #5671 ), #27405, .F. ) ;
#6714 = VECTOR ( 'NONE', #12220, 1000.000000000000114 ) ;
#6715 = CARTESIAN_POINT ( 'NONE',  ( 0.7338048310729522461, 2.699466831487369323, -1.587941003800196871 ) ) ;
#6716 = ORIENTED_EDGE ( 'NONE', *, *, #43878, .T. ) ;
#6717 = CARTESIAN_POINT ( 'NONE',  ( 17.92302462176263944, -1.881539600472786677, -13.87303898716210426 ) ) ;
#6718 = CARTESIAN_POINT ( 'NONE',  ( 10.54675686666999823, -5.053011711995999633, 4.944839641817000420 ) ) ;
#6719 = CARTESIAN_POINT ( 'NONE',  ( 7.969305479088424349, 4.593434306755666441, -6.274929750779866033 ) ) ;
#6720 = CARTESIAN_POINT ( 'NONE',  ( 9.352250488097009651, 2.907725329094806188, 8.129544561320940943 ) ) ;
#6721 = CARTESIAN_POINT ( 'NONE',  ( 12.60257768741563567, 1.908613650260960526, 13.78119617999061397 ) ) ;
#6722 = CARTESIAN_POINT ( 'NONE',  ( 10.68361719090999884, -2.603550124652000086, 7.762065570229999878 ) ) ;
#6723 = CARTESIAN_POINT ( 'NONE',  ( 12.80505043854144276, 0.6249999999999994449, -12.67928921589118652 ) ) ;
#6724 = CARTESIAN_POINT ( 'NONE',  ( 12.18532581790793223, -0.08167545936615885904, 13.89968205666727386 ) ) ;
#6725 = ORIENTED_EDGE ( 'NONE', *, *, #28353, .T. ) ;
#6726 = CARTESIAN_POINT ( 'NONE',  ( 6.711228317543000088, 3.668692617901999853, -8.939602259005999585 ) ) ;
#6727 = CARTESIAN_POINT ( 'NONE',  ( 13.63328756540912323, -11.47070279790941072, -2.387969831734693127 ) ) ;
#6728 = CARTESIAN_POINT ( 'NONE',  ( 9.733483075504627990, 3.885520926571138567, 6.632574608010647133 ) ) ;
#6729 = CARTESIAN_POINT ( 'NONE',  ( 9.393930206848999376, 2.750000000000000000, 7.500000000000000000 ) ) ;
#6730 = CARTESIAN_POINT ( 'NONE',  ( 8.690229719593000723, 2.414630869937000046, -6.801495146585999407 ) ) ;
#6731 = EDGE_CURVE ( 'NONE', #62111, #57125, #47525, .T. ) ;
#6732 = LINE ( 'NONE', #39250, #5643 ) ;
#6733 = CARTESIAN_POINT ( 'NONE',  ( 10.23643195768000069, -5.517145045299000294, -6.754127937316000363 ) ) ;
#6734 = CARTESIAN_POINT ( 'NONE',  ( 5.399999746777999654, -12.99045401563999924, 1.690592933733000125 ) ) ;
#6735 = CARTESIAN_POINT ( 'NONE',  ( 23.85395620458804800, 3.593169595889099899, 13.20269660471672601 ) ) ;
#6736 = EDGE_CURVE ( 'NONE', #33656, #1808, #25210, .T. ) ;
#6737 = CARTESIAN_POINT ( 'NONE',  ( 10.90000000000000036, -2.899999999999999911, 6.414037451299000381 ) ) ;
#6738 = CARTESIAN_POINT ( 'NONE',  ( 17.65355681326706261, -3.248032782086183179, 13.61801318301550268 ) ) ;
#6739 = CARTESIAN_POINT ( 'NONE',  ( 21.70000039307920048, 13.99999960683000033, 1.736067127764999983E-09 ) ) ;
#6740 = CARTESIAN_POINT ( 'NONE',  ( 12.44006281456469232, 0.6285461057673268348, 12.58436427553280801 ) ) ;
#6741 = CARTESIAN_POINT ( 'NONE',  ( 10.69057802013490033, 2.966773425016000054, -7.475947032624040034 ) ) ;
#6742 = CARTESIAN_POINT ( 'NONE',  ( 9.761304848515999666, 4.913464051101100516, -7.917643062525700159 ) ) ;
#6744 = CARTESIAN_POINT ( 'NONE',  ( 10.10000000000000142, 0.000000000000000000, 0.000000000000000000 ) ) ;
#6743 = CARTESIAN_POINT ( 'NONE',  ( 10.30497570133299945, -3.363922674822000136, 6.910836541441499392 ) ) ;
#6745 = CARTESIAN_POINT ( 'NONE',  ( 6.999999085428001422, 12.01420426511556094, -3.456409902911533383 ) ) ;
#6746 = VERTEX_POINT ( 'NONE', #62268 ) ;
#6747 = AXIS2_PLACEMENT_3D ( 'NONE', #68158, #20623, #41947 ) ;
#6748 = CARTESIAN_POINT ( 'NONE',  ( 10.39969598649000027, 4.888000489779200208, 6.971269690999399415 ) ) ;
#6749 = CARTESIAN_POINT ( 'NONE',  ( 8.228217774218997249, -3.441349337319001389, 6.127431371819001882 ) ) ;
#6750 = CARTESIAN_POINT ( 'NONE',  ( 10.21426717315699939, 3.130949526459800403, 8.240598219300300897 ) ) ;
#6751 = CARTESIAN_POINT ( 'NONE',  ( 10.11342028323962694, 3.127145521393861038, -7.439524153027672781 ) ) ;
#6752 = CARTESIAN_POINT ( 'NONE',  ( 9.820206362952999868, -3.883324525498000224, 6.055606607331999847 ) ) ;
#6753 = CARTESIAN_POINT ( 'NONE',  ( 10.90227331380999942, -2.900050252960999941, -5.143660774000999858 ) ) ;
#6754 = LINE ( 'NONE', #28094, #20879 ) ;
#6755 = ORIENTED_EDGE ( 'NONE', *, *, #55489, .T. ) ;
#6756 = AXIS2_PLACEMENT_3D ( 'NONE', #22405, #43746, #38491 ) ;
#6757 = B_SPLINE_CURVE_WITH_KNOTS ( 'NONE', 3,
 ( #34314, #7384, #55637, #29077, #24157, #50388 ),
 .UNSPECIFIED., .F., .F.,
 ( 4, 1, 1, 4 ),
 ( 0.000000000000000000, 0.3333333333333000081, 0.6666666666667000474, 1.000000000000000000 ),
 .UNSPECIFIED. ) ;
#6758 = CARTESIAN_POINT ( 'NONE',  ( 10.06525461470299909, -4.973404788313100511, -7.747639695388999215 ) ) ;
#6759 = LINE ( 'NONE', #60600, #18728 ) ;
#6760 = CARTESIAN_POINT ( 'NONE',  ( 6.484746979524000032, 1.270915225504000157, -0.3650349355777000038 ) ) ;
#6761 = B_SPLINE_SURFACE_WITH_KNOTS ( 'NONE', 3, 3, ( 
 ( #64998, #700, #11871, #31574 ),
 ( #48598, #48944, #57786, #20733 ),
 ( #30887, #49279, #36123, #27617 ),
 ( #15146, #17113, #65355, #63366 ),
 ( #68614, #31237, #57438, #33211 ),
 ( #9542, #38447, #54530, #5933 ),
 ( #15494, #10239, #4641, #52200 ),
 ( #22706, #11520, #53836, #43702 ),
 ( #27275, #22013, #9898, #64661 ) ),
 .UNSPECIFIED., .F., .F., .F.,
 ( 4, 1, 1, 1, 1, 1, 4 ),
 ( 4, 4 ),
 ( 0.05214259105098999897, 0.1666666666667000196, 0.3333333333333000081, 0.5000000000000000000, 0.6666666666667000474, 0.8333333333333000637, 0.9777068595523999983 ),
 ( -0.1900882580235000174, 1.190231865545000156 ),
 .UNSPECIFIED. ) ;
#6762 = CARTESIAN_POINT ( 'NONE',  ( 10.58521345716900086, -3.075109701058799772, 6.659120737011199331 ) ) ;
#6763 = CARTESIAN_POINT ( 'NONE',  ( 11.49999672495000524, 11.64999999999999680, -1.217117305822887241 ) ) ;
#6764 = CARTESIAN_POINT ( 'NONE',  ( 12.64262999012820998, 0.6038699852804525481, -12.68066884516331783 ) ) ;
#6765 = CARTESIAN_POINT ( 'NONE',  ( 11.19102897915239936, 4.256858847510399890, -8.470038342183499935 ) ) ;
#6766 = CARTESIAN_POINT ( 'NONE',  ( 12.21880568482660934, 2.282463263829442646, -13.71720984526209364 ) ) ;
#6767 = FACE_OUTER_BOUND ( 'NONE', #68845, .T. ) ;
#6768 = CARTESIAN_POINT ( 'NONE',  ( 10.81746213571000048, 5.100000000000000533, 6.571291218949999902 ) ) ;
#6769 = ORIENTED_EDGE ( 'NONE', *, *, #64209, .T. ) ;
#6770 = CARTESIAN_POINT ( 'NONE',  ( 25.36445432553700030, -11.12586087667000001, -3.379826431974999768 ) ) ;
#6771 = ADVANCED_FACE ( 'NONE', ( #7756 ), #46424, .T. ) ;
#6772 = CARTESIAN_POINT ( 'NONE',  ( 12.42469545966024214, 0.4960449563116388627, -13.88808666890936827 ) ) ;
#6773 = EDGE_CURVE ( 'NONE', #6658, #24788, #34685, .T. ) ;
#6774 = CARTESIAN_POINT ( 'NONE',  ( 13.99947726215000188, -8.835099311859000437, -7.952110511812001015 ) ) ;
#6775 = CARTESIAN_POINT ( 'NONE',  ( 11.49200216175158396, 3.580169417146517485, -8.702070774814039567 ) ) ;
#6776 = CARTESIAN_POINT ( 'NONE',  ( 21.05000072320139992, -1.355183834107999921E-13, 1.088018564133000035E-14 ) ) ;
#6777 = CARTESIAN_POINT ( 'NONE',  ( 7.000000000000000000, 8.307879248642999315, 4.307879248643000203 ) ) ;
#6778 = CARTESIAN_POINT ( 'NONE',  ( 13.21722669115800031, 12.32379348829999977, 1.906876488274000137 ) ) ;
#6779 = EDGE_LOOP ( 'NONE', ( #43510, #1120, #19957, #16138, #65081 ) ) ;
#6780 = PRESENTATION_STYLE_ASSIGNMENT (( #33367 ) ) ;
#6781 = CARTESIAN_POINT ( 'NONE',  ( 18.02738429465118486, 2.090191673117355542, -13.75189211025434410 ) ) ;
#6782 = VERTEX_POINT ( 'NONE', #3872 ) ;
#6783 = CARTESIAN_POINT ( 'NONE',  ( 11.30000000000000071, 18.88101580703000337, 3.105963843451999828 ) ) ;
#6784 = CARTESIAN_POINT ( 'NONE',  ( 18.23980063339601898, 2.972525812591880534, 11.47315805767759578 ) ) ;
#6785 = CARTESIAN_POINT ( 'NONE',  ( 8.921614158776000281, 3.251172436837000301, -6.320036569851000152 ) ) ;
#6786 = CARTESIAN_POINT ( 'NONE',  ( -2.444943969992999916E-05, 2.899969545325999931, 0.000000000000000000 ) ) ;
#6787 = CARTESIAN_POINT ( 'NONE',  ( 17.77845184731630468, 1.823244735605227484, -13.88077056497939665 ) ) ;
#6788 = CARTESIAN_POINT ( 'NONE',  ( 17.86524243511767196, 0.5426972542083243756, -12.68439075057428944 ) ) ;
#6789 = CARTESIAN_POINT ( 'NONE',  ( 8.737764228571977654, 3.223862676119972903, -8.634700618639806535 ) ) ;
#6790 = VECTOR ( 'NONE', #67621, 1000.000000000000000 ) ;
#6791 = CARTESIAN_POINT ( 'NONE',  ( 10.96666666666865453, -4.766458981284529273, 8.714450223968791320 ) ) ;
#6792 = ORIENTED_EDGE ( 'NONE', *, *, #48925, .T. ) ;
#6793 = CARTESIAN_POINT ( 'NONE',  ( 9.509907746701999898, -5.077451867123000007, 8.469011304701000498 ) ) ;
#6794 = CARTESIAN_POINT ( 'NONE',  ( 17.98396147894309749, -2.954720660964888168, -13.56638041066537070 ) ) ;
#6795 = CARTESIAN_POINT ( 'NONE',  ( 11.25361999289386539, 3.455907502640804374, -6.342116603374310380 ) ) ;
#6796 = ORIENTED_EDGE ( 'NONE', *, *, #28498, .T. ) ;
#6797 = EDGE_CURVE ( 'NONE', #34183, #44937, #48439, .T. ) ;
#6798 = CARTESIAN_POINT ( 'NONE',  ( 10.61094409420999973, -5.100000000000000533, -6.571291218949999902 ) ) ;
#6799 = CARTESIAN_POINT ( 'NONE',  ( 2.750973465876000557, -3.500000000000000000, 0.000000000000000000 ) ) ;
#6800 = ORIENTED_EDGE ( 'NONE', *, *, #23622, .T. ) ;
#6801 = CARTESIAN_POINT ( 'NONE',  ( 10.11390035061499937, 4.304339077956200299, 6.399494776650000105 ) ) ;
#6802 = CARTESIAN_POINT ( 'NONE',  ( 18.26479085099342115, -2.332519703358805874, -12.38222476794584814 ) ) ;
#6803 = VECTOR ( 'NONE', #9467, 1000.000000000000114 ) ;
#6804 = CARTESIAN_POINT ( 'NONE',  ( 7.798175108423000879, 4.827257594231999960, -6.306127835448002372 ) ) ;
#6805 = CARTESIAN_POINT ( 'NONE',  ( 16.13837349797499954, 3.856691945087999951, 11.95672051617999898 ) ) ;
#6806 = DIRECTION ( 'NONE',  ( 0.000000000000000000, 1.000000000000000000, 0.000000000000000000 ) ) ;
#6807 = VECTOR ( 'NONE', #42522, 1000.000000000000000 ) ;
#6808 = CARTESIAN_POINT ( 'NONE',  ( 9.180747021775998107, 3.348327362764200288, 6.928134003122899287 ) ) ;
#6809 = CARTESIAN_POINT ( 'NONE',  ( 8.691343736187999269, 3.625767601089900261, -8.309341309902798400 ) ) ;
#6810 = B_SPLINE_CURVE_WITH_KNOTS ( 'NONE', 3,
 ( #5815, #20523, #31712, #47445 ),
 .UNSPECIFIED., .F., .F.,
 ( 4, 4 ),
 ( 0.000000000000000000, 0.5000023781865966521 ),
 .UNSPECIFIED. ) ;
#6811 = ORIENTED_EDGE ( 'NONE', *, *, #48044, .T. ) ;
#6812 = CARTESIAN_POINT ( 'NONE',  ( 10.85737917744000036, 2.754548910086000113, 8.976376585747001258 ) ) ;
#6813 = CARTESIAN_POINT ( 'NONE',  ( 10.96332971959000169, 5.283550306828000309, -8.592773337476000250 ) ) ;
#6814 = DIRECTION ( 'NONE',  ( 1.000000000000000000, 0.000000000000000000, 0.000000000000000000 ) ) ;
#6815 = CARTESIAN_POINT ( 'NONE',  ( 12.25820678327523616, 2.802802780256932191, -13.60456178155848050 ) ) ;
#6816 = CARTESIAN_POINT ( 'NONE',  ( 11.13559687351579974, -2.907767014557175678, 8.129523725463618788 ) ) ;
#6817 = B_SPLINE_CURVE_WITH_KNOTS ( 'NONE', 3,
 ( #16200, #48359, #465, #28080, #60929, #6740, #44858, #28785, #17592, #49394, #61274, #7787, #38917, #13391, #13041, #34371 ),
 .UNSPECIFIED., .F., .F.,
 ( 4, 2, 2, 2, 2, 2, 2, 4 ),
 ( 0.000000000000000000, 0.06249999999999897304, 0.1249999999999979461, 0.2499999999999980016, 0.4999999999999981126, 0.7499999999999982236, 0.8749999999999990008, 1.000000000000000000 ),
 .UNSPECIFIED. ) ;
#6818 = CARTESIAN_POINT ( 'NONE',  ( 24.69847935754600243, 3.637896099757999657, 12.18598438281999918 ) ) ;
#6819 = CARTESIAN_POINT ( 'NONE',  ( 17.75589283472434232, 0.5919407257947367773, 13.88303015925714590 ) ) ;
#6820 = CLOSED_SHELL ( 'NONE', ( #7260, #17489, #31796, #11532, #25813, #51411 ) ) ;
#6821 = CARTESIAN_POINT ( 'NONE',  ( 11.09999999999999964, 4.000000000000000000, -7.500000000000000000 ) ) ;
#6822 = B_SPLINE_CURVE_WITH_KNOTS ( 'NONE', 3,
 ( #26648, #42717, #64022, #22415, #48301, #5642, #37812, #32574, #16822, #48993, #53886, #27326, #38148, #1104 ),
 .UNSPECIFIED., .F., .F.,
 ( 4, 2, 2, 2, 2, 2, 4 ),
 ( 0.000000000000000000, 0.1249999999999998335, 0.2499999999999996669, 0.4999999999999993339, 0.6249999999999983347, 0.7499999999999972244, 1.000000000000000000 ),
 .UNSPECIFIED. ) ;
#6823 = ORIENTED_EDGE ( 'NONE', *, *, #46237, .F. ) ;
#6824 = VERTEX_POINT ( 'NONE', #56344 ) ;
#6825 = CARTESIAN_POINT ( 'NONE',  ( 8.500189158773000742, 2.724453559418999582, -8.908010318766001134 ) ) ;
#6826 = EDGE_CURVE ( 'NONE', #30666, #24248, #39278, .T. ) ;
#6827 = CARTESIAN_POINT ( 'NONE',  ( 12.18827041299910796, -0.1029057169788573228, 13.89950510286037044 ) ) ;
#6828 = CARTESIAN_POINT ( 'NONE',  ( 10.67349413291699811, -2.837298848764000514, 8.030511425625498134 ) ) ;
#6829 = CARTESIAN_POINT ( 'NONE',  ( 10.97865453029000093, -5.273142482194999481, 7.958032781726000593 ) ) ;
#6830 = CYLINDRICAL_SURFACE ( 'NONE', #1707, 1.500000000000000000 ) ;
#6831 = CARTESIAN_POINT ( 'NONE',  ( 8.026331853209001110, -5.601799093797000140, 7.176147756900999930 ) ) ;
#6832 = CARTESIAN_POINT ( 'NONE',  ( 6.999999691988000095, 13.87069231928999891, 4.225386915259999654 ) ) ;
#6834 = CARTESIAN_POINT ( 'NONE',  ( 11.02143415462000142, -6.120828910132000367, 5.114867263064000191 ) ) ;
#6833 = CARTESIAN_POINT ( 'NONE',  ( 10.00706361050499993, -3.475294527116599586, 6.333351572150998976 ) ) ;
#6835 = CARTESIAN_POINT ( 'NONE',  ( 9.105958040553998600, -5.104280076368001851, -6.665288755903000073 ) ) ;
#6836 = CARTESIAN_POINT ( 'NONE',  ( 12.09999999999999964, -4.198022108741683134, 6.428664210949555979 ) ) ;
#6837 = CARTESIAN_POINT ( 'NONE',  ( 24.53428993882599940, 8.855929947951999281, -9.286429770520999938 ) ) ;
#6838 = CARTESIAN_POINT ( 'NONE',  ( 18.00459872918310467, 0.4343244881883151498, 12.69000555157926868 ) ) ;
#6839 = CARTESIAN_POINT ( 'NONE',  ( 11.03776785110999903, -5.237767851104999650, 6.571291218949999902 ) ) ;
#6840 = CARTESIAN_POINT ( 'NONE',  ( 10.81905590578999998, -2.899999999999999911, -6.571291218949999902 ) ) ;
#6841 = ORIENTED_EDGE ( 'NONE', *, *, #62668, .T. ) ;
#6843 = CARTESIAN_POINT ( 'NONE',  ( 18.17745566903306198, 10.88889238843098362, -4.142628063308990249 ) ) ;
#6842 = CARTESIAN_POINT ( 'NONE',  ( 11.70158531382784517, -3.727547057523674212, 8.749999999999998224 ) ) ;
#6844 = CARTESIAN_POINT ( 'NONE',  ( 9.310554719594000161, 3.934138271021000222, -9.063586117809000697 ) ) ;
#6845 = FACE_OUTER_BOUND ( 'NONE', #36731, .T. ) ;
#6846 = CARTESIAN_POINT ( 'NONE',  ( 10.18576633586640767, -4.069734382926335492, -8.865705745738447163 ) ) ;
#6847 = CARTESIAN_POINT ( 'NONE',  ( 0.7901652630780000575, -0.8195100712853999880, -3.441407140921999730 ) ) ;
#6848 = CARTESIAN_POINT ( 'NONE',  ( 9.299999999999998934, 4.537600397704999899, 9.154563893594000135 ) ) ;
#6849 = CARTESIAN_POINT ( 'NONE',  ( 2.256745668234000135, 2.821651784608999680, 1.942419289100000057 ) ) ;
#6850 = ORIENTED_EDGE ( 'NONE', *, *, #67342, .T. ) ;
#6851 = CARTESIAN_POINT ( 'NONE',  ( 12.14435919815817932, 0.2964030593063847197, -12.59651778044212556 ) ) ;
#6852 = CARTESIAN_POINT ( 'NONE',  ( 9.565773468336619345, -5.100000000000000533, 6.304440313901286785 ) ) ;
#6853 = CARTESIAN_POINT ( 'NONE',  ( 24.14647106071498683, -12.47146082256108457, -3.359356504527230225 ) ) ;
#6854 = CARTESIAN_POINT ( 'NONE',  ( 8.154704719592000828, 4.255646040929000229, 9.114085578076998928 ) ) ;
#6855 = ORIENTED_EDGE ( 'NONE', *, *, #52410, .T. ) ;
#6856 = CARTESIAN_POINT ( 'NONE',  ( 6.760161299141000057, 1.377540824270000019, 0.5088348457508999889 ) ) ;
#6857 = EDGE_CURVE ( 'NONE', #23757, #51247, #41293, .T. ) ;
#6858 = EDGE_CURVE ( 'NONE', #10241, #35517, #7579, .T. ) ;
#6859 = CARTESIAN_POINT ( 'NONE',  ( 7.590035841228000457, 5.397217548590999669, -7.528974776547999959 ) ) ;
#6861 = CARTESIAN_POINT ( 'NONE',  ( -0.2999999999999999889, 0.000000000000000000, 0.000000000000000000 ) ) ;
#6860 = DIRECTION ( 'NONE',  ( -1.000000000000000000, 0.000000000000000000, 0.000000000000000000 ) ) ;
#6862 = CARTESIAN_POINT ( 'NONE',  ( 6.999998782146999332, 11.95749337870000062, 3.642574926947999892 ) ) ;
#6863 = VERTEX_POINT ( 'NONE', #29794 ) ;
#6864 = DIRECTION ( 'NONE',  ( 0.000000000000000000, 0.4812255921203881792, -0.8765967884314782577 ) ) ;
#6865 = SURFACE_SIDE_STYLE ('',( #65246 ) ) ;
#6866 = ORIENTED_EDGE ( 'NONE', *, *, #24021, .T. ) ;
#6867 = CARTESIAN_POINT ( 'NONE',  ( 9.498146308785210934, -4.816854805705224507, 8.576504408122966439 ) ) ;
#6868 = CARTESIAN_POINT ( 'NONE',  ( 16.29314246895800267, 3.193172571147000038, 11.44978050968999916 ) ) ;
#6869 = TOROIDAL_SURFACE ( 'NONE', #11357, 12.35000000006999876, 0.5000000000000000000 ) ;
#6870 = CARTESIAN_POINT ( 'NONE',  ( 18.08578335600534359, -0.3302328523437055852, -13.89472426752320899 ) ) ;
#6871 = ORIENTED_EDGE ( 'NONE', *, *, #56040, .F. ) ;
#6872 = FACE_OUTER_BOUND ( 'NONE', #9623, .T. ) ;
#6873 = CARTESIAN_POINT ( 'NONE',  ( 25.60000000000000142, -2.023988666086999899, -11.01546541709000060 ) ) ;
#6874 = CARTESIAN_POINT ( 'NONE',  ( 10.37199293566600034, 4.633387186021100668, -8.276990458557699881 ) ) ;
#6875 = CARTESIAN_POINT ( 'NONE',  ( 11.58810207955109917, 3.203462856645999945, -7.174999999999999822 ) ) ;
#6876 = LINE ( 'NONE', #39051, #29603 ) ;
#6877 = EDGE_LOOP ( 'NONE', ( #17403, #38876, #33635, #13754 ) ) ;
#6878 = DIRECTION ( 'NONE',  ( -1.000000000000000000, 0.000000000000000000, 0.000000000000000000 ) ) ;
#6879 = CARTESIAN_POINT ( 'NONE',  ( 12.27415370856040511, -2.829964016113827530, -13.59786649615824672 ) ) ;
#6880 = EDGE_CURVE ( 'NONE', #44713, #11166, #24526, .T. ) ;
#6881 = CARTESIAN_POINT ( 'NONE',  ( 9.310585478579783469, -4.629544268302964838, -6.407725666907082562 ) ) ;
#6882 = CARTESIAN_POINT ( 'NONE',  ( 15.83019412026500206, -8.948785863751000491, -8.423203147821000769 ) ) ;
#6883 = ORIENTED_EDGE ( 'NONE', *, *, #267, .F. ) ;
#6884 = CARTESIAN_POINT ( 'NONE',  ( 10.62947109217999930, -5.100000000000000533, 6.152188490330000370 ) ) ;
#6885 = EDGE_CURVE ( 'NONE', #2551, #30098, #14041, .T. ) ;
#6886 = CARTESIAN_POINT ( 'NONE',  ( 1.700000000000000178, 0.000000000000000000, 0.000000000000000000 ) ) ;
#6887 = DIRECTION ( 'NONE',  ( 0.000000000000000000, 0.7198977633594747516, 0.6940801180771756229 ) ) ;
#6888 = CARTESIAN_POINT ( 'NONE',  ( 5.000030787343000327, 2.099962892530999881, 0.000000000000000000 ) ) ;
#6889 = CARTESIAN_POINT ( 'NONE',  ( 11.49978667957999967, -12.49365449110754867, -1.022561121909996817 ) ) ;
#6890 = CARTESIAN_POINT ( 'NONE',  ( 11.45764291764649911, -5.132124077409000229, -7.360052904210999891 ) ) ;
#6891 = DIRECTION ( 'NONE',  ( 0.000000000000000000, -1.000000000000000000, 0.000000000000000000 ) ) ;
#6892 = CARTESIAN_POINT ( 'NONE',  ( 17.65791272883258500, -3.116819718221111035, 12.28623542600055352 ) ) ;
#6893 = ORIENTED_EDGE ( 'NONE', *, *, #14074, .T. ) ;
#6894 = DIRECTION ( 'NONE',  ( 0.000000000000000000, 0.000000000000000000, -1.000000000000000000 ) ) ;
#6895 = ORIENTED_EDGE ( 'NONE', *, *, #53701, .F. ) ;
#6896 = DIRECTION ( 'NONE',  ( 0.000000000000000000, 1.000000000000000000, 0.000000000000000000 ) ) ;
#6897 = CARTESIAN_POINT ( 'NONE',  ( 9.263353253171903390, -4.132446745988497483, 6.586646690369097890 ) ) ;
#6898 = AXIS2_PLACEMENT_3D ( 'NONE', #33009, #22164, #26391 ) ;
#6899 = CARTESIAN_POINT ( 'NONE',  ( 2.873654761058999973, 0.1588290254405000101, 3.211125886561999820 ) ) ;
#6900 = CARTESIAN_POINT ( 'NONE',  ( 9.780291077142999612, -3.021588645102999848, -8.450043670922001482 ) ) ;
#6901 = CARTESIAN_POINT ( 'NONE',  ( 10.81905590578999998, 2.899999999999999911, -6.571291218949999902 ) ) ;
#6902 = CARTESIAN_POINT ( 'NONE',  ( 27.25811388278000180, 0.000000000000000000, 0.000000000000000000 ) ) ;
#6903 = CARTESIAN_POINT ( 'NONE',  ( 9.099999999999999645, 0.000000000000000000, 11.84999999999999964 ) ) ;
#6904 = B_SPLINE_CURVE_WITH_KNOTS ( 'NONE', 3,
 ( #52195, #36460, #68261, #29867, #19350, #40672, #57779, #14116 ),
 .UNSPECIFIED., .F., .F.,
 ( 4, 2, 2, 4 ),
 ( 0.000000000000000000, 0.5000000000000005551, 0.7500000000000002220, 1.000000000000000000 ),
 .UNSPECIFIED. ) ;
#6905 = ORIENTED_EDGE ( 'NONE', *, *, #68635, .F. ) ;
#6906 = CARTESIAN_POINT ( 'NONE',  ( 18.53959992722300143, 2.682146997965999979, 11.29770844980000000 ) ) ;
#6907 = CARTESIAN_POINT ( 'NONE',  ( 11.54333729122640051, -5.003122373830000136, 7.526388557597149642 ) ) ;
#6908 = CARTESIAN_POINT ( 'NONE',  ( 11.20904666305999875, 5.937823941418000295, 7.147334722859000067 ) ) ;
#6909 = CARTESIAN_POINT ( 'NONE',  ( 19.99999987597299977, 0.000000000000000000, 5.040412531797999279E-14 ) ) ;
#6910 = CARTESIAN_POINT ( 'NONE',  ( 9.140753410162000492, -5.100000000000000533, 6.175944241622000064 ) ) ;
#6911 = CARTESIAN_POINT ( 'NONE',  ( 9.192115766384521436, 2.763712191446816568, 8.049223208410250407 ) ) ;
#6912 = CIRCLE ( 'NONE', #62747, 1.449999999999999956 ) ;
#6913 = CARTESIAN_POINT ( 'NONE',  ( 11.48641235500450009, 3.260080192309100067, -6.822158181405299615 ) ) ;
#6914 = CARTESIAN_POINT ( 'NONE',  ( 10.50477421009230738, 2.640760156097457401, 6.397741617862033436 ) ) ;
#6915 = CIRCLE ( 'NONE', #52735, 2.400000066501999818 ) ;
#6916 = EDGE_CURVE ( 'NONE', #43113, #45838, #52813, .T. ) ;
#6917 = CARTESIAN_POINT ( 'NONE',  ( 9.505051052051998184, 5.120555153167999585, -7.719295683256799379 ) ) ;
#6918 = CARTESIAN_POINT ( 'NONE',  ( 24.45387054266700133, -8.897469717442998416, -9.225144726131999207 ) ) ;
#6919 = CARTESIAN_POINT ( 'NONE',  ( 23.68233444796700127, -9.990153342492000377, 9.401313137095000272 ) ) ;
#6920 = DIRECTION ( 'NONE',  ( 1.000000000000000000, 0.000000000000000000, 0.000000000000000000 ) ) ;
#6921 = ORIENTED_EDGE ( 'NONE', *, *, #15801, .F. ) ;
#6922 = CARTESIAN_POINT ( 'NONE',  ( 8.528441940379998698, -2.472358291268000219, 6.234202627038999189 ) ) ;
#6923 = CARTESIAN_POINT ( 'NONE',  ( 9.795737326637999232, -4.289037785427000316, -5.816478295321999781 ) ) ;
#6924 = CARTESIAN_POINT ( 'NONE',  ( 18.11732105061182452, 2.226901518982099759, 13.72755281718821507 ) ) ;
#6925 = CARTESIAN_POINT ( 'NONE',  ( 23.59999196693599899, 2.915561532799999966, -13.58550759281999909 ) ) ;
#6926 = CARTESIAN_POINT ( 'NONE',  ( 10.88733729122639993, -5.277570687708000641, -7.466391690027689876 ) ) ;
#6927 = VERTEX_POINT ( 'NONE', #9812 ) ;
#6928 = CARTESIAN_POINT ( 'NONE',  ( 25.09299537199500207, 3.211994377626000041, -11.60337666361999887 ) ) ;
#6929 = CARTESIAN_POINT ( 'NONE',  ( 7.962142219590999659, 4.874567052833000069, 6.119507471270999588 ) ) ;
#6931 = CARTESIAN_POINT ( 'NONE',  ( 11.34523293495530005, 2.684794526488000432, 7.552870914315270134 ) ) ;
#6930 = CARTESIAN_POINT ( 'NONE',  ( 9.243110841233001196, 4.112741311853999271, -5.603466076760000192 ) ) ;
#6932 = CARTESIAN_POINT ( 'NONE',  ( 6.799999999999999822, -9.295462635088998837, -5.399710584805999858 ) ) ;
#6933 = VERTEX_POINT ( 'NONE', #5590 ) ;
#6934 = CARTESIAN_POINT ( 'NONE',  ( 17.55505043854143565, 1.875000000000000000, -25.00000000000000000 ) ) ;
#6935 = CARTESIAN_POINT ( 'NONE',  ( 17.92097207270829173, -1.887179018856798507, -13.87222722961340793 ) ) ;
#6936 = CARTESIAN_POINT ( 'NONE',  ( 11.70794988689359961, 4.455786710255300598, 6.606015074393400077 ) ) ;
#6937 = CARTESIAN_POINT ( 'NONE',  ( 10.30047649312000146, -4.027768368024999823, 9.431342508940000258 ) ) ;
#6938 = CARTESIAN_POINT ( 'NONE',  ( 8.256683059623998844, -2.876278577719999952, 6.568889245344999850 ) ) ;
#6939 = ORIENTED_EDGE ( 'NONE', *, *, #5266, .F. ) ;
#6940 = CARTESIAN_POINT ( 'NONE',  ( 24.53429014209899961, 12.47024915613999951, 3.026245713505000268 ) ) ;
#6941 = EDGE_CURVE ( 'NONE', #15478, #115, #10498, .T. ) ;
#6943 = EDGE_CURVE ( 'NONE', #11525, #61746, #66019, .T. ) ;
#6942 = B_SPLINE_CURVE_WITH_KNOTS ( 'NONE', 3,
 ( #14876, #25707, #24684, #41788, #9619, #47038 ),
 .UNSPECIFIED., .F., .F.,
 ( 4, 2, 4 ),
 ( 0.000000000000000000, 0.5000000000000005551, 1.000000000000000000 ),
 .UNSPECIFIED. ) ;
#6945 = CARTESIAN_POINT ( 'NONE',  ( 10.54684435321000002, -3.691674321452999674, -9.157280075569998345 ) ) ;
#6944 = CARTESIAN_POINT ( 'NONE',  ( 12.24011731813700088, -12.12177778538999995, 3.303327906654999868 ) ) ;
#6946 = CARTESIAN_POINT ( 'NONE',  ( 8.079085852406842960, -4.100770249492976305, 5.760890686963834106 ) ) ;
#6947 = CARTESIAN_POINT ( 'NONE',  ( 9.504901164121001500, -3.934733502342999678, 5.704835336325999151 ) ) ;
#6948 = CARTESIAN_POINT ( 'NONE',  ( 23.55757892560500011, 3.265738280757000123, 13.70122728612999907 ) ) ;
#6949 = CARTESIAN_POINT ( 'NONE',  ( 9.450772138681999834, -4.373757805842100055, 8.432280753260499750 ) ) ;
#6950 = ORIENTED_EDGE ( 'NONE', *, *, #26456, .T. ) ;
#6952 = CARTESIAN_POINT ( 'NONE',  ( 24.26287124489074998, -8.985590579641673514, 8.985591852965418624 ) ) ;
#6951 = CONICAL_SURFACE ( 'NONE', #32651, 13.94232983116000035, 1.233427434088588903 ) ;
#6953 = EDGE_CURVE ( 'NONE', #1839, #15133, #25161, .T. ) ;
#6954 = CARTESIAN_POINT ( 'NONE',  ( 11.53502897915239878, -3.672866099873000056, 6.264564938179000286 ) ) ;
#6955 = VERTEX_POINT ( 'NONE', #12577 ) ;
#6956 = CARTESIAN_POINT ( 'NONE',  ( 7.544198296194000619, 2.929983868333001951, 6.556648683638004016 ) ) ;
#6957 = EDGE_LOOP ( 'NONE', ( #20963, #52770, #12328, #63020, #61505, #20280 ) ) ;
#6958 = B_SPLINE_CURVE_WITH_KNOTS ( 'NONE', 3,
 ( #39412, #61761, #13879, #56521 ),
 .UNSPECIFIED., .F., .F.,
 ( 4, 4 ),
 ( 0.000000000000000000, 1.000000000000000000 ),
 .UNSPECIFIED. ) ;
#6959 = CARTESIAN_POINT ( 'NONE',  ( 9.749220280410998640, 5.656948148960999845, -6.994239053114000626 ) ) ;
#6960 = CARTESIAN_POINT ( 'NONE',  ( 23.91260600754999999, 12.75253188547999983, -3.592041058436000078 ) ) ;
#6961 = CARTESIAN_POINT ( 'NONE',  ( 12.37983597880427133, 3.063558859249376987, -12.22189795429199144 ) ) ;
#6962 = CARTESIAN_POINT ( 'NONE',  ( 11.89700581613019992, -3.130347327833300053, 6.941573685175900010 ) ) ;
#6963 = EDGE_LOOP ( 'NONE', ( #20810, #7046, #27523, #12854 ) ) ;
#6964 = CARTESIAN_POINT ( 'NONE',  ( 9.273175939532153578, 2.820663304098465218, -8.179560065238094424 ) ) ;
#6965 = VECTOR ( 'NONE', #12371, 1000.000000000000000 ) ;
#6966 = ORIENTED_EDGE ( 'NONE', *, *, #64769, .F. ) ;
#6967 = CARTESIAN_POINT ( 'NONE',  ( 9.558834163536230832, 4.704973616088495625, 8.704082162066606898 ) ) ;
#6968 = CARTESIAN_POINT ( 'NONE',  ( 23.74397628692652518, 9.837201187003470793, 9.448856396694791826 ) ) ;
#6969 = ORIENTED_EDGE ( 'NONE', *, *, #59509, .F. ) ;
#6970 = CARTESIAN_POINT ( 'NONE',  ( 12.47126843887709846, -3.119056300612248034, -12.20784669583220072 ) ) ;
#6971 = ADVANCED_FACE ( 'NONE', ( #38802 ), #1736, .T. ) ;
#6972 = CARTESIAN_POINT ( 'NONE',  ( 11.26072066707849828, 4.976067344118500380, 8.090408888831799317 ) ) ;
#6973 = CIRCLE ( 'NONE', #63901, 12.42499880353999941 ) ;
#6974 = CARTESIAN_POINT ( 'NONE',  ( 10.07763305961999833, -2.169024213715999849, -7.244986319234999250 ) ) ;
#6975 = CARTESIAN_POINT ( 'NONE',  ( 10.20918109782000016, 3.334760637131999772, -5.769467581755999497 ) ) ;
#6976 = CARTESIAN_POINT ( 'NONE',  ( 8.518405616243800438, 5.127171463238822113, -6.752698291457244650 ) ) ;
#6977 = CARTESIAN_POINT ( 'NONE',  ( 8.733215486276282746, 4.027942412209718270, 6.616784466747247073 ) ) ;
#6978 = CARTESIAN_POINT ( 'NONE',  ( 12.43888651633847608, -3.006915248264998564, -13.55273156457844230 ) ) ;
#6979 = B_SPLINE_CURVE_WITH_KNOTS ( 'NONE', 3,
 ( #55783, #27485, #17692, #7195 ),
 .UNSPECIFIED., .F., .F.,
 ( 4, 4 ),
 ( 0.000000000000000000, 0.1324350869623206473 ),
 .UNSPECIFIED. ) ;
#6980 = CARTESIAN_POINT ( 'NONE',  ( 17.99001832964330561, -0.4489258298041840511, -12.68932177688765428 ) ) ;
#6981 = CARTESIAN_POINT ( 'NONE',  ( 12.20035750765601179, 2.340667166415539402, -12.48730567878040176 ) ) ;
#6982 = CARTESIAN_POINT ( 'NONE',  ( 11.28533594839949750, -3.249987070165300196, -6.640482273977399430 ) ) ;
#6983 = CARTESIAN_POINT ( 'NONE',  ( 8.829017219593000121, 5.290207928847999064, 8.768105151414001597 ) ) ;
#6984 = EDGE_LOOP ( 'NONE', ( #7840, #18310, #14962, #25943, #55344, #29450 ) ) ;
#6985 = CARTESIAN_POINT ( 'NONE',  ( -15.86200481174999943, -2.399999999999999911, 6.571291218949999902 ) ) ;
#6986 = CARTESIAN_POINT ( 'NONE',  ( 7.350689587839424277, 3.996361938020618343, 6.125274922243029607 ) ) ;
#6987 = FACE_OUTER_BOUND ( 'NONE', #1290, .T. ) ;
#6988 = CARTESIAN_POINT ( 'NONE',  ( 23.64843185931299985, -3.331590877846000165, 13.50015817444000099 ) ) ;
#6989 = CARTESIAN_POINT ( 'NONE',  ( 17.60340893540758600, 3.198498114537103199, 12.18727270072288604 ) ) ;
#6990 = CARTESIAN_POINT ( 'NONE',  ( 18.44717847589300064, 2.901259342162000543, -12.12894967335999930 ) ) ;
#6991 = CARTESIAN_POINT ( 'NONE',  ( 10.65050915380999896, 5.200037120669999346, 5.937706951697999891 ) ) ;
#6992 = CARTESIAN_POINT ( 'NONE',  ( 9.929533309317628564, -3.366787958683358006, 8.103800281262431682 ) ) ;
#6993 = DIRECTION ( 'NONE',  ( 0.000000000000000000, 0.9421243786071880066, 0.3352635608502960163 ) ) ;
#6994 = ORIENTED_EDGE ( 'NONE', *, *, #13551, .T. ) ;
#6995 = CARTESIAN_POINT ( 'NONE',  ( 12.29866314003343319, -2.995318252715390095, 12.23879431495722336 ) ) ;
#6996 = CARTESIAN_POINT ( 'NONE',  ( 10.38955864497999926, -3.209241371122599773, -8.119307134446700047 ) ) ;
#6997 = CARTESIAN_POINT ( 'NONE',  ( 24.66271477989500127, -3.625397779087000227, -12.20587930303000057 ) ) ;
#6998 = CARTESIAN_POINT ( 'NONE',  ( 5.599999772733800008, -6.661338147750999827E-14, -1.931788062847999572E-14 ) ) ;
#6999 = VECTOR ( 'NONE', #38668, 1000.000000000000000 ) ;
#7000 = CARTESIAN_POINT ( 'NONE',  ( 10.89564560330029863, 4.307504762655200103, -6.544808043482999160 ) ) ;
#7001 = VERTEX_POINT ( 'NONE', #33907 ) ;
#7002 = CARTESIAN_POINT ( 'NONE',  ( 12.44180168752029481, -0.6226057762474820345, 12.58460959628226483 ) ) ;
#7003 = EDGE_CURVE ( 'NONE', #19885, #44936, #16722, .T. ) ;
#7004 = EDGE_CURVE ( 'NONE', #62483, #61390, #703, .T. ) ;
#7005 = CARTESIAN_POINT ( 'NONE',  ( 8.239948341229000661, 2.735218126362000124, 6.771983639047999937 ) ) ;
#7006 = CARTESIAN_POINT ( 'NONE',  ( 10.34021053755999908, 4.202028620710000162, 9.459600235481000041 ) ) ;
#7007 = CARTESIAN_POINT ( 'NONE',  ( 12.29593341745174584, 2.863102696958911508, 12.35953065740858570 ) ) ;
#7008 = ORIENTED_EDGE ( 'NONE', *, *, #42532, .F. ) ;
#7009 = CARTESIAN_POINT ( 'NONE',  ( 9.444964158775000840, 3.920043641733999884, -9.398198753036000497 ) ) ;
#7010 = CARTESIAN_POINT ( 'NONE',  ( 11.42887348028849992, 2.875789035466000065, -8.107837221875000111 ) ) ;
#7011 = CARTESIAN_POINT ( 'NONE',  ( 11.30671024775549505, 4.620655945117460028, 6.880623181275071332 ) ) ;
#7013 = CARTESIAN_POINT ( 'NONE',  ( 18.04535692654280155, -0.3877536850946274871, 12.69203640188686144 ) ) ;
#7012 = CARTESIAN_POINT ( 'NONE',  ( 8.335548698406999080, 5.102342278510997531, 6.653323484791000553 ) ) ;
#7014 = CARTESIAN_POINT ( 'NONE',  ( 9.224822372493999723, -4.249211653873900651, 6.684745346084599582 ) ) ;
#7015 = CARTESIAN_POINT ( 'NONE',  ( 10.72749279009019929, -4.225282629687599822, -8.336388861178200216 ) ) ;
#7016 = CARTESIAN_POINT ( 'NONE',  ( 13.00000000001300116, 11.52577654661000039, 1.696746661728000038 ) ) ;
#7017 = EDGE_LOOP ( 'NONE', ( #8355, #26327, #34770, #7723 ) ) ;
#7018 = CONICAL_SURFACE ( 'NONE', #2573, 12.44999944941000081, 0.7853981146832407223 ) ;
#7019 = CARTESIAN_POINT ( 'NONE',  ( 1.400837695952000139, 2.565043520226999885, 2.270544068615000022 ) ) ;
#7020 = CARTESIAN_POINT ( 'NONE',  ( 24.11583679491036136, -9.189166502811682236, -9.154374719221291201 ) ) ;
#7021 = CARTESIAN_POINT ( 'NONE',  ( 9.337278925393347251, -3.116678102649798277, 8.012901425336814043 ) ) ;
#7022 = CARTESIAN_POINT ( 'NONE',  ( 8.724265421554999733, 3.837285628664199866, 6.658304367510099908 ) ) ;
#7023 = CARTESIAN_POINT ( 'NONE',  ( 10.51293113580700123, 5.100000000000000533, 6.444141223116233164 ) ) ;
#7024 = CARTESIAN_POINT ( 'NONE',  ( 12.29779067500862944, -1.996199619003550918, 13.85695719179636853 ) ) ;
#7025 = CARTESIAN_POINT ( 'NONE',  ( 11.30000000000000071, 12.07633927192662782, 1.479860929215916832 ) ) ;
#7026 = CARTESIAN_POINT ( 'NONE',  ( 23.99067072799600098, 3.573053042975999904, -12.95875606115999901 ) ) ;
#7027 = CARTESIAN_POINT ( 'NONE',  ( 12.96385332268500079, -12.32790784140999918, -1.878650414825000059 ) ) ;
#7028 = VERTEX_POINT ( 'NONE', #11186 ) ;
#7029 = CARTESIAN_POINT ( 'NONE',  ( 7.406666666664500021, 2.820388375721751384, -6.820114376499287978 ) ) ;
#7030 = CARTESIAN_POINT ( 'NONE',  ( 4.999999999844999543, 0.04999999984535999364, 9.776630291645998838 ) ) ;
#7031 = CARTESIAN_POINT ( 'NONE',  ( 8.975133055567869889, 5.349981391149201571, 7.499992565666659949 ) ) ;
#7032 = CARTESIAN_POINT ( 'NONE',  ( 9.716851002543000604, 2.832432432432000269, 6.822293592207000934 ) ) ;
#7033 = DIRECTION ( 'NONE',  ( 0.000000000000000000, -1.000000000000000000, 0.000000000000000000 ) ) ;
#7034 = VERTEX_POINT ( 'NONE', #55224 ) ;
#7035 = CARTESIAN_POINT ( 'NONE',  ( 16.00000000028333602, 12.11987147417543298, -3.159800697744812314 ) ) ;
#7036 = EDGE_CURVE ( 'NONE', #63565, #47991, #7324, .T. ) ;
#7037 = MANIFOLD_SOLID_BREP ( 'Stock-MAS-678-1', #49290 ) ;
#7038 = DIRECTION ( 'NONE',  ( 0.000000000000000000, 1.000000000000000000, 0.000000000000000000 ) ) ;
#7039 = CARTESIAN_POINT ( 'NONE',  ( 9.685590450029499365, -2.907727159402498707, 8.129537449122588910 ) ) ;
#7040 = CARTESIAN_POINT ( 'NONE',  ( 10.70287750876920008, 3.530799696887600092, 6.771886227364699806 ) ) ;
#7041 = DIRECTION ( 'NONE',  ( 1.000000000000000000, 0.000000000000000000, 0.000000000000000000 ) ) ;
#7042 = CARTESIAN_POINT ( 'NONE',  ( 10.20608185320999972, -2.622355301673999772, -6.528538675937999969 ) ) ;
#7043 = CARTESIAN_POINT ( 'NONE',  ( 18.00086112087954149, 0.5837697426924873811, -13.98798827748158580 ) ) ;
#7044 = CARTESIAN_POINT ( 'NONE',  ( 12.65361177982750185, -10.78680294142912643, 4.401676341558338201 ) ) ;
#7045 = CARTESIAN_POINT ( 'NONE',  ( 12.34817707648056917, -2.926896462556495493, 12.34181790735160256 ) ) ;
#7046 = ORIENTED_EDGE ( 'NONE', *, *, #53436, .F. ) ;
#7047 = CARTESIAN_POINT ( 'NONE',  ( 9.143660841233000269, 2.235961884443999459, -6.794506518623999902 ) ) ;
#7048 = ORIENTED_EDGE ( 'NONE', *, *, #33791, .F. ) ;
#7049 = CONICAL_SURFACE ( 'NONE', #58399, 8.515178490300000291, 1.329165865441747751 ) ;
#7050 = CARTESIAN_POINT ( 'NONE',  ( 17.96876343269825327, -2.968584057511098440, 13.56283743052909152 ) ) ;
#7051 = CARTESIAN_POINT ( 'NONE',  ( 7.744301850232000461, 3.130385018321999890, 6.467396599055999395 ) ) ;
#7052 = ORIENTED_EDGE ( 'NONE', *, *, #65670, .T. ) ;
#7053 = CARTESIAN_POINT ( 'NONE',  ( 11.23589666366019912, 3.960399224793059947, 6.608753462694600067 ) ) ;
#7054 = CARTESIAN_POINT ( 'NONE',  ( 6.746322592394366602, -0.5615255549191391360, 0.9835864943946899253 ) ) ;
#7055 = ADVANCED_FACE ( 'NONE', ( #13620 ), #11874, .F. ) ;
#7056 = CARTESIAN_POINT ( 'NONE',  ( 9.709204462304001026, -2.899999999999999911, 6.662590550603789019 ) ) ;
#7057 = CARTESIAN_POINT ( 'NONE',  ( 9.657553581808000942, 5.333455947841000189, 6.049916795084000043 ) ) ;
#7058 = DIRECTION ( 'NONE',  ( 0.000000000000000000, 1.000000000000000000, 0.000000000000000000 ) ) ;
#7059 = CARTESIAN_POINT ( 'NONE',  ( 10.85226354018316108, -5.092232985442820770, 8.129523725463624118 ) ) ;
#7060 = FACE_OUTER_BOUND ( 'NONE', #67336, .T. ) ;
#7061 = CARTESIAN_POINT ( 'NONE',  ( 11.02205565301999890, -2.309485172892000282, -7.515673712097999726 ) ) ;
#7062 = CARTESIAN_POINT ( 'NONE',  ( 25.30000327618300204, -8.756202924575998026, -7.455126447192999883 ) ) ;
#7063 = EDGE_LOOP ( 'NONE', ( #28202, #63086, #35856, #21103 ) ) ;
#7064 = CARTESIAN_POINT ( 'NONE',  ( 8.956149159797568871, 2.922971693198220144, -7.209669135134798346 ) ) ;
#7065 = VERTEX_POINT ( 'NONE', #40186 ) ;
#7066 = CARTESIAN_POINT ( 'NONE',  ( 17.74422827376958267, -3.224484589758234598, -13.62361160044833674 ) ) ;
#7067 = CARTESIAN_POINT ( 'NONE',  ( 10.41599088719999955, -4.897727109276999613, 5.040303808578999956 ) ) ;
#7068 = AXIS2_PLACEMENT_3D ( 'NONE', #30556, #41729, #63034 ) ;
#7069 = CARTESIAN_POINT ( 'NONE',  ( 10.27427173964635898, -3.287502775498966301, 4.944156915057607016 ) ) ;
#7070 = CARTESIAN_POINT ( 'NONE',  ( 10.29226717315700057, 3.026371913119300316, -6.670281532133299329 ) ) ;
#7071 = CARTESIAN_POINT ( 'NONE',  ( 12.19342855462627817, 2.370970601743435324, 13.69993124892199532 ) ) ;
#7072 = CARTESIAN_POINT ( 'NONE',  ( 10.14750362918999826, -2.602959084636999876, 6.738575912023000214 ) ) ;
#7073 = ORIENTED_EDGE ( 'NONE', *, *, #13683, .T. ) ;
#7074 = DIRECTION ( 'NONE',  ( -1.000000000000000000, 0.000000000000000000, 0.000000000000000000 ) ) ;
#7075 = CARTESIAN_POINT ( 'NONE',  ( 12.70318375531252286, -0.6169787192598757963, 13.88156336867697149 ) ) ;
#7076 = VERTEX_POINT ( 'NONE', #45088 ) ;
#7077 = CARTESIAN_POINT ( 'NONE',  ( 6.892409439180999797, 3.668692617901999853, -8.939602259005999585 ) ) ;
#7078 = DIRECTION ( 'NONE',  ( 1.000000000000000000, 0.000000000000000000, 0.000000000000000000 ) ) ;
#7079 = CARTESIAN_POINT ( 'NONE',  ( 24.56891840910600067, -3.717059876636999771, -12.37205664472999977 ) ) ;
#7080 = CARTESIAN_POINT ( 'NONE',  ( 4.819736545624000890, -1.162446983990999883, 0.2403212362009999881 ) ) ;
#7081 = CARTESIAN_POINT ( 'NONE',  ( 8.889129719593999113, 5.687930027805999877, -7.109876198051000351 ) ) ;
#7082 = CARTESIAN_POINT ( 'NONE',  ( 9.958513540182876156, 3.836375382625530239, -8.749999999999998224 ) ) ;
#7083 = CARTESIAN_POINT ( 'NONE',  ( 10.68054891417000007, -2.768175152062000155, -6.114413274984999980 ) ) ;
#7084 = B_SPLINE_CURVE_WITH_KNOTS ( 'NONE', 3,
 ( #35109, #56421, #46278, #51511 ),
 .UNSPECIFIED., .F., .F.,
 ( 4, 4 ),
 ( 0.000000000000000000, 1.000000000000000000 ),
 .UNSPECIFIED. ) ;
#7085 = ADVANCED_FACE ( 'NONE', ( #51353 ), #66395, .T. ) ;
#7086 = EDGE_CURVE ( 'NONE', #8323, #32376, #35286, .T. ) ;
#7087 = DIRECTION ( 'NONE',  ( 0.000000000000000000, 0.1807154286439995039, -0.9835354258236027603 ) ) ;
#7088 = DIRECTION ( 'NONE',  ( -0.000000000000000000, 1.000000000000000000, 0.000000000000000000 ) ) ;
#7089 = CARTESIAN_POINT ( 'NONE',  ( 4.425837751058333325, 0.07782213664712105128, 1.517643997376458609 ) ) ;
#7090 = CARTESIAN_POINT ( 'NONE',  ( 18.30003129332100187, 2.732683818840999646, 11.53064095373000164 ) ) ;
#7091 = ADVANCED_FACE ( 'NONE', ( #24782 ), #36869, .F. ) ;
#7092 = EDGE_CURVE ( 'NONE', #66190, #66492, #68481, .T. ) ;
#7093 = CARTESIAN_POINT ( 'NONE',  ( 14.70000000000000107, -8.824259102667999954, -7.756628703356000187 ) ) ;
#7094 = LINE ( 'NONE', #23172, #59499 ) ;
#7095 = CARTESIAN_POINT ( 'NONE',  ( 11.10612378248509913, 3.517039242046199998, -6.586279795136899651 ) ) ;
#7096 = CARTESIAN_POINT ( 'NONE',  ( 9.305380199233999505, 4.996570247675600207, -7.374740103075099640 ) ) ;
#7098 = FACE_OUTER_BOUND ( 'NONE', #9322, .T. ) ;
#7097 = CARTESIAN_POINT ( 'NONE',  ( 9.697076168957998732, -4.439974903344300117, 6.752918994396699404 ) ) ;
#7099 = CARTESIAN_POINT ( 'NONE',  ( 7.716851002542999716, 2.832432432432000269, 6.822293592207000934 ) ) ;
#7100 = ORIENTED_EDGE ( 'NONE', *, *, #28896, .T. ) ;
#7101 = CARTESIAN_POINT ( 'NONE',  ( 10.56080513895999928, 5.026880838510000338, 8.070849345005600028 ) ) ;
#7102 = CARTESIAN_POINT ( 'NONE',  ( 7.426677373658002956, -3.232655724474999381, 6.473459691208998557 ) ) ;
#7103 = CARTESIAN_POINT ( 'NONE',  ( 9.076468108405999047, 5.230803879475000251, 7.151422676278199830 ) ) ;
#7104 = CARTESIAN_POINT ( 'NONE',  ( 10.77934687351631382, -4.163624617374463988, -6.249999999999999112 ) ) ;
#7105 = B_SPLINE_CURVE_WITH_KNOTS ( 'NONE', 3,
 ( #11597, #1467, #54250, #65072 ),
 .UNSPECIFIED., .F., .F.,
 ( 4, 4 ),
 ( 0.000000000000000000, 0.1255288371561983085 ),
 .UNSPECIFIED. ) ;
#7106 = CARTESIAN_POINT ( 'NONE',  ( 10.96580795178999956, -4.930647899304999804, 6.170539049947000088 ) ) ;
#7107 = CARTESIAN_POINT ( 'NONE',  ( 9.791887411239740047, -4.711645841719509953, 9.126404666217009520 ) ) ;
#7109 = CARTESIAN_POINT ( 'NONE',  ( 10.63351354018304740, 5.250000000000001776, 7.336375382625529795 ) ) ;
#7108 = UNCERTAINTY_MEASURE_WITH_UNIT (LENGTH_MEASURE( 1.000000000000000082E-05 ), #28402, 'distance_accuracy_value', 'NONE');
#7110 = ORIENTED_EDGE ( 'NONE', *, *, #6916, .T. ) ;
#7111 = VECTOR ( 'NONE', #68108, 1000.000000000000000 ) ;
#7112 = CARTESIAN_POINT ( 'NONE',  ( 8.976101285863999024, -4.646739515667500875, -6.731514281717299930 ) ) ;
#7113 = DIRECTION ( 'NONE',  ( 0.000000000000000000, 0.9421243786072194260, -0.3352635608502069764 ) ) ;
#7114 = CARTESIAN_POINT ( 'NONE',  ( 5.016063833727000265, -0.8125565852189000626, 1.395285458375999932 ) ) ;
#7115 = CARTESIAN_POINT ( 'NONE',  ( 10.99798614923244600, -2.813325336768271345, -5.071883290842238878 ) ) ;
#7116 = AXIS2_PLACEMENT_3D ( 'NONE', #29639, #35888, #34534 ) ;
#7117 = CARTESIAN_POINT ( 'NONE',  ( 7.000000000000000000, 0.5292307692307999245, -2.083846153846000249 ) ) ;
#7118 = CARTESIAN_POINT ( 'NONE',  ( 11.86749010443640096, -3.136214309321499805, 7.435402237490909449 ) ) ;
#7119 = CARTESIAN_POINT ( 'NONE',  ( 11.09256785386839894, 3.167490253789400523, -8.060248494254899754 ) ) ;
#7120 = CARTESIAN_POINT ( 'NONE',  ( 12.33198418664063034, 2.089544947752365101, -13.75203186101843578 ) ) ;
#7121 = DIRECTION ( 'NONE',  ( 0.000000000000000000, 0.8648648648648720183, -0.5020047465136825426 ) ) ;
#7122 = CARTESIAN_POINT ( 'NONE',  ( 5.679181296657521472, 13.00268187854355517, 2.124261045359595812 ) ) ;
#7123 = ORIENTED_EDGE ( 'NONE', *, *, #28758, .T. ) ;
#7124 = CARTESIAN_POINT ( 'NONE',  ( 18.20318779768322770, 2.896782429289181504, -13.69773569390626555 ) ) ;
#7125 = CARTESIAN_POINT ( 'NONE',  ( 12.11827043973742590, -0.2342631834278633973, -13.99804438501501203 ) ) ;
#7126 = DIRECTION ( 'NONE',  ( 1.000000000000000000, 0.000000000000000000, 0.000000000000000000 ) ) ;
#7127 = CARTESIAN_POINT ( 'NONE',  ( 25.58980421686700168, -8.350728274839999798, -7.985160199510000112 ) ) ;
#7128 = CARTESIAN_POINT ( 'NONE',  ( 10.62309687351639020, -2.782534154164605145, -7.827184855449101697 ) ) ;
#7129 = CARTESIAN_POINT ( 'NONE',  ( 9.048601287889788125, 4.000000467705929985, -8.698595322193607871 ) ) ;
#7130 = CARTESIAN_POINT ( 'NONE',  ( 5.695116968501675814, 12.04237015855112958, -3.723491068767787127 ) ) ;
#7131 = ORIENTED_EDGE ( 'NONE', *, *, #34669, .F. ) ;
#7132 = CARTESIAN_POINT ( 'NONE',  ( 0.1359928592618749876, 2.324556273228959184E-06, -3.136013406113613122 ) ) ;
#7133 = CARTESIAN_POINT ( 'NONE',  ( 17.65136412466922522, 3.242045876614677358, -13.61943996000380785 ) ) ;
#7134 = ORIENTED_EDGE ( 'NONE', *, *, #66607, .T. ) ;
#7135 = CARTESIAN_POINT ( 'NONE',  ( 11.37299956498129916, -5.207010770456999893, -7.174999999999999822 ) ) ;
#7136 = CARTESIAN_POINT ( 'NONE',  ( 8.481683059623998489, -2.472358291268000219, 6.234202627038999189 ) ) ;
#7137 = EDGE_CURVE ( 'NONE', #5123, #54862, #38875, .T. ) ;
#7138 = CARTESIAN_POINT ( 'NONE',  ( 9.791229719590001324, 4.294368353031000396, -8.968663198664000191 ) ) ;
#7139 = CARTESIAN_POINT ( 'NONE',  ( 24.04055935422329782, -12.64665599039150479, 3.439787933675944487 ) ) ;
#7140 = CARTESIAN_POINT ( 'NONE',  ( 17.60314900679412631, 1.789028854058313689, -13.88522169503354142 ) ) ;
#7141 = DIRECTION ( 'NONE',  ( -1.000000000000000000, 0.000000000000000000, 0.000000000000000000 ) ) ;
#7142 = ADVANCED_FACE ( 'NONE', ( #33634 ), #1810, .T. ) ;
#7143 = CARTESIAN_POINT ( 'NONE',  ( 10.27934687351566545, -4.163624617374463988, 8.750000000000001776 ) ) ;
#7144 = ORIENTED_EDGE ( 'NONE', *, *, #47586, .T. ) ;
#7145 = CARTESIAN_POINT ( 'NONE',  ( 11.02786767503999954, -5.596230239120999705, 7.209501483790000442 ) ) ;
#7146 = DIRECTION ( 'NONE',  ( -1.000000000000000000, 0.000000000000000000, 0.000000000000000000 ) ) ;
#7147 = CARTESIAN_POINT ( 'NONE',  ( 8.450464158772000189, 3.789127741898000057, -9.388182174781999123 ) ) ;
#7148 = EDGE_LOOP ( 'NONE', ( #34568, #37429, #33518 ) ) ;
#7149 = AXIS2_PLACEMENT_3D ( 'NONE', #39235, #45178, #56351 ) ;
#7150 = CARTESIAN_POINT ( 'NONE',  ( 9.662441121991999893, 4.824173073626999653, -8.517602418144999632 ) ) ;
#7151 = CARTESIAN_POINT ( 'NONE',  ( 4.500000000000000000, 0.000000000000000000, 0.000000000000000000 ) ) ;
#7152 = VERTEX_POINT ( 'NONE', #46868 ) ;
#7153 = CARTESIAN_POINT ( 'NONE',  ( 9.508013376692998619, 3.104586782631499897, 7.955057656228099461 ) ) ;
#7154 = CARTESIAN_POINT ( 'NONE',  ( 18.22068658462134749, -2.765866853816883353, -12.29268492208001362 ) ) ;
#7155 = CARTESIAN_POINT ( 'NONE',  ( 8.253230575588379025, 2.714951384259811196, 7.027308161653112784 ) ) ;
#7156 = DIRECTION ( 'NONE',  ( 0.000000000000000000, 1.000000000000000000, 0.000000000000000000 ) ) ;
#7157 = CARTESIAN_POINT ( 'NONE',  ( 11.68610928851700237, -11.49703662065999943, -1.632765284408000062 ) ) ;
#7158 = CARTESIAN_POINT ( 'NONE',  ( 8.800809814040999157, 4.530359890157599878, 6.814123855771700100 ) ) ;
#7159 = CARTESIAN_POINT ( 'NONE',  ( 9.377480346882569151, -2.931296748430716193, 8.873990698568421820 ) ) ;
#7160 = EDGE_LOOP ( 'NONE', ( #179, #67454, #42323, #60090, #9476 ) ) ;
#7161 = DIRECTION ( 'NONE',  ( 0.000000000000000000, -1.000000000000000000, 0.000000000000000000 ) ) ;
#7162 = CARTESIAN_POINT ( 'NONE',  ( 10.48598278040999965, 5.506034726153999692, -7.274787238512000265 ) ) ;
#7163 = CIRCLE ( 'NONE', #10547, 0.6999999999999992895 ) ;
#7164 = DIRECTION ( 'NONE',  ( -0.8660254037844289376, 1.235977903561818058E-11, 0.5000000000000169864 ) ) ;
#7165 = CARTESIAN_POINT ( 'NONE',  ( 12.60268547648130522, 3.091422767983463604, -13.53007486046832852 ) ) ;
#7166 = CARTESIAN_POINT ( 'NONE',  ( 10.57088779216199903, -2.816792857868000155, -7.926693309523199282 ) ) ;
#7167 = CARTESIAN_POINT ( 'NONE',  ( 9.504901164121001500, -3.934733502342999678, 5.704835336325999151 ) ) ;
#7168 = CARTESIAN_POINT ( 'NONE',  ( 18.03351914841129400, -0.5491314443420109992, 13.98923457196397990 ) ) ;
#7169 = CIRCLE ( 'NONE', #23943, 11.84999999999999964 ) ;
#7170 = CARTESIAN_POINT ( 'NONE',  ( 17.59542397727922847, 0.6250000000000002220, 13.88107975724994958 ) ) ;
#7171 = ADVANCED_FACE ( 'NONE', ( #29436 ), #57290, .T. ) ;
#7172 = ORIENTED_EDGE ( 'NONE', *, *, #5594, .T. ) ;
#7173 = VERTEX_POINT ( 'NONE', #24856 ) ;
#7174 = CARTESIAN_POINT ( 'NONE',  ( 9.933354719590999693, 5.639765292528999829, -8.059103558718000215 ) ) ;
#7175 = LINE ( 'NONE', #22555, #7702 ) ;
#7176 = AXIS2_PLACEMENT_3D ( 'NONE', #19326, #55711, #39629 ) ;
#7177 = EDGE_CURVE ( 'NONE', #5246, #10441, #52859, .T. ) ;
#7178 = CARTESIAN_POINT ( 'NONE',  ( 12.44983642699930471, -0.5143249053040993557, -13.88719129591020618 ) ) ;
#7179 = EDGE_CURVE ( 'NONE', #55729, #17154, #13409, .T. ) ;
#7180 = CARTESIAN_POINT ( 'NONE',  ( 11.00009108335970609, -2.881106418324590468, -7.597657431955929574 ) ) ;
#7181 = FACE_OUTER_BOUND ( 'NONE', #3464, .T. ) ;
#7182 = CARTESIAN_POINT ( 'NONE',  ( 8.539831853209999935, -5.633481712366999794, 7.451234046297000368 ) ) ;
#7183 = CARTESIAN_POINT ( 'NONE',  ( 25.46372676430900128, 8.354609436172999892, -8.148458316574000548 ) ) ;
#7185 = CARTESIAN_POINT ( 'NONE',  ( 11.12373728587000166, -5.759484258661999867, 5.183808156345000029 ) ) ;
#7184 = CARTESIAN_POINT ( 'NONE',  ( 11.06244474310100045, -2.862064370975999861, 6.947770206896899836 ) ) ;
#7186 = CARTESIAN_POINT ( 'NONE',  ( 10.83810672858429847, 2.978701842912999886, -6.731711997412900494 ) ) ;
#7187 = B_SPLINE_CURVE_WITH_KNOTS ( 'NONE', 3,
 ( #52366, #41531, #57258, #41877, #9359, #69134, #47474, #51675, #21240, #52013, #19867, #41198, #56929, #26494, #30704, #14289, #36638, #20898 ),
 .UNSPECIFIED., .F., .F.,
 ( 4, 2, 2, 2, 2, 2, 2, 2, 4 ),
 ( 0.000000000000000000, 0.1250000000000000000, 0.2500000000000000000, 0.3750000000000000000, 0.5000000000000000000, 0.6250000000000000000, 0.7500000000000000000, 0.8750000000000000000, 1.000000000000000000 ),
 .UNSPECIFIED. ) ;
#7188 = CARTESIAN_POINT ( 'NONE',  ( 24.46580263708699832, -8.828315330680998940, -8.953816637776000675 ) ) ;
#7189 = CARTESIAN_POINT ( 'NONE',  ( 18.29995936595984674, 11.60802783711982400, -4.146429233279109283 ) ) ;
#7190 = CARTESIAN_POINT ( 'NONE',  ( 18.11801110581809127, 0.2715269968477682094, 12.69609476950841120 ) ) ;
#7191 = B_SPLINE_SURFACE_WITH_KNOTS ( 'NONE', 3, 3, ( 
 ( #30583, #40722, #34808, #67284 ),
 ( #29222, #56815, #19057, #46668 ),
 ( #51895, #3993, #2976, #50534 ),
 ( #8230, #51554, #2636, #23963 ),
 ( #66946, #24652, #57479, #52936 ) ),
 .UNSPECIFIED., .F., .F., .F.,
 ( 4, 1, 4 ),
 ( 4, 4 ),
 ( 0.9547086424368000923, 1.000000000000000000, 1.007144313228999888 ),
 ( -0.1721939420595999803, 1.172193941872999856 ),
 .UNSPECIFIED. ) ;
#7192 = CARTESIAN_POINT ( 'NONE',  ( 23.56665676678100141, -10.37811504717999966, -9.381458738969000066 ) ) ;
#7193 = CARTESIAN_POINT ( 'NONE',  ( 17.83361872140014270, -3.059864849510719242, -12.30332992014196591 ) ) ;
#7194 = VERTEX_POINT ( 'NONE', #8435 ) ;
#7196 = CARTESIAN_POINT ( 'NONE',  ( 10.82145113417867677, 4.723115832319042084, 7.008885863206549161 ) ) ;
#7195 = CARTESIAN_POINT ( 'NONE',  ( 11.08380555355832620, -3.999999927290649460, -9.033895164528411570 ) ) ;
#7197 = CARTESIAN_POINT ( 'NONE',  ( 9.161379719595000637, 5.511689883260999956, -7.095113581311000672 ) ) ;
#7198 = CARTESIAN_POINT ( 'NONE',  ( 12.48958479105538011, -1.960066648180105453, 13.77326086059893306 ) ) ;
#7199 = ADVANCED_FACE ( 'NONE', ( #40251 ), #10430, .T. ) ;
#7200 = CARTESIAN_POINT ( 'NONE',  ( 7.004886577543231851, -1.395112899767755987, -0.1834843011541621716 ) ) ;
#7201 = CARTESIAN_POINT ( 'NONE',  ( 8.500365452454994752, -5.097361224984004124, 6.605627025648004746 ) ) ;
#7202 = FACE_OUTER_BOUND ( 'NONE', #17132, .T. ) ;
#7203 = B_SPLINE_SURFACE_WITH_KNOTS ( 'NONE', 3, 3, ( 
 ( #27950, #54160, #11503, #5915, #53817, #336, #48926, #1034, #22346, #16750, #26575, #26915, #43683, #65336, #27257, #42645, #64980, #685, #17095, #11853, #5574, #17455, #38427, #47899, #59751, #21652, #6259, #63955, #59404, #54510, #48230, #33191, #42986, #60105, #34114 ),
 ( #64294, #21315, #6611, #21996, #43339, #16409, #49261, #16066, #48580, #53137, #37398, #64644, #38077, #32848, #1371, #22689, #27598, #38780, #44033, #37740, #12211, #59067, #10824, #5237, #58720, #32167, #53481, #11168, #32502, #40493, #29690, #7304, #8002, #23729, #18149 ),
 ( #61820, #24424, #33540, #45749, #6959, #44385, #54857, #55204, #29337, #28646, #28290, #39470, #13257, #60449, #56237, #49610, #67059, #2069, #44727, #49956, #40166, #61481, #50991, #23388, #34921, #45411, #34233, #66025, #2405, #2750, #45067, #3088, #19169, #66371, #65684 ),
 ( #8344, #17807, #66720, #1717, #55552, #60792, #12905, #23036, #18495, #39124, #39820, #55898, #61140, #7650, #12555, #28998, #50649, #33887, #50307, #34582, #24074, #18839, #13600, #52702, #47466, #25792, #25444, #52005, #31049, #42225, #30360, #36630, #67396, #47122, #30031 ) ),
 .UNSPECIFIED., .F., .F., .F.,
 ( 4, 4 ),
 ( 4, 1, 1, 1, 1, 1, 1, 1, 1, 1, 1, 1, 1, 1, 1, 1, 1, 1, 1, 1, 1, 1, 1, 1, 1, 1, 1, 1, 1, 1, 1, 1, 4 ),
 ( -0.1039370721279000015, 1.103937072127999963 ),
 ( -0.02000000000000000042, 0.01250000000000000069, 0.04499999999999999833, 0.07749999999999999944, 0.1100000000000000006, 0.1424999999999999878, 0.1749999999999999889, 0.2074999999999999900, 0.2399999999999999911, 0.2725000000000000200, 0.3049999999999999933, 0.3375000000000000222, 0.3699999999999999956, 0.4025000000000000244, 0.4349999999999999978, 0.4675000000000000266, 0.5000000000000000000, 0.5324999999999999734, 0.5649999999999999467, 0.5975000000000000311, 0.6300000000000000044, 0.6624999999999999778, 0.6949999999999999512, 0.7275000000000000355, 0.7600000000000000089, 0.7924999999999999822, 0.8249999999999999556, 0.8575000000000000400, 0.8900000000000000133, 0.9224999999999999867, 0.9549999999999999600, 0.9875000000000000444, 1.020000000000000018 ),
 .UNSPECIFIED. ) ;
#7204 = CARTESIAN_POINT ( 'NONE',  ( 9.318998833837817131, 4.145059358747968048, 9.246721409219425425 ) ) ;
#7205 = CARTESIAN_POINT ( 'NONE',  ( 2.828929061525000233, 0.2082079807930999893, 3.419278880862000047 ) ) ;
#7206 = ORIENTED_EDGE ( 'NONE', *, *, #12277, .T. ) ;
#7207 = CARTESIAN_POINT ( 'NONE',  ( 12.13082219998073086, -0.2646961475753908943, -12.59722401988189588 ) ) ;
#7208 = FACE_OUTER_BOUND ( 'NONE', #56679, .T. ) ;
#7209 = CARTESIAN_POINT ( 'NONE',  ( 23.91316333561315943, -12.85062081998795058, -3.562165271204711825 ) ) ;
#7210 = CARTESIAN_POINT ( 'NONE',  ( 7.962142219590999659, 4.874567052833000069, 6.119507471270999588 ) ) ;
#7211 = VERTEX_POINT ( 'NONE', #14710 ) ;
#7212 = CARTESIAN_POINT ( 'NONE',  ( 6.486216479700000370, -0.9533226957039999672, 1.303269410926999994 ) ) ;
#7213 = CARTESIAN_POINT ( 'NONE',  ( 10.91096346280954599, 9.739945009095949402, 5.808747756428651599 ) ) ;
#7215 = CARTESIAN_POINT ( 'NONE',  ( 11.00000177645999955, -1.199999999999999956, 9.776630298829998011 ) ) ;
#7214 = CARTESIAN_POINT ( 'NONE',  ( 8.577663641219146484, -4.062279398746261094, 5.761468528428593139 ) ) ;
#7216 = CARTESIAN_POINT ( 'NONE',  ( 10.52606775832647656, -4.343526402396090447, -6.696209471835564919 ) ) ;
#7217 = VERTEX_POINT ( 'NONE', #52100 ) ;
#7218 = CARTESIAN_POINT ( 'NONE',  ( 21.10000000000000142, 0.000000000000000000, 0.000000000000000000 ) ) ;
#7219 = VERTEX_POINT ( 'NONE', #24515 ) ;
#7220 = CARTESIAN_POINT ( 'NONE',  ( 9.502127015675981170, -4.762560867020375177, 8.617745476188831688 ) ) ;
#7221 = CARTESIAN_POINT ( 'NONE',  ( 12.80505043854146940, -3.125000000000000000, -13.52078605991414761 ) ) ;
#7222 = CARTESIAN_POINT ( 'NONE',  ( 17.75589283472434232, -0.5919407257947371104, -13.88303015925713879 ) ) ;
#7223 = ORIENTED_EDGE ( 'NONE', *, *, #43570, .T. ) ;
#7224 = CARTESIAN_POINT ( 'NONE',  ( 10.94043540126313374, 9.310192335818811671, -6.236500861513892602 ) ) ;
#7225 = CARTESIAN_POINT ( 'NONE',  ( 18.30017264560541790, -1.838307226984665865, 11.74271423091507494 ) ) ;
#7226 = CARTESIAN_POINT ( 'NONE',  ( 10.23976354018333268, -4.327184855449098144, 8.717465845835395299 ) ) ;
#7227 = EDGE_CURVE ( 'NONE', #42472, #10401, #5958, .T. ) ;
#7228 = CARTESIAN_POINT ( 'NONE',  ( 6.555026506349999948, -1.500000000000000000, 0.000000000000000000 ) ) ;
#7229 = CARTESIAN_POINT ( 'NONE',  ( 8.613182395984926742, -4.653584300239352878, 5.903187239484563698 ) ) ;
#7230 = VERTEX_POINT ( 'NONE', #67493 ) ;
#7231 = FACE_BOUND ( 'NONE', #30639, .T. ) ;
#7232 = CARTESIAN_POINT ( 'NONE',  ( 24.03127826811100221, -13.13555942676999955, -3.280046834557000413 ) ) ;
#7233 = CIRCLE ( 'NONE', #16153, 1.300165623003000981 ) ;
#7234 = CARTESIAN_POINT ( 'NONE',  ( 9.841846873515665450, 3.000416447002276943, 8.268183399968647151 ) ) ;
#7235 = CARTESIAN_POINT ( 'NONE',  ( 4.599999999999999645, 0.6250000000000001110, -13.88107975066922428 ) ) ;
#7236 = VERTEX_POINT ( 'NONE', #35356 ) ;
#7237 = CARTESIAN_POINT ( 'NONE',  ( 23.77343974722910502, 13.06033031041715020, -3.746575852910564386 ) ) ;
#7238 = LINE ( 'NONE', #44997, #35494 ) ;
#7239 = CARTESIAN_POINT ( 'NONE',  ( 7.540822165042829539, 2.490019829878222790, -8.581199080916018573 ) ) ;
#7240 = CARTESIAN_POINT ( 'NONE',  ( 5.000030787343001215, -1.679270695423617399, 1.290525307673965560 ) ) ;
#7241 = CARTESIAN_POINT ( 'NONE',  ( 24.44496351116800170, 3.224881296174999967, 12.03535797436000010 ) ) ;
#7242 = CARTESIAN_POINT ( 'NONE',  ( 5.825859839684249586, 1.460959015002472494, 0.3926218265389232465 ) ) ;
#7243 = CARTESIAN_POINT ( 'NONE',  ( 17.92144340210922948, -1.859318429515438353, 12.46206136722991786 ) ) ;
#7244 = VERTEX_POINT ( 'NONE', #45836 ) ;
#7245 = CARTESIAN_POINT ( 'NONE',  ( 11.67766954483535891, -3.284117569315500251, -6.395429936871999566 ) ) ;
#7246 = EDGE_LOOP ( 'NONE', ( #64907, #58050, #4991, #22806, #16389, #37407, #16091, #37478, #48295, #28051, #32225 ) ) ;
#7247 = CARTESIAN_POINT ( 'NONE',  ( 11.56571517796000137, -12.12283255502000046, -1.989142034170999995 ) ) ;
#7248 = CARTESIAN_POINT ( 'NONE',  ( 8.649364158774000444, 3.038023536984999939, -5.861661709981000001 ) ) ;
#7249 = CARTESIAN_POINT ( 'NONE',  ( 3.551082810560999725, -2.917487451239999530, 1.705317907324000126 ) ) ;
#7250 = CARTESIAN_POINT ( 'NONE',  ( 10.30297040315999979, -4.081263557776000361, -9.025012210052000938 ) ) ;
#7251 = CARTESIAN_POINT ( 'NONE',  ( 24.37816192318917174, 3.385901465919856523, 12.24459555508155972 ) ) ;
#7252 = MECHANICAL_DESIGN_GEOMETRIC_PRESENTATION_REPRESENTATION (  '', ( #34362 ), #57486 ) ;
#7253 = CARTESIAN_POINT ( 'NONE',  ( 7.686616257283001907, 3.172402717919002413, -6.371572564913001280 ) ) ;
#7254 = CYLINDRICAL_SURFACE ( 'NONE', #25509, 1.250000000000000222 ) ;
#7255 = VERTEX_POINT ( 'NONE', #50742 ) ;
#7256 = CARTESIAN_POINT ( 'NONE',  ( 25.60000000000000142, 11.10814700232000085, 2.976419018679000050 ) ) ;
#7257 = EDGE_CURVE ( 'NONE', #51205, #54348, #51762, .T. ) ;
#7258 = CARTESIAN_POINT ( 'NONE',  ( 12.10948876160955479, -4.695527826393099957, 6.776679950459500112 ) ) ;
#7259 = CARTESIAN_POINT ( 'NONE',  ( 10.25461802485000007, 2.860644035673999941, 6.604613005744999654 ) ) ;
#7260 = ADVANCED_FACE ( 'NONE', ( #30449 ), #48360, .T. ) ;
#7261 = DIRECTION ( 'NONE',  ( 0.000000000000000000, 0.000000000000000000, -1.000000000000000000 ) ) ;
#7262 = DIRECTION ( 'NONE',  ( -1.000000000000000000, 0.000000000000000000, 0.000000000000000000 ) ) ;
#7263 = CARTESIAN_POINT ( 'NONE',  ( 9.108372294250248302, 3.858766891214160832, 8.849156255801389648 ) ) ;
#7264 = CARTESIAN_POINT ( 'NONE',  ( 10.92441504065829960, 4.694414232677499577, -6.982228367137699898 ) ) ;
#7265 = CARTESIAN_POINT ( 'NONE',  ( -15.86200481174999943, 2.399999999999999911, -6.571291218949999902 ) ) ;
#7266 = CIRCLE ( 'NONE', #28490, 12.50000000000000000 ) ;
#7267 = CARTESIAN_POINT ( 'NONE',  ( 9.809000818239997699, 2.989704013253000614, -8.032011717116800398 ) ) ;
#7268 = CARTESIAN_POINT ( 'NONE',  ( 23.58312295925200175, -10.33205725754000071, 9.361132995946999102 ) ) ;
#7269 = DIRECTION ( 'NONE',  ( 0.000000000000000000, 0.9630775622489645693, -0.2692240871329898422 ) ) ;
#7270 = ORIENTED_EDGE ( 'NONE', *, *, #10523, .F. ) ;
#7271 = CARTESIAN_POINT ( 'NONE',  ( 8.721004440379999778, -5.983034890242000081, 7.440798487724999966 ) ) ;
#7272 = CARTESIAN_POINT ( 'NONE',  ( 10.10891502095999961, -5.332339947063000629, -7.851654145788001138 ) ) ;
#7273 = CARTESIAN_POINT ( 'NONE',  ( 18.17327101506963061, 2.135860178445227575, 13.83613041148202782 ) ) ;
#7274 = ADVANCED_FACE ( 'NONE', ( #40933 ), #68175, .T. ) ;
#7275 = CARTESIAN_POINT ( 'NONE',  ( 15.90000000000360991, -3.781197540827905712, -11.56430939782970668 ) ) ;
#7276 = CARTESIAN_POINT ( 'NONE',  ( 11.57656516821460890, -3.100463633631699967, -8.407828142327998577 ) ) ;
#7277 = ORIENTED_EDGE ( 'NONE', *, *, #48695, .T. ) ;
#7278 = CARTESIAN_POINT ( 'NONE',  ( 25.57799048303400014, 2.767957921537000043, -11.23360358486999999 ) ) ;
#7279 = ADVANCED_FACE ( 'NONE', ( #14376, #62588 ), #3518, .T. ) ;
#7280 = CARTESIAN_POINT ( 'NONE',  ( 17.85446786537200126, 3.297647132553999771, 11.83458225989999946 ) ) ;
#7282 = CARTESIAN_POINT ( 'NONE',  ( 9.191343736187999269, -4.374232398910099739, 6.690658690097199823 ) ) ;
#7281 = CARTESIAN_POINT ( 'NONE',  ( 9.839810841229999383, 5.817107086401000160, -6.945352709928000579 ) ) ;
#7283 = CARTESIAN_POINT ( 'NONE',  ( 3.442208132701131351, -1.604827515477729838, 2.835269537469987888 ) ) ;
#7284 = ORIENTED_EDGE ( 'NONE', *, *, #11991, .F. ) ;
#7285 = CARTESIAN_POINT ( 'NONE',  ( 10.13339736671999880, 5.653645990693000556, 6.501823474484000442 ) ) ;
#7286 = CARTESIAN_POINT ( 'NONE',  ( 25.00276452419147333, 3.413701559985177436, -11.76138395131285108 ) ) ;
#7287 = CARTESIAN_POINT ( 'NONE',  ( 11.40841235500449891, 3.158861363519000154, 8.270568563129298667 ) ) ;
#7288 = CARTESIAN_POINT ( 'NONE',  ( 9.260912867475999732, -4.901383038209000453, 9.090314591495999963 ) ) ;
#7289 = CARTESIAN_POINT ( 'NONE',  ( 9.069724726289001282, -4.108965473266000146, 8.851626696081998702 ) ) ;
#7290 = ORIENTED_EDGE ( 'NONE', *, *, #35829, .F. ) ;
#7291 = CARTESIAN_POINT ( 'NONE',  ( 24.54223752888965748, 12.46060277337064370, 3.023618805785813990 ) ) ;
#7292 = AXIS2_PLACEMENT_3D ( 'NONE', #9645, #36922, #58237 ) ;
#7293 = CARTESIAN_POINT ( 'NONE',  ( 10.23580444037999904, -3.621838308198000345, -8.806219190581000333 ) ) ;
#7294 = CARTESIAN_POINT ( 'NONE',  ( 7.955723615552813044, -2.265131536788511646, 7.358139940862454154 ) ) ;
#7295 = CARTESIAN_POINT ( 'NONE',  ( 9.124702828701000357, -4.778665285493000070, 8.799745834808000211 ) ) ;
#7296 = CARTESIAN_POINT ( 'NONE',  ( 23.63066751290400092, 3.422883563399000018, 13.57573942691999846 ) ) ;
#7297 = CARTESIAN_POINT ( 'NONE',  ( 9.955342523875000182, -5.128664655368000425, 7.672773098917999413 ) ) ;
#7298 = VERTEX_POINT ( 'NONE', #24166 ) ;
#7299 = CARTESIAN_POINT ( 'NONE',  ( 23.67317744432095949, -9.998263301726394658, 9.464660330969566715 ) ) ;
#7300 = CARTESIAN_POINT ( 'NONE',  ( 12.05194988689359903, -3.419512757306400363, 6.361426117087999543 ) ) ;
#7301 = ORIENTED_EDGE ( 'NONE', *, *, #39725, .T. ) ;
#7302 = CARTESIAN_POINT ( 'NONE',  ( 9.107059081473819262, -5.098368162008560134, -6.579893398394093929 ) ) ;
#7303 = VERTEX_POINT ( 'NONE', #35695 ) ;
#7304 = CARTESIAN_POINT ( 'NONE',  ( 8.316054719590999511, 3.826300099041999747, -9.055335252254000267 ) ) ;
#7305 = CARTESIAN_POINT ( 'NONE',  ( 15.40000000009400161, -8.833277835210999740, -7.896561221812000930 ) ) ;
#7306 = DIRECTION ( 'NONE',  ( -1.000000000000000000, 0.000000000000000000, 1.554312234491000161E-14 ) ) ;
#7307 = CARTESIAN_POINT ( 'NONE',  ( 12.78419053748684675, 1.875000590519849908, -12.57545628621518041 ) ) ;
#7308 = CARTESIAN_POINT ( 'NONE',  ( 11.77745123989519982, -3.589787500396900199, 6.707778874960499849 ) ) ;
#7309 = ORIENTED_EDGE ( 'NONE', *, *, #20604, .F. ) ;
#7310 = CARTESIAN_POINT ( 'NONE',  ( 18.18005044575082252, 2.500000006795693785, 13.67340643792831045 ) ) ;
#7311 = VERTEX_POINT ( 'NONE', #3858 ) ;
#7312 = CARTESIAN_POINT ( 'NONE',  ( 9.433105646793000787, -4.954907757874000396, 8.825780921426000347 ) ) ;
#7313 = CARTESIAN_POINT ( 'NONE',  ( 7.942841246801999766, 3.400849348593999899, -6.290208884758000885 ) ) ;
#7314 = ORIENTED_EDGE ( 'NONE', *, *, #47552, .T. ) ;
#7315 = CARTESIAN_POINT ( 'NONE',  ( 12.13758509790272910, -2.198972988417293273, -12.40663693328272288 ) ) ;
#7316 = CARTESIAN_POINT ( 'NONE',  ( 11.60533460557258323, 4.184174550317700358, 6.374224726731999802 ) ) ;
#7317 = PRODUCT_DEFINITION ( 'UNKNOWN', '', #615, #39973 ) ;
#7318 = CARTESIAN_POINT ( 'NONE',  ( 10.53198305961999992, -2.323723769066000422, -8.279488812962998878 ) ) ;
#7319 = CARTESIAN_POINT ( 'NONE',  ( 6.419609839683333874, 0.1963495408493571848, 1.500000000000000666 ) ) ;
#7320 = CARTESIAN_POINT ( 'NONE',  ( 18.21401021018400002, -11.54142174797000031, 4.213216475886000012 ) ) ;
#7321 = CARTESIAN_POINT ( 'NONE',  ( 9.110163692916374956, 5.234200089434220438, -7.245561603203542589 ) ) ;
#7322 = DIRECTION ( 'NONE',  ( 0.000000000000000000, -1.000000000000000000, 0.000000000000000000 ) ) ;
#7323 = CARTESIAN_POINT ( 'NONE',  ( 17.81340500845573871, -0.5691963043021742719, -12.68282590392938225 ) ) ;
#7324 = LINE ( 'NONE', #28665, #26314 ) ;
#7325 = CARTESIAN_POINT ( 'NONE',  ( 10.91610672858429965, -4.911600290708499905, -6.814233985789400094 ) ) ;
#7326 = CARTESIAN_POINT ( 'NONE',  ( 8.545864158774001851, 3.856772556595000179, 5.521246073317000125 ) ) ;
#7327 = ORIENTED_EDGE ( 'NONE', *, *, #49248, .T. ) ;
#7328 =( NAMED_UNIT ( * ) PLANE_ANGLE_UNIT ( ) SI_UNIT ( $, .RADIAN. ) );
#7329 = CARTESIAN_POINT ( 'NONE',  ( 11.59999999999999787, -4.292035002842709446, -8.536357045506706598 ) ) ;
#7330 = CARTESIAN_POINT ( 'NONE',  ( 8.225195096046167720, 2.649880853682612614, 7.500010424662513664 ) ) ;
#7331 = CARTESIAN_POINT ( 'NONE',  ( 10.68375192593000023, 4.547306763790999184, -8.749120576764999768 ) ) ;
#7332 = CARTESIAN_POINT ( 'NONE',  ( 17.65155715295176719, 3.193702317672029611, 12.18853033496119842 ) ) ;
#7333 = CARTESIAN_POINT ( 'NONE',  ( 18.31587707751100069, 3.089759977613000252, -11.98885651319999823 ) ) ;
#7334 = CARTESIAN_POINT ( 'NONE',  ( 9.347254965556000883, 4.028327103212000715, 9.469449669541999626 ) ) ;
#7335 = CARTESIAN_POINT ( 'NONE',  ( 10.98768503802999952, -8.067884818888000353, -6.818830313157000056 ) ) ;
#7336 = CARTESIAN_POINT ( 'NONE',  ( 12.61463924707910245, 0.7003689475937157072, -12.58057160030251254 ) ) ;
#7337 = EDGE_CURVE ( 'NONE', #47809, #45267, #59332, .T. ) ;
#7338 = ORIENTED_EDGE ( 'NONE', *, *, #19922, .F. ) ;
#7339 = CARTESIAN_POINT ( 'NONE',  ( 12.13037555192281047, -2.744322634620805612, 12.29751256722372865 ) ) ;
#7340 = ADVANCED_FACE ( 'NONE', ( #16416 ), #40583, .F. ) ;
#7341 = CARTESIAN_POINT ( 'NONE',  ( 9.756329965421999262, -4.697624103824200148, -8.222608407156599242 ) ) ;
#7342 = DIRECTION ( 'NONE',  ( 0.000000000000000000, 1.000000000000000000, 0.000000000000000000 ) ) ;
#7343 = CARTESIAN_POINT ( 'NONE',  ( 3.350000000000000089, 0.000000000000000000, 0.000000000000000000 ) ) ;
#7344 = AXIS2_PLACEMENT_3D ( 'NONE', #40946, #55656, #2850 ) ;
#7345 = CARTESIAN_POINT ( 'NONE',  ( 10.30072469555899950, 4.570852684939899824, -6.512367818249299667 ) ) ;
#7346 = CARTESIAN_POINT ( 'NONE',  ( 12.63954751664500442, -0.7006927685644985804, 12.58050281163331796 ) ) ;
#7347 = CARTESIAN_POINT ( 'NONE',  ( 7.764232780408999446, 4.628941086829000184, 5.991667691044999522 ) ) ;
#7348 = CARTESIAN_POINT ( 'NONE',  ( 11.02286749330999882, 2.398743616553999924, 6.352468982205000891 ) ) ;
#7349 = CARTESIAN_POINT ( 'NONE',  ( 12.18021258978585486, 2.482515821435916870, 12.45562150274660596 ) ) ;
#7350 = VERTEX_POINT ( 'NONE', #68517 ) ;
#7351 = CARTESIAN_POINT ( 'NONE',  ( 8.947714158774999760, 3.854507394315999758, -9.394302886912999639 ) ) ;
#7352 = CARTESIAN_POINT ( 'NONE',  ( 11.13349010443639919, 5.274453806861999716, -7.595309363461700158 ) ) ;
#7353 = DIRECTION ( 'NONE',  ( 0.000000000000000000, 0.2437104050146043921, -0.9698480491745176124 ) ) ;
#7355 = CARTESIAN_POINT ( 'NONE',  ( 17.94896820980294905, -0.4852478459816373935, 12.68752000237651778 ) ) ;
#7354 = CARTESIAN_POINT ( 'NONE',  ( 11.79999999550100220, -3.351258778187000242, 11.15757272551999968 ) ) ;
#7356 = CARTESIAN_POINT ( 'NONE',  ( 9.906696787962999906, -3.827518619249500098, 8.489491017455099708 ) ) ;
#7357 = CARTESIAN_POINT ( 'NONE',  ( 11.24441369783139777, -4.043700988887960257, -8.365094684940499903 ) ) ;
#7358 = ORIENTED_EDGE ( 'NONE', *, *, #45539, .T. ) ;
#7359 = CARTESIAN_POINT ( 'NONE',  ( 1.543883544273999986, -2.789116823352000285, 1.988880583162999871 ) ) ;
#7360 = EDGE_CURVE ( 'NONE', #56202, #38546, #13793, .T. ) ;
#7361 = CARTESIAN_POINT ( 'NONE',  ( 24.01909549956856793, -9.335994749712794416, -9.253314179451693988 ) ) ;
#7362 = VECTOR ( 'NONE', #30297, 1000.000000000000000 ) ;
#7363 = CARTESIAN_POINT ( 'NONE',  ( 25.46373185538400463, 11.23406899464000119, 3.161078463958999496 ) ) ;
#7364 = DIRECTION ( 'NONE',  ( -0.7071067811865474617, -0.7071067811865474617, 9.304624505883612300E-09 ) ) ;
#7365 = B_SPLINE_CURVE_WITH_KNOTS ( 'NONE', 3,
 ( #16723, #5550, #10114, #31445 ),
 .UNSPECIFIED., .F., .F.,
 ( 4, 4 ),
 ( 0.000000000000000000, 1.000000000000000000 ),
 .UNSPECIFIED. ) ;
#7366 = B_SPLINE_CURVE_WITH_KNOTS ( 'NONE', 3,
 ( #5261, #26253, #43369, #64669 ),
 .UNSPECIFIED., .F., .F.,
 ( 4, 4 ),
 ( 0.000000000000000000, 1.000000000000000000 ),
 .UNSPECIFIED. ) ;
#7367 = CARTESIAN_POINT ( 'NONE',  ( 24.55996189856299949, -12.50738814765000129, 2.996555333579999925 ) ) ;
#7368 = CARTESIAN_POINT ( 'NONE',  ( 12.12494527865627880, -2.264899384641844815, 13.81558393673957141 ) ) ;
#7369 = CARTESIAN_POINT ( 'NONE',  ( 11.89975833414730033, -3.203462856645999945, 7.825000000000000178 ) ) ;
#7370 = DIRECTION ( 'NONE',  ( 1.000000000000000000, 0.000000000000000000, 0.000000000000000000 ) ) ;
#7371 = DIRECTION ( 'NONE',  ( 1.000000000000000000, 0.000000000000000000, 0.000000000000000000 ) ) ;
#7372 = B_SPLINE_CURVE_WITH_KNOTS ( 'NONE', 3,
 ( #16329, #37658, #64214, #48499, #11091, #5500 ),
 .UNSPECIFIED., .F., .F.,
 ( 4, 2, 4 ),
 ( 0.000000000000000000, 0.5000000000000000000, 1.000000000000000000 ),
 .UNSPECIFIED. ) ;
#7373 = ORIENTED_EDGE ( 'NONE', *, *, #303, .F. ) ;
#7374 = CARTESIAN_POINT ( 'NONE',  ( 10.38528584683667688, -3.267379250638399846, -8.166081851074052267 ) ) ;
#7375 = CARTESIAN_POINT ( 'NONE',  ( 11.13711610220999937, 5.336572488559999883, 5.178750058134000689 ) ) ;
#7376 = DIRECTION ( 'NONE',  ( -1.000000000000000000, 0.000000000000000000, 0.000000000000000000 ) ) ;
#7377 = CARTESIAN_POINT ( 'NONE',  ( 7.600000000000000533, -12.34999999999999964, -4.046978686977000011E-05 ) ) ;
#7378 = DIRECTION ( 'NONE',  ( -0.000000000000000000, -0.000000000000000000, 1.000000000000000000 ) ) ;
#7379 = VERTEX_POINT ( 'NONE', #5242 ) ;
#7380 = CARTESIAN_POINT ( 'NONE',  ( 10.68797807636180863, 4.829546767829883791, -8.579382731882136071 ) ) ;
#7381 = CARTESIAN_POINT ( 'NONE',  ( 17.68665174764113246, -11.41076566300253425, 4.624016165095039099 ) ) ;
#7382 = CARTESIAN_POINT ( 'NONE',  ( 9.681187238460999822, 2.612249048987000055, 7.804677627401999551 ) ) ;
#7383 = CARTESIAN_POINT ( 'NONE',  ( 10.89564560330029863, 4.307504762655200103, 8.455191956516999952 ) ) ;
#7384 = CARTESIAN_POINT ( 'NONE',  ( 11.13459739833729856, -4.823158118387800286, -7.825000000000000178 ) ) ;
#7385 = FACE_OUTER_BOUND ( 'NONE', #63555, .T. ) ;
#7386 = CARTESIAN_POINT ( 'NONE',  ( 10.25000000000000000, 0.000000000000000000, 0.000000000000000000 ) ) ;
#7387 = CARTESIAN_POINT ( 'NONE',  ( 7.000000000000000000, 10.80467225524999897, 3.475853594956999970 ) ) ;
#7388 = CARTESIAN_POINT ( 'NONE',  ( 9.512931135678952543, 5.100000000000000533, 6.444141223441286925 ) ) ;
#7389 = VERTEX_POINT ( 'NONE', #48235 ) ;
#7390 = CARTESIAN_POINT ( 'NONE',  ( 8.596685841231000325, 2.141799395716999843, -7.895788736628000848 ) ) ;
#7391 = VERTEX_POINT ( 'NONE', #5922 ) ;
#7392 = CARTESIAN_POINT ( 'NONE',  ( 18.11747123342424715, -2.226643993407489308, 13.72766178540381254 ) ) ;
#7393 = CARTESIAN_POINT ( 'NONE',  ( 10.98579841651039857, -4.449968941611500028, -8.696179055230999211 ) ) ;
#7394 = ORIENTED_EDGE ( 'NONE', *, *, #40389, .F. ) ;
#7395 = CARTESIAN_POINT ( 'NONE',  ( 24.79997670811756194, -3.079643851578497848, -11.72208648962189415 ) ) ;
#7396 = CARTESIAN_POINT ( 'NONE',  ( 5.389000765264640336, -0.8358857551952053599, -0.7645196268596808897 ) ) ;
#7397 = CARTESIAN_POINT ( 'NONE',  ( 8.734200250017998712, -3.906155787512310074, -8.386722339907899837 ) ) ;
#7398 = EDGE_CURVE ( 'NONE', #21003, #16931, #63272, .T. ) ;
#7399 = DIRECTION ( 'NONE',  ( 1.000000000000000000, 0.000000000000000000, 0.000000000000000000 ) ) ;
#7400 = EDGE_CURVE ( 'NONE', #42097, #51258, #49300, .T. ) ;
#7401 = FACE_OUTER_BOUND ( 'NONE', #13406, .T. ) ;
#7402 = CARTESIAN_POINT ( 'NONE',  ( 10.74809687351608289, -3.672815144550895194, 8.717465845835393523 ) ) ;
#7403 = CARTESIAN_POINT ( 'NONE',  ( 11.26374551471000274, 3.753781600817000186, -11.28122097457000095 ) ) ;
#7404 = CARTESIAN_POINT ( 'NONE',  ( 10.19715077290999972, -4.982624057277000418, -6.124316828241999744 ) ) ;
#7405 = CARTESIAN_POINT ( 'NONE',  ( 7.100000000000000533, -12.59999999999999964, 1.543054966925665076E-15 ) ) ;
#7406 = VERTEX_POINT ( 'NONE', #20986 ) ;
#7407 = B_SPLINE_CURVE_WITH_KNOTS ( 'NONE', 3,
 ( #47850, #57988, #9738, #41562, #25483, #4145, #42597, #52392, #46812, #30734, #10086, #68805, #26521, #20927, #58326, #62871, #15340, #47156 ),
 .UNSPECIFIED., .F., .F.,
 ( 4, 2, 2, 2, 2, 2, 2, 2, 4 ),
 ( 0.000000000000000000, 0.1250000000000000555, 0.2500000000000001110, 0.3750000000000001665, 0.5000000000000002220, 0.6250000000000001110, 0.7500000000000001110, 0.8750000000000000000, 1.000000000000000000 ),
 .UNSPECIFIED. ) ;
#7408 = CARTESIAN_POINT ( 'NONE',  ( 20.00000000000000000, 11.79499999999999993, 0.000000000000000000 ) ) ;
#7409 = SHAPE_REPRESENTATION_RELATIONSHIP ( 'NONE' , 'NONE' ,  #22871, #30277 ) ;
#7410 = CARTESIAN_POINT ( 'NONE',  ( 10.09999999999999964, 0.000000000000000000, -11.84999999999999964 ) ) ;
#7411 = CARTESIAN_POINT ( 'NONE',  ( 11.00643352828999966, -5.061761008800999662, 5.194533778134999835 ) ) ;
#7412 = CARTESIAN_POINT ( 'NONE',  ( 8.224726226261992679, 8.026539296952000413, 4.869553275538997639 ) ) ;
#7413 = CARTESIAN_POINT ( 'NONE',  ( 10.44424205625099944, 3.541248877825399877, -8.694123841252999085 ) ) ;
#7414 = CARTESIAN_POINT ( 'NONE',  ( 12.20116045406118310, 2.662322297126387571, 13.63765712018377663 ) ) ;
#7415 = CARTESIAN_POINT ( 'NONE',  ( 10.78089914631999946, -5.735295708369000600, 7.801561210335000496 ) ) ;
#7416 = ORIENTED_EDGE ( 'NONE', *, *, #54800, .F. ) ;
#7417 = DIRECTION ( 'NONE',  ( 1.000000000000000000, 0.000000000000000000, 0.000000000000000000 ) ) ;
#7418 = CARTESIAN_POINT ( 'NONE',  ( 12.08233492791620378, 0.05915529127692535638, 13.99988012777929214 ) ) ;
#7419 = B_SPLINE_CURVE_WITH_KNOTS ( 'NONE', 3,
 ( #27561, #48888, #995, #24727 ),
 .UNSPECIFIED., .F., .F.,
 ( 4, 4 ),
 ( 0.000000000000000000, 1.000000000000000000 ),
 .UNSPECIFIED. ) ;
#7420 = ORIENTED_EDGE ( 'NONE', *, *, #66623, .T. ) ;
#7421 = CARTESIAN_POINT ( 'NONE',  ( 7.126409439180999783, 4.037115771921000018, -6.023232697733999608 ) ) ;
#7422 = EDGE_CURVE ( 'NONE', #54502, #28894, #40160, .T. ) ;
#7423 = CARTESIAN_POINT ( 'NONE',  ( 10.59999999999999964, 4.599999999999999645, -4.756097560976000338 ) ) ;
#7424 = CARTESIAN_POINT ( 'NONE',  ( 24.02031753346800258, -3.259282138741000256, -12.61500720365999939 ) ) ;
#7425 = DIRECTION ( 'NONE',  ( 0.000000000000000000, 0.000000000000000000, 1.000000000000000000 ) ) ;
#7426 = EDGE_CURVE ( 'NONE', #21138, #438, #37067, .T. ) ;
#7427 = CARTESIAN_POINT ( 'NONE',  ( 8.979720280412999855, 5.524776413195999325, -7.147585171405999915 ) ) ;
#7428 = DIRECTION ( 'NONE',  ( -0.000000000000000000, -0.000000000000000000, 1.000000000000000000 ) ) ;
#7429 = CARTESIAN_POINT ( 'NONE',  ( 11.07109161080999904, 7.831824785490000274, -6.601376317068999633 ) ) ;
#7430 = CARTESIAN_POINT ( 'NONE',  ( 4.599999999999999645, 12.59999999999999964, 0.000000000000000000 ) ) ;
#7431 = CARTESIAN_POINT ( 'NONE',  ( 15.40000000000000036, -40.50079594190999899, -35.53525775058000136 ) ) ;
#7432 = CARTESIAN_POINT ( 'NONE',  ( 9.524152735436000938, -4.911674715448000050, -6.466751564808000730 ) ) ;
#7433 = CARTESIAN_POINT ( 'NONE',  ( 10.57980110216399972, 3.260758259645400337, -7.048535450274799885 ) ) ;
#7434 = CARTESIAN_POINT ( 'NONE',  ( 1.230140132541749809, -3.408904368339107815, 0.9161175952574674985 ) ) ;
#7435 = CARTESIAN_POINT ( 'NONE',  ( 11.56322412107030928, 4.054600656575539475, -6.467939235001000320 ) ) ;
#7436 = CARTESIAN_POINT ( 'NONE',  ( 10.06525461470299909, 3.026595211686900377, -7.747639695388999215 ) ) ;
#7438 = CARTESIAN_POINT ( 'NONE',  ( 11.04989271531000128, -2.849679502984999946, 5.124329486915000231 ) ) ;
#7437 = LINE ( 'NONE', #8821, #629 ) ;
#7439 = CARTESIAN_POINT ( 'NONE',  ( 7.491953176340000908, -3.528027000165000704, 6.607934030033999484 ) ) ;
#7440 = EDGE_LOOP ( 'NONE', ( #9883, #36078, #55500, #900, #34301, #45290, #29182, #20319, #31149 ) ) ;
#7441 = EDGE_CURVE ( 'NONE', #50078, #59647, #45967, .T. ) ;
#7442 = CARTESIAN_POINT ( 'NONE',  ( 11.14256920625030034, 4.042230905578960254, 8.674127893687000324 ) ) ;
#7443 = VECTOR ( 'NONE', #49107, 1000.000000000000000 ) ;
#7444 = CARTESIAN_POINT ( 'NONE',  ( 9.137549407199999862, -2.995696424181999884, 8.544763501938000161 ) ) ;
#7445 = CARTESIAN_POINT ( 'NONE',  ( 9.049126402770998112, 5.068373778467000434, 7.902879529556599891 ) ) ;
#7446 = CARTESIAN_POINT ( 'NONE',  ( 10.06276198887462847, 3.334064478527818842, -6.932494801640175730 ) ) ;
#7447 = CARTESIAN_POINT ( 'NONE',  ( 9.662553763536999796, -4.094830574823999925, 9.119950378356000087 ) ) ;
#7448 = AXIS2_PLACEMENT_3D ( 'NONE', #26036, #31290, #64795 ) ;
#7449 = DIRECTION ( 'NONE',  ( -1.000000000000000000, 0.000000000000000000, 0.000000000000000000 ) ) ;
#7450 = CARTESIAN_POINT ( 'NONE',  ( 11.60578299225600141, 3.447612089971000326, -11.88742905964999963 ) ) ;
#7451 = VERTEX_POINT ( 'NONE', #38082 ) ;
#7452 =( REPRESENTATION_RELATIONSHIP ('NONE','NONE', #10823, #55423 ) REPRESENTATION_RELATIONSHIP_WITH_TRANSFORMATION ( #38241 )SHAPE_REPRESENTATION_RELATIONSHIP( ) );
#7453 = CARTESIAN_POINT ( 'NONE',  ( 9.961925467520998723, -5.139081147506999514, -7.421078600323300023 ) ) ;
#7454 = LINE ( 'NONE', #38936, #20863 ) ;
#7455 = CARTESIAN_POINT ( 'NONE',  ( 5.952062685092999850, 1.402153912072999997, 0.4364538398439999911 ) ) ;
#7456 = CARTESIAN_POINT ( 'NONE',  ( 10.52052890781999928, 2.899999999999999911, 6.152188490330000370 ) ) ;
#7457 = CARTESIAN_POINT ( 'NONE',  ( 11.49999672495000347, 10.14910021683508567, -5.848045769722699738 ) ) ;
#7458 = CARTESIAN_POINT ( 'NONE',  ( 11.06795257254739973, 3.036453385827900142, -7.780229861306499295 ) ) ;
#7459 = CARTESIAN_POINT ( 'NONE',  ( 7.766851002543999627, -2.832432432432000269, 6.822293592207000934 ) ) ;
#7460 = CARTESIAN_POINT ( 'NONE',  ( 9.262725409949998934, -4.818302824158000597, -8.808202952968999355 ) ) ;
#7461 = CARTESIAN_POINT ( 'NONE',  ( 25.40241868561099992, 11.40895027791000160, 3.011581611870999708 ) ) ;
#7462 = VERTEX_POINT ( 'NONE', #59409 ) ;
#7463 = CARTESIAN_POINT ( 'NONE',  ( 24.69847945454000282, -12.37231998179999870, -2.942481676297000082 ) ) ;
#7464 = CARTESIAN_POINT ( 'NONE',  ( 12.08472014176157394, 0.08359636179363652553, -13.99975542440154719 ) ) ;
#7465 = CARTESIAN_POINT ( 'NONE',  ( 5.700000000000000178, -13.04986661130000059, 1.811520473896000016 ) ) ;
#7466 = DIRECTION ( 'NONE',  ( 0.000000000000000000, -0.8077502949377767250, 0.5895247755844827964 ) ) ;
#7467 = CARTESIAN_POINT ( 'NONE',  ( 3.500000000000000444, -2.306765131595603258, 2.202630344077171287 ) ) ;
#7468 = DIRECTION ( 'NONE',  ( 0.000000000000000000, -1.000000000000000000, 0.000000000000000000 ) ) ;
#7469 = CARTESIAN_POINT ( 'NONE',  ( 13.15534550153200044, 12.11329499872000071, 2.052871598439000245 ) ) ;
#7470 = EDGE_LOOP ( 'NONE', ( #31768, #67954, #52884, #4898 ) ) ;
#7471 = DIRECTION ( 'NONE',  ( 0.000000000000000000, 0.000000000000000000, -1.000000000000000000 ) ) ;
#7472 = CARTESIAN_POINT ( 'NONE',  ( 17.87830683576860125, 3.171613455744695109, -13.63601469363850249 ) ) ;
#7473 = ORIENTED_EDGE ( 'NONE', *, *, #4469, .F. ) ;
#7474 = DIRECTION ( 'NONE',  ( 0.000000000000000000, 0.000000000000000000, 1.000000000000000000 ) ) ;
#7475 = CARTESIAN_POINT ( 'NONE',  ( 24.98038038036339969, 8.548001386182342287, -8.348258811873629170 ) ) ;
#7476 = CARTESIAN_POINT ( 'NONE',  ( 9.649770280412001355, 4.042991257420999851, -5.768106221333000327 ) ) ;
#7477 = EDGE_CURVE ( 'NONE', #20699, #5868, #36090, .T. ) ;
#7478 = CARTESIAN_POINT ( 'NONE',  ( 11.10000000000000142, -2.933222718292388898, -8.703884637941042612 ) ) ;
#7479 = EDGE_CURVE ( 'NONE', #53059, #24256, #28312, .T. ) ;
#7480 = CARTESIAN_POINT ( 'NONE',  ( 11.05435090131019926, -2.880552878538999995, -8.192386390235398608 ) ) ;
#7481 = CARTESIAN_POINT ( 'NONE',  ( 18.11245859367112132, 0.2828884610753772400, -12.69576253191497983 ) ) ;
#7482 = EDGE_CURVE ( 'NONE', #51100, #5246, #60112, .T. ) ;
#7483 = CARTESIAN_POINT ( 'NONE',  ( 10.95833333333531634, -4.952949899268980438, 8.562434272073259578 ) ) ;
#7484 = ORIENTED_EDGE ( 'NONE', *, *, #53664, .F. ) ;
#7485 = CYLINDRICAL_SURFACE ( 'NONE', #53278, 3.500000000000000000 ) ;
#7486 = CARTESIAN_POINT ( 'NONE',  ( 18.16706615800142544, -2.626761369726613005, -13.64570327821840579 ) ) ;
#7487 = CARTESIAN_POINT ( 'NONE',  ( 8.848264158775000610, 5.751585344281000545, -8.235867044345999588 ) ) ;
#7488 = EDGE_LOOP ( 'NONE', ( #41766, #52500, #33784, #50204 ) ) ;
#7489 = AXIS2_PLACEMENT_3D ( 'NONE', #29115, #3548, #14406 ) ;
#7490 = CARTESIAN_POINT ( 'NONE',  ( 9.858847045824999711, 2.668090821818000169, -7.206973500459000093 ) ) ;
#7491 = ORIENTED_EDGE ( 'NONE', *, *, #68326, .T. ) ;
#7492 = CARTESIAN_POINT ( 'NONE',  ( 8.672151519676999598, 4.021721698617580110, 6.495824366094999469 ) ) ;
#7493 = CARTESIAN_POINT ( 'NONE',  ( 18.06564745257667326, -2.991132176950372479, -12.23981809347030847 ) ) ;
#7494 = CARTESIAN_POINT ( 'NONE',  ( 9.643930206848999376, 5.250000000000000000, 7.500000000000000000 ) ) ;
#7495 = DIRECTION ( 'NONE',  ( 0.000000000000000000, -1.000000000000000000, 0.000000000000000000 ) ) ;
#7496 = CARTESIAN_POINT ( 'NONE',  ( 11.71278712779700015, -11.72302084951000190, -1.966028253584000129 ) ) ;
#7497 = AXIS2_PLACEMENT_3D ( 'NONE', #64328, #22384, #27644 ) ;
#7498 = CARTESIAN_POINT ( 'NONE',  ( 9.484696787962999309, 4.148886440911999429, 8.354131589521699652 ) ) ;
#7499 = CARTESIAN_POINT ( 'NONE',  ( 4.599999999999999645, 0.6250000000000001110, 13.88107975066923494 ) ) ;
#7500 = EDGE_LOOP ( 'NONE', ( #61739, #42826, #29328, #25414, #6143 ) ) ;
#7501 = CARTESIAN_POINT ( 'NONE',  ( 8.235184868407717573, -4.918172741149095195, 6.252519622020343171 ) ) ;
#7502 = CARTESIAN_POINT ( 'NONE',  ( 11.28109528040999976, 2.660125405577999924, -6.904121770750999865 ) ) ;
#7503 = FACE_OUTER_BOUND ( 'NONE', #38319, .T. ) ;
#7504 = CIRCLE ( 'NONE', #34324, 1.249999999999999778 ) ;
#7505 = CARTESIAN_POINT ( 'NONE',  ( 12.19498122944100515, 2.912558373969582171, -13.69368860183518066 ) ) ;
#7506 = CARTESIAN_POINT ( 'NONE',  ( 3.452384183491000069, 1.140396268832999827, -3.309002319436000317 ) ) ;
#7507 = CARTESIAN_POINT ( 'NONE',  ( 9.471368011205999693, -2.030678448189000118, 7.549764202121000523 ) ) ;
#7508 = CARTESIAN_POINT ( 'NONE',  ( 17.63678025734559540, 0.6199690124688018722, 13.88138352397878705 ) ) ;
#7509 = CARTESIAN_POINT ( 'NONE',  ( 24.87965846251700341, -2.960046916869999656, 11.62351360425999935 ) ) ;
#7510 = ORIENTED_EDGE ( 'NONE', *, *, #9823, .F. ) ;
#7511 = EDGE_LOOP ( 'NONE', ( #11837, #65314, #18952, #24131 ) ) ;
#7512 = CIRCLE ( 'NONE', #781, 13.89999852641999922 ) ;
#7513 = CARTESIAN_POINT ( 'NONE',  ( 9.643864158774000828, 2.927176851028000293, -5.932007155957999878 ) ) ;
#7514 = CARTESIAN_POINT ( 'NONE',  ( 12.26182380061670152, 0.3097576186857741720, 13.89536933047994083 ) ) ;
#7515 = CARTESIAN_POINT ( 'NONE',  ( 12.19113298427591552, -2.617185168745339574, 13.64790684748871818 ) ) ;
#7516 = CARTESIAN_POINT ( 'NONE',  ( 9.164312934263135091, -5.579507257161629319, 6.755493088102384469 ) ) ;
#7517 = CARTESIAN_POINT ( 'NONE',  ( 8.860769353209001054, -2.935738482289000029, 6.259841087764999479 ) ) ;
#7518 = DIRECTION ( 'NONE',  ( 0.000000000000000000, 0.000000000000000000, 1.000000000000000000 ) ) ;
#7520 = CARTESIAN_POINT ( 'NONE',  ( 11.07074853682000004, -6.638037936241000025, 5.577182366698000493 ) ) ;
#7519 = CARTESIAN_POINT ( 'NONE',  ( 10.15903849359899880, -3.074215132699300135, 8.382783533462799141 ) ) ;
#7521 = CARTESIAN_POINT ( 'NONE',  ( 10.39503166480599994, 2.725152142215999884, -7.589885038193400213 ) ) ;
#7522 = ORIENTED_EDGE ( 'NONE', *, *, #30336, .T. ) ;
#7523 = CARTESIAN_POINT ( 'NONE',  ( 7.335819197764073429, 2.649620978275905703, -7.146853263626653074 ) ) ;
#7524 = EDGE_CURVE ( 'NONE', #38985, #48366, #12527, .T. ) ;
#7525 = CARTESIAN_POINT ( 'NONE',  ( 11.08558905797000094, -2.762729330199000355, -5.050875529400999930 ) ) ;
#7526 = CARTESIAN_POINT ( 'NONE',  ( 17.96738117868769535, 0.4698014501121438591, 12.68830453558791405 ) ) ;
#7527 = CARTESIAN_POINT ( 'NONE',  ( 12.58522439494062084, -0.5851582065386651266, 12.68184838022285099 ) ) ;
#7528 = ADVANCED_FACE ( 'NONE', ( #50573 ), #55824, .F. ) ;
#7529 = DIRECTION ( 'NONE',  ( 0.000000000000000000, 1.000000000000000000, 0.000000000000000000 ) ) ;
#7530 = ORIENTED_EDGE ( 'NONE', *, *, #66129, .F. ) ;
#7532 = CARTESIAN_POINT ( 'NONE',  ( 10.91991225946278199, 4.700767082376348327, 8.022508467459166681 ) ) ;
#7531 = CARTESIAN_POINT ( 'NONE',  ( 9.316120559621998254, -3.677416446733000388, 9.250734868033999803 ) ) ;
#7533 = CARTESIAN_POINT ( 'NONE',  ( 9.848670280409999478, 5.002683760508999988, -8.912673867568997821 ) ) ;
#7534 = CARTESIAN_POINT ( 'NONE',  ( 12.42175510762291779, -2.005905104281934470, 13.76592701692032783 ) ) ;
#7535 = B_SPLINE_CURVE_WITH_KNOTS ( 'NONE', 3,
 ( #18911, #51066, #8762, #3169 ),
 .UNSPECIFIED., .F., .F.,
 ( 4, 4 ),
 ( 0.000000000000000000, 1.000000000000000000 ),
 .UNSPECIFIED. ) ;
#7536 = CARTESIAN_POINT ( 'NONE',  ( 10.73964560330029983, 4.391636236366600166, 8.716526793355999558 ) ) ;
#7537 = VECTOR ( 'NONE', #33347, 1000.000000000000000 ) ;
#7538 = FACE_OUTER_BOUND ( 'NONE', #42085, .T. ) ;
#7539 = MECHANICAL_DESIGN_GEOMETRIC_PRESENTATION_REPRESENTATION (  '', ( #48873 ), #62246 ) ;
#7540 = CARTESIAN_POINT ( 'NONE',  ( 9.355690472842169925, 3.345172699598239596, 9.147100720064839763 ) ) ;
#7541 = CARTESIAN_POINT ( 'NONE',  ( 2.213837056856000185, 1.294680128176000089, 3.350772176593999951 ) ) ;
#7542 = ORIENTED_EDGE ( 'NONE', *, *, #3791, .F. ) ;
#7543 = CARTESIAN_POINT ( 'NONE',  ( 12.12622238209132419, 0.2528603812084147529, -12.59746735456352873 ) ) ;
#7544 = CARTESIAN_POINT ( 'NONE',  ( 12.33152592714634288, -2.090072125112540036, -12.53771354782229963 ) ) ;
#7545 = CARTESIAN_POINT ( 'NONE',  ( 23.78804302077149302, -13.03937298471759654, -3.724210977727982819 ) ) ;
#7547 = FACE_OUTER_BOUND ( 'NONE', #9975, .T. ) ;
#7546 = VECTOR ( 'NONE', #14577, 1000.000000000000000 ) ;
#7548 = VERTEX_POINT ( 'NONE', #24347 ) ;
#7549 = CARTESIAN_POINT ( 'NONE',  ( 5.499803308717000405, -1.431922326323000094, -0.3257311615064000243 ) ) ;
#7550 = B_SPLINE_CURVE_WITH_KNOTS ( 'NONE', 3,
 ( #4445, #68415, #15297, #19164 ),
 .UNSPECIFIED., .F., .F.,
 ( 4, 4 ),
 ( 0.000000000000000000, 1.000000000000000000 ),
 .UNSPECIFIED. ) ;
#7551 = B_SPLINE_CURVE_WITH_KNOTS ( 'NONE', 3,
 ( #12668, #29108, #66143, #56006, #18261, #8113, #55315, #60905, #18607, #39581, #39236, #60217, #39933, #38540, #6720, #22452, #60561, #50075 ),
 .UNSPECIFIED., .F., .F.,
 ( 4, 2, 2, 2, 2, 2, 2, 2, 4 ),
 ( 0.1494581667962507632, 0.2557758959467194004, 0.3620936250971880654, 0.4684113542476566749, 0.5747290833981253400, 0.6810468125485940050, 0.7873645416990626700, 0.8936822708495313350, 1.000000000000000000 ),
 .UNSPECIFIED. ) ;
#7552 = CARTESIAN_POINT ( 'NONE',  ( 7.938110841225999970, 3.563552687850000122, -6.172381771908999504 ) ) ;
#7554 = CARTESIAN_POINT ( 'NONE',  ( 9.073148997461000675, -5.167567567567999731, -6.822293592207000934 ) ) ;
#7553 = CARTESIAN_POINT ( 'NONE',  ( 8.579433303903055474, -4.102305646687347540, 5.763126848776402689 ) ) ;
#7555 = CONICAL_SURFACE ( 'NONE', #36554, 1.150083888163000223, 0.7854614995501695285 ) ;
#7556 = CARTESIAN_POINT ( 'NONE',  ( 10.67375944625267614, -4.674697381537265883, -8.055763479958521600 ) ) ;
#7557 = VERTEX_POINT ( 'NONE', #65343 ) ;
#7558 =( NAMED_UNIT ( * ) SI_UNIT ( $, .STERADIAN. ) SOLID_ANGLE_UNIT ( ) );
#7559 = ORIENTED_EDGE ( 'NONE', *, *, #23517, .F. ) ;
#7560 = CARTESIAN_POINT ( 'NONE',  ( 9.488131779409266997, -4.942974209866618729, 8.465868502208129698 ) ) ;
#7561 = CARTESIAN_POINT ( 'NONE',  ( 16.27289819560299833, 3.403267206945999934, 11.10251878130000058 ) ) ;
#7562 = CARTESIAN_POINT ( 'NONE',  ( 18.27544000105305599, 0.08309727575449966930, -13.99975851644561686 ) ) ;
#7563 = B_SPLINE_CURVE_WITH_KNOTS ( 'NONE', 3,
 ( #51998, #4102, #25437, #61475 ),
 .UNSPECIFIED., .F., .F.,
 ( 4, 4 ),
 ( 0.000000000000000000, 1.000000000000000000 ),
 .UNSPECIFIED. ) ;
#7564 = ORIENTED_EDGE ( 'NONE', *, *, #68206, .T. ) ;
#7565 = CARTESIAN_POINT ( 'NONE',  ( 10.98895755164048005, 7.482542893969703179, -6.234366245063336365 ) ) ;
#7566 = EDGE_CURVE ( 'NONE', #12398, #45043, #59541, .T. ) ;
#7567 = CARTESIAN_POINT ( 'NONE',  ( 10.64393020684899938, -2.750000000000000000, 7.500000000000000000 ) ) ;
#7568 = AXIS2_PLACEMENT_3D ( 'NONE', #62773, #41807, #14213 ) ;
#7569 = CARTESIAN_POINT ( 'NONE',  ( 7.938589158768999177, 3.517942668285999996, -6.188254172171000711 ) ) ;
#7570 = DIRECTION ( 'NONE',  ( -1.000000000000000000, 0.000000000000000000, -9.837659932951999203E-14 ) ) ;
#7571 = EDGE_CURVE ( 'NONE', #33283, #23956, #38436, .T. ) ;
#7572 = CARTESIAN_POINT ( 'NONE',  ( 8.620740978634000129, -4.599999999999999645, 5.898823289756999877 ) ) ;
#7573 = ORIENTED_EDGE ( 'NONE', *, *, #9709, .F. ) ;
#7574 = CARTESIAN_POINT ( 'NONE',  ( 9.091114158770999154, 3.762712042852999872, 8.787816121229999666 ) ) ;
#7575 = ADVANCED_FACE ( 'NONE', ( #35192 ), #27605, .F. ) ;
#7576 = CARTESIAN_POINT ( 'NONE',  ( 12.42368232297769204, -2.995580128734608660, -13.55572452362624425 ) ) ;
#7577 = PRESENTATION_STYLE_ASSIGNMENT (( #2676 ) ) ;
#7578 = LINE ( 'NONE', #7929, #49338 ) ;
#7579 = B_SPLINE_CURVE_WITH_KNOTS ( 'NONE', 3,
 ( #45516, #3532, #66826, #51097 ),
 .UNSPECIFIED., .F., .F.,
 ( 4, 4 ),
 ( 0.000000000000000000, 1.000000000000000000 ),
 .UNSPECIFIED. ) ;
#7580 = ORIENTED_EDGE ( 'NONE', *, *, #960, .F. ) ;
#7581 = DIRECTION ( 'NONE',  ( 1.000000000000000000, 0.000000000000000000, 0.000000000000000000 ) ) ;
#7582 = CARTESIAN_POINT ( 'NONE',  ( 8.923129650240841926, -4.658877085170329835, -6.641242496392400163 ) ) ;
#7583 = CARTESIAN_POINT ( 'NONE',  ( 10.92594639468418194, 2.912972570981688492, -4.995424234945515352 ) ) ;
#7584 = CARTESIAN_POINT ( 'NONE',  ( 23.85847252464887802, -3.325664090202163248, -13.01555661423517485 ) ) ;
#7585 = DIRECTION ( 'NONE',  ( 1.000000000000000000, 0.000000000000000000, 0.000000000000000000 ) ) ;
#7586 = CARTESIAN_POINT ( 'NONE',  ( 6.055026506350000837, -1.500000000000000000, 0.000000000000000000 ) ) ;
#7587 = CONICAL_SURFACE ( 'NONE', #37726, 13.94999927503000059, 0.7853981058017837080 ) ;
#7588 = CARTESIAN_POINT ( 'NONE',  ( 17.79082714041179969, -1.799831594964177661, 12.47079078729190904 ) ) ;
#7589 = ORIENTED_EDGE ( 'NONE', *, *, #20910, .T. ) ;
#7590 = CARTESIAN_POINT ( 'NONE',  ( 11.68788784977535933, -4.985985832792199979, -7.443657794094239222 ) ) ;
#7591 = ORIENTED_EDGE ( 'NONE', *, *, #15083, .F. ) ;
#7592 = ADVANCED_FACE ( 'NONE', ( #2675 ), #358, .T. ) ;
#7593 = CARTESIAN_POINT ( 'NONE',  ( 0.1499942179680000542, -2.749953718116144863, 0.3599680999393964353 ) ) ;
#7594 = CARTESIAN_POINT ( 'NONE',  ( 8.699089158774000907, 4.178200486578000472, -5.608493638783999202 ) ) ;
#7595 = CARTESIAN_POINT ( 'NONE',  ( 3.083239578446000273, -1.700413634830000076, -2.728580140816999844 ) ) ;
#7596 = CARTESIAN_POINT ( 'NONE',  ( 9.831596185961002377, -3.539228349258999984, -8.956015611440999891 ) ) ;
#7597 = AXIS2_PLACEMENT_3D ( 'NONE', #11231, #5980, #59817 ) ;
#7598 = CARTESIAN_POINT ( 'NONE',  ( 6.605026506349999771, -1.500000000000000000, 0.000000000000000000 ) ) ;
#7599 = CARTESIAN_POINT ( 'NONE',  ( 24.02995475322400054, 13.13684421285999981, 3.281205399872999973 ) ) ;
#7600 = CARTESIAN_POINT ( 'NONE',  ( 10.53521345716899837, 4.924890298941200228, -8.340879262988799780 ) ) ;
#7601 = VERTEX_POINT ( 'NONE', #43691 ) ;
#7602 = VECTOR ( 'NONE', #59369, 1000.000000000000000 ) ;
#7603 = CARTESIAN_POINT ( 'NONE',  ( 17.60000001287599858, 11.53033693765999779, -4.891431908114999949 ) ) ;
#7604 = CARTESIAN_POINT ( 'NONE',  ( 11.66641369783139837, -4.050626550392200542, 6.497808498716000081 ) ) ;
#7605 = CARTESIAN_POINT ( 'NONE',  ( 11.08992526467999973, 5.210543602612999869, 8.327598319864998544 ) ) ;
#7606 = CARTESIAN_POINT ( 'NONE',  ( 10.76087777166854131, -3.646736399437864762, -8.814656132371565533 ) ) ;
#7607 = DIRECTION ( 'NONE',  ( -1.070254833719000005E-12, -1.000000000000000000, 8.737453881089000797E-12 ) ) ;
#7608 = FACE_OUTER_BOUND ( 'NONE', #43895, .T. ) ;
#7609 = AXIS2_PLACEMENT_3D ( 'NONE', #48742, #1193, #22852 ) ;
#7610 = CARTESIAN_POINT ( 'NONE',  ( 11.70794988689359961, 4.455786710255300598, -8.393984925606600811 ) ) ;
#7611 = LINE ( 'NONE', #29992, #2327 ) ;
#7612 = CARTESIAN_POINT ( 'NONE',  ( 10.49288779216199785, 5.056118594996999782, -7.880862084500499520 ) ) ;
#7613 = CARTESIAN_POINT ( 'NONE',  ( 18.25212943717076541, -0.1980440493285358372, 12.59844852634975787 ) ) ;
#7614 = CARTESIAN_POINT ( 'NONE',  ( 5.805026506351000037, 1.500000000000000000, 0.000000000000000000 ) ) ;
#7615 = AXIS2_PLACEMENT_3D ( 'NONE', #63685, #54230, #21048 ) ;
#7616 = CARTESIAN_POINT ( 'NONE',  ( 0.8776366609678249997, 0.07532896536173545876, -3.521742350970665125 ) ) ;
#7617 = EDGE_CURVE ( 'NONE', #62212, #58209, #49172, .T. ) ;
#7618 = CARTESIAN_POINT ( 'NONE',  ( 10.22094528040999961, 2.563078870232999851, -8.004103956955001209 ) ) ;
#7619 = ORIENTED_EDGE ( 'NONE', *, *, #25356, .T. ) ;
#7620 = CARTESIAN_POINT ( 'NONE',  ( 8.271691940379001906, -5.629389383493999865, 8.631822608164000599 ) ) ;
#7621 = CARTESIAN_POINT ( 'NONE',  ( 18.26357562437058490, 2.673039206754507902, 13.74245258260623892 ) ) ;
#7622 = CARTESIAN_POINT ( 'NONE',  ( 23.89320776801300283, -2.594336453560998734, 11.06325219636999435 ) ) ;
#7623 = CARTESIAN_POINT ( 'NONE',  ( 10.34580110216399973, -5.090698144635000588, -6.833896451085399448 ) ) ;
#7624 = ORIENTED_EDGE ( 'NONE', *, *, #35410, .T. ) ;
#7625 = CARTESIAN_POINT ( 'NONE',  ( 17.88701341325399952, 3.642483061606999861, 12.02409215997000125 ) ) ;
#7627 = CARTESIAN_POINT ( 'NONE',  ( 9.212501735000000025, -4.358851904410700584, 6.723921629386799381 ) ) ;
#7626 = CARTESIAN_POINT ( 'NONE',  ( 8.745860841232000027, 4.178200486578000472, -5.608493638783999202 ) ) ;
#7628 = CARTESIAN_POINT ( 'NONE',  ( 9.926176658771000305, 4.356412802752999802, -9.313960415320000408 ) ) ;
#7629 = EDGE_LOOP ( 'NONE', ( #1695, #1355, #8209, #1460, #67568, #48005 ) ) ;
#7630 = CARTESIAN_POINT ( 'NONE',  ( 10.22398792753999963, 5.507894434963000130, 6.589802269404000157 ) ) ;
#7631 = DIRECTION ( 'NONE',  ( 0.000000000000000000, -1.000000000000000000, 0.000000000000000000 ) ) ;
#7632 = CARTESIAN_POINT ( 'NONE',  ( 11.58071932425156980, 3.832730087831799803, 6.371589232479998977 ) ) ;
#7633 = CARTESIAN_POINT ( 'NONE',  ( 10.39106278671000005, -4.025320977579999848, 9.261121875182000807 ) ) ;
#7634 = CARTESIAN_POINT ( 'NONE',  ( 7.415011787918005304, 3.233093659812002585, 6.479723185591006462 ) ) ;
#7635 = ORIENTED_EDGE ( 'NONE', *, *, #15398, .F. ) ;
#7636 = CARTESIAN_POINT ( 'NONE',  ( 27.64127793187000037, 5.599999999999999645, -6.571291218949999902 ) ) ;
#7637 = CARTESIAN_POINT ( 'NONE',  ( 1.271806799208249794, -3.408904368339104263, -0.9161175952574814874 ) ) ;
#7638 = B_SPLINE_CURVE_WITH_KNOTS ( 'NONE', 3,
 ( #6434, #48752, #6092, #6784, #44216, #17982, #65511, #37912 ),
 .UNSPECIFIED., .F., .F.,
 ( 4, 2, 2, 4 ),
 ( 0.000000000000000000, 0.2500000000000000000, 0.5000000000000000000, 1.000000000000000000 ),
 .UNSPECIFIED. ) ;
#7639 = CARTESIAN_POINT ( 'NONE',  ( 7.965071509961973995, -2.295647626639265138, 7.153698218240838180 ) ) ;
#7640 = CARTESIAN_POINT ( 'NONE',  ( 10.74609562913000005, -4.263104965433000437, 9.276976808608999647 ) ) ;
#7641 = CARTESIAN_POINT ( 'NONE',  ( 11.68277869730536977, -4.531392946702499813, -6.452143920160000157 ) ) ;
#7642 = CARTESIAN_POINT ( 'NONE',  ( 9.425442991499998868, -4.063228561016970275, 8.502419298200999620 ) ) ;
#7643 = ORIENTED_EDGE ( 'NONE', *, *, #2538, .T. ) ;
#7644 = DIRECTION ( 'NONE',  ( 1.000000000000000000, 0.000000000000000000, 0.000000000000000000 ) ) ;
#7645 = CARTESIAN_POINT ( 'NONE',  ( 11.55964426047339977, -3.312306505177499805, 6.422784126663999338 ) ) ;
#7646 = EDGE_LOOP ( 'NONE', ( #6448, #41064, #57237, #20410, #7975, #65939, #64922, #22599, #43616, #55490 ) ) ;
#7647 = DIRECTION ( 'NONE',  ( -1.000000000000000000, 0.000000000000000000, 0.000000000000000000 ) ) ;
#7648 = ORIENTED_EDGE ( 'NONE', *, *, #23411, .T. ) ;
#7649 = CARTESIAN_POINT ( 'NONE',  ( 9.355720302797999821, -5.362859773739999447, -6.470306978669999154 ) ) ;
#7650 = CARTESIAN_POINT ( 'NONE',  ( 9.392285841233000809, 5.775964236216999836, -8.174909295649001706 ) ) ;
#7651 = AXIS2_PLACEMENT_3D ( 'NONE', #55097, #13829, #28537 ) ;
#7652 = DIRECTION ( 'NONE',  ( 0.000000000000000000, 0.000000000000000000, -1.000000000000000000 ) ) ;
#7653 = CARTESIAN_POINT ( 'NONE',  ( 8.281372984174815599, 5.064944289833863245, 6.454156656949499471 ) ) ;
#7654 = CARTESIAN_POINT ( 'NONE',  ( 12.55399154093075431, 1.927548249315100382, -12.56670145065455380 ) ) ;
#7655 = EDGE_CURVE ( 'NONE', #21434, #63258, #50053, .T. ) ;
#7656 = CARTESIAN_POINT ( 'NONE',  ( 11.81410538575740077, -3.024036709177600368, 7.733337754805098996 ) ) ;
#7657 = CARTESIAN_POINT ( 'NONE',  ( 11.44501463001509833, -3.527519786474400121, 8.256737112932800216 ) ) ;
#7658 = ADVANCED_FACE ( 'NONE', ( #62429 ), #14548, .T. ) ;
#7659 = ORIENTED_EDGE ( 'NONE', *, *, #18538, .F. ) ;
#7660 = CARTESIAN_POINT ( 'NONE',  ( 7.560652572975699037, 4.656871241626066471, 8.697129146950519640 ) ) ;
#7661 = AXIS2_PLACEMENT_3D ( 'NONE', #52698, #35349, #26482 ) ;
#7662 = EDGE_LOOP ( 'NONE', ( #30546, #11248, #56079, #66465, #41623, #6636, #8140 ) ) ;
#7663 = CARTESIAN_POINT ( 'NONE',  ( 8.829019353210000531, -5.290204991635000020, 8.768102264518001121 ) ) ;
#7664 = CARTESIAN_POINT ( 'NONE',  ( 25.39991507554827521, -8.680020025995577981, 7.390263434114647367 ) ) ;
#7665 = ORIENTED_EDGE ( 'NONE', *, *, #56672, .F. ) ;
#7666 = CARTESIAN_POINT ( 'NONE',  ( 12.11673986888017929, -2.253747544392083135, -12.39680392560332223 ) ) ;
#7667 = CARTESIAN_POINT ( 'NONE',  ( 11.06379841651039797, 3.598362324325699912, 6.432302808027999141 ) ) ;
#7668 = CARTESIAN_POINT ( 'NONE',  ( 10.26694555961999988, -5.500014128486999887, -6.419508248405999318 ) ) ;
#7669 = CARTESIAN_POINT ( 'NONE',  ( 10.79184687351629535, 3.000416447002276943, 8.268183399968645375 ) ) ;
#7670 = AXIS2_PLACEMENT_3D ( 'NONE', #12659, #33991, #28399 ) ;
#7671 = CARTESIAN_POINT ( 'NONE',  ( 18.36455407565900089, -12.06439799272000002, 3.505004330567000004 ) ) ;
#7672 = DIRECTION ( 'NONE',  ( 1.000000000000000000, 0.000000000000000000, 0.000000000000000000 ) ) ;
#7673 = DIRECTION ( 'NONE',  ( -1.000000000000000000, 0.000000000000000000, 0.000000000000000000 ) ) ;
#7674 = CARTESIAN_POINT ( 'NONE',  ( 18.17005379958825273, -0.1118057330073155969, -12.69934308675517620 ) ) ;
#7675 = CARTESIAN_POINT ( 'NONE',  ( 17.55505043854144276, 0.000000000000000000, -25.00000000000000000 ) ) ;
#7676 = CARTESIAN_POINT ( 'NONE',  ( 10.05862282008599884, -3.333723918618700210, -8.574682153725998290 ) ) ;
#7677 = CARTESIAN_POINT ( 'NONE',  ( 7.866204719590000671, 4.580608786027000612, 9.213365309690999538 ) ) ;
#7678 = ORIENTED_EDGE ( 'NONE', *, *, #2438, .F. ) ;
#7679 = EDGE_CURVE ( 'NONE', #57810, #22584, #47739, .T. ) ;
#7680 = B_SPLINE_CURVE_WITH_KNOTS ( 'NONE', 3,
 ( #66574, #34780, #8198, #19028, #13792, #24624, #56438, #8539, #29889, #51197, #3290, #58834, #53246, #63727, #63030, #4313 ),
 .UNSPECIFIED., .F., .F.,
 ( 4, 2, 2, 2, 2, 2, 2, 4 ),
 ( 0.000000000000000000, 0.06250000000000055511, 0.1250000000000011102, 0.2500000000000009437, 0.3750000000000007772, 0.5000000000000005551, 0.7500000000000003331, 1.000000000000000000 ),
 .UNSPECIFIED. ) ;
#7681 = CIRCLE ( 'NONE', #64599, 0.6999999999999992895 ) ;
#7682 = FILL_AREA_STYLE_COLOUR ( '', #51117 ) ;
#7683 = DIRECTION ( 'NONE',  ( 0.000000000000000000, 2.692747184616903860E-07, -0.9999999999999636957 ) ) ;
#7684 = CARTESIAN_POINT ( 'NONE',  ( 7.319425230799852855, 3.475664936878117839, 6.226553775891153109 ) ) ;
#7685 = CARTESIAN_POINT ( 'NONE',  ( 23.61357289147300165, -3.134997397370999916, 13.53670803788000043 ) ) ;
#7686 = ADVANCED_FACE ( 'NONE', ( #35867 ), #26064, .F. ) ;
#7687 = CARTESIAN_POINT ( 'NONE',  ( 17.75782926003066819, 1.908786995103509021, 12.56982197457662842 ) ) ;
#7688 = CARTESIAN_POINT ( 'NONE',  ( 18.40156003475500057, 3.148349829928000165, -12.06792178657999948 ) ) ;
#7689 = CARTESIAN_POINT ( 'NONE',  ( 9.349999778958000718, -4.000000000000000000, 7.500000000000000000 ) ) ;
#7690 = CARTESIAN_POINT ( 'NONE',  ( 11.56493925477931306, -2.826469659297513370, -7.948835763880663485 ) ) ;
#7691 = CARTESIAN_POINT ( 'NONE',  ( 8.706426979769998908, 3.641148095589300304, 6.723921629386799381 ) ) ;
#7692 = ORIENTED_EDGE ( 'NONE', *, *, #66861, .T. ) ;
#7693 = CARTESIAN_POINT ( 'NONE',  ( 12.61213290433104106, -1.905496177770261479, 12.57041190218061644 ) ) ;
#7694 = CARTESIAN_POINT ( 'NONE',  ( 10.05826717315599872, -4.659895246859299789, -6.937642277832399174 ) ) ;
#7695 = CARTESIAN_POINT ( 'NONE',  ( 11.29622358543999994, 3.561657733933999648, 6.266050246368000565 ) ) ;
#7696 = CARTESIAN_POINT ( 'NONE',  ( 4.600000533658372248, 13.89999946622000060, 2.316961247309999772E-09 ) ) ;
#7697 = B_SPLINE_CURVE_WITH_KNOTS ( 'NONE', 3,
 ( #5283, #53532, #64341, #26965, #16458, #10190, #53186, #15778, #22044, #5967, #57731, #47256, #27305, #68910, #20681, #31187, #58087, #732, #15093, #36417, #42012, #15441, #36766, #52842, #4937, #26277 ),
 .UNSPECIFIED., .F., .F.,
 ( 4, 2, 2, 2, 2, 2, 2, 2, 2, 2, 2, 2, 4 ),
 ( 0.000000000000000000, 0.06249999999999739098, 0.09374999999999711342, 0.1249999999999968359, 0.2499999999999964473, 0.3749999999999960032, 0.4999999999999955591, 0.6249999999999951150, 0.7499999999999946709, 0.8124999999999942268, 0.8437499999999948930, 0.8749999999999954481, 1.000000000000000000 ),
 .UNSPECIFIED. ) ;
#7698 = CARTESIAN_POINT ( 'NONE',  ( 11.61759063708296047, 5.217265640542000149, -7.842242470354300110 ) ) ;
#7699 = CARTESIAN_POINT ( 'NONE',  ( 12.11457469949691834, -0.2196334679052307781, 12.59809060309703277 ) ) ;
#7700 = CARTESIAN_POINT ( 'NONE',  ( 8.251329719592000345, 5.773189794777000117, 7.141495931231999883 ) ) ;
#7701 = CARTESIAN_POINT ( 'NONE',  ( 9.380783851237000093, 2.204242311415999911, 7.545378292079000460 ) ) ;
#7702 = VECTOR ( 'NONE', #49826, 1000.000000000000114 ) ;
#7703 = CARTESIAN_POINT ( 'NONE',  ( 12.76340515712443491, 1.876302067334184809, 12.57520337466226223 ) ) ;
#7704 = ADVANCED_FACE ( 'NONE', ( #51594, #52285 ), #20813, .T. ) ;
#7705 = EDGE_LOOP ( 'NONE', ( #46413, #26130, #32641, #18078, #23436, #52952 ) ) ;
#7706 = CARTESIAN_POINT ( 'NONE',  ( 9.933354719590999693, 5.639765292528999829, -8.059103558718000215 ) ) ;
#7707 = CARTESIAN_POINT ( 'NONE',  ( 11.55194988689359903, 4.580487242693600081, -8.638573882912000457 ) ) ;
#7708 = DIRECTION ( 'NONE',  ( 1.000000000000000000, 0.000000000000000000, 0.000000000000000000 ) ) ;
#7710 = CARTESIAN_POINT ( 'NONE',  ( 17.81145623641422304, -0.5702806495523290442, 12.68276204030464349 ) ) ;
#7709 = CARTESIAN_POINT ( 'NONE',  ( 9.010191940380000375, -5.040796345420999636, 8.522966281393001609 ) ) ;
#7711 = CARTESIAN_POINT ( 'NONE',  ( 10.59058376188600015, -4.847012523549299345, 6.960174024681499816 ) ) ;
#7712 = CARTESIAN_POINT ( 'NONE',  ( 10.77672335273219950, -3.698477709264200275, -8.312023951944400579 ) ) ;
#7713 = ORIENTED_EDGE ( 'NONE', *, *, #24719, .F. ) ;
#7714 = CARTESIAN_POINT ( 'NONE',  ( 1.686929392597000144, -1.310877008326999826, -3.164872840607000359 ) ) ;
#7715 = CARTESIAN_POINT ( 'NONE',  ( 12.71442162208154691, 11.86191914805647230, -3.298674357357656906 ) ) ;
#7716 = CARTESIAN_POINT ( 'NONE',  ( 9.376902336861421716, -3.730411824524082931, 8.499844062317453819 ) ) ;
#7717 = CARTESIAN_POINT ( 'NONE',  ( 18.29999330150736014, 11.02846243710159868, -3.754394858750199848 ) ) ;
#7718 = CARTESIAN_POINT ( 'NONE',  ( 24.50399615207700066, -12.34862307763000011, 3.085465605386000121 ) ) ;
#7719 = FACE_OUTER_BOUND ( 'NONE', #50103, .T. ) ;
#7720 = CARTESIAN_POINT ( 'NONE',  ( 7.000000000000000000, -9.370210309074998634, 5.370210309075000410 ) ) ;
#7721 = CARTESIAN_POINT ( 'NONE',  ( 7.100000000000000533, -11.84999999999999964, 0.000000000000000000 ) ) ;
#7722 = CARTESIAN_POINT ( 'NONE',  ( 7.936333771302000351, 5.123034328734999754, 6.721303713258000023 ) ) ;
#7723 = ORIENTED_EDGE ( 'NONE', *, *, #10751, .F. ) ;
#7724 = CARTESIAN_POINT ( 'NONE',  ( 9.566490007895001924, 4.108964550738000376, 8.851615252874999840 ) ) ;
#7725 = CARTESIAN_POINT ( 'NONE',  ( 10.95282897519000009, 5.154323752254000190, 5.175250089408000242 ) ) ;
#7726 = CARTESIAN_POINT ( 'NONE',  ( 18.02726358174409782, 2.088564957010012435, -13.75219797956691714 ) ) ;
#7727 = CARTESIAN_POINT ( 'NONE',  ( 7.000000000000000000, 6.255435840762999966, -3.000000000000000000 ) ) ;
#7728 = CARTESIAN_POINT ( 'NONE',  ( 0.5718663363677000122, 2.877489654231000227, -1.904074875451999826 ) ) ;
#7729 = EDGE_LOOP ( 'NONE', ( #14112, #23245, #37244, #33535 ) ) ;
#7730 = CARTESIAN_POINT ( 'NONE',  ( 1.917640132539666808, 1.762666431298152370, -3.058252359239900464 ) ) ;
#7731 = CARTESIAN_POINT ( 'NONE',  ( 10.72614816446315267, -5.074971087576590989, 5.079084875746824324 ) ) ;
#7732 = CARTESIAN_POINT ( 'NONE',  ( 9.664757945270775252, -2.782574339883951087, 7.827174490145253571 ) ) ;
#7733 = CARTESIAN_POINT ( 'NONE',  ( 10.67410807141119911, 4.046361247106100123, 6.497602131078999754 ) ) ;
#7734 = CARTESIAN_POINT ( 'NONE',  ( 11.59999999999999964, -4.817420948848700313, -7.174999999999999822 ) ) ;
#7735 = CARTESIAN_POINT ( 'NONE',  ( 18.30003129332100187, -2.732683818840999646, -11.53064095373000164 ) ) ;
#7736 = CARTESIAN_POINT ( 'NONE',  ( 17.55505043854147118, -3.125000000000000000, 12.28374638332999780 ) ) ;
#7737 = CARTESIAN_POINT ( 'NONE',  ( 9.694386075239211920, 4.746878242517505342, -8.656463215293298319 ) ) ;
#7738 = ADVANCED_FACE ( 'NONE', ( #46707 ), #3691, .F. ) ;
#7739 = CARTESIAN_POINT ( 'NONE',  ( 12.43937386265613476, -3.007228867393120897, 12.31882001147781658 ) ) ;
#7740 = EDGE_CURVE ( 'NONE', #59934, #60441, #26647, .T. ) ;
#7741 = CARTESIAN_POINT ( 'NONE',  ( 8.602991695318323195, 4.582460011752433005, 5.856014114908588475 ) ) ;
#7742 = ORIENTED_EDGE ( 'NONE', *, *, #19397, .T. ) ;
#7743 = EDGE_CURVE ( 'NONE', #20902, #37580, #30624, .T. ) ;
#7744 = B_SPLINE_CURVE_WITH_KNOTS ( 'NONE', 3,
 ( #69038, #21825, #58545, #43158 ),
 .UNSPECIFIED., .F., .F.,
 ( 4, 4 ),
 ( 0.000000000000000000, 1.000000000000000000 ),
 .UNSPECIFIED. ) ;
#7745 = CARTESIAN_POINT ( 'NONE',  ( 18.02597764372135813, -3.073197451853428408, 13.65853278380549085 ) ) ;
#7746 = CARTESIAN_POINT ( 'NONE',  ( 10.46887750876899936, -4.692271380433699512, -8.574279626736998949 ) ) ;
#7747 = VERTEX_POINT ( 'NONE', #47392 ) ;
#7748 = ORIENTED_EDGE ( 'NONE', *, *, #51855, .T. ) ;
#7749 = CARTESIAN_POINT ( 'NONE',  ( 24.66908130708416635, -3.147928273865472804, -11.83338230875681418 ) ) ;
#7750 = CARTESIAN_POINT ( 'NONE',  ( 5.356683578904362086, -1.067991396972500784, -0.3776072067835719026 ) ) ;
#7751 = CARTESIAN_POINT ( 'NONE',  ( 7.000000000000000000, -0.2392304845412999981, 3.000000000000000000 ) ) ;
#7752 = DIRECTION ( 'NONE',  ( 0.000000000000000000, 0.000000000000000000, -1.000000000000000000 ) ) ;
#7753 = DIRECTION ( 'NONE',  ( 0.000000000000000000, 0.000000000000000000, -1.000000000000000000 ) ) ;
#7754 = CARTESIAN_POINT ( 'NONE',  ( 9.716846873515667227, -3.231816600031351516, -6.500416447002277387 ) ) ;
#7755 = DIRECTION ( 'NONE',  ( 0.000000000000000000, 0.000000000000000000, 1.000000000000000000 ) ) ;
#7756 = FACE_OUTER_BOUND ( 'NONE', #37370, .T. ) ;
#7757 = CARTESIAN_POINT ( 'NONE',  ( 10.99570321855695099, 5.445259508076459198, -7.243346639199888415 ) ) ;
#7758 = CARTESIAN_POINT ( 'NONE',  ( 10.36409413284604497, -3.282837288405540122, -4.954046114881531793 ) ) ;
#7759 = ORIENTED_EDGE ( 'NONE', *, *, #1278, .T. ) ;
#7760 = EDGE_CURVE ( 'NONE', #34321, #55891, #8316, .T. ) ;
#7761 = CARTESIAN_POINT ( 'NONE',  ( 9.861802827889565748, 2.874603711571212639, -6.749639981086963836 ) ) ;
#7762 = DIRECTION ( 'NONE',  ( 0.000000000000000000, -1.000000000000000000, 0.000000000000000000 ) ) ;
#7763 = CARTESIAN_POINT ( 'NONE',  ( 10.26028798067999936, -4.571539164417999679, 4.531786735957999745 ) ) ;
#7764 = EDGE_CURVE ( 'NONE', #65548, #14966, #38328, .T. ) ;
#7765 = CARTESIAN_POINT ( 'NONE',  ( 9.051300837857860770, 5.190117543293265356, 7.276433888703319752 ) ) ;
#7766 = DIRECTION ( 'NONE',  ( 1.000000000000000000, 0.000000000000000000, 0.000000000000000000 ) ) ;
#7767 = CARTESIAN_POINT ( 'NONE',  ( 12.18524896721726769, 2.583003884521776872, 13.65547336762760189 ) ) ;
#7768 = CARTESIAN_POINT ( 'NONE',  ( 10.42595817177000050, -5.042180160032999403, 8.702227297563000619 ) ) ;
#7769 = ORIENTED_EDGE ( 'NONE', *, *, #41995, .F. ) ;
#7770 = CARTESIAN_POINT ( 'NONE',  ( 12.61465226482422608, 0.5953800883773135988, -12.68120857324976036 ) ) ;
#7771 = B_SPLINE_CURVE_WITH_KNOTS ( 'NONE', 3,
 ( #63095, #20121, #41451, #62759 ),
 .UNSPECIFIED., .F., .F.,
 ( 4, 4 ),
 ( 0.000000000000000000, 1.000000000000000000 ),
 .UNSPECIFIED. ) ;
#7772 = CARTESIAN_POINT ( 'NONE',  ( 12.34868974583248580, -0.4275223103465197738, 13.89116040406442565 ) ) ;
#7773 = ORIENTED_EDGE ( 'NONE', *, *, #43227, .F. ) ;
#7774 = FACE_OUTER_BOUND ( 'NONE', #65599, .T. ) ;
#7775 = CARTESIAN_POINT ( 'NONE',  ( 10.54885391751724022, -4.021057898797131713, 8.964616684112781897 ) ) ;
#7776 = AXIS2_PLACEMENT_3D ( 'NONE', #31716, #26121, #42545 ) ;
#7777 = CARTESIAN_POINT ( 'NONE',  ( 23.54916697122300207, -2.964289671590000008, -13.72170765701000050 ) ) ;
#7778 = CARTESIAN_POINT ( 'NONE',  ( 4.650000881942629505, 3.375077994860000042E-14, 1.048050535245999973E-13 ) ) ;
#7779 = B_SPLINE_SURFACE_WITH_KNOTS ( 'NONE', 3, 3, ( 
 ( #52914, #43465, #37861, #5357, #59185, #37514, #27037, #53252, #16190, #63732, #58496, #58839, #6039, #4659, #25998, #48349, #47329, #68986, #36837, #43109, #15163, #21099, #64072, #42424, #64412, #27376, #11286, #48703, #10598, #31940, #26696, #36485, #57807, #9915, #20753 ),
 ( #42080, #48011, #63390, #15512, #58156, #111, #21427, #42764, #44162, #28775, #28423, #16876, #1846, #17931, #39595, #49381, #22462, #27733, #64758, #22815, #54637, #23163, #65104, #39249, #7081, #13981, #23508, #44849, #6730, #30070, #60573, #11980, #65459, #38202, #3471 ),
 ( #28071, #60231, #66156, #1153, #12334, #38551, #33665, #44511, #35306, #65806, #56622, #33319, #12680, #54984, #11627, #49736, #59531, #34013, #18273, #60916, #59874, #32966, #2196, #55329, #7427, #1497, #50087, #54280, #8727, #6382, #49044, #17581, #51373, #24807, #43808 ),
 ( #38908, #17229, #63573, #62203, #35649, #10094, #56961, #14661, #67781, #31429, #46130, #62540, #25832, #41229, #26181, #37019, #57639, #14324, #31774, #52745, #35977, #51711, #63217, #15685, #5191, #36323, #20934, #58331, #68813, #9063, #15346, #4492, #30402, #57293, #9396 ) ),
 .UNSPECIFIED., .F., .F., .F.,
 ( 4, 4 ),
 ( 4, 1, 1, 1, 1, 1, 1, 1, 1, 1, 1, 1, 1, 1, 1, 1, 1, 1, 1, 1, 1, 1, 1, 1, 1, 1, 1, 1, 1, 1, 1, 1, 4 ),
 ( -0.1039370721279000015, 1.103937072127999963 ),
 ( -0.02000000000000000042, 0.01250000000000000069, 0.04499999999999999833, 0.07749999999999999944, 0.1100000000000000006, 0.1424999999999999878, 0.1749999999999999889, 0.2074999999999999900, 0.2399999999999999911, 0.2725000000000000200, 0.3049999999999999933, 0.3375000000000000222, 0.3699999999999999956, 0.4025000000000000244, 0.4349999999999999978, 0.4675000000000000266, 0.5000000000000000000, 0.5324999999999999734, 0.5649999999999999467, 0.5975000000000000311, 0.6300000000000000044, 0.6624999999999999778, 0.6949999999999999512, 0.7275000000000000355, 0.7600000000000000089, 0.7924999999999999822, 0.8249999999999999556, 0.8575000000000000400, 0.8900000000000000133, 0.9224999999999999867, 0.9549999999999999600, 0.9875000000000000444, 1.020000000000000018 ),
 .UNSPECIFIED. ) ;
#7780 = DIRECTION ( 'NONE',  ( 0.000000000000000000, -1.000000000000000000, 0.000000000000000000 ) ) ;
#7781 = CARTESIAN_POINT ( 'NONE',  ( 11.12723081016999949, 8.477322043720000977, -6.786959512705000641 ) ) ;
#7782 = CARTESIAN_POINT ( 'NONE',  ( 8.137846616029218438, 4.829271229625343054, -8.579069916537873652 ) ) ;
#7783 = FACE_OUTER_BOUND ( 'NONE', #5663, .T. ) ;
#7784 = CARTESIAN_POINT ( 'NONE',  ( 12.50326937753801992, 3.134539878383339584, 12.20388000700441999 ) ) ;
#7785 = CARTESIAN_POINT ( 'NONE',  ( 9.656157842586999607, -4.949038487346999915, -8.498994087616001281 ) ) ;
#7786 = CARTESIAN_POINT ( 'NONE',  ( 11.09672200990539892, 3.182132064022000328, -7.214709569664399247 ) ) ;
#7787 = CARTESIAN_POINT ( 'NONE',  ( 12.35923484894147251, -0.5750310236205122827, 12.58704914195723390 ) ) ;
#7788 = CARTESIAN_POINT ( 'NONE',  ( 10.29399293566599916, 4.546741702992100009, -8.170700474995699736 ) ) ;
#7789 = CARTESIAN_POINT ( 'NONE',  ( 9.328696787962998727, 4.196076320588900010, -6.375149554610999303 ) ) ;
#7791 = CARTESIAN_POINT ( 'NONE',  ( 10.85025860864000080, -2.931433838835999950, 5.153723152236999283 ) ) ;
#7790 = DIRECTION ( 'NONE',  ( -1.000000000000000000, 0.000000000000000000, 0.000000000000000000 ) ) ;
#7792 = CARTESIAN_POINT ( 'NONE',  ( 23.59396203638712919, -13.38681815648950035, 4.024094169786141428 ) ) ;
#7793 = ORIENTED_EDGE ( 'NONE', *, *, #26616, .F. ) ;
#7794 = CARTESIAN_POINT ( 'NONE',  ( 10.27427156480999848, -3.399999787207999447, 4.944156960757000618 ) ) ;
#7795 = CARTESIAN_POINT ( 'NONE',  ( 9.290195424034999760, -2.377814350880000038, 7.540992175424999999 ) ) ;
#7796 = EDGE_CURVE ( 'NONE', #56866, #54214, #22528, .T. ) ;
#7797 = ADVANCED_FACE ( 'NONE', ( #33032 ), #43171, .F. ) ;
#7798 = CARTESIAN_POINT ( 'NONE',  ( 9.655013376692998861, 3.104586782631499897, 7.955057656228099461 ) ) ;
#7799 = CARTESIAN_POINT ( 'NONE',  ( 10.71684687351633869, -3.231816600031351516, -6.500416447002277387 ) ) ;
#7800 = CARTESIAN_POINT ( 'NONE',  ( 9.228135700785001561, -2.875364528161000077, 8.669943154892999715 ) ) ;
#7801 = CARTESIAN_POINT ( 'NONE',  ( 12.37676482144652290, 2.955308392773305926, 13.56622858938220055 ) ) ;
#7802 = UNCERTAINTY_MEASURE_WITH_UNIT (LENGTH_MEASURE( 1.000000000000000082E-05 ), #48604, 'distance_accuracy_value', 'NONE');
#7803 = ORIENTED_EDGE ( 'NONE', *, *, #65075, .F. ) ;
#7804 = CARTESIAN_POINT ( 'NONE',  ( 9.784621437244998887, -3.241588663654300095, -6.646450532840099790 ) ) ;
#7805 = CARTESIAN_POINT ( 'NONE',  ( 9.791846873516668381, -4.999583552997724389, -6.731816600031356401 ) ) ;
#7806 = CARTESIAN_POINT ( 'NONE',  ( 5.772278627981999755, 0.9190761964769998960, -1.327642370976000130 ) ) ;
#7807 = CARTESIAN_POINT ( 'NONE',  ( 17.75579847504522135, 3.171737058802235776, -12.19426492080490831 ) ) ;
#7808 = CARTESIAN_POINT ( 'NONE',  ( 8.675212715831998267, -2.915713811628002361, -6.499218380552004071 ) ) ;
#7809 = CARTESIAN_POINT ( 'NONE',  ( 11.79999999771000141, -3.595163221087000149, 11.99793848941000007 ) ) ;
#7810 = CARTESIAN_POINT ( 'NONE',  ( 11.48641235500450009, 3.260080192309100067, -6.822158181405299615 ) ) ;
#7811 = CARTESIAN_POINT ( 'NONE',  ( 6.999998782146999332, 0.000000000000000000, 0.000000000000000000 ) ) ;
#7812 = CARTESIAN_POINT ( 'NONE',  ( 9.397313405920000307, -4.010297355695000121, -9.208122400763999238 ) ) ;
#7813 = CARTESIAN_POINT ( 'NONE',  ( 29.60000000000000142, 0.000000000000000000, 0.000000000000000000 ) ) ;
#7814 = ORIENTED_EDGE ( 'NONE', *, *, #65875, .T. ) ;
#7815 = CARTESIAN_POINT ( 'NONE',  ( 24.95408811465000198, -12.04589448677999997, -2.875991317726000140 ) ) ;
#7816 = CARTESIAN_POINT ( 'NONE',  ( 12.57146999070152127, -0.6916885356984082689, -13.98290438115173551 ) ) ;
#7817 = DIRECTION ( 'NONE',  ( 0.000000000000000000, -0.2588190451024932059, 0.9659258262890756397 ) ) ;
#7818 = EDGE_CURVE ( 'NONE', #1231, #32603, #10779, .T. ) ;
#7820 = EDGE_CURVE ( 'NONE', #35032, #7987, #56204, .T. ) ;
#7819 = B_SPLINE_CURVE_WITH_KNOTS ( 'NONE', 3,
 ( #56682, #45162, #18930, #8781, #60889, #40255, #13005, #34677, #30124, #3191, #66468, #67152, #40594, #23825, #51427, #34331, #3522, #55650 ),
 .UNSPECIFIED., .F., .F.,
 ( 4, 2, 2, 2, 2, 2, 2, 2, 4 ),
 ( 0.000000000000000000, 0.1249999999999996669, 0.2499999999999993339, 0.3749999999999990008, 0.4999999999999986677, 0.6249999999999990008, 0.7499999999999993339, 0.8749999999999996669, 1.000000000000000000 ),
 .UNSPECIFIED. ) ;
#7821 = FACE_OUTER_BOUND ( 'NONE', #67419, .T. ) ;
#7822 = AXIS2_PLACEMENT_3D ( 'NONE', #21243, #32093, #64222 ) ;
#7823 = CARTESIAN_POINT ( 'NONE',  ( 10.64393020684969926, -2.750000000000000000, -7.500000000000000000 ) ) ;
#7824 = CARTESIAN_POINT ( 'NONE',  ( 8.424364158774000799, 3.292387953886000140, -6.294868737226000377 ) ) ;
#7825 = CARTESIAN_POINT ( 'NONE',  ( 13.60156003475500164, 12.26415473033000048, 2.266572665737999870 ) ) ;
#7826 = ORIENTED_EDGE ( 'NONE', *, *, #39621, .T. ) ;
#7827 = EDGE_CURVE ( 'NONE', #28283, #9687, #10042, .T. ) ;
#7828 = B_SPLINE_CURVE_WITH_KNOTS ( 'NONE', 3,
 ( #24029, #18105, #17763, #28244 ),
 .UNSPECIFIED., .F., .F.,
 ( 4, 4 ),
 ( 0.000000000000000000, 1.000000000000000000 ),
 .UNSPECIFIED. ) ;
#7829 =( NAMED_UNIT ( * ) SI_UNIT ( $, .STERADIAN. ) SOLID_ANGLE_UNIT ( ) );
#7830 = CARTESIAN_POINT ( 'NONE',  ( 17.96192083627959590, 2.025460433975771579, -13.76272661095429406 ) ) ;
#7831 = ORIENTED_EDGE ( 'NONE', *, *, #27139, .T. ) ;
#7832 = DIRECTION ( 'NONE',  ( 0.000000000000000000, 1.000000000000000000, 0.000000000000000000 ) ) ;
#7833 = CARTESIAN_POINT ( 'NONE',  ( 2.728056799211040495, -2.150913519912213800, 2.798833948393621540 ) ) ;
#7834 = CARTESIAN_POINT ( 'NONE',  ( 8.266329719591000824, 4.769017407621999993, -8.862909124839001507 ) ) ;
#7835 = B_SPLINE_CURVE_WITH_KNOTS ( 'NONE', 3,
 ( #64485, #37585, #26772, #1224, #37248, #43875, #65181, #32358, #48084, #188, #37932, #64834, #6456, #16943, #38275, #42837, #16607, #27110, #21504, #54009, #11021, #59251, #11701, #27806, #11358, #42498, #63806, #64147, #6111, #33040 ),
 .UNSPECIFIED., .F., .F.,
 ( 4, 2, 1, 1, 2, 2, 2, 2, 2, 2, 2, 2, 2, 2, 2, 4 ),
 ( 0.000000000000000000, 0.1249999999999982792, 0.1874999999999971134, 0.2187499999999965583, 0.2343749999999966416, 0.2499999999999967248, 0.3749999999999978351, 0.4374999999999978906, 0.4999999999999980016, 0.5624999999999981126, 0.6249999999999982236, 0.6874999999999984457, 0.7499999999999985567, 0.8124999999999986677, 0.8749999999999987788, 1.000000000000000000 ),
 .UNSPECIFIED. ) ;
#7836 = CARTESIAN_POINT ( 'NONE',  ( 11.10000000000000320, -2.858656910680171581, -8.645179761462580714 ) ) ;
#7837 = CARTESIAN_POINT ( 'NONE',  ( 11.68277869730536977, -4.531392946702499813, -6.452143920160000157 ) ) ;
#7838 = CARTESIAN_POINT ( 'NONE',  ( 9.312954706844832842, -5.052526710679146049, -6.210582334949435790 ) ) ;
#7839 = CARTESIAN_POINT ( 'NONE',  ( 10.22726354018233152, -3.370476274536371442, 8.592232985442818105 ) ) ;
#7840 = ORIENTED_EDGE ( 'NONE', *, *, #60971, .T. ) ;
#7841 = DIRECTION ( 'NONE',  ( -1.000000000000000000, 0.000000000000000000, 0.000000000000000000 ) ) ;
#7842 = FACE_OUTER_BOUND ( 'NONE', #46897, .T. ) ;
#7843 = CARTESIAN_POINT ( 'NONE',  ( 8.897989158775001073, 4.990139824845000405, -9.121472988377998803 ) ) ;
#7844 = ORIENTED_EDGE ( 'NONE', *, *, #54778, .T. ) ;
#7845 = CARTESIAN_POINT ( 'NONE',  ( 10.65649893244999902, 5.448184228579000532, -7.015214795518000201 ) ) ;
#7846 = CARTESIAN_POINT ( 'NONE',  ( 10.98768491210000064, -8.067891622241001315, 6.818837029638999958 ) ) ;
#7847 = ORIENTED_EDGE ( 'NONE', *, *, #41512, .F. ) ;
#7848 = CARTESIAN_POINT ( 'NONE',  ( 9.379355082327998971, 3.488994418336600400, 8.521081653687000212 ) ) ;
#7849 = CARTESIAN_POINT ( 'NONE',  ( 18.25351233825843522, -2.286726172143648483, -12.39076325940497725 ) ) ;
#7850 = EDGE_CURVE ( 'NONE', #19641, #68613, #43525, .T. ) ;
#7851 = CARTESIAN_POINT ( 'NONE',  ( 5.500000000000000000, 13.94845324556000143, -4.312847325879000770 ) ) ;
#7852 = DIRECTION ( 'NONE',  ( 1.000000000000000000, 0.000000000000000000, 0.000000000000000000 ) ) ;
#7853 = FACE_OUTER_BOUND ( 'NONE', #14405, .T. ) ;
#7854 = B_SPLINE_CURVE_WITH_KNOTS ( 'NONE', 3,
 ( #2407, #23730, #45068, #66721 ),
 .UNSPECIFIED., .F., .F.,
 ( 4, 4 ),
 ( 0.000000000000000000, 1.000000000000000000 ),
 .UNSPECIFIED. ) ;
#7855 = CARTESIAN_POINT ( 'NONE',  ( 8.775480666858998191, 4.289077172771600388, 6.682599852064000423 ) ) ;
#7856 = CARTESIAN_POINT ( 'NONE',  ( 9.409633934533484734, -2.474451488929216403, 8.335641178190561718 ) ) ;
#7857 = EDGE_LOOP ( 'NONE', ( #17791, #42585, #22625, #62031, #54240 ) ) ;
#7858 = DIRECTION ( 'NONE',  ( 0.000000000000000000, -0.8676120656550951882, 0.4972416952847970584 ) ) ;
#7859 = CARTESIAN_POINT ( 'NONE',  ( 11.01605778040999972, 5.482856203356999636, -7.846408531951999166 ) ) ;
#7860 = CARTESIAN_POINT ( 'NONE',  ( 12.80505043854143388, 3.166036643249212634, -13.55322769257718996 ) ) ;
#7861 = CARTESIAN_POINT ( 'NONE',  ( 12.09654996457810050, 2.673023974430118521, -13.74245554503370670 ) ) ;
#7862 = CARTESIAN_POINT ( 'NONE',  ( 10.03897570133299944, -3.061513547538400104, -8.369268408503399925 ) ) ;
#7863 = CARTESIAN_POINT ( 'NONE',  ( 11.08992739829000129, -5.210546653347999602, 8.327600405525998895 ) ) ;
#7864 = CIRCLE ( 'NONE', #11194, 12.60000000000000142 ) ;
#7865 = CARTESIAN_POINT ( 'NONE',  ( 18.13088524799816881, -0.4443071882833248831, 13.99296005428181644 ) ) ;
#7866 = CARTESIAN_POINT ( 'NONE',  ( 18.16418420727211824, -2.358504521599060322, 12.48345420460293376 ) ) ;
#7867 = ORIENTED_EDGE ( 'NONE', *, *, #49435, .F. ) ;
#7868 = VERTEX_POINT ( 'NONE', #12048 ) ;
#7869 = CARTESIAN_POINT ( 'NONE',  ( 9.684729719592999331, 2.370176859044999862, -6.912649125838000508 ) ) ;
#7870 = FACE_OUTER_BOUND ( 'NONE', #46432, .T. ) ;
#7871 = CARTESIAN_POINT ( 'NONE',  ( 12.18033707850589131, -2.521449564331566418, 13.66889060756772167 ) ) ;
#7872 = CARTESIAN_POINT ( 'NONE',  ( 9.263741181053154250, -5.204002092419764303, 8.765996337996943666 ) ) ;
#7873 = CARTESIAN_POINT ( 'NONE',  ( 8.668206853210000062, -3.979464503892999439, 9.134080454305001595 ) ) ;
#7875 = CONICAL_SURFACE ( 'NONE', #64787, 11.75015521449999945, 0.7854113701714536822 ) ;
#7874 = CARTESIAN_POINT ( 'NONE',  ( 18.44720874474599981, -2.702894824448000222, -11.38760777189999907 ) ) ;
#7877 = CARTESIAN_POINT ( 'NONE',  ( 16.39999997324030190, 3.261216865579172008, 11.32142606715090061 ) ) ;
#7876 = CARTESIAN_POINT ( 'NONE',  ( 10.10636764078099858, -3.461752753411900141, 8.506987760366000018 ) ) ;
#7878 = CARTESIAN_POINT ( 'NONE',  ( 12.80505043854143388, 3.174798964346249530, 12.21921514949791820 ) ) ;
#7879 = EDGE_LOOP ( 'NONE', ( #13596, #49156, #25901, #14079, #37011 ) ) ;
#7880 = CARTESIAN_POINT ( 'NONE',  ( 12.70736722666912044, 0.7301396911442955551, 13.98094760870049491 ) ) ;
#7881 = CARTESIAN_POINT ( 'NONE',  ( 7.904992389751000381, 3.357074527946999787, -6.312906081255999169 ) ) ;
#7882 = EDGE_CURVE ( 'NONE', #63419, #65344, #28895, .T. ) ;
#7883 = EDGE_CURVE ( 'NONE', #67571, #37125, #69054, .T. ) ;
#7884 = CARTESIAN_POINT ( 'NONE',  ( 17.91965136929538005, 0.5080407711865452258, 12.68632595416892883 ) ) ;
#7885 = CARTESIAN_POINT ( 'NONE',  ( 12.72336162097400880, -0.6199801057863054687, 12.67962184309742923 ) ) ;
#7886 = CARTESIAN_POINT ( 'NONE',  ( 18.05156413928683534, -2.879751443183493187, -12.35493952382125116 ) ) ;
#7887 = ORIENTED_EDGE ( 'NONE', *, *, #62507, .T. ) ;
#7889 = CARTESIAN_POINT ( 'NONE',  ( 10.21685100254000034, -2.832432432432000269, 6.822293592207000934 ) ) ;
#7888 = DIRECTION ( 'NONE',  ( -1.000000000000000000, 0.000000000000000000, 0.000000000000000000 ) ) ;
#7890 = CARTESIAN_POINT ( 'NONE',  ( 9.459729719592999686, 2.527713920559999661, -6.969421869128999525 ) ) ;
#7891 = CARTESIAN_POINT ( 'NONE',  ( 25.60000000000000142, 0.000000000000000000, 0.000000000000000000 ) ) ;
#7892 = CARTESIAN_POINT ( 'NONE',  ( 7.729221580034996819, -5.085115902530001897, 6.553339126910996626 ) ) ;
#7893 = CARTESIAN_POINT ( 'NONE',  ( 25.60000000000000142, -9.899494936611999307, -9.899494936611999307 ) ) ;
#7894 = CARTESIAN_POINT ( 'NONE',  ( 4.599999999999999645, 0.000000000000000000, 0.000000000000000000 ) ) ;
#7895 = CARTESIAN_POINT ( 'NONE',  ( 2.261519006296000001, -0.8206105251038000592, 3.497205449952000222 ) ) ;
#7896 = VERTEX_POINT ( 'NONE', #16253 ) ;
#7897 = CARTESIAN_POINT ( 'NONE',  ( 12.30935811146625980, -0.3808128809978846840, -12.69231869260113754 ) ) ;
#7898 = CARTESIAN_POINT ( 'NONE',  ( 9.365090231804463983, 2.650133164351947013, -7.500005474590564880 ) ) ;
#7899 = CARTESIAN_POINT ( 'NONE',  ( 23.59999445750599989, -13.22316420035999940, -4.267800004853000040 ) ) ;
#7900 = CARTESIAN_POINT ( 'NONE',  ( 24.40628504395400000, 3.359328441570999857, -12.19433831731000062 ) ) ;
#7901 = CARTESIAN_POINT ( 'NONE',  ( 7.100000000000000533, 13.04986661130000059, -1.811520473896000016 ) ) ;
#7902 = EDGE_LOOP ( 'NONE', ( #57443, #56918, #12612, #5830, #27021 ) ) ;
#7903 = CARTESIAN_POINT ( 'NONE',  ( 6.529962922412000381, 0.03180299129944000325, -1.321917036380999999 ) ) ;
#7904 = CARTESIAN_POINT ( 'NONE',  ( 10.93892583729919110, 9.336001207588561002, 6.217743753063594170 ) ) ;
#7905 = B_SPLINE_CURVE_WITH_KNOTS ( 'NONE', 3,
 ( #54487, #59728, #64273, #26895 ),
 .UNSPECIFIED., .F., .F.,
 ( 4, 4 ),
 ( 0.8745818872751025541, 1.000000000000000000 ),
 .UNSPECIFIED. ) ;
#7907 = CARTESIAN_POINT ( 'NONE',  ( 10.66914689902456281, 4.353380376947314723, -8.814970433265305161 ) ) ;
#7906 = CARTESIAN_POINT ( 'NONE',  ( 9.567166575710958298, -2.899999999999999911, -6.351075879690426973 ) ) ;
#7908 = CARTESIAN_POINT ( 'NONE',  ( 10.54272335273199879, 4.444874504667400750, 6.301916924546999255 ) ) ;
#7909 = CARTESIAN_POINT ( 'NONE',  ( 10.31652245563454073, -3.317579219585636174, -8.028218637173727856 ) ) ;
#7910 = ORIENTED_EDGE ( 'NONE', *, *, #19837, .T. ) ;
#7911 = EDGE_CURVE ( 'NONE', #50154, #14855, #36676, .T. ) ;
#7912 = ORIENTED_EDGE ( 'NONE', *, *, #11337, .F. ) ;
#7913 = CARTESIAN_POINT ( 'NONE',  ( 9.490614771213035539, -4.913405583856841119, 8.493963967124175340 ) ) ;
#7915 = CARTESIAN_POINT ( 'NONE',  ( 15.86018463513499910, 3.716003765078999876, 11.29289727949000088 ) ) ;
#7914 = AXIS2_PLACEMENT_3D ( 'NONE', #63210, #53086, #5186 ) ;
#7916 = CARTESIAN_POINT ( 'NONE',  ( 18.10090605892218463, 0.4811670829680798622, -13.99174107639406373 ) ) ;
#7917 = VERTEX_POINT ( 'NONE', #64137 ) ;
#7918 = CARTESIAN_POINT ( 'NONE',  ( 9.131856313922000368, -8.648524463724998057, 6.068074759017999753 ) ) ;
#7919 = CARTESIAN_POINT ( 'NONE',  ( 10.97843137008999825, 5.235400103863000254, 6.782920672145000829 ) ) ;
#7920 = AXIS2_PLACEMENT_3D ( 'NONE', #60918, #45193, #32968 ) ;
#7921 = CARTESIAN_POINT ( 'NONE',  ( 11.50000000000000000, -3.008232475376599879, 7.825000000000000178 ) ) ;
#7922 = CARTESIAN_POINT ( 'NONE',  ( 24.96666885033332761, 2.078227436549349605, -11.31065739565387496 ) ) ;
#7923 = CARTESIAN_POINT ( 'NONE',  ( 18.05828166255871636, -3.296090596061253652, 11.87625419658844805 ) ) ;
#7924 = ORIENTED_EDGE ( 'NONE', *, *, #58830, .T. ) ;
#7925 = CARTESIAN_POINT ( 'NONE',  ( 8.849999778957998942, 4.000000000000000000, 7.500000000000000000 ) ) ;
#7926 = CARTESIAN_POINT ( 'NONE',  ( 23.83637917632099956, -13.03948500899999985, -3.620862819564000468 ) ) ;
#7927 = CARTESIAN_POINT ( 'NONE',  ( 10.39393020684999946, 2.750000000000000000, -7.500000000000000000 ) ) ;
#7928 = CARTESIAN_POINT ( 'NONE',  ( 9.779346873515665450, 3.836375382625536012, 8.750000000000001776 ) ) ;
#7929 = CARTESIAN_POINT ( 'NONE',  ( 8.751496707488000126, 4.081676005979390176, 6.643597378104299622 ) ) ;
#7930 = VERTEX_POINT ( 'NONE', #11013 ) ;
#7931 = CARTESIAN_POINT ( 'NONE',  ( 25.29995422340600086, 2.596935224161999844, 11.35301931920000129 ) ) ;
#7932 = EDGE_CURVE ( 'NONE', #7930, #36190, #11003, .T. ) ;
#7933 = CARTESIAN_POINT ( 'NONE',  ( 10.98845665678465799, -2.811543343220049174, -6.624101343727395452 ) ) ;
#7934 = CARTESIAN_POINT ( 'NONE',  ( 6.904593832438223444, 5.247842549850568972, -8.795830109246409734 ) ) ;
#7935 = CARTESIAN_POINT ( 'NONE',  ( 24.00938379501951658, -3.345592699034538153, -12.72992676416136604 ) ) ;
#7936 = CARTESIAN_POINT ( 'NONE',  ( 11.49978667957999967, -12.43119799159999950, -1.530013559959999991 ) ) ;
#7937 = CARTESIAN_POINT ( 'NONE',  ( 12.24892445252029205, -0.2854033456632662502, -13.89606078824646929 ) ) ;
#7938 = CARTESIAN_POINT ( 'NONE',  ( 18.12481736082888517, -2.757674955237352510, 12.38783183949682787 ) ) ;
#7939 = ORIENTED_EDGE ( 'NONE', *, *, #30558, .T. ) ;
#7940 = CARTESIAN_POINT ( 'NONE',  ( 10.77368717260499942, -4.539928529895099985, -8.381256426168800289 ) ) ;
#7941 = ORIENTED_EDGE ( 'NONE', *, *, #13063, .F. ) ;
#7942 = CARTESIAN_POINT ( 'NONE',  ( 18.14117786275468092, 2.282023444416499292, 13.71724589037855502 ) ) ;
#7943 = CARTESIAN_POINT ( 'NONE',  ( 8.929995280412999392, 5.030502105212999453, -6.322203460290999999 ) ) ;
#7944 = CARTESIAN_POINT ( 'NONE',  ( 3.250907432355000015, 3.214334891372999881, -0.06787714083755000405 ) ) ;
#7945 = CARTESIAN_POINT ( 'NONE',  ( 10.36629943602999937, -5.852732332139999549, -7.568014220767000033 ) ) ;
#7946 = CARTESIAN_POINT ( 'NONE',  ( 7.856038276909000473, 2.869044596334999753, -6.744487387516000076 ) ) ;
#7947 = CARTESIAN_POINT ( 'NONE',  ( 9.032937857236275292, -5.014695576459849313, 8.393597907926556800 ) ) ;
#7948 = ORIENTED_EDGE ( 'NONE', *, *, #68351, .T. ) ;
#7949 = VECTOR ( 'NONE', #25673, 1000.000000000000114 ) ;
#7950 = CARTESIAN_POINT ( 'NONE',  ( 10.78026357027499849, -3.014700852776899698, 7.309904858193100097 ) ) ;
#7951 = CARTESIAN_POINT ( 'NONE',  ( 10.84168637167000071, 2.681011538858999899, 6.554754637093000547 ) ) ;
#7952 = CARTESIAN_POINT ( 'NONE',  ( 17.55505043854143565, 1.760910691117812954, 12.47634535983622861 ) ) ;
#7953 = B_SPLINE_CURVE_WITH_KNOTS ( 'NONE', 3,
 ( #2831, #29428, #55979, #38868, #33968, #1803 ),
 .UNSPECIFIED., .F., .F.,
 ( 4, 2, 4 ),
 ( 0.000000000000000000, 0.5000000000000000000, 1.000000000000000000 ),
 .UNSPECIFIED. ) ;
#7954 = DIRECTION ( 'NONE',  ( 1.000000000000000000, 0.000000000000000000, 0.000000000000000000 ) ) ;
#7956 = DIRECTION ( 'NONE',  ( 0.000000000000000000, 0.000000000000000000, -1.000000000000000000 ) ) ;
#7955 = CARTESIAN_POINT ( 'NONE',  ( 9.256664404737000140, 4.025830366070999311, 9.295863330698999505 ) ) ;
#7957 = CARTESIAN_POINT ( 'NONE',  ( 10.99826088462129903, 4.001843064679911244, -6.633804182961699603 ) ) ;
#7958 = MANIFOLD_SOLID_BREP ( 'Stock-MAS-678-1', #44823 ) ;
#7959 = DIRECTION ( 'NONE',  ( -1.000000000000000000, 0.000000000000000000, 0.000000000000000000 ) ) ;
#7960 = CARTESIAN_POINT ( 'NONE',  ( 9.376392757686998536, 4.677963304775400566, -8.241085728986799808 ) ) ;
#7961 = EDGE_CURVE ( 'NONE', #7303, #26199, #34205, .T. ) ;
#7962 = EDGE_CURVE ( 'NONE', #62147, #63419, #19948, .T. ) ;
#7963 = CARTESIAN_POINT ( 'NONE',  ( 18.21544979345814141, -0.2970375428997804046, 12.59650273238872487 ) ) ;
#7964 = CARTESIAN_POINT ( 'NONE',  ( 17.79999999998900151, 3.595165934733000057, 11.99793354950999991 ) ) ;
#7965 = AXIS2_PLACEMENT_3D ( 'NONE', #60903, #30137, #39931 ) ;
#7966 = CARTESIAN_POINT ( 'NONE',  ( 8.123290826992597857, 5.010513939749104750, -6.421869068174552275 ) ) ;
#7967 = CARTESIAN_POINT ( 'NONE',  ( 5.500000000000000000, 12.78667792605000031, 2.345384795462000405 ) ) ;
#7968 = VERTEX_POINT ( 'NONE', #28484 ) ;
#7969 = CARTESIAN_POINT ( 'NONE',  ( 8.977754440379998258, -2.019079883662000086, 7.390983468784999566 ) ) ;
#7970 = EDGE_CURVE ( 'NONE', #65620, #25656, #61682, .T. ) ;
#7971 = EDGE_CURVE ( 'NONE', #31995, #38535, #33336, .T. ) ;
#7972 = CARTESIAN_POINT ( 'NONE',  ( 18.02709866344912726, 1.963667282347026477, 13.86160417883469975 ) ) ;
#7973 = CARTESIAN_POINT ( 'NONE',  ( 11.09998944727697356, -2.658360006774485917, 6.717872455900587347 ) ) ;
#7974 = CARTESIAN_POINT ( 'NONE',  ( 7.600000000000000533, 12.34999999999999964, 4.046978687741000012E-05 ) ) ;
#7975 = ORIENTED_EDGE ( 'NONE', *, *, #8016, .T. ) ;
#7976 = CARTESIAN_POINT ( 'NONE',  ( 7.293864158771000028, 3.416213390569000197, 6.162512717529000206 ) ) ;
#7978 = CARTESIAN_POINT ( 'NONE',  ( 0.5181103717477000270, 3.205765437135000173, -1.404659375816999844 ) ) ;
#7977 = CARTESIAN_POINT ( 'NONE',  ( 8.406645280410000254, 3.807713920470999991, -9.221758713517999695 ) ) ;
#7979 = CARTESIAN_POINT ( 'NONE',  ( 11.19050471959000070, 2.516756593394000152, -6.840361808223000217 ) ) ;
#7980 = ORIENTED_EDGE ( 'NONE', *, *, #18573, .F. ) ;
#7981 = B_SPLINE_CURVE_WITH_KNOTS ( 'NONE', 3,
 ( #24128, #66777, #61876, #51386, #19916, #41241, #45800, #14675, #30084, #61194, #45463, #57306, #19222, #24819, #18893, #9409, #52060, #30753 ),
 .UNSPECIFIED., .F., .F.,
 ( 4, 2, 2, 2, 2, 2, 2, 2, 4 ),
 ( 0.000000000000000000, 0.1249999999999996669, 0.2499999999999993339, 0.3749999999999990008, 0.4999999999999986677, 0.6249999999999990008, 0.7499999999999993339, 0.8749999999999996669, 1.000000000000000000 ),
 .UNSPECIFIED. ) ;
#7982 = CARTESIAN_POINT ( 'NONE',  ( 10.27967883605999866, 5.739712809045000697, 7.774963411801000923 ) ) ;
#7983 = CARTESIAN_POINT ( 'NONE',  ( 18.17146957700712662, -2.902473988487527468, -13.69582979195751271 ) ) ;
#7984 = CARTESIAN_POINT ( 'NONE',  ( 10.81764560330029923, 4.349570499512200428, 8.585859374935999710 ) ) ;
#7985 = CARTESIAN_POINT ( 'NONE',  ( 10.94797187187000098, -2.864324950622999744, 8.846246404612999825 ) ) ;
#7986 = CARTESIAN_POINT ( 'NONE',  ( 9.049999337612000261, 3.268496584495999908E-13, -12.44999944940996350 ) ) ;
#7987 = VERTEX_POINT ( 'NONE', #65868 ) ;
#7988 = FACE_OUTER_BOUND ( 'NONE', #25873, .T. ) ;
#7989 = ADVANCED_FACE ( 'NONE', ( #39658 ), #32998, .T. ) ;
#7990 = CARTESIAN_POINT ( 'NONE',  ( 10.27366694038000006, -3.065543393453000309, -8.487918777453998587 ) ) ;
#7991 = CARTESIAN_POINT ( 'NONE',  ( 7.932978819056404340, -2.299600510671482301, 7.867486896083077497 ) ) ;
#7992 = CARTESIAN_POINT ( 'NONE',  ( 9.075489683949001574, -4.020837068201999820, 8.948702918089999514 ) ) ;
#7993 = CARTESIAN_POINT ( 'NONE',  ( 11.64633327354034797, -4.864904118400500188, -6.934277916748599502 ) ) ;
#7994 = CARTESIAN_POINT ( 'NONE',  ( 10.61390035061499937, -3.695660922043800145, 6.399494776650000105 ) ) ;
#7995 = VERTEX_POINT ( 'NONE', #64740 ) ;
#7996 = DIRECTION ( 'NONE',  ( 0.000000000000000000, 0.7614089499631907509, -0.6482718649732928107 ) ) ;
#7997 = CARTESIAN_POINT ( 'NONE',  ( 10.99764694612700033, -5.059486515935999407, 7.077178005756699974 ) ) ;
#7998 = ORIENTED_EDGE ( 'NONE', *, *, #46266, .F. ) ;
#7999 = CARTESIAN_POINT ( 'NONE',  ( 16.10005255078199937, -3.632778330393000132, -11.06917548872000090 ) ) ;
#8000 = VERTEX_POINT ( 'NONE', #52894 ) ;
#8001 = CARTESIAN_POINT ( 'NONE',  ( 11.08923508776216238, 3.836355264003908250, -9.039235091853335291 ) ) ;
#8002 = CARTESIAN_POINT ( 'NONE',  ( 8.266329719591000824, 4.769017407621999993, -8.862909124839001507 ) ) ;
#8003 = CARTESIAN_POINT ( 'NONE',  ( 11.01279632507519857, 4.624908853805600906, -8.658468685623999406 ) ) ;
#8004 = FACE_BOUND ( 'NONE', #33386, .T. ) ;
#8005 = CARTESIAN_POINT ( 'NONE',  ( 12.18117696241645653, 2.542707536216995301, -12.44156325543625385 ) ) ;
#8006 = CARTESIAN_POINT ( 'NONE',  ( 10.97718582084299932, -4.656536239972400182, 8.258888014436699621 ) ) ;
#8007 = CARTESIAN_POINT ( 'NONE',  ( 11.60612378248510090, -4.482960757953799558, 8.413720204863100349 ) ) ;
#8008 = ORIENTED_EDGE ( 'NONE', *, *, #62724, .F. ) ;
#8009 = CARTESIAN_POINT ( 'NONE',  ( 5.019676782403333704, -0.7288346947182942070, 1.349937054441816775 ) ) ;
#8010 = EDGE_LOOP ( 'NONE', ( #66841, #69170, #45360 ) ) ;
#8011 = CARTESIAN_POINT ( 'NONE',  ( 8.213543146793000460, -3.608524635952000459, 5.913372239166000632 ) ) ;
#8012 = CARTESIAN_POINT ( 'NONE',  ( 11.14975833414749928, 3.203462856645999945, -7.825000000000000178 ) ) ;
#8013 = VERTEX_POINT ( 'NONE', #439 ) ;
#8014 = CARTESIAN_POINT ( 'NONE',  ( 12.08892279761561106, -2.366838896507808876, -12.37571060269618961 ) ) ;
#8015 = CARTESIAN_POINT ( 'NONE',  ( 11.40841235500449891, 3.158861363519000154, 8.270568563129298667 ) ) ;
#8016 = EDGE_CURVE ( 'NONE', #19886, #64076, #67491, .T. ) ;
#8017 = FACE_OUTER_BOUND ( 'NONE', #6043, .T. ) ;
#8018 = DIRECTION ( 'NONE',  ( -0.7071067811865329178, -0.1740570520339079497, 0.6853496499140319109 ) ) ;
#8019 = CARTESIAN_POINT ( 'NONE',  ( 9.048601287889788125, 4.000000467705929985, -8.698595322193607871 ) ) ;
#8020 = DIRECTION ( 'NONE',  ( 0.000000000000000000, -1.000000000000000000, 0.000000000000000000 ) ) ;
#8021 = CARTESIAN_POINT ( 'NONE',  ( 5.411172656737999631, 0.4773362029658999584, 1.482571116122999966 ) ) ;
#8022 = ADVANCED_FACE ( 'NONE', ( #27016, #47993 ), #21753, .T. ) ;
#8023 = CARTESIAN_POINT ( 'NONE',  ( 11.71210404293059959, -4.381818659177399766, -8.277504409418298792 ) ) ;
#8024 = CARTESIAN_POINT ( 'NONE',  ( 10.88733729122639993, -5.277570687708000641, -7.466391690027689876 ) ) ;
#8025 = CARTESIAN_POINT ( 'NONE',  ( 8.443892219592001425, 2.905861847853000057, 8.940690431604000565 ) ) ;
#8026 = ORIENTED_EDGE ( 'NONE', *, *, #34589, .T. ) ;
#8027 =( NAMED_UNIT ( * ) SI_UNIT ( $, .STERADIAN. ) SOLID_ANGLE_UNIT ( ) );
#8028 = CARTESIAN_POINT ( 'NONE',  ( 9.299999999999998934, 4.537600397704999899, 9.154563893594000135 ) ) ;
#8029 = CARTESIAN_POINT ( 'NONE',  ( 18.16596415324148950, 2.632031933676235891, 13.64451525667362652 ) ) ;
#8030 = CARTESIAN_POINT ( 'NONE',  ( 24.25970375843899873, -3.166447075414999812, 12.13786225095999960 ) ) ;
#8031 = CARTESIAN_POINT ( 'NONE',  ( 17.65794081825375272, 1.883184384514173360, 12.57407373858317712 ) ) ;
#8032 = VECTOR ( 'NONE', #525, 1000.000000000000000 ) ;
#8033 = CARTESIAN_POINT ( 'NONE',  ( 11.01665240710999960, 5.432459446251999502, 4.991866823696000210 ) ) ;
#8034 = CARTESIAN_POINT ( 'NONE',  ( 9.719613305057999142, 5.967773797872000685, 7.406643507784999692 ) ) ;
#8035 = DIRECTION ( 'NONE',  ( 0.000000000000000000, 0.8648648648648717963, 0.5020047465136829867 ) ) ;
#8036 = ORIENTED_EDGE ( 'NONE', *, *, #42614, .F. ) ;
#8037 = CARTESIAN_POINT ( 'NONE',  ( 12.21195445704744209, -2.302603597045700390, 12.49539791649142373 ) ) ;
#8038 = CARTESIAN_POINT ( 'NONE',  ( 9.982279731608999285, -3.922199073804859992, -6.636486849903699969 ) ) ;
#8039 = CARTESIAN_POINT ( 'NONE',  ( 11.20563302462000088, 3.509134285281999777, 6.118194788334999856 ) ) ;
#8040 = CARTESIAN_POINT ( 'NONE',  ( 9.232128830620874638, 3.792804146276640864, 8.743003876391233220 ) ) ;
#8041 = CARTESIAN_POINT ( 'NONE',  ( 10.57149279008999798, 3.703313553258400059, -8.601484120896000007 ) ) ;
#8042 = CARTESIAN_POINT ( 'NONE',  ( 12.19409707445300306, 0.1321628250398321214, 12.69908003149455133 ) ) ;
#8043 = CARTESIAN_POINT ( 'NONE',  ( 7.802017219589999719, 5.638704226117999596, 8.266404648244000342 ) ) ;
#8044 = CARTESIAN_POINT ( 'NONE',  ( 11.06923869026000062, 5.425682056982999768, 8.012911262916999178 ) ) ;
#8045 = B_SPLINE_CURVE_WITH_KNOTS ( 'NONE', 3,
 ( #62879, #68125, #2198, #50426 ),
 .UNSPECIFIED., .F., .F.,
 ( 4, 4 ),
 ( 0.000000000000000000, 1.000000000000000000 ),
 .UNSPECIFIED. ) ;
#8046 = CARTESIAN_POINT ( 'NONE',  ( 12.18014475499750837, 2.522932601087060966, 12.44621172798972708 ) ) ;
#8047 = ORIENTED_EDGE ( 'NONE', *, *, #5822, .T. ) ;
#8048 = CARTESIAN_POINT ( 'NONE',  ( 25.25798339014900051, 8.562781525512001224, 7.910461493226999430 ) ) ;
#8049 = CARTESIAN_POINT ( 'NONE',  ( 10.73964560330029983, 4.391636236366600166, -6.283473206644000442 ) ) ;
#8050 = EDGE_CURVE ( 'NONE', #2983, #7548, #59163, .T. ) ;
#8051 = ADVANCED_FACE ( 'NONE', ( #49362 ), #1475, .T. ) ;
#8052 = CARTESIAN_POINT ( 'NONE',  ( 10.81771127433663970, -4.157152761341111891, 9.232783412159369263 ) ) ;
#8054 = CARTESIAN_POINT ( 'NONE',  ( 11.59999999999999964, 5.179498027601999510, -7.174999999999999822 ) ) ;
#8053 = CARTESIAN_POINT ( 'NONE',  ( 7.533879440377999614, -4.623636604834999275, 8.651469651195000665 ) ) ;
#8055 = CARTESIAN_POINT ( 'NONE',  ( 9.780051052052000315, -3.014287398677499841, 7.307093369932900373 ) ) ;
#8056 = CARTESIAN_POINT ( 'NONE',  ( 11.56025819896753859, -4.986099335708799707, -7.685900384398899554 ) ) ;
#8057 = VERTEX_POINT ( 'NONE', #12314 ) ;
#8058 = B_SPLINE_CURVE_WITH_KNOTS ( 'NONE', 3,
 ( #30038, #51340, #18502, #60799, #66033, #24082, #34929, #61827, #8351, #45757, #50314, #50657, #55906, #33892, #45418, #49963, #44735, #19179 ),
 .UNSPECIFIED., .F., .F.,
 ( 4, 2, 2, 2, 2, 2, 2, 2, 4 ),
 ( 0.000000000000000000, 0.1249999999999996669, 0.2499999999999993339, 0.3749999999999990008, 0.4999999999999986677, 0.6249999999999990008, 0.7499999999999993339, 0.8749999999999996669, 1.000000000000000000 ),
 .UNSPECIFIED. ) ;
#8059 = VECTOR ( 'NONE', #29857, 1000.000000000000114 ) ;
#8060 = CARTESIAN_POINT ( 'NONE',  ( 1.734611342038000048, 0.7023893950988999713, -3.352829814747000370 ) ) ;
#8061 = DIRECTION ( 'NONE',  ( 0.000000000000000000, -1.000000000000000000, 0.000000000000000000 ) ) ;
#8062 = CARTESIAN_POINT ( 'NONE',  ( 9.469356963619999235, -5.119357025014000584, 7.500000000085178087 ) ) ;
#8063 = CYLINDRICAL_SURFACE ( 'NONE', #55886, 1.350000000000000089 ) ;
#8064 = CARTESIAN_POINT ( 'NONE',  ( 24.41456973747800063, -12.00390065690999997, 3.256048965932000439 ) ) ;
#8065 = CARTESIAN_POINT ( 'NONE',  ( 4.900006121742000786, -1.007237960741800276, -1.747572776708515407 ) ) ;
#8066 = CARTESIAN_POINT ( 'NONE',  ( 44.24148000000000280, 11.77655473258999841, -4.190794510628000680 ) ) ;
#8067 = DIRECTION ( 'NONE',  ( -8.953094821931283005E-11, 0.9867385579967302700, 0.1623176458754050089 ) ) ;
#8068 = CARTESIAN_POINT ( 'NONE',  ( 7.731793146792000471, -4.580607464247000493, 9.213361409141999303 ) ) ;
#8069 = ORIENTED_EDGE ( 'NONE', *, *, #30622, .F. ) ;
#8070 = CARTESIAN_POINT ( 'NONE',  ( 9.240545280410998430, 4.158911560497999815, 5.873540104660999184 ) ) ;
#8071 = EDGE_CURVE ( 'NONE', #61687, #42399, #27507, .T. ) ;
#8072 = CARTESIAN_POINT ( 'NONE',  ( 11.05576033064000185, 5.199216738862999954, 4.875271020876000172 ) ) ;
#8073 = CARTESIAN_POINT ( 'NONE',  ( 7.433354470783482881, -2.295550242067167179, 7.846515896910211119 ) ) ;
#8074 = VECTOR ( 'NONE', #61270, 1000.000000000000000 ) ;
#8075 = CARTESIAN_POINT ( 'NONE',  ( 17.71608705225915514, -0.6042412280147623216, 13.88231902343041924 ) ) ;
#8076 = CARTESIAN_POINT ( 'NONE',  ( 0.6942448634807999452, 3.368557921162000479, -0.6219103594335000373 ) ) ;
#8077 = ORIENTED_EDGE ( 'NONE', *, *, #34512, .T. ) ;
#8078 = LINE ( 'NONE', #55631, #60070 ) ;
#8079 = MANIFOLD_SOLID_BREP ( 'Stock-MAS-678-1', #6820 ) ;
#8080 = DIRECTION ( 'NONE',  ( 0.000000000000000000, -0.1807154286440004198, -0.9835354258236025382 ) ) ;
#8081 = CARTESIAN_POINT ( 'NONE',  ( 11.03856029907000114, 2.974095820320000083, 8.716122353065999917 ) ) ;
#8082 = CARTESIAN_POINT ( 'NONE',  ( 10.30903300763299946, 4.597717337857299746, 6.873077781830399857 ) ) ;
#8083 = AXIS2_PLACEMENT_3D ( 'NONE', #21270, #37350, #58675 ) ;
#8084 = CARTESIAN_POINT ( 'NONE',  ( 5.700000000000000178, -1.300000000000000044, -9.662944685757000940 ) ) ;
#8085 = CARTESIAN_POINT ( 'NONE',  ( 7.000000000000000000, 0.8000000000000000444, 3.149999999999999911 ) ) ;
#8086 = CARTESIAN_POINT ( 'NONE',  ( 17.65273365045183596, 0.7301396911442742388, -13.98094760870049313 ) ) ;
#8087 = LINE ( 'NONE', #44473, #12031 ) ;
#8088 = CARTESIAN_POINT ( 'NONE',  ( 12.80505043854146940, -3.125000000000000000, 12.28374638332999780 ) ) ;
#8089 = CARTESIAN_POINT ( 'NONE',  ( 8.259865135739552500, 5.282034867868143913, 8.692621038018929269 ) ) ;
#8090 = VERTEX_POINT ( 'NONE', #66828 ) ;
#8091 = CARTESIAN_POINT ( 'NONE',  ( 17.86981019193749631, -1.959656554206103962, 13.77332550900839969 ) ) ;
#8092 = CARTESIAN_POINT ( 'NONE',  ( 17.98398272105957219, 2.954699841475006306, -13.56644208774675597 ) ) ;
#8093 = ORIENTED_EDGE ( 'NONE', *, *, #5814, .F. ) ;
#8094 = DIRECTION ( 'NONE',  ( 1.267684193041221762E-20, 0.9999999999999997780, 2.657887364712999055E-08 ) ) ;
#8095 = CARTESIAN_POINT ( 'NONE',  ( 10.52946886766499901, 3.569835351907400423, 8.281567006984099422 ) ) ;
#8096 = CARTESIAN_POINT ( 'NONE',  ( 4.149992563291999836, 1.947893036340042183, -0.5234817089163682491 ) ) ;
#8097 = CARTESIAN_POINT ( 'NONE',  ( 12.80505043854143388, 3.199751711897557804, -12.18694338143115630 ) ) ;
#8098 = CARTESIAN_POINT ( 'NONE',  ( 9.318724127987000116, 2.755029797911999978, 8.795125756257000660 ) ) ;
#8099 = CARTESIAN_POINT ( 'NONE',  ( 10.09453415443000068, 5.362844031509000686, -7.550030311027999375 ) ) ;
#8100 = CARTESIAN_POINT ( 'NONE',  ( 10.20851354018233614, -3.836375382625528019, -6.250000000000001776 ) ) ;
#8101 = CARTESIAN_POINT ( 'NONE',  ( 9.681180837610000367, -2.612237299844000216, 7.804680206899999639 ) ) ;
#8102 = CARTESIAN_POINT ( 'NONE',  ( 17.67321935251239751, 0.7100593550699959566, -12.57997761080729582 ) ) ;
#8103 = EDGE_CURVE ( 'NONE', #20902, #16735, #66763, .T. ) ;
#8104 = DIRECTION ( 'NONE',  ( -1.000000000000000000, -8.790925318715999585E-10, -6.356715264083000235E-09 ) ) ;
#8105 = CARTESIAN_POINT ( 'NONE',  ( 10.33364828895399867, -3.239803852721999888, -7.915211961479200475 ) ) ;
#8106 = CARTESIAN_POINT ( 'NONE',  ( 25.29987667925500361, 11.77655473258999841, 4.190794510628000680 ) ) ;
#8107 = ORIENTED_EDGE ( 'NONE', *, *, #41759, .T. ) ;
#8108 = CARTESIAN_POINT ( 'NONE',  ( 8.903317944506801140, 3.725094887964650603, -6.473766235688634296 ) ) ;
#8109 = CIRCLE ( 'NONE', #25968, 13.10000000000000320 ) ;
#8110 = PRESENTATION_STYLE_ASSIGNMENT (( #29453 ) ) ;
#8111 = CARTESIAN_POINT ( 'NONE',  ( 24.63610587989722234, 8.692490458917935925, 8.668794396725420626 ) ) ;
#8112 = PLANE ( 'NONE',  #7149 ) ;
#8113 = CARTESIAN_POINT ( 'NONE',  ( 9.216839207166817260, 4.768179003839036589, 8.499566091636108212 ) ) ;
#8114 = CARTESIAN_POINT ( 'NONE',  ( 12.26189125119389978, 2.190632771808445067, 13.73417700668422725 ) ) ;
#8115 = CARTESIAN_POINT ( 'NONE',  ( 10.20319453770999907, -3.421758889707999796, 6.017729046583999875 ) ) ;
#8116 = VERTEX_POINT ( 'NONE', #17909 ) ;
#8117 = CARTESIAN_POINT ( 'NONE',  ( 12.21279950747578269, -0.1999332404816966391, -12.69788654131174610 ) ) ;
#8118 = CARTESIAN_POINT ( 'NONE',  ( 12.36315992512968975, 0.5793931417437889753, 13.98801390351337481 ) ) ;
#8119 = EDGE_LOOP ( 'NONE', ( #53420, #25848, #39685, #49955 ) ) ;
#8120 = FACE_BOUND ( 'NONE', #4380, .T. ) ;
#8121 = DIRECTION ( 'NONE',  ( 0.000000000000000000, -0.9659258262890757507, -0.2588190451024934835 ) ) ;
#8122 = CARTESIAN_POINT ( 'NONE',  ( 24.21979545967400327, -3.760914022703000459, -12.77961884926999936 ) ) ;
#8123 = DIRECTION ( 'NONE',  ( -1.000000000000000000, 0.000000000000000000, 0.000000000000000000 ) ) ;
#8124 = AXIS2_PLACEMENT_3D ( 'NONE', #66391, #43700, #34602 ) ;
#8125 = CARTESIAN_POINT ( 'NONE',  ( 8.970944094206998898, -5.100000000000000533, 6.571291218949999902 ) ) ;
#8126 = CARTESIAN_POINT ( 'NONE',  ( 24.44496488009700030, 8.810487470433001178, 8.810507756548000557 ) ) ;
#8127 = CARTESIAN_POINT ( 'NONE',  ( 0.01379484080271000009, 3.646234950436999966, -0.6383912046097000026 ) ) ;
#8128 = CARTESIAN_POINT ( 'NONE',  ( 10.06493315628555862, -5.349942305088194239, -7.500003965376651038 ) ) ;
#8129 = CARTESIAN_POINT ( 'NONE',  ( 10.42363156114900136, -4.684311564990209398, -8.575598637068461372 ) ) ;
#8130 = FACE_OUTER_BOUND ( 'NONE', #6957, .T. ) ;
#8131 = CARTESIAN_POINT ( 'NONE',  ( 11.26902897915239876, 4.221721321201099997, -8.337339982364900592 ) ) ;
#8132 = CARTESIAN_POINT ( 'NONE',  ( 10.90000000000000036, -8.263403946409999534, 6.953859016290999229 ) ) ;
#8133 = EDGE_CURVE ( 'NONE', #36015, #38805, #31140, .T. ) ;
#8134 = EDGE_CURVE ( 'NONE', #40685, #54822, #28385, .T. ) ;
#8135 = CARTESIAN_POINT ( 'NONE',  ( 12.80505043854144276, 0.7192913403693124152, -12.57945229203838267 ) ) ;
#8136 = CARTESIAN_POINT ( 'NONE',  ( 9.354025935145999782, 3.834207658792500251, -6.370288821165999593 ) ) ;
#8138 = CARTESIAN_POINT ( 'NONE',  ( 12.72212784907325833, 1.874999999999999556, 12.57541659658320476 ) ) ;
#8137 = CARTESIAN_POINT ( 'NONE',  ( 16.04504292973000190, -8.364028678926000993, -8.186631590245999845 ) ) ;
#8139 = CARTESIAN_POINT ( 'NONE',  ( 23.64971691489271421, -13.39987426919188707, 3.835034287296173350 ) ) ;
#8140 = ORIENTED_EDGE ( 'NONE', *, *, #30948, .T. ) ;
#8141 = DIRECTION ( 'NONE',  ( 0.000000000000000000, -0.9466492601157001641, 0.3222656952305000266 ) ) ;
#8142 = CARTESIAN_POINT ( 'NONE',  ( 10.68403590588000007, -5.436611040123999317, 8.578433628717998971 ) ) ;
#8143 = CARTESIAN_POINT ( 'NONE',  ( 9.528367640780999182, 4.473477001189199775, 8.385811396220899994 ) ) ;
#8144 = CARTESIAN_POINT ( 'NONE',  ( 10.31021345716899873, 4.636538040886300394, -8.078719053813800954 ) ) ;
#8145 = CARTESIAN_POINT ( 'NONE',  ( 9.601186317138909132, -5.349829778710892825, -7.263235859471102174 ) ) ;
#8146 = CARTESIAN_POINT ( 'NONE',  ( 12.33523313525534526, 2.912685155779578317, 13.57718188376387225 ) ) ;
#8147 = ORIENTED_EDGE ( 'NONE', *, *, #62966, .F. ) ;
#8148 = ADVANCED_FACE ( 'NONE', ( #34342 ), #65785, .T. ) ;
#8149 = CARTESIAN_POINT ( 'NONE',  ( 8.822113844317998499, -3.711648483798899889, -6.395197822644999697 ) ) ;
#8150 = AXIS2_PLACEMENT_3D ( 'NONE', #53023, #921, #42534 ) ;
#8151 = CARTESIAN_POINT ( 'NONE',  ( 10.73543045066558399, -5.073272730021160193, -5.075194819112775590 ) ) ;
#8152 = PRODUCT_DEFINITION_SHAPE ( 'NONE', 'NONE',  #69196 ) ;
#8153 = ADVANCED_FACE ( 'NONE', ( #67163, #67850 ), #24870, .F. ) ;
#8154 = CARTESIAN_POINT ( 'NONE',  ( 17.56715138999748760, 1.760845446529456071, -12.47635456592353442 ) ) ;
#8155 = CARTESIAN_POINT ( 'NONE',  ( 10.87180915648999857, -2.933919166010999557, 5.127994723445000069 ) ) ;
#8156 = CARTESIAN_POINT ( 'NONE',  ( 5.477523075960999854, 12.82224764859999766, 2.276049205300000100 ) ) ;
#8157 = CONICAL_SURFACE ( 'NONE', #68420, 12.42515511468000078, 0.7854106315584118425 ) ;
#8158 = CARTESIAN_POINT ( 'NONE',  ( 12.19234151428706880, 2.623341430473556724, -13.64652576295699404 ) ) ;
#8159 = CARTESIAN_POINT ( 'NONE',  ( 9.177304894000000601, -4.588307032459999490, -5.987050435448999508 ) ) ;
#8160 = CARTESIAN_POINT ( 'NONE',  ( 5.700000000378000031, -0.2999999996220999443, 3.150000004979999879 ) ) ;
#8161 = ORIENTED_EDGE ( 'NONE', *, *, #15940, .F. ) ;
#8162 = LINE ( 'NONE', #29509, #15448 ) ;
#8163 = CARTESIAN_POINT ( 'NONE',  ( 12.44118158293134613, 0.5082612142235577446, -13.88749228919889767 ) ) ;
#8164 = CARTESIAN_POINT ( 'NONE',  ( 13.70003001321900271, 9.668726926528000476, 7.961868161445000425 ) ) ;
#8165 = CARTESIAN_POINT ( 'NONE',  ( 20.00000000000000000, 0.000000000000000000, 0.000000000000000000 ) ) ;
#8166 = CARTESIAN_POINT ( 'NONE',  ( 24.74439240416100105, -8.626915347824999358, -8.720184348590999335 ) ) ;
#8167 = CARTESIAN_POINT ( 'NONE',  ( 17.60000000000000142, -11.23412379136000006, 3.084957477885999833 ) ) ;
#8169 = AXIS2_PLACEMENT_3D ( 'NONE', #29257, #39048, #2326 ) ;
#8168 = CARTESIAN_POINT ( 'NONE',  ( 8.709204462306734840, 2.899999999999999911, 6.662590550601094286 ) ) ;
#8170 = ORIENTED_EDGE ( 'NONE', *, *, #16471, .F. ) ;
#8171 = PLANE ( 'NONE',  #68578 ) ;
#8172 = CARTESIAN_POINT ( 'NONE',  ( 17.65776394871754107, 1.883156081309886432, -13.78509897404220830 ) ) ;
#8173 = EDGE_LOOP ( 'NONE', ( #26537, #34674, #40491, #36390 ) ) ;
#8174 = CARTESIAN_POINT ( 'NONE',  ( 8.507804550190710913, 4.678883388517513175, 8.679043930491522119 ) ) ;
#8175 = CARTESIAN_POINT ( 'NONE',  ( 25.26126129534557307, 2.660454058625374874, 11.37585472950963883 ) ) ;
#8176 = CARTESIAN_POINT ( 'NONE',  ( 9.211104719594999324, 5.462898983065000102, -8.055936939571999744 ) ) ;
#8177 = CARTESIAN_POINT ( 'NONE',  ( 24.60115027442303770, 8.755275597086985329, -9.042371280549295065 ) ) ;
#8178 = CARTESIAN_POINT ( 'NONE',  ( 11.59966954483535773, -3.361010663344000005, -6.514072057539499916 ) ) ;
#8179 = DIRECTION ( 'NONE',  ( 0.000000000000000000, 0.000000000000000000, 1.000000000000000000 ) ) ;
#8180 = DIRECTION ( 'NONE',  ( 0.000000000000000000, 0.000000000000000000, -1.000000000000000000 ) ) ;
#8181 = ORIENTED_EDGE ( 'NONE', *, *, #5292, .T. ) ;
#8182 = CARTESIAN_POINT ( 'NONE',  ( 7.736620384918536431, 4.059907268619843634, -8.863659910720466328 ) ) ;
#8183 = CARTESIAN_POINT ( 'NONE',  ( 24.30000000000000071, -12.03537377768999939, 3.224868684338999980 ) ) ;
#8184 = CARTESIAN_POINT ( 'NONE',  ( 25.60000000000000142, -8.527654132749999505, 7.260537518967999482 ) ) ;
#8185 = VERTEX_POINT ( 'NONE', #25900 ) ;
#8186 = CARTESIAN_POINT ( 'NONE',  ( 10.76231429546999863, 3.259156861436999897, -8.644989069184999764 ) ) ;
#8187 = DIRECTION ( 'NONE',  ( -1.000000000000000000, 0.000000000000000000, 0.000000000000000000 ) ) ;
#8188 = ORIENTED_EDGE ( 'NONE', *, *, #28669, .F. ) ;
#8189 = CARTESIAN_POINT ( 'NONE',  ( 9.176721904869998170, 4.995641764568400589, 6.941043897400199114 ) ) ;
#8190 = CARTESIAN_POINT ( 'NONE',  ( 18.02641336659269555, -3.027085105403487297, -12.23097768044556055 ) ) ;
#8191 = CARTESIAN_POINT ( 'NONE',  ( 9.404346873515669003, 2.750000000000000000, 7.336375382625536901 ) ) ;
#8192 = PRODUCT_RELATED_PRODUCT_CATEGORY ( 'part', '', ( #3134 ) ) ;
#8193 = DIRECTION ( 'NONE',  ( 1.000000000000000000, 0.000000000000000000, 0.000000000000000000 ) ) ;
#8194 = EDGE_CURVE ( 'NONE', #58012, #10018, #68190, .T. ) ;
#8195 = CARTESIAN_POINT ( 'NONE',  ( 24.40777907822999993, -12.23846661367000088, -3.187421709680999804 ) ) ;
#8196 = CARTESIAN_POINT ( 'NONE',  ( 9.381146409496318839, -2.870643679914145707, 8.823445380589753029 ) ) ;
#8197 = ORIENTED_EDGE ( 'NONE', *, *, #66834, .T. ) ;
#8198 = CARTESIAN_POINT ( 'NONE',  ( 11.59999999999999964, 3.137911629819545745, 7.087473780876516471 ) ) ;
#8199 = AXIS2_PLACEMENT_3D ( 'NONE', #31658, #52977, #43867 ) ;
#8200 = CARTESIAN_POINT ( 'NONE',  ( 10.84161084123000052, 2.641275823976000137, -7.444905437480000110 ) ) ;
#8201 = DIRECTION ( 'NONE',  ( 0.000000000000000000, 0.000000000000000000, 1.000000000000000000 ) ) ;
#8202 = CARTESIAN_POINT ( 'NONE',  ( 12.08142877465142107, 2.567860614650635753, -13.76250926564159016 ) ) ;
#8203 = AXIS2_PLACEMENT_3D ( 'NONE', #40802, #35571, #50954 ) ;
#8204 = CARTESIAN_POINT ( 'NONE',  ( 9.608380199233998553, -2.730774061183999901, -7.340469740450900282 ) ) ;
#8205 = CARTESIAN_POINT ( 'NONE',  ( 11.05639424537999993, -5.030223832177999732, 6.028291574375000295 ) ) ;
#8206 = CARTESIAN_POINT ( 'NONE',  ( 18.26845486291481535, -0.1306247939804510705, 13.99939550958098522 ) ) ;
#8207 = CARTESIAN_POINT ( 'NONE',  ( 7.844724277266999835, 4.719412473309000156, 6.357657803787000184 ) ) ;
#8208 = ORIENTED_EDGE ( 'NONE', *, *, #51566, .F. ) ;
#8209 = ORIENTED_EDGE ( 'NONE', *, *, #9564, .F. ) ;
#8210 = CARTESIAN_POINT ( 'NONE',  ( 9.883629719592001095, 5.656948148960999845, -6.994239053114000626 ) ) ;
#8211 = DIRECTION ( 'NONE',  ( 1.000000000000000000, 0.000000000000000000, 0.000000000000000000 ) ) ;
#8212 = CARTESIAN_POINT ( 'NONE',  ( 12.41737123621465599, -2.003119782556758821, 13.76653501053765716 ) ) ;
#8213 = CARTESIAN_POINT ( 'NONE',  ( 9.299999999999998934, -4.537600397704999899, 9.154563893594000135 ) ) ;
#8214 = ADVANCED_FACE ( 'NONE', ( #30803 ), #40266, .F. ) ;
#8215 = EDGE_CURVE ( 'NONE', #3750, #40516, #46711, .T. ) ;
#8216 = CARTESIAN_POINT ( 'NONE',  ( 24.22085326866800159, 9.185890470428999421, -9.646242683205999313 ) ) ;
#8217 = CARTESIAN_POINT ( 'NONE',  ( 18.40429364930200151, -2.938801558760000265, -11.32979830910000096 ) ) ;
#8219 = CARTESIAN_POINT ( 'NONE',  ( 10.96504121510999852, -5.560326135739999565, 4.905747935756999745 ) ) ;
#8218 = CARTESIAN_POINT ( 'NONE',  ( 10.33432996542199866, -4.793057006135000186, 6.678540912152799436 ) ) ;
#8220 =( GEOMETRIC_REPRESENTATION_CONTEXT ( 3 ) GLOBAL_UNCERTAINTY_ASSIGNED_CONTEXT ( ( #15020 ) ) GLOBAL_UNIT_ASSIGNED_CONTEXT ( ( #39578, #33651, #54967 ) ) REPRESENTATION_CONTEXT ( 'NONE', 'WORKASPACE' ) );
#8221 = CARTESIAN_POINT ( 'NONE',  ( 8.429610941929999157, -5.086930576191002196, -6.619396742377001708 ) ) ;
#8222 = ORIENTED_EDGE ( 'NONE', *, *, #18790, .T. ) ;
#8223 = EDGE_CURVE ( 'NONE', #5660, #64040, #5414, .T. ) ;
#8224 = CARTESIAN_POINT ( 'NONE',  ( 10.90000000000000036, 4.000000000000000000, 7.500000000000000000 ) ) ;
#8225 = CARTESIAN_POINT ( 'NONE',  ( 11.03789961707000167, -2.850875858055000212, -5.120756380231999749 ) ) ;
#8226 = CARTESIAN_POINT ( 'NONE',  ( 17.63732991102260073, 0.6196453797482972536, 12.67964297675817598 ) ) ;
#8227 = DIRECTION ( 'NONE',  ( 0.000000000000000000, -1.000000000000000000, 0.000000000000000000 ) ) ;
#8228 = DIRECTION ( 'NONE',  ( 1.000000000000000000, 0.000000000000000000, 0.000000000000000000 ) ) ;
#8229 = VERTEX_POINT ( 'NONE', #20308 ) ;
#8231 = CARTESIAN_POINT ( 'NONE',  ( 11.08810207955139937, 3.203462856645999945, 7.825000000000000178 ) ) ;
#8230 = CARTESIAN_POINT ( 'NONE',  ( 11.13477878846000024, -5.334327202385000355, 5.176824473787999814 ) ) ;
#8232 = CARTESIAN_POINT ( 'NONE',  ( 9.740360841231000322, 4.047146749018000200, -5.600703114891000034 ) ) ;
#8233 = CARTESIAN_POINT ( 'NONE',  ( 10.83810672858429847, 2.978701842912999886, 8.268288002587098617 ) ) ;
#8234 = CARTESIAN_POINT ( 'NONE',  ( 8.784678295047998020, -4.000000000000000000, -7.500000000000000000 ) ) ;
#8235 = EDGE_CURVE ( 'NONE', #58563, #44202, #11644, .T. ) ;
#8236 = FACE_OUTER_BOUND ( 'NONE', #50299, .T. ) ;
#8237 = CARTESIAN_POINT ( 'NONE',  ( 2.499928753500999523, 0.3043608712121999571, -3.579275528594000111 ) ) ;
#8238 = VERTEX_POINT ( 'NONE', #41295 ) ;
#8239 = CARTESIAN_POINT ( 'NONE',  ( 12.74530398939899634, 0.7169431667913611639, -12.57958639523259059 ) ) ;
#8240 = CARTESIAN_POINT ( 'NONE',  ( 7.790489386131184801, -2.917550760077413763, 6.652506093142642740 ) ) ;
#8241 = CARTESIAN_POINT ( 'NONE',  ( 23.71889146657003167, -13.13858983292066718, -3.830114772933163270 ) ) ;
#8242 = CARTESIAN_POINT ( 'NONE',  ( 24.35145719007200071, 3.377064811435000369, -12.26055847765000095 ) ) ;
#8243 = CARTESIAN_POINT ( 'NONE',  ( 4.700001368028300597, 0.000000000000000000, 0.000000000000000000 ) ) ;
#8244 = ORIENTED_EDGE ( 'NONE', *, *, #20066, .T. ) ;
#8245 = CARTESIAN_POINT ( 'NONE',  ( 5.471262210455999586, -0.8655273653155000080, -0.9996707749736001292 ) ) ;
#8246 = CARTESIAN_POINT ( 'NONE',  ( 7.002195280409999611, 5.464161011425000325, -7.581039036848999935 ) ) ;
#8247 = CARTESIAN_POINT ( 'NONE',  ( 10.42499241036494162, 5.349775919985349404, 7.500001834605750872 ) ) ;
#8248 = CARTESIAN_POINT ( 'NONE',  ( 10.19810941423799910, 4.946022705791000007, 8.359277272599898723 ) ) ;
#8249 = CARTESIAN_POINT ( 'NONE',  ( 10.89835090130999973, 4.878966983716200190, -8.043647632228999811 ) ) ;
#8250 = ORIENTED_EDGE ( 'NONE', *, *, #12146, .F. ) ;
#8251 = CONICAL_SURFACE ( 'NONE', #37288, 0.3796172482170003804, 0.7853981633972997312 ) ;
#8252 = CARTESIAN_POINT ( 'NONE',  ( 9.444317341922999987, -2.927260449021000355, 8.897015448164999896 ) ) ;
#8253 = ORIENTED_EDGE ( 'NONE', *, *, #27478, .F. ) ;
#8254 = DIRECTION ( 'NONE',  ( 1.000000000000000000, 0.000000000000000000, 0.000000000000000000 ) ) ;
#8255 = CARTESIAN_POINT ( 'NONE',  ( 7.892605646791999163, -5.480312458445999901, 8.192326492433998908 ) ) ;
#8256 = CARTESIAN_POINT ( 'NONE',  ( 18.24552752486710716, 0.2229649748661320929, -13.99822903660538564 ) ) ;
#8257 = VERTEX_POINT ( 'NONE', #61585 ) ;
#8258 = CARTESIAN_POINT ( 'NONE',  ( 6.871402371741999637, -9.249258202502000259, 5.114981648749999721 ) ) ;
#8259 = CARTESIAN_POINT ( 'NONE',  ( 24.32156006308829888, -9.044158311594529209, -9.474452558964053139 ) ) ;
#8260 = CARTESIAN_POINT ( 'NONE',  ( 10.33351354018333446, -5.249999999999999112, 7.663624617374471093 ) ) ;
#8261 = CARTESIAN_POINT ( 'NONE',  ( 9.385596873516666605, -5.092232985442824322, -8.129523725463620565 ) ) ;
#8262 = CARTESIAN_POINT ( 'NONE',  ( 25.29987654162099986, 8.533547811387000692, 7.925584028117998336 ) ) ;
#8263 = VERTEX_POINT ( 'NONE', #46545 ) ;
#8264 = CARTESIAN_POINT ( 'NONE',  ( 8.709204462306566086, -2.899999999999999911, 6.662590550605525408 ) ) ;
#8265 = CARTESIAN_POINT ( 'NONE',  ( 23.61806551351500261, -13.16805540424999954, -4.269441848944000029 ) ) ;
#8266 = CARTESIAN_POINT ( 'NONE',  ( 5.552943173016877232, -1.199500263597274685, 0.9218200799623673669 ) ) ;
#8267 =( LENGTH_UNIT ( ) NAMED_UNIT ( * ) SI_UNIT ( .MILLI., .METRE. ) );
#8268 = AXIS2_PLACEMENT_3D ( 'NONE', #41183, #56915, #30355 ) ;
#8269 = CARTESIAN_POINT ( 'NONE',  ( 12.15512143695920599, -2.141660958086382127, 13.83591020989070053 ) ) ;
#8270 = B_SPLINE_CURVE_WITH_KNOTS ( 'NONE', 3,
 ( #28009, #1433, #12614, #44096 ),
 .UNSPECIFIED., .F., .F.,
 ( 4, 4 ),
 ( 0.000000000000000000, 1.000000000000000000 ),
 .UNSPECIFIED. ) ;
#8271 = VERTEX_POINT ( 'NONE', #57704 ) ;
#8272 = CARTESIAN_POINT ( 'NONE',  ( 25.46371819568200223, 2.879482785682999868, 11.30954024936000124 ) ) ;
#8273 = AXIS2_PLACEMENT_3D ( 'NONE', #35603, #15299, #10388 ) ;
#8274 = CARTESIAN_POINT ( 'NONE',  ( 8.916525748329496182, -4.536323992761255752, -6.567753456898076436 ) ) ;
#8275 = CARTESIAN_POINT ( 'NONE',  ( 3.500000000000000444, 3.257391245615596898, 1.180021364213383883 ) ) ;
#8276 = EDGE_CURVE ( 'NONE', #34762, #24471, #42491, .T. ) ;
#8277 = CARTESIAN_POINT ( 'NONE',  ( 11.16486084871730000, 5.207010770456999893, -7.174999999999999822 ) ) ;
#8278 = CYLINDRICAL_SURFACE ( 'NONE', #7568, 1.350000000000000533 ) ;
#8279 = EDGE_CURVE ( 'NONE', #65964, #27255, #53391, .T. ) ;
#8280 = AXIS2_PLACEMENT_3D ( 'NONE', #61634, #60951, #3251 ) ;
#8281 = CARTESIAN_POINT ( 'NONE',  ( 12.49177480397739615, -0.5412024733746028105, -13.88582008197801976 ) ) ;
#8282 = CARTESIAN_POINT ( 'NONE',  ( 18.17519250343470461, -2.421563205337722291, 12.46952409297816544 ) ) ;
#8283 = ORIENTED_EDGE ( 'NONE', *, *, #21319, .T. ) ;
#8284 = CARTESIAN_POINT ( 'NONE',  ( 10.48280513895999988, -3.096689368913399854, -6.997844089834400094 ) ) ;
#8285 = VERTEX_POINT ( 'NONE', #31163 ) ;
#8286 = CARTESIAN_POINT ( 'NONE',  ( 9.590596677641999079, 2.445964682955000136, 7.841184989245001624 ) ) ;
#8287 = B_SPLINE_CURVE_WITH_KNOTS ( 'NONE', 3,
 ( #62197, #24459, #14318, #40529, #35643, #56273, #19205, #34958, #45782, #61854, #13973, #35300, #51703, #56955, #9057, #3800, #42263, #31769 ),
 .UNSPECIFIED., .F., .F.,
 ( 4, 2, 2, 2, 2, 2, 2, 2, 4 ),
 ( 0.1254120260046326096, 0.2190586444436944391, 0.3127052628827562963, 0.4063518813218180981, 0.4999984997608799553, 0.5936451181999418125, 0.6872917366390036698, 0.7809383550780655270, 0.8745849735171273842 ),
 .UNSPECIFIED. ) ;
#8288 = DIRECTION ( 'NONE',  ( -1.000000000000000000, 0.000000000000000000, 0.000000000000000000 ) ) ;
#8289 = CARTESIAN_POINT ( 'NONE',  ( 10.19741084123000086, 4.262870449202000422, -8.811513791423999820 ) ) ;
#8290 = CARTESIAN_POINT ( 'NONE',  ( 3.215747102742000152, -0.1032237435928999997, -3.377807273626999951 ) ) ;
#8291 = CARTESIAN_POINT ( 'NONE',  ( 10.64126772939999910, -2.258710642251000156, -6.863482599505999815 ) ) ;
#8292 = CARTESIAN_POINT ( 'NONE',  ( 7.858540647797734202, 2.846821975048335229, -6.797502970372296005 ) ) ;
#8293 = CARTESIAN_POINT ( 'NONE',  ( 23.55066246010500208, 13.34856924552999935, 4.338579446700999931 ) ) ;
#8294 = ORIENTED_EDGE ( 'NONE', *, *, #53094, .T. ) ;
#8295 = CARTESIAN_POINT ( 'NONE',  ( 11.48995257254740032, -5.095356924909000718, 7.181435527216799564 ) ) ;
#8296 = CARTESIAN_POINT ( 'NONE',  ( 10.56491664109999995, 4.212242527248999835, 8.933458498617000032 ) ) ;
#8297 = DIRECTION ( 'NONE',  ( -0.8660254017760760092, -3.364876958529905008E-12, 0.5000000034785859748 ) ) ;
#8298 = ADVANCED_FACE ( 'NONE', ( #56346 ), #38581, .F. ) ;
#8299 = DIRECTION ( 'NONE',  ( -1.000000000000000000, 0.000000000000000000, 0.000000000000000000 ) ) ;
#8301 = CARTESIAN_POINT ( 'NONE',  ( 10.94166666666763987, 5.229667600279960915, 8.191470186740231085 ) ) ;
#8300 = CARTESIAN_POINT ( 'NONE',  ( 10.80815748598999981, 2.937526572573000205, 8.948458885032000154 ) ) ;
#8302 = CARTESIAN_POINT ( 'NONE',  ( 11.11302897915239818, 4.291996373817799970, -8.602736702002999891 ) ) ;
#8303 = EDGE_CURVE ( 'NONE', #42217, #12398, #34482, .T. ) ;
#8304 = CARTESIAN_POINT ( 'NONE',  ( 10.95957739177982226, 2.825857471007950039, -6.683619889684592863 ) ) ;
#8305 = CARTESIAN_POINT ( 'NONE',  ( 9.806988259785999418, 3.868581654116200141, -8.495776841814999258 ) ) ;
#8306 = DIRECTION ( 'NONE',  ( -1.000000000000000000, 0.000000000000000000, 0.000000000000000000 ) ) ;
#8307 = LINE ( 'NONE', #35229, #56209 ) ;
#8308 = CARTESIAN_POINT ( 'NONE',  ( 8.228368194308000483, 4.806758213781000322, 6.177034601037000527 ) ) ;
#8309 = CARTESIAN_POINT ( 'NONE',  ( 10.18308278041000037, 2.953582937013000009, -8.606284720264998356 ) ) ;
#8310 = VERTEX_POINT ( 'NONE', #35631 ) ;
#8311 = CARTESIAN_POINT ( 'NONE',  ( 8.437855646795000553, -2.606998386752999775, 6.345764833140000505 ) ) ;
#8312 = CARTESIAN_POINT ( 'NONE',  ( 18.26224557552276551, 2.355566563843568773, 13.80042983216602259 ) ) ;
#8313 = CARTESIAN_POINT ( 'NONE',  ( 8.564919648097475857, 5.350116636189168773, -7.500005043868485544 ) ) ;
#8314 = DIRECTION ( 'NONE',  ( 0.9999999999938153916, -3.516990153967782703E-06, -1.152484550329262306E-11 ) ) ;
#8315 = ORIENTED_EDGE ( 'NONE', *, *, #27574, .F. ) ;
#8316 = B_SPLINE_CURVE_WITH_KNOTS ( 'NONE', 3,
 ( #4031, #62764, #15575, #9626, #68699, #25714, #41796, #63100, #36903, #58218 ),
 .UNSPECIFIED., .F., .F.,
 ( 4, 2, 2, 2, 4 ),
 ( 0.000000000000000000, 0.2500000000000000000, 0.5000000000000000000, 0.7500000000000000000, 1.000000000000000000 ),
 .UNSPECIFIED. ) ;
#8317 = CARTESIAN_POINT ( 'NONE',  ( 8.860767219592000643, 2.935741164366000522, 6.259844213126999790 ) ) ;
#8318 = ADVANCED_FACE ( 'NONE', ( #67418 ), #57619, .F. ) ;
#8319 = VECTOR ( 'NONE', #166, 1000.000000000000000 ) ;
#8321 = CARTESIAN_POINT ( 'NONE',  ( 11.67766954483535891, 4.715882430684499305, 8.604570063127999546 ) ) ;
#8320 = CARTESIAN_POINT ( 'NONE',  ( 8.555820280412000045, 2.414630869937000046, -6.801495146585999407 ) ) ;
#8322 = CARTESIAN_POINT ( 'NONE',  ( 10.15335165876999923, 3.144981324235999853, -5.860948306964999688 ) ) ;
#8323 = VERTEX_POINT ( 'NONE', #52028 ) ;
#8324 = B_SPLINE_CURVE_WITH_KNOTS ( 'NONE', 3,
 ( #50629, #28978, #55877, #39798 ),
 .UNSPECIFIED., .F., .F.,
 ( 4, 4 ),
 ( 0.000000000000000000, 1.000000000000000000 ),
 .UNSPECIFIED. ) ;
#8325 = CARTESIAN_POINT ( 'NONE',  ( 5.190443173016666023, 0.1963495408493637351, -1.499999999999999778 ) ) ;
#8326 = CARTESIAN_POINT ( 'NONE',  ( 24.84574153431059429, 3.513914038403941564, -11.93620105921934638 ) ) ;
#8327 = CARTESIAN_POINT ( 'NONE',  ( 10.49764694612699856, 2.940513484064000149, 7.077178005756699974 ) ) ;
#8328 = CARTESIAN_POINT ( 'NONE',  ( 9.353731048338000065, -2.823575173856999410, 9.032043499493001448 ) ) ;
#8329 = DIRECTION ( 'NONE',  ( 1.000000000000000000, 0.000000000000000000, 0.000000000000000000 ) ) ;
#8330 = ORIENTED_EDGE ( 'NONE', *, *, #7003, .T. ) ;
#8331 = CARTESIAN_POINT ( 'NONE',  ( 11.55259020248000112, -3.617313325735000085, 11.93403632987999963 ) ) ;
#8332 = CARTESIAN_POINT ( 'NONE',  ( 10.57656694038000111, -5.344897889496000865, -7.298883676216999739 ) ) ;
#8333 = CARTESIAN_POINT ( 'NONE',  ( 8.059281404067426990, -3.659214940308822328, 5.794006878043420627 ) ) ;
#8334 = CARTESIAN_POINT ( 'NONE',  ( 10.03491210303999992, -5.615910465798999773, 7.351455544018000943 ) ) ;
#8335 = CARTESIAN_POINT ( 'NONE',  ( 11.43856039236529831, -2.967715280237000375, -7.550239075043479353 ) ) ;
#8336 = CARTESIAN_POINT ( 'NONE',  ( 9.222809814040999754, -3.385590752329799891, 6.705428891605899722 ) ) ;
#8337 = EDGE_LOOP ( 'NONE', ( #10384, #513, #62071, #6474, #6517 ) ) ;
#8338 = CARTESIAN_POINT ( 'NONE',  ( 10.33482971575999976, -4.577985512478999652, -4.713492043800000530 ) ) ;
#8339 = CARTESIAN_POINT ( 'NONE',  ( 19.39373726536100051, 0.000000000000000000, 0.000000000000000000 ) ) ;
#8340 = EDGE_LOOP ( 'NONE', ( #21266, #32630, #60473, #25648, #49451 ) ) ;
#8341 = CARTESIAN_POINT ( 'NONE',  ( 16.13140881196668630, -3.487052973475988527, -11.11602635788098148 ) ) ;
#8342 = EDGE_LOOP ( 'NONE', ( #53348, #49608, #5197, #35275 ) ) ;
#8343 = CARTESIAN_POINT ( 'NONE',  ( 11.08380555355736163, 3.999999927305438963, -9.033895164528459532 ) ) ;
#8344 = CARTESIAN_POINT ( 'NONE',  ( 9.988985841228000595, 3.986577607995999806, -9.280166295424001177 ) ) ;
#8345 = CARTESIAN_POINT ( 'NONE',  ( 11.09590547754519996, 5.315605332491999846, -7.541753805330609239 ) ) ;
#8346 = CYLINDRICAL_SURFACE ( 'NONE', #62312, 0.5000000000000002220 ) ;
#8347 = CARTESIAN_POINT ( 'NONE',  ( 12.30671156051920612, 2.122656121997152479, -12.53154589464477553 ) ) ;
#8348 = CARTESIAN_POINT ( 'NONE',  ( 11.59256785386839894, -4.832509746210599921, 6.939751505745099358 ) ) ;
#8349 = CARTESIAN_POINT ( 'NONE',  ( 8.400073341230999802, 2.800103557244999930, 9.079946116129001155 ) ) ;
#8350 = EDGE_LOOP ( 'NONE', ( #35809, #43896, #34833, #30574 ) ) ;
#8351 = CARTESIAN_POINT ( 'NONE',  ( 9.708513540183332680, 4.163624617374472869, 8.749999999999996447 ) ) ;
#8352 = AXIS2_PLACEMENT_3D ( 'NONE', #15701, #26541, #65221 ) ;
#8353 = CARTESIAN_POINT ( 'NONE',  ( 7.956793146791999227, -4.524489047957000132, 9.047757046927999980 ) ) ;
#8354 = CARTESIAN_POINT ( 'NONE',  ( 24.13560165115514167, 9.160542504100666505, 9.132857127789494101 ) ) ;
#8355 = ORIENTED_EDGE ( 'NONE', *, *, #38511, .F. ) ;
#8356 = B_SPLINE_SURFACE_WITH_KNOTS ( 'NONE', 3, 3, ( 
 ( #53046, #5829, #69117, #48488 ),
 ( #31381, #21225, #5141, #64892 ),
 ( #48144, #59315, #32416, #594 ),
 ( #58979, #37305, #32076, #15977 ),
 ( #53730, #27166, #10730, #26478 ),
 ( #21903, #63525, #26132, #10043 ),
 ( #54070, #31725, #43242, #247 ),
 ( #21561, #16663, #64549, #64204 ),
 ( #4790, #17006, #37988, #47458 ) ),
 .UNSPECIFIED., .F., .F., .F.,
 ( 4, 1, 1, 1, 1, 1, 4 ),
 ( 4, 4 ),
 ( 0.05136528901824000126, 0.1666666666667000196, 0.3333333333333000081, 0.5000000000000000000, 0.6666666666667000474, 0.8333333333333000637, 0.9784615765758000183 ),
 ( -0.1917159053268999991, 1.191863452461999984 ),
 .UNSPECIFIED. ) ;
#8357 = CARTESIAN_POINT ( 'NONE',  ( 12.37879419969807415, -1.897860824706870453, -12.45625557883630208 ) ) ;
#8358 = CARTESIAN_POINT ( 'NONE',  ( 10.50180110216399854, 3.143606124884799957, 8.023010882787499298 ) ) ;
#8359 = CARTESIAN_POINT ( 'NONE',  ( 9.978906853208000527, -5.007779786185999171, -8.772596342864998675 ) ) ;
#8360 = CARTESIAN_POINT ( 'NONE',  ( 9.140753410162000492, 5.100000000000000533, 6.175944241622000064 ) ) ;
#8361 = CARTESIAN_POINT ( 'NONE',  ( 17.79046541331000242, -3.643254180937999909, -12.02383733079000017 ) ) ;
#8362 = EDGE_CURVE ( 'NONE', #10252, #52199, #22548, .T. ) ;
#8363 = CARTESIAN_POINT ( 'NONE',  ( 9.022188178962251115, 3.408865106546499657, -8.523911321890818016 ) ) ;
#8364 = CARTESIAN_POINT ( 'NONE',  ( 12.47278092208625999, -3.029458323191939861, -13.54674174801984066 ) ) ;
#8365 = EDGE_CURVE ( 'NONE', #69034, #8802, #68104, .T. ) ;
#8366 = DIRECTION ( 'NONE',  ( 0.000000000000000000, 0.000000000000000000, -1.000000000000000000 ) ) ;
#8367 = CARTESIAN_POINT ( 'NONE',  ( 11.36749010443639918, -3.136214309321499805, -7.564597762509089662 ) ) ;
#8368 = CARTESIAN_POINT ( 'NONE',  ( 10.66579975933730040, -2.791514215189000225, -7.084213409908699965 ) ) ;
#8369 = EDGE_CURVE ( 'NONE', #33960, #7236, #24446, .T. ) ;
#8370 = DIRECTION ( 'NONE',  ( 0.000000000000000000, -0.7071067811865475727, 0.7071067811865475727 ) ) ;
#8371 = VERTEX_POINT ( 'NONE', #30718 ) ;
#8372 = ORIENTED_EDGE ( 'NONE', *, *, #30018, .F. ) ;
#8373 =( NAMED_UNIT ( * ) SI_UNIT ( $, .STERADIAN. ) SOLID_ANGLE_UNIT ( ) );
#8374 = CARTESIAN_POINT ( 'NONE',  ( 8.486008579191000933, -3.399999999999999911, 5.976611076844000614 ) ) ;
#8375 = CARTESIAN_POINT ( 'NONE',  ( 18.18005044575082252, 2.500000006795693785, 13.67340643792831045 ) ) ;
#8376 = CARTESIAN_POINT ( 'NONE',  ( 24.57034142978699975, -3.716692469271000387, 12.37044818449999894 ) ) ;
#8377 = CARTESIAN_POINT ( 'NONE',  ( 13.00000000009400303, 11.69118001589999878, 1.923222888683999932 ) ) ;
#8378 = CARTESIAN_POINT ( 'NONE',  ( 17.67527538783543406, 3.190136231796164346, 12.18946489087518970 ) ) ;
#8379 = CARTESIAN_POINT ( 'NONE',  ( -0.2999999999999999889, -1.154700538379000108, 0.000000000000000000 ) ) ;
#8380 = CARTESIAN_POINT ( 'NONE',  ( 9.848730799670999403, 2.769737997918999994, 6.441853401936000090 ) ) ;
#8381 = CARTESIAN_POINT ( 'NONE',  ( 9.257986382567203520, -3.848432872973400087, 6.650284907739020035 ) ) ;
#8382 = B_SPLINE_CURVE_WITH_KNOTS ( 'NONE', 3,
 ( #22818, #44516, #54988, #13036, #34365, #64764, #55685, #59535, #65809, #50091, #7782, #29122, #11631, #33669 ),
 .UNSPECIFIED., .F., .F.,
 ( 4, 2, 2, 2, 2, 2, 4 ),
 ( 0.1253988501910747455, 0.3126983667838658665, 0.4063481250802616351, 0.4999978833766571817, 0.5936476416730528394, 0.6872973999694486080, 0.8745969165622392572 ),
 .UNSPECIFIED. ) ;
#8383 = ORIENTED_EDGE ( 'NONE', *, *, #36136, .T. ) ;
#8384 = CARTESIAN_POINT ( 'NONE',  ( 12.24230779986662476, -2.227307356672650229, 12.51097363402015361 ) ) ;
#8385 = CARTESIAN_POINT ( 'NONE',  ( 10.23557120343299864, -4.042028078047379402, -8.365991721916298474 ) ) ;
#8386 = CARTESIAN_POINT ( 'NONE',  ( 9.945533384955998812, 2.906048475816000121, 8.880389653997999844 ) ) ;
#8387 = CARTESIAN_POINT ( 'NONE',  ( 12.01145123989533126, -3.394760891061399999, 6.331134574721999364 ) ) ;
#8388 = CARTESIAN_POINT ( 'NONE',  ( 11.35502763632549872, 2.839566963815999934, -6.964545474268299508 ) ) ;
#8389 = CARTESIAN_POINT ( 'NONE',  ( 12.47502136616923529, 0.5311517451680617397, 12.68505220952105184 ) ) ;
#8390 = CARTESIAN_POINT ( 'NONE',  ( 7.518864158771000561, 3.206360348473000332, 5.681727837477000165 ) ) ;
#8391 = CARTESIAN_POINT ( 'NONE',  ( 10.12550053024000007, 5.788811067708000024, 7.335561454339999621 ) ) ;
#8392 = CARTESIAN_POINT ( 'NONE',  ( 12.43764207941351607, 1.993980486415519726, 12.55516735266245298 ) ) ;
#8393 = ORIENTED_EDGE ( 'NONE', *, *, #8990, .T. ) ;
#8394 = CARTESIAN_POINT ( 'NONE',  ( 9.544414158773999901, 2.173570076733999823, -8.023168429484000441 ) ) ;
#8395 = CARTESIAN_POINT ( 'NONE',  ( 10.98579841651039857, 3.550031058388499972, -8.696179055230999211 ) ) ;
#8396 = CARTESIAN_POINT ( 'NONE',  ( 11.09998944727679060, 2.658360006774582285, 6.717872455900629092 ) ) ;
#8398 = CARTESIAN_POINT ( 'NONE',  ( 24.57709918591382348, 11.91258060227069393, 3.191967924368984466 ) ) ;
#8397 = CARTESIAN_POINT ( 'NONE',  ( 7.635855646791999796, -2.466384407480000096, 6.935560677555000275 ) ) ;
#8399 = CARTESIAN_POINT ( 'NONE',  ( 10.18531740696900023, -3.813190776280700245, 6.513113677132300161 ) ) ;
#8400 = CARTESIAN_POINT ( 'NONE',  ( 11.70794988689359961, -3.544213289744700290, -8.393984925606600811 ) ) ;
#8401 = VERTEX_POINT ( 'NONE', #35289 ) ;
#8402 = B_SPLINE_CURVE_WITH_KNOTS ( 'NONE', 3,
 ( #42952, #11134, #5879, #48544, #43994, #21960 ),
 .UNSPECIFIED., .F., .F.,
 ( 4, 2, 4 ),
 ( 0.000000000000000000, 0.5000000000000000000, 1.000000000000000000 ),
 .UNSPECIFIED. ) ;
#8403 = CARTESIAN_POINT ( 'NONE',  ( 1.443746307329000000, 3.563994061069000185, 0.4492161910706000127 ) ) ;
#8404 = CARTESIAN_POINT ( 'NONE',  ( 17.93438960660997950, -0.4968201169902036751, -12.68691926186208541 ) ) ;
#8405 = ADVANCED_FACE ( 'NONE', ( #67080 ), #25466, .T. ) ;
#8406 = CARTESIAN_POINT ( 'NONE',  ( 25.00270149670823017, 11.89258197074110335, 2.924337394597763318 ) ) ;
#8407 = CARTESIAN_POINT ( 'NONE',  ( 7.000000000000000000, -6.255435840762999966, 3.000000000000000000 ) ) ;
#8408 = CARTESIAN_POINT ( 'NONE',  ( 13.56683625432869178, 9.108504156368613991, 7.475700167246387196 ) ) ;
#8409 = ADVANCED_FACE ( 'NONE', ( #19193 ), #23288, .T. ) ;
#8410 = CARTESIAN_POINT ( 'NONE',  ( 17.77733961940316121, -1.915504334253006036, -13.78014422891541813 ) ) ;
#8411 = CARTESIAN_POINT ( 'NONE',  ( 4.855026506350000659, 1.500000000000000000, 0.000000000000000000 ) ) ;
#8412 = DIRECTION ( 'NONE',  ( 1.000000000000000000, 0.000000000000000000, 0.000000000000000000 ) ) ;
#8413 = CARTESIAN_POINT ( 'NONE',  ( 8.464254440379999522, -2.029110377978999846, 7.726994002375999315 ) ) ;
#8414 = ORIENTED_EDGE ( 'NONE', *, *, #36053, .T. ) ;
#8415 = CARTESIAN_POINT ( 'NONE',  ( 9.497295280408998508, 3.734279507827999556, 8.942126004519000304 ) ) ;
#8416 = CARTESIAN_POINT ( 'NONE',  ( 13.49999720188825769, -11.61513859405366844, -2.353594668653351096 ) ) ;
#8417 = CARTESIAN_POINT ( 'NONE',  ( 18.08703349541059424, 2.171337118988397208, -13.73770667396175149 ) ) ;
#8418 = CARTESIAN_POINT ( 'NONE',  ( 10.64200660897471451, -3.294104879791286855, 8.705431914969567586 ) ) ;
#8419 = CARTESIAN_POINT ( 'NONE',  ( 1.557293291478000219, 2.591090368091000240, -2.487991068387999771 ) ) ;
#8420 = ORIENTED_EDGE ( 'NONE', *, *, #31889, .F. ) ;
#8421 = CARTESIAN_POINT ( 'NONE',  ( 0.7496340823758137484, 2.944778677366191921, -1.029289356940257694 ) ) ;
#8422 = CARTESIAN_POINT ( 'NONE',  ( 11.47364560330029981, -3.734560974198899874, 8.324524538096799375 ) ) ;
#8423 = CARTESIAN_POINT ( 'NONE',  ( 4.599999999999999645, -0.7192913403693119712, -12.57945229203838267 ) ) ;
#8424 = CARTESIAN_POINT ( 'NONE',  ( 9.701978494675000064, 3.399139198672999740, 6.026757051093999173 ) ) ;
#8425 = VECTOR ( 'NONE', #23958, 1000.000000000000000 ) ;
#8426 = CARTESIAN_POINT ( 'NONE',  ( 11.60948876160955479, 3.304472173606900043, 6.776679950459500112 ) ) ;
#8427 = CARTESIAN_POINT ( 'NONE',  ( 10.39709479648126944, -5.286020290092475094, 7.026710849311109008 ) ) ;
#8428 = CARTESIAN_POINT ( 'NONE',  ( 18.29995268966800026, -2.861739928647000220, -11.98821236628000086 ) ) ;
#8429 = CARTESIAN_POINT ( 'NONE',  ( 12.80505043854143388, 1.836948468694464820, -12.54242247073720051 ) ) ;
#8430 = CARTESIAN_POINT ( 'NONE',  ( 15.96663596566263976, -3.844870426479619852, -11.78010250471071174 ) ) ;
#8431 = CARTESIAN_POINT ( 'NONE',  ( 12.30936054504846311, -2.880824963478894052, 12.35466577905677354 ) ) ;
#8432 = CARTESIAN_POINT ( 'NONE',  ( 7.953337875888457198, 2.248440269089167387, 7.443232059063713102 ) ) ;
#8433 = ORIENTED_EDGE ( 'NONE', *, *, #23039, .T. ) ;
#8434 = CARTESIAN_POINT ( 'NONE',  ( 17.87830683576864033, -3.171613455744689336, 13.63601469363850072 ) ) ;
#8435 = CARTESIAN_POINT ( 'NONE',  ( 25.59997324745700098, -8.218963665681000563, -8.043524865771999544 ) ) ;
#8436 = VERTEX_POINT ( 'NONE', #51690 ) ;
#8437 = VERTEX_POINT ( 'NONE', #46800 ) ;
#8438 = CARTESIAN_POINT ( 'NONE',  ( 24.74122145672611239, -3.111613011112996041, -11.77168806187908778 ) ) ;
#8439 = CARTESIAN_POINT ( 'NONE',  ( 11.04384236319999957, 1.600344243522999976, -5.035088906224999938 ) ) ;
#8440 = CARTESIAN_POINT ( 'NONE',  ( 4.599999999999999645, -1.787816316115923509, 13.88537766212462898 ) ) ;
#8441 = CARTESIAN_POINT ( 'NONE',  ( 9.013423559847998590, 4.933953210258000155, 8.417881984655998906 ) ) ;
#8442 = CARTESIAN_POINT ( 'NONE',  ( 6.949999692073999924, 11.00717859340000082, 1.432487142323000118 ) ) ;
#8443 = FACE_BOUND ( 'NONE', #4996, .T. ) ;
#8444 = CARTESIAN_POINT ( 'NONE',  ( 11.18483536755999808, -2.599651619047000040, 7.740676724427999922 ) ) ;
#8445 = EDGE_CURVE ( 'NONE', #16254, #7548, #9041, .T. ) ;
#8446 = CARTESIAN_POINT ( 'NONE',  ( 18.18333067157144001, -0.3597103837128303727, -12.59488153751295769 ) ) ;
#8447 = CARTESIAN_POINT ( 'NONE',  ( 24.30001683613300045, -12.21047198529999989, -3.271805531187999883 ) ) ;
#8448 = CARTESIAN_POINT ( 'NONE',  ( 11.44133594839949986, -3.430493414882899827, -6.847343244997600387 ) ) ;
#8449 = EDGE_CURVE ( 'NONE', #26212, #2243, #51014, .T. ) ;
#8450 = ADVANCED_FACE ( 'NONE', ( #40515 ), #27763, .F. ) ;
#8451 = CARTESIAN_POINT ( 'NONE',  ( 7.662260841227999997, 2.688365364125000045, 8.140015608605001063 ) ) ;
#8452 = ORIENTED_EDGE ( 'NONE', *, *, #38258, .F. ) ;
#8453 = STYLED_ITEM ( 'NONE', ( #7577 ), #6570 ) ;
#8454 = CARTESIAN_POINT ( 'NONE',  ( 11.12483846379999974, -6.576344547557000375, -5.637698688823999937 ) ) ;
#8455 =( NAMED_UNIT ( * ) PLANE_ANGLE_UNIT ( ) SI_UNIT ( $, .RADIAN. ) );
#8456 = DIRECTION ( 'NONE',  ( 1.000000000000000000, 0.000000000000000000, 0.000000000000000000 ) ) ;
#8457 = DIRECTION ( 'NONE',  ( 0.8480635683784220058, 0.000000000000000000, 0.5298945026977139872 ) ) ;
#8458 = CARTESIAN_POINT ( 'NONE',  ( 9.431076168958000494, 3.350848599899200142, -8.602264418015000302 ) ) ;
#8459 = CARTESIAN_POINT ( 'NONE',  ( 12.12605828839490663, 2.774939115234940967, 13.72225238672862346 ) ) ;
#8460 = CARTESIAN_POINT ( 'NONE',  ( 10.55813551225999980, -2.466564559586000183, 6.633531786299999844 ) ) ;
#8461 = ORIENTED_EDGE ( 'NONE', *, *, #69132, .T. ) ;
#8462 = CARTESIAN_POINT ( 'NONE',  ( 12.26246716472426712, -0.3103928899670306274, -12.69489813901335573 ) ) ;
#8463 = CARTESIAN_POINT ( 'NONE',  ( 12.13047358906991846, 0.2678304234473986578, 13.99744223245316199 ) ) ;
#8464 = ORIENTED_EDGE ( 'NONE', *, *, #18006, .F. ) ;
#8465 = DIRECTION ( 'NONE',  ( -1.000000000000000000, 0.000000000000000000, 0.000000000000000000 ) ) ;
#8466 = CARTESIAN_POINT ( 'NONE',  ( 10.58079553768976666, -5.100000000000000533, -6.662590550605365536 ) ) ;
#8467 = EDGE_CURVE ( 'NONE', #2511, #28950, #17738, .T. ) ;
#8468 = CARTESIAN_POINT ( 'NONE',  ( 8.772923981633081070, 4.310454296184184741, 6.685328252913995684 ) ) ;
#8469 = CARTESIAN_POINT ( 'NONE',  ( 4.367692514209000620, 1.585437927459000029, 0.3774489839997999807 ) ) ;
#8470 = AXIS2_PLACEMENT_3D ( 'NONE', #69011, #21124, #42450 ) ;
#8471 = AXIS2_PLACEMENT_3D ( 'NONE', #20261, #25851, #52766 ) ;
#8472 = CARTESIAN_POINT ( 'NONE',  ( 23.59999441188499958, 10.30760541648000128, -9.317696302454001156 ) ) ;
#8473 = CARTESIAN_POINT ( 'NONE',  ( 0.3839841414396000241, -0.8575131787502999758, -3.600995375387999964 ) ) ;
#8474 = FACE_OUTER_BOUND ( 'NONE', #18888, .T. ) ;
#8475 = CARTESIAN_POINT ( 'NONE',  ( 12.58710648703385360, 3.166459836794169647, 12.19563591444343231 ) ) ;
#8476 = CARTESIAN_POINT ( 'NONE',  ( 9.128137413980999426, -5.235394649229000663, -8.110359502241001550 ) ) ;
#8477 = CARTESIAN_POINT ( 'NONE',  ( 11.68748876160954886, 3.399618311400500303, -8.124372018288600117 ) ) ;
#8478 = CARTESIAN_POINT ( 'NONE',  ( 18.18005043854143565, 2.500000000000000000, -25.00000000000000000 ) ) ;
#8479 = CARTESIAN_POINT ( 'NONE',  ( 10.65413259636999932, 3.216622244594500302, -7.926858177843299380 ) ) ;
#8480 = CARTESIAN_POINT ( 'NONE',  ( 9.885938025973999288, 3.406370524467499994, -6.524634174392399899 ) ) ;
#8482 = CARTESIAN_POINT ( 'NONE',  ( 12.18001542466622844, 2.493364570375297795, 12.45310825070289340 ) ) ;
#8481 = DIRECTION ( 'NONE',  ( -0.000000000000000000, -0.000000000000000000, 1.000000000000000000 ) ) ;
#8483 = CARTESIAN_POINT ( 'NONE',  ( 23.56669596105687248, -13.32134171675407686, 4.273005797680200502 ) ) ;
#8484 = ORIENTED_EDGE ( 'NONE', *, *, #58395, .F. ) ;
#8485 = CARTESIAN_POINT ( 'NONE',  ( 10.35814141025499957, 4.483492689244800822, 6.638851159159999682 ) ) ;
#8486 = CARTESIAN_POINT ( 'NONE',  ( 10.43579701286999928, -2.587605342384000195, 6.390039770907999461 ) ) ;
#8487 = CARTESIAN_POINT ( 'NONE',  ( 10.40644474310099810, 4.893483781708200198, 7.066400461213500073 ) ) ;
#8488 = CARTESIAN_POINT ( 'NONE',  ( 9.150912690312626552, 3.194792839887663938, -7.842306439064141266 ) ) ;
#8489 = CARTESIAN_POINT ( 'NONE',  ( 10.62698276521000196, -3.142914536759000121, 8.668455626664998803 ) ) ;
#8490 = ADVANCED_FACE ( 'NONE', ( #67757 ), #43028, .T. ) ;
#8491 = CARTESIAN_POINT ( 'NONE',  ( 13.50018479229797386, 9.763984779744731668, 6.782114604289404269 ) ) ;
#8492 = CARTESIAN_POINT ( 'NONE',  ( 10.28912155192348621, -2.704284023348029642, -7.938084390888727526 ) ) ;
#8493 = ORIENTED_EDGE ( 'NONE', *, *, #1740, .T. ) ;
#8494 = CARTESIAN_POINT ( 'NONE',  ( 9.531329965421999617, -4.793057006135000186, -8.321459087847200564 ) ) ;
#8495 = FACE_OUTER_BOUND ( 'NONE', #53902, .T. ) ;
#8496 = CARTESIAN_POINT ( 'NONE',  ( 17.91108626730879649, 1.853415294216377962, -12.46294044425349945 ) ) ;
#8497 = CARTESIAN_POINT ( 'NONE',  ( 8.517762173746001864, -3.198146119290998346, -6.396303957889001524 ) ) ;
#8498 = AXIS2_PLACEMENT_3D ( 'NONE', #6054, #44527, #11300 ) ;
#8499 = DIRECTION ( 'NONE',  ( -1.000000000000000000, 0.000000000000000000, 0.000000000000000000 ) ) ;
#8500 = CARTESIAN_POINT ( 'NONE',  ( 7.832795987768000678, 2.851255020980998811, 6.795938453665997692 ) ) ;
#8501 = CARTESIAN_POINT ( 'NONE',  ( 9.656157842586999607, -4.949038487346999915, -8.498994087616001281 ) ) ;
#8502 = CARTESIAN_POINT ( 'NONE',  ( 0.8113901325419543564, -3.500000000000000888, -0.4581489286485119217 ) ) ;
#8503 = VERTEX_POINT ( 'NONE', #9640 ) ;
#8504 = CARTESIAN_POINT ( 'NONE',  ( 17.74431590774614165, 1.811500042942241873, -13.88231098336932590 ) ) ;
#8505 = CARTESIAN_POINT ( 'NONE',  ( 23.60000000000000142, -9.517611874540000017, -8.103398312166000039 ) ) ;
#8506 = CARTESIAN_POINT ( 'NONE',  ( 23.58937261997547807, 13.38214254373811407, 4.047428957154697748 ) ) ;
#8507 = CARTESIAN_POINT ( 'NONE',  ( 8.933148997457999840, -5.167567567567999731, 6.822293592207000934 ) ) ;
#8508 = DIRECTION ( 'NONE',  ( 1.000000000000000000, 0.000000000000000000, 0.000000000000000000 ) ) ;
#8509 = CARTESIAN_POINT ( 'NONE',  ( 8.822164158776001130, 2.644017913812000131, -7.838184857420000817 ) ) ;
#8510 = CARTESIAN_POINT ( 'NONE',  ( 11.96595122972050085, -3.656201404350900130, 8.295047870239098842 ) ) ;
#8511 = ORIENTED_EDGE ( 'NONE', *, *, #63757, .F. ) ;
#8512 = AXIS2_PLACEMENT_3D ( 'NONE', #46241, #67204, #18297 ) ;
#8513 = CARTESIAN_POINT ( 'NONE',  ( 4.000000000000000000, 1.321180510578203071, 1.719428477289353552 ) ) ;
#8514 = CARTESIAN_POINT ( 'NONE',  ( 17.97976423439214955, 3.110159202364623621, -13.65016833014880859 ) ) ;
#8515 = ORIENTED_EDGE ( 'NONE', *, *, #3228, .T. ) ;
#8516 = CARTESIAN_POINT ( 'NONE',  ( 9.984696787962999309, -3.851113559088000127, 8.354131589521699652 ) ) ;
#8517 = CARTESIAN_POINT ( 'NONE',  ( 24.89161351175072312, 3.022277498610428825, 11.64684786725776533 ) ) ;
#8518 = CARTESIAN_POINT ( 'NONE',  ( 9.102795280413999990, 3.071719032003000116, -6.037263251225000182 ) ) ;
#8519 = CARTESIAN_POINT ( 'NONE',  ( 8.795853127542962113, 4.029789221522052323, -8.445853177989366856 ) ) ;
#8520 = CARTESIAN_POINT ( 'NONE',  ( 11.23078751119019891, -4.915752892793999962, -7.979095341142500075 ) ) ;
#8521 = ADVANCED_BREP_SHAPE_REPRESENTATION ( '', ( #6570, #9676 ), #42081 ) ;
#8522 = CARTESIAN_POINT ( 'NONE',  ( 4.600000207916445483, 13.27499874714999883, 0.000000000000000000 ) ) ;
#8523 = DIRECTION ( 'NONE',  ( 0.000000000000000000, 0.9916377111174247139, -0.1290528957048031888 ) ) ;
#8524 = ORIENTED_EDGE ( 'NONE', *, *, #13444, .F. ) ;
#8525 = CARTESIAN_POINT ( 'NONE',  ( 7.858238185142895738, 2.638874411158420141, -7.614836700234859812 ) ) ;
#8526 = ADVANCED_FACE ( 'NONE', ( #47061 ), #55666, .T. ) ;
#8527 = CARTESIAN_POINT ( 'NONE',  ( 10.72934687351566652, -4.163624617374463099, 8.750000000000000000 ) ) ;
#8528 = CARTESIAN_POINT ( 'NONE',  ( 18.14066966380071833, -2.280775195390137178, 13.71753029190269046 ) ) ;
#8529 = ORIENTED_EDGE ( 'NONE', *, *, #62917, .T. ) ;
#8530 = CARTESIAN_POINT ( 'NONE',  ( 10.95552360838999917, 4.744046441415999738, -9.198140387677000263 ) ) ;
#8531 = FILL_AREA_STYLE ('',( #24612 ) ) ;
#8532 = VERTEX_POINT ( 'NONE', #27028 ) ;
#8533 = CARTESIAN_POINT ( 'NONE',  ( 8.619480666858999385, 4.380700808321400075, 6.423523106103999680 ) ) ;
#8534 = CARTESIAN_POINT ( 'NONE',  ( 17.86252378965070164, -3.131846597291660927, -12.20457061699601375 ) ) ;
#8535 = CARTESIAN_POINT ( 'NONE',  ( 16.09999335515345464, 3.810015139075933366, 11.93171563566236948 ) ) ;
#8536 = CARTESIAN_POINT ( 'NONE',  ( 4.400000000000000355, -0.7080094843779000113, -0.8552562627201000245 ) ) ;
#8537 = DIRECTION ( 'NONE',  ( 0.8660254037844289376, 0.000000000000000000, -0.5000000000000169864 ) ) ;
#8538 = EDGE_LOOP ( 'NONE', ( #42409, #40463, #60314, #50560, #37986 ) ) ;
#8539 = CARTESIAN_POINT ( 'NONE',  ( 11.60000000000000142, 3.450002592736672646, 6.620235306175750623 ) ) ;
#8540 = CARTESIAN_POINT ( 'NONE',  ( 10.16008584122999991, 4.812959680871000678, -8.526582921144999716 ) ) ;
#8541 = EDGE_CURVE ( 'NONE', #50591, #13432, #37530, .T. ) ;
#8542 = B_SPLINE_CURVE_WITH_KNOTS ( 'NONE', 3,
 ( #51291, #67355, #34193, #45368 ),
 .UNSPECIFIED., .F., .F.,
 ( 4, 4 ),
 ( 0.000000000000000000, 1.000000000000000000 ),
 .UNSPECIFIED. ) ;
#8543 = CARTESIAN_POINT ( 'NONE',  ( 11.09999999999999964, -4.000000000000000000, 7.500000000000000000 ) ) ;
#8544 = CARTESIAN_POINT ( 'NONE',  ( 12.12630585043895159, 2.775512167237635275, -13.72213635400578191 ) ) ;
#8545 = AXIS2_PLACEMENT_3D ( 'NONE', #10055, #5838, #36283 ) ;
#8546 = CARTESIAN_POINT ( 'NONE',  ( 9.910317406968998100, -3.787635830142400462, -8.621889436328999068 ) ) ;
#8547 = EDGE_CURVE ( 'NONE', #37826, #13082, #22111, .T. ) ;
#8548 = CARTESIAN_POINT ( 'NONE',  ( 17.67321579093595219, 0.7208442004938064862, 13.98143072948223775 ) ) ;
#8549 = VECTOR ( 'NONE', #31731, 999.9999999999998863 ) ;
#8550 = CARTESIAN_POINT ( 'NONE',  ( 10.90635170712999980, -3.089674976714000376, -6.534319251717000121 ) ) ;
#8551 = ORIENTED_EDGE ( 'NONE', *, *, #69048, .T. ) ;
#8552 = VERTEX_POINT ( 'NONE', #4394 ) ;
#8553 = CARTESIAN_POINT ( 'NONE',  ( 9.517835841233001304, 4.883347899767999323, -6.417062834774999835 ) ) ;
#8554 = CARTESIAN_POINT ( 'NONE',  ( 9.265220490506111517, 5.204037557847910556, 8.765935439646369787 ) ) ;
#8555 = CARTESIAN_POINT ( 'NONE',  ( 12.21945847189276435, -2.718477924323257966, 13.62469170132030705 ) ) ;
#8556 = CARTESIAN_POINT ( 'NONE',  ( 25.08237298766499990, 8.543494775977999112, -8.158987811473000562 ) ) ;
#8557 = B_SPLINE_CURVE_WITH_KNOTS ( 'NONE', 3,
 ( #7062, #18251, #65437, #60208 ),
 .UNSPECIFIED., .F., .F.,
 ( 4, 4 ),
 ( 0.000000000000000000, 1.000000000000000000 ),
 .UNSPECIFIED. ) ;
#8558 = CARTESIAN_POINT ( 'NONE',  ( 25.27000123253231223, -3.169726888505174145, -11.48329030453897914 ) ) ;
#8559 = CARTESIAN_POINT ( 'NONE',  ( 10.34588779216199939, 4.801941500727100021, -7.789199634454999632 ) ) ;
#8561 = DIRECTION ( 'NONE',  ( 1.000000000000000000, 0.000000000000000000, 0.000000000000000000 ) ) ;
#8560 = CARTESIAN_POINT ( 'NONE',  ( 10.13169678796399964, -3.803923679411099990, 8.624850445389000697 ) ) ;
#8562 = CARTESIAN_POINT ( 'NONE',  ( 8.627495311384997478, -5.082984106378005684, -6.521832623478995394 ) ) ;
#8563 = VERTEX_POINT ( 'NONE', #14898 ) ;
#8564 = AXIS2_PLACEMENT_3D ( 'NONE', #44284, #3329, #39368 ) ;
#8565 = DIRECTION ( 'NONE',  ( 0.000000000000000000, -1.000000000000000000, 0.000000000000000000 ) ) ;
#8566 = CARTESIAN_POINT ( 'NONE',  ( 23.60205915885299888, -11.56239291746998710, -3.974820703396001242 ) ) ;
#8567 = CARTESIAN_POINT ( 'NONE',  ( 9.751735624253999646, -3.361793157411000266, -5.915550373431999631 ) ) ;
#8568 = DIRECTION ( 'NONE',  ( 0.000000000000000000, -0.6195591179857913300, 0.7849499979748191247 ) ) ;
#8569 = CARTESIAN_POINT ( 'NONE',  ( 25.59994555223599733, -2.024003533649000097, 11.01554633311000053 ) ) ;
#8570 = FACE_OUTER_BOUND ( 'NONE', #44875, .T. ) ;
#8571 = FACE_OUTER_BOUND ( 'NONE', #17035, .T. ) ;
#8572 = CARTESIAN_POINT ( 'NONE',  ( 10.22272469555899832, 4.639546521693399761, 8.606479382885998675 ) ) ;
#8573 =( LENGTH_UNIT ( ) NAMED_UNIT ( * ) SI_UNIT ( .MILLI., .METRE. ) );
#8574 = DIRECTION ( 'NONE',  ( 0.000000000000000000, -1.000000000000000000, 0.000000000000000000 ) ) ;
#8575 = CARTESIAN_POINT ( 'NONE',  ( 2.395018178493999894, 1.174603829501999819, 3.040001730748000508 ) ) ;
#8576 = ORIENTED_EDGE ( 'NONE', *, *, #63735, .T. ) ;
#8577 = B_SPLINE_CURVE_WITH_KNOTS ( 'NONE', 3,
 ( #47399, #58224, #52986, #51011, #31320, #41464, #21167, #30981, #24444 ),
 .UNSPECIFIED., .F., .F.,
 ( 4, 1, 1, 1, 1, 1, 4 ),
 ( 0.000000000000000000, 0.1176715969261405564, 0.3173201826739889819, 0.5169687684225861002, 0.7166173541704345951, 0.9162659399182834230, 1.000000000000000000 ),
 .UNSPECIFIED. ) ;
#8578 = CARTESIAN_POINT ( 'NONE',  ( 12.41659929819182473, -0.4896501542853357036, -12.68729270499358108 ) ) ;
#8579 = SHAPE_REPRESENTATION ( 'Airflow Sleeve', ( #9676 ), #58898 ) ;
#8580 = CARTESIAN_POINT ( 'NONE',  ( 5.700000000000000178, 13.04986661130000059, 1.811520473896000016 ) ) ;
#8581 = CARTESIAN_POINT ( 'NONE',  ( 11.00000000000000000, 2.941427501403999667, 7.174999999999999822 ) ) ;
#8582 = LINE ( 'NONE', #25003, #31240 ) ;
#8583 = CARTESIAN_POINT ( 'NONE',  ( 10.47253786429000044, -2.899999999999999911, -6.571291218949999902 ) ) ;
#8584 = ORIENTED_EDGE ( 'NONE', *, *, #23148, .T. ) ;
#8585 = CARTESIAN_POINT ( 'NONE',  ( 5.946864308364999907, -0.03293945794144000072, -1.175625617539999945 ) ) ;
#8586 = APPLICATION_PROTOCOL_DEFINITION ( 'draft international standard', 'automotive_design', 1998, #56566 ) ;
#8587 = CARTESIAN_POINT ( 'NONE',  ( 17.63677106488414026, 0.6210356003491741550, 12.67955509032280048 ) ) ;
#8588 = CARTESIAN_POINT ( 'NONE',  ( 13.09162860438300058, -11.49399796109000071, -1.653788228654999859 ) ) ;
#8589 = CARTESIAN_POINT ( 'NONE',  ( 7.803806111238657195, 2.990843308588816640, 6.553755180521002366 ) ) ;
#8590 = CARTESIAN_POINT ( 'NONE',  ( 11.14767835872009982, 3.125658946326500320, -6.948943352864199952 ) ) ;
#8591 = ORIENTED_EDGE ( 'NONE', *, *, #36867, .T. ) ;
#8592 = AXIS2_PLACEMENT_3D ( 'NONE', #19642, #8465, #50773 ) ;
#8593 = CARTESIAN_POINT ( 'NONE',  ( 10.62792628238999981, -3.100579357212000176, 8.599905962393000536 ) ) ;
#8594 = ORIENTED_EDGE ( 'NONE', *, *, #68408, .F. ) ;
#8595 = CARTESIAN_POINT ( 'NONE',  ( 8.379867906070000316, -2.923743482135000349, 6.439439799216000182 ) ) ;
#8596 = CARTESIAN_POINT ( 'NONE',  ( 7.443293146792999693, -4.698358408974000255, 8.789434435623999065 ) ) ;
#8597 = CARTESIAN_POINT ( 'NONE',  ( 18.21571869486623996, -0.3016537271415190569, -13.99676704218776813 ) ) ;
#8598 = ORIENTED_EDGE ( 'NONE', *, *, #15016, .F. ) ;
#8599 = CARTESIAN_POINT ( 'NONE',  ( 10.97977755915654541, 8.327332208918569734, -6.553115839673279375 ) ) ;
#8600 = CARTESIAN_POINT ( 'NONE',  ( 11.04859286640970417, -4.978068212541741033, -8.665561624479661162 ) ) ;
#8601 = CARTESIAN_POINT ( 'NONE',  ( 7.640239158768000749, 5.144639763962000067, -8.301783154141999077 ) ) ;
#8602 = AXIS2_PLACEMENT_3D ( 'NONE', #14176, #19066, #14858 ) ;
#8603 = CYLINDRICAL_SURFACE ( 'NONE', #29780, 0.5000000000000000000 ) ;
#8604 = CARTESIAN_POINT ( 'NONE',  ( 17.92118024654466168, -3.006907963399408690, 12.31891425463948941 ) ) ;
#8605 = ORIENTED_EDGE ( 'NONE', *, *, #56125, .F. ) ;
#8606 = CARTESIAN_POINT ( 'NONE',  ( 9.099999931440999390, -2.935682118448999844, -8.155535999783198875 ) ) ;
#8607 = ADVANCED_FACE ( 'NONE', ( #43456 ), #21245, .T. ) ;
#8608 = EDGE_CURVE ( 'NONE', #45386, #855, #19954, .T. ) ;
#8609 = CARTESIAN_POINT ( 'NONE',  ( 11.60000000000000320, 4.590480015894799593, 8.459313701734300750 ) ) ;
#8610 = CARTESIAN_POINT ( 'NONE',  ( 5.584193173016749334, -1.460959015002474937, 0.3926218265389144757 ) ) ;
#8611 = CARTESIAN_POINT ( 'NONE',  ( 9.758513540182331525, 4.163624617374472869, 8.749999999999996447 ) ) ;
#8612 = VECTOR ( 'NONE', #58961, 1000.000000000000000 ) ;
#8613 = DIRECTION ( 'NONE',  ( -1.000000000000000000, 0.000000000000000000, 0.000000000000000000 ) ) ;
#8614 = VERTEX_POINT ( 'NONE', #14052 ) ;
#8615 = CARTESIAN_POINT ( 'NONE',  ( 17.69809243813181254, 0.6087680664020044263, -13.88205110007294607 ) ) ;
#8616 = CARTESIAN_POINT ( 'NONE',  ( 10.94592196013603136, -2.831029695124928747, -6.714227100558820993 ) ) ;
#8617 = CARTESIAN_POINT ( 'NONE',  ( 24.14104189581271953, -3.327735444545656840, -12.48993067524683021 ) ) ;
#8618 = CARTESIAN_POINT ( 'NONE',  ( 3.198890132544458531, -2.798833948393640192, 2.150913519912191152 ) ) ;
#8619 = AXIS2_PLACEMENT_3D ( 'NONE', #5654, #32585, #27337 ) ;
#8620 = CARTESIAN_POINT ( 'NONE',  ( 12.29653044000528617, -0.3639325664385079095, -13.89360161040561970 ) ) ;
#8621 = CARTESIAN_POINT ( 'NONE',  ( 18.17458387927301899, -2.583096938294931366, 12.43185036011799305 ) ) ;
#8622 = ORIENTED_EDGE ( 'NONE', *, *, #62974, .F. ) ;
#8623 = CARTESIAN_POINT ( 'NONE',  ( 10.93990547754509812, -2.967013601007999934, -7.532784233952049213 ) ) ;
#8624 = ORIENTED_EDGE ( 'NONE', *, *, #36751, .T. ) ;
#8625 = CARTESIAN_POINT ( 'NONE',  ( 9.757669403192000601, 4.489270656625000022, 5.986034819543999852 ) ) ;
#8626 = CYLINDRICAL_SURFACE ( 'NONE', #22189, 12.52500000000000036 ) ;
#8627 = CARTESIAN_POINT ( 'NONE',  ( 9.716735841232001292, 3.941185585667000169, -8.896279800194999865 ) ) ;
#8628 = CARTESIAN_POINT ( 'NONE',  ( 3.229260370471000119, -3.128337010252999928, 1.990763144092999593 ) ) ;
#8629 = EDGE_CURVE ( 'NONE', #45182, #48412, #14395, .T. ) ;
#8630 = CARTESIAN_POINT ( 'NONE',  ( 10.68054891417000007, -2.768175152062000155, -6.114413274984999980 ) ) ;
#8631 = DIRECTION ( 'NONE',  ( 2.186520856378935359E-10, -0.9979498542811711115, 0.06400069015400811079 ) ) ;
#8632 = CARTESIAN_POINT ( 'NONE',  ( 23.62001755077699983, 13.19613008251999986, 4.178531453471999946 ) ) ;
#8633 = ORIENTED_EDGE ( 'NONE', *, *, #35876, .T. ) ;
#8634 = CARTESIAN_POINT ( 'NONE',  ( 11.98225819896750011, -5.120994791668000090, 7.288668995979000087 ) ) ;
#8635 = CARTESIAN_POINT ( 'NONE',  ( 10.15902941591999920, 4.166415211384999040, 9.114163806478000396 ) ) ;
#8636 = CARTESIAN_POINT ( 'NONE',  ( 15.72310803393400036, 9.201544169428000686, 8.280720087647999605 ) ) ;
#8637 = CARTESIAN_POINT ( 'NONE',  ( 8.079129440378000737, -3.524751762020000179, 5.573845465339999805 ) ) ;
#8639 = CARTESIAN_POINT ( 'NONE',  ( 17.80000000005199823, -3.345268251980999974, 11.86064071431999878 ) ) ;
#8638 = CARTESIAN_POINT ( 'NONE',  ( 10.00138108374000012, 3.855364958793999985, 5.709478909302000638 ) ) ;
#8640 = CARTESIAN_POINT ( 'NONE',  ( 11.18687482311539938, 5.057677595549000316, -7.927326830586499007 ) ) ;
#8641 = AXIS2_PLACEMENT_3D ( 'NONE', #405, #37811, #11235 ) ;
#8642 = CARTESIAN_POINT ( 'NONE',  ( 11.00624930493297882, 2.793750695071733681, -6.598047929500610032 ) ) ;
#8643 = CARTESIAN_POINT ( 'NONE',  ( 9.452380199233999747, 4.996570247675600207, -7.374740103075099640 ) ) ;
#8644 = CARTESIAN_POINT ( 'NONE',  ( 18.10028187597347582, -0.4746736627229541927, 12.59106879393900513 ) ) ;
#8645 = CARTESIAN_POINT ( 'NONE',  ( 24.66271477989500127, 3.625397779087000227, 12.20587930303000057 ) ) ;
#8646 = B_SPLINE_CURVE_WITH_KNOTS ( 'NONE', 3,
 ( #8343, #8001, #50990, #2749 ),
 .UNSPECIFIED., .F., .F.,
 ( 4, 4 ),
 ( 0.8675649130336897663, 1.000000000000000000 ),
 .UNSPECIFIED. ) ;
#8647 = CARTESIAN_POINT ( 'NONE',  ( 23.50387503050299998, 0.01709925755191780278, -13.79998940635069005 ) ) ;
#8648 = VECTOR ( 'NONE', #7607, 1000.000000000000000 ) ;
#8649 = CARTESIAN_POINT ( 'NONE',  ( 23.74238067972500232, 9.838688633414999885, 9.383767474846001377 ) ) ;
#8650 = EDGE_LOOP ( 'NONE', ( #1762, #68053, #10448, #45691 ) ) ;
#8651 = CARTESIAN_POINT ( 'NONE',  ( 8.154706853209001238, -4.255646685191999623, 9.114089645792999406 ) ) ;
#8652 = CARTESIAN_POINT ( 'NONE',  ( 17.55505043854143565, 3.125000000000000000, 13.52078605991414939 ) ) ;
#8653 = CARTESIAN_POINT ( 'NONE',  ( 8.642077642326000841, 2.899999999999999911, 6.463854830420999953 ) ) ;
#8654 = CARTESIAN_POINT ( 'NONE',  ( 10.24457120343299898, 3.957971921952620598, 6.634008278083699750 ) ) ;
#8655 = EDGE_LOOP ( 'NONE', ( #21146, #13733, #16496, #42396, #28053, #51499 ) ) ;
#8656 = CIRCLE ( 'NONE', #44410, 1.100000000000000089 ) ;
#8657 = CARTESIAN_POINT ( 'NONE',  ( 9.026926658770998202, 4.852728889087999598, 8.683917172082999514 ) ) ;
#8659 = CARTESIAN_POINT ( 'NONE',  ( 11.43856039236529831, 5.032284719763000069, 7.449760924956519759 ) ) ;
#8658 = CARTESIAN_POINT ( 'NONE',  ( 8.826138961223998436, -3.281636118526699786, -7.985449642667900250 ) ) ;
#8660 = CARTESIAN_POINT ( 'NONE',  ( 10.20607971959000082, 2.622352165399999713, -6.528536464360000124 ) ) ;
#8661 = ADVANCED_FACE ( 'NONE', ( #61939 ), #14400, .F. ) ;
#8662 = ORIENTED_EDGE ( 'NONE', *, *, #30159, .F. ) ;
#8663 = ADVANCED_FACE ( 'NONE', ( #57034 ), #9136, .F. ) ;
#8664 = CARTESIAN_POINT ( 'NONE',  ( 1.415556799207333905, -0.4581489286485083134, -3.500000000000000888 ) ) ;
#8665 = AXIS2_PLACEMENT_3D ( 'NONE', #50632, #9337, #66356 ) ;
#8666 = CARTESIAN_POINT ( 'NONE',  ( 9.416094968574279633, -5.100000000000000533, -6.473186325184255629 ) ) ;
#8667 = CARTESIAN_POINT ( 'NONE',  ( 11.67918044953561996, 5.011483761127000669, 6.972563939641199582 ) ) ;
#8668 = CARTESIAN_POINT ( 'NONE',  ( 10.91307648679999964, -2.096298111716999646, 7.827187677719999570 ) ) ;
#8669 = DIRECTION ( 'NONE',  ( 0.7071067811865474617, -0.7071067811865474617, 1.247903205617082848E-09 ) ) ;
#8670 = ORIENTED_EDGE ( 'NONE', *, *, #46449, .T. ) ;
#8671 = CARTESIAN_POINT ( 'NONE',  ( 11.84748603848200155, -3.299681227315999887, 11.83395064283000053 ) ) ;
#8672 = CARTESIAN_POINT ( 'NONE',  ( 10.91732944037999964, -3.256268970540999952, -6.361552695759000287 ) ) ;
#8673 = CARTESIAN_POINT ( 'NONE',  ( 8.128394320951036534, -5.084803757088047327, 6.140078532315731863 ) ) ;
#8674 = CARTESIAN_POINT ( 'NONE',  ( 11.05435090131019926, -2.880552878538999995, -8.192386390235398608 ) ) ;
#8675 = CARTESIAN_POINT ( 'NONE',  ( 9.220797255587999786, -2.859210004667000149, 7.548297453605989027 ) ) ;
#8676 = ORIENTED_EDGE ( 'NONE', *, *, #5136, .F. ) ;
#8677 = CARTESIAN_POINT ( 'NONE',  ( 2.855140132543084519, -0.9161175952574772685, -3.408904368339104707 ) ) ;
#8678 = CARTESIAN_POINT ( 'NONE',  ( 11.04272335273199879, -3.555125495332600138, 6.301916924546999255 ) ) ;
#8679 = ORIENTED_EDGE ( 'NONE', *, *, #324, .T. ) ;
#8680 = DIRECTION ( 'NONE',  ( -1.000000000000000000, 0.000000000000000000, -5.786858784138000079E-14 ) ) ;
#8681 = ORIENTED_EDGE ( 'NONE', *, *, #55577, .T. ) ;
#8682 = CARTESIAN_POINT ( 'NONE',  ( 9.221132306829000314, -4.645169647889000331, -5.840816811670999975 ) ) ;
#8683 = CARTESIAN_POINT ( 'NONE',  ( 10.97413042750000045, -2.700916140920000430, -4.938597722914999544 ) ) ;
#8684 = CARTESIAN_POINT ( 'NONE',  ( 11.76077869730539938, 3.404661623424200201, -6.326049646822999861 ) ) ;
#8685 = CARTESIAN_POINT ( 'NONE',  ( 18.50001572531400029, 2.908166856580999937, -12.18270046149000052 ) ) ;
#8686 = CARTESIAN_POINT ( 'NONE',  ( 12.42174667009958533, 2.006228232438482362, -12.55302761990816407 ) ) ;
#8687 = AXIS2_PLACEMENT_3D ( 'NONE', #67329, #52293, #4388 ) ;
#8688 = CARTESIAN_POINT ( 'NONE',  ( 10.97303166480599934, -5.137916160623999140, 7.419769534118209720 ) ) ;
#8689 = CARTESIAN_POINT ( 'NONE',  ( 8.143323341229999457, 5.061727314042999915, 5.824077473724000420 ) ) ;
#8691 = EDGE_CURVE ( 'NONE', #12641, #58572, #53251, .T. ) ;
#8690 = B_SPLINE_CURVE_WITH_KNOTS ( 'NONE', 3,
 ( #24923, #56049, #2230, #51157 ),
 .UNSPECIFIED., .F., .F.,
 ( 4, 4 ),
 ( 0.000000000000000000, 1.000000000000000000 ),
 .UNSPECIFIED. ) ;
#8692 = ORIENTED_EDGE ( 'NONE', *, *, #22654, .T. ) ;
#8693 = CARTESIAN_POINT ( 'NONE',  ( 7.609170034105995128, 3.848214081969753231, 8.855880787058648451 ) ) ;
#8694 = VECTOR ( 'NONE', #55980, 1000.000000000000000 ) ;
#8695 = ADVANCED_FACE ( 'NONE', ( #62613 ), #16791, .F. ) ;
#8696 = CARTESIAN_POINT ( 'NONE',  ( 9.368918146792999835, -5.618388245857000030, 7.727743016644000207 ) ) ;
#8697 = DIRECTION ( 'NONE',  ( -0.9486832980505238710, -8.389522287884208957E-10, 0.3162277660168079652 ) ) ;
#8698 = ORIENTED_EDGE ( 'NONE', *, *, #28343, .F. ) ;
#8699 = CARTESIAN_POINT ( 'NONE',  ( 12.48081329218153002, -1.836727633573115970, -12.46541050266128181 ) ) ;
#8700 = CARTESIAN_POINT ( 'NONE',  ( 11.30579707368350029, 3.365167912142600137, 8.609190966793999422 ) ) ;
#8701 = CONICAL_SURFACE ( 'NONE', #28830, 8.515178490300000291, 1.329165865441747751 ) ;
#8702 = CARTESIAN_POINT ( 'NONE',  ( 10.96333185321000059, -5.283547384770999500, -8.592770849731000027 ) ) ;
#8703 = CARTESIAN_POINT ( 'NONE',  ( 14.46666666253433498, 8.815232490335741744, 7.616703758276837988 ) ) ;
#8704 = CARTESIAN_POINT ( 'NONE',  ( 18.44718133169100227, -2.901187496916000086, -12.12896678136999995 ) ) ;
#8705 = CARTESIAN_POINT ( 'NONE',  ( 24.61098151485200347, -8.751788807863999153, 9.056922189874999418 ) ) ;
#8706 = CARTESIAN_POINT ( 'NONE',  ( 12.43989325004536362, -3.148871498663014634, -13.64128470488402201 ) ) ;
#8707 = AXIS2_PLACEMENT_3D ( 'NONE', #51882, #25318, #19042 ) ;
#8708 = CARTESIAN_POINT ( 'NONE',  ( 11.13349010443639919, -2.725546193138000284, -7.595309363461700158 ) ) ;
#8709 = CARTESIAN_POINT ( 'NONE',  ( 24.30000000000000071, 9.305479840184000651, -8.315530346521999405 ) ) ;
#8710 = ORIENTED_EDGE ( 'NONE', *, *, #65643, .F. ) ;
#8711 = EDGE_LOOP ( 'NONE', ( #3777, #29558, #62418, #56276 ) ) ;
#8712 = SURFACE_SIDE_STYLE ('',( #30385 ) ) ;
#8713 = DIRECTION ( 'NONE',  ( -1.000000000000000000, 0.000000000000000000, 0.000000000000000000 ) ) ;
#8714 = CARTESIAN_POINT ( 'NONE',  ( 18.01235687062835567, 2.926439070439386558, 13.57366610795702755 ) ) ;
#8715 = CARTESIAN_POINT ( 'NONE',  ( 10.01597178489000051, 4.792666960550000077, -6.390258598531999290 ) ) ;
#8716 = ADVANCED_FACE ( 'NONE', ( #37770 ), #16780, .F. ) ;
#8717 = PLANE ( 'NONE',  #52064 ) ;
#8718 = CARTESIAN_POINT ( 'NONE',  ( 18.02661896923962104, 2.910306870311579530, 12.34644497411517428 ) ) ;
#8719 = CARTESIAN_POINT ( 'NONE',  ( 20.10000000000000142, 12.35000000006999876, 0.000000000000000000 ) ) ;
#8720 = CARTESIAN_POINT ( 'NONE',  ( 10.43579914648999996, 2.587602126999999808, 6.390037244031000263 ) ) ;
#8721 = CARTESIAN_POINT ( 'NONE',  ( 9.524266954400626872, -4.325581995510845879, 8.312113682386053526 ) ) ;
#8722 = ORIENTED_EDGE ( 'NONE', *, *, #64091, .T. ) ;
#8723 = CARTESIAN_POINT ( 'NONE',  ( 12.36741688735896361, -2.053674487412247451, 12.54445365011033608 ) ) ;
#8724 = CARTESIAN_POINT ( 'NONE',  ( 9.224417874593999755, -4.924352284713100047, -7.892956936667999912 ) ) ;
#8725 = CARTESIAN_POINT ( 'NONE',  ( 9.646287586158999616, 2.591467678478000192, 6.760055064032999717 ) ) ;
#8726 = CARTESIAN_POINT ( 'NONE',  ( 11.47124174884019965, -4.036194082918090231, 6.184229974648999928 ) ) ;
#8727 = CARTESIAN_POINT ( 'NONE',  ( 8.780820280412001466, 2.567871051582000241, -6.869011921437000012 ) ) ;
#8728 = PRODUCT ( 'O Ring Seal 1', 'O Ring Seal 1', '', ( #51573 ) ) ;
#8729 = CARTESIAN_POINT ( 'NONE',  ( 10.78887616594230003, 3.613544262574699850, -6.281817606595999415 ) ) ;
#8730 = CARTESIAN_POINT ( 'NONE',  ( 12.33502333850778143, 0.4124490627810437071, 12.69099791225215235 ) ) ;
#8731 = CARTESIAN_POINT ( 'NONE',  ( 7.775614158771000817, 4.636729845879000500, 9.378977473003999421 ) ) ;
#8732 = CARTESIAN_POINT ( 'NONE',  ( 10.93227693248999977, 2.539877577705000000, 6.453611809651000009 ) ) ;
#8733 = CARTESIAN_POINT ( 'NONE',  ( 12.38986377076836476, 2.032719501308456245, 12.54823268863295382 ) ) ;
#8734 = VERTEX_POINT ( 'NONE', #59435 ) ;
#8735 = CARTESIAN_POINT ( 'NONE',  ( 10.06481084123000080, 5.336630274082000192, -7.092011739486999922 ) ) ;
#8736 = CARTESIAN_POINT ( 'NONE',  ( 7.326821631775000121, 1.159189395797000088, 0.9313610730889000378 ) ) ;
#8737 = CARTESIAN_POINT ( 'NONE',  ( 10.92125287134683909, -2.370162430443217616, 8.128085326470900540 ) ) ;
#8739 = CARTESIAN_POINT ( 'NONE',  ( 24.72252720687009386, 11.76897357382126685, 3.190821958176780715 ) ) ;
#8738 = CARTESIAN_POINT ( 'NONE',  ( 9.566483607044000692, -4.108965473266000146, 8.851626696081998702 ) ) ;
#8740 = CARTESIAN_POINT ( 'NONE',  ( 12.09999999999999787, -4.254640155007241908, 8.477868186285952845 ) ) ;
#8741 = CARTESIAN_POINT ( 'NONE',  ( 11.60948876160955479, -4.695527826393099957, -8.223320049540498999 ) ) ;
#8742 = ORIENTED_EDGE ( 'NONE', *, *, #35614, .T. ) ;
#8743 = CARTESIAN_POINT ( 'NONE',  ( 1.586792155651000291, -1.239015738333000050, 3.371748634333000094 ) ) ;
#8744 = CARTESIAN_POINT ( 'NONE',  ( 17.77478288653529503, -0.5854877331960374187, -12.68183053514018077 ) ) ;
#8746 = CARTESIAN_POINT ( 'NONE',  ( 11.09999999999999964, -0.5000000000000000000, -5.124965750789000296 ) ) ;
#8745 = CARTESIAN_POINT ( 'NONE',  ( 8.374639158773000247, 2.721111233225000259, -6.936528696292000085 ) ) ;
#8747 = CARTESIAN_POINT ( 'NONE',  ( 17.63932472559630327, -3.120604413325592130, 13.52206336586401569 ) ) ;
#8748 = EDGE_CURVE ( 'NONE', #18146, #42619, #3237, .T. ) ;
#8749 = ADVANCED_FACE ( 'NONE', ( #24109 ), #47873, .T. ) ;
#8750 = CARTESIAN_POINT ( 'NONE',  ( 16.10004050617000004, 3.886235259787000018, 11.90683839252000098 ) ) ;
#8752 = CARTESIAN_POINT ( 'NONE',  ( 16.10006098462790902, 8.380959734829373176, 8.092216891312055793 ) ) ;
#8751 = AXIS2_PLACEMENT_3D ( 'NONE', #35731, #56022, #9149 ) ;
#8753 = DIRECTION ( 'NONE',  ( -1.000000000000000000, 0.000000000000000000, 0.000000000000000000 ) ) ;
#8754 = CARTESIAN_POINT ( 'NONE',  ( 11.09999999999999964, 0.000000000000000000, 0.000000000000000000 ) ) ;
#8755 = CARTESIAN_POINT ( 'NONE',  ( 8.566230646795000681, -5.212258818969000451, 6.157189191035000064 ) ) ;
#8756 = ORIENTED_EDGE ( 'NONE', *, *, #11001, .F. ) ;
#8757 = ADVANCED_FACE ( 'NONE', ( #49642 ), #20673, .F. ) ;
#8758 = CARTESIAN_POINT ( 'NONE',  ( 8.881823341230997926, 4.977909614887999545, 6.416776202806000029 ) ) ;
#8759 = CARTESIAN_POINT ( 'NONE',  ( 24.72252701717521006, -8.647819769236338772, 8.596819301983423145 ) ) ;
#8760 = CARTESIAN_POINT ( 'NONE',  ( 7.451068553725185062, -2.261323975060523850, 7.457013478475167823 ) ) ;
#8761 = AXIS2_PLACEMENT_3D ( 'NONE', #13693, #54954, #45842 ) ;
#8762 = CARTESIAN_POINT ( 'NONE',  ( 11.48513281071060277, 2.915426916004881353, -7.824999134348144203 ) ) ;
#8763 = CARTESIAN_POINT ( 'NONE',  ( 1.271201594832999993, -1.239015738333000050, 3.371748634333000094 ) ) ;
#8764 = ORIENTED_EDGE ( 'NONE', *, *, #42389, .F. ) ;
#8765 = DIRECTION ( 'NONE',  ( 1.000000000000000000, 0.000000000000000000, 0.000000000000000000 ) ) ;
#8766 = CARTESIAN_POINT ( 'NONE',  ( 11.78949010443639978, -2.999324937259999935, 7.425165037173959703 ) ) ;
#8767 = CARTESIAN_POINT ( 'NONE',  ( 10.84530628050273293, -5.097570467516499448, 5.114908450777414295 ) ) ;
#8768 = CARTESIAN_POINT ( 'NONE',  ( 11.20563302462000088, 3.509134285281999777, 6.118194788334999856 ) ) ;
#8769 = CARTESIAN_POINT ( 'NONE',  ( 10.72333863405319931, 4.619094858989799768, 6.710270673950399889 ) ) ;
#8770 = AXIS2_PLACEMENT_3D ( 'NONE', #47229, #30465, #13701 ) ;
#8771 = DIRECTION ( 'NONE',  ( 1.000000000000000000, 0.000000000000000000, 0.000000000000000000 ) ) ;
#8772 = CARTESIAN_POINT ( 'NONE',  ( 8.005415440112999548, 4.520303302631999642, -6.254081655062000422 ) ) ;
#8773 = DIRECTION ( 'NONE',  ( 1.000000000000000000, 0.000000000000000000, 0.000000000000000000 ) ) ;
#8774 = CARTESIAN_POINT ( 'NONE',  ( 11.03776785110999903, -5.237767851104999650, 6.571291218949999902 ) ) ;
#8775 = CARTESIAN_POINT ( 'NONE',  ( 8.114521557114207084, 4.828697020333564183, 5.952393600668290929 ) ) ;
#8776 = EDGE_LOOP ( 'NONE', ( #37083, #19165, #53632, #41820 ) ) ;
#8777 = CARTESIAN_POINT ( 'NONE',  ( 17.60330540716448411, -3.246896514464381767, 13.61828436941213205 ) ) ;
#8778 = ORIENTED_EDGE ( 'NONE', *, *, #43879, .T. ) ;
#8779 = ORIENTED_EDGE ( 'NONE', *, *, #44146, .F. ) ;
#8780 = CARTESIAN_POINT ( 'NONE',  ( 10.40480513895999870, 4.779740423663599636, 7.933462475324499330 ) ) ;
#8781 = CARTESIAN_POINT ( 'NONE',  ( 9.635596873516668381, 5.092232985442826099, -6.870476274536379435 ) ) ;
#8782 = CARTESIAN_POINT ( 'NONE',  ( 11.14595257254739913, 3.168263696564200149, 7.258104750172799768 ) ) ;
#8783 = CARTESIAN_POINT ( 'NONE',  ( 10.62197831623999988, 5.779783227492000464, 7.256572995198999898 ) ) ;
#8784 = CARTESIAN_POINT ( 'NONE',  ( 10.17309652395999997, 4.709165316578000748, -8.664874001714000684 ) ) ;
#8785 = CARTESIAN_POINT ( 'NONE',  ( 9.429533309317625012, -3.366787958683358006, -6.896199718737570095 ) ) ;
#8786 = CARTESIAN_POINT ( 'NONE',  ( 9.903944471677000649, -5.205019707614999547, 6.747219600580999455 ) ) ;
#8787 = CARTESIAN_POINT ( 'NONE',  ( 18.20001934199752824, 0.3287229608534117942, -12.59571550161850340 ) ) ;
#8788 = B_SPLINE_CURVE_WITH_KNOTS ( 'NONE', 3,
 ( #28790, #16890, #23523, #7099 ),
 .UNSPECIFIED., .F., .F.,
 ( 4, 4 ),
 ( 0.000000000000000000, 1.000000000000000000 ),
 .UNSPECIFIED. ) ;
#8789 = CARTESIAN_POINT ( 'NONE',  ( 10.79839246847000034, -5.269358106415999110, -6.148714306659999629 ) ) ;
#8790 = CARTESIAN_POINT ( 'NONE',  ( 11.70794988689359961, -3.544213289744700290, -8.393984925606600811 ) ) ;
#8791 = CARTESIAN_POINT ( 'NONE',  ( 7.790635841228000125, 3.416213390569000197, 6.162512717529000206 ) ) ;
#8792 = VERTEX_POINT ( 'NONE', #63564 ) ;
#8793 = APPLICATION_CONTEXT ( 'automotive_design' ) ;
#8794 = CARTESIAN_POINT ( 'NONE',  ( 11.07074860546000039, -6.638029483401999720, -5.577172573415000834 ) ) ;
#8795 = FILL_AREA_STYLE_COLOUR ( '', #29883 ) ;
#8796 = CARTESIAN_POINT ( 'NONE',  ( 5.500000000000000000, -12.43893545635000031, -2.828937028792000152 ) ) ;
#8797 = EDGE_CURVE ( 'NONE', #55894, #34904, #44111, .T. ) ;
#8798 = CARTESIAN_POINT ( 'NONE',  ( 10.71081754702595923, -3.646708176540920832, -8.814774986206142415 ) ) ;
#8799 = CARTESIAN_POINT ( 'NONE',  ( 9.608380199233998553, 5.269225938816000543, -7.340469740450900282 ) ) ;
#8800 = CARTESIAN_POINT ( 'NONE',  ( 12.15975302296892124, 2.850959433913112129, 13.70664605376239287 ) ) ;
#8801 = DIRECTION ( 'NONE',  ( 1.000000000000000000, 0.000000000000000000, 0.000000000000000000 ) ) ;
#8802 = VERTEX_POINT ( 'NONE', #5867 ) ;
#8803 = VECTOR ( 'NONE', #23969, 1000.000000000000000 ) ;
#8804 = CARTESIAN_POINT ( 'NONE',  ( 12.27274573043892580, 0.3283020094446014170, -12.69430739907382488 ) ) ;
#8805 = LINE ( 'NONE', #51111, #5767 ) ;
#8806 = ORIENTED_EDGE ( 'NONE', *, *, #13361, .F. ) ;
#8807 = CARTESIAN_POINT ( 'NONE',  ( 11.21022026213526601, -2.954246606487285209, -7.824998325091605977 ) ) ;
#8808 = CARTESIAN_POINT ( 'NONE',  ( 9.893930206848997599, 2.750000000000000000, -7.500000000000000000 ) ) ;
#8809 = LINE ( 'NONE', #4237, #40773 ) ;
#8810 = CARTESIAN_POINT ( 'NONE',  ( 4.475281403099000244, -0.02432966049531000083, 1.629565400900000016 ) ) ;
#8811 = CARTESIAN_POINT ( 'NONE',  ( 10.22514748322304534, -2.649941783575446408, 7.500008211948054004 ) ) ;
#8812 = CARTESIAN_POINT ( 'NONE',  ( 6.999999691988000095, -12.11716380430000051, 3.069905306952000146 ) ) ;
#8813 = CARTESIAN_POINT ( 'NONE',  ( 7.976886985233497818, 5.078974948772304820, 8.328785302375242949 ) ) ;
#8814 = CARTESIAN_POINT ( 'NONE',  ( 12.51412939328308305, 3.139365204187051006, 12.20263940233110489 ) ) ;
#8815 = CYLINDRICAL_SURFACE ( 'NONE', #46394, 1.099999999999999867 ) ;
#8816 = CARTESIAN_POINT ( 'NONE',  ( 11.46595122972049907, 4.343798595649099425, -6.704952129760900270 ) ) ;
#8817 = CYLINDRICAL_SURFACE ( 'NONE', #3447, 1.350000000000000533 ) ;
#8818 = B_SPLINE_CURVE_WITH_KNOTS ( 'NONE', 3,
 ( #27686, #49000, #10904, #33278, #32582, #59140, #59482, #58454, #28033, #42724 ),
 .UNSPECIFIED., .F., .F.,
 ( 4, 2, 2, 2, 4 ),
 ( 0.000000000000000000, 0.2500000000000000000, 0.5000000000000000000, 0.7500000000000000000, 1.000000000000000000 ),
 .UNSPECIFIED. ) ;
#8819 = CARTESIAN_POINT ( 'NONE',  ( 10.64556415877000006, 2.988929467935999895, -5.952329570726999641 ) ) ;
#8820 = CARTESIAN_POINT ( 'NONE',  ( 9.151392757686998891, 4.770706668257700400, -8.342464052342599246 ) ) ;
#8822 = DIRECTION ( 'NONE',  ( -1.000000000000000000, 0.000000000000000000, 0.000000000000000000 ) ) ;
#8821 = CARTESIAN_POINT ( 'NONE',  ( 11.59999999999999964, 5.207010770456999893, -7.825000000000000178 ) ) ;
#8823 = CARTESIAN_POINT ( 'NONE',  ( 23.60648250789430236, -13.39605720553294432, 3.969101063526361273 ) ) ;
#8824 = ORIENTED_EDGE ( 'NONE', *, *, #60613, .T. ) ;
#8825 = FACE_OUTER_BOUND ( 'NONE', #61080, .T. ) ;
#8826 = CARTESIAN_POINT ( 'NONE',  ( 10.53138988903999973, -5.607755226963999640, 7.280101849877000042 ) ) ;
#8827 = CARTESIAN_POINT ( 'NONE',  ( 10.03495058442699950, 4.398663815465100768, 8.421905343605699201 ) ) ;
#8828 = CARTESIAN_POINT ( 'NONE',  ( 8.922950365671626471, 4.680938325111460685, -6.950586433956124743 ) ) ;
#8829 = ADVANCED_FACE ( 'NONE', ( #64591 ), #16565, .T. ) ;
#8830 = EDGE_CURVE ( 'NONE', #46950, #25841, #48528, .T. ) ;
#8831 = CARTESIAN_POINT ( 'NONE',  ( 10.44080359545000114, -5.435731278187999393, 7.303630150377999009 ) ) ;
#8832 = CARTESIAN_POINT ( 'NONE',  ( 7.099999886593999499, 1.243449787579999883E-13, -1.714758320200999846E-13 ) ) ;
#8833 = CARTESIAN_POINT ( 'NONE',  ( 6.899999691988000450, -12.20988339176000004, 3.111064831549000154 ) ) ;
#8834 = ORIENTED_EDGE ( 'NONE', *, *, #32487, .F. ) ;
#8835 = EDGE_CURVE ( 'NONE', #12254, #47064, #47439, .T. ) ;
#8836 = ADVANCED_FACE ( 'NONE', ( #26173 ), #26266, .F. ) ;
#8837 = CARTESIAN_POINT ( 'NONE',  ( 9.911267173156000254, -4.869050473540199597, -6.759401780699699103 ) ) ;
#8838 = LINE ( 'NONE', #30510, #57789 ) ;
#8839 = CARTESIAN_POINT ( 'NONE',  ( 11.85545123989520100, -3.524778630617700248, 6.582230774881299595 ) ) ;
#8840 = CARTESIAN_POINT ( 'NONE',  ( 18.27533594408734530, 2.564445959844773526, -12.33627802783496286 ) ) ;
#8841 = CARTESIAN_POINT ( 'NONE',  ( 2.750973465876000557, -3.500000000000000000, 0.000000000000000000 ) ) ;
#8842 = FACE_OUTER_BOUND ( 'NONE', #25375, .T. ) ;
#8843 = CARTESIAN_POINT ( 'NONE',  ( 8.057199896074001444, 2.877672799700000450, 6.732802633655004421 ) ) ;
#8845 = CARTESIAN_POINT ( 'NONE',  ( 9.306727112333998519, -4.009302068291999532, -9.043024413115999138 ) ) ;
#8844 = VECTOR ( 'NONE', #45624, 1000.000000000000000 ) ;
#8846 = LINE ( 'NONE', #2905, #38248 ) ;
#8847 = ORIENTED_EDGE ( 'NONE', *, *, #25959, .F. ) ;
#8848 = CARTESIAN_POINT ( 'NONE',  ( -17.56123417799999942, -11.06886219213000011, -1.536526853569999851 ) ) ;
#8849 = CARTESIAN_POINT ( 'NONE',  ( 12.68688508614694044, 0.7208442004938129255, -13.98143072948223775 ) ) ;
#8850 = DIRECTION ( 'NONE',  ( 0.000000000000000000, 0.000000000000000000, -1.000000000000000000 ) ) ;
#8851 = DIRECTION ( 'NONE',  ( -1.000000000000000000, 0.000000000000000000, 0.000000000000000000 ) ) ;
#8852 = CARTESIAN_POINT ( 'NONE',  ( 18.17882542848376559, 2.459571230201114567, 12.46089164816697270 ) ) ;
#8853 = EDGE_CURVE ( 'NONE', #57495, #51180, #69074, .T. ) ;
#8854 = CARTESIAN_POINT ( 'NONE',  ( 8.275189158773001097, 3.061731693614000438, -8.535706278603999664 ) ) ;
#8855 = CARTESIAN_POINT ( 'NONE',  ( 12.11364291764652990, -4.859654669415900408, 7.606265891492399511 ) ) ;
#8856 = ORIENTED_EDGE ( 'NONE', *, *, #66872, .F. ) ;
#8857 = CARTESIAN_POINT ( 'NONE',  ( 8.539089945104535673, -4.176610156107928518, 8.851086029037793068 ) ) ;
#8858 = CARTESIAN_POINT ( 'NONE',  ( 18.25624423923968109, 2.332236704353569223, -13.80437652844153718 ) ) ;
#8859 = ORIENTED_EDGE ( 'NONE', *, *, #61977, .T. ) ;
#8860 = CARTESIAN_POINT ( 'NONE',  ( 10.51660887879199890, -4.196341783741199372, 8.344486736701099971 ) ) ;
#8861 = DIRECTION ( 'NONE',  ( -1.000000000000000000, 0.000000000000000000, -1.275169027325000072E-14 ) ) ;
#8862 = CARTESIAN_POINT ( 'NONE',  ( 9.848670280409999478, 5.002683760508999988, -8.912673867568997821 ) ) ;
#8863 = CARTESIAN_POINT ( 'NONE',  ( 11.06049777433069892, 3.148547701490199913, 7.825000000000000178 ) ) ;
#8864 = CARTESIAN_POINT ( 'NONE',  ( 11.05946005378019947, -2.963614890480000152, -6.946587256304699309 ) ) ;
#8865 = CARTESIAN_POINT ( 'NONE',  ( 8.940795537697701079, 5.100000000000000533, 6.662590550608718409 ) ) ;
#8866 = CARTESIAN_POINT ( 'NONE',  ( 5.000000000000000000, -1.199999999999999956, 9.776630298829998011 ) ) ;
#8867 = ORIENTED_EDGE ( 'NONE', *, *, #59175, .F. ) ;
#8868 = CARTESIAN_POINT ( 'NONE',  ( 10.16000000000000014, -4.496968146123999865, -8.755198255949000696 ) ) ;
#8869 =( BOUNDED_SURFACE ( )  B_SPLINE_SURFACE ( 3, 3, ( 
 ( #33592, #16803, #26968, #7012, #6311, #28003, #38130, #27309, #54211 ),
 ( #11908, #11220, #54566, #59115, #48633, #48283, #389, #32557, #21705 ),
 ( #17150, #22048, #53869, #38482, #735, #54909, #59457, #28346, #5970 ),
 ( #49663, #59805, #65387, #17508, #43394, #43737, #12263, #1772, #22398 ) ),
 .UNSPECIFIED., .F., .F., .F. ) 
 B_SPLINE_SURFACE_WITH_KNOTS ( ( 4, 4 ),
 ( 4, 1, 1, 1, 1, 1, 4 ),
 ( 0.000000000000000000, 1.000000000000000000 ),
 ( -0.004644144098274999473, 0.000000000000000000, 0.03269534097185999855, 0.06255479614191999937, 0.08986301827557000022, 0.1148786485006000058, 0.1342276000085000087 ),
 .UNSPECIFIED. ) 
 GEOMETRIC_REPRESENTATION_ITEM ( )  RATIONAL_B_SPLINE_SURFACE ( (
 ( 1.157365337832999996, 1.157365337832999996, 1.157365337832999996, 1.157365337832999996, 1.157365337832999996, 1.157365337832999996, 1.157365337832999996, 1.157365337832999996, 1.157365337832999996),
 ( 0.9475448873890999213, 0.9475448873890999213, 0.9475448873890999213, 0.9475448873890999213, 0.9475448873890999213, 0.9475448873890999213, 0.9475448873890999213, 0.9475448873890999213, 0.9475448873890999213),
 ( 0.9475448873890999213, 0.9475448873890999213, 0.9475448873890999213, 0.9475448873890999213, 0.9475448873890999213, 0.9475448873890999213, 0.9475448873890999213, 0.9475448873890999213, 0.9475448873890999213),
 ( 1.157365337832999996, 1.157365337832999996, 1.157365337832999996, 1.157365337832999996, 1.157365337832999996, 1.157365337832999996, 1.157365337832999996, 1.157365337832999996, 1.157365337832999996) ) ) 
 REPRESENTATION_ITEM ( '' )  SURFACE ( )  );
#8870 = DIRECTION ( 'NONE',  ( 0.000000000000000000, 1.000000000000000000, 0.000000000000000000 ) ) ;
#8871 = CARTESIAN_POINT ( 'NONE',  ( 9.436104719595000745, 5.619431609641999614, -8.115423117607999615 ) ) ;
#8872 = EDGE_LOOP ( 'NONE', ( #52442, #32116, #26317, #65496, #53602 ) ) ;
#8873 = AXIS2_PLACEMENT_3D ( 'NONE', #50208, #13502, #56134 ) ;
#8874 = CARTESIAN_POINT ( 'NONE',  ( 10.27571527605999968, 5.689443924112000062, -7.562019866568999049 ) ) ;
#8875 =( NAMED_UNIT ( * ) PLANE_ANGLE_UNIT ( ) SI_UNIT ( $, .RADIAN. ) );
#8876 = B_SPLINE_CURVE_WITH_KNOTS ( 'NONE', 3,
 ( #57492, #41085, #56477, #30261 ),
 .UNSPECIFIED., .F., .F.,
 ( 4, 4 ),
 ( 0.000000000000000000, 1.000000000000000000 ),
 .UNSPECIFIED. ) ;
#8877 = EDGE_LOOP ( 'NONE', ( #53539, #16072, #61479, #31907 ) ) ;
#8878 = CARTESIAN_POINT ( 'NONE',  ( 9.430013376692999216, 2.982096917914000223, 8.017308190024898806 ) ) ;
#8879 = CARTESIAN_POINT ( 'NONE',  ( 17.81550493765278986, -1.931762299006051897, -12.56594712229140143 ) ) ;
#8880 = EDGE_CURVE ( 'NONE', #63766, #67307, #55150, .T. ) ;
#8881 = CARTESIAN_POINT ( 'NONE',  ( 9.356851002546999752, 2.832432432432000269, -6.822293592207000934 ) ) ;
#8882 = ADVANCED_FACE ( 'NONE', ( #2356 ), #43635, .F. ) ;
#8883 = CARTESIAN_POINT ( 'NONE',  ( 4.400037259600882322, -0.9678509383598562499, 0.9369558473984443969 ) ) ;
#8884 = CARTESIAN_POINT ( 'NONE',  ( 9.049519800792998225, -8.676607829236999692, -6.163757080959000767 ) ) ;
#8885 = ORIENTED_EDGE ( 'NONE', *, *, #46673, .F. ) ;
#8886 = CARTESIAN_POINT ( 'NONE',  ( 4.600000207916445483, 2.033928581112999763E-13, -2.806643806251999915E-13 ) ) ;
#8887 = DIRECTION ( 'NONE',  ( 1.000000000000000000, 0.000000000000000000, 0.000000000000000000 ) ) ;
#8888 = CARTESIAN_POINT ( 'NONE',  ( 11.04678944127999962, -5.235596213805000509, -5.039805523473999571 ) ) ;
#8889 = CARTESIAN_POINT ( 'NONE',  ( 12.10494519979306460, 2.707806787687952799, -13.73564420130114172 ) ) ;
#8890 = CARTESIAN_POINT ( 'NONE',  ( 18.27044831935228686, 0.1190513140356058014, 13.99949878896183719 ) ) ;
#8891 = CARTESIAN_POINT ( 'NONE',  ( 10.12947109217999930, 5.100000000000000533, 6.152188490330000370 ) ) ;
#8892 = CARTESIAN_POINT ( 'NONE',  ( 10.72303951155000057, -3.890113427500999421, -8.859339185702999941 ) ) ;
#8893 = VERTEX_POINT ( 'NONE', #6903 ) ;
#8894 = ORIENTED_EDGE ( 'NONE', *, *, #25790, .T. ) ;
#8895 = CARTESIAN_POINT ( 'NONE',  ( 8.929995280412999392, 5.030502105212999453, -6.322203460290999999 ) ) ;
#8896 = DIRECTION ( 'NONE',  ( -1.000000000000000000, 0.000000000000000000, 0.000000000000000000 ) ) ;
#8897 = CARTESIAN_POINT ( 'NONE',  ( 12.22548351784305432, -2.734003476492731899, 13.62103941681218267 ) ) ;
#8898 = CARTESIAN_POINT ( 'NONE',  ( 25.40238653257500090, 8.312591668607000273, -8.374698588276999089 ) ) ;
#8899 = FACE_OUTER_BOUND ( 'NONE', #44955, .T. ) ;
#8900 = CARTESIAN_POINT ( 'NONE',  ( 18.23887202961200060, -3.252214874110999965, -11.14733497513999971 ) ) ;
#8902 = CARTESIAN_POINT ( 'NONE',  ( 21.35000154058000277, 0.000000000000000000, 0.000000000000000000 ) ) ;
#8901 = CARTESIAN_POINT ( 'NONE',  ( 10.28367167105700020, -5.126041103316000047, 7.310881302803900361 ) ) ;
#8903 = CARTESIAN_POINT ( 'NONE',  ( 10.31746213571000048, 5.100000000000000533, 6.571291218949999902 ) ) ;
#8904 = ORIENTED_EDGE ( 'NONE', *, *, #4679, .T. ) ;
#8905 = CARTESIAN_POINT ( 'NONE',  ( 7.387904567572019410, 3.170618095687768090, -6.421005598970153549 ) ) ;
#8906 = CARTESIAN_POINT ( 'NONE',  ( 10.75775061949999944, -2.788892539766000045, -4.903545070807000528 ) ) ;
#8907 = CARTESIAN_POINT ( 'NONE',  ( 9.441140818749000019, -4.011292643094999555, -9.373220388412001114 ) ) ;
#8908 = CARTESIAN_POINT ( 'NONE',  ( 9.099999886593998610, 3.268496584495999908E-13, 3.613587358477999789E-14 ) ) ;
#8909 = B_SPLINE_CURVE_WITH_KNOTS ( 'NONE', 3,
 ( #61767, #34866, #56183, #45700, #13885, #67009, #9652, #68721, #20495, #202, #21521, #52651, #5783, #27126, #42854, #63476, #64165, #4746, #36231, #9999, #62788, #37265, #16279, #63127, #48443, #53003 ),
 .UNSPECIFIED., .F., .F.,
 ( 4, 2, 2, 2, 2, 2, 2, 2, 2, 2, 2, 2, 4 ),
 ( 0.000000000000000000, 0.06249999999999986122, 0.1249999999999997224, 0.2499999999999992506, 0.3749999999999987788, 0.4999999999999983347, 0.6249999999999978906, 0.6874999999999977796, 0.7499999999999977796, 0.8124999999999983347, 0.8749999999999987788, 0.9374999999999993339, 1.000000000000000000 ),
 .UNSPECIFIED. ) ;
#8910 = CARTESIAN_POINT ( 'NONE',  ( 11.79999998400527517, 11.58088844914904314, 1.772255231651886254 ) ) ;
#8911 = DIRECTION ( 'NONE',  ( 1.000000000000000000, 0.000000000000000000, 1.094362695702000107E-14 ) ) ;
#8912 = CARTESIAN_POINT ( 'NONE',  ( 8.497235841230001085, 3.789127741898000057, -9.388182174781999123 ) ) ;
#8913 = ADVANCED_FACE ( 'NONE', ( #18100 ), #7254, .T. ) ;
#8914 = EDGE_CURVE ( 'NONE', #32326, #11941, #19076, .T. ) ;
#8915 = AXIS2_PLACEMENT_3D ( 'NONE', #52599, #20443, #48048 ) ;
#8916 = CARTESIAN_POINT ( 'NONE',  ( 16.09999335515346885, -3.810015139062473466, -11.93171563566676419 ) ) ;
#8917 = CARTESIAN_POINT ( 'NONE',  ( 11.06059687351646481, -3.370476274536376771, 6.407767014557177454 ) ) ;
#8918 = B_SPLINE_SURFACE_WITH_KNOTS ( 'NONE', 3, 3, ( 
 ( #3829, #31119, #52422, #4518, #25855, #68489, #20613, #63245, #34988, #56303, #24488, #45811, #19232, #40559, #61886, #14002, #35330, #56645, #43664, #6238, #15370, #27579, #58019, #26207, #36698, #37040, #11150, #58355, #10121, #69184, #64275, #26553, #47879, #21296, #10457 ),
 ( #53462, #68840, #42626, #32484, #42295, #31452, #31799, #32824, #59383, #10803, #54140, #48905, #27236, #26898, #5556, #53798, #52771, #53115, #38059, #20958, #48561, #4866, #16047, #5217, #63936, #47535, #48210, #63594, #21633, #37719, #11484, #37378, #15712, #58700, #32147 ),
 ( #1013, #16392, #42968, #317, #59047, #5895, #665, #21976, #43318, #64621, #16730, #22322, #55531, #34213, #28624, #38407, #38759, #7630, #7982, #39104, #54489, #28977, #12536, #60769, #23709, #17431, #29315, #50284, #59731, #2385, #12190, #66005, #6589, #2049, #66351 ),
 ( #49937, #64961, #45044, #18471, #39797, #60085, #11832, #61120, #33865, #55180, #33519, #13237, #33172, #60428, #17074, #27931, #17785, #7285, #23368, #34563, #55876, #44708, #18128, #44363, #39450, #49240, #28269, #22667, #12884, #65663, #50628, #1349, #44010, #65315, #2729 ) ),
 .UNSPECIFIED., .F., .F., .F.,
 ( 4, 4 ),
 ( 4, 1, 1, 1, 1, 1, 1, 1, 1, 1, 1, 1, 1, 1, 1, 1, 1, 1, 1, 1, 1, 1, 1, 1, 1, 1, 1, 1, 1, 1, 1, 1, 4 ),
 ( -0.1039370721279000015, 1.103937072127999963 ),
 ( -0.01735257130020999988, 0.01084535706264999969, 0.03904328542550000031, 0.06724121378835999641, 0.09543914215121999944, 0.1236370705141000004, 0.1518349988768999959, 0.1800329272397999947, 0.2082308556026999935, 0.2364287839655000167, 0.2646267123283999601, 0.2928246406912000110, 0.3210225690540999821, 0.3492204974169000331, 0.3774184257798000042, 0.4056163541427000307, 0.4338142825054999707, 0.4620122108683999973, 0.4902101392311999928, 0.5184080675940999638, 0.5466059959569999904, 0.5748039243197999859, 0.6030018526827000125, 0.6311997810455000080, 0.6593977094084000345, 0.6875956377712000300, 0.7157935661340999456, 0.7439914944969999722, 0.7721894228597999676, 0.8003873512226999942, 0.8285852795854999897, 0.8567832079484000163, 0.8849811363112999318 ),
 .UNSPECIFIED. ) ;
#8919 = DIRECTION ( 'NONE',  ( 1.000000000000000000, 0.000000000000000000, 0.000000000000000000 ) ) ;
#8920 = CARTESIAN_POINT ( 'NONE',  ( 3.401112454814999797, -2.565134483810000088, 2.270441050239000003 ) ) ;
#8921 = EDGE_LOOP ( 'NONE', ( #34562, #9256, #12423, #4733, #23007 ) ) ;
#8922 = CARTESIAN_POINT ( 'NONE',  ( 12.58275800453940185, 0.6847469513499626625, -12.58138041838080490 ) ) ;
#8923 = CARTESIAN_POINT ( 'NONE',  ( 12.30934879319026720, -2.881204795959748211, -12.35454860660538579 ) ) ;
#8924 = CYLINDRICAL_SURFACE ( 'NONE', #8602, 0.4999999999999998335 ) ;
#8925 = CARTESIAN_POINT ( 'NONE',  ( 24.44916829770000177, 3.519946668155999880, -12.30317708153000034 ) ) ;
#8926 = DIRECTION ( 'NONE',  ( 0.9999999999999998890, -1.106867307615999853E-09, -9.864841365411998611E-09 ) ) ;
#8927 = ORIENTED_EDGE ( 'NONE', *, *, #19754, .T. ) ;
#8928 = PLANE ( 'NONE',  #67887 ) ;
#8929 =( NAMED_UNIT ( * ) PLANE_ANGLE_UNIT ( ) SI_UNIT ( $, .RADIAN. ) );
#8930 = CARTESIAN_POINT ( 'NONE',  ( 10.96729999554885282, 8.729492799572236450, 6.507753220594684862 ) ) ;
#8931 = EDGE_CURVE ( 'NONE', #63126, #1201, #64571, .T. ) ;
#8932 = CARTESIAN_POINT ( 'NONE',  ( 13.38404792230800133, -11.55332361678999931, -1.871151989399000071 ) ) ;
#8933 = CARTESIAN_POINT ( 'NONE',  ( 7.808141753486895986, 2.638822403986486265, -7.614799956045625429 ) ) ;
#8934 = CARTESIAN_POINT ( 'NONE',  ( 10.52799293566599914, 4.806678152079100208, -8.489570425681801424 ) ) ;
#8935 = ORIENTED_EDGE ( 'NONE', *, *, #24998, .T. ) ;
#8936 = CARTESIAN_POINT ( 'NONE',  ( 11.29621718459000057, -3.561654022787999807, 6.266039799355000106 ) ) ;
#8937 = ORIENTED_EDGE ( 'NONE', *, *, #3851, .F. ) ;
#8938 = DIRECTION ( 'NONE',  ( 1.000000000000000000, 0.000000000000000000, 0.000000000000000000 ) ) ;
#8939 = CARTESIAN_POINT ( 'NONE',  ( 7.507480646791999668, -3.501517589953999643, 9.055975309745999624 ) ) ;
#8940 = CARTESIAN_POINT ( 'NONE',  ( 18.26845486291482601, 0.1306247939804529856, -13.99939550958098344 ) ) ;
#8941 = EDGE_LOOP ( 'NONE', ( #23986, #46338, #7580, #60553, #59756, #14186 ) ) ;
#8942 = CARTESIAN_POINT ( 'NONE',  ( 8.404999999999999361, 5.190914425723000214, -8.768195054477999406 ) ) ;
#8943 = CARTESIAN_POINT ( 'NONE',  ( 10.97807333593999957, -5.235090452703000885, -6.783100406990000053 ) ) ;
#8944 = CARTESIAN_POINT ( 'NONE',  ( 7.631379719587999766, 5.256485075641999849, -6.567055966373000153 ) ) ;
#8945 = DIRECTION ( 'NONE',  ( 0.8660254037844289376, 0.000000000000000000, -0.5000000000000169864 ) ) ;
#8946 = CARTESIAN_POINT ( 'NONE',  ( 17.59622528268192099, -3.125000000000000444, 12.28374666422326378 ) ) ;
#8947 = ORIENTED_EDGE ( 'NONE', *, *, #16170, .T. ) ;
#8948 = CARTESIAN_POINT ( 'NONE',  ( 9.533427734455999669, -2.564762519363000148, 6.150594768287000136 ) ) ;
#8949 = CARTESIAN_POINT ( 'NONE',  ( 11.59999999999999609, 5.139199170149530538, 7.925587283338801470 ) ) ;
#8950 = CARTESIAN_POINT ( 'NONE',  ( 11.39975833414730033, 4.796537143354000499, -7.174999999999999822 ) ) ;
#8951 = CARTESIAN_POINT ( 'NONE',  ( 10.88016425062000003, -2.793121555136000023, -6.864957546339999439 ) ) ;
#8952 = LINE ( 'NONE', #30293, #24740 ) ;
#8953 = VERTEX_POINT ( 'NONE', #44679 ) ;
#8954 = CARTESIAN_POINT ( 'NONE',  ( 23.80818184942661730, 13.01048713944770441, -3.693375169791979662 ) ) ;
#8955 = FACE_OUTER_BOUND ( 'NONE', #55282, .T. ) ;
#8956 = CARTESIAN_POINT ( 'NONE',  ( 7.100000000000000533, 5.350000000000000533, -7.500000000000000000 ) ) ;
#8957 = DIRECTION ( 'NONE',  ( 0.000000000000000000, -1.000000000000000000, 0.000000000000000000 ) ) ;
#8958 = EDGE_CURVE ( 'NONE', #26424, #55718, #60821, .T. ) ;
#8959 = CARTESIAN_POINT ( 'NONE',  ( 12.21991984215965310, 0.2205930660282648670, -13.89766156610767034 ) ) ;
#8960 = CARTESIAN_POINT ( 'NONE',  ( 18.17829451895835291, -2.452078260301032930, 12.46263202712693996 ) ) ;
#8961 = ORIENTED_EDGE ( 'NONE', *, *, #7655, .T. ) ;
#8962 = CARTESIAN_POINT ( 'NONE',  ( 10.47769598648999967, -2.990523684589000197, -8.101059042556599366 ) ) ;
#8963 = ORIENTED_EDGE ( 'NONE', *, *, #17925, .T. ) ;
#8964 = CARTESIAN_POINT ( 'NONE',  ( 9.869051220224999810, 5.575171928796999410, 7.724300137354000562 ) ) ;
#8965 = AXIS2_PLACEMENT_3D ( 'NONE', #32511, #11862, #53827 ) ;
#8966 = FACE_OUTER_BOUND ( 'NONE', #23300, .T. ) ;
#8967 = CARTESIAN_POINT ( 'NONE',  ( 9.327795280414001411, 3.161445734422999809, -6.178649910536000434 ) ) ;
#8968 = CARTESIAN_POINT ( 'NONE',  ( 3.348254627038999676, 1.687100406436000011, -3.116347325074999564 ) ) ;
#8969 = DIRECTION ( 'NONE',  ( 2.887772199312943602E-10, -0.4812251768484908099, -0.8765970164032835799 ) ) ;
#8970 = CARTESIAN_POINT ( 'NONE',  ( 10.38528584683667688, 4.732620749361600154, -8.166081851074052267 ) ) ;
#8971 = CARTESIAN_POINT ( 'NONE',  ( 23.62925782967800004, 13.46920268230999973, 3.826620036219000376 ) ) ;
#8972 = B_SPLINE_CURVE_WITH_KNOTS ( 'NONE', 3,
 ( #41048, #10947, #805, #53936 ),
 .UNSPECIFIED., .F., .F.,
 ( 4, 4 ),
 ( 0.000000000000000000, 1.000000000000000000 ),
 .UNSPECIFIED. ) ;
#8973 = VERTEX_POINT ( 'NONE', #11804 ) ;
#8974 = CARTESIAN_POINT ( 'NONE',  ( 11.66225954179439839, -3.122605388210700106, 6.770980925167799036 ) ) ;
#8975 = CARTESIAN_POINT ( 'NONE',  ( 10.35911162173837319, 5.698273092209690915, -7.916014385706306555 ) ) ;
#8976 = CARTESIAN_POINT ( 'NONE',  ( 11.09999999999999964, -2.488501404117073434, -6.685067957705506991 ) ) ;
#8977 = PLANE ( 'NONE',  #48824 ) ;
#8979 = CARTESIAN_POINT ( 'NONE',  ( 24.35365242081699932, -1.906711579079999552, -11.36048031428999572 ) ) ;
#8978 = CARTESIAN_POINT ( 'NONE',  ( 10.93227693248999977, 2.539877577705000000, 6.453611809651000009 ) ) ;
#8980 = CARTESIAN_POINT ( 'NONE',  ( 10.92026088462129962, 4.002135146349410810, -6.496532863517000322 ) ) ;
#8981 = CARTESIAN_POINT ( 'NONE',  ( 24.78226685285000386, -12.26744358842999993, 2.911641580551999731 ) ) ;
#8982 = CARTESIAN_POINT ( 'NONE',  ( 9.072442991499999110, 3.936771438983030169, -6.497580701799000380 ) ) ;
#8983 = CARTESIAN_POINT ( 'NONE',  ( 17.57898592363197210, 0.7189971323193946606, 12.57946912511938109 ) ) ;
#8984 = CARTESIAN_POINT ( 'NONE',  ( 24.31006797060300073, 3.215953369236999926, 12.14991815011999954 ) ) ;
#8985 = CARTESIAN_POINT ( 'NONE',  ( 10.51414141025500015, 4.615773412711500434, 6.403245959303999868 ) ) ;
#8986 = CARTESIAN_POINT ( 'NONE',  ( 23.58473471199800287, 10.19686565968999936, 9.579920953980000320 ) ) ;
#8987 = EDGE_LOOP ( 'NONE', ( #55378, #31073, #13094 ) ) ;
#8988 = CARTESIAN_POINT ( 'NONE',  ( 7.256081853207000165, -2.531197775378000170, 8.216705951490000714 ) ) ;
#8989 = EDGE_CURVE ( 'NONE', #15838, #35693, #44333, .T. ) ;
#8990 = EDGE_CURVE ( 'NONE', #45676, #1231, #22414, .T. ) ;
#8991 = LINE ( 'NONE', #35910, #52817 ) ;
#8992 = PLANE ( 'NONE',  #42346 ) ;
#8993 = CARTESIAN_POINT ( 'NONE',  ( 11.09999999999999964, -7.940796613052000019, -6.945951997396999644 ) ) ;
#8994 = VERTEX_POINT ( 'NONE', #17756 ) ;
#8995 = CARTESIAN_POINT ( 'NONE',  ( 0.2387948408026999980, 3.161455490150999914, -0.5535149012972000460 ) ) ;
#8996 = CARTESIAN_POINT ( 'NONE',  ( 11.22567835872029995, 3.006051690924700370, 8.126439557340900066 ) ) ;
#8997 = CARTESIAN_POINT ( 'NONE',  ( 11.03905471959000018, 3.855072614532999875, -9.179480010827999692 ) ) ;
#8998 = VERTEX_POINT ( 'NONE', #39075 ) ;
#8999 = CARTESIAN_POINT ( 'NONE',  ( 10.76685100253999927, -2.832432432432000269, 6.822293592207000934 ) ) ;
#9000 = FACE_OUTER_BOUND ( 'NONE', #23145, .T. ) ;
#9001 = CARTESIAN_POINT ( 'NONE',  ( 11.55194988689359903, 4.580487242693600081, 6.361426117087999543 ) ) ;
#9002 = CARTESIAN_POINT ( 'NONE',  ( 17.60000000000000142, -10.78295181803999903, 4.410266442048000002 ) ) ;
#9003 = CARTESIAN_POINT ( 'NONE',  ( 9.766851002543001314, 2.832432432432000269, 6.822293592207000934 ) ) ;
#9004 = ORIENTED_EDGE ( 'NONE', *, *, #26760, .F. ) ;
#9005 = CARTESIAN_POINT ( 'NONE',  ( 11.56599877858000092, -3.774257655232999831, 11.98333518513999962 ) ) ;
#9006 = CARTESIAN_POINT ( 'NONE',  ( 6.970189158770000226, 3.332350081667999842, -9.278694849147001378 ) ) ;
#9007 = EDGE_CURVE ( 'NONE', #39123, #44844, #60398, .T. ) ;
#9008 = CIRCLE ( 'NONE', #48094, 12.35000000006999876 ) ;
#9009 = CARTESIAN_POINT ( 'NONE',  ( 8.210268599937796452, -5.723642697224037512, 7.747033231994619129 ) ) ;
#9010 = CARTESIAN_POINT ( 'NONE',  ( 10.92968717260509948, -4.687649763627899979, -8.622362941748999532 ) ) ;
#9011 = CARTESIAN_POINT ( 'NONE',  ( 10.07997570133299980, -3.061513547538400104, 6.630731591496600075 ) ) ;
#9012 = EDGE_LOOP ( 'NONE', ( #60936, #37395, #23838, #20036 ) ) ;
#9013 = CARTESIAN_POINT ( 'NONE',  ( 11.08464238854999984, -5.237407606198999588, -5.050454952618999904 ) ) ;
#9014 = CARTESIAN_POINT ( 'NONE',  ( 10.59964828895399869, -2.878385131502000149, 6.887384543790600056 ) ) ;
#9015 = ORIENTED_EDGE ( 'NONE', *, *, #68558, .F. ) ;
#9016 = EDGE_CURVE ( 'NONE', #8185, #8090, #33836, .T. ) ;
#9017 = CARTESIAN_POINT ( 'NONE',  ( 8.748821772879614045, 4.302364887094737966, 6.625936606111492821 ) ) ;
#9018 = ORIENTED_EDGE ( 'NONE', *, *, #60871, .F. ) ;
#9019 = CARTESIAN_POINT ( 'NONE',  ( 10.15291672334000062, -4.949038487346999915, -8.498994087616001281 ) ) ;
#9020 = CARTESIAN_POINT ( 'NONE',  ( 17.55505043854147118, -1.787816316115923954, 13.88537766212463254 ) ) ;
#9021 = CARTESIAN_POINT ( 'NONE',  ( 10.43614141025499897, 4.549633050978300730, -8.478951440767898973 ) ) ;
#9022 = FACE_OUTER_BOUND ( 'NONE', #69110, .T. ) ;
#9023 = CARTESIAN_POINT ( 'NONE',  ( 12.23541831425119675, 2.757387829712824701, -12.38789221355391312 ) ) ;
#9024 = CARTESIAN_POINT ( 'NONE',  ( 10.67764828895399987, -2.998858038575999974, 6.953185708700699408 ) ) ;
#9025 = CARTESIAN_POINT ( 'NONE',  ( 9.041948341230998665, 2.707986230053999854, 5.994446745591000436 ) ) ;
#9026 = ORIENTED_EDGE ( 'NONE', *, *, #63603, .T. ) ;
#9027 = DIRECTION ( 'NONE',  ( 2.888706471568024494E-10, -0.06432770287657048336, -0.9979288284455077873 ) ) ;
#9028 = CARTESIAN_POINT ( 'NONE',  ( 9.406706853206999952, -3.705847642455000202, 9.096432253453999195 ) ) ;
#9029 = CARTESIAN_POINT ( 'NONE',  ( 7.315000000000000391, 2.649999999999999911, -7.500000000000000000 ) ) ;
#9030 = ORIENTED_EDGE ( 'NONE', *, *, #46488, .F. ) ;
#9031 = CARTESIAN_POINT ( 'NONE',  ( 12.46441593768246570, -3.024116347931780524, -12.31386760464157781 ) ) ;
#9032 = CARTESIAN_POINT ( 'NONE',  ( 11.60118044953561878, 5.133201153721000054, 6.909094663619399945 ) ) ;
#9033 = CARTESIAN_POINT ( 'NONE',  ( 10.66043185321000131, -2.315667072036000196, -7.431702410656999547 ) ) ;
#9034 = CARTESIAN_POINT ( 'NONE',  ( 8.644512467439003700, 8.815297989570002102, -6.028160447578001957 ) ) ;
#9035 = CARTESIAN_POINT ( 'NONE',  ( 17.61265229197699966, -11.81477306456000065, 3.322807805102999890 ) ) ;
#9036 = CARTESIAN_POINT ( 'NONE',  ( 24.53002386606399909, -8.771528676250001766, 8.897041952682000598 ) ) ;
#9037 = CARTESIAN_POINT ( 'NONE',  ( 12.33410680267665960, -3.073228032305979962, -13.65852590327789962 ) ) ;
#9038 = CARTESIAN_POINT ( 'NONE',  ( 11.51518179236248862, -4.180996681294200101, -6.652923384986699773 ) ) ;
#9039 = CARTESIAN_POINT ( 'NONE',  ( 10.05041772631199848, -3.450375740502100275, -8.631352948887998977 ) ) ;
#9040 = VECTOR ( 'NONE', #14418, 1000.000000000000000 ) ;
#9041 = LINE ( 'NONE', #56602, #983 ) ;
#9042 = VERTEX_POINT ( 'NONE', #26397 ) ;
#9043 = ORIENTED_EDGE ( 'NONE', *, *, #48715, .T. ) ;
#9044 = CARTESIAN_POINT ( 'NONE',  ( 12.75652363867719252, 0.7301778992647915967, -13.98094561311457440 ) ) ;
#9045 =( LENGTH_UNIT ( ) NAMED_UNIT ( * ) SI_UNIT ( .MILLI., .METRE. ) );
#9046 = CARTESIAN_POINT ( 'NONE',  ( 8.999999001754000361, 0.000000000000000000, 0.000000000000000000 ) ) ;
#9047 = CARTESIAN_POINT ( 'NONE',  ( 18.16759718491386977, 2.624144391529842579, 13.64629239149777185 ) ) ;
#9048 = CARTESIAN_POINT ( 'NONE',  ( 9.870875237110999123, 2.904361819252000210, -8.563871667095998674 ) ) ;
#9049 = AXIS2_PLACEMENT_3D ( 'NONE', #9046, #51359, #2776 ) ;
#9050 = FACE_OUTER_BOUND ( 'NONE', #34352, .T. ) ;
#9051 = CARTESIAN_POINT ( 'NONE',  ( 18.13653212795700753, 2.729361600744797389, 12.39516738912175597 ) ) ;
#9052 = EDGE_CURVE ( 'NONE', #18020, #66620, #56809, .T. ) ;
#9053 = CARTESIAN_POINT ( 'NONE',  ( 11.09999999999999964, -4.000000000000000000, 7.500000000000000000 ) ) ;
#9054 = ADVANCED_FACE ( 'NONE', ( #22171 ), #10629, .F. ) ;
#9055 = CARTESIAN_POINT ( 'NONE',  ( 11.02786554143000153, 5.596226216413000110, 7.209502215883999199 ) ) ;
#9056 = AXIS2_PLACEMENT_3D ( 'NONE', #60748, #61440, #13560 ) ;
#9057 = CARTESIAN_POINT ( 'NONE',  ( 10.15670292967786104, -5.179682183662243311, -8.179940953559762917 ) ) ;
#9058 = ORIENTED_EDGE ( 'NONE', *, *, #37888, .F. ) ;
#9059 = CARTESIAN_POINT ( 'NONE',  ( 12.47244801656840174, -3.029249266520640305, 12.31238128988859515 ) ) ;
#9060 = CARTESIAN_POINT ( 'NONE',  ( 9.678329965421998082, -4.602191201513400109, -8.123757726465999696 ) ) ;
#9061 = CARTESIAN_POINT ( 'NONE',  ( 9.667078842372998082, 4.541623431405000133, 5.824038024834000460 ) ) ;
#9062 = CARTESIAN_POINT ( 'NONE',  ( 12.25203632436370071, -5.109717061557999429, 7.759151359668400083 ) ) ;
#9063 = CARTESIAN_POINT ( 'NONE',  ( 8.821685841230998193, 2.633142096252999664, -7.791134854666999843 ) ) ;
#9064 = DIRECTION ( 'NONE',  ( 0.000000000000000000, 1.000000000000000000, 0.000000000000000000 ) ) ;
#9065 = CARTESIAN_POINT ( 'NONE',  ( 12.24445512745668019, 0.2765170649790821833, 12.69595318831094133 ) ) ;
#9066 = CLOSED_SHELL ( 'NONE', ( #538, #16438, #8749, #22515, #69092, #43742, #37728, #33930, #8913, #5647, #67242, #29082, #27532, #40872, #58827, #47969, #11124, #50802, #4328, #54968, #31590, #64768, #59178, #59820, #56964, #50716, #14278, #12700, #21395, #67469, #37751 ) ) ;
#9067 = CARTESIAN_POINT ( 'NONE',  ( 7.647239158771000689, 5.850290547079999293, 6.784176679236000318 ) ) ;
#9068 = CARTESIAN_POINT ( 'NONE',  ( 9.104014120666999332, 5.045862207587999748, 8.527865280865999154 ) ) ;
#9069 = CARTESIAN_POINT ( 'NONE',  ( 9.220176149162259804, -2.652345172034098475, 7.581873905328563090 ) ) ;
#9070 = ORIENTED_EDGE ( 'NONE', *, *, #54469, .T. ) ;
#9071 = CARTESIAN_POINT ( 'NONE',  ( 9.974220280410998285, 5.496789211521000418, -7.043125396300999874 ) ) ;
#9072 = CARTESIAN_POINT ( 'NONE',  ( -0.000000000000000000, -2.899969545325999931, 0.3811992978302040092 ) ) ;
#9073 = EDGE_CURVE ( 'NONE', #16664, #4537, #11332, .T. ) ;
#9074 = ADVANCED_FACE ( 'NONE', ( #59230 ), #15085, .T. ) ;
#9075 = DIRECTION ( 'NONE',  ( -1.000000000000000000, 0.000000000000000000, 0.000000000000000000 ) ) ;
#9076 = CARTESIAN_POINT ( 'NONE',  ( 9.924988015501618577, 5.349815781279066762, 7.500001845592777272 ) ) ;
#9077 = CARTESIAN_POINT ( 'NONE',  ( 24.54174074856956267, 8.849271461504201852, 9.279828214275216425 ) ) ;
#9078 = CARTESIAN_POINT ( 'NONE',  ( 10.89564560330029863, -3.692495237344800341, -6.544808043482999160 ) ) ;
#9079 = ORIENTED_EDGE ( 'NONE', *, *, #7961, .T. ) ;
#9080 = EDGE_CURVE ( 'NONE', #51168, #9263, #34078, .T. ) ;
#9081 = CARTESIAN_POINT ( 'NONE',  ( 1.682156054532000011, -3.591455136169999562, 0.07279325410826999188 ) ) ;
#9082 = CARTESIAN_POINT ( 'NONE',  ( 12.37336427446297016, 11.82897199538926358, -3.432444870274659277 ) ) ;
#9084 = CARTESIAN_POINT ( 'NONE',  ( 13.99955778315600163, -9.394084143528001363, -8.201088258230999628 ) ) ;
#9083 = CARTESIAN_POINT ( 'NONE',  ( 9.319414158774000256, 2.656512020013999997, -7.884832994446999699 ) ) ;
#9085 = DIRECTION ( 'NONE',  ( 0.7071066261840305289, -0.7071069361890305327, 2.950983023348127876E-10 ) ) ;
#9086 = CARTESIAN_POINT ( 'NONE',  ( 15.89979320885400327, 3.824231472901999496, 11.71686814605000038 ) ) ;
#9087 = CARTESIAN_POINT ( 'NONE',  ( 12.30746066369764691, -3.049480053538148105, 13.66385627579028039 ) ) ;
#9088 = CARTESIAN_POINT ( 'NONE',  ( 11.61364291764652812, 3.140345330584100036, 7.606265891492399511 ) ) ;
#9089 = CARTESIAN_POINT ( 'NONE',  ( 24.95277496327178213, -11.53322809624908274, 3.220796833695926953 ) ) ;
#9090 = CARTESIAN_POINT ( 'NONE',  ( 7.475043146792000215, -3.276313010012999793, 5.841993238691999935 ) ) ;
#9091 = VERTEX_POINT ( 'NONE', #34068 ) ;
#9092 = CARTESIAN_POINT ( 'NONE',  ( 7.545267219589999463, 2.302289264429000504, 6.875166305059000393 ) ) ;
#9094 = FACE_OUTER_BOUND ( 'NONE', #31983, .T. ) ;
#9093 = CARTESIAN_POINT ( 'NONE',  ( 5.061409705193999464, -0.1429527940584000290, 1.396516134632999950 ) ) ;
#9095 = CARTESIAN_POINT ( 'NONE',  ( 7.555344015604732455, -3.596964894108017230, 5.798493967524453119 ) ) ;
#9096 = CARTESIAN_POINT ( 'NONE',  ( 5.699999545467999695, 0.000000000000000000, 0.000000000000000000 ) ) ;
#9097 = CARTESIAN_POINT ( 'NONE',  ( 1.409474105092999974, -2.789116823352000285, 1.988880583162999871 ) ) ;
#9098 = ORIENTED_EDGE ( 'NONE', *, *, #13106, .F. ) ;
#9099 = CARTESIAN_POINT ( 'NONE',  ( 0.9525933052797602718, -1.981538156914185667, 2.642344845388179486 ) ) ;
#9100 = CARTESIAN_POINT ( 'NONE',  ( 11.42441504065829960, -3.305585767322499979, 8.017771632862299214 ) ) ;
#9101 = EDGE_CURVE ( 'NONE', #50154, #62603, #12400, .T. ) ;
#9102 = CARTESIAN_POINT ( 'NONE',  ( 10.64116087492386420, -5.048254848383018079, 5.053851215417545006 ) ) ;
#9103 = CARTESIAN_POINT ( 'NONE',  ( 10.42596030538999941, 5.042177533603999784, 8.702224267793999601 ) ) ;
#9104 = CARTESIAN_POINT ( 'NONE',  ( 10.20641772631199906, 4.431553727090300043, 6.611684804099500212 ) ) ;
#9105 = CARTESIAN_POINT ( 'NONE',  ( 9.702711596877973577, 5.100000000000000533, 6.305985889537642386 ) ) ;
#9106 = CARTESIAN_POINT ( 'NONE',  ( 18.26079396959535828, 3.428468831596959365, -12.04667397462516298 ) ) ;
#9107 = CARTESIAN_POINT ( 'NONE',  ( 5.399999732039999500, 13.10000000000000142, 0.000000000000000000 ) ) ;
#9108 = CARTESIAN_POINT ( 'NONE',  ( 8.453783575583390331, 2.251044692578384687, 7.420277725347735220 ) ) ;
#9109 = VERTEX_POINT ( 'NONE', #34420 ) ;
#9110 = CARTESIAN_POINT ( 'NONE',  ( 18.21576355877877162, -2.818661318639680058, 13.71332454644887200 ) ) ;
#9111 = DIRECTION ( 'NONE',  ( 1.000000000000000000, 0.000000000000000000, 0.000000000000000000 ) ) ;
#9112 = ORIENTED_EDGE ( 'NONE', *, *, #19795, .T. ) ;
#9113 = EDGE_LOOP ( 'NONE', ( #10583, #7484, #36259, #68221, #52697, #44349, #5451, #442, #67044, #39540, #56298 ) ) ;
#9114 = CARTESIAN_POINT ( 'NONE',  ( 9.769471092180999960, -5.100000000000000533, -6.152188490330000370 ) ) ;
#9115 = ORIENTED_EDGE ( 'NONE', *, *, #4163, .F. ) ;
#9116 = CARTESIAN_POINT ( 'NONE',  ( 8.220491111160100672, 2.863432725431082737, 6.768885602738127893 ) ) ;
#9117 = CARTESIAN_POINT ( 'NONE',  ( 11.31825954179440075, 4.666231193203100425, 6.946434658287599540 ) ) ;
#9118 = VECTOR ( 'NONE', #37243, 1000.000000000000000 ) ;
#9119 = CARTESIAN_POINT ( 'NONE',  ( 10.37373942323999998, 2.215265813302000009, 7.703982730183001060 ) ) ;
#9120 = CARTESIAN_POINT ( 'NONE',  ( 10.33022126302999943, 2.650190549566000087, -7.694579890082000162 ) ) ;
#9121 = CARTESIAN_POINT ( 'NONE',  ( 9.860128811416625894, -3.130392736003965393, -7.596516710088708990 ) ) ;
#9122 = CARTESIAN_POINT ( 'NONE',  ( 10.09181272066999924, -2.440908155048000516, 7.817368209339999652 ) ) ;
#9123 = CARTESIAN_POINT ( 'NONE',  ( 18.20808481425077474, -0.3124912280145399346, -12.59612551846059780 ) ) ;
#9124 = CARTESIAN_POINT ( 'NONE',  ( 10.05204995789999955, -2.669899884077999719, -8.791535702747999892 ) ) ;
#9125 = CARTESIAN_POINT ( 'NONE',  ( 11.41672066707849886, -3.258843737379200078, -7.051685395375099752 ) ) ;
#9126 = CARTESIAN_POINT ( 'NONE',  ( 8.304135841228999837, 3.650414032626000171, 6.083147621602999600 ) ) ;
#9127 = ORIENTED_EDGE ( 'NONE', *, *, #29338, .T. ) ;
#9128 = CARTESIAN_POINT ( 'NONE',  ( 9.495772571291157149, -5.001491341851799888, 6.923765800360898837 ) ) ;
#9129 = CARTESIAN_POINT ( 'NONE',  ( 10.35646369189390192, -5.100000000000000533, 6.665341197326519307 ) ) ;
#9130 = DIRECTION ( 'NONE',  ( 1.000000000000000000, 0.000000000000000000, 0.000000000000000000 ) ) ;
#9131 = B_SPLINE_CURVE_WITH_KNOTS ( 'NONE', 3,
 ( #62558, #35998, #52417, #62897 ),
 .UNSPECIFIED., .F., .F.,
 ( 4, 4 ),
 ( 0.000000000000000000, 1.000000000000000000 ),
 .UNSPECIFIED. ) ;
#9132 = CARTESIAN_POINT ( 'NONE',  ( 8.374301491561006117, 10.15552111561999915, 5.491315164875996579 ) ) ;
#9133 = EDGE_CURVE ( 'NONE', #18819, #12380, #38609, .T. ) ;
#9134 = CARTESIAN_POINT ( 'NONE',  ( 12.20666462242724215, 2.105579624229084068, 13.84076000201157974 ) ) ;
#9135 = ADVANCED_FACE ( 'NONE', ( #49097 ), #1184, .F. ) ;
#9136 = CYLINDRICAL_SURFACE ( 'NONE', #24421, 1.350000000000000089 ) ;
#9137 = ORIENTED_EDGE ( 'NONE', *, *, #27535, .T. ) ;
#9138 = CARTESIAN_POINT ( 'NONE',  ( 12.29580549756552088, 0.3624889076790000497, -12.69304043452270214 ) ) ;
#9139 = CARTESIAN_POINT ( 'NONE',  ( 12.22983020848964486, -0.4451122480341178633, 13.99293440828418866 ) ) ;
#9140 = ORIENTED_EDGE ( 'NONE', *, *, #41706, .F. ) ;
#9141 = FACE_OUTER_BOUND ( 'NONE', #57242, .T. ) ;
#9142 = CARTESIAN_POINT ( 'NONE',  ( 10.89393020684999946, -5.250000000000000000, 7.500000000000000000 ) ) ;
#9143 = DIRECTION ( 'NONE',  ( 1.000000000000000000, 0.000000000000000000, 0.000000000000000000 ) ) ;
#9144 = CARTESIAN_POINT ( 'NONE',  ( 10.93210941423800087, -3.358814833524500276, 8.082391773166900606 ) ) ;
#9145 = VECTOR ( 'NONE', #45672, 1000.000000000000000 ) ;
#9146 = CARTESIAN_POINT ( 'NONE',  ( 10.09393020684899867, 5.250000000000000000, -7.500000000000000000 ) ) ;
#9147 = CARTESIAN_POINT ( 'NONE',  ( 0.3100461241979999838, -2.634961698279000064, 2.360490016663000290 ) ) ;
#9148 = CARTESIAN_POINT ( 'NONE',  ( 5.700000000000000178, -1.433333333332999837, -10.65401593558000037 ) ) ;
#9149 = DIRECTION ( 'NONE',  ( 0.000000000000000000, 1.000000000000000000, 0.000000000000000000 ) ) ;
#9150 = CARTESIAN_POINT ( 'NONE',  ( 9.663906509039998483, -2.491831134779999957, -6.388915175267000812 ) ) ;
#9151 = CARTESIAN_POINT ( 'NONE',  ( 11.58487348028854846, 3.117292544139400157, -7.977261354519500358 ) ) ;
#9152 = FACE_OUTER_BOUND ( 'NONE', #41111, .T. ) ;
#9153 = B_SPLINE_CURVE_WITH_KNOTS ( 'NONE', 3,
 ( #7423, #34358, #2190, #50422, #43804, #65100, #17223, #38548, #3890, #14060 ),
 .UNSPECIFIED., .F., .F.,
 ( 4, 2, 2, 2, 4 ),
 ( 0.000000000000000000, 0.2500000000000000000, 0.5000000000000000000, 0.7500000000000000000, 1.000000000000000000 ),
 .UNSPECIFIED. ) ;
#9154 = CARTESIAN_POINT ( 'NONE',  ( 10.94501463001509833, 4.472480213525599879, -6.743262887067199784 ) ) ;
#9155 = CARTESIAN_POINT ( 'NONE',  ( 8.872772138681998655, 3.575113238066399912, -6.440186012775000357 ) ) ;
#9157 = CARTESIAN_POINT ( 'NONE',  ( 12.48752230519103357, 1.955425561929305056, 12.56195022952150353 ) ) ;
#9156 = DIRECTION ( 'NONE',  ( 0.7071067486699967874, -0.7071068137030968037, 9.022793105466955192E-11 ) ) ;
#9158 = CARTESIAN_POINT ( 'NONE',  ( 10.96291115432987340, -5.162911154332890717, -6.648309209561353406 ) ) ;
#9159 = VERTEX_POINT ( 'NONE', #63361 ) ;
#9160 = EDGE_CURVE ( 'NONE', #20915, #63154, #43221, .T. ) ;
#9161 = CARTESIAN_POINT ( 'NONE',  ( 11.52677869730533011, 3.596497913043499750, 8.295667533166499297 ) ) ;
#9162 = FACE_OUTER_BOUND ( 'NONE', #49547, .T. ) ;
#9163 = CARTESIAN_POINT ( 'NONE',  ( 9.072442991499999110, 3.936771438983030169, 8.502419298200999620 ) ) ;
#9164 = DIRECTION ( 'NONE',  ( 0.000000000000000000, -0.4595937023756062056, -0.8881292860483110951 ) ) ;
#9165 = CARTESIAN_POINT ( 'NONE',  ( 23.60205915885299888, 11.53346724329999873, -4.150849519444998137 ) ) ;
#9166 = FACE_OUTER_BOUND ( 'NONE', #65473, .T. ) ;
#9167 = DIRECTION ( 'NONE',  ( -1.000000000000000000, 0.000000000000000000, 0.000000000000000000 ) ) ;
#9168 = FACE_OUTER_BOUND ( 'NONE', #33717, .T. ) ;
#9169 = ORIENTED_EDGE ( 'NONE', *, *, #16901, .T. ) ;
#9170 = CARTESIAN_POINT ( 'NONE',  ( 10.03590035061499997, -3.659038130401700339, -8.732935057095000175 ) ) ;
#9171 = CARTESIAN_POINT ( 'NONE',  ( 10.60267905665539523, -5.009718911382226025, -5.031837394736871083 ) ) ;
#9172 = CARTESIAN_POINT ( 'NONE',  ( 11.61123293495519881, -4.891405920092699589, 7.535834283667469435 ) ) ;
#9173 = ADVANCED_FACE ( 'NONE', ( #9538 ), #31569, .F. ) ;
#9174 = CARTESIAN_POINT ( 'NONE',  ( 18.27898910297786372, 2.436826214745338337, -12.36212035235843487 ) ) ;
#9175 = CARTESIAN_POINT ( 'NONE',  ( 2.605140132542667075, 0.9161175952574701631, 3.408904368339106927 ) ) ;
#9176 = PLANE ( 'NONE',  #38412 ) ;
#9177 = CARTESIAN_POINT ( 'NONE',  ( 12.27869449350294850, 2.837185661393637481, -13.59614283363436549 ) ) ;
#9178 = CARTESIAN_POINT ( 'NONE',  ( 9.349999778958000718, -4.000000000000000000, 7.500000000000000000 ) ) ;
#9179 = CARTESIAN_POINT ( 'NONE',  ( 24.63409004136600089, 11.78082236971000007, 3.229000081171000236 ) ) ;
#9180 = FACE_OUTER_BOUND ( 'NONE', #13174, .T. ) ;
#9181 = CARTESIAN_POINT ( 'NONE',  ( 12.48412837678613485, 0.6552116771452474175, -13.98466387211990281 ) ) ;
#9182 = CARTESIAN_POINT ( 'NONE',  ( 23.59108006868057572, 13.38394536322959283, 4.038510903308840660 ) ) ;
#9183 = CARTESIAN_POINT ( 'NONE',  ( 11.09999999991999964, 8.127394258944999450, 6.728184650804999833 ) ) ;
#9184 = CARTESIAN_POINT ( 'NONE',  ( 2.946806799211333594, 0.9161175952574844850, -3.408904368339102930 ) ) ;
#9185 = CARTESIAN_POINT ( 'NONE',  ( 8.722714158775000115, 3.892978337449999771, -8.893414073324001023 ) ) ;
#9186 = CARTESIAN_POINT ( 'NONE',  ( 6.655923744767410888, -0.4625088890374065564, -1.452003029584873595 ) ) ;
#9187 = ORIENTED_EDGE ( 'NONE', *, *, #55258, .F. ) ;
#9188 = CARTESIAN_POINT ( 'NONE',  ( 9.219210542222684879, -4.353245349593146685, -8.814482920002204125 ) ) ;
#9189 = CARTESIAN_POINT ( 'NONE',  ( 17.90989566141528755, 3.154773125069392670, -13.63992084652273817 ) ) ;
#9190 = ORIENTED_EDGE ( 'NONE', *, *, #30043, .F. ) ;
#9191 = DIRECTION ( 'NONE',  ( 1.000000000000000000, 0.000000000000000000, 0.000000000000000000 ) ) ;
#9192 = LINE ( 'NONE', #67232, #32383 ) ;
#9193 = CARTESIAN_POINT ( 'NONE',  ( 18.48326398027718653, 2.855662837657351183, -11.29488646771110893 ) ) ;
#9194 = CARTESIAN_POINT ( 'NONE',  ( 13.73886390325583484, 9.223149073484993465, 8.172668166918892751 ) ) ;
#9195 = CARTESIAN_POINT ( 'NONE',  ( 11.18412378248529926, -4.549028353065900809, -6.461285588983000316 ) ) ;
#9196 = CARTESIAN_POINT ( 'NONE',  ( 11.60000000000000142, -3.636382150325345730, -6.469788275435904623 ) ) ;
#9197 = FACE_OUTER_BOUND ( 'NONE', #28755, .T. ) ;
#9198 = ORIENTED_EDGE ( 'NONE', *, *, #36321, .T. ) ;
#9199 = CARTESIAN_POINT ( 'NONE',  ( 9.973631561148998514, 3.315688435009791490, -8.575598637068459595 ) ) ;
#9200 = CARTESIAN_POINT ( 'NONE',  ( 9.476970280414001024, 5.511689883260999956, -7.095113581311000672 ) ) ;
#9201 = EDGE_LOOP ( 'NONE', ( #35788, #61805, #59490, #66780 ) ) ;
#9202 = CARTESIAN_POINT ( 'NONE',  ( 10.52343057594999998, 3.209665745824000105, -9.177097971982000502 ) ) ;
#9203 = SURFACE_STYLE_USAGE ( .BOTH. , #26332 ) ;
#9204 = ORIENTED_EDGE ( 'NONE', *, *, #60921, .F. ) ;
#9205 = CARTESIAN_POINT ( 'NONE',  ( 9.985242056249999720, 3.541248877825399877, 6.305876158747000026 ) ) ;
#9206 = CARTESIAN_POINT ( 'NONE',  ( 17.83404768640024685, -1.940633243441993505, -12.56443520114847345 ) ) ;
#9207 = CARTESIAN_POINT ( 'NONE',  ( 11.35563158142000262, -11.71552011691000139, -1.381878615183999903 ) ) ;
#9208 = ADVANCED_FACE ( 'NONE', ( #15823 ), #10922, .F. ) ;
#9209 = ADVANCED_FACE ( 'NONE', ( #41710 ), #42288, .T. ) ;
#9210 = DIRECTION ( 'NONE',  ( -1.000000000000000000, 0.000000000000000000, 0.000000000000000000 ) ) ;
#9211 = EDGE_CURVE ( 'NONE', #16713, #61413, #46580, .T. ) ;
#9212 = ADVANCED_FACE ( 'NONE', ( #25631 ), #36461, .T. ) ;
#9213 = CARTESIAN_POINT ( 'NONE',  ( 10.99698512684000029, -8.058258747261000110, -7.169000291589999740 ) ) ;
#9214 = ORIENTED_EDGE ( 'NONE', *, *, #5437, .T. ) ;
#9215 = CARTESIAN_POINT ( 'NONE',  ( 10.27706886429732158, 2.899999999999999911, -6.444141223373538452 ) ) ;
#9216 = CARTESIAN_POINT ( 'NONE',  ( 10.53871084122999946, 5.103389446345000025, -6.705205355781999721 ) ) ;
#9217 = CARTESIAN_POINT ( 'NONE',  ( 8.174990947233128580, -2.650692654197974729, 7.500004443805800669 ) ) ;
#9218 = CARTESIAN_POINT ( 'NONE',  ( 8.916525748329494405, 3.463676007238744692, 8.432246543101921787 ) ) ;
#9219 = CARTESIAN_POINT ( 'NONE',  ( 18.26841422636658052, 0.1308528744652167064, 13.99939340647621044 ) ) ;
#9220 = FACE_OUTER_BOUND ( 'NONE', #41042, .T. ) ;
#9221 = CARTESIAN_POINT ( 'NONE',  ( 17.55505043854147118, -1.875000000000000000, 12.57545641911172396 ) ) ;
#9222 = ORIENTED_EDGE ( 'NONE', *, *, #65897, .F. ) ;
#9223 = EDGE_LOOP ( 'NONE', ( #48877, #25276, #33251 ) ) ;
#9224 = CARTESIAN_POINT ( 'NONE',  ( 9.128895280414001334, 3.880154689736000417, -9.060377011187000562 ) ) ;
#9225 = CARTESIAN_POINT ( 'NONE',  ( 5.599999772733800008, -6.661338147750999827E-14, -1.931788062847999572E-14 ) ) ;
#9226 = B_SPLINE_CURVE_WITH_KNOTS ( 'NONE', 3,
 ( #15579, #37581, #36907, #4726, #26417, #26769, #36557, #58915, #15911, #30979 ),
 .UNSPECIFIED., .F., .F.,
 ( 4, 2, 2, 2, 4 ),
 ( 0.000000000000000000, 0.2500000000000000000, 0.5000000000000000000, 0.7500000000000000000, 1.000000000000000000 ),
 .UNSPECIFIED. ) ;
#9227 = CARTESIAN_POINT ( 'NONE',  ( 1.071806799208249839, 3.408904368339104263, 0.9161175952574878156 ) ) ;
#9228 = CARTESIAN_POINT ( 'NONE',  ( 24.84733913753600021, 8.571409823520001581, -8.858777810802999753 ) ) ;
#9229 = CARTESIAN_POINT ( 'NONE',  ( 24.08756655391700008, 9.258138178154998954, -9.301679906964000821 ) ) ;
#9230 = CARTESIAN_POINT ( 'NONE',  ( 18.35192027319500241, -2.803655468537999962, -11.45922931039000048 ) ) ;
#9232 = CARTESIAN_POINT ( 'NONE',  ( 7.777243094059180351, 3.624681904425790968, 6.194791476713995770 ) ) ;
#9231 = CARTESIAN_POINT ( 'NONE',  ( 10.46097570133300003, -3.162316589966200020, 6.724099908144899551 ) ) ;
#9233 = CARTESIAN_POINT ( 'NONE',  ( 8.833308238655002143, -4.875955647784997460, -6.190001260256996929 ) ) ;
#9234 = ORIENTED_EDGE ( 'NONE', *, *, #64028, .T. ) ;
#9235 = VECTOR ( 'NONE', #53368, 1000.000000000000000 ) ;
#9236 = CARTESIAN_POINT ( 'NONE',  ( 9.883513540182333301, 2.750000000000000000, -7.336375382625530683 ) ) ;
#9237 = CARTESIAN_POINT ( 'NONE',  ( 10.31495997652000085, -3.356726044455999425, -4.564232296395000610 ) ) ;
#9238 = CARTESIAN_POINT ( 'NONE',  ( 9.793154437819998392, -5.792391408692000532, -6.955579396894000510 ) ) ;
#9239 = DIRECTION ( 'NONE',  ( -0.8987684456439055669, 0.000000000000000000, 0.4384236320214022764 ) ) ;
#9240 = CARTESIAN_POINT ( 'NONE',  ( 7.100000000000000533, -13.94845324556000143, -4.312847325879000770 ) ) ;
#9241 = DIRECTION ( 'NONE',  ( 0.000000000000000000, 0.000000000000000000, -1.000000000000000000 ) ) ;
#9242 = CARTESIAN_POINT ( 'NONE',  ( 9.093935841232999806, 2.156584729807999867, -7.959751745006000689 ) ) ;
#9243 = CARTESIAN_POINT ( 'NONE',  ( 13.92975648157900004, 8.821327856275999579, 7.690719526968000430 ) ) ;
#9244 = CARTESIAN_POINT ( 'NONE',  ( 8.251326917914997949, -4.957166827433998613, 6.172577619222003875 ) ) ;
#9245 = CARTESIAN_POINT ( 'NONE',  ( 10.97726354018323214, -4.629523725463626782, 6.407767014557177454 ) ) ;
#9246 = EDGE_CURVE ( 'NONE', #25113, #48331, #65727, .T. ) ;
#9247 = CARTESIAN_POINT ( 'NONE',  ( 15.40000000001299973, -8.815237407733999220, -7.616696375847999967 ) ) ;
#9248 = CARTESIAN_POINT ( 'NONE',  ( 3.210384657052000268, 3.424905925778999993, 0.06955616133957001623 ) ) ;
#9249 = EDGE_LOOP ( 'NONE', ( #48750, #45665, #35548, #3055 ) ) ;
#9250 = CARTESIAN_POINT ( 'NONE',  ( 12.42472005158248294, -0.4959841406075989889, -12.68696163625449813 ) ) ;
#9251 = CARTESIAN_POINT ( 'NONE',  ( 12.20227052514783672, -2.665223630829422596, -12.41153314577902833 ) ) ;
#9252 = ADVANCED_FACE ( 'NONE', ( #33985 ), #53912, .F. ) ;
#9253 = DIRECTION ( 'NONE',  ( 0.000000000000000000, -0.7071067811865474617, -0.7071067811865474617 ) ) ;
#9254 = DIRECTION ( 'NONE',  ( 1.000000000000000000, 3.572267238224000438E-11, -8.761989184571999838E-10 ) ) ;
#9255 = LINE ( 'NONE', #45655, #60667 ) ;
#9256 = ORIENTED_EDGE ( 'NONE', *, *, #18810, .T. ) ;
#9257 = LINE ( 'NONE', #52263, #58959 ) ;
#9258 = SHAPE_DEFINITION_REPRESENTATION ( #13187, #30050 ) ;
#9259 = CARTESIAN_POINT ( 'NONE',  ( 17.75512362461813964, 0.5924617913754783860, 12.68139389762679770 ) ) ;
#9260 = CARTESIAN_POINT ( 'NONE',  ( 13.51802873821100270, -11.59174185862000073, -2.195273509308000026 ) ) ;
#9261 = CARTESIAN_POINT ( 'NONE',  ( 10.34580110216399973, 2.909301855364999856, 8.166103548914600552 ) ) ;
#9262 = CARTESIAN_POINT ( 'NONE',  ( 10.60235971519489873, 4.605301262871499546, -6.493038401303000029 ) ) ;
#9263 = VERTEX_POINT ( 'NONE', #16849 ) ;
#9264 = CARTESIAN_POINT ( 'NONE',  ( 9.757667269575000191, -4.489271889653999814, 5.986031004145000445 ) ) ;
#9265 = ORIENTED_EDGE ( 'NONE', *, *, #55405, .F. ) ;
#9266 = CARTESIAN_POINT ( 'NONE',  ( 8.505089800085370300, -3.298395928475978511, 5.974470256167060178 ) ) ;
#9267 = CARTESIAN_POINT ( 'NONE',  ( 9.566483607044000692, -4.108965473266000146, 8.851626696081998702 ) ) ;
#9268 = CARTESIAN_POINT ( 'NONE',  ( 21.72233714749290101, 0.000000000000000000, 0.000000000000000000 ) ) ;
#9269 = ORIENTED_EDGE ( 'NONE', *, *, #9550, .T. ) ;
#9270 = CARTESIAN_POINT ( 'NONE',  ( 8.547797334239181311, 2.488073269087734296, -8.392070911480191242 ) ) ;
#9271 = CARTESIAN_POINT ( 'NONE',  ( 7.619022079480754606, 2.947662252026352459, 8.377606513860623494 ) ) ;
#9272 = CARTESIAN_POINT ( 'NONE',  ( 7.142989158770000735, 5.116254232901999544, -8.340852485897000790 ) ) ;
#9273 = CARTESIAN_POINT ( 'NONE',  ( 10.08521345716899908, 4.924890298941200228, 6.659120737011199331 ) ) ;
#9274 = CARTESIAN_POINT ( 'NONE',  ( 17.55505043854147118, -3.125000000000000000, 12.28374638332999780 ) ) ;
#9275 = ORIENTED_EDGE ( 'NONE', *, *, #67301, .F. ) ;
#9276 = CARTESIAN_POINT ( 'NONE',  ( 2.230140132540584297, -3.408904368339107815, 0.9161175952574674985 ) ) ;
#9277 = B_SPLINE_CURVE_WITH_KNOTS ( 'NONE', 3,
 ( #22225, #7881, #51217, #55778, #45292 ),
 .UNSPECIFIED., .F., .F.,
 ( 4, 1, 4 ),
 ( 0.000000000000000000, 0.5000000000000000000, 1.000000000000000000 ),
 .UNSPECIFIED. ) ;
#9278 = AXIS2_PLACEMENT_3D ( 'NONE', #30120, #9111, #41619 ) ;
#9279 = CARTESIAN_POINT ( 'NONE',  ( 12.30281274453381535, -2.118998859563833381, -13.74704000636702084 ) ) ;
#9280 = DIRECTION ( 'NONE',  ( 0.000000000000000000, 0.000000000000000000, 1.000000000000000000 ) ) ;
#9281 = ORIENTED_EDGE ( 'NONE', *, *, #14470, .T. ) ;
#9282 = LINE ( 'NONE', #14551, #49762 ) ;
#9283 = AXIS2_PLACEMENT_3D ( 'NONE', #44615, #43213, #57394 ) ;
#9284 = CARTESIAN_POINT ( 'NONE',  ( 9.258050732556000639, -4.895927245463000510, -6.008721945297999412 ) ) ;
#9285 = B_SPLINE_CURVE_WITH_KNOTS ( 'NONE', 3,
 ( #16895, #38224, #5716, #59204, #16209, #10970, #26368 ),
 .UNSPECIFIED., .F., .F.,
 ( 4, 1, 1, 1, 4 ),
 ( 0.000000000000000000, 0.2500000590475000006, 0.5000000002693999468, 0.7499999414914000351, 1.000000000000000000 ),
 .UNSPECIFIED. ) ;
#9286 = ORIENTED_EDGE ( 'NONE', *, *, #39309, .T. ) ;
#9287 = CARTESIAN_POINT ( 'NONE',  ( 23.98813794683320921, 12.73148067554796725, -3.487252914621118638 ) ) ;
#9288 = LINE ( 'NONE', #47057, #3093 ) ;
#9289 = DIRECTION ( 'NONE',  ( 1.000000000000000000, 0.000000000000000000, 0.000000000000000000 ) ) ;
#9290 = FACE_OUTER_BOUND ( 'NONE', #29011, .T. ) ;
#9291 = EDGE_CURVE ( 'NONE', #60176, #51578, #55744, .T. ) ;
#9292 = CARTESIAN_POINT ( 'NONE',  ( 12.39133745138800613, 2.968584063660573147, 13.56278128057737042 ) ) ;
#9293 = EDGE_CURVE ( 'NONE', #35342, #26251, #64873, .T. ) ;
#9295 = EDGE_CURVE ( 'NONE', #48911, #19729, #69100, .T. ) ;
#9294 = CARTESIAN_POINT ( 'NONE',  ( 17.75825915738909444, -1.908867900852240673, 12.56984843829418885 ) ) ;
#9296 = ORIENTED_EDGE ( 'NONE', *, *, #66539, .F. ) ;
#9297 = CARTESIAN_POINT ( 'NONE',  ( 3.300973465876999580, -3.500000000000000000, 0.000000000000000000 ) ) ;
#9298 = ORIENTED_EDGE ( 'NONE', *, *, #15779, .T. ) ;
#9299 = CARTESIAN_POINT ( 'NONE',  ( 10.01533268956000100, 4.946987614118000032, 8.559212393557999121 ) ) ;
#9300 = MECHANICAL_DESIGN_GEOMETRIC_PRESENTATION_REPRESENTATION (  '', ( #68480 ), #8220 ) ;
#9301 = DIRECTION ( 'NONE',  ( -1.000000000000000000, 0.000000000000000000, 0.000000000000000000 ) ) ;
#9302 = CARTESIAN_POINT ( 'NONE',  ( 8.640504719592000171, 2.305580295895999665, -7.860904109308999743 ) ) ;
#9303 = CARTESIAN_POINT ( 'NONE',  ( 3.599756407902999999, -1.745607925010999928, 3.083988108660999927 ) ) ;
#9304 = CARTESIAN_POINT ( 'NONE',  ( 9.843620110012999191, -5.021680390140000227, -8.761463725090999688 ) ) ;
#9305 = CARTESIAN_POINT ( 'NONE',  ( 9.233215486276282746, -3.972057587790281730, 6.616784466747247073 ) ) ;
#9306 = CARTESIAN_POINT ( 'NONE',  ( 9.005622771607709964, -5.254628312680063473, 7.997745863565469904 ) ) ;
#9307 = ORIENTED_EDGE ( 'NONE', *, *, #44625, .T. ) ;
#9308 = CARTESIAN_POINT ( 'NONE',  ( 11.83456651104149948, -3.887457492043800311, 8.635175889530000148 ) ) ;
#9309 = CARTESIAN_POINT ( 'NONE',  ( 10.26947109217999810, 5.100000000000000533, -6.152188490330000370 ) ) ;
#9310 = CARTESIAN_POINT ( 'NONE',  ( 15.45446786537200090, 9.133287421996001854, 8.216743560820999548 ) ) ;
#9311 = EDGE_CURVE ( 'NONE', #20987, #19641, #18221, .T. ) ;
#9312 = CARTESIAN_POINT ( 'NONE',  ( 20.10000000000000142, -11.84999999999999964, 0.000000000000000000 ) ) ;
#9314 = CARTESIAN_POINT ( 'NONE',  ( 23.89320776801300283, -3.226867021103002831, -11.46303308828999867 ) ) ;
#9313 = CARTESIAN_POINT ( 'NONE',  ( 9.166073843917999397, 4.023333628930999772, 9.122276991855001071 ) ) ;
#9315 = CARTESIAN_POINT ( 'NONE',  ( 10.60026222744819790, 3.225465054973100099, -8.138001937130599828 ) ) ;
#9316 = DIRECTION ( 'NONE',  ( 0.000000000000000000, 0.000000000000000000, -1.000000000000000000 ) ) ;
#9317 = CARTESIAN_POINT ( 'NONE',  ( 10.06027973160899869, 4.090130512164860122, -6.499640669006000238 ) ) ;
#9318 = CARTESIAN_POINT ( 'NONE',  ( 18.22962529608892623, 0.2638285456865405720, 12.59724228039519645 ) ) ;
#9319 = CARTESIAN_POINT ( 'NONE',  ( 7.147951193688999005, -1.276447038156000025, 0.5071930294755999657 ) ) ;
#9320 = CARTESIAN_POINT ( 'NONE',  ( 11.34523293495530005, 2.684794526488000432, 7.552870914315270134 ) ) ;
#9321 = CARTESIAN_POINT ( 'NONE',  ( 0.4755637383194235568, 3.469857622234496120, -0.4961820259388217691 ) ) ;
#9322 = EDGE_LOOP ( 'NONE', ( #26176, #19142, #29261, #67001 ) ) ;
#9323 = CARTESIAN_POINT ( 'NONE',  ( 8.320870559624999885, -3.894643656844000379, 6.044452984962999764 ) ) ;
#9324 = DIRECTION ( 'NONE',  ( -0.000000000000000000, 0.3222656952305000266, 0.9466492601157001641 ) ) ;
#9325 = FACE_BOUND ( 'NONE', #33574, .T. ) ;
#9326 = ORIENTED_EDGE ( 'NONE', *, *, #50455, .F. ) ;
#9327 = CIRCLE ( 'NONE', #68515, 12.39999890530000037 ) ;
#9328 = CARTESIAN_POINT ( 'NONE',  ( 0.7323805749852000391, 2.971343835407000089, -0.7711576440234000351 ) ) ;
#9329 = CARTESIAN_POINT ( 'NONE',  ( 11.59966954483535773, 4.638989336656000440, 8.485927942460499196 ) ) ;
#9330 = CARTESIAN_POINT ( 'NONE',  ( 10.48598278040999965, 5.506034726153999692, -7.274787238512000265 ) ) ;
#9331 = VERTEX_POINT ( 'NONE', #1469 ) ;
#9332 = LINE ( 'NONE', #13917, #46244 ) ;
#9333 = CARTESIAN_POINT ( 'NONE',  ( 18.20209611035324926, -2.854851737566545644, 12.27307487512611317 ) ) ;
#9334 = CARTESIAN_POINT ( 'NONE',  ( 10.61656919669529842, 5.225637333137999718, 7.137881914002699446 ) ) ;
#9335 = ADVANCED_FACE ( 'NONE', ( #7401 ), #7587, .T. ) ;
#9336 = CARTESIAN_POINT ( 'NONE',  ( 23.50387503050299998, 6.998357211011000167, -12.12530396926999998 ) ) ;
#9337 = DIRECTION ( 'NONE',  ( -1.000000000000000000, 0.000000000000000000, 0.000000000000000000 ) ) ;
#9338 = ORIENTED_EDGE ( 'NONE', *, *, #3732, .T. ) ;
#9339 = CARTESIAN_POINT ( 'NONE',  ( 7.835503439526941172, -4.950930448547884666, 6.483249265681529927 ) ) ;
#9340 = CARTESIAN_POINT ( 'NONE',  ( 15.80279819343546244, 8.703657694420872559, 8.043987028914530768 ) ) ;
#9341 = CARTESIAN_POINT ( 'NONE',  ( 8.099647544207300598, -4.546102203237349038, 5.848288472323551090 ) ) ;
#9342 = CIRCLE ( 'NONE', #12708, 0.5499999999999998224 ) ;
#9343 = CARTESIAN_POINT ( 'NONE',  ( 9.676721904869999946, -3.004358235431599855, 6.941043897400199114 ) ) ;
#9344 = VERTEX_POINT ( 'NONE', #60203 ) ;
#9345 = CARTESIAN_POINT ( 'NONE',  ( 11.13224971717000145, -5.325575099955998759, -4.980474265038999704 ) ) ;
#9346 = CARTESIAN_POINT ( 'NONE',  ( 11.31349144726329925, -4.738947899111299655, 8.542723541016000510 ) ) ;
#9347 = ORIENTED_EDGE ( 'NONE', *, *, #23348, .T. ) ;
#9348 = CARTESIAN_POINT ( 'NONE',  ( 12.80505043854146940, -1.845932447629014872, -13.81930785430178155 ) ) ;
#9349 = CIRCLE ( 'NONE', #49536, 0.6999999999999992895 ) ;
#9350 = VERTEX_POINT ( 'NONE', #54607 ) ;
#9351 = CARTESIAN_POINT ( 'NONE',  ( 9.523148997461001741, -5.167567567567999731, -6.822293592207000934 ) ) ;
#9352 = CARTESIAN_POINT ( 'NONE',  ( 10.98768577056000062, -2.700436730051000378, -4.945210085382000464 ) ) ;
#9353 = CARTESIAN_POINT ( 'NONE',  ( 10.85168717260509830, 3.386210853237200169, -8.501809683958001074 ) ) ;
#9354 = CARTESIAN_POINT ( 'NONE',  ( 11.13880513895979973, -2.849548954067000039, 8.139542779846600240 ) ) ;
#9355 = CARTESIAN_POINT ( 'NONE',  ( 12.27338658866627341, 2.829189413748181003, -12.36878769217040741 ) ) ;
#9356 = CARTESIAN_POINT ( 'NONE',  ( 12.07656516821461068, -3.100463633631699967, 6.592171857671999646 ) ) ;
#9357 = CARTESIAN_POINT ( 'NONE',  ( 8.913573341230998537, 2.550580605805000012, 8.854682662413999594 ) ) ;
#9358 = ORIENTED_EDGE ( 'NONE', *, *, #10950, .T. ) ;
#9359 = CARTESIAN_POINT ( 'NONE',  ( 9.396013540183334456, 3.000416447002273834, -8.268183399968641822 ) ) ;
#9360 = CARTESIAN_POINT ( 'NONE',  ( 11.41486084871699802, -5.207010770456999893, -7.825000000000000178 ) ) ;
#9361 = LINE ( 'NONE', #42239, #40220 ) ;
#9362 = ORIENTED_EDGE ( 'NONE', *, *, #30925, .F. ) ;
#9363 = CARTESIAN_POINT ( 'NONE',  ( 12.33364337825308965, -2.910866508044257728, -12.34629936699908015 ) ) ;
#9364 = CARTESIAN_POINT ( 'NONE',  ( 11.40425819896749893, 2.744109752373000255, 7.263238376356399684 ) ) ;
#9365 = CARTESIAN_POINT ( 'NONE',  ( 10.47111935320999976, -5.170637620872999385, -8.712950754783999940 ) ) ;
#9366 = CARTESIAN_POINT ( 'NONE',  ( 8.842615099866989681, 7.893622066425994177, -5.162893036762002730 ) ) ;
#9367 = CARTESIAN_POINT ( 'NONE',  ( 18.26281931570200356, -2.856833007231000199, -11.95042392763000016 ) ) ;
#9368 = FACE_OUTER_BOUND ( 'NONE', #65845, .T. ) ;
#9369 = CARTESIAN_POINT ( 'NONE',  ( 12.70233692021773564, -1.883156082608298032, -13.78505115204619713 ) ) ;
#9370 = AXIS2_PLACEMENT_3D ( 'NONE', #50309, #28648, #39126 ) ;
#9371 = CARTESIAN_POINT ( 'NONE',  ( 11.68333460557258796, -3.837988184179999873, -8.490304555719900392 ) ) ;
#9372 = FACE_OUTER_BOUND ( 'NONE', #21580, .T. ) ;
#9373 = ADVANCED_FACE ( 'NONE', ( #28746, #778 ), #64733, .F. ) ;
#9375 = EDGE_CURVE ( 'NONE', #26060, #12138, #44437, .T. ) ;
#9374 = CARTESIAN_POINT ( 'NONE',  ( 17.72109462663384605, -3.180738073285652945, 12.19192004217518743 ) ) ;
#9376 = EDGE_LOOP ( 'NONE', ( #18571, #14377, #32930, #25442, #66746 ) ) ;
#9377 = ORIENTED_EDGE ( 'NONE', *, *, #224, .T. ) ;
#9378 = CARTESIAN_POINT ( 'NONE',  ( 12.61731565722499759, 0.7069209314914761677, -13.98214394338181954 ) ) ;
#9379 = VECTOR ( 'NONE', #65471, 1000.000000000000114 ) ;
#9380 = FILL_AREA_STYLE_COLOUR ( '', #26226 ) ;
#9381 = CARTESIAN_POINT ( 'NONE',  ( 11.09999999999999964, -2.399999999999999911, 6.571291218949999902 ) ) ;
#9382 = CARTESIAN_POINT ( 'NONE',  ( 7.996487690580179830, 5.313957503662987136, 7.853744048643257258 ) ) ;
#9383 = CARTESIAN_POINT ( 'NONE',  ( 10.74708949327000163, 5.603142351927999698, -6.963341971584000589 ) ) ;
#9384 = CARTESIAN_POINT ( 'NONE',  ( 13.48832048419379426, 11.62805077016393440, 2.291814632468947899 ) ) ;
#9385 = CARTESIAN_POINT ( 'NONE',  ( 18.12879050829617711, 2.748092781515380612, 12.39029782533441093 ) ) ;
#9386 = CYLINDRICAL_SURFACE ( 'NONE', #13818, 0.5000000000000004441 ) ;
#9387 = CARTESIAN_POINT ( 'NONE',  ( 10.34520858566999912, 2.724123081339000052, 6.497325124886000225 ) ) ;
#9388 = CARTESIAN_POINT ( 'NONE',  ( 10.81746213571000048, -5.100000000000000533, 6.571291218949999902 ) ) ;
#9389 = ORIENTED_EDGE ( 'NONE', *, *, #66517, .T. ) ;
#9390 = CARTESIAN_POINT ( 'NONE',  ( 12.43857111758547163, -3.006687177877844785, 12.31897860641675635 ) ) ;
#9391 = CARTESIAN_POINT ( 'NONE',  ( 13.73895793914716634, 8.868838256396804454, 7.856013393113998156 ) ) ;
#9392 = CARTESIAN_POINT ( 'NONE',  ( 10.44675156161000018, 2.885046387990999772, 8.863482298832000339 ) ) ;
#9393 = ADVANCED_FACE ( 'NONE', ( #59157, #33640 ), #11261, .F. ) ;
#9394 = CARTESIAN_POINT ( 'NONE',  ( 11.76723293495529887, -5.173938955706000264, 7.547192037433419820 ) ) ;
#9395 = B_SPLINE_CURVE_WITH_KNOTS ( 'NONE', 3,
 ( #38536, #60214, #59860, #28056, #33650, #1829, #17915, #49719, #39232, #23146, #44496, #35376, #67512, #13707, #28759, #24184, #51442, #13367 ),
 .UNSPECIFIED., .F., .F.,
 ( 4, 1, 2, 2, 1, 2, 2, 2, 2, 4 ),
 ( 0.000000000000000000, 0.1249999999999908962, 0.1874999999999859557, 0.2499999999999810152, 0.3749999999999767963, 0.4374999999999779066, 0.4999999999999790168, 0.6249999999999841238, 0.7499999999999892308, 1.000000000000000000 ),
 .UNSPECIFIED. ) ;
#9396 = CARTESIAN_POINT ( 'NONE',  ( 8.622785841227999626, 5.189036231907000030, -8.048606212067999977 ) ) ;
#9397 = CARTESIAN_POINT ( 'NONE',  ( 11.07072899110000108, 7.292403078108999459, -6.230988430885999740 ) ) ;
#9398 = EDGE_CURVE ( 'NONE', #57810, #22542, #51643, .T. ) ;
#9399 = CARTESIAN_POINT ( 'NONE',  ( 25.29881401420400167, 8.389234982073000779, 8.297993602990999307 ) ) ;
#9400 = CARTESIAN_POINT ( 'NONE',  ( 12.26373771493048181, 0.3125877143166541638, 12.69482668528968183 ) ) ;
#9401 = VECTOR ( 'NONE', #7647, 1000.000000000000000 ) ;
#9402 = CARTESIAN_POINT ( 'NONE',  ( 5.664191326654759884, -12.07183080424680988, -3.732901064427135207 ) ) ;
#9403 = CARTESIAN_POINT ( 'NONE',  ( 10.59344747867000081, 5.297752619853000944, 8.474195539311001113 ) ) ;
#9404 = CARTESIAN_POINT ( 'NONE',  ( 14.93333333161133503, 9.471995579709359347, 8.194932869644874884 ) ) ;
#9405 = VERTEX_POINT ( 'NONE', #65076 ) ;
#9406 = CARTESIAN_POINT ( 'NONE',  ( 9.286929719595001131, 4.102804347295999854, -5.770625657082999460 ) ) ;
#9407 = CARTESIAN_POINT ( 'NONE',  ( -0.000000000000000000, 1.781870588985605464, 2.319407620233724820 ) ) ;
#9408 = B_SPLINE_CURVE_WITH_KNOTS ( 'NONE', 3,
 ( #35527, #56848, #20122, #30287, #51590, #25026, #46357, #57518, #52281, #11688, #16247, #63449, #11345, #26757, #58214, #64133, #6098 ),
 .UNSPECIFIED., .F., .F.,
 ( 4, 2, 2, 2, 1, 2, 2, 2, 4 ),
 ( 0.000000000000000000, 0.2500000000000272560, 0.3750000000000394684, 0.4375000000000455747, 0.4687500000000475731, 0.4843750000000475731, 0.5000000000000476286, 0.7500000000000237588, 1.000000000000000000 ),
 .UNSPECIFIED. ) ;
#9409 = CARTESIAN_POINT ( 'NONE',  ( 10.32309687351566652, 2.782534154164606921, 7.827184855449101697 ) ) ;
#9410 = CARTESIAN_POINT ( 'NONE',  ( 12.10000000000000320, -4.094072174251358831, 8.528759793293474445 ) ) ;
#9411 = CARTESIAN_POINT ( 'NONE',  ( 11.46179707368349909, -4.498457171163099844, -6.629085939160999530 ) ) ;
#9412 = EDGE_LOOP ( 'NONE', ( #33382, #41495, #64323, #47840 ) ) ;
#9413 = CARTESIAN_POINT ( 'NONE',  ( 2.297248059201999482, -3.604362431180999859, -1.066289260138999939 ) ) ;
#9414 = CARTESIAN_POINT ( 'NONE',  ( 10.48170095836776028, -2.322637725008158238, 6.770404810779447224 ) ) ;
#9417 = CARTESIAN_POINT ( 'NONE',  ( 13.91137892731300063, -9.265832517555999459, -8.206449300197000696 ) ) ;
#9416 = LINE ( 'NONE', #9763, #11801 ) ;
#9415 = PRODUCT_DEFINITION_CONTEXT ( 'detailed design', #51657, 'design' ) ;
#9418 = CARTESIAN_POINT ( 'NONE',  ( 18.14647333850305699, -2.702177529538977829, 13.62849908381775066 ) ) ;
#9419 = ORIENTED_EDGE ( 'NONE', *, *, #53518, .F. ) ;
#9420 = FACE_OUTER_BOUND ( 'NONE', #39938, .T. ) ;
#9421 = CARTESIAN_POINT ( 'NONE',  ( 18.17537806675986545, -2.421014888063410808, -13.68986186821174122 ) ) ;
#9422 = CARTESIAN_POINT ( 'NONE',  ( 11.34287482311539996, 4.803125295093300551, 7.175518335304800210 ) ) ;
#9423 = CARTESIAN_POINT ( 'NONE',  ( 24.63612324460100211, -11.85362448828802151, 3.193519006004666316 ) ) ;
#9424 = CARTESIAN_POINT ( 'NONE',  ( 7.886566940378000545, -3.084082018960999871, 9.259837032825000591 ) ) ;
#9425 = EDGE_LOOP ( 'NONE', ( #43323, #44695, #65662, #54629 ) ) ;
#9426 = CARTESIAN_POINT ( 'NONE',  ( 8.893204719592999297, 3.977267228909999730, 9.308925224542001331 ) ) ;
#9428 = CARTESIAN_POINT ( 'NONE',  ( 10.91194340358000048, 5.022355073325999619, 4.912227978166000320 ) ) ;
#9427 = CARTESIAN_POINT ( 'NONE',  ( 10.69837472757367713, 3.526507217177279330, -8.234774922628410820 ) ) ;
#9429 = CARTESIAN_POINT ( 'NONE',  ( 7.591617075526322367, -4.370784861422539080, 5.800362021175127225 ) ) ;
#9430 = VECTOR ( 'NONE', #10990, 1000.000000000000000 ) ;
#9431 = CARTESIAN_POINT ( 'NONE',  ( 18.11727536438081643, -0.2737665426917151312, 13.89638618295341743 ) ) ;
#9432 = CARTESIAN_POINT ( 'NONE',  ( 0.7848354242999000530, 3.204751743350000126, -0.5916681129576000231 ) ) ;
#9433 = ORIENTED_EDGE ( 'NONE', *, *, #722, .T. ) ;
#9434 = CYLINDRICAL_SURFACE ( 'NONE', #28852, 1.999999999999999778 ) ;
#9435 = CARTESIAN_POINT ( 'NONE',  ( 11.96179707368349909, -4.498457171163099844, 8.370914060838998694 ) ) ;
#9436 = CARTESIAN_POINT ( 'NONE',  ( 11.52531641787287597, 3.660964319297691283, 8.308706962315561384 ) ) ;
#9437 = CARTESIAN_POINT ( 'NONE',  ( 11.29622358543999994, 3.561657733933999648, 6.266050246368000565 ) ) ;
#9438 = CARTESIAN_POINT ( 'NONE',  ( 10.81764560330029923, 4.349570499512200428, 8.585859374935999710 ) ) ;
#9439 = B_SPLINE_CURVE_WITH_KNOTS ( 'NONE', 3,
 ( #19550, #35296, #41556, #57628 ),
 .UNSPECIFIED., .F., .F.,
 ( 4, 4 ),
 ( 0.000000000000000000, 1.000000000000000000 ),
 .UNSPECIFIED. ) ;
#9440 = CARTESIAN_POINT ( 'NONE',  ( 24.11583145280971507, -3.333338908579203341, 12.53524871031152088 ) ) ;
#9441 = CARTESIAN_POINT ( 'NONE',  ( 8.710288521113000115, -4.352953559891299840, -8.284550957747498501 ) ) ;
#9442 = CARTESIAN_POINT ( 'NONE',  ( 7.399999875133000060, -0.9999998751120001694, -1.219899823892999791E-10 ) ) ;
#9443 = CARTESIAN_POINT ( 'NONE',  ( 25.19548435074899828, -3.342129198621000441, -11.59778229319999987 ) ) ;
#9444 = CIRCLE ( 'NONE', #6103, 0.8000000000000000444 ) ;
#9445 = CARTESIAN_POINT ( 'NONE',  ( 24.38453341727200296, -12.23039280200000078, -3.201153185139999913 ) ) ;
#9446 = CARTESIAN_POINT ( 'NONE',  ( 17.83317199299634126, 3.060086213980319769, -13.53858764060185216 ) ) ;
#9447 = VERTEX_POINT ( 'NONE', #60893 ) ;
#9448 = FACE_OUTER_BOUND ( 'NONE', #3624, .T. ) ;
#9449 = CARTESIAN_POINT ( 'NONE',  ( 9.652931135702420562, -5.100000000000000533, -6.444141223381761208 ) ) ;
#9450 = ORIENTED_EDGE ( 'NONE', *, *, #30926, .T. ) ;
#9451 = CARTESIAN_POINT ( 'NONE',  ( 8.199995020667000034, 2.894508905068999827, 6.645190348705000360 ) ) ;
#9453 = CARTESIAN_POINT ( 'NONE',  ( 10.67826222744820086, 3.331419131587999960, 6.949274830123499669 ) ) ;
#9452 = AXIS2_PLACEMENT_3D ( 'NONE', #53334, #48774, #32021 ) ;
#9454 = CARTESIAN_POINT ( 'NONE',  ( 9.104014120666999332, 5.045862207587999748, 8.527865280865999154 ) ) ;
#9455 = CARTESIAN_POINT ( 'NONE',  ( 10.11859053700000111, 3.393394511985999618, -5.921995869926000466 ) ) ;
#9456 = CARTESIAN_POINT ( 'NONE',  ( 9.353545867770625577, -3.141341610201948686, -7.668041776205901883 ) ) ;
#9457 = CARTESIAN_POINT ( 'NONE',  ( 10.46085355684000007, -5.403406918566000527, 7.721809917403000156 ) ) ;
#9458 = CARTESIAN_POINT ( 'NONE',  ( 18.26152580467100250, -0.1632583333441851581, -12.59896334813831409 ) ) ;
#9459 = CARTESIAN_POINT ( 'NONE',  ( 12.27407495021074801, 2.829836729549234153, -12.36860105340628557 ) ) ;
#9460 = CARTESIAN_POINT ( 'NONE',  ( 10.82595391537419971, -3.283439621430300104, -7.986661909549199301 ) ) ;
#9461 = ADVANCED_FACE ( 'NONE', ( #35363 ), #16513, .T. ) ;
#9463 = EDGE_CURVE ( 'NONE', #39016, #53063, #29095, .T. ) ;
#9462 = CARTESIAN_POINT ( 'NONE',  ( 7.598073341229000022, 3.554857159507999853, 8.889479859586000288 ) ) ;
#9464 = EDGE_LOOP ( 'NONE', ( #13688, #27267, #42855, #341, #48566, #1429 ) ) ;
#9465 = CARTESIAN_POINT ( 'NONE',  ( 11.01655322883999943, -5.424331390032000044, -4.991943751707999866 ) ) ;
#9466 =( NAMED_UNIT ( * ) PLANE_ANGLE_UNIT ( ) SI_UNIT ( $, .RADIAN. ) );
#9467 = DIRECTION ( 'NONE',  ( 0.000000000000000000, -0.7071067811865474617, -0.7071067811865474617 ) ) ;
#9468 = LINE ( 'NONE', #55399, #46152 ) ;
#9469 = CARTESIAN_POINT ( 'NONE',  ( 10.14393020684899938, -2.750000000000000000, -7.500000000000000000 ) ) ;
#9470 = CARTESIAN_POINT ( 'NONE',  ( 17.91028475965235600, 1.853043856158717251, 12.46299565389693065 ) ) ;
#9471 = CARTESIAN_POINT ( 'NONE',  ( 12.25717089523534753, 2.039201503940123228, 13.85070424198621097 ) ) ;
#9472 = CARTESIAN_POINT ( 'NONE',  ( 10.18909467608999897, -5.907859813488999912, 7.801539220053999912 ) ) ;
#9473 = ORIENTED_EDGE ( 'NONE', *, *, #11814, .T. ) ;
#9474 = LINE ( 'NONE', #63646, #64930 ) ;
#9475 = CARTESIAN_POINT ( 'NONE',  ( 10.90000000000000036, 0.2999999999999999889, 4.902439024389999567 ) ) ;
#9476 = ORIENTED_EDGE ( 'NONE', *, *, #7337, .F. ) ;
#9477 = CARTESIAN_POINT ( 'NONE',  ( 24.50399615158200106, 8.846403136021999458, 9.151488484734001005 ) ) ;
#9478 = CARTESIAN_POINT ( 'NONE',  ( 6.899999691988000450, -12.43893545635000031, -2.828937028792000152 ) ) ;
#9479 = CARTESIAN_POINT ( 'NONE',  ( 9.124702828701000357, -4.778665285493000070, 8.799745834808000211 ) ) ;
#9480 = CARTESIAN_POINT ( 'NONE',  ( 10.66684687351589744, -3.231816600031351516, -6.500416447002278275 ) ) ;
#9481 = CARTESIAN_POINT ( 'NONE',  ( 11.15364694612719809, -4.804498860841600383, 7.178938988280099132 ) ) ;
#9482 = B_SPLINE_SURFACE_WITH_KNOTS ( 'NONE', 3, 3, ( 
 ( #38941, #12366, #55016, #22495 ),
 ( #64792, #53966, #1878, #6071 ),
 ( #27409, #38583, #22152, #16903 ),
 ( #23196, #65839, #38233, #11659 ),
 ( #59907, #12015, #33351, #56746 ),
 ( #24918, #66529, #14095, #18305 ) ),
 .UNSPECIFIED., .F., .F., .F.,
 ( 4, 1, 1, 4 ),
 ( 4, 4 ),
 ( 0.1811037619699999990, 0.3333333333333000081, 0.6666666666667000474, 0.8725156331704999602 ),
 ( -0.1256563615239000009, 1.125656361510000147 ),
 .UNSPECIFIED. ) ;
#9483 = EDGE_CURVE ( 'NONE', #28703, #29686, #30458, .T. ) ;
#9484 = CARTESIAN_POINT ( 'NONE',  ( 23.60000000000000497, 11.54188747559392958, -7.798329221074294715 ) ) ;
#9485 =( GEOMETRIC_REPRESENTATION_CONTEXT ( 3 ) GLOBAL_UNCERTAINTY_ASSIGNED_CONTEXT ( ( #50449 ) ) GLOBAL_UNIT_ASSIGNED_CONTEXT ( ( #63078, #8929, #20106 ) ) REPRESENTATION_CONTEXT ( 'NONE', 'WORKASPACE' ) );
#9486 = CARTESIAN_POINT ( 'NONE',  ( -0.1096015927428999892, -0.5648807336705999882, -3.658284285490000176 ) ) ;
#9487 = CARTESIAN_POINT ( 'NONE',  ( 24.30000000000000071, 9.289189189551001036, 7.908916752674000072 ) ) ;
#9488 = CARTESIAN_POINT ( 'NONE',  ( 12.08128888832027137, 2.529854562579153754, 12.34343511423995388 ) ) ;
#9489 = CARTESIAN_POINT ( 'NONE',  ( 9.265308298767999773, -5.700621988293000264, -7.339579610785999186 ) ) ;
#9490 = CARTESIAN_POINT ( 'NONE',  ( 10.25564828895399927, 4.880669054351300495, -7.981013126389099099 ) ) ;
#9491 = CARTESIAN_POINT ( 'NONE',  ( 17.92628981779796860, 3.345291551605440894, 11.86067033226837708 ) ) ;
#9492 = CARTESIAN_POINT ( 'NONE',  ( 11.16750778041000025, 3.188704589882000118, -8.788663768996000769 ) ) ;
#9493 = CARTESIAN_POINT ( 'NONE',  ( 9.428000818238999159, 2.868129552070000088, -8.096031607030200306 ) ) ;
#9495 = CARTESIAN_POINT ( 'NONE',  ( 9.268793171738000325, -4.404188085824999987, 6.625874414451000227 ) ) ;
#9494 = CARTESIAN_POINT ( 'NONE',  ( 10.14577299472025551, 2.689531466963051454, 7.995537948248067295 ) ) ;
#9496 = B_SPLINE_CURVE_WITH_KNOTS ( 'NONE', 3,
 ( #22364, #1390, #42062, #46964, #44050 ),
 .UNSPECIFIED., .F., .F.,
 ( 4, 1, 4 ),
 ( 0.000000000000000000, 0.5000000000000000000, 1.000000000000000000 ),
 .UNSPECIFIED. ) ;
#9497 = CARTESIAN_POINT ( 'NONE',  ( 10.11501430098066656, 5.350017391163124358, -7.499999134156894343 ) ) ;
#9498 = ORIENTED_EDGE ( 'NONE', *, *, #62502, .F. ) ;
#9499 = FACE_OUTER_BOUND ( 'NONE', #50283, .T. ) ;
#9500 = CARTESIAN_POINT ( 'NONE',  ( 7.763719363403000173, 2.858336808333000079, 6.771132197038999934 ) ) ;
#9501 = AXIS2_PLACEMENT_3D ( 'NONE', #14476, #9906, #15154 ) ;
#9502 = CARTESIAN_POINT ( 'NONE',  ( 9.447848023450999833, -5.447470167531999863, 7.431328114251999573 ) ) ;
#9503 = CARTESIAN_POINT ( 'NONE',  ( 10.18491290906799840, 3.451408805716100314, 6.828616613600999585 ) ) ;
#9504 = CARTESIAN_POINT ( 'NONE',  ( 8.897621218489625505, 4.818672874536578554, -7.191281694476484354 ) ) ;
#9505 = CARTESIAN_POINT ( 'NONE',  ( 15.90003771078200145, -3.695138809391000034, -11.25918926437999978 ) ) ;
#9506 = CARTESIAN_POINT ( 'NONE',  ( 12.60268547648134074, -3.091422767983464492, 13.53007486046831964 ) ) ;
#9507 = DIRECTION ( 'NONE',  ( 1.000000000000000000, 0.000000000000000000, -5.786858783960000242E-14 ) ) ;
#9508 = CARTESIAN_POINT ( 'NONE',  ( 23.73961666470999887, 3.322481645952000129, -13.28128432273999948 ) ) ;
#9509 = ORIENTED_EDGE ( 'NONE', *, *, #26997, .T. ) ;
#9510 = CARTESIAN_POINT ( 'NONE',  ( 4.353273069765999814, -1.059004588577999950, -0.4067126231303999639 ) ) ;
#9511 = CARTESIAN_POINT ( 'NONE',  ( 8.921417874593998931, -5.177249570814000279, -8.000467616829000761 ) ) ;
#9512 = CARTESIAN_POINT ( 'NONE',  ( 5.000000004630999584, 0.6153846187707999738, -2.423076926994999880 ) ) ;
#9513 = CARTESIAN_POINT ( 'NONE',  ( 11.65278751119019951, -4.790480620979200133, 7.086443476450299706 ) ) ;
#9514 = CARTESIAN_POINT ( 'NONE',  ( 18.28010889142759865, 2.506697083851606056, -12.34815906022513410 ) ) ;
#9515 = CARTESIAN_POINT ( 'NONE',  ( 10.95359096189000070, -2.844919157736999882, 5.175303575009000845 ) ) ;
#9516 = CARTESIAN_POINT ( 'NONE',  ( 17.76019544538929296, 3.091716410417681526, 12.29381940408887530 ) ) ;
#9517 = ADVANCED_FACE ( 'NONE', ( #34336 ), #46191, .T. ) ;
#9518 = ADVANCED_FACE ( 'NONE', ( #55653 ), #27993, .T. ) ;
#9519 = CARTESIAN_POINT ( 'NONE',  ( 12.21427240567356876, 2.704226675929312762, -13.62802533659631798 ) ) ;
#9520 = CARTESIAN_POINT ( 'NONE',  ( 10.88138019924999966, -2.936733240055999783, -5.079281455792999722 ) ) ;
#9521 = CARTESIAN_POINT ( 'NONE',  ( 24.48514021601400259, 12.12976263849000169, 3.164527443243999816 ) ) ;
#9522 = DIRECTION ( 'NONE',  ( 0.000000000000000000, -1.000000000000000000, 0.000000000000000000 ) ) ;
#9523 = AXIS2_PLACEMENT_3D ( 'NONE', #36406, #40618, #19644 ) ;
#9524 = CARTESIAN_POINT ( 'NONE',  ( 4.950033214355999966, 0.000000000000000000, 0.000000000000000000 ) ) ;
#9525 = CARTESIAN_POINT ( 'NONE',  ( 23.60864783563093638, 13.39760228683210741, 3.959825147115396238 ) ) ;
#9526 = PLANE ( 'NONE',  #13124 ) ;
#9527 = CARTESIAN_POINT ( 'NONE',  ( 18.05693606621465719, 2.118559450777698583, 12.53247283884194019 ) ) ;
#9528 = CARTESIAN_POINT ( 'NONE',  ( 8.323770280408998801, 5.332332124071999857, -8.487089944253000340 ) ) ;
#9529 = CARTESIAN_POINT ( 'NONE',  ( 6.842747251585779900, 1.356930585311906690, 0.6940459256229121188 ) ) ;
#9530 = VERTEX_POINT ( 'NONE', #32517 ) ;
#9531 = CARTESIAN_POINT ( 'NONE',  ( 13.35060253487349335, 12.37707099949019707, 1.919647290784784133 ) ) ;
#9532 = CARTESIAN_POINT ( 'NONE',  ( 18.20564091649229610, 2.840274733304992694, -13.70886432971491509 ) ) ;
#9533 = ORIENTED_EDGE ( 'NONE', *, *, #26406, .T. ) ;
#9534 = CARTESIAN_POINT ( 'NONE',  ( 10.33930484851599907, -3.211495113978299898, 7.139489266142899915 ) ) ;
#9535 = CARTESIAN_POINT ( 'NONE',  ( 10.84657802013509986, 2.684088780794000151, 7.530633716161349689 ) ) ;
#9536 = CARTESIAN_POINT ( 'NONE',  ( 4.149992563291999836, -1.947893036340040629, -0.5234817089163749104 ) ) ;
#9537 = CARTESIAN_POINT ( 'NONE',  ( 9.857732874095237463, 2.650112054261821726, -7.624707679117006975 ) ) ;
#9538 = FACE_OUTER_BOUND ( 'NONE', #21085, .T. ) ;
#9539 = CARTESIAN_POINT ( 'NONE',  ( 23.66004879239100234, 9.998910715289998308, -9.691527791130999603 ) ) ;
#9540 = CARTESIAN_POINT ( 'NONE',  ( 4.982109839683335650, -0.9218200799623778030, 1.199500263597266914 ) ) ;
#9541 = ORIENTED_EDGE ( 'NONE', *, *, #7524, .T. ) ;
#9542 = CARTESIAN_POINT ( 'NONE',  ( 13.87269624719400163, 9.544758557629000606, 8.169753052074002042 ) ) ;
#9545 = ADVANCED_FACE ( 'NONE', ( #23050 ), #31859, .F. ) ;
#9544 = CARTESIAN_POINT ( 'NONE',  ( 9.924495280410999598, 4.946705552514000459, -6.253848946732999181 ) ) ;
#9543 = B_SPLINE_CURVE_WITH_KNOTS ( 'NONE', 3,
 ( #7735, #40579, #18578, #8428 ),
 .UNSPECIFIED., .F., .F.,
 ( 4, 4 ),
 ( 0.000000000000000000, 1.000000000000000000 ),
 .UNSPECIFIED. ) ;
#9546 = EDGE_LOOP ( 'NONE', ( #25218, #26804, #17563, #18813 ) ) ;
#9547 = VECTOR ( 'NONE', #40057, 1000.000000000000000 ) ;
#9548 = CARTESIAN_POINT ( 'NONE',  ( 10.98277660187000215, 2.518725482848000130, -8.314790074023999722 ) ) ;
#9549 = SURFACE_STYLE_FILL_AREA ( #57105 ) ;
#9550 = EDGE_CURVE ( 'NONE', #21890, #21254, #68222, .T. ) ;
#9551 = ORIENTED_EDGE ( 'NONE', *, *, #29876, .T. ) ;
#9552 = CARTESIAN_POINT ( 'NONE',  ( 8.617468108405999416, 5.230803879475000251, 7.151422676278199830 ) ) ;
#9553 = CARTESIAN_POINT ( 'NONE',  ( 18.04714676118040018, -2.114551447792224703, -12.53305202231724635 ) ) ;
#9554 = AXIS2_PLACEMENT_3D ( 'NONE', #17357, #17713, #39036 ) ;
#9555 = CARTESIAN_POINT ( 'NONE',  ( 5.500000000000000000, 11.00717859340000082, -1.432487142323000118 ) ) ;
#9556 = B_SPLINE_CURVE_WITH_KNOTS ( 'NONE', 3,
 ( #5997, #59486, #6694, #1457, #43769, #53897, #26658, #17182, #53215, #59834 ),
 .UNSPECIFIED., .F., .F.,
 ( 4, 2, 2, 2, 4 ),
 ( 0.000000000000000000, 0.1482977669950275301, 0.2224466504925418642, 0.2595210922412991561, 0.2965955339900564480 ),
 .UNSPECIFIED. ) ;
#9557 = CYLINDRICAL_SURFACE ( 'NONE', #29092, 0.4999999999999998335 ) ;
#9558 = CARTESIAN_POINT ( 'NONE',  ( 11.77531844363629965, -3.660964894626073107, 6.691304915923902641 ) ) ;
#9559 = ORIENTED_EDGE ( 'NONE', *, *, #3554, .T. ) ;
#9560 = CARTESIAN_POINT ( 'NONE',  ( 12.50062609531600089, 11.46460001353999836, -4.648225426428999718 ) ) ;
#9561 = DIRECTION ( 'NONE',  ( -1.000000000000000000, 0.000000000000000000, 0.000000000000000000 ) ) ;
#9562 = CARTESIAN_POINT ( 'NONE',  ( 8.060295491240839993, -3.823126980273272579, 8.848192560902774062 ) ) ;
#9563 = CARTESIAN_POINT ( 'NONE',  ( 5.305026506349999948, 1.500000000000000000, 0.000000000000000000 ) ) ;
#9564 = EDGE_CURVE ( 'NONE', #31683, #34006, #58937, .T. ) ;
#9565 = CARTESIAN_POINT ( 'NONE',  ( 17.93787990420808853, 0.6205713442106982614, 13.98624562867391496 ) ) ;
#9566 = CARTESIAN_POINT ( 'NONE',  ( 18.40429364930200151, 2.938801558760000265, 11.32979830910000096 ) ) ;
#9567 = CARTESIAN_POINT ( 'NONE',  ( 10.21238410957999854, -4.072568653311000375, -8.861841462475000597 ) ) ;
#9568 = ORIENTED_EDGE ( 'NONE', *, *, #67246, .T. ) ;
#9569 = ORIENTED_EDGE ( 'NONE', *, *, #4079, .F. ) ;
#9570 = CARTESIAN_POINT ( 'NONE',  ( 9.865910841232000905, 2.685250982074999904, -7.026194612421999608 ) ) ;
#9571 = CYLINDRICAL_SURFACE ( 'NONE', #67875, 1.250000000000000222 ) ;
#9572 = CARTESIAN_POINT ( 'NONE',  ( 6.899999691988000450, -13.10000000000000142, 0.000000000000000000 ) ) ;
#9573 = CARTESIAN_POINT ( 'NONE',  ( 25.48369865294700176, 8.423008303568998656, -7.952430695590999576 ) ) ;
#9574 = CARTESIAN_POINT ( 'NONE',  ( 11.34523293495530005, 2.684794526488000432, -7.447129085684729866 ) ) ;
#9575 = CARTESIAN_POINT ( 'NONE',  ( 10.24457120343299898, 3.957971921952620598, -8.365991721916298474 ) ) ;
#9577 = CARTESIAN_POINT ( 'NONE',  ( 7.827627258077122008, 4.479918276951376122, 6.205276188899031098 ) ) ;
#9576 = CARTESIAN_POINT ( 'NONE',  ( 9.422480666858998433, -3.619299191678599925, 6.423523106103999680 ) ) ;
#9578 = CARTESIAN_POINT ( 'NONE',  ( 7.722414202460995192, -2.834216095980001349, 6.826613447391997269 ) ) ;
#9579 = VERTEX_POINT ( 'NONE', #66735 ) ;
#9580 = CARTESIAN_POINT ( 'NONE',  ( 9.685596873515667227, 5.092232985442825210, -6.870476274536379435 ) ) ;
#9581 = AXIS2_PLACEMENT_3D ( 'NONE', #28876, #50184, #44947 ) ;
#9582 = FACE_OUTER_BOUND ( 'NONE', #45929, .T. ) ;
#9583 = CARTESIAN_POINT ( 'NONE',  ( 9.912329965421998068, 3.111510091554099855, 6.579690231462300254 ) ) ;
#9584 = CARTESIAN_POINT ( 'NONE',  ( 12.04684497800060150, -4.976842342332563618, 7.175001354288133015 ) ) ;
#9585 = CARTESIAN_POINT ( 'NONE',  ( 18.17508965101259832, -2.579233224755918208, -12.43275545427360385 ) ) ;
#9586 = CARTESIAN_POINT ( 'NONE',  ( 18.17514718081074676, 2.578773340588377483, -12.43289648652257995 ) ) ;
#9587 = CYLINDRICAL_SURFACE ( 'NONE', #823, 11.35000000000000142 ) ;
#9588 = CARTESIAN_POINT ( 'NONE',  ( 13.73862479881500143, 8.949604875896001843, 7.398842444207000213 ) ) ;
#9589 = CARTESIAN_POINT ( 'NONE',  ( 7.802608290491005683, -4.876635182444005068, 6.352765399118998069 ) ) ;
#9590 = AXIS2_PLACEMENT_3D ( 'NONE', #39901, #18574, #3507 ) ;
#9591 = CARTESIAN_POINT ( 'NONE',  ( 11.10328610135029948, 3.121939224269600022, 7.174999999999999822 ) ) ;
#9592 = CARTESIAN_POINT ( 'NONE',  ( 9.202182965154774408, 2.714244241234048616, 7.027734220012949784 ) ) ;
#9593 = CARTESIAN_POINT ( 'NONE',  ( 0.1499942179680000265, -2.402872127494064536, -1.384928887584821133 ) ) ;
#9594 = CARTESIAN_POINT ( 'NONE',  ( 3.353430505373999893, -0.8378046959084999301, 3.321581098373000529 ) ) ;
#9595 = ORIENTED_EDGE ( 'NONE', *, *, #40876, .F. ) ;
#9596 = EDGE_CURVE ( 'NONE', #54370, #68077, #50794, .T. ) ;
#9597 = EDGE_CURVE ( 'NONE', #25656, #49930, #6569, .T. ) ;
#9598 = CARTESIAN_POINT ( 'NONE',  ( 12.25868397512095243, -0.3036663359794735673, -12.69511825016613749 ) ) ;
#9599 = CARTESIAN_POINT ( 'NONE',  ( 12.18024789519250284, -2.481080537702162303, -12.45595244967812576 ) ) ;
#9600 = PLANE ( 'NONE',  #24219 ) ;
#9601 = CARTESIAN_POINT ( 'NONE',  ( 7.100000000000000533, -4.000000000000000000, 8.849999999999999645 ) ) ;
#9602 = CARTESIAN_POINT ( 'NONE',  ( 9.035438658680838842, -2.896181042233768377, -6.646458295446667108 ) ) ;
#9603 = ORIENTED_EDGE ( 'NONE', *, *, #46926, .F. ) ;
#9604 = CARTESIAN_POINT ( 'NONE',  ( -15.86200481174999943, -5.599999999999999645, -6.571291218949999902 ) ) ;
#9605 = EDGE_CURVE ( 'NONE', #67571, #27153, #66630, .T. ) ;
#9606 = APPLICATION_PROTOCOL_DEFINITION ( 'draft international standard', 'automotive_design', 1998, #12359 ) ;
#9607 = CARTESIAN_POINT ( 'NONE',  ( 17.95718847840442578, 0.4784641824370373109, 12.68786700119948208 ) ) ;
#9608 = CARTESIAN_POINT ( 'NONE',  ( 12.97447410014400226, -11.72278459482000024, -1.967342116188999679 ) ) ;
#9609 = CARTESIAN_POINT ( 'NONE',  ( 7.801010157780201126, 2.973106524567316278, 6.575014448996248539 ) ) ;
#9610 = CARTESIAN_POINT ( 'NONE',  ( 10.93990547754509812, 5.032986398992000510, -7.532784233952049213 ) ) ;
#9611 = ORIENTED_EDGE ( 'NONE', *, *, #67215, .T. ) ;
#9612 = CARTESIAN_POINT ( 'NONE',  ( 11.18706725482999964, -3.186788126275999833, 6.232699537089999353 ) ) ;
#9613 = EDGE_LOOP ( 'NONE', ( #8576, #85, #22098, #5763, #39661, #33629, #21717, #53218, #32869, #42767, #63276, #15 ) ) ;
#9614 = CARTESIAN_POINT ( 'NONE',  ( 8.506326034927656821, -3.199837828248755844, 6.012289131673731468 ) ) ;
#9615 = CARTESIAN_POINT ( 'NONE',  ( 9.278331853207999913, -5.791549888895000109, 7.752110689268000954 ) ) ;
#9616 = CARTESIAN_POINT ( 'NONE',  ( 15.78404792230800346, 8.744893293839998805, 7.778646260181000471 ) ) ;
#9617 = ORIENTED_EDGE ( 'NONE', *, *, #46115, .T. ) ;
#9618 = CARTESIAN_POINT ( 'NONE',  ( 23.58038622399895701, 10.23758691150733036, 9.527246697258645369 ) ) ;
#9619 = CARTESIAN_POINT ( 'NONE',  ( 7.965270188005331597, 3.582163548059296598, -6.202867177960278866 ) ) ;
#9620 = CARTESIAN_POINT ( 'NONE',  ( 8.070045280407001087, 2.564091104321999826, -6.530737592441999695 ) ) ;
#9621 = DIRECTION ( 'NONE',  ( -1.000000000000000000, 0.000000000000000000, 0.000000000000000000 ) ) ;
#9622 = CARTESIAN_POINT ( 'NONE',  ( 18.07108758008967442, -2.852736468728856778, 12.36237742789788641 ) ) ;
#9623 = EDGE_LOOP ( 'NONE', ( #1117, #23046, #11223, #23625, #7759 ) ) ;
#9624 = LINE ( 'NONE', #61406, #37656 ) ;
#9625 = CARTESIAN_POINT ( 'NONE',  ( 12.19454236345195852, -2.633904201044235727, -13.64409272160013487 ) ) ;
#9626 = CARTESIAN_POINT ( 'NONE',  ( 9.502599499754323276, -2.949662297526366661, 7.001638755957637628 ) ) ;
#9627 = ORIENTED_EDGE ( 'NONE', *, *, #3103, .T. ) ;
#9628 = CARTESIAN_POINT ( 'NONE',  ( 9.179055905797000037, 2.899999999999999911, 6.571291218949999902 ) ) ;
#9629 = B_SPLINE_CURVE_WITH_KNOTS ( 'NONE', 3,
 ( #29350, #23740, #7313, #39830, #61151 ),
 .UNSPECIFIED., .F., .F.,
 ( 4, 1, 4 ),
 ( 0.000000000000000000, 0.5000000000000000000, 1.000000000000000000 ),
 .UNSPECIFIED. ) ;
#9630 = CARTESIAN_POINT ( 'NONE',  ( 9.082700812465912321, 2.899999999999999911, -6.316220168737575413 ) ) ;
#9631 = ORIENTED_EDGE ( 'NONE', *, *, #17757, .T. ) ;
#9632 = CARTESIAN_POINT ( 'NONE',  ( 23.61278980179503151, -10.11611562016859445, 9.631329498146783408 ) ) ;
#9633 = CARTESIAN_POINT ( 'NONE',  ( 10.69357525437983725, 5.769078639290308175, 7.350227077746113835 ) ) ;
#9634 = CARTESIAN_POINT ( 'NONE',  ( 5.308543490071000015, 1.556797599500999940, -0.04728230666302999513 ) ) ;
#9635 = VECTOR ( 'NONE', #40658, 1000.000000000000114 ) ;
#9636 = CARTESIAN_POINT ( 'NONE',  ( 11.79999999742034511, -12.31348763297674331, -1.888274624276562896 ) ) ;
#9637 = DIRECTION ( 'NONE',  ( 1.000000000000000000, 0.000000000000000000, 0.000000000000000000 ) ) ;
#9638 = CARTESIAN_POINT ( 'NONE',  ( 7.881897435323000245, -5.128252730674000226, 6.737016898340999482 ) ) ;
#9639 = CARTESIAN_POINT ( 'NONE',  ( 12.78422293702843326, 3.124999446934218383, 13.52078617650838055 ) ) ;
#9640 = CARTESIAN_POINT ( 'NONE',  ( 8.455992358796999397, 5.100000000000000533, 6.571291218954000257 ) ) ;
#9641 = VERTEX_POINT ( 'NONE', #18513 ) ;
#9642 = CARTESIAN_POINT ( 'NONE',  ( 7.674540706797001732, -4.591334964886001124, 6.448517731106997886 ) ) ;
#9643 = EDGE_LOOP ( 'NONE', ( #60801, #5206, #17017, #32786 ) ) ;
#9644 = CARTESIAN_POINT ( 'NONE',  ( 9.532678149083000818, 4.663044775770000427, 8.669813205957000335 ) ) ;
#9645 = CARTESIAN_POINT ( 'NONE',  ( 23.60000000000000142, 0.000000000000000000, 0.000000000000000000 ) ) ;
#9646 = AXIS2_PLACEMENT_3D ( 'NONE', #1438, #11565, #39189 ) ;
#9647 = CARTESIAN_POINT ( 'NONE',  ( 12.23409240334733461, 2.245563803222850208, -13.72414218390522578 ) ) ;
#9648 = CARTESIAN_POINT ( 'NONE',  ( 2.593749284444999859, -1.508056830049999908, 3.206819776970000202 ) ) ;
#9649 = CARTESIAN_POINT ( 'NONE',  ( 25.47112285341500026, 2.702203117016999556, 11.27946744962999936 ) ) ;
#9650 = EDGE_CURVE ( 'NONE', #56347, #33649, #63270, .T. ) ;
#9651 = CARTESIAN_POINT ( 'NONE',  ( 8.082873386424997975, 5.111739203374999541, -6.679001318365999751 ) ) ;
#9652 = CARTESIAN_POINT ( 'NONE',  ( 9.576555093678434716, -2.247948244796866835, -7.800247541287225417 ) ) ;
#9653 = EDGE_LOOP ( 'NONE', ( #28500, #39028, #26519 ) ) ;
#9654 = EDGE_CURVE ( 'NONE', #36055, #66683, #19186, .T. ) ;
#9655 = CARTESIAN_POINT ( 'NONE',  ( 11.58425954179440076, -3.017023678917100327, 6.683254058608399717 ) ) ;
#9656 = CARTESIAN_POINT ( 'NONE',  ( 10.52204676658863391, 2.851933436354328499, -8.818745687284273771 ) ) ;
#9657 = FACE_OUTER_BOUND ( 'NONE', #41993, .T. ) ;
#9658 = CARTESIAN_POINT ( 'NONE',  ( 17.55505043854144276, 0.6250000000000001110, -12.67928921589118474 ) ) ;
#9660 = CARTESIAN_POINT ( 'NONE',  ( 8.100000113405998903, 12.39999890530000037, 0.000000000000000000 ) ) ;
#9659 = CARTESIAN_POINT ( 'NONE',  ( 11.04678944127999962, -5.235596213805000509, -5.039805523473999571 ) ) ;
#9661 = CARTESIAN_POINT ( 'NONE',  ( 10.99410672858429905, 3.198097575668700010, -6.896755974168000236 ) ) ;
#9662 = CARTESIAN_POINT ( 'NONE',  ( 14.46666666253433498, -8.815232490335725757, -7.616703758276854863 ) ) ;
#9663 = CARTESIAN_POINT ( 'NONE',  ( 9.121088727410999297, 3.136022381937999981, -7.572461161969050281 ) ) ;
#9664 = CARTESIAN_POINT ( 'NONE',  ( 17.55505043854144276, -0.6250000000000001110, 12.67928921589117586 ) ) ;
#9665 = CARTESIAN_POINT ( 'NONE',  ( 6.695576494045999638, -0.8862304417126000144, 0.8626632806168000878 ) ) ;
#9666 = CARTESIAN_POINT ( 'NONE',  ( 9.472537864290000442, -2.899999999999999911, -6.571291218949999902 ) ) ;
#9667 = CARTESIAN_POINT ( 'NONE',  ( 23.58444450794900149, 10.35808252348000025, 9.328052187805999651 ) ) ;
#9668 = EDGE_LOOP ( 'NONE', ( #57220, #67380, #19225, #7912 ) ) ;
#9669 = CARTESIAN_POINT ( 'NONE',  ( 7.577019353207000485, -5.480312458445999901, 8.192326492433998908 ) ) ;
#9670 = B_SPLINE_CURVE_WITH_KNOTS ( 'NONE', 3,
 ( #30520, #58117, #3928, #67910 ),
 .UNSPECIFIED., .F., .F.,
 ( 4, 4 ),
 ( 0.000000000000000000, 1.000000000000000000 ),
 .UNSPECIFIED. ) ;
#9671 = CARTESIAN_POINT ( 'NONE',  ( 4.000000000000000000, 2.149963194831999491, -0.2827069376517958310 ) ) ;
#9672 = CARTESIAN_POINT ( 'NONE',  ( 9.065735834902588053, 4.411345979885467727, 6.337235623390005124 ) ) ;
#9673 = ORIENTED_EDGE ( 'NONE', *, *, #162, .T. ) ;
#9674 = CIRCLE ( 'NONE', #4083, 13.98989063585999837 ) ;
#9675 = CARTESIAN_POINT ( 'NONE',  ( 0.1153984072571000025, -0.4897778999536001043, -3.171902824723000336 ) ) ;
#9676 = AXIS2_PLACEMENT_3D ( 'NONE', #40345, #19020, #18341 ) ;
#9677 = CARTESIAN_POINT ( 'NONE',  ( 11.26723293495529887, 2.826061044294000180, 7.547192037433419820 ) ) ;
#9678 = CARTESIAN_POINT ( 'NONE',  ( 9.978904719591000116, 5.007782080444000528, -8.772599239991000886 ) ) ;
#9679 = VERTEX_POINT ( 'NONE', #3441 ) ;
#9680 = ADVANCED_FACE ( 'NONE', ( #8017 ), #24778, .F. ) ;
#9681 = CARTESIAN_POINT ( 'NONE',  ( 8.623777853204000365, 5.100000000000000533, -6.534061169358333920 ) ) ;
#9682 = LINE ( 'NONE', #47799, #15249 ) ;
#9683 = CARTESIAN_POINT ( 'NONE',  ( 11.57656516821460890, 4.899536366368299589, 6.592171857671999646 ) ) ;
#9684 = CARTESIAN_POINT ( 'NONE',  ( 13.69999628573842543, -9.617752440245887158, -8.023770515523462876 ) ) ;
#9686 = CARTESIAN_POINT ( 'NONE',  ( 8.977760841230999489, 2.019067547072999957, 7.390982789861999969 ) ) ;
#9685 = AXIS2_PLACEMENT_3D ( 'NONE', #24663, #29928, #51908 ) ;
#9687 = VERTEX_POINT ( 'NONE', #39487 ) ;
#9688 = CARTESIAN_POINT ( 'NONE',  ( 8.751496707488000126, 4.081676005979390176, 6.643597378104299622 ) ) ;
#9689 = ADVANCED_FACE ( 'NONE', ( #19535 ), #34402, .T. ) ;
#9690 = ADVANCED_FACE ( 'NONE', ( #61157 ), #66031, .F. ) ;
#9691 = CARTESIAN_POINT ( 'NONE',  ( 7.467439158767000151, 3.394203523730999539, -9.300711568980998933 ) ) ;
#9692 = CARTESIAN_POINT ( 'NONE',  ( 8.093953312661190225, -4.429161490856333039, 5.814587964491527039 ) ) ;
#9693 = AXIS2_PLACEMENT_3D ( 'NONE', #19233, #56304, #35670 ) ;
#9694 = CARTESIAN_POINT ( 'NONE',  ( 10.28260887879199892, -4.289688213680199702, 8.745979585038000437 ) ) ;
#9695 = ORIENTED_EDGE ( 'NONE', *, *, #10872, .F. ) ;
#9696 = CARTESIAN_POINT ( 'NONE',  ( 10.37122190540000055, -4.584050552809999068, -5.010296351866999842 ) ) ;
#9697 = CARTESIAN_POINT ( 'NONE',  ( 10.67349413291699811, -2.837298848764000514, 8.030511425625498134 ) ) ;
#9698 = EDGE_LOOP ( 'NONE', ( #7573, #67176, #29673, #22140, #61349, #34525 ) ) ;
#9699 = CARTESIAN_POINT ( 'NONE',  ( 16.10005255078199937, -3.632778330393000132, -11.06917548872000090 ) ) ;
#9700 = CARTESIAN_POINT ( 'NONE',  ( 16.39999999231800132, -3.216285993016000155, -11.40340220863999932 ) ) ;
#9701 = ORIENTED_EDGE ( 'NONE', *, *, #2438, .T. ) ;
#9702 = CARTESIAN_POINT ( 'NONE',  ( 9.668897997121000287, -4.730747404809998891, -8.668230005597001409 ) ) ;
#9703 = CARTESIAN_POINT ( 'NONE',  ( 9.050000000000000711, 0.000000000000000000, -4.000000000000000000 ) ) ;
#9704 = CARTESIAN_POINT ( 'NONE',  ( 11.43856039236529831, 5.032284719763000069, -7.550239075043479353 ) ) ;
#9705 = CARTESIAN_POINT ( 'NONE',  ( 11.42968717260509948, -4.687649763627899979, 6.377637058250999580 ) ) ;
#9706 = CARTESIAN_POINT ( 'NONE',  ( 24.44496350777200178, -12.03536639536000052, -3.224849854974999985 ) ) ;
#9707 = CARTESIAN_POINT ( 'NONE',  ( 10.63662282008600002, -3.405288783432600219, 6.540749699823199315 ) ) ;
#9708 = CARTESIAN_POINT ( 'NONE',  ( 7.346670280409000497, 2.374037589774999901, 8.293392681990997772 ) ) ;
#9709 = EDGE_CURVE ( 'NONE', #47311, #50417, #35952, .T. ) ;
#9710 = VERTEX_POINT ( 'NONE', #58303 ) ;
#9711 = CARTESIAN_POINT ( 'NONE',  ( 3.500000000000000000, -3.033011252059000018, -1.020217008720000207 ) ) ;
#9712 = CARTESIAN_POINT ( 'NONE',  ( 8.545870559624999530, -3.856773448568000084, 5.521258396339000285 ) ) ;
#9713 = CARTESIAN_POINT ( 'NONE',  ( 9.958513540182876156, 3.836375382625530239, 6.250000000000000000 ) ) ;
#9714 = ORIENTED_EDGE ( 'NONE', *, *, #66043, .T. ) ;
#9715 = CARTESIAN_POINT ( 'NONE',  ( 12.27327344217068905, -2.829024202110182351, -12.36880877243790344 ) ) ;
#9716 = CARTESIAN_POINT ( 'NONE',  ( 7.245144510450004738, 10.37974071282999411, -4.936574216131997872 ) ) ;
#9717 = CARTESIAN_POINT ( 'NONE',  ( 17.57198699599700120, -11.81437355489000041, 3.324579570925000116 ) ) ;
#9718 = CARTESIAN_POINT ( 'NONE',  ( 23.61718184453616942, -13.40540285613228910, -3.918713763237630765 ) ) ;
#9719 = CARTESIAN_POINT ( 'NONE',  ( 12.39818000720382152, -2.025460462753591706, -13.76267819017275329 ) ) ;
#9720 = CARTESIAN_POINT ( 'NONE',  ( 10.29262282008599882, -3.548418513060800361, -8.228386593078399258 ) ) ;
#9721 = CARTESIAN_POINT ( 'NONE',  ( 24.34832118744133211, -3.224867653600234529, -12.03536993091778129 ) ) ;
#9722 = CARTESIAN_POINT ( 'NONE',  ( 8.498030440990834933, -5.100000000000000533, 6.489929440899814495 ) ) ;
#9723 = ORIENTED_EDGE ( 'NONE', *, *, #61622, .F. ) ;
#9724 = ORIENTED_EDGE ( 'NONE', *, *, #22195, .T. ) ;
#9725 = DIRECTION ( 'NONE',  ( 0.000000000000000000, -1.000000000000000000, 0.000000000000000000 ) ) ;
#9726 = CARTESIAN_POINT ( 'NONE',  ( 7.100000000000000533, 11.84999999999999964, 0.000000000000000000 ) ) ;
#9727 = DIRECTION ( 'NONE',  ( 1.000000000000000000, 0.000000000000000000, 0.000000000000000000 ) ) ;
#9728 = CARTESIAN_POINT ( 'NONE',  ( 10.51140238467000110, 2.326714339996000191, -7.741210149842999932 ) ) ;
#9729 = CARTESIAN_POINT ( 'NONE',  ( 8.664497909817340471, 5.045291088815394787, 6.188051271826346067 ) ) ;
#9730 = EDGE_CURVE ( 'NONE', #68446, #14991, #52022, .T. ) ;
#9731 =( GEOMETRIC_REPRESENTATION_CONTEXT ( 3 ) GLOBAL_UNCERTAINTY_ASSIGNED_CONTEXT ( ( #60943 ) ) GLOBAL_UNIT_ASSIGNED_CONTEXT ( ( #20656, #3537, #24531 ) ) REPRESENTATION_CONTEXT ( 'NONE', 'WORKASPACE' ) );
#9732 = CARTESIAN_POINT ( 'NONE',  ( 18.16381471383434487, 2.642962562933662163, 12.41712880859051893 ) ) ;
#9733 = CARTESIAN_POINT ( 'NONE',  ( 17.75883778089099962, 3.641526152925000037, -12.02434993381999995 ) ) ;
#9734 = CARTESIAN_POINT ( 'NONE',  ( 9.634020792350998619, 3.042978295541999945, 8.588098960242001922 ) ) ;
#9735 = ORIENTED_EDGE ( 'NONE', *, *, #28774, .T. ) ;
#9736 = EDGE_CURVE ( 'NONE', #65585, #63838, #26155, .T. ) ;
#9737 = VECTOR ( 'NONE', #34873, 1000.000000000000114 ) ;
#9738 = CARTESIAN_POINT ( 'NONE',  ( 9.127723954448535792, 2.415158738379607595, -6.695780460953873359 ) ) ;
#9739 = ORIENTED_EDGE ( 'NONE', *, *, #26547, .F. ) ;
#9740 = CARTESIAN_POINT ( 'NONE',  ( 12.55417570215098166, -3.072462724870960393, 12.29958987976102058 ) ) ;
#9741 = CARTESIAN_POINT ( 'NONE',  ( 9.551684229509998403, -4.611171355610000688, -6.885038603985500494 ) ) ;
#9742 = CARTESIAN_POINT ( 'NONE',  ( 10.72520610419000064, 5.521650664120000940, 6.612990918765000004 ) ) ;
#9743 = CARTESIAN_POINT ( 'NONE',  ( 11.55946005378019947, -2.963614890480000152, 8.053412743695298914 ) ) ;
#9744 = CARTESIAN_POINT ( 'NONE',  ( 5.399998984437000438, 12.99045401563999924, 1.690592933733000125 ) ) ;
#9745 = CIRCLE ( 'NONE', #48830, 1.449999999999999956 ) ;
#9746 = CARTESIAN_POINT ( 'NONE',  ( 24.52301487189109253, 8.782814486076295779, 8.926451907308345923 ) ) ;
#9747 = FACE_OUTER_BOUND ( 'NONE', #59032, .T. ) ;
#9748 = CARTESIAN_POINT ( 'NONE',  ( 12.30864223534304003, -0.3802890292809111283, 12.69234946364259287 ) ) ;
#9749 = CARTESIAN_POINT ( 'NONE',  ( 11.60000000000000142, 3.528833218773709035, -8.438845841270557813 ) ) ;
#9750 = CARTESIAN_POINT ( 'NONE',  ( 10.96291115433076868, 5.162911154333786889, -6.648309209566408917 ) ) ;
#9751 = AXIS2_PLACEMENT_3D ( 'NONE', #15238, #30985, #40771 ) ;
#9752 = CARTESIAN_POINT ( 'NONE',  ( 9.136334870123905105, -3.395591289844346328, 8.727132796763758193 ) ) ;
#9753 = ORIENTED_EDGE ( 'NONE', *, *, #61642, .T. ) ;
#9754 = CARTESIAN_POINT ( 'NONE',  ( 9.228345280414000484, 2.481540185810000132, -7.878707153279001396 ) ) ;
#9755 = DIRECTION ( 'NONE',  ( 0.000000000000000000, 1.000000000000000000, 0.000000000000000000 ) ) ;
#9756 = CYLINDRICAL_SURFACE ( 'NONE', #50575, 1.250000000000000222 ) ;
#9757 = CARTESIAN_POINT ( 'NONE',  ( 17.55505043854143921, -0.7302158263239086899, 13.98094363220831049 ) ) ;
#9758 = CARTESIAN_POINT ( 'NONE',  ( 12.09999999999999964, -4.640264089079229493, 8.191831084107846550 ) ) ;
#9759 = CARTESIAN_POINT ( 'NONE',  ( 11.35918179236250047, -4.238363971154499588, -6.384440618559000136 ) ) ;
#9760 = ORIENTED_EDGE ( 'NONE', *, *, #16089, .F. ) ;
#9761 = CARTESIAN_POINT ( 'NONE',  ( 2.397385296146999689, 3.036063727655999855, -1.493670828108000004 ) ) ;
#9762 = CARTESIAN_POINT ( 'NONE',  ( 7.822385841228999048, 4.636729845879000500, 9.378977473003999421 ) ) ;
#9764 = CARTESIAN_POINT ( 'NONE',  ( 13.73732479921000049, -9.700721122729000001, -7.982825098500999417 ) ) ;
#9763 = CARTESIAN_POINT ( 'NONE',  ( 4.999999999765999625, 0.04999999976595000117, -9.776630293088999224 ) ) ;
#9765 = FACE_OUTER_BOUND ( 'NONE', #51283, .T. ) ;
#9766 = ORIENTED_EDGE ( 'NONE', *, *, #31012, .T. ) ;
#9767 = CARTESIAN_POINT ( 'NONE',  ( 25.46372797112000086, -8.354608193938998895, 8.148457429720000533 ) ) ;
#9769 = CARTESIAN_POINT ( 'NONE',  ( 18.06966903239552735, -2.854820418091305712, -13.59172178685414245 ) ) ;
#9768 = B_SPLINE_CURVE_WITH_KNOTS ( 'NONE', 3,
 ( #68036, #19465, #14229, #3715, #40441, #67685, #9306, #40117, #19811, #50942, #18787, #66667, #7947, #14572, #57203, #29980, #4057, #25392, #20152, #61086, #29284, #24369, #50598, #2700, #45359 ),
 .UNSPECIFIED., .F., .F.,
 ( 4, 2, 2, 2, 2, 2, 2, 2, 2, 1, 2, 2, 4 ),
 ( 0.2955573413587750942, 0.4716680060191286161, 0.4936818391016731256, 0.5156956721842176350, 0.5597233383493066539, 0.6477786706794828042, 0.7358340030096590656, 0.7468409195509307930, 0.7523443778215666011, 0.7578478360922024093, 0.7798616691747313201, 0.8238893353397851449, 1.000000000000000000 ),
 .UNSPECIFIED. ) ;
#9770 = CARTESIAN_POINT ( 'NONE',  ( 10.75210807141120029, 4.040019166404060336, 6.634727177901499573 ) ) ;
#9771 = FACE_OUTER_BOUND ( 'NONE', #20522, .T. ) ;
#9772 = CARTESIAN_POINT ( 'NONE',  ( 9.143918146793000190, -5.791549888895000109, 7.752110689268000954 ) ) ;
#9773 = ORIENTED_EDGE ( 'NONE', *, *, #35829, .T. ) ;
#9774 = CARTESIAN_POINT ( 'NONE',  ( 7.518864158771000561, 3.206360348473000332, 5.681727837477000165 ) ) ;
#9775 = EDGE_CURVE ( 'NONE', #10227, #18501, #16974, .T. ) ;
#9776 = EDGE_CURVE ( 'NONE', #10297, #26251, #56704, .T. ) ;
#9778 = CARTESIAN_POINT ( 'NONE',  ( 10.91060805961999947, -4.702347118766000200, -9.210032991522000501 ) ) ;
#9777 = CARTESIAN_POINT ( 'NONE',  ( 11.01837338474678063, 3.735675910162961078, -6.666799917282374643 ) ) ;
#9779 = CARTESIAN_POINT ( 'NONE',  ( 7.495957138799123065, -2.535418675573966052, 6.532461274932616746 ) ) ;
#9780 = CARTESIAN_POINT ( 'NONE',  ( 17.96719322784330330, -0.4698824116306926091, 13.88931020049250087 ) ) ;
#9781 = CARTESIAN_POINT ( 'NONE',  ( 23.85292962156700014, 3.520417378894999949, 13.16609032570999993 ) ) ;
#9783 = ORIENTED_EDGE ( 'NONE', *, *, #15355, .T. ) ;
#9782 = B_SPLINE_CURVE_WITH_KNOTS ( 'NONE', 3,
 ( #24328, #57163, #45661, #66967, #40401, #19073, #61723, #13843, #29939, #51243, #24672, #25350, #67993, #45992, #62745, #67305, #19421, #30269 ),
 .UNSPECIFIED., .F., .F.,
 ( 4, 2, 2, 2, 2, 2, 2, 2, 4 ),
 ( 0.000000000000000000, 0.1250000000000000000, 0.2500000000000000000, 0.3750000000000000000, 0.5000000000000000000, 0.6250000000000000000, 0.7500000000000000000, 0.8750000000000000000, 1.000000000000000000 ),
 .UNSPECIFIED. ) ;
#9784 = CARTESIAN_POINT ( 'NONE',  ( 1.953914243537261619, -2.025123852575706707, 2.609090518642736889 ) ) ;
#9785 = CARTESIAN_POINT ( 'NONE',  ( 11.15364694612719809, -4.804498860841600383, 7.178938988280099132 ) ) ;
#9786 = CARTESIAN_POINT ( 'NONE',  ( 9.843732751558000871, 4.115124343450999866, 9.466620196856998959 ) ) ;
#9787 = CARTESIAN_POINT ( 'NONE',  ( 9.260906466624998501, 4.901388651757999426, 9.090324495507999814 ) ) ;
#9788 = STYLED_ITEM ( 'NONE', ( #21674 ), #5248 ) ;
#9789 = CARTESIAN_POINT ( 'NONE',  ( 10.28026357027499849, 4.985299147223100746, 7.309904858193100097 ) ) ;
#9790 = CARTESIAN_POINT ( 'NONE',  ( 23.94495401785119171, -3.343212669807313020, 12.85029054808020987 ) ) ;
#9791 = VECTOR ( 'NONE', #62313, 1000.000000000000114 ) ;
#9792 = CARTESIAN_POINT ( 'NONE',  ( 12.08521996405947974, 2.390121770085890329, -12.37125191860131324 ) ) ;
#9793 = CARTESIAN_POINT ( 'NONE',  ( 11.30361999289329766, 3.455907502640805262, -6.342116603374313044 ) ) ;
#9794 = EDGE_CURVE ( 'NONE', #34400, #14644, #42919, .T. ) ;
#9795 = DIRECTION ( 'NONE',  ( 0.000000000000000000, -0.2588190451024934835, 0.9659258262890757507 ) ) ;
#9796 = CIRCLE ( 'NONE', #52216, 0.3000000000000007105 ) ;
#9797 = CARTESIAN_POINT ( 'NONE',  ( 18.16658511877958659, -2.125673232124642986, 13.83768827471936547 ) ) ;
#9798 = CARTESIAN_POINT ( 'NONE',  ( 18.13153191398660624, 2.741475808336658382, -13.61927240697805175 ) ) ;
#9799 = ORIENTED_EDGE ( 'NONE', *, *, #20744, .T. ) ;
#9800 = CARTESIAN_POINT ( 'NONE',  ( 10.99664311227126312, 4.444039568019539033, 6.293666904468254941 ) ) ;
#9801 = ADVANCED_FACE ( 'NONE', ( #1303 ), #6189, .T. ) ;
#9802 = CARTESIAN_POINT ( 'NONE',  ( 9.232128830620874638, -4.207195853723359136, -6.256996123608767668 ) ) ;
#9803 = ORIENTED_EDGE ( 'NONE', *, *, #23440, .T. ) ;
#9804 = CARTESIAN_POINT ( 'NONE',  ( 10.27335506660999975, -4.750713325691999778, 4.596758554457999857 ) ) ;
#9805 = CARTESIAN_POINT ( 'NONE',  ( 11.19518313518939934, 3.462699341914400097, 6.820583637845799352 ) ) ;
#9806 = CARTESIAN_POINT ( 'NONE',  ( 10.74609776273999984, 4.263105564403999459, 9.276980853981999786 ) ) ;
#9807 = CARTESIAN_POINT ( 'NONE',  ( 10.00074698269999907, 2.373893144840999891, -7.962435130300000274 ) ) ;
#9808 = CARTESIAN_POINT ( 'NONE',  ( 10.28877584378239796, -3.533998264153197510, -8.236827240972795394 ) ) ;
#9809 = CARTESIAN_POINT ( 'NONE',  ( 10.02202195053999922, -3.298019507654999849, 5.700533868754000366 ) ) ;
#9810 = CARTESIAN_POINT ( 'NONE',  ( 18.22055608408779648, -0.2856017019952077352, -12.59676745213710447 ) ) ;
#9811 = AXIS2_PLACEMENT_3D ( 'NONE', #53204, #64360, #27679 ) ;
#9812 = CARTESIAN_POINT ( 'NONE',  ( 4.805026506350000837, 1.500000000000000000, 0.000000000000000000 ) ) ;
#9813 = CARTESIAN_POINT ( 'NONE',  ( 10.45257053952200010, -4.394359323863099576, -6.577269499510100204 ) ) ;
#9814 = CARTESIAN_POINT ( 'NONE',  ( 10.90454231406000041, -5.099691312770999296, -5.130383474399000221 ) ) ;
#9815 = ORIENTED_EDGE ( 'NONE', *, *, #60490, .T. ) ;
#9816 = B_SPLINE_CURVE_WITH_KNOTS ( 'NONE', 3,
 ( #2055, #22328, #16736, #60091, #49596 ),
 .UNSPECIFIED., .F., .F.,
 ( 4, 1, 4 ),
 ( 0.000000000000000000, 0.5000000000000000000, 1.000000000000000000 ),
 .UNSPECIFIED. ) ;
#9817 = CARTESIAN_POINT ( 'NONE',  ( 11.09999999999999964, 4.000000000000000000, 7.500000000000000000 ) ) ;
#9818 = CARTESIAN_POINT ( 'NONE',  ( 8.957462135714999718, 5.100000000000000533, -6.571291218949999902 ) ) ;
#9819 = DIRECTION ( 'NONE',  ( 0.000000000000000000, -0.9127899773906427150, -0.4084292560226189250 ) ) ;
#9820 = CARTESIAN_POINT ( 'NONE',  ( 17.88934697238257243, 1.841816770035708872, 12.46465977041040141 ) ) ;
#9821 = CARTESIAN_POINT ( 'NONE',  ( 12.45019282332726185, 3.154806840457482053, 13.63991304855491649 ) ) ;
#9822 = CARTESIAN_POINT ( 'NONE',  ( 9.632185590920999019, -5.638162562978999759, 6.476633609657000079 ) ) ;
#9823 = EDGE_CURVE ( 'NONE', #60343, #11189, #616, .T. ) ;
#9824 = CARTESIAN_POINT ( 'NONE',  ( 12.41737000014478376, -0.4903651762333725017, -12.68725775796614741 ) ) ;
#9825 = CARTESIAN_POINT ( 'NONE',  ( 12.25981791760051465, -0.4818816852691660824, 13.99171642476389721 ) ) ;
#9826 = ORIENTED_EDGE ( 'NONE', *, *, #40923, .F. ) ;
#9827 = CARTESIAN_POINT ( 'NONE',  ( 24.41456973790700147, 8.821771448540999927, 8.767658430047001517 ) ) ;
#9828 = CARTESIAN_POINT ( 'NONE',  ( 10.31558376188599802, -4.962881317320600338, -8.113672563022399586 ) ) ;
#9829 = CARTESIAN_POINT ( 'NONE',  ( 8.200000304434999165, 12.49999969551000056, -3.568532357647000425E-10 ) ) ;
#9830 = CARTESIAN_POINT ( 'NONE',  ( 9.972852379787999766, -5.044471434015000533, 6.258101649750000384 ) ) ;
#9831 = CARTESIAN_POINT ( 'NONE',  ( 16.09996065438095414, 9.056490835163806707, 8.652417574211018092 ) ) ;
#9832 = CARTESIAN_POINT ( 'NONE',  ( 12.13825819896753977, -4.851203879749700576, 7.339530235223699073 ) ) ;
#9833 = CARTESIAN_POINT ( 'NONE',  ( 8.705449068729999240, 3.636021264089499994, 6.712833982956899703 ) ) ;
#9834 = CARTESIAN_POINT ( 'NONE',  ( 23.66004879239100234, 9.998910715289998308, -9.691527791130999603 ) ) ;
#9835 = B_SPLINE_CURVE_WITH_KNOTS ( 'NONE', 3,
 ( #43641, #48190, #48883, #59710 ),
 .UNSPECIFIED., .F., .F.,
 ( 4, 4 ),
 ( 0.000000000000000000, 1.000000000000000000 ),
 .UNSPECIFIED. ) ;
#9836 = B_SPLINE_CURVE_WITH_KNOTS ( 'NONE', 3,
 ( #42340, #52820, #68536, #58742 ),
 .UNSPECIFIED., .F., .F.,
 ( 4, 4 ),
 ( 0.000000000000000000, 1.000000000000000000 ),
 .UNSPECIFIED. ) ;
#9837 = CARTESIAN_POINT ( 'NONE',  ( 11.40000717739000002, 3.090860900556000105E-13, -1.000866056699999936E-13 ) ) ;
#9838 = VECTOR ( 'NONE', #65464, 1000.000000000000227 ) ;
#9839 = CARTESIAN_POINT ( 'NONE',  ( 12.40831127361655462, 1.878029834076329951, 12.45925554172551486 ) ) ;
#9840 = DIRECTION ( 'NONE',  ( 0.000000000000000000, 0.9840640231862776144, 0.1778145052306959739 ) ) ;
#9841 = CARTESIAN_POINT ( 'NONE',  ( 10.92026088462129962, 4.002135146349410810, -6.496532863517000322 ) ) ;
#9842 = CARTESIAN_POINT ( 'NONE',  ( 7.805976048735002948, 2.918573024645998881, -6.499545638216004839 ) ) ;
#9843 = CARTESIAN_POINT ( 'NONE',  ( 11.01605778040999972, 5.482856203356999636, -7.846408531951999166 ) ) ;
#9844 = CARTESIAN_POINT ( 'NONE',  ( 9.326684229509998758, 3.098260518542999886, -6.592668585875199661 ) ) ;
#9846 = CARTESIAN_POINT ( 'NONE',  ( 18.05195279573837297, -0.3792326064291314247, 12.69238213821911643 ) ) ;
#9845 = CARTESIAN_POINT ( 'NONE',  ( 9.991933421518185199, 4.976296783332229801, 8.591994908148388177 ) ) ;
#9847 = LINE ( 'NONE', #58429, #60950 ) ;
#9848 = ORIENTED_EDGE ( 'NONE', *, *, #63517, .F. ) ;
#9849 = CIRCLE ( 'NONE', #33267, 0.5000000000000000000 ) ;
#9850 = CARTESIAN_POINT ( 'NONE',  ( 12.24304070173655390, -0.2736148577199287724, 12.69603606445621402 ) ) ;
#9851 = CARTESIAN_POINT ( 'NONE',  ( 10.25851354018279160, 4.163624617374472869, 8.749999999999996447 ) ) ;
#9852 = CARTESIAN_POINT ( 'NONE',  ( 10.50286331871000023, -5.158900740613000302, 8.369962360110999811 ) ) ;
#9853 = CARTESIAN_POINT ( 'NONE',  ( 9.249747021775998945, 3.245052836381700168, 6.837506920432799618 ) ) ;
#9854 = VECTOR ( 'NONE', #49171, 999.9999999999998863 ) ;
#9855 = CARTESIAN_POINT ( 'NONE',  ( 23.58931645927405896, -3.186881233604905272, -13.61284225936185166 ) ) ;
#9856 = CARTESIAN_POINT ( 'NONE',  ( 12.21305109721492066, -2.701423549395647328, 13.62869161905334181 ) ) ;
#9857 = CARTESIAN_POINT ( 'NONE',  ( 12.25785601946420478, 2.186712656649328235, 13.73518136001305479 ) ) ;
#9858 = CARTESIAN_POINT ( 'NONE',  ( 9.523148997461001741, -5.167567567567999731, -6.822293592207000934 ) ) ;
#9859 = ORIENTED_EDGE ( 'NONE', *, *, #50008, .T. ) ;
#9860 = EDGE_CURVE ( 'NONE', #11941, #17206, #23678, .T. ) ;
#9861 = EDGE_CURVE ( 'NONE', #59329, #9965, #18735, .T. ) ;
#9862 = CARTESIAN_POINT ( 'NONE',  ( 5.150632654315000281, 1.274863079208999883, -0.03871952724233999887 ) ) ;
#9863 = CARTESIAN_POINT ( 'NONE',  ( 9.250696787962999323, -3.780328739572700325, -6.239790126677999815 ) ) ;
#9864 = CARTESIAN_POINT ( 'NONE',  ( 17.92913687513156873, -3.216295279492283665, 11.40344415250781118 ) ) ;
#9865 = CARTESIAN_POINT ( 'NONE',  ( 11.14902344389989963, -4.883530143601199747, 8.036199780531900316 ) ) ;
#9866 = B_SPLINE_CURVE_WITH_KNOTS ( 'NONE', 3,
 ( #22506, #11671, #5738, #33010 ),
 .UNSPECIFIED., .F., .F.,
 ( 4, 4 ),
 ( 0.5000000000000298650, 1.000000000000000000 ),
 .UNSPECIFIED. ) ;
#9867 = CARTESIAN_POINT ( 'NONE',  ( 17.77721830936820879, 3.084271799839128914, -12.29605728393571873 ) ) ;
#9868 = CARTESIAN_POINT ( 'NONE',  ( 9.640654977342496323, -2.950420301507454379, 8.197403194024859729 ) ) ;
#9869 = CARTESIAN_POINT ( 'NONE',  ( 7.100000000000000533, 0.000000000000000000, 0.000000000000000000 ) ) ;
#9870 = CARTESIAN_POINT ( 'NONE',  ( 17.55505043854143565, 3.248147246781390329, 13.61798588129781074 ) ) ;
#9871 = CARTESIAN_POINT ( 'NONE',  ( 10.95383834890000152, -2.844912728619000131, -5.168232267893999143 ) ) ;
#9872 = CARTESIAN_POINT ( 'NONE',  ( 11.02419555961999897, -2.407899345275000158, -8.439548421502999886 ) ) ;
#9873 = CARTESIAN_POINT ( 'NONE',  ( 9.090964864865910045, -3.294502121218175983, 8.704449896995548386 ) ) ;
#9874 = CARTESIAN_POINT ( 'NONE',  ( 12.17712534909926170, 0.3652063536484317918, -13.99523956222174448 ) ) ;
#9875 = CARTESIAN_POINT ( 'NONE',  ( 17.55505043854143565, 3.199698446519375850, 12.18695736643652694 ) ) ;
#9876 = CARTESIAN_POINT ( 'NONE',  ( 24.39664237511399847, -8.810499461477174776, 8.810499461443630054 ) ) ;
#9877 = CARTESIAN_POINT ( 'NONE',  ( 9.087099331641999456, -5.286372936495260966, -7.026974105800379178 ) ) ;
#9878 = ADVANCED_FACE ( 'NONE', ( #22277 ), #28222, .T. ) ;
#9879 = B_SPLINE_CURVE_WITH_KNOTS ( 'NONE', 3,
 ( #3970, #2021, #35471, #8891 ),
 .UNSPECIFIED., .F., .F.,
 ( 4, 4 ),
 ( 0.000000000000000000, 1.000000000000000000 ),
 .UNSPECIFIED. ) ;
#9880 = EDGE_LOOP ( 'NONE', ( #31444, #34198, #47144, #16840 ) ) ;
#9881 = CARTESIAN_POINT ( 'NONE',  ( 9.450870280412999591, 2.928319778732999978, -8.861178115809998701 ) ) ;
#9882 = CARTESIAN_POINT ( 'NONE',  ( 12.25718044953559982, -3.110233631466100324, 7.036033215662999218 ) ) ;
#9883 = ORIENTED_EDGE ( 'NONE', *, *, #68032, .F. ) ;
#9884 = CYLINDRICAL_SURFACE ( 'NONE', #27283, 0.4999999999999998335 ) ;
#9885 = CARTESIAN_POINT ( 'NONE',  ( 18.13175260058826055, 2.961013189755318908, -13.68330200419957166 ) ) ;
#9886 = ORIENTED_EDGE ( 'NONE', *, *, #58007, .T. ) ;
#9887 = EDGE_CURVE ( 'NONE', #64134, #57964, #20327, .T. ) ;
#9888 = CARTESIAN_POINT ( 'NONE',  ( 11.13746005378019888, 5.161099018038999731, 8.120007936598501175 ) ) ;
#9889 = CARTESIAN_POINT ( 'NONE',  ( 8.497235841230001085, 3.789127741898000057, -9.388182174781999123 ) ) ;
#9890 = AXIS2_PLACEMENT_3D ( 'NONE', #21407, #4296, #4987 ) ;
#9891 = CARTESIAN_POINT ( 'NONE',  ( 11.08810207955139937, 3.203462856645999945, 7.825000000000000178 ) ) ;
#9892 = CARTESIAN_POINT ( 'NONE',  ( 10.48791429142999831, -3.983006558652820051, -6.608036045330599961 ) ) ;
#9893 = CARTESIAN_POINT ( 'NONE',  ( 12.18105065344216165, 0.04081304491956393166, -13.89993877190634564 ) ) ;
#9894 = CARTESIAN_POINT ( 'NONE',  ( 24.14470172087083455, 9.246870630047478556, -9.586744156808173045 ) ) ;
#9895 = CONICAL_SURFACE ( 'NONE', #7651, 0.9346783463124002100, 0.7853981908209605178 ) ;
#9896 = CARTESIAN_POINT ( 'NONE',  ( 12.99229341877100019, 11.49414526569999850, 1.652619848542000058 ) ) ;
#9897 = ORIENTED_EDGE ( 'NONE', *, *, #22389, .F. ) ;
#9898 = CARTESIAN_POINT ( 'NONE',  ( 14.03986884071600016, 9.265369649631999494, 8.206962993589000277 ) ) ;
#9899 = B_SPLINE_CURVE_WITH_KNOTS ( 'NONE', 3,
 ( #36067, #29817, #41657, #66849, #8813, #35730, #18963, #30156, #19995, #15089, #40622, #51122, #57382, #61954, #36413, #40289, #14068, #35392 ),
 .UNSPECIFIED., .F., .F.,
 ( 4, 2, 2, 2, 2, 2, 2, 2, 4 ),
 ( 0.1254918003289636208, 0.2191362172194401547, 0.3127806341099167442, 0.4064250510003932781, 0.5000694678908698121, 0.5937138847813465681, 0.6873583016718234351, 0.7810027185623000801, 0.8746471354527769471 ),
 .UNSPECIFIED. ) ;
#9900 = CARTESIAN_POINT ( 'NONE',  ( 9.327795280414001411, 3.161445734422999809, -6.178649910536000434 ) ) ;
#9901 = ORIENTED_EDGE ( 'NONE', *, *, #9887, .F. ) ;
#9902 = CARTESIAN_POINT ( 'NONE',  ( 10.91624242361999997, 5.459834480072999874, -8.642877574935999618 ) ) ;
#9903 = EDGE_LOOP ( 'NONE', ( #12999, #34948, #61448, #14604, #30563, #9389, #62828, #67746, #19544, #30818, #3185, #63526, #28765, #31204, #58648, #3972, #17854 ) ) ;
#9904 = CARTESIAN_POINT ( 'NONE',  ( 8.566809814040999171, 4.782507962695600412, 6.488038963273999649 ) ) ;
#9905 = CARTESIAN_POINT ( 'NONE',  ( 17.85706045311523127, -3.134356930968903665, -12.20392612899626528 ) ) ;
#9906 = DIRECTION ( 'NONE',  ( 1.000000000000000000, 0.000000000000000000, 0.000000000000000000 ) ) ;
#9907 = DIRECTION ( 'NONE',  ( 1.000000000000000000, 0.000000000000000000, 0.000000000000000000 ) ) ;
#9908 = LINE ( 'NONE', #58148, #40408 ) ;
#9909 = ORIENTED_EDGE ( 'NONE', *, *, #53656, .T. ) ;
#9910 = CARTESIAN_POINT ( 'NONE',  ( 12.69408977940800121, 11.93156085714000092, -3.263088413970000268 ) ) ;
#9911 = CARTESIAN_POINT ( 'NONE',  ( 17.89937390468400125, 11.46460001353999836, -4.648225426428999718 ) ) ;
#9912 = AXIS2_PLACEMENT_3D ( 'NONE', #4135, #62526, #41894 ) ;
#9913 = CARTESIAN_POINT ( 'NONE',  ( 7.924878289113923557, -5.349357204871147076, 7.500005630225521358 ) ) ;
#9914 = FACE_OUTER_BOUND ( 'NONE', #68233, .T. ) ;
#9915 = CARTESIAN_POINT ( 'NONE',  ( 8.367589158771000513, 5.461114003844000031, -8.582501063019000398 ) ) ;
#9916 = CARTESIAN_POINT ( 'NONE',  ( 18.44717847589300064, -2.901259342162000543, 12.12894967335999930 ) ) ;
#9917 = CARTESIAN_POINT ( 'NONE',  ( 10.44807121817999906, -3.684978196963999864, -6.173109031625999776 ) ) ;
#9918 = ADVANCED_FACE ( 'NONE', ( #11101 ), #38011, .T. ) ;
#9919 = EDGE_CURVE ( 'NONE', #54460, #35032, #23204, .T. ) ;
#9920 = ORIENTED_EDGE ( 'NONE', *, *, #49256, .F. ) ;
#9921 = ORIENTED_EDGE ( 'NONE', *, *, #13363, .F. ) ;
#9922 = CARTESIAN_POINT ( 'NONE',  ( 8.970860841232001448, 4.131080973160000447, -6.108642999115999395 ) ) ;
#9923 = DIRECTION ( 'NONE',  ( 0.000000000000000000, 1.000000000000000000, 0.000000000000000000 ) ) ;
#9924 = CARTESIAN_POINT ( 'NONE',  ( 1.300973465874000201, -3.500000000000000000, 0.000000000000000000 ) ) ;
#9925 = CARTESIAN_POINT ( 'NONE',  ( 25.27035628967400172, 8.566978069849998434, -7.889731756040999855 ) ) ;
#9926 = CARTESIAN_POINT ( 'NONE',  ( 10.55569598648999907, 5.130952141044000214, -8.173387776112500447 ) ) ;
#9927 = CARTESIAN_POINT ( 'NONE',  ( 9.839304848515999069, 4.788504886021700102, -7.860510733857099197 ) ) ;
#9929 = CARTESIAN_POINT ( 'NONE',  ( 8.878099260413335969, 2.921496745512210058, 8.876672705295140631 ) ) ;
#9928 = CARTESIAN_POINT ( 'NONE',  ( 10.78824205624999877, -4.360201998293100623, 6.562398383267799673 ) ) ;
#9930 = CARTESIAN_POINT ( 'NONE',  ( 7.411085905969002852, -3.233236485764999113, 6.481842843012996624 ) ) ;
#9931 = VERTEX_POINT ( 'NONE', #48857 ) ;
#9932 = CARTESIAN_POINT ( 'NONE',  ( 8.883148997460001084, 5.167567567567999731, 6.822293592207000934 ) ) ;
#9933 = CARTESIAN_POINT ( 'NONE',  ( 7.666438387056996540, -3.213133027605000525, 6.349775630263004622 ) ) ;
#9934 = CARTESIAN_POINT ( 'NONE',  ( 9.624896294737000702, -5.235394649229000663, -8.110359502241001550 ) ) ;
#9935 = LINE ( 'NONE', #63055, #21316 ) ;
#9936 = AXIS2_PLACEMENT_3D ( 'NONE', #47542, #20966, #63604 ) ;
#9937 = CARTESIAN_POINT ( 'NONE',  ( 10.06343867337000120, -5.156226070197000411, 6.125223053176999777 ) ) ;
#9938 = CARTESIAN_POINT ( 'NONE',  ( 18.15933590956319321, 2.660621712302206454, -12.41273490623410858 ) ) ;
#9939 = DIRECTION ( 'NONE',  ( 1.000000000000000000, 0.000000000000000000, 0.000000000000000000 ) ) ;
#9940 = EDGE_CURVE ( 'NONE', #35088, #10760, #11167, .T. ) ;
#9941 = EDGE_CURVE ( 'NONE', #63357, #44911, #24307, .T. ) ;
#9942 = DIRECTION ( 'NONE',  ( -1.000000000000000000, 0.000000000000000000, 0.000000000000000000 ) ) ;
#9943 = CARTESIAN_POINT ( 'NONE',  ( 7.995237948509533510, 3.187523905036820704, -6.308808669286300130 ) ) ;
#9944 = CARTESIAN_POINT ( 'NONE',  ( 9.788646554150998824, -3.580250267348600079, -8.258629096756299859 ) ) ;
#9945 = EDGE_CURVE ( 'NONE', #17206, #48127, #5344, .T. ) ;
#9946 = CARTESIAN_POINT ( 'NONE',  ( 10.93559687351661580, -5.092232985442824322, 6.870476274536375882 ) ) ;
#9947 = CARTESIAN_POINT ( 'NONE',  ( 21.60000000000000142, 0.000000000000000000, 0.000000000000000000 ) ) ;
#9948 = CARTESIAN_POINT ( 'NONE',  ( 5.500000000000000000, 12.87590651766999983, -2.791353855799999728 ) ) ;
#9949 = CARTESIAN_POINT ( 'NONE',  ( 3.544158303137000310, -1.635632129023999903, -3.009968172588000535 ) ) ;
#9950 = EDGE_LOOP ( 'NONE', ( #35019, #24666 ) ) ;
#9951 = CARTESIAN_POINT ( 'NONE',  ( 12.37753504985973940, 0.4560270868711863157, -12.68898073362801071 ) ) ;
#9952 = CARTESIAN_POINT ( 'NONE',  ( 12.27854653042187039, -2.836954440265831767, -12.36664979425283839 ) ) ;
#9953 = CARTESIAN_POINT ( 'NONE',  ( 7.000000000000000000, 0.000000000000000000, 0.000000000000000000 ) ) ;
#9954 = DIRECTION ( 'NONE',  ( 0.000000000000000000, 1.000000000000000000, 0.000000000000000000 ) ) ;
#9955 = CARTESIAN_POINT ( 'NONE',  ( 12.09999999999999964, -2.750000000000000000, 7.500000000000000000 ) ) ;
#9956 = ORIENTED_EDGE ( 'NONE', *, *, #44943, .F. ) ;
#9957 = CARTESIAN_POINT ( 'NONE',  ( 9.584226531641581559, -2.899999999999999911, 6.304440313841762844 ) ) ;
#9958 = DIRECTION ( 'NONE',  ( 1.000000000000000000, 0.000000000000000000, 0.000000000000000000 ) ) ;
#9959 = CARTESIAN_POINT ( 'NONE',  ( 10.88834686957638631, 2.694378745199484282, -7.104278543674602098 ) ) ;
#9960 = CARTESIAN_POINT ( 'NONE',  ( 13.44051303026600053, -11.61511980691000012, -2.065108503055999911 ) ) ;
#9961 = CARTESIAN_POINT ( 'NONE',  ( 7.771669714201605572, 2.830702833142050512, -8.205313987515433283 ) ) ;
#9962 = CARTESIAN_POINT ( 'NONE',  ( 10.73724174883999893, 3.975468761016990094, -8.391788556008700439 ) ) ;
#9963 = ORIENTED_EDGE ( 'NONE', *, *, #24084, .F. ) ;
#9964 = CARTESIAN_POINT ( 'NONE',  ( 10.35616740164000049, -2.777283710737999733, 8.995265811011998736 ) ) ;
#9965 = VERTEX_POINT ( 'NONE', #39402 ) ;
#9966 = EDGE_CURVE ( 'NONE', #36211, #62671, #42006, .T. ) ;
#9967 = DIRECTION ( 'NONE',  ( 0.000000000000000000, -0.8648648648648717963, 0.5020047465136829867 ) ) ;
#9968 = CARTESIAN_POINT ( 'NONE',  ( 9.342519353207999089, -5.057079407184000175, 8.967634647348999621 ) ) ;
#9969 = FACE_OUTER_BOUND ( 'NONE', #28768, .T. ) ;
#9970 = ORIENTED_EDGE ( 'NONE', *, *, #29481, .F. ) ;
#9971 = CARTESIAN_POINT ( 'NONE',  ( 23.60854598900385781, 10.12895705728418960, 9.621631069965385308 ) ) ;
#9972 = CARTESIAN_POINT ( 'NONE',  ( 6.944089158771000747, 3.609683333014999995, -6.158094852492999927 ) ) ;
#9973 = CARTESIAN_POINT ( 'NONE',  ( 20.75138802851920161, 0.000000000000000000, 0.000000000000000000 ) ) ;
#9974 = CARTESIAN_POINT ( 'NONE',  ( 12.80505043854146940, -3.125000000000000000, 13.52084414783465860 ) ) ;
#9975 = EDGE_LOOP ( 'NONE', ( #65606, #32788, #9760, #45834 ) ) ;
#9976 = CARTESIAN_POINT ( 'NONE',  ( 10.43579701286999928, -2.587605342384000195, 6.390039770907999461 ) ) ;
#9977 = CARTESIAN_POINT ( 'NONE',  ( 11.59999999999999609, 4.988477031107064086, 8.147838400233640144 ) ) ;
#9978 = DIRECTION ( 'NONE',  ( -1.000000000000000000, 0.000000000000000000, 0.000000000000000000 ) ) ;
#9979 = ORIENTED_EDGE ( 'NONE', *, *, #44597, .F. ) ;
#9980 = DIRECTION ( 'NONE',  ( 1.077198146790999955E-09, 7.359447821342999600E-11, 1.000000000000000000 ) ) ;
#9981 = ORIENTED_EDGE ( 'NONE', *, *, #56990, .T. ) ;
#9982 = LINE ( 'NONE', #183, #62188 ) ;
#9983 = CARTESIAN_POINT ( 'NONE',  ( 10.85378311793296469, 3.372467802742289411, 9.158846416527032019 ) ) ;
#9984 = CARTESIAN_POINT ( 'NONE',  ( 4.966446267845999962, -0.5822046538191000264, 1.444608038638999892 ) ) ;
#9985 = CARTESIAN_POINT ( 'NONE',  ( 5.157109839683540642, -1.199500263597270022, -0.9218200799623730290 ) ) ;
#9986 = CARTESIAN_POINT ( 'NONE',  ( 8.013720397008766483, 5.129092373936881444, -6.745135665648876788 ) ) ;
#9987 = DIRECTION ( 'NONE',  ( 1.000000000000000000, 0.000000000000000000, 0.000000000000000000 ) ) ;
#9988 = CARTESIAN_POINT ( 'NONE',  ( 12.66131753640901714, 3.108595072584060315, 13.52531149670803501 ) ) ;
#9989 = CARTESIAN_POINT ( 'NONE',  ( 9.959635380193999410, -5.406637819064000539, 7.700301345050000634 ) ) ;
#9990 = ORIENTED_EDGE ( 'NONE', *, *, #25501, .T. ) ;
#9991 = FACE_OUTER_BOUND ( 'NONE', #53822, .T. ) ;
#9992 = ORIENTED_EDGE ( 'NONE', *, *, #66046, .T. ) ;
#9993 = CARTESIAN_POINT ( 'NONE',  ( 11.14994211610999919, 2.627136771666999771, 6.696094414592000277 ) ) ;
#9994 = CARTESIAN_POINT ( 'NONE',  ( 10.98768553379999879, -5.299329486732999861, 4.945210549701000602 ) ) ;
#9995 = FACE_OUTER_BOUND ( 'NONE', #65288, .T. ) ;
#9996 = CARTESIAN_POINT ( 'NONE',  ( 3.306337663562000095, -0.1082433060725999929, -3.542063228793999485 ) ) ;
#9997 = DIRECTION ( 'NONE',  ( 1.000000000000000000, 0.000000000000000000, 0.000000000000000000 ) ) ;
#9998 = CARTESIAN_POINT ( 'NONE',  ( 10.46029575260939026, 4.828733415692241238, -8.253465265694869046 ) ) ;
#9999 = CARTESIAN_POINT ( 'NONE',  ( 9.324996057314875131, -5.719375876571866968, -7.175980490421300040 ) ) ;
#10000 = EDGE_CURVE ( 'NONE', #35196, #65063, #62059, .T. ) ;
#10001 = EDGE_CURVE ( 'NONE', #35521, #31036, #49555, .T. ) ;
#10002 = ORIENTED_EDGE ( 'NONE', *, *, #13586, .F. ) ;
#10003 = CARTESIAN_POINT ( 'NONE',  ( 12.72336452611786051, 0.6199804606742643776, 13.88138355690256276 ) ) ;
#10004 = CARTESIAN_POINT ( 'NONE',  ( 10.87041638348499895, -5.241705141469999774, 7.802464414828100381 ) ) ;
#10005 = CARTESIAN_POINT ( 'NONE',  ( 10.49760649485983954, 3.288391178207342502, -9.127049713605428494 ) ) ;
#10006 = CARTESIAN_POINT ( 'NONE',  ( 15.37415039705200215, 9.132871822554998076, 8.217191491449000296 ) ) ;
#10007 = CARTESIAN_POINT ( 'NONE',  ( 7.218293146793000048, -4.773080213113000347, 8.927399220053999329 ) ) ;
#10008 = VECTOR ( 'NONE', #12991, 1000.000000000000000 ) ;
#10010 = CARTESIAN_POINT ( 'NONE',  ( 12.43804048110095017, 3.154843637346236740, -13.63995574168323266 ) ) ;
#10009 = CARTESIAN_POINT ( 'NONE',  ( 11.02786554143000153, 5.596226216413000110, 7.209502215883999199 ) ) ;
#10011 = CARTESIAN_POINT ( 'NONE',  ( 11.47810404293059960, 3.436653965247300047, -8.647151967355000579 ) ) ;
#10012 = CARTESIAN_POINT ( 'NONE',  ( 25.19966571366900254, -11.70908055238000145, 2.905889386239000061 ) ) ;
#10013 = CARTESIAN_POINT ( 'NONE',  ( 8.971126402771000485, 4.939810497841199854, -7.145601175474399547 ) ) ;
#10014 = CARTESIAN_POINT ( 'NONE',  ( 18.28003407448206730, -0.02395120399003650841, 12.59999907117300033 ) ) ;
#10015 = CARTESIAN_POINT ( 'NONE',  ( 7.136881816240999932, -1.205895524350000025, 0.6847492370762000569 ) ) ;
#10016 = CARTESIAN_POINT ( 'NONE',  ( 10.98768472633000037, -6.720753151621999599, -5.471698430863999540 ) ) ;
#10017 = CARTESIAN_POINT ( 'NONE',  ( 23.51705919471800144, 10.50857783028999926, 9.449538485383000008 ) ) ;
#10018 = VERTEX_POINT ( 'NONE', #55135 ) ;
#10019 = CARTESIAN_POINT ( 'NONE',  ( 7.326308059621999824, -3.394845988290999816, 9.388942682504000103 ) ) ;
#10020 = CARTESIAN_POINT ( 'NONE',  ( 8.225464158772000545, 3.844886277615000125, -8.888911790991000927 ) ) ;
#10021 = B_SPLINE_CURVE_WITH_KNOTS ( 'NONE', 3,
 ( #46561, #57040, #45870, #56362 ),
 .UNSPECIFIED., .F., .F.,
 ( 4, 4 ),
 ( 0.000000000000000000, 1.000000000000000000 ),
 .UNSPECIFIED. ) ;
#10022 = DIRECTION ( 'NONE',  ( -1.000000000000000000, 0.000000000000000000, 0.000000000000000000 ) ) ;
#10023 = FACE_OUTER_BOUND ( 'NONE', #27442, .T. ) ;
#10024 = ORIENTED_EDGE ( 'NONE', *, *, #51714, .T. ) ;
#10025 = EDGE_CURVE ( 'NONE', #49363, #20272, #7238, .T. ) ;
#10026 = DIRECTION ( 'NONE',  ( 0.000000000000000000, -0.8764402124317022258, 0.4815106998112011483 ) ) ;
#10027 = CARTESIAN_POINT ( 'NONE',  ( 11.14256920625030034, 4.042230905578960254, 8.674127893687000324 ) ) ;
#10028 = CARTESIAN_POINT ( 'NONE',  ( 10.14522028041000112, 3.576529456695000331, -8.962721799438000403 ) ) ;
#10029 = VERTEX_POINT ( 'NONE', #18080 ) ;
#10030 = CARTESIAN_POINT ( 'NONE',  ( 12.75734966356159994, -0.7181168112306600682, -12.57951960855069551 ) ) ;
#10031 = CYLINDRICAL_SURFACE ( 'NONE', #14160, 0.4999999999999998335 ) ;
#10032 = CARTESIAN_POINT ( 'NONE',  ( 10.34580110216399973, 2.909301855364999856, 8.166103548914600552 ) ) ;
#10033 = CARTESIAN_POINT ( 'NONE',  ( 24.30000564797063234, -12.09374148493534840, 3.240508264358131107 ) ) ;
#10034 = CARTESIAN_POINT ( 'NONE',  ( 7.218295280410000458, 4.773081973066999772, 8.927402469597002010 ) ) ;
#10035 = ORIENTED_EDGE ( 'NONE', *, *, #56935, .F. ) ;
#10036 = CARTESIAN_POINT ( 'NONE',  ( 0.1499996298882999846, 0.000000000000000000, -2.250000000000000000 ) ) ;
#10037 = CARTESIAN_POINT ( 'NONE',  ( 6.870739158771000277, 5.477119873501999692, -8.694708770948999188 ) ) ;
#10038 = CARTESIAN_POINT ( 'NONE',  ( 8.151588397734400360, -5.460081713051196495, 6.513119554412222456 ) ) ;
#10039 = CARTESIAN_POINT ( 'NONE',  ( 9.651392757687000667, -3.229293331742300044, 6.657535947657399866 ) ) ;
#10040 = ORIENTED_EDGE ( 'NONE', *, *, #28810, .F. ) ;
#10041 = CARTESIAN_POINT ( 'NONE',  ( 16.13854985688900001, -3.352851047014000052, -11.81842075147999971 ) ) ;
#10042 = B_SPLINE_CURVE_WITH_KNOTS ( 'NONE', 3,
 ( #522, #59937, #54698, #32009 ),
 .UNSPECIFIED., .F., .F.,
 ( 4, 4 ),
 ( 0.000000000000000000, 1.000000000000000000 ),
 .UNSPECIFIED. ) ;
#10043 = CARTESIAN_POINT ( 'NONE',  ( 11.31919037786000182, 11.76444917719000038, 1.692529869092999961 ) ) ;
#10044 = ORIENTED_EDGE ( 'NONE', *, *, #21080, .T. ) ;
#10045 = EDGE_CURVE ( 'NONE', #39230, #46950, #43747, .T. ) ;
#10046 = CARTESIAN_POINT ( 'NONE',  ( 9.457462135716001583, 5.100000000000000533, -6.571291218949999902 ) ) ;
#10047 = CARTESIAN_POINT ( 'NONE',  ( 7.000000000000000000, 10.80467228076000019, -3.475853456584999890 ) ) ;
#10048 = EDGE_LOOP ( 'NONE', ( #26734, #68870, #49326, #66479, #56771, #37347, #29267, #68258 ) ) ;
#10049 = CARTESIAN_POINT ( 'NONE',  ( 17.75641289383300148, 0.5920240553917505144, -13.88302649426327307 ) ) ;
#10050 = B_SPLINE_CURVE_WITH_KNOTS ( 'NONE', 3,
 ( #45388, #66699, #18821, #40146, #30343, #69106, #47446, #4090, #19843, #31370, #31713, #42542 ),
 .UNSPECIFIED., .F., .F.,
 ( 4, 2, 1, 1, 2, 2, 4 ),
 ( 0.000000000000000000, 0.2500000000000195954, 0.3750000000000261458, 0.4375000000000285327, 0.4687500000000288103, 0.5000000000000290878, 1.000000000000000000 ),
 .UNSPECIFIED. ) ;
#10051 = CARTESIAN_POINT ( 'NONE',  ( 9.507558421712998253, -4.699533657262000119, -6.366989705700999203 ) ) ;
#10052 = CARTESIAN_POINT ( 'NONE',  ( 2.300973465875999935, -3.500000000000000000, 0.000000000000000000 ) ) ;
#10053 = CARTESIAN_POINT ( 'NONE',  ( 10.56080513895999928, 5.026880838510000338, -6.929150654994399083 ) ) ;
#10054 = CARTESIAN_POINT ( 'NONE',  ( 12.01656039236534923, -2.826501801118000312, 7.442888368925779652 ) ) ;
#10055 = CARTESIAN_POINT ( 'NONE',  ( 4.000000000000000000, 0.000000000000000000, 0.000000000000000000 ) ) ;
#10056 = CARTESIAN_POINT ( 'NONE',  ( 11.41610672858429965, -4.911600290708499905, 8.185766014210599906 ) ) ;
#10057 = CARTESIAN_POINT ( 'NONE',  ( 8.283079719592000956, 2.376526778640999815, 7.686980884243000745 ) ) ;
#10058 = VERTEX_POINT ( 'NONE', #23321 ) ;
#10059 = VECTOR ( 'NONE', #31397, 1000.000000000000000 ) ;
#10060 = DIRECTION ( 'NONE',  ( 1.000000000000000000, 0.000000000000000000, 0.000000000000000000 ) ) ;
#10061 = CARTESIAN_POINT ( 'NONE',  ( 18.00096484318083867, -0.5748214922774377289, 12.58705572532630157 ) ) ;
#10062 = LINE ( 'NONE', #14628, #10059 ) ;
#10063 = EDGE_LOOP ( 'NONE', ( #16335, #66900, #60267, #60210, #69133, #48590, #29114, #4596 ) ) ;
#10064 = B_SPLINE_SURFACE_WITH_KNOTS ( 'NONE', 1, 3, ( 
 ( #6374, #54274, #22114, #16182, #1147, #32960, #64404, #10940, #11973, #42418, #37168, #48004, #38545, #16870, #54628, #53592, #43459, #63725, #32285, #43102, #5350, #27030, #11620, #22456, #64752, #28065, #15837, #21766, #38193, #59524, #27724, #58488, #49038, #59179, #43801, #65096, #37508, #37854, #449, #16528, #17220, #10592, #31934, #49374, #6724, #5688, #48343, #58832, #21092, #53244, #26689, #103, #11278, #32618, #53929, #21420, #6032, #42757, #27370, #48696, #797, #24193, #7772, #45530, #54976, #56011, #49728, #60566, #45184, #44504, #60910, #29464, #29808, #28767, #66840, #2187, #18612, #17924, #39587, #29113, #50419, #7075, #61258, #2522, #18951, #40280 ),
 ( #55674, #61597, #2864, #50080, #35043, #50770, #34700, #1490, #39241, #23849, #39940, #44155, #13028, #22805, #8118, #17574, #38902, #23501, #65453, #44842, #13375, #60223, #66148, #23155, #12327, #13714, #56358, #8463, #66491, #65798, #33658, #28415, #18266, #12674, #1838, #34005, #55323, #7418, #34354, #46896, #20666, #14404, #52130, #24541, #40962, #3887, #35383, #57037, #41645, #31173, #25571, #58073, #45866, #51790, #68199, #20318, #62952, #67175, #15074, #19986, #9139, #9825, #4232, #62616, #62285, #36400, #57717, #57371, #52476, #63299, #51451, #36753, #4573, #25910, #46212, #67863, #30475, #25222, #47241, #19289, #40614, #10176, #68544, #35720, #46558, #24882 ) ),
 .UNSPECIFIED., .F., .F., .F.,
 ( 2, 2 ),
 ( 4, 2, 2, 2, 2, 2, 2, 2, 2, 2, 2, 2, 2, 2, 2, 2, 2, 2, 2, 2, 2, 2, 2, 2, 2, 2, 2, 2, 2, 2, 2, 2, 2, 2, 2, 2, 2, 2, 2, 2, 2, 2, 4 ),
 ( 0.000000000000000000, 1.000000000000000000 ),
 ( 0.000000000000000000, 7.083094307561015621E-05, 0.0001416618861512203124, 0.0002124928292268304822, 0.0002833237723024406248, 0.0003541547153780508217, 0.0004249856584536609643, 0.0004958166015292711070, 0.0005666475446048812497, 0.0006374784876804913923, 0.0007083094307561016434, 0.0007791403738317117860, 0.0008145558453695168032, 0.0008499713169073219287, 0.0008853867884451270542, 0.0009208022599829320714, 0.0009916332030585422140, 0.001027048674596347340, 0.001062464146134152465, 0.001097879617671957374, 0.001133295089209762499, 0.001204126032285372534, 0.001239541503823177659, 0.001274956975360982785, 0.001310372446898787910, 0.001345787918436593036, 0.001416618861512203287, 0.001487449804587813538, 0.001522865276125618447, 0.001558280747663423572, 0.001629111690739033606, 0.001699942633814643857, 0.001735358105352448983, 0.001770773576890254108, 0.001806189048428059017, 0.001841604519965864143, 0.001912435463041474177, 0.001983266406117084428, 0.002018681877654889337, 0.002054097349192694679, 0.002124928292268304930, 0.002195759235343914748, 0.002266590178419524999 ),
 .UNSPECIFIED. ) ;
#10065 = CARTESIAN_POINT ( 'NONE',  ( 12.67305101672403822, -1.772831636685044066, -12.47465725448102170 ) ) ;
#10066 = CARTESIAN_POINT ( 'NONE',  ( 9.670777473741994257, 8.576669611614002875, -6.497511528403997261 ) ) ;
#10067 = LINE ( 'NONE', #4465, #40502 ) ;
#10068 = LINE ( 'NONE', #270, #10698 ) ;
#10069 = CARTESIAN_POINT ( 'NONE',  ( 12.61244651655888838, -1.905326457160024356, -13.78169738549997447 ) ) ;
#10070 = CARTESIAN_POINT ( 'NONE',  ( 11.21564426047340035, -3.460037133261700149, -8.345807871442598724 ) ) ;
#10071 = FACE_OUTER_BOUND ( 'NONE', #6345, .T. ) ;
#10072 = CARTESIAN_POINT ( 'NONE',  ( 18.20615948710265286, -2.797893282243149038, 12.28544817418252677 ) ) ;
#10073 = EDGE_LOOP ( 'NONE', ( #54784, #316, #23502, #60287, #40505, #66136, #64191, #36110, #66770, #28147 ) ) ;
#10074 = ORIENTED_EDGE ( 'NONE', *, *, #53898, .T. ) ;
#10075 = DIRECTION ( 'NONE',  ( 0.000000000000000000, 0.000000000000000000, 1.000000000000000000 ) ) ;
#10076 = CARTESIAN_POINT ( 'NONE',  ( 11.83830977893730463, -4.976598135215292373, 8.326430086672809594 ) ) ;
#10077 = CARTESIAN_POINT ( 'NONE',  ( 4.900006121741999898, -2.000000000000000444, 0.2617993877991496299 ) ) ;
#10078 = CARTESIAN_POINT ( 'NONE',  ( 9.898128230592000421, 2.965931985296999862, -6.610871072364999712 ) ) ;
#10079 = CARTESIAN_POINT ( 'NONE',  ( 18.28771814374053761, 2.987295517884132501, -11.95930540589378488 ) ) ;
#10080 = CARTESIAN_POINT ( 'NONE',  ( 17.63823367518480367, 3.119790641614041959, 12.28531617466518355 ) ) ;
#10081 = CARTESIAN_POINT ( 'NONE',  ( 8.335548758400999958, 2.897657723982001166, -6.653323589456997311 ) ) ;
#10082 = ADVANCED_FACE ( 'NONE', ( #29269 ), #50580, .F. ) ;
#10084 = EDGE_CURVE ( 'NONE', #63350, #7311, #61204, .T. ) ;
#10083 = CARTESIAN_POINT ( 'NONE',  ( 17.55505043854147118, -3.199698446519375850, -12.18695736643652694 ) ) ;
#10085 = VERTEX_POINT ( 'NONE', #26421 ) ;
#10086 = CARTESIAN_POINT ( 'NONE',  ( 8.930139513018188424, 4.760571299603993722, -9.106213216995776349 ) ) ;
#10087 = EDGE_CURVE ( 'NONE', #58209, #46886, #24551, .T. ) ;
#10088 = EDGE_CURVE ( 'NONE', #59692, #33837, #22056, .T. ) ;
#10089 = VERTEX_POINT ( 'NONE', #20135 ) ;
#10090 = CARTESIAN_POINT ( 'NONE',  ( 12.76336819523230126, -3.123957167202323859, 12.28406425424631898 ) ) ;
#10091 = CARTESIAN_POINT ( 'NONE',  ( 9.450367640780999778, -3.591293244209800228, -6.735364967924099666 ) ) ;
#10092 = CARTESIAN_POINT ( 'NONE',  ( 10.50244247011999832, 2.268911387573000038, 7.824865741583000300 ) ) ;
#10093 = CARTESIAN_POINT ( 'NONE',  ( 12.09603632436369125, -4.842640371965599932, 7.696781148700499564 ) ) ;
#10094 = CARTESIAN_POINT ( 'NONE',  ( 10.01508584123000034, 4.845406482350000488, -6.387189183984999907 ) ) ;
#10095 = CARTESIAN_POINT ( 'NONE',  ( 11.04779087299999851, 9.995284108896999697, -5.683129190753000159 ) ) ;
#10096 = CARTESIAN_POINT ( 'NONE',  ( 24.67559749782400047, 8.698784986637999594, 9.015141820286999064 ) ) ;
#10097 = AXIS2_PLACEMENT_3D ( 'NONE', #21308, #4876, #47199 ) ;
#10098 = CARTESIAN_POINT ( 'NONE',  ( 12.51886017880454816, -0.5557204214162426714, 12.68363025601216520 ) ) ;
#10099 = CARTESIAN_POINT ( 'NONE',  ( 11.60000000000000320, 4.924024592270518141, -8.335607184109882439 ) ) ;
#10100 = CARTESIAN_POINT ( 'NONE',  ( 10.75109581085999899, 2.822145500011000063, 6.655897464539000552 ) ) ;
#10101 = CARTESIAN_POINT ( 'NONE',  ( 9.160381251338680642, -3.070110540811217703, 8.479443955494096130 ) ) ;
#10102 = ORIENTED_EDGE ( 'NONE', *, *, #51141, .F. ) ;
#10103 = CARTESIAN_POINT ( 'NONE',  ( 8.548770280408998445, 5.203550244299999683, -8.391678825488000371 ) ) ;
#10104 = CARTESIAN_POINT ( 'NONE',  ( 0.000000000000000000, 0.3800960799355100339, 2.899897457380500310 ) ) ;
#10105 = ADVANCED_FACE ( 'NONE', ( #20822 ), #33244, .T. ) ;
#10106 = CARTESIAN_POINT ( 'NONE',  ( 17.59662294266145466, 1.876036575741765189, 13.78611707749647763 ) ) ;
#10107 = LINE ( 'NONE', #63924, #50778 ) ;
#10108 =( REPRESENTATION_RELATIONSHIP ('NONE','NONE', #10823, #19687 ) REPRESENTATION_RELATIONSHIP_WITH_TRANSFORMATION ( #58883 )SHAPE_REPRESENTATION_RELATIONSHIP( ) );
#10109 = CARTESIAN_POINT ( 'NONE',  ( 10.26059687351566652, 3.370476274536378547, -6.407767014557177454 ) ) ;
#10110 = VECTOR ( 'NONE', #57146, 1000.000000000000114 ) ;
#10111 = B_SPLINE_CURVE_WITH_KNOTS ( 'NONE', 3,
 ( #50400, #29439, #23824, #40254 ),
 .UNSPECIFIED., .F., .F.,
 ( 4, 4 ),
 ( 0.000000000000000000, 1.000000000000000000 ),
 .UNSPECIFIED. ) ;
#10112 = CARTESIAN_POINT ( 'NONE',  ( 11.30995122972050027, -3.547233695387300045, -6.452959986593999275 ) ) ;
#10113 = VERTEX_POINT ( 'NONE', #68359 ) ;
#10114 = CARTESIAN_POINT ( 'NONE',  ( 15.96647867633516427, -8.895858221259741683, -8.626805212950843682 ) ) ;
#10115 = CARTESIAN_POINT ( 'NONE',  ( 7.501448341228000416, 2.138190256467000339, 6.814770510101999967 ) ) ;
#10118 = CARTESIAN_POINT ( 'NONE',  ( 11.25950692870000047, 3.811441498709999820, -11.68087307222999982 ) ) ;
#10117 = CARTESIAN_POINT ( 'NONE',  ( 8.623264158775000965, 5.288433695693000480, -8.041290150997999930 ) ) ;
#10116 = UNCERTAINTY_MEASURE_WITH_UNIT (LENGTH_MEASURE( 1.000000000000000082E-05 ), #20568, 'distance_accuracy_value', 'NONE');
#10119 = CARTESIAN_POINT ( 'NONE',  ( 18.16762906240597530, -2.624018810214523434, 13.64637396502913269 ) ) ;
#10120 = ORIENTED_EDGE ( 'NONE', *, *, #60053, .F. ) ;
#10121 = CARTESIAN_POINT ( 'NONE',  ( 11.01776904286000125, 4.914120883409999863, 8.587704221454000475 ) ) ;
#10122 = CARTESIAN_POINT ( 'NONE',  ( 17.83426395974178291, -1.940453161589465791, -13.77628863228519229 ) ) ;
#10123 = CARTESIAN_POINT ( 'NONE',  ( 11.53979707368350027, 3.569730287184500472, 8.251775607861899786 ) ) ;
#10124 = CARTESIAN_POINT ( 'NONE',  ( -15.86200481174999943, -2.399999999999999911, 6.571291218949999902 ) ) ;
#10125 = CARTESIAN_POINT ( 'NONE',  ( 8.283081853209001366, -2.376522687267000222, 7.686981355459999499 ) ) ;
#10126 = ORIENTED_EDGE ( 'NONE', *, *, #10950, .F. ) ;
#10127 = CARTESIAN_POINT ( 'NONE',  ( 8.379704719592000473, 4.283000592898000392, 9.286795422009001655 ) ) ;
#10129 = LINE ( 'NONE', #35678, #13946 ) ;
#10128 = CARTESIAN_POINT ( 'NONE',  ( 9.957462135714001406, 5.100000000000000533, -6.571291218949999902 ) ) ;
#10130 = CARTESIAN_POINT ( 'NONE',  ( 7.472002294636990172, -2.326570465340251026, 7.022491050036767213 ) ) ;
#10131 = CARTESIAN_POINT ( 'NONE',  ( 11.59999999999999964, 3.116215992411100366, -7.825000000000000178 ) ) ;
#10132 = CARTESIAN_POINT ( 'NONE',  ( 24.08756693569399943, 3.426422008827000099, 12.66862219457000016 ) ) ;
#10133 = EDGE_LOOP ( 'NONE', ( #1897, #43445, #5477, #46828, #29204 ) ) ;
#10134 = CARTESIAN_POINT ( 'NONE',  ( 5.834193173016667622, 1.460959015002474048, -0.3926218265389178064 ) ) ;
#10135 = CARTESIAN_POINT ( 'NONE',  ( 11.59256785386839894, -4.832509746210599921, 6.939751505745099358 ) ) ;
#10136 = FACE_OUTER_BOUND ( 'NONE', #64724, .T. ) ;
#10137 = CARTESIAN_POINT ( 'NONE',  ( 10.13339736671999880, 5.653645990693000556, 6.501823474484000442 ) ) ;
#10138 = EDGE_CURVE ( 'NONE', #41410, #13264, #9288, .T. ) ;
#10139 = CARTESIAN_POINT ( 'NONE',  ( 11.62994988689359843, 4.518136976474400157, 6.483720595741000459 ) ) ;
#10140 = ORIENTED_EDGE ( 'NONE', *, *, #6731, .T. ) ;
#10141 = CARTESIAN_POINT ( 'NONE',  ( 23.71152327822508354, -3.235048976924307595, 13.31086256645365928 ) ) ;
#10142 = EDGE_CURVE ( 'NONE', #7391, #17504, #25377, .T. ) ;
#10143 = CARTESIAN_POINT ( 'NONE',  ( 12.07997135281818579, 2.506142839463715521, -12.34827158344147868 ) ) ;
#10144 = CARTESIAN_POINT ( 'NONE',  ( 12.21922412107039868, -3.930460928605089777, 8.814426450544999625 ) ) ;
#10145 = B_SPLINE_CURVE_WITH_KNOTS ( 'NONE', 3,
 ( #52469, #25904, #10506, #15759, #42671, #37087, #4914, #52821, #68887, #52122, #15420 ),
 .UNSPECIFIED., .F., .F.,
 ( 4, 2, 1, 2, 2, 4 ),
 ( 0.000000000000000000, 0.2499999999999993339, 0.3749999999999968359, 0.4374999999999955591, 0.4999999999999942824, 1.000000000000000000 ),
 .UNSPECIFIED. ) ;
#10146 = CARTESIAN_POINT ( 'NONE',  ( 24.98214466478799878, -3.089315488182000191, -11.61702660961000078 ) ) ;
#10147 = CARTESIAN_POINT ( 'NONE',  ( 18.12530810765561640, -2.066994332627602571, 13.84657437950017744 ) ) ;
#10148 = CARTESIAN_POINT ( 'NONE',  ( 18.02549019385832096, 2.911978589154019748, -13.57741733930033590 ) ) ;
#10149 = ORIENTED_EDGE ( 'NONE', *, *, #52872, .F. ) ;
#10150 = DIRECTION ( 'NONE',  ( 0.000000000000000000, 1.000000000000000000, 0.000000000000000000 ) ) ;
#10151 = DIRECTION ( 'NONE',  ( 1.654177832420999993E-10, 1.654177150564999918E-10, 1.000000000000000000 ) ) ;
#10153 = VERTEX_POINT ( 'NONE', #30632 ) ;
#10152 = AXIS2_PLACEMENT_3D ( 'NONE', #46804, #62863, #26510 ) ;
#10154 = CARTESIAN_POINT ( 'NONE',  ( 9.364763540183330903, 2.782534154164605589, 7.172815144550902744 ) ) ;
#10155 = CARTESIAN_POINT ( 'NONE',  ( 11.49056651104150006, 4.085456792591960706, 8.361971998931499783 ) ) ;
#10156 = CARTESIAN_POINT ( 'NONE',  ( 10.58728840301827923, -2.899999999999999911, -6.305985889763610963 ) ) ;
#10157 = CARTESIAN_POINT ( 'NONE',  ( 11.15192953222999961, 2.359300361215999953, -6.636686939130999718 ) ) ;
#10158 = CARTESIAN_POINT ( 'NONE',  ( 8.757986382567201744, -3.848432872973398755, -8.349715092260979077 ) ) ;
#10159 = CARTESIAN_POINT ( 'NONE',  ( 10.39106278671000005, -4.025320977579999848, 9.261121875182000807 ) ) ;
#10160 = CARTESIAN_POINT ( 'NONE',  ( 18.02507753857510764, 0.4124490627810463161, -12.69099791225217189 ) ) ;
#10161 = VECTOR ( 'NONE', #50186, 1000.000000000000000 ) ;
#10162 = CARTESIAN_POINT ( 'NONE',  ( 12.25778805736141841, 2.802014929491043471, -12.37607946563925942 ) ) ;
#10163 = CARTESIAN_POINT ( 'NONE',  ( 11.69559063708295987, -2.913481137622000006, -7.805482129094999166 ) ) ;
#10165 = CARTESIAN_POINT ( 'NONE',  ( 7.700045280408999382, 3.346262376537000094, 6.002251090845000192 ) ) ;
#10164 = B_SPLINE_CURVE_WITH_KNOTS ( 'NONE', 3,
 ( #40470, #9681, #14598, #40145 ),
 .UNSPECIFIED., .F., .F.,
 ( 4, 4 ),
 ( 0.000000000000000000, 1.000000000000000000 ),
 .UNSPECIFIED. ) ;
#10167 = ORIENTED_EDGE ( 'NONE', *, *, #63027, .F. ) ;
#10166 = B_SPLINE_CURVE_WITH_KNOTS ( 'NONE', 3,
 ( #12658, #2509, #7757, #49714, #59852, #66132, #60551, #32946, #33990, #44138 ),
 .UNSPECIFIED., .F., .F.,
 ( 4, 2, 2, 2, 4 ),
 ( 0.000000000000000000, 0.2168912282584224416, 0.4337824565168448832, 0.6506736847752673247, 0.8675649130336897663 ),
 .UNSPECIFIED. ) ;
#10168 = DIRECTION ( 'NONE',  ( -1.000000000000000000, 0.000000000000000000, 0.000000000000000000 ) ) ;
#10169 = CARTESIAN_POINT ( 'NONE',  ( 9.239025325185552973, 2.669691822737871423, 7.269879417777145747 ) ) ;
#10170 = CARTESIAN_POINT ( 'NONE',  ( 11.79999998109721204, -11.63601885445003248, -1.847750289993327133 ) ) ;
#10171 = CARTESIAN_POINT ( 'NONE',  ( 8.962855452004999890, 10.45518530739999896, 4.395433839652001851 ) ) ;
#10172 = CARTESIAN_POINT ( 'NONE',  ( 11.36663496983795874, -3.844885926410422705, 11.78015091829274752 ) ) ;
#10173 = DIRECTION ( 'NONE',  ( -1.000000000000000000, 0.000000000000000000, 0.000000000000000000 ) ) ;
#10174 = LINE ( 'NONE', #41990, #56020 ) ;
#10175 = ADVANCED_FACE ( 'NONE', ( #40769 ), #4729, .F. ) ;
#10176 = CARTESIAN_POINT ( 'NONE',  ( 12.68688508614694044, -0.7208442004938080405, 13.98143072948223953 ) ) ;
#10177 = ADVANCED_FACE ( 'NONE', ( #31666 ), #46714, .F. ) ;
#10178 = VERTEX_POINT ( 'NONE', #15236 ) ;
#10179 = CARTESIAN_POINT ( 'NONE',  ( 24.36453968238300050, 8.917854847619999248, 9.043337665091998545 ) ) ;
#10180 = CARTESIAN_POINT ( 'NONE',  ( 9.152455549953000258, -3.004437130344999929, -6.696732323226999739 ) ) ;
#10181 = CARTESIAN_POINT ( 'NONE',  ( 12.80505043854143388, 1.845938772038641318, -13.81933890150171074 ) ) ;
#10182 = CARTESIAN_POINT ( 'NONE',  ( 11.15982711745999900, -5.578228817597000955, 8.067792329320999656 ) ) ;
#10183 = CARTESIAN_POINT ( 'NONE',  ( 11.57210672858429845, -4.692204557952299737, 8.020722037455799480 ) ) ;
#10184 = CARTESIAN_POINT ( 'NONE',  ( 12.50564389185357683, 0.6551943188411649688, 12.58295456804123091 ) ) ;
#10185 = CARTESIAN_POINT ( 'NONE',  ( 0.4829009740474999868, -3.219656052487999798, -1.007448552055000057 ) ) ;
#10186 = CARTESIAN_POINT ( 'NONE',  ( 25.29987333571600061, -10.83443035398000021, -3.855530949778000149 ) ) ;
#10187 = CARTESIAN_POINT ( 'NONE',  ( 12.22840029456386723, 2.917071392396657803, 12.25769309035714727 ) ) ;
#10188 = CARTESIAN_POINT ( 'NONE',  ( 9.397313405920000307, -4.010297355695000121, -9.208122400763999238 ) ) ;
#10189 = CARTESIAN_POINT ( 'NONE',  ( 11.16641369783139837, 3.949373449607799902, -8.502191501283999031 ) ) ;
#10190 = CARTESIAN_POINT ( 'NONE',  ( 12.52002425203523650, 12.10842255864620753, -3.203403679956843941 ) ) ;
#10191 = CARTESIAN_POINT ( 'NONE',  ( 10.20607971959000082, 2.622352165399999713, -6.528536464360000124 ) ) ;
#10192 = ADVANCED_FACE ( 'NONE', ( #36560 ), #57885, .F. ) ;
#10193 = CARTESIAN_POINT ( 'NONE',  ( 9.883925467520999320, 2.723846966067000164, -7.411581555133209598 ) ) ;
#10195 = CARTESIAN_POINT ( 'NONE',  ( 10.90145065189000029, -2.900000000488999863, 5.151029872614000027 ) ) ;
#10194 = DIRECTION ( 'NONE',  ( 0.000000000000000000, -0.9549051095262108824, 0.2969111513580035000 ) ) ;
#10196 = CARTESIAN_POINT ( 'NONE',  ( 25.44993984453400060, 11.77655473258999841, 4.190794510628000680 ) ) ;
#10197 = ORIENTED_EDGE ( 'NONE', *, *, #52103, .F. ) ;
#10198 = CARTESIAN_POINT ( 'NONE',  ( 12.27345231316480678, 0.3288522286145963980, 12.69427358703447695 ) ) ;
#10199 = CARTESIAN_POINT ( 'NONE',  ( 23.73953418927302650, -9.827640250138356848, 9.725489356616225933 ) ) ;
#10200 = CARTESIAN_POINT ( 'NONE',  ( 9.595408426582343608, 2.229238661835026392, -7.375658712783358162 ) ) ;
#10201 = CARTESIAN_POINT ( 'NONE',  ( 9.931621437244999129, 4.575883738927100097, 8.148124882831599081 ) ) ;
#10202 = DIRECTION ( 'NONE',  ( 0.000000000000000000, -1.000000000000000000, 0.000000000000000000 ) ) ;
#10203 = CARTESIAN_POINT ( 'NONE',  ( 12.27908368890585322, -2.837770472453527315, 13.59599796867854593 ) ) ;
#10204 = CARTESIAN_POINT ( 'NONE',  ( 23.57792053481616534, -3.138450412106891463, 13.63071449664701085 ) ) ;
#10205 = CARTESIAN_POINT ( 'NONE',  ( 23.58664969842400083, 3.018451562790000153, -13.60679499663999970 ) ) ;
#10206 = EDGE_LOOP ( 'NONE', ( #45351, #40761, #58544, #9269 ) ) ;
#10207 = CARTESIAN_POINT ( 'NONE',  ( 5.219052098759999758, 0.8613139015395000486, 0.9406969777927000065 ) ) ;
#10208 = CARTESIAN_POINT ( 'NONE',  ( 8.946747021775999897, -4.961496216383199709, -8.343747244947598674 ) ) ;
#10209 = CARTESIAN_POINT ( 'NONE',  ( 4.400000000000000355, 1.266759534686000110, 0.8033182938792000627 ) ) ;
#10210 = CARTESIAN_POINT ( 'NONE',  ( 11.69434208742519843, -4.478858766422799675, 6.747282993577999655 ) ) ;
#10211 = CARTESIAN_POINT ( 'NONE',  ( 18.01290626049236820, 2.925915981747411632, -12.34209597222820776 ) ) ;
#10212 = CARTESIAN_POINT ( 'NONE',  ( 9.711801307670127059, -3.888124047000113048, 8.755178286007271993 ) ) ;
#10213 = CARTESIAN_POINT ( 'NONE',  ( 18.16637421239960659, 2.630058152923315351, 12.42030992595579697 ) ) ;
#10214 = AXIS2_PLACEMENT_3D ( 'NONE', #63274, #15404, #36729 ) ;
#10215 = CARTESIAN_POINT ( 'NONE',  ( 8.040182825300005831, 3.147885656133000420, 6.175979896252004053 ) ) ;
#10216 = LINE ( 'NONE', #68587, #69193 ) ;
#10217 = CARTESIAN_POINT ( 'NONE',  ( 10.98633305961999973, -3.015090804604000141, -9.064432363387998848 ) ) ;
#10218 = ADVANCED_FACE ( 'NONE', ( #8955 ), #54815, .T. ) ;
#10219 = CARTESIAN_POINT ( 'NONE',  ( 24.53429011008099891, 3.614318944477000084, -12.31267538233000103 ) ) ;
#10220 = CARTESIAN_POINT ( 'NONE',  ( 3.500000000000000000, 0.000000000000000000, 0.000000000000000000 ) ) ;
#10221 = CARTESIAN_POINT ( 'NONE',  ( 10.45746213570999927, -5.100000000000000533, -6.571291218949999902 ) ) ;
#10222 = CARTESIAN_POINT ( 'NONE',  ( 8.999999001754000361, -12.50000000000000000, 0.000000000000000000 ) ) ;
#10223 = CARTESIAN_POINT ( 'NONE',  ( 23.61700585920300099, 13.18055929188999897, -4.241175825786999809 ) ) ;
#10224 = ORIENTED_EDGE ( 'NONE', *, *, #50008, .F. ) ;
#10225 = CARTESIAN_POINT ( 'NONE',  ( 8.614404719593999005, 5.030502105212999453, -6.322203460290999999 ) ) ;
#10226 = CARTESIAN_POINT ( 'NONE',  ( 10.78441772631200024, -3.627481539113199815, 6.733203680593099705 ) ) ;
#10227 = VERTEX_POINT ( 'NONE', #30296 ) ;
#10228 = DIRECTION ( 'NONE',  ( 1.000000000000000000, 0.000000000000000000, 0.000000000000000000 ) ) ;
#10229 = CARTESIAN_POINT ( 'NONE',  ( 11.01456785386839954, -4.946394603182100447, -8.136888821800198457 ) ) ;
#10230 = EDGE_LOOP ( 'NONE', ( #29275, #51325, #23557, #24081 ) ) ;
#10231 = CARTESIAN_POINT ( 'NONE',  ( 11.10101463001529964, 4.622233839778099984, 8.496586578655598743 ) ) ;
#10232 = CARTESIAN_POINT ( 'NONE',  ( 8.994485841233000656, 3.854507394315999758, -9.394302886912999639 ) ) ;
#10233 = FACE_OUTER_BOUND ( 'NONE', #55910, .T. ) ;
#10234 = CARTESIAN_POINT ( 'NONE',  ( 14.93333333161133503, -9.471995579709343360, -8.194932869644890872 ) ) ;
#10235 = CARTESIAN_POINT ( 'NONE',  ( 9.893930206848997599, -5.250000000000000000, -7.500000000000000000 ) ) ;
#10236 = CARTESIAN_POINT ( 'NONE',  ( 10.98768472569999943, 5.449702578894000560, 4.945212061318999375 ) ) ;
#10237 = CARTESIAN_POINT ( 'NONE',  ( 13.64720874474600087, 11.45913667646999912, 2.381478076492999918 ) ) ;
#10238 = EDGE_LOOP ( 'NONE', ( #2734, #29714, #41854, #20895 ) ) ;
#10239 = CARTESIAN_POINT ( 'NONE',  ( 13.92966272177200260, 9.396431546200000540, 8.198412206645000921 ) ) ;
#10240 = CARTESIAN_POINT ( 'NONE',  ( 9.816185841232000442, 2.656512020013999997, -7.884832994446999699 ) ) ;
#10241 = VERTEX_POINT ( 'NONE', #51600 ) ;
#10242 = CARTESIAN_POINT ( 'NONE',  ( 2.500973465876000112, 3.500000000000000000, 0.000000000000000000 ) ) ;
#10243 = ORIENTED_EDGE ( 'NONE', *, *, #44598, .F. ) ;
#10244 = CARTESIAN_POINT ( 'NONE',  ( 8.744113844317999096, 4.323050436788100193, 8.737749087159000894 ) ) ;
#10245 = CARTESIAN_POINT ( 'NONE',  ( 17.69900574642235824, -3.108543425041114805, -12.28872856983836748 ) ) ;
#10246 = CARTESIAN_POINT ( 'NONE',  ( 13.49980696792483137, 10.68794281923483780, 6.218617845733617422 ) ) ;
#10247 = B_SPLINE_CURVE_WITH_KNOTS ( 'NONE', 3,
 ( #20118, #68690, #41106, #62419, #20806, #14540, #25361, #33024, #38257, #6786 ),
 .UNSPECIFIED., .F., .F.,
 ( 4, 2, 2, 2, 4 ),
 ( 0.5000000000000000000, 0.6250000000000000000, 0.7500000000000000000, 0.8750000000000000000, 1.000000000000000000 ),
 .UNSPECIFIED. ) ;
#10248 = DIRECTION ( 'NONE',  ( -1.000000000000000000, 0.000000000000000000, 0.000000000000000000 ) ) ;
#10249 = ADVANCED_FACE ( 'NONE', ( #533 ), #61146, .F. ) ;
#10250 = CARTESIAN_POINT ( 'NONE',  ( 11.79999999550100220, -11.52577121388000059, -1.696750555870000010 ) ) ;
#10251 = EDGE_CURVE ( 'NONE', #22879, #53681, #7835, .T. ) ;
#10252 = VERTEX_POINT ( 'NONE', #49112 ) ;
#10253 = CARTESIAN_POINT ( 'NONE',  ( 12.40355051044899959, 11.78614875273999907, -3.442261952866000119 ) ) ;
#10254 = LINE ( 'NONE', #36834, #30671 ) ;
#10255 = CARTESIAN_POINT ( 'NONE',  ( 8.029017301488174496, -4.353549739959088782, 8.815463536202724271 ) ) ;
#10256 = DIRECTION ( 'NONE',  ( 0.000000000000000000, 1.000000000000000000, 0.000000000000000000 ) ) ;
#10257 = AXIS2_PLACEMENT_3D ( 'NONE', #4235, #8121, #24544 ) ;
#10258 = CARTESIAN_POINT ( 'NONE',  ( 12.24143698068809982, -11.79508855325971162, 3.559061050736494813 ) ) ;
#10259 = CARTESIAN_POINT ( 'NONE',  ( 17.85449583315300259, -3.297641659324999974, 11.83458394846000061 ) ) ;
#10260 = AXIS2_PLACEMENT_3D ( 'NONE', #23317, #45681, #24006 ) ;
#10261 = CARTESIAN_POINT ( 'NONE',  ( 10.52663358771999924, -4.933730002636999679, -6.506004698255999585 ) ) ;
#10262 = ORIENTED_EDGE ( 'NONE', *, *, #63952, .F. ) ;
#10263 = ORIENTED_EDGE ( 'NONE', *, *, #19823, .T. ) ;
#10264 = CARTESIAN_POINT ( 'NONE',  ( 10.85956136592000121, 5.063047012783000511, -5.179223560113999980 ) ) ;
#10265 = DIRECTION ( 'NONE',  ( 0.000000000000000000, -0.1333333333333049375, -0.9910712498212375099 ) ) ;
#10266 = CARTESIAN_POINT ( 'NONE',  ( 1.103056799208124827, 2.798833948393625981, 2.150913519912208471 ) ) ;
#10267 = CARTESIAN_POINT ( 'NONE',  ( 0.000000000000000000, 0.000000000000000000, 0.000000000000000000 ) ) ;
#10268 = CARTESIAN_POINT ( 'NONE',  ( 11.07925595036916633, 5.279255950369167394, 6.503434303641999925 ) ) ;
#10269 = EDGE_CURVE ( 'NONE', #30037, #46374, #15914, .T. ) ;
#10270 = CARTESIAN_POINT ( 'NONE',  ( 9.358051052051999719, 4.850870049477099322, -7.666517576877299511 ) ) ;
#10272 = CARTESIAN_POINT ( 'NONE',  ( 10.26648554153000070, -3.436497692079999666, 4.689477345002000419 ) ) ;
#10271 = CARTESIAN_POINT ( 'NONE',  ( 9.699088727410998700, -5.000897406023000258, 7.416055476975279781 ) ) ;
#10273 = CARTESIAN_POINT ( 'NONE',  ( 8.030239402831002238, -2.905307396403002507, 6.399703979581998325 ) ) ;
#10274 = VERTEX_POINT ( 'NONE', #60641 ) ;
#10275 = EDGE_CURVE ( 'NONE', #27749, #25016, #12405, .T. ) ;
#10276 = CARTESIAN_POINT ( 'NONE',  ( 11.59999999999999964, 5.179498027601999510, -7.174999999999999822 ) ) ;
#10277 = CARTESIAN_POINT ( 'NONE',  ( 8.437014469680988782, -2.901284097310000920, 6.624005965434003329 ) ) ;
#10278 = CARTESIAN_POINT ( 'NONE',  ( 10.03897570133299944, 4.938486452461599896, 6.630731591496600075 ) ) ;
#10279 = LINE ( 'NONE', #31961, #24668 ) ;
#10280 = CARTESIAN_POINT ( 'NONE',  ( 10.87021507563000000, -2.226042145532000305, 7.782753277595999997 ) ) ;
#10281 = CARTESIAN_POINT ( 'NONE',  ( 17.71828964454860511, 3.103661179295900574, -12.29022416950854613 ) ) ;
#10282 = CARTESIAN_POINT ( 'NONE',  ( 16.39947726215000046, -3.188035298175999621, -11.45126509954999960 ) ) ;
#10283 = CARTESIAN_POINT ( 'NONE',  ( 13.64514873068900158, 9.050862583665999495, 7.420564490681000436 ) ) ;
#10284 = CARTESIAN_POINT ( 'NONE',  ( 7.696680409794002919, -4.865376733307997803, 6.399695646141002392 ) ) ;
#10285 = CARTESIAN_POINT ( 'NONE',  ( 10.09058376188599837, -4.847012523549299345, -8.039825975318500184 ) ) ;
#10286 = VECTOR ( 'NONE', #31234, 1000.000000000000114 ) ;
#10287 = CARTESIAN_POINT ( 'NONE',  ( 10.96684687351657672, -4.768183399968645375, 6.500416447002276499 ) ) ;
#10288 = CARTESIAN_POINT ( 'NONE',  ( 25.44993329535400051, 2.258942858049999725, 12.29419282279000036 ) ) ;
#10289 = CARTESIAN_POINT ( 'NONE',  ( 5.700000000000000178, 13.02829083129866738, -1.966948499731759448 ) ) ;
#10290 = DIRECTION ( 'NONE',  ( 1.000000000000000000, 0.000000000000000000, 0.000000000000000000 ) ) ;
#10291 = ORIENTED_EDGE ( 'NONE', *, *, #46673, .T. ) ;
#10292 = CARTESIAN_POINT ( 'NONE',  ( 12.19409707445299773, -0.1321628250398325377, -12.69908003149456377 ) ) ;
#10293 = CARTESIAN_POINT ( 'NONE',  ( 8.227533346878596276, -4.737976145727974320, 6.141445531791949186 ) ) ;
#10294 = CARTESIAN_POINT ( 'NONE',  ( 5.500000000000000000, -12.78667792605000031, 2.345384795463000049 ) ) ;
#10295 = CARTESIAN_POINT ( 'NONE',  ( 7.175632800635331598, -4.000032153724883521, 8.979538128313718559 ) ) ;
#10296 = DIRECTION ( 'NONE',  ( 1.000000000000000000, 1.157371756818000115E-14, 6.365544662497999016E-14 ) ) ;
#10297 = VERTEX_POINT ( 'NONE', #61333 ) ;
#10298 = DIRECTION ( 'NONE',  ( 0.000000000000000000, -0.000000000000000000, 1.000000000000000000 ) ) ;
#10299 = CARTESIAN_POINT ( 'NONE',  ( 10.52946886766499901, -4.430164648092599577, -6.718432993015899690 ) ) ;
#10300 = CARTESIAN_POINT ( 'NONE',  ( 18.06139130780318780, 0.3666439886240649426, 12.69288249683096303 ) ) ;
#10301 = DIRECTION ( 'NONE',  ( 1.000000000000000000, 0.000000000000000000, 0.000000000000000000 ) ) ;
#10302 = CARTESIAN_POINT ( 'NONE',  ( 11.08482133862618113, 4.942979055179590908, -8.373613860257941965 ) ) ;
#10304 = AXIS2_PLACEMENT_3D ( 'NONE', #56708, #45187, #39943 ) ;
#10303 = DIRECTION ( 'NONE',  ( 0.000000000000000000, -0.8648648648648720183, -0.5020047465136825426 ) ) ;
#10305 = VERTEX_POINT ( 'NONE', #34083 ) ;
#10306 = CARTESIAN_POINT ( 'NONE',  ( 9.743567407955000093, -5.287392049455999832, 8.939957179821000466 ) ) ;
#10307 = CARTESIAN_POINT ( 'NONE',  ( 17.57587793826696299, 3.124999446933518943, -13.52084426442464604 ) ) ;
#10308 = ORIENTED_EDGE ( 'NONE', *, *, #20177, .F. ) ;
#10309 = CARTESIAN_POINT ( 'NONE',  ( 3.999999615355000149, -1.825000384556999977, 7.326405409749999507E-10 ) ) ;
#10310 = CARTESIAN_POINT ( 'NONE',  ( 8.379706853209000883, -4.282999948634999221, 9.286791354293999490 ) ) ;
#10311 = AXIS2_PLACEMENT_3D ( 'NONE', #547, #42850, #58582 ) ;
#10312 = DIRECTION ( 'NONE',  ( -0.8231338744408063235, 0.000000000000000000, -0.5678473604306591982 ) ) ;
#10313 = ORIENTED_EDGE ( 'NONE', *, *, #28144, .T. ) ;
#10314 = CARTESIAN_POINT ( 'NONE',  ( 23.57438223407208966, 10.27284394070036555, 9.492890931809894184 ) ) ;
#10315 = B_SPLINE_CURVE_WITH_KNOTS ( 'NONE', 3,
 ( #31461, #68848, #46852, #57670 ),
 .UNSPECIFIED., .F., .F.,
 ( 4, 4 ),
 ( 0.8745879739953518195, 1.000000000000000000 ),
 .UNSPECIFIED. ) ;
#10316 = CARTESIAN_POINT ( 'NONE',  ( 6.885504719591000189, 2.696863807693000048, -8.366590973307999946 ) ) ;
#10317 = CYLINDRICAL_SURFACE ( 'NONE', #24164, 1.250000000000000222 ) ;
#10318 = CARTESIAN_POINT ( 'NONE',  ( 7.871384581343000342, 5.129340811002999878, 6.740051537885999977 ) ) ;
#10319 = ORIENTED_EDGE ( 'NONE', *, *, #41824, .F. ) ;
#10320 = CARTESIAN_POINT ( 'NONE',  ( 9.600494040286998043, -5.206548117663999165, 8.585114612872999373 ) ) ;
#10321 = CARTESIAN_POINT ( 'NONE',  ( 24.78225873320400297, 12.26745412634999965, -2.911642956740000177 ) ) ;
#10322 = DIRECTION ( 'NONE',  ( 1.000000000000000000, 0.000000000000000000, 0.000000000000000000 ) ) ;
#10323 = VERTEX_POINT ( 'NONE', #36046 ) ;
#10324 = CARTESIAN_POINT ( 'NONE',  ( 10.98768472625999948, -5.449702614167000192, -4.945212061590999575 ) ) ;
#10325 = ORIENTED_EDGE ( 'NONE', *, *, #14526, .F. ) ;
#10326 = CARTESIAN_POINT ( 'NONE',  ( 23.58536431466287553, -10.21357488779519684, 9.549750708585223791 ) ) ;
#10327 = CARTESIAN_POINT ( 'NONE',  ( 17.98741890681814937, 0.4515201818990199345, -13.89013314509501917 ) ) ;
#10328 = CARTESIAN_POINT ( 'NONE',  ( 18.43329252113700889, 2.892698357136549880, -12.11790064375146336 ) ) ;
#10329 = DIRECTION ( 'NONE',  ( 0.000000000000000000, 0.000000000000000000, -1.000000000000000000 ) ) ;
#10330 = CARTESIAN_POINT ( 'NONE',  ( 24.30000000000000071, -11.77655473258999841, 4.190794510628000680 ) ) ;
#10331 = CYLINDRICAL_SURFACE ( 'NONE', #42162, 2.000000000000000444 ) ;
#10332 = FACE_OUTER_BOUND ( 'NONE', #3255, .T. ) ;
#10333 = ORIENTED_EDGE ( 'NONE', *, *, #61779, .F. ) ;
#10334 = EDGE_CURVE ( 'NONE', #49203, #36697, #42867, .T. ) ;
#10335 = CARTESIAN_POINT ( 'NONE',  ( 7.591287949680001645, -4.587787988499997915, 6.499994349715005448 ) ) ;
#10336 = EDGE_CURVE ( 'NONE', #13445, #57692, #55383, .T. ) ;
#10337 = VERTEX_POINT ( 'NONE', #12406 ) ;
#10338 = CARTESIAN_POINT ( 'NONE',  ( 9.353724647487000610, 2.823567847429000022, 9.032053040610000139 ) ) ;
#10339 = CARTESIAN_POINT ( 'NONE',  ( 4.485427710978749261, -0.1089645256540823087, 1.530309145191555364 ) ) ;
#10340 = CARTESIAN_POINT ( 'NONE',  ( 9.115000000004000569, -5.349999999999999645, -7.500000000000000000 ) ) ;
#10341 = CARTESIAN_POINT ( 'NONE',  ( 9.517835841233001304, 4.883347899767999323, -6.417062834774999835 ) ) ;
#10342 = AXIS2_PLACEMENT_3D ( 'NONE', #47306, #68610, #62006 ) ;
#10343 = CARTESIAN_POINT ( 'NONE',  ( 9.393246442089999704, -5.100000000000000533, -6.421387671005999387 ) ) ;
#10344 = FILL_AREA_STYLE_COLOUR ( '', #1921 ) ;
#10345 = CARTESIAN_POINT ( 'NONE',  ( 18.08617702649035763, -0.3300666952397341425, 13.89473968862478870 ) ) ;
#10346 = CARTESIAN_POINT ( 'NONE',  ( 18.08719402100870610, 0.3285636529947569273, 13.89479065952357573 ) ) ;
#10347 = ORIENTED_EDGE ( 'NONE', *, *, #16560, .T. ) ;
#10348 = CARTESIAN_POINT ( 'NONE',  ( 12.29146891697695132, 0.3563501258281275286, 13.89385640120309340 ) ) ;
#10349 = CARTESIAN_POINT ( 'NONE',  ( 11.33810672858430024, -5.021298157087000114, 8.268288002587098617 ) ) ;
#10350 = CARTESIAN_POINT ( 'NONE',  ( 10.32652459277042212, 5.723289909120445884, -7.204243127669484714 ) ) ;
#10351 = CARTESIAN_POINT ( 'NONE',  ( 18.12515256033828592, -0.2563263767734609844, -13.89682277887181527 ) ) ;
#10352 = CARTESIAN_POINT ( 'NONE',  ( 7.731793146792000471, -4.580607464247000493, 9.213361409141999303 ) ) ;
#10354 = CARTESIAN_POINT ( 'NONE',  ( 7.890669427268998781, -4.660296165433000404, 6.322498843348999920 ) ) ;
#10353 = CARTESIAN_POINT ( 'NONE',  ( 10.97864812944000157, 5.273131703456000352, 7.958028903907000462 ) ) ;
#10355 = CONICAL_SURFACE ( 'NONE', #59461, 11.75017108327000059, 0.7854127224616339609 ) ;
#10356 = CARTESIAN_POINT ( 'NONE',  ( 11.37964291764649971, 2.731641218595000087, -7.343212302062899433 ) ) ;
#10357 = EDGE_CURVE ( 'NONE', #24707, #64627, #1142, .T. ) ;
#10358 = CARTESIAN_POINT ( 'NONE',  ( 25.20466218340900255, -11.19856126556000042, 3.405324039013999826 ) ) ;
#10359 = CARTESIAN_POINT ( 'NONE',  ( 8.996455549952997899, 4.781695603001899997, -6.869290649434700136 ) ) ;
#10360 = CARTESIAN_POINT ( 'NONE',  ( 17.74345815918222158, 0.6949735217938506349, 12.58082105808780682 ) ) ;
#10361 = CARTESIAN_POINT ( 'NONE',  ( 7.139821367719000555, 0.8827681146003000245, 0.7092679259177999684 ) ) ;
#10362 = CARTESIAN_POINT ( 'NONE',  ( 24.42336652060700075, 8.981205186855000022, 9.518213142638000335 ) ) ;
#10363 = EDGE_LOOP ( 'NONE', ( #65329, #10808, #35851, #36160 ) ) ;
#10364 = CARTESIAN_POINT ( 'NONE',  ( 8.443894353209000059, -2.905864338704999827, 8.940687151810998046 ) ) ;
#10365 = CARTESIAN_POINT ( 'NONE',  ( 9.559179719593000613, 4.038835765825999680, -5.935509327774999733 ) ) ;
#10366 = DIRECTION ( 'NONE',  ( -1.000000000000000000, 0.000000000000000000, 0.000000000000000000 ) ) ;
#10367 = CARTESIAN_POINT ( 'NONE',  ( 10.09999999999999964, 0.000000000000000000, 11.84999999999999964 ) ) ;
#10368 = ORIENTED_EDGE ( 'NONE', *, *, #11992, .F. ) ;
#10369 = CARTESIAN_POINT ( 'NONE',  ( 18.23019412026599895, 3.031170125296999807, 11.90979123982999965 ) ) ;
#10370 = CARTESIAN_POINT ( 'NONE',  ( 10.36325056272499978, 4.892034740700499817, 7.486779603004729111 ) ) ;
#10371 = CARTESIAN_POINT ( 'NONE',  ( 10.87947334122999976, 2.817426144593000004, -6.828668581221999823 ) ) ;
#10372 = VERTEX_POINT ( 'NONE', #1563 ) ;
#10373 = CARTESIAN_POINT ( 'NONE',  ( 9.289752973821551407, 3.672827138550766257, -6.282573595533350819 ) ) ;
#10375 = CARTESIAN_POINT ( 'NONE',  ( 17.55505043854147118, -1.760845406083394682, 12.47635457398814829 ) ) ;
#10374 = B_SPLINE_CURVE_WITH_KNOTS ( 'NONE', 3,
 ( #42387, #4973, #26993, #26306, #11245, #21392, #32583, #37138, #58455, #38156 ),
 .UNSPECIFIED., .F., .F.,
 ( 4, 2, 2, 2, 4 ),
 ( 0.000000000000000000, 0.2500000000000001110, 0.5000000000000000000, 0.7500000000000000000, 1.000000000000000000 ),
 .UNSPECIFIED. ) ;
#10376 = CARTESIAN_POINT ( 'NONE',  ( 11.13349010443639919, 5.274453806861999716, 7.404690636538299842 ) ) ;
#10377 = DIRECTION ( 'NONE',  ( 0.5000000000000169864, 0.000000000000000000, 0.8660254037844288266 ) ) ;
#10378 = CARTESIAN_POINT ( 'NONE',  ( 7.282482780409000434, 3.448180532882000104, 9.222462917385000125 ) ) ;
#10379 = ORIENTED_EDGE ( 'NONE', *, *, #2692, .T. ) ;
#10380 = CARTESIAN_POINT ( 'NONE',  ( 25.26995798061230403, -11.52974591960634143, -2.996559586417926191 ) ) ;
#10381 = CARTESIAN_POINT ( 'NONE',  ( 8.453079719590000707, 5.452311718892000059, -8.444358433472999081 ) ) ;
#10382 = CARTESIAN_POINT ( 'NONE',  ( 8.382401718153786874, -2.849781230174281532, 8.805156601495802704 ) ) ;
#10383 = CARTESIAN_POINT ( 'NONE',  ( 10.92328601976000080, -8.084347899873000287, 7.050238229386000199 ) ) ;
#10384 = ORIENTED_EDGE ( 'NONE', *, *, #14666, .T. ) ;
#10385 = CARTESIAN_POINT ( 'NONE',  ( 16.39944283128300029, -3.410739012457999930, -11.89826262991000050 ) ) ;
#10386 = CARTESIAN_POINT ( 'NONE',  ( 6.282109839683333696, 0.9218200799623742503, -1.199500263597268912 ) ) ;
#10387 = EDGE_LOOP ( 'NONE', ( #56927, #260, #62030, #55809 ) ) ;
#10388 = DIRECTION ( 'NONE',  ( 0.000000000000000000, -1.000000000000000000, 0.000000000000000000 ) ) ;
#10389 = CARTESIAN_POINT ( 'NONE',  ( 7.726719819322242166, -3.010539059095759029, 6.557630456826268883 ) ) ;
#10390 = DIRECTION ( 'NONE',  ( 0.000000000000000000, 0.000000000000000000, -1.000000000000000000 ) ) ;
#10391 = EDGE_CURVE ( 'NONE', #37575, #36489, #64832, .T. ) ;
#10392 = EDGE_CURVE ( 'NONE', #35162, #57180, #37060, .T. ) ;
#10393 = CYLINDRICAL_SURFACE ( 'NONE', #26420, 1.250000000000000222 ) ;
#10394 = CARTESIAN_POINT ( 'NONE',  ( 24.37808884581836111, -8.911082519650753042, -9.054599882782522258 ) ) ;
#10395 = CARTESIAN_POINT ( 'NONE',  ( 11.31389666366019853, 3.954123449088899900, -8.532487796751999198 ) ) ;
#10396 = CARTESIAN_POINT ( 'NONE',  ( 12.34388784977539899, -5.255745690988000263, 7.571757098260779806 ) ) ;
#10397 = CARTESIAN_POINT ( 'NONE',  ( 12.66109513597118408, 3.108543426238434382, -12.28874474902926117 ) ) ;
#10398 = CARTESIAN_POINT ( 'NONE',  ( 24.67921311619700120, 3.567517360056999820, 12.13750603036999998 ) ) ;
#10399 = ORIENTED_EDGE ( 'NONE', *, *, #10000, .F. ) ;
#10400 = CARTESIAN_POINT ( 'NONE',  ( 8.860767219592000643, 2.935741164366000522, 6.259844213126999790 ) ) ;
#10401 = VERTEX_POINT ( 'NONE', #22885 ) ;
#10402 = CARTESIAN_POINT ( 'NONE',  ( 3.499999999999999556, -3.170392682610728041, -0.3463127203071835192 ) ) ;
#10403 = CARTESIAN_POINT ( 'NONE',  ( 8.896432056425130241, 5.285622111567785275, 7.027794277398490053 ) ) ;
#10404 = CARTESIAN_POINT ( 'NONE',  ( 11.09049845538999968, -5.289010560972999819, 5.109759112891000044 ) ) ;
#10405 = ORIENTED_EDGE ( 'NONE', *, *, #14607, .F. ) ;
#10406 = CARTESIAN_POINT ( 'NONE',  ( 12.47303194318978647, -3.029615900428510589, -12.31225512782602927 ) ) ;
#10407 = CARTESIAN_POINT ( 'NONE',  ( 18.47905117804075914, 2.854821129078588982, 11.29488031137690207 ) ) ;
#10408 = DIRECTION ( 'NONE',  ( 1.000000000000000000, 0.000000000000000000, 0.000000000000000000 ) ) ;
#10409 = CARTESIAN_POINT ( 'NONE',  ( 23.56682100824491144, -13.33070654784838993, -4.243923923310612523 ) ) ;
#10410 = CARTESIAN_POINT ( 'NONE',  ( 12.38020518697568839, -1.926193139504583707, -13.86686096623706987 ) ) ;
#10411 = CARTESIAN_POINT ( 'NONE',  ( 10.62903166480609940, -4.864052766304100217, -7.560921321260908989 ) ) ;
#10412 = CARTESIAN_POINT ( 'NONE',  ( 18.48260618742725114, 3.086131726339705672, 12.13914505220553686 ) ) ;
#10413 = CARTESIAN_POINT ( 'NONE',  ( 18.22257245894170907, -2.198943951577552625, 12.40664208059732410 ) ) ;
#10414 = ORIENTED_EDGE ( 'NONE', *, *, #47128, .F. ) ;
#10415 = EDGE_CURVE ( 'NONE', #56969, #8552, #51472, .T. ) ;
#10416 = ORIENTED_EDGE ( 'NONE', *, *, #47128, .T. ) ;
#10417 = DIRECTION ( 'NONE',  ( 0.000000000000000000, 0.000000000000000000, 1.000000000000000000 ) ) ;
#10418 = CARTESIAN_POINT ( 'NONE',  ( 11.68220574173929727, -2.863826994586552210, 8.088082908809445470 ) ) ;
#10419 = CARTESIAN_POINT ( 'NONE',  ( 4.900006121741999898, 1.229093439949832334, 1.599333684796358401 ) ) ;
#10420 = EDGE_CURVE ( 'NONE', #24248, #28381, #35852, .T. ) ;
#10421 = CARTESIAN_POINT ( 'NONE',  ( 10.48414939117999900, 4.098653981087000631, -9.351365234892998757 ) ) ;
#10422 = CARTESIAN_POINT ( 'NONE',  ( 12.79999999914999975, -12.11987927271999865, 3.159802730921999814 ) ) ;
#10423 = CARTESIAN_POINT ( 'NONE',  ( 18.10184288977456646, 2.186031417495633455, -12.51954808657351848 ) ) ;
#10424 = CARTESIAN_POINT ( 'NONE',  ( 8.231600168468999001, 3.072304018142998139, -6.138007231110007567 ) ) ;
#10425 = CARTESIAN_POINT ( 'NONE',  ( 18.20426522488219589, -2.108767964861150368, -12.42302121882717536 ) ) ;
#10426 = EDGE_LOOP ( 'NONE', ( #2018, #47983, #45995, #34328, #21470, #24970, #39620, #55480, #36089, #66880 ) ) ;
#10427 = CARTESIAN_POINT ( 'NONE',  ( 8.654133428465479838, -4.873369502965289257, -6.470443573412346439 ) ) ;
#10428 = CARTESIAN_POINT ( 'NONE',  ( 12.55891702277100563, -3.074517471785633838, 12.29897628258782483 ) ) ;
#10429 = CARTESIAN_POINT ( 'NONE',  ( 13.86904166957594953, 8.833215535550262842, 7.896538540699785003 ) ) ;
#10430 = CONICAL_SURFACE ( 'NONE', #68459, 12.47499939740000130, 0.7853981102588313279 ) ;
#10431 = CARTESIAN_POINT ( 'NONE',  ( 10.35616100078999935, 2.777276096020000029, 8.995275123087999702 ) ) ;
#10432 = CARTESIAN_POINT ( 'NONE',  ( 11.19568717260499824, -4.466067913030199676, 6.739296831621899742 ) ) ;
#10433 = CARTESIAN_POINT ( 'NONE',  ( 6.949999999999961986, 5.456597484868912495, -8.185422748483135891 ) ) ;
#10434 = CONICAL_SURFACE ( 'NONE', #14888, 0.3062142749367001149, 0.7853981633972997312 ) ;
#10435 = CARTESIAN_POINT ( 'NONE',  ( 11.06517113529999996, 8.815199625753001200, -6.641975173320999737 ) ) ;
#10436 = EDGE_CURVE ( 'NONE', #46074, #28855, #43643, .T. ) ;
#10437 = CARTESIAN_POINT ( 'NONE',  ( 12.70247988648369386, -0.6166112555940445050, 12.67984200623734381 ) ) ;
#10438 = CARTESIAN_POINT ( 'NONE',  ( 6.055026506350000837, -1.500000000000000000, 0.000000000000000000 ) ) ;
#10439 = CARTESIAN_POINT ( 'NONE',  ( 9.820199962102000413, 3.883325513302000154, 6.055618835924000187 ) ) ;
#10440 = CARTESIAN_POINT ( 'NONE',  ( 15.39999999998900293, 9.471998555523999386, 8.194929586088999685 ) ) ;
#10441 = VERTEX_POINT ( 'NONE', #1918 ) ;
#10442 = CARTESIAN_POINT ( 'NONE',  ( 9.169760841232999837, 4.728328492779000136, -8.692725459657999920 ) ) ;
#10443 = CARTESIAN_POINT ( 'NONE',  ( 6.961532175979001202, -1.035056448321000078, 1.007531618533000106 ) ) ;
#10444 = CARTESIAN_POINT ( 'NONE',  ( 17.55505043854143565, 1.874999999999999556, 13.78627172894481667 ) ) ;
#10445 = CARTESIAN_POINT ( 'NONE',  ( 9.229794494861661036, 4.176538781553355228, -8.850125647912786775 ) ) ;
#10446 = CARTESIAN_POINT ( 'NONE',  ( 24.26733149983100191, 8.951944080867999531, -8.897842724163000483 ) ) ;
#10447 = CARTESIAN_POINT ( 'NONE',  ( 11.23610538575739959, -2.890527834009000152, -7.234742334405199315 ) ) ;
#10448 = ORIENTED_EDGE ( 'NONE', *, *, #16807, .F. ) ;
#10449 = AXIS2_PLACEMENT_3D ( 'NONE', #50579, #23657, #61069 ) ;
#10450 = CARTESIAN_POINT ( 'NONE',  ( 10.08521345716899908, -3.075109701058799772, -8.340879262988799780 ) ) ;
#10451 = CARTESIAN_POINT ( 'NONE',  ( 8.014948341228999240, 2.280568568659000483, 6.510284508622999233 ) ) ;
#10452 = VECTOR ( 'NONE', #14909, 1000.000000000000000 ) ;
#10454 = CARTESIAN_POINT ( 'NONE',  ( 13.50567905817900183, -9.332645239999999731, -7.987984570204999635 ) ) ;
#10453 = CARTESIAN_POINT ( 'NONE',  ( 8.813304719595000947, 3.880154689736000417, -9.060377011187000562 ) ) ;
#10455 = CARTESIAN_POINT ( 'NONE',  ( 18.17602379430269011, -2.571655014620207069, 13.65800652342065469 ) ) ;
#10456 = EDGE_LOOP ( 'NONE', ( #62577, #9701, #39880 ) ) ;
#10457 = CARTESIAN_POINT ( 'NONE',  ( 11.29622358543999994, 3.561657733933999648, 6.266050246368000565 ) ) ;
#10458 = CARTESIAN_POINT ( 'NONE',  ( 17.91230600709726772, -3.012931617833825904, -13.55113455194569028 ) ) ;
#10459 = CARTESIAN_POINT ( 'NONE',  ( 11.49056651104150006, 4.085456792591960706, 8.361971998931499783 ) ) ;
#10460 = CARTESIAN_POINT ( 'NONE',  ( 10.25888544622000076, -4.512389816463000081, 5.993697694029000544 ) ) ;
#10461 = CARTESIAN_POINT ( 'NONE',  ( 7.486433059621999675, -5.321924421352999701, 8.118250081378000971 ) ) ;
#10462 = ORIENTED_EDGE ( 'NONE', *, *, #66436, .T. ) ;
#10463 = CARTESIAN_POINT ( 'NONE',  ( 9.406704719590001318, 3.705846972803000128, 9.096435887808000942 ) ) ;
#10465 = CARTESIAN_POINT ( 'NONE',  ( 10.98633305961999973, -3.015090804604000141, -9.064432363387998848 ) ) ;
#10464 = DIRECTION ( 'NONE',  ( 0.000000000000000000, 1.000000000000000000, 0.000000000000000000 ) ) ;
#10466 = CARTESIAN_POINT ( 'NONE',  ( 7.613456797751473992, -4.810924280407760989, 5.960869268491793882 ) ) ;
#10467 = CARTESIAN_POINT ( 'NONE',  ( 17.96365918304935860, -0.4729502184326867531, 13.88916975807169862 ) ) ;
#10468 = DIRECTION ( 'NONE',  ( 1.000000000000000000, 0.000000000000000000, 0.000000000000000000 ) ) ;
#10469 = ORIENTED_EDGE ( 'NONE', *, *, #60409, .T. ) ;
#10470 = CARTESIAN_POINT ( 'NONE',  ( 5.802943173016667622, 1.199500263597271799, -0.9218200799623701425 ) ) ;
#10471 = B_SPLINE_CURVE_WITH_KNOTS ( 'NONE', 3,
 ( #36181, #40393, #14521, #51233, #2986, #3662 ),
 .UNSPECIFIED., .F., .F.,
 ( 4, 2, 4 ),
 ( 0.000000000000000000, 0.5000000000000000000, 1.000000000000000000 ),
 .UNSPECIFIED. ) ;
#10472 = CARTESIAN_POINT ( 'NONE',  ( 11.83456651104149948, -3.887457492043800311, 8.635175889530000148 ) ) ;
#10473 = CARTESIAN_POINT ( 'NONE',  ( 10.85737917744000036, 2.754548910086000113, 8.976376585747001258 ) ) ;
#10474 = CARTESIAN_POINT ( 'NONE',  ( 11.33456651104149948, 4.112542507956200133, 8.635175889530000148 ) ) ;
#10475 = ORIENTED_EDGE ( 'NONE', *, *, #75, .F. ) ;
#10476 = EDGE_CURVE ( 'NONE', #32830, #27541, #38979, .T. ) ;
#10477 = EDGE_CURVE ( 'NONE', #31379, #60315, #64515, .T. ) ;
#10478 = B_SPLINE_SURFACE_WITH_KNOTS ( 'NONE', 3, 3, ( 
 ( #24730, #9667, #40804, #10017 ),
 ( #46747, #14586, #67702, #20166 ),
 ( #35573, #50956, #68052, #41494 ),
 ( #61784, #3054, #8986, #30328 ),
 ( #19829, #13903, #56543, #41160 ),
 ( #8649, #51636, #3733, #25067 ),
 ( #62466, #35904, #62805, #15614 ),
 ( #69093, #59285, #32391, #37281 ),
 ( #53706, #63837, #917, #53363 ),
 ( #21197, #11390, #63494, #10362 ),
 ( #42872, #31697, #52669, #5466 ),
 ( #47784, #10702, #38310, #54044 ) ),
 .UNSPECIFIED., .F., .F., .F.,
 ( 4, 1, 1, 1, 1, 1, 1, 1, 1, 4 ),
 ( 4, 4 ),
 ( 0.5527793964264999804, 0.5999999999999999778, 0.6500000000000000222, 0.6999999999999999556, 0.7500000000000000000, 0.8000000000000000444, 0.8499999999999999778, 0.9000000000000000222, 0.9499999999999999556, 0.9893861203041000030 ),
 ( -0.2706700323135999842, 1.270791129485999926 ),
 .UNSPECIFIED. ) ;
#10479 = CARTESIAN_POINT ( 'NONE',  ( 8.470944094208999076, -5.100000000000000533, 6.571291218949999902 ) ) ;
#10480 = ADVANCED_FACE ( 'NONE', ( #26599 ), #37085, .F. ) ;
#10481 = CARTESIAN_POINT ( 'NONE',  ( 12.80505043854143388, 1.760845406083386910, -12.47635457398815007 ) ) ;
#10482 = CARTESIAN_POINT ( 'NONE',  ( 11.42968717260509948, -4.687649763627899979, 6.377637058250999580 ) ) ;
#10483 = CARTESIAN_POINT ( 'NONE',  ( 24.39664803201866405, -8.853227592127330681, 8.853227592127330681 ) ) ;
#10484 = VECTOR ( 'NONE', #6566, 1000.000000000000114 ) ;
#10485 = CARTESIAN_POINT ( 'NONE',  ( 17.74403704562418937, -1.812651413143275381, 13.88215924362445897 ) ) ;
#10486 = CARTESIAN_POINT ( 'NONE',  ( 18.16582246963814384, 2.632686764026700654, -13.64442020596820271 ) ) ;
#10487 = ORIENTED_EDGE ( 'NONE', *, *, #30154, .F. ) ;
#10488 = CARTESIAN_POINT ( 'NONE',  ( 11.03482133862663517, 4.942979055179590908, 6.626386139742056258 ) ) ;
#10489 = CARTESIAN_POINT ( 'NONE',  ( 13.43777338887480610, -12.12041883920679730, -2.246947635350974970 ) ) ;
#10490 = ORIENTED_EDGE ( 'NONE', *, *, #3768, .F. ) ;
#10491 = PLANE ( 'NONE',  #13814 ) ;
#10492 = CARTESIAN_POINT ( 'NONE',  ( 10.72333863405319931, 4.619094858989799768, 6.710270673950399889 ) ) ;
#10493 = CARTESIAN_POINT ( 'NONE',  ( 10.06843885510000014, 4.148608506723999945, 8.941445591976998841 ) ) ;
#10494 = CARTESIAN_POINT ( 'NONE',  ( 10.69578011722000177, 5.505003832924999507, -7.759263776825999770 ) ) ;
#10495 = LINE ( 'NONE', #64308, #49865 ) ;
#10496 = CARTESIAN_POINT ( 'NONE',  ( 11.18706725482999964, -3.186788126275999833, 6.232699537089999353 ) ) ;
#10497 = CARTESIAN_POINT ( 'NONE',  ( 17.86760901219547293, 0.5416145769730069670, -12.68445494689095732 ) ) ;
#10498 = LINE ( 'NONE', #20306, #55355 ) ;
#10499 = CARTESIAN_POINT ( 'NONE',  ( 10.79718447801629999, -2.996774412198000448, -7.477880487566260115 ) ) ;
#10500 = CARTESIAN_POINT ( 'NONE',  ( 9.523698341228998387, 4.852728889087999598, 8.683917172082999514 ) ) ;
#10501 = ORIENTED_EDGE ( 'NONE', *, *, #52556, .T. ) ;
#10502 = B_SPLINE_CURVE_WITH_KNOTS ( 'NONE', 3,
 ( #5846, #48506, #611, #64567 ),
 .UNSPECIFIED., .F., .F.,
 ( 4, 4 ),
 ( 0.000000000000000000, 1.000000000000000000 ),
 .UNSPECIFIED. ) ;
#10503 = CONICAL_SURFACE ( 'NONE', #8268, 12.49999584805000019, 0.7853981146832407223 ) ;
#10504 = CARTESIAN_POINT ( 'NONE',  ( 24.70905524881975523, -3.127839019168523027, 11.79917697410494171 ) ) ;
#10505 = CARTESIAN_POINT ( 'NONE',  ( 9.242854517844085294, 2.682272565524075780, 7.207860447134208037 ) ) ;
#10506 = CARTESIAN_POINT ( 'NONE',  ( 8.647846113052866102, 2.999226622549716392, -6.113461772567276853 ) ) ;
#10507 = VECTOR ( 'NONE', #8680, 1000.000000000000000 ) ;
#10508 = CARTESIAN_POINT ( 'NONE',  ( 10.21908538701999625, 9.735603468294996787, 6.344040641747004550 ) ) ;
#10509 = DIRECTION ( 'NONE',  ( 1.000000000000000000, 0.000000000000000000, 0.000000000000000000 ) ) ;
#10510 = CARTESIAN_POINT ( 'NONE',  ( 11.04779069327000052, 9.995291468210998787, 5.683114286574999952 ) ) ;
#10511 = CIRCLE ( 'NONE', #2686, 2.000000000000000444 ) ;
#10512 = CARTESIAN_POINT ( 'NONE',  ( 9.896013540183126622, -4.999583552997726166, -8.268183399968641822 ) ) ;
#10513 = VERTEX_POINT ( 'NONE', #63291 ) ;
#10514 = CARTESIAN_POINT ( 'NONE',  ( 24.60999195316300003, 8.752663949940000521, 9.057796881813999335 ) ) ;
#10515 = CARTESIAN_POINT ( 'NONE',  ( 9.557721904870000174, -2.884547197234000215, -8.126218358304999612 ) ) ;
#10516 = CARTESIAN_POINT ( 'NONE',  ( 18.30000000000000071, 0.000000000000000000, 0.000000000000000000 ) ) ;
#10517 = CARTESIAN_POINT ( 'NONE',  ( 9.696086916451999826, -2.554404004330999900, 7.600685922079000179 ) ) ;
#10518 = CARTESIAN_POINT ( 'NONE',  ( 11.17826222744820086, -4.668580868411999596, 6.949274830123499669 ) ) ;
#10519 = ADVANCED_FACE ( 'NONE', ( #62942 ), #57708, .F. ) ;
#10520 = CARTESIAN_POINT ( 'NONE',  ( 12.34976886901036863, 0.5598083480993562011, 12.58755849294668394 ) ) ;
#10521 = CARTESIAN_POINT ( 'NONE',  ( 0.6748509817850999459, 2.983562695318000113, -1.348686013867999911 ) ) ;
#10522 = DIRECTION ( 'NONE',  ( 1.000000000000000000, 0.000000000000000000, 0.000000000000000000 ) ) ;
#10523 = EDGE_CURVE ( 'NONE', #49128, #4545, #53506, .T. ) ;
#10524 = CARTESIAN_POINT ( 'NONE',  ( 12.08005347077622460, 2.506700685333588918, 12.34815832536655655 ) ) ;
#10526 = CARTESIAN_POINT ( 'NONE',  ( 5.700000000000000178, -13.04986661130000059, -1.811520473896000016 ) ) ;
#10525 = CARTESIAN_POINT ( 'NONE',  ( 9.302417874593999159, 2.949199072237000063, -7.946712276748498560 ) ) ;
#10527 = CARTESIAN_POINT ( 'NONE',  ( 10.87103032197929942, 4.583685623598699799, -6.683751296690399357 ) ) ;
#10528 = CARTESIAN_POINT ( 'NONE',  ( 7.964620641636996901, 2.867893108869000507, -6.758951315555000505 ) ) ;
#10529 = CARTESIAN_POINT ( 'NONE',  ( 10.35752971959000135, 5.367812128871999988, -6.514736131541999598 ) ) ;
#10530 = CARTESIAN_POINT ( 'NONE',  ( 8.946747021775999897, 3.038503783616799847, -8.343747244947598674 ) ) ;
#10532 = CARTESIAN_POINT ( 'NONE',  ( 12.20453436425304261, 2.673271222929743285, 12.40950569879642629 ) ) ;
#10531 = CARTESIAN_POINT ( 'NONE',  ( 4.999999999906999726, -1.352284263165000056, 11.01731942304999912 ) ) ;
#10533 = LINE ( 'NONE', #30839, #46431 ) ;
#10534 = ORIENTED_EDGE ( 'NONE', *, *, #49708, .T. ) ;
#10535 = AXIS2_PLACEMENT_3D ( 'NONE', #35223, #12511, #33843 ) ;
#10536 = CARTESIAN_POINT ( 'NONE',  ( 0.9764734890463999673, -3.085119672805999524, 1.050391531144999835 ) ) ;
#10537 = CARTESIAN_POINT ( 'NONE',  ( 7.717918988116000634, 2.852331522235000083, 6.784355039830999523 ) ) ;
#10538 = CARTESIAN_POINT ( 'NONE',  ( 10.19256470245000123, -2.560274838243000062, 7.664550593243999899 ) ) ;
#10539 = CARTESIAN_POINT ( 'NONE',  ( 10.28622949779699880, 4.480999174483200065, 6.778648208007999720 ) ) ;
#10540 = CARTESIAN_POINT ( 'NONE',  ( 23.56664322114200161, -2.935586410151000081, -13.67842711829000102 ) ) ;
#10541 = CARTESIAN_POINT ( 'NONE',  ( 12.18763606713065073, -2.400822034753087753, 13.69401148367744270 ) ) ;
#10542 = CARTESIAN_POINT ( 'NONE',  ( 10.45746213570999927, -5.100000000000000533, -6.571291218949999902 ) ) ;
#10543 = FACE_OUTER_BOUND ( 'NONE', #10581, .T. ) ;
#10544 = EDGE_LOOP ( 'NONE', ( #69001, #35232, #553, #51402 ) ) ;
#10545 = B_SPLINE_CURVE_WITH_KNOTS ( 'NONE', 3,
 ( #11550, #48627, #32551, #26623, #16797, #730, #28000, #59109, #42, #49309, #43389, #65029, #53864, #43035 ),
 .UNSPECIFIED., .F., .F.,
 ( 4, 2, 2, 2, 2, 2, 4 ),
 ( 0.000000000000000000, 0.1250000000000030809, 0.2500000000000061617, 0.5000000000000043299, 0.6250000000000035527, 0.7500000000000026645, 1.000000000000000000 ),
 .UNSPECIFIED. ) ;
#10546 = CARTESIAN_POINT ( 'NONE',  ( 4.329599320976000421, -0.7696520519970999619, 1.017058582320000015 ) ) ;
#10547 = AXIS2_PLACEMENT_3D ( 'NONE', #28825, #1202, #13080 ) ;
#10548 = CARTESIAN_POINT ( 'NONE',  ( 9.807938025973999885, -4.665064168510499876, -6.407263051216999017 ) ) ;
#10549 = CARTESIAN_POINT ( 'NONE',  ( 4.555026506349999948, -1.500000000000000000, 0.000000000000000000 ) ) ;
#10550 = CARTESIAN_POINT ( 'NONE',  ( 11.15413259636999932, -4.783377755405500587, 7.073141822156699732 ) ) ;
#10551 = CARTESIAN_POINT ( 'NONE',  ( 18.17995611468269246, 2.522932803854499806, -12.44624262618112631 ) ) ;
#10552 = CARTESIAN_POINT ( 'NONE',  ( 10.38462472191413255, -2.899999999999999911, 6.445686799157043012 ) ) ;
#10553 = VECTOR ( 'NONE', #53676, 1000.000000000000000 ) ;
#10554 = CARTESIAN_POINT ( 'NONE',  ( 18.15140653315626196, 2.687261712024030746, 12.40596587094356984 ) ) ;
#10555 = ADVANCED_FACE ( 'NONE', ( #36744 ), #31843, .T. ) ;
#10556 = DIRECTION ( 'NONE',  ( 1.000000000000000000, 0.000000000000000000, 0.000000000000000000 ) ) ;
#10557 = CARTESIAN_POINT ( 'NONE',  ( 24.39664890306633183, 3.240506439362909497, -12.09373467396045854 ) ) ;
#10558 = DIRECTION ( 'NONE',  ( 0.000000000000000000, 0.000000000000000000, -1.000000000000000000 ) ) ;
#10559 = EDGE_CURVE ( 'NONE', #43884, #68795, #68192, .T. ) ;
#10560 = CARTESIAN_POINT ( 'NONE',  ( 10.52052890781999928, 2.899999999999999911, 6.152188490330000370 ) ) ;
#10561 = EDGE_CURVE ( 'NONE', #44978, #52369, #48691, .T. ) ;
#10562 = CARTESIAN_POINT ( 'NONE',  ( 11.49664311227126490, -3.555960431980461411, 6.293666904468254941 ) ) ;
#10563 = CARTESIAN_POINT ( 'NONE',  ( 11.03111947020579819, -4.908799224006100026, -7.174999999999999822 ) ) ;
#10564 = CARTESIAN_POINT ( 'NONE',  ( 23.63098021901300072, 13.46819232204000016, -3.822892805028000218 ) ) ;
#10565 = VECTOR ( 'NONE', #43956, 1000.000000000000000 ) ;
#10566 = ORIENTED_EDGE ( 'NONE', *, *, #67862, .F. ) ;
#10567 = CARTESIAN_POINT ( 'NONE',  ( 8.655270280412999284, 4.162493982103000256, -5.775210092227999858 ) ) ;
#10568 = CARTESIAN_POINT ( 'NONE',  ( 11.71979841651039855, -4.304975143798100312, 6.689266534545799558 ) ) ;
#10569 = ORIENTED_EDGE ( 'NONE', *, *, #34743, .T. ) ;
#10570 = CARTESIAN_POINT ( 'NONE',  ( 13.04552286951901330, 12.39025300375190142, 1.832281502500254566 ) ) ;
#10571 = CARTESIAN_POINT ( 'NONE',  ( 11.37964291764649971, -5.268358781405000357, -7.343212302062899433 ) ) ;
#10572 = ORIENTED_EDGE ( 'NONE', *, *, #44866, .F. ) ;
#10573 = CARTESIAN_POINT ( 'NONE',  ( 12.79999999468004646, -11.20144845259485678, 4.552734317499857575 ) ) ;
#10574 = CYLINDRICAL_SURFACE ( 'NONE', #26633, 1.350000000000000089 ) ;
#10575 = CARTESIAN_POINT ( 'NONE',  ( 18.18404792230800382, -3.205001206845999651, 11.25648540289999922 ) ) ;
#10576 = CARTESIAN_POINT ( 'NONE',  ( 10.77879632507499785, -3.576455950783300253, -8.285174533868300273 ) ) ;
#10577 = CARTESIAN_POINT ( 'NONE',  ( 9.748096873515667227, -3.672815144550895194, -6.282534154164607365 ) ) ;
#10578 = B_SPLINE_CURVE_WITH_KNOTS ( 'NONE', 3,
 ( #27051, #127, #31605, #43122, #820, #10613, #58854, #15524, #37878, #48718, #26362, #42095, #68999, #31953, #48024, #11299, #10964, #68647 ),
 .UNSPECIFIED., .F., .F.,
 ( 4, 2, 2, 2, 2, 2, 2, 2, 4 ),
 ( 0.000000000000000000, 0.1249999999999999445, 0.2499999999999998890, 0.3749999999999998890, 0.4999999999999997780, 0.6249999999999997780, 0.7499999999999998890, 0.8749999999999998890, 1.000000000000000000 ),
 .UNSPECIFIED. ) ;
#10579 = CARTESIAN_POINT ( 'NONE',  ( 11.60000000000000142, -4.531190383827668811, -6.694115079111574218 ) ) ;
#10580 = CARTESIAN_POINT ( 'NONE',  ( 12.99325612864500279, 11.57041205278999918, 1.757148387262999822 ) ) ;
#10581 = EDGE_LOOP ( 'NONE', ( #46918, #57769, #66926, #27673 ) ) ;
#10582 = CARTESIAN_POINT ( 'NONE',  ( 8.517351160491474005, 5.205057563154839251, 8.206039936683215075 ) ) ;
#10583 = ORIENTED_EDGE ( 'NONE', *, *, #13802, .F. ) ;
#10584 = EDGE_CURVE ( 'NONE', #27904, #32611, #54509, .T. ) ;
#10585 = VECTOR ( 'NONE', #27843, 1000.000000000000000 ) ;
#10586 = CARTESIAN_POINT ( 'NONE',  ( 10.72726354018300121, 4.629523725463627670, -6.407767014557179230 ) ) ;
#10587 = ORIENTED_EDGE ( 'NONE', *, *, #40265, .F. ) ;
#10588 = CARTESIAN_POINT ( 'NONE',  ( 8.642797255587998606, 5.278067516796999925, 7.554109351283189611 ) ) ;
#10589 = CARTESIAN_POINT ( 'NONE',  ( 18.11597065765687375, -2.775858272760586498, -12.38300578299706345 ) ) ;
#10590 = CARTESIAN_POINT ( 'NONE',  ( 10.32101354018304207, 3.231816600031359510, -6.500416447002272946 ) ) ;
#10591 = DIRECTION ( 'NONE',  ( 0.000000000000000000, 1.000000000000000000, 0.000000000000000000 ) ) ;
#10592 = CARTESIAN_POINT ( 'NONE',  ( 12.18006450918421990, -0.02080959496299183628, 13.89999914846831963 ) ) ;
#10593 = ORIENTED_EDGE ( 'NONE', *, *, #3647, .F. ) ;
#10594 = CARTESIAN_POINT ( 'NONE',  ( 12.17512857912400115, 11.55078329699999884, -4.188961560869000067 ) ) ;
#10595 = CARTESIAN_POINT ( 'NONE',  ( 18.13017043268600048, 11.56648533137999912, -4.655999611355000845 ) ) ;
#10596 = CARTESIAN_POINT ( 'NONE',  ( 9.834799664234624927, 4.795722374051563541, 7.136189372949617749 ) ) ;
#10597 = CARTESIAN_POINT ( 'NONE',  ( 8.956149159797568871, 2.922971693198220144, 7.790330864865198990 ) ) ;
#10598 = CARTESIAN_POINT ( 'NONE',  ( 8.599639158772999892, 2.261390688294000029, -6.733978371730000134 ) ) ;
#10599 = AXIS2_PLACEMENT_3D ( 'NONE', #37506, #793, #446 ) ;
#10600 = CARTESIAN_POINT ( 'NONE',  ( 17.60000000085000238, 12.11987927271999865, -3.159802730921999814 ) ) ;
#10601 = CARTESIAN_POINT ( 'NONE',  ( 10.22440803363000050, -5.317414323721999736, -8.272454209812998727 ) ) ;
#10602 = ORIENTED_EDGE ( 'NONE', *, *, #41654, .F. ) ;
#10603 = ORIENTED_EDGE ( 'NONE', *, *, #28580, .T. ) ;
#10604 = CARTESIAN_POINT ( 'NONE',  ( 10.89182486572000030, 5.053346025730999891, -5.014777255665999078 ) ) ;
#10605 = EDGE_CURVE ( 'NONE', #15028, #20142, #26156, .T. ) ;
#10606 = CARTESIAN_POINT ( 'NONE',  ( 10.52462472184161157, 2.899999999999999911, -6.445686799303610215 ) ) ;
#10607 = DIRECTION ( 'NONE',  ( 0.000000000000000000, 0.8648648648648470383, -0.5020047465137256193 ) ) ;
#10608 = CARTESIAN_POINT ( 'NONE',  ( 1.259306799207500438, -3.058252359239909346, 1.762666431298136605 ) ) ;
#10609 = DIRECTION ( 'NONE',  ( 1.000000000000000000, 0.000000000000000000, 0.000000000000000000 ) ) ;
#10610 = FACE_OUTER_BOUND ( 'NONE', #6385, .T. ) ;
#10611 = CARTESIAN_POINT ( 'NONE',  ( 9.662000818238999145, 3.232852935619000334, -7.903971937289999694 ) ) ;
#10613 = CARTESIAN_POINT ( 'NONE',  ( 4.399744774746779719, 0.1610061330520185519, -1.221142052500258313 ) ) ;
#10612 = CARTESIAN_POINT ( 'NONE',  ( 10.38297570133299885, -3.263119632394200220, 6.817468224793199916 ) ) ;
#10614 = CARTESIAN_POINT ( 'NONE',  ( 4.784193173016666911, 1.460959015002474493, -0.3926218265389176953 ) ) ;
#10615 = ORIENTED_EDGE ( 'NONE', *, *, #5823, .T. ) ;
#10616 = DIRECTION ( 'NONE',  ( 1.000000000000000000, 0.000000000000000000, -1.332267629588000161E-14 ) ) ;
#10617 = CARTESIAN_POINT ( 'NONE',  ( 7.555544676565999040, -2.930005555947998275, 6.552699291324001862 ) ) ;
#10618 = CARTESIAN_POINT ( 'NONE',  ( 9.937659112603999034, 3.444147913214900214, 6.347865960448999090 ) ) ;
#10619 = CARTESIAN_POINT ( 'NONE',  ( 4.950033214355999966, 0.000000000000000000, 0.000000000000000000 ) ) ;
#10620 = CARTESIAN_POINT ( 'NONE',  ( 9.967845797207999681, -2.034786297409000078, 7.636877353231999344 ) ) ;
#10621 = CARTESIAN_POINT ( 'NONE',  ( 17.88880419370435604, 3.028786488651918685, -12.31252201556902470 ) ) ;
#10622 = CARTESIAN_POINT ( 'NONE',  ( 23.50387503050299998, 0.000000000000000000, 0.000000000000000000 ) ) ;
#10623 = AXIS2_PLACEMENT_3D ( 'NONE', #35592, #30014, #69109 ) ;
#10624 = CARTESIAN_POINT ( 'NONE',  ( 25.30000327618300204, 10.83443035398000021, -3.855530949778000149 ) ) ;
#10625 = CARTESIAN_POINT ( 'NONE',  ( 7.100000000000000533, 5.326087788487999575, -7.247035225330000330 ) ) ;
#10626 = AXIS2_PLACEMENT_3D ( 'NONE', #28871, #17322, #33412 ) ;
#10627 = CARTESIAN_POINT ( 'NONE',  ( 9.282063610504998508, -3.644370728184199937, -8.290718512198798962 ) ) ;
#10628 = CARTESIAN_POINT ( 'NONE',  ( 6.153719963560999595, -1.400415568386000009, 0.4419997549869000286 ) ) ;
#10629 = B_SPLINE_SURFACE_WITH_KNOTS ( 'NONE', 3, 3, ( 
 ( #58204, #37225, #27781, #59577 ),
 ( #31994, #65155, #48749, #11678 ),
 ( #58542, #31641, #36888, #6088 ),
 ( #37561, #47724, #58894, #27087 ) ),
 .UNSPECIFIED., .F., .F., .F.,
 ( 4, 4 ),
 ( 4, 4 ),
 ( 0.7363163806532000422, 1.013499456067999960 ),
 ( -0.0005287450254680999126, 0.02696599629895000266 ),
 .UNSPECIFIED. ) ;
#10630 = CARTESIAN_POINT ( 'NONE',  ( 6.999999999999999112, 9.536570502379751346, -4.676103187607473011 ) ) ;
#10631 = FACE_OUTER_BOUND ( 'NONE', #42504, .T. ) ;
#10632 = ORIENTED_EDGE ( 'NONE', *, *, #30154, .T. ) ;
#10633 = CARTESIAN_POINT ( 'NONE',  ( 12.18407639872240189, -0.07155418421575461541, -12.69973420405193032 ) ) ;
#10634 = CARTESIAN_POINT ( 'NONE',  ( 11.78594988689359901, 4.393436444036099786, -8.271690446953899212 ) ) ;
#10635 = CARTESIAN_POINT ( 'NONE',  ( 12.80000000000000071, -11.23412379136000006, 3.084957477885999833 ) ) ;
#10636 = CARTESIAN_POINT ( 'NONE',  ( 3.500000000000000000, -3.033011252059000018, -1.020217008720000207 ) ) ;
#10637 = CARTESIAN_POINT ( 'NONE',  ( 1.696806799207916550, -0.9161175952574931447, 3.408904368339101598 ) ) ;
#10638 = ORIENTED_EDGE ( 'NONE', *, *, #66802, .T. ) ;
#10639 = CARTESIAN_POINT ( 'NONE',  ( 7.558872858590611088, -4.679401687839340518, 8.680096940894596713 ) ) ;
#10640 = EDGE_CURVE ( 'NONE', #67987, #49260, #38656, .T. ) ;
#10641 = CARTESIAN_POINT ( 'NONE',  ( 10.81524174883999834, -4.028418853626810403, -8.533115712456000423 ) ) ;
#10642 = CARTESIAN_POINT ( 'NONE',  ( 18.08681263782093396, 0.3285869677314403048, 12.69428288850128084 ) ) ;
#10643 = CARTESIAN_POINT ( 'NONE',  ( 10.85685100254000091, -2.832432432432000269, -6.822293592207000934 ) ) ;
#10644 = DIRECTION ( 'NONE',  ( -0.8660254037844289376, 0.000000000000000000, 0.5000000000000169864 ) ) ;
#10645 = CARTESIAN_POINT ( 'NONE',  ( 11.02812378248509795, 3.583106837161099900, -6.711274001288999536 ) ) ;
#10646 = VERTEX_POINT ( 'NONE', #12239 ) ;
#10647 = CARTESIAN_POINT ( 'NONE',  ( 9.945535518573000999, -2.906050966242999856, 8.880386511481999534 ) ) ;
#10648 = CARTESIAN_POINT ( 'NONE',  ( 18.06424752491733798, 2.862976204506490596, -13.58975765073224551 ) ) ;
#10649 = VERTEX_POINT ( 'NONE', #22371 ) ;
#10650 = CARTESIAN_POINT ( 'NONE',  ( 13.69997185827400266, 11.40547114375999982, 2.374390024598000082 ) ) ;
#10651 = CARTESIAN_POINT ( 'NONE',  ( 7.903995559621998623, -2.095727472214000020, 8.056487497515000484 ) ) ;
#10652 = CIRCLE ( 'NONE', #35277, 2.000000000000000444 ) ;
#10653 = DIRECTION ( 'NONE',  ( 0.000000000000000000, 0.000000000000000000, -1.000000000000000000 ) ) ;
#10654 = ORIENTED_EDGE ( 'NONE', *, *, #67293, .F. ) ;
#10655 = DIRECTION ( 'NONE',  ( -1.000000000000000000, 0.000000000000000000, 0.000000000000000000 ) ) ;
#10656 = CARTESIAN_POINT ( 'NONE',  ( 7.721970280404999443, 5.390931070480998955, -6.467229401624000396 ) ) ;
#10657 = CARTESIAN_POINT ( 'NONE',  ( 12.09999999999999964, -4.000000000000000000, 7.500000000000000000 ) ) ;
#10658 = CARTESIAN_POINT ( 'NONE',  ( 12.80000000000000071, -11.23412379136000006, 3.084957477885999833 ) ) ;
#10659 = ORIENTED_EDGE ( 'NONE', *, *, #21132, .F. ) ;
#10660 = CARTESIAN_POINT ( 'NONE',  ( 9.877259503622999759, -2.207992199716000137, 7.624813542847999059 ) ) ;
#10661 = CARTESIAN_POINT ( 'NONE',  ( 24.87965957765100100, 11.54628040307999903, -3.248281071505000117 ) ) ;
#10662 = SURFACE_STYLE_FILL_AREA ( #5758 ) ;
#10663 = VERTEX_POINT ( 'NONE', #43368 ) ;
#10664 = EDGE_CURVE ( 'NONE', #59800, #9344, #18000, .T. ) ;
#10665 = CARTESIAN_POINT ( 'NONE',  ( 15.90003771078200145, 3.695138809391000034, 11.25918926437999978 ) ) ;
#10666 = CARTESIAN_POINT ( 'NONE',  ( 10.92546935320999957, -5.641520548727999795, -7.883473948564999390 ) ) ;
#10667 = EDGE_LOOP ( 'NONE', ( #65720, #39584, #29240, #25139 ) ) ;
#10668 = LINE ( 'NONE', #5764, #11927 ) ;
#10669 = CARTESIAN_POINT ( 'NONE',  ( 18.01649462541978508, 0.4224288466528487440, -13.89137824132244425 ) ) ;
#10670 = ADVANCED_FACE ( 'NONE', ( #27976 ), #3952, .F. ) ;
#10671 = CARTESIAN_POINT ( 'NONE',  ( 4.396284230805000526, 0.7308517094458000241, 1.339263914767000019 ) ) ;
#10672 = CARTESIAN_POINT ( 'NONE',  ( 8.207992688182997654, 5.113487315348997697, -6.366574791658999644 ) ) ;
#10673 = FACE_OUTER_BOUND ( 'NONE', #28299, .T. ) ;
#10674 = CARTESIAN_POINT ( 'NONE',  ( 9.406851002546000373, 2.832432432432000269, -6.822293592207000934 ) ) ;
#10675 = CARTESIAN_POINT ( 'NONE',  ( 23.80953365092410579, 13.00795969425658249, 3.692987363579084192 ) ) ;
#10676 = ORIENTED_EDGE ( 'NONE', *, *, #54147, .F. ) ;
#10677 = CARTESIAN_POINT ( 'NONE',  ( 12.99999999998900080, -12.39025855408000076, -1.832244667012999928 ) ) ;
#10678 = ORIENTED_EDGE ( 'NONE', *, *, #59344, .T. ) ;
#10679 = CARTESIAN_POINT ( 'NONE',  ( 10.11260611051000069, 3.359887741436999864, 5.859127722154000573 ) ) ;
#10680 = CARTESIAN_POINT ( 'NONE',  ( 10.87273915876999908, 5.407616985330000681, -8.698399706473999515 ) ) ;
#10681 = CARTESIAN_POINT ( 'NONE',  ( 24.30000000000000071, 0.000000000000000000, 0.000000000000000000 ) ) ;
#10682 = CARTESIAN_POINT ( 'NONE',  ( 12.47202999840589754, 1.970716439074157611, -13.77157652140723165 ) ) ;
#10683 = CARTESIAN_POINT ( 'NONE',  ( 10.34393020684899867, -5.250000000000000000, -7.500000000000000000 ) ) ;
#10684 =( NAMED_UNIT ( * ) PLANE_ANGLE_UNIT ( ) SI_UNIT ( $, .RADIAN. ) );
#10685 = CARTESIAN_POINT ( 'NONE',  ( 17.91964795130430588, -0.5080432161604405694, 13.88750743611951854 ) ) ;
#10686 = AXIS2_PLACEMENT_3D ( 'NONE', #5972, #64696, #38838 ) ;
#10687 = CARTESIAN_POINT ( 'NONE',  ( 9.214598350284001427, -2.899999999999999911, -6.571291218949999902 ) ) ;
#10688 = ORIENTED_EDGE ( 'NONE', *, *, #26456, .F. ) ;
#10689 = CARTESIAN_POINT ( 'NONE',  ( 24.39664176096000148, 8.810499011074819364, -8.810499011034677252 ) ) ;
#10690 = CARTESIAN_POINT ( 'NONE',  ( 10.84995525820099971, -4.107710726525199973, 8.635644537520001052 ) ) ;
#10691 = FACE_OUTER_BOUND ( 'NONE', #44640, .T. ) ;
#10692 = CARTESIAN_POINT ( 'NONE',  ( 9.341483607044001047, -4.148132978932999926, 9.337467253566000380 ) ) ;
#10694 = CARTESIAN_POINT ( 'NONE',  ( 6.355026506350000659, 1.500000000000000000, 0.000000000000000000 ) ) ;
#10693 = CARTESIAN_POINT ( 'NONE',  ( 9.199602729599000384, 2.551394566582000145, 7.536605852160000119 ) ) ;
#10695 = CARTESIAN_POINT ( 'NONE',  ( 10.86687616594229944, 3.655053560864600204, -6.412662853391999818 ) ) ;
#10696 = AXIS2_PLACEMENT_3D ( 'NONE', #23878, #3243, #67546 ) ;
#10697 = CARTESIAN_POINT ( 'NONE',  ( 25.25798371868100034, -11.13205096074000089, 3.460355926395999759 ) ) ;
#10698 = VECTOR ( 'NONE', #37672, 1000.000000000000000 ) ;
#10699 = CARTESIAN_POINT ( 'NONE',  ( 10.10892546752099896, 3.135062625344399834, -7.440072690703440017 ) ) ;
#10700 = CARTESIAN_POINT ( 'NONE',  ( 18.15003166281171332, -0.1916424759571756231, 12.69805926625132209 ) ) ;
#10701 = CARTESIAN_POINT ( 'NONE',  ( 7.094074082186000219, 0.5841380621085999758, 1.131277061175999910 ) ) ;
#10702 = CARTESIAN_POINT ( 'NONE',  ( 24.38581293668700312, 8.886045982725999437, 8.989759919345001293 ) ) ;
#10703 = VERTEX_POINT ( 'NONE', #38456 ) ;
#10704 = CARTESIAN_POINT ( 'NONE',  ( 8.122956853208000538, -3.566638198986999964, 5.743608852252999775 ) ) ;
#10705 = CARTESIAN_POINT ( 'NONE',  ( 8.705995559625000269, -2.542850487891999745, 7.419808283050000064 ) ) ;
#10706 = B_SPLINE_CURVE_WITH_KNOTS ( 'NONE', 3,
 ( #45831, #2834, #62922, #9441 ),
 .UNSPECIFIED., .F., .F.,
 ( 4, 4 ),
 ( 0.000000000000000000, 1.000000000000000000 ),
 .UNSPECIFIED. ) ;
#10707 = LINE ( 'NONE', #225, #9235 ) ;
#10708 = CARTESIAN_POINT ( 'NONE',  ( 10.99338701711408106, 6.182907969993329367, 5.102573636763008125 ) ) ;
#10709 = ORIENTED_EDGE ( 'NONE', *, *, #23791, .T. ) ;
#10710 = CARTESIAN_POINT ( 'NONE',  ( 0.6339629568059000908, 0.7117304887930000490, 3.632629627798000360 ) ) ;
#10711 = CARTESIAN_POINT ( 'NONE',  ( 10.37199293566600034, 4.633387186021100668, 6.723009541442299231 ) ) ;
#10712 = CARTESIAN_POINT ( 'NONE',  ( 3.029203535413000026, 3.757998461040000127, 0.07632091300853000027 ) ) ;
#10713 = ORIENTED_EDGE ( 'NONE', *, *, #10476, .F. ) ;
#10714 = CARTESIAN_POINT ( 'NONE',  ( 12.47371306568758875, -0.6398865404514904043, -12.58374251866278648 ) ) ;
#10715 = CARTESIAN_POINT ( 'NONE',  ( 10.92028665956053324, -4.742415037725373317, -8.549395343567624650 ) ) ;
#10716 = CARTESIAN_POINT ( 'NONE',  ( 17.85685707441188086, 3.134587784889869333, -12.20386770240991581 ) ) ;
#10717 = CARTESIAN_POINT ( 'NONE',  ( 5.624287198480771188, 12.11015306275865733, 3.744045437480294947 ) ) ;
#10718 = CARTESIAN_POINT ( 'NONE',  ( 13.99999999231800096, -8.833253877201999060, -7.896562762484000686 ) ) ;
#10719 = VERTEX_POINT ( 'NONE', #18174 ) ;
#10720 = CARTESIAN_POINT ( 'NONE',  ( 7.837267527055786331, -4.794208482798125281, 6.382611110956646350 ) ) ;
#10721 = ADVANCED_FACE ( 'NONE', ( #12582 ), #44060, .T. ) ;
#10722 = EDGE_CURVE ( 'NONE', #43345, #64217, #41142, .T. ) ;
#10723 = CARTESIAN_POINT ( 'NONE',  ( 7.946970280407001042, 5.256485075641999849, -6.567055966373000153 ) ) ;
#10724 = CARTESIAN_POINT ( 'NONE',  ( 8.415023682605584199, -2.417956104865769618, 8.222459336996642776 ) ) ;
#10725 = CARTESIAN_POINT ( 'NONE',  ( 11.49978667957999967, -12.43119799159999950, -1.530013559959999991 ) ) ;
#10726 = ORIENTED_EDGE ( 'NONE', *, *, #5481, .T. ) ;
#10727 = CARTESIAN_POINT ( 'NONE',  ( 16.04647714749799903, -3.814092932148000159, -11.87318743920999964 ) ) ;
#10728 = B_SPLINE_CURVE_WITH_KNOTS ( 'NONE', 3,
 ( #12365, #61294, #33695, #54665 ),
 .UNSPECIFIED., .F., .F.,
 ( 4, 4 ),
 ( 0.000000000000000000, 1.000000000000000000 ),
 .UNSPECIFIED. ) ;
#10729 = B_SPLINE_CURVE_WITH_KNOTS ( 'NONE', 3,
 ( #60419, #23700, #33855, #40137, #28614, #24044, #50275, #55171, #44353, #2377 ),
 .UNSPECIFIED., .F., .F.,
 ( 4, 2, 2, 2, 4 ),
 ( 0.000000000000000000, 0.2499999999999967804, 0.3749999999999971689, 0.4999999999999975575, 1.000000000000000000 ),
 .UNSPECIFIED. ) ;
#10730 = CARTESIAN_POINT ( 'NONE',  ( 11.48831242699000121, 11.66400889920000061, 1.747256858593000173 ) ) ;
#10731 = ORIENTED_EDGE ( 'NONE', *, *, #57541, .T. ) ;
#10732 = CARTESIAN_POINT ( 'NONE',  ( 11.10000000000000320, 2.488563452597234882, -8.216671174298946667 ) ) ;
#10733 = CARTESIAN_POINT ( 'NONE',  ( 9.865041550948088656, -2.650034642413194419, -7.500002425457253707 ) ) ;
#10734 = VECTOR ( 'NONE', #59322, 1000.000000000000000 ) ;
#10735 = CARTESIAN_POINT ( 'NONE',  ( 9.163298641743953254, 2.899999999999999911, -6.158784435141193114 ) ) ;
#10736 = ORIENTED_EDGE ( 'NONE', *, *, #49392, .T. ) ;
#10737 = CARTESIAN_POINT ( 'NONE',  ( 17.55505043854143565, 1.875000000000000000, 12.57541666120756041 ) ) ;
#10738 = DIRECTION ( 'NONE',  ( 0.000000000000000000, -0.7198977633594745296, 0.6940801180771756229 ) ) ;
#10739 = CARTESIAN_POINT ( 'NONE',  ( 23.85399111800575156, -13.23042136191713958, 3.489530933266961288 ) ) ;
#10740 = CARTESIAN_POINT ( 'NONE',  ( 12.43857111758543788, 3.006687177877848338, -12.31897860641675102 ) ) ;
#10741 = CARTESIAN_POINT ( 'NONE',  ( 10.67349413291699811, -2.837298848764000514, 8.030511425625498134 ) ) ;
#10742 = VERTEX_POINT ( 'NONE', #28315 ) ;
#10743 = CARTESIAN_POINT ( 'NONE',  ( 8.694607780412001219, 5.290207928847999064, 8.768105151414001597 ) ) ;
#10744 = ORIENTED_EDGE ( 'NONE', *, *, #36072, .F. ) ;
#10745 = CARTESIAN_POINT ( 'NONE',  ( 9.979346873516666605, -3.836375382625532904, 6.249999999999999112 ) ) ;
#10746 = CIRCLE ( 'NONE', #6249, 3.199999999999999289 ) ;
#10747 = CARTESIAN_POINT ( 'NONE',  ( 15.86281931570199966, -8.823480018325001950, -8.551042465543998716 ) ) ;
#10748 = DIRECTION ( 'NONE',  ( 0.000000000000000000, 0.000000000000000000, 1.000000000000000000 ) ) ;
#10749 = ORIENTED_EDGE ( 'NONE', *, *, #56665, .T. ) ;
#10750 = CYLINDRICAL_SURFACE ( 'NONE', #41698, 2.200000000000000178 ) ;
#10751 = EDGE_CURVE ( 'NONE', #47043, #64287, #27630, .T. ) ;
#10752 = CARTESIAN_POINT ( 'NONE',  ( 11.00000000000000000, 4.000000000000000000, 7.500000000000000000 ) ) ;
#10753 = DIRECTION ( 'NONE',  ( 0.000000000000000000, -1.000000000000000000, 0.000000000000000000 ) ) ;
#10754 = CARTESIAN_POINT ( 'NONE',  ( 10.77934687351631382, 3.836375382625536012, 8.750000000000001776 ) ) ;
#10755 = CARTESIAN_POINT ( 'NONE',  ( 12.54752909501217673, -1.835309592424128056, -13.87918066653183224 ) ) ;
#10756 = CARTESIAN_POINT ( 'NONE',  ( 11.78179573085659904, -3.026866171144600326, -7.668383662421899061 ) ) ;
#10757 = CYLINDRICAL_SURFACE ( 'NONE', #31958, 1.250000000000000222 ) ;
#10758 = CARTESIAN_POINT ( 'NONE',  ( 17.94028104512299393, -3.089952709746686121, 12.21524586714252969 ) ) ;
#10760 = VERTEX_POINT ( 'NONE', #48951 ) ;
#10759 = B_SPLINE_CURVE_WITH_KNOTS ( 'NONE', 3,
 ( #619, #43267, #64574, #16685, #38013, #59338, #35541, #35201, #56511, #8617, #3025, #61752, #66654, #29966, #13870, #55831, #7935, #19104, #40770, #51267, #7584, #50583, #45345, #40426, #39753, #29271, #12838, #14212, #28933, #62094, #3363 ),
 .UNSPECIFIED., .F., .F.,
 ( 4, 2, 2, 1, 1, 2, 2, 2, 1, 2, 2, 2, 2, 2, 2, 2, 4 ),
 ( 0.000000000000000000, 0.06250000000002108036, 0.09375000000003078093, 0.1093750000000356382, 0.1171875000000380668, 0.1210937500000392325, 0.1250000000000403844, 0.1875000000000528744, 0.2187500000000581757, 0.2343750000000596745, 0.2500000000000611733, 0.3750000000000564548, 0.4375000000000552891, 0.4687500000000547340, 0.5000000000000541789, 0.7500000000000270894, 1.000000000000000000 ),
 .UNSPECIFIED. ) ;
#10761 = CARTESIAN_POINT ( 'NONE',  ( 11.12438586031000121, -5.546372646562000241, -5.163676736721000360 ) ) ;
#10762 = VERTEX_POINT ( 'NONE', #33912 ) ;
#10763 = DIRECTION ( 'NONE',  ( 0.000000000000000000, 0.000000000000000000, 1.000000000000000000 ) ) ;
#10764 = LINE ( 'NONE', #5522, #23298 ) ;
#10765 = CARTESIAN_POINT ( 'NONE',  ( 12.80505043854144276, -0.6951438842159466391, -13.94765567169527998 ) ) ;
#10766 = CARTESIAN_POINT ( 'NONE',  ( 10.87696123885999810, 5.827079664135999870, -7.814747088295999511 ) ) ;
#10767 = CARTESIAN_POINT ( 'NONE',  ( 10.40879003340999986, -3.093879171920000282, -6.480773124728999690 ) ) ;
#10768 = DIRECTION ( 'NONE',  ( 1.000000000000000000, 0.000000000000000000, 0.000000000000000000 ) ) ;
#10769 = CARTESIAN_POINT ( 'NONE',  ( 23.68247649694000145, -13.13665233500999996, 3.950736996479999874 ) ) ;
#10770 = CARTESIAN_POINT ( 'NONE',  ( 8.748004441081999261, 3.610923974646400136, -8.341443180570399463 ) ) ;
#10771 = ORIENTED_EDGE ( 'NONE', *, *, #60141, .T. ) ;
#10772 = FACE_OUTER_BOUND ( 'NONE', #62901, .T. ) ;
#10773 = CARTESIAN_POINT ( 'NONE',  ( 10.68403803949000164, 5.436614310638000269, 8.578436083822998270 ) ) ;
#10774 = CARTESIAN_POINT ( 'NONE',  ( 2.300973465875999935, -3.500000000000000000, 0.000000000000000000 ) ) ;
#10775 = CARTESIAN_POINT ( 'NONE',  ( 11.35679632507500081, -3.509334349252600127, 6.590394082213600235 ) ) ;
#10776 = CARTESIAN_POINT ( 'NONE',  ( 18.53960231418900051, 2.682082126742999950, -11.29772413421000188 ) ) ;
#10777 = CARTESIAN_POINT ( 'NONE',  ( 11.68748876160954886, 3.399618311400500303, -8.124372018288600117 ) ) ;
#10778 = AXIS2_PLACEMENT_3D ( 'NONE', #27790, #17285, #54691 ) ;
#10779 = B_SPLINE_CURVE_WITH_KNOTS ( 'NONE', 3,
 ( #48763, #38267, #63798, #37924 ),
 .UNSPECIFIED., .F., .F.,
 ( 4, 4 ),
 ( 0.000000000000000000, 1.000000000000000000 ),
 .UNSPECIFIED. ) ;
#10780 = CARTESIAN_POINT ( 'NONE',  ( 12.20096618732085680, -0.1616215023347950530, 12.69863621249087871 ) ) ;
#10781 = STYLED_ITEM ( 'NONE', ( #46969 ), #8521 ) ;
#10782 = ADVANCED_FACE ( 'NONE', ( #59430 ), #32530, .T. ) ;
#10783 = EDGE_CURVE ( 'NONE', #4475, #64347, #16113, .T. ) ;
#10784 = CARTESIAN_POINT ( 'NONE',  ( 8.211023395313091555, 4.489943607116844149, -8.784467515373197699 ) ) ;
#10785 = DIRECTION ( 'NONE',  ( 1.000000000000000000, 0.000000000000000000, -1.776356839443000099E-14 ) ) ;
#10786 = AXIS2_PLACEMENT_3D ( 'NONE', #6417, #27767, #18307 ) ;
#10787 = VERTEX_POINT ( 'NONE', #27284 ) ;
#10788 = CARTESIAN_POINT ( 'NONE',  ( 8.871410841230998656, 2.721111233225000259, -6.936528696292000085 ) ) ;
#10789 = CARTESIAN_POINT ( 'NONE',  ( 9.925159544971000614, -4.365624317997999881, -9.242254741729000855 ) ) ;
#10790 = CARTESIAN_POINT ( 'NONE',  ( 17.78650313621483647, 3.080655036186602302, 13.53295239609827050 ) ) ;
#10791 = CARTESIAN_POINT ( 'NONE',  ( 9.281866024821542993, 3.294723229065558368, -8.705120403943604757 ) ) ;
#10792 = CARTESIAN_POINT ( 'NONE',  ( 8.205992358813000820, 3.399999999999999911, 6.138278517057000450 ) ) ;
#10793 = CARTESIAN_POINT ( 'NONE',  ( 10.52226222744799955, -4.880489021643899861, -8.225278704382400718 ) ) ;
#10794 = ORIENTED_EDGE ( 'NONE', *, *, #6608, .T. ) ;
#10795 = AXIS2_PLACEMENT_3D ( 'NONE', #59299, #48131, #64193 ) ;
#10796 = DIRECTION ( 'NONE',  ( 1.000000000000000000, 0.000000000000000000, 0.000000000000000000 ) ) ;
#10797 = FACE_OUTER_BOUND ( 'NONE', #42084, .T. ) ;
#10800 = UNCERTAINTY_MEASURE_WITH_UNIT (LENGTH_MEASURE( 1.000000000000000082E-05 ), #56258, 'distance_accuracy_value', 'NONE');
#10799 = DIRECTION ( 'NONE',  ( 1.000000000000000000, 0.000000000000000000, 0.000000000000000000 ) ) ;
#10798 = CARTESIAN_POINT ( 'NONE',  ( 9.351420280414000530, 4.953415418491999844, -8.946479654552000227 ) ) ;
#10801 = CARTESIAN_POINT ( 'NONE',  ( 2.310450118812109377, 2.961138536375865993, 1.358551000647025164 ) ) ;
#10802 = ORIENTED_EDGE ( 'NONE', *, *, #46092, .F. ) ;
#10803 = CARTESIAN_POINT ( 'NONE',  ( 9.869051220224999810, 5.575171928796999410, 7.724300137354000562 ) ) ;
#10804 = CARTESIAN_POINT ( 'NONE',  ( 17.86935674558758080, -3.040604463256959544, -13.54376658945627021 ) ) ;
#10805 = CARTESIAN_POINT ( 'NONE',  ( 10.84641504065830020, 4.804462279649600376, 8.099826052678000821 ) ) ;
#10806 = CARTESIAN_POINT ( 'NONE',  ( 11.18483536755999808, -2.599651619047000040, 7.740676724427999922 ) ) ;
#10807 = CARTESIAN_POINT ( 'NONE',  ( 8.192495559623999668, -2.550228841911000188, 7.666975032000999946 ) ) ;
#10808 = ORIENTED_EDGE ( 'NONE', *, *, #59257, .T. ) ;
#10809 = CARTESIAN_POINT ( 'NONE',  ( 9.059364158773000497, 4.192919163547999872, 5.525472271700999194 ) ) ;
#10810 = EDGE_CURVE ( 'NONE', #65610, #21934, #30057, .T. ) ;
#10811 = EDGE_CURVE ( 'NONE', #10372, #47157, #15743, .T. ) ;
#10813 = CARTESIAN_POINT ( 'NONE',  ( 10.39539435320999949, -5.667179153637999178, -7.250689665673000661 ) ) ;
#10812 = CARTESIAN_POINT ( 'NONE',  ( 13.70003001321900271, 10.86123379505843545, 6.319444516909296539 ) ) ;
#10814 = CARTESIAN_POINT ( 'NONE',  ( 7.773757704034534477, -5.028764116645290549, 8.902433763654059362 ) ) ;
#10815 = CARTESIAN_POINT ( 'NONE',  ( 9.877259503622999759, -2.207992199716000137, 7.624813542847999059 ) ) ;
#10816 = CARTESIAN_POINT ( 'NONE',  ( 24.56914408408099959, 3.716987283419999955, 12.37180464569999927 ) ) ;
#10817 = ORIENTED_EDGE ( 'NONE', *, *, #33229, .F. ) ;
#10818 = CARTESIAN_POINT ( 'NONE',  ( 9.571013540182331525, 4.768183399968643599, -8.499583552997725278 ) ) ;
#10819 = EDGE_CURVE ( 'NONE', #7211, #55031, #42739, .T. ) ;
#10820 = CARTESIAN_POINT ( 'NONE',  ( 11.46533729122639933, -5.140346530769000388, 7.529998433785960010 ) ) ;
#10821 = CARTESIAN_POINT ( 'NONE',  ( 10.20226357027499908, 5.120085139777000194, 7.283900408233900059 ) ) ;
#10822 = ORIENTED_EDGE ( 'NONE', *, *, #17260, .F. ) ;
#10823 = SHAPE_REPRESENTATION ( 'MAS-678', ( #64176, #68622, #67527, #19533, #20675, #40732, #5000, #65285, #61951, #29638, #12851, #68664, #56368, #29583, #66433 ), #9485 ) ;
#10824 = CARTESIAN_POINT ( 'NONE',  ( 8.763579719593998618, 4.815598936798999752, -8.835641302565999666 ) ) ;
#10825 = CARTESIAN_POINT ( 'NONE',  ( 6.999999692086999126, -12.89129024276999935, 1.677687656890000101 ) ) ;
#10826 = CARTESIAN_POINT ( 'NONE',  ( 12.01656039236534923, -2.826501801118000312, 7.442888368925779652 ) ) ;
#10827 = CARTESIAN_POINT ( 'NONE',  ( 24.77999963990900056, -3.612931897559000127, -12.08259271626999976 ) ) ;
#10828 = AXIS2_PLACEMENT_3D ( 'NONE', #1157, #44852, #1849 ) ;
#10829 = CARTESIAN_POINT ( 'NONE',  ( 18.13616101482883636, 2.730220173529687600, -13.62193317606529241 ) ) ;
#10830 = ORIENTED_EDGE ( 'NONE', *, *, #44622, .T. ) ;
#10831 = CARTESIAN_POINT ( 'NONE',  ( 9.683745612763171806, 2.796157461452848825, 8.204744624355011950 ) ) ;
#10832 = CARTESIAN_POINT ( 'NONE',  ( 23.58885147429595719, 10.33108476000267828, 9.338978122152829187 ) ) ;
#10833 = ORIENTED_EDGE ( 'NONE', *, *, #16868, .F. ) ;
#10834 = FACE_OUTER_BOUND ( 'NONE', #3695, .T. ) ;
#10835 = EDGE_CURVE ( 'NONE', #2041, #33857, #55924, .T. ) ;
#10836 = CARTESIAN_POINT ( 'NONE',  ( 10.62487750876920067, 3.456442671114800191, 6.656497609330299881 ) ) ;
#10837 =( GEOMETRIC_REPRESENTATION_CONTEXT ( 3 ) GLOBAL_UNCERTAINTY_ASSIGNED_CONTEXT ( ( #42289 ) ) GLOBAL_UNIT_ASSIGNED_CONTEXT ( ( #24874, #46887, #45858 ) ) REPRESENTATION_CONTEXT ( 'NONE', 'WORKASPACE' ) );
#10838 = CARTESIAN_POINT ( 'NONE',  ( 10.30204095393054509, 2.650238144765166837, -7.719132294906656533 ) ) ;
#10839 = CARTESIAN_POINT ( 'NONE',  ( 10.26368708477999903, 4.794139572939999816, -8.804452601708000259 ) ) ;
#10840 = LINE ( 'NONE', #38094, #61709 ) ;
#10841 = CARTESIAN_POINT ( 'NONE',  ( 10.55813551225999980, -2.466564559586000183, 6.633531786299999844 ) ) ;
#10842 = CARTESIAN_POINT ( 'NONE',  ( 17.77532606275349636, 0.5849872192492382439, -12.68185863724643170 ) ) ;
#10843 = CIRCLE ( 'NONE', #46586, 2.999989272562999965 ) ;
#10844 = CARTESIAN_POINT ( 'NONE',  ( 9.040632417955841049, 4.918936971883569598, 8.488836720954758164 ) ) ;
#10845 = CARTESIAN_POINT ( 'NONE',  ( 11.01872200990539952, -4.947480442174099657, -7.169497859994799605 ) ) ;
#10846 = CARTESIAN_POINT ( 'NONE',  ( 7.571670280409000142, 2.531201476950000195, 8.216704145297999418 ) ) ;
#10847 = VERTEX_POINT ( 'NONE', #66400 ) ;
#10848 = CARTESIAN_POINT ( 'NONE',  ( 11.59999999999999964, 4.000000000000000000, 7.500000000000000000 ) ) ;
#10849 = CARTESIAN_POINT ( 'NONE',  ( 11.00294879349999988, 5.167578603197999776, -4.969641262464000953 ) ) ;
#10850 = CARTESIAN_POINT ( 'NONE',  ( 7.888294342220998345, 2.872416928457999674, -6.735169506715999788 ) ) ;
#10851 = CARTESIAN_POINT ( 'NONE',  ( 18.26132062505687159, 2.644858796842615156, 12.31930452622237127 ) ) ;
#10852 = CARTESIAN_POINT ( 'NONE',  ( 19.99999987597299977, 1.497200531649000015E-13, 3.463895836829999943E-14 ) ) ;
#10853 = CARTESIAN_POINT ( 'NONE',  ( 10.95881151040999946, 8.162134461319000778, 6.507868381347999609 ) ) ;
#10854 = AXIS2_PLACEMENT_3D ( 'NONE', #64032, #54596, #11247 ) ;
#10855 = CARTESIAN_POINT ( 'NONE',  ( 9.231612022449091626, -2.652299246284962830, 7.391249027395923932 ) ) ;
#10856 = FACE_OUTER_BOUND ( 'NONE', #27986, .T. ) ;
#10857 = ORIENTED_EDGE ( 'NONE', *, *, #35469, .T. ) ;
#10858 = CARTESIAN_POINT ( 'NONE',  ( 24.60170725920900026, 8.811863727701000570, 9.296544040758000449 ) ) ;
#10859 = CARTESIAN_POINT ( 'NONE',  ( 9.783671671056998420, -5.126041103316000047, -7.689118697196099639 ) ) ;
#10860 = CARTESIAN_POINT ( 'NONE',  ( 10.10000011340999926, -1.190159082397999942E-13, -12.39999890530012117 ) ) ;
#10861 = DIRECTION ( 'NONE',  ( 1.000000000000000000, 0.000000000000000000, 0.000000000000000000 ) ) ;
#10862 = CARTESIAN_POINT ( 'NONE',  ( 11.44487616594229884, -4.303437140848100029, 8.456491899811199531 ) ) ;
#10863 = CARTESIAN_POINT ( 'NONE',  ( 11.58071932425156980, 3.832730087831799803, -8.628410767520000135 ) ) ;
#10864 = CARTESIAN_POINT ( 'NONE',  ( 8.748305582559998683, 4.091272957481129957, 6.637573130164000190 ) ) ;
#10865 = ADVANCED_FACE ( 'NONE', ( #25129 ), #67762, .T. ) ;
#10866 = ADVANCED_FACE ( 'NONE', ( #62189 ), #34612, .T. ) ;
#10867 = CARTESIAN_POINT ( 'NONE',  ( 0.4912272458363000083, -2.390579753276000030, 2.141564200098999837 ) ) ;
#10868 = FACE_OUTER_BOUND ( 'NONE', #60542, .T. ) ;
#10869 = CARTESIAN_POINT ( 'NONE',  ( 12.09902206169133265, 2.644659774828324039, 12.31933076163361207 ) ) ;
#10871 = DIRECTION ( 'NONE',  ( 0.000000000000000000, 0.000000000000000000, -1.000000000000000000 ) ) ;
#10870 = CARTESIAN_POINT ( 'NONE',  ( 10.18893802597399834, 3.406370524467499994, -6.524634174392399899 ) ) ;
#10872 = EDGE_CURVE ( 'NONE', #52078, #13783, #30275, .T. ) ;
#10873 = CARTESIAN_POINT ( 'NONE',  ( 11.23610538575739959, 5.109472165990999848, -7.234742334405199315 ) ) ;
#10874 = CARTESIAN_POINT ( 'NONE',  ( 7.698447294381004724, 2.921226879009002797, -6.534475276641003916 ) ) ;
#10875 = CARTESIAN_POINT ( 'NONE',  ( 10.39539221959000059, 5.667182949051000840, -7.250689098107000241 ) ) ;
#10876 = LINE ( 'NONE', #17149, #61698 ) ;
#10878 = DIRECTION ( 'NONE',  ( 1.000000000000000000, 0.000000000000000000, 0.000000000000000000 ) ) ;
#10877 = CARTESIAN_POINT ( 'NONE',  ( 12.09999999995609521, 11.00695867686506269, -3.817557009248758959 ) ) ;
#10879 = CARTESIAN_POINT ( 'NONE',  ( 8.015378205837999204, 5.116433164263000322, -6.698485005943000559 ) ) ;
#10880 = VERTEX_POINT ( 'NONE', #46462 ) ;
#10881 = AXIS2_PLACEMENT_3D ( 'NONE', #51161, #30866, #25617 ) ;
#10882 = CARTESIAN_POINT ( 'NONE',  ( 12.20957360714451490, 0.1900975197669926287, 12.69808960362405870 ) ) ;
#10883 = CARTESIAN_POINT ( 'NONE',  ( 23.60000000000000142, -9.289189189551001036, 7.908916752675001050 ) ) ;
#10884 = MECHANICAL_DESIGN_GEOMETRIC_PRESENTATION_REPRESENTATION (  '', ( #9788 ), #31010 ) ;
#10885 = CARTESIAN_POINT ( 'NONE',  ( 17.60358162561344741, 0.7192569394295647012, -12.57945425907935366 ) ) ;
#10886 = CARTESIAN_POINT ( 'NONE',  ( 9.070430433046999141, 3.262177192690499883, 7.955330044604899342 ) ) ;
#10888 = CARTESIAN_POINT ( 'NONE',  ( 12.49074413817431406, -3.040604467177681958, 13.54382360563873000 ) ) ;
#10887 = AXIS2_PLACEMENT_3D ( 'NONE', #62049, #25328, #35491 ) ;
#10889 = CARTESIAN_POINT ( 'NONE',  ( 12.18428608238131794, 2.573446268032343998, 13.65756128989349349 ) ) ;
#10890 = CARTESIAN_POINT ( 'NONE',  ( 10.22514748322308797, 2.649941783575544108, 7.500008211948054893 ) ) ;
#10891 = ORIENTED_EDGE ( 'NONE', *, *, #65478, .F. ) ;
#10892 = CARTESIAN_POINT ( 'NONE',  ( 4.524321680877999796, 0.9196732308882999973, -0.6641588674314000684 ) ) ;
#10893 = CARTESIAN_POINT ( 'NONE',  ( 11.35565467195930367, -5.136173005413449566, -6.911917091190551865 ) ) ;
#10894 = CONICAL_SURFACE ( 'NONE', #15347, 12.47499939740000130, 0.7853981102588313279 ) ;
#10895 = CARTESIAN_POINT ( 'NONE',  ( 25.26995024675264290, 3.169784517860001039, 11.48334038991926320 ) ) ;
#10896 = CARTESIAN_POINT ( 'NONE',  ( 10.26685100253999927, 2.832432432432000269, 6.822293592207000934 ) ) ;
#10897 = EDGE_CURVE ( 'NONE', #47885, #49595, #60329, .T. ) ;
#10898 = CARTESIAN_POINT ( 'NONE',  ( 17.86072591669549681, 3.045244688009580702, -12.30767216807748810 ) ) ;
#10899 = CARTESIAN_POINT ( 'NONE',  ( 9.599999931441001166, -2.753634353389999845, 7.595250590283559866 ) ) ;
#10900 = CARTESIAN_POINT ( 'NONE',  ( 11.73671932425159881, 3.872987101045399783, 6.643164954553199664 ) ) ;
#10901 = AXIS2_PLACEMENT_3D ( 'NONE', #60432, #50288, #27935 ) ;
#10902 = CARTESIAN_POINT ( 'NONE',  ( 9.317462135714000837, -5.100000000000000533, 6.571291218949999902 ) ) ;
#10903 = CARTESIAN_POINT ( 'NONE',  ( 10.22094314679000071, -2.563075248996000255, -8.004105227364998854 ) ) ;
#10904 = CARTESIAN_POINT ( 'NONE',  ( 11.30671024775549505, 4.620655945117460028, -8.119376818724933997 ) ) ;
#10905 = B_SPLINE_SURFACE_WITH_KNOTS ( 'NONE', 3, 3, ( 
 ( #57282, #35298, #56613, #41559 ),
 ( #67428, #30731, #19553, #40871 ),
 ( #52038, #25477, #46809, #14315 ),
 ( #35641, #68115, #5527, #47498 ),
 ( #10769, #32453, #26867, #59018 ),
 ( #64589, #42593, #63207, #63902 ),
 ( #48181, #4830, #31419, #636 ),
 ( #52736, #68452, #47847, #16016 ),
 ( #285, #16699, #21944, #38026 ),
 ( #52387, #59353, #31082, #26517 ),
 ( #43283, #20574, #57984, #4482 ),
 ( #32114, #16359, #25822, #47153 ) ),
 .UNSPECIFIED., .F., .F., .F.,
 ( 4, 1, 1, 1, 1, 1, 1, 1, 1, 4 ),
 ( 4, 4 ),
 ( 0.5527591097492000616, 0.5999999999999999778, 0.6500000000000000222, 0.6999999999999999556, 0.7500000000000000000, 0.8000000000000000444, 0.8499999999999999778, 0.9000000000000000222, 0.9499999999999999556, 0.9893860793656999997 ),
 ( -0.2706700118377999842, 1.270791066829999982 ),
 .UNSPECIFIED. ) ;
#10906 = CARTESIAN_POINT ( 'NONE',  ( 25.60000000000000142, 2.023980670379999847, 11.01542190082000161 ) ) ;
#10907 = CARTESIAN_POINT ( 'NONE',  ( 24.41555930013399944, 12.00270549100999951, 3.255728780632000330 ) ) ;
#10908 = CARTESIAN_POINT ( 'NONE',  ( 17.80000000005199823, -3.345268251980999974, 11.86064071431999878 ) ) ;
#10909 = ORIENTED_EDGE ( 'NONE', *, *, #48802, .F. ) ;
#10910 = CARTESIAN_POINT ( 'NONE',  ( 9.839810841229999383, 5.817107086401000160, -6.945352709928000579 ) ) ;
#10911 = CARTESIAN_POINT ( 'NONE',  ( 11.03057053952199951, -4.340412141385700195, 8.296503712697200328 ) ) ;
#10912 = ORIENTED_EDGE ( 'NONE', *, *, #4642, .T. ) ;
#10913 = CARTESIAN_POINT ( 'NONE',  ( 25.30000327618300204, 10.83443035398000021, -3.855530949778000149 ) ) ;
#10914 = CARTESIAN_POINT ( 'NONE',  ( 10.54687750876899877, -4.617914354660699772, -8.458891008702400072 ) ) ;
#10915 = ORIENTED_EDGE ( 'NONE', *, *, #62650, .T. ) ;
#10916 = CARTESIAN_POINT ( 'NONE',  ( 11.43856039236529831, 5.032284719763000069, 7.449760924956519759 ) ) ;
#10917 = DIRECTION ( 'NONE',  ( -0.7071067811864950592, 0.6115519262857961325, 0.3549707614102975417 ) ) ;
#10918 = ADVANCED_FACE ( 'NONE', ( #67423 ), #18522, .F. ) ;
#10919 = CARTESIAN_POINT ( 'NONE',  ( 23.94496671461785198, 3.343214108386058037, -12.85026700558185020 ) ) ;
#10920 = CARTESIAN_POINT ( 'NONE',  ( 8.704862649514634398, -2.649860810595624283, 7.852951878455955992 ) ) ;
#10921 = B_SPLINE_CURVE_WITH_KNOTS ( 'NONE', 3,
 ( #19220, #2458, #19574, #50013 ),
 .UNSPECIFIED., .F., .F.,
 ( 4, 4 ),
 ( 0.000000000000000000, 1.000000000000000000 ),
 .UNSPECIFIED. ) ;
#10922 = CYLINDRICAL_SURFACE ( 'NONE', #3206, 0.6250000000000005551 ) ;
#10923 = CARTESIAN_POINT ( 'NONE',  ( 12.33073330736950268, 0.4072264705458581990, -13.89197624348239479 ) ) ;
#10924 = CARTESIAN_POINT ( 'NONE',  ( 7.263286839971717868, -0.7590492731972352525, 0.8424490475276925627 ) ) ;
#10925 = CARTESIAN_POINT ( 'NONE',  ( 9.819572261909000233, -2.688237737290000151, -7.873041261681999359 ) ) ;
#10926 = CARTESIAN_POINT ( 'NONE',  ( 13.46242637979000101, 11.63956415132000011, 2.420148064723000481 ) ) ;
#10927 = VERTEX_POINT ( 'NONE', #8028 ) ;
#10928 = VECTOR ( 'NONE', #19448, 1000.000000000000000 ) ;
#10929 = CARTESIAN_POINT ( 'NONE',  ( 8.639360841228999277, 5.074768364528000397, -8.296267706722000312 ) ) ;
#10930 = ORIENTED_EDGE ( 'NONE', *, *, #48616, .F. ) ;
#10931 = CARTESIAN_POINT ( 'NONE',  ( 0.3034990810464371913, 3.062178106342674067, 1.095474795892486197 ) ) ;
#10932 = DIRECTION ( 'NONE',  ( 1.000000000000000000, 0.000000000000000000, 0.000000000000000000 ) ) ;
#10933 = VERTEX_POINT ( 'NONE', #34950 ) ;
#10934 = CARTESIAN_POINT ( 'NONE',  ( 9.503988259786000370, 3.832626376493700082, 6.231784538167999266 ) ) ;
#10935 = CARTESIAN_POINT ( 'NONE',  ( 17.96903643132316475, -2.968342805378974436, -12.33002008018445039 ) ) ;
#10936 = AXIS2_PLACEMENT_3D ( 'NONE', #37296, #38323, #16996 ) ;
#10937 = CARTESIAN_POINT ( 'NONE',  ( 16.39999999231800132, 3.216285993016000155, 11.40340220863999932 ) ) ;
#10938 = CARTESIAN_POINT ( 'NONE',  ( 10.28976354018291239, 3.672815144550904076, -6.282534154164603812 ) ) ;
#10939 = CARTESIAN_POINT ( 'NONE',  ( 18.17813554645151797, -2.450019327192359597, -12.46306814186711520 ) ) ;
#10940 = CARTESIAN_POINT ( 'NONE',  ( 12.60368798324988582, 0.5920240553917486270, 13.88302649426328372 ) ) ;
#10941 = EDGE_LOOP ( 'NONE', ( #13440, #60992, #66888, #61211, #37071, #38839, #59162, #66443, #32146 ) ) ;
#10942 = CARTESIAN_POINT ( 'NONE',  ( 5.699999772733999492, -12.03770622561999915, -3.722046322334000124 ) ) ;
#10943 = CARTESIAN_POINT ( 'NONE',  ( 18.36290965255400209, 11.69601057336999972, -4.586677359659000253 ) ) ;
#10944 = CARTESIAN_POINT ( 'NONE',  ( 9.252229279041625176, 4.091138914130668880, 6.629812682664218748 ) ) ;
#10945 = AXIS2_PLACEMENT_3D ( 'NONE', #24060, #51655, #2735 ) ;
#10946 = CARTESIAN_POINT ( 'NONE',  ( 5.153205201823999992, -0.3383038778767000210, 1.221805324548000060 ) ) ;
#10947 = CARTESIAN_POINT ( 'NONE',  ( 9.157839096883044760, 2.900038627299713401, -6.157793193892236339 ) ) ;
#10948 = CARTESIAN_POINT ( 'NONE',  ( 18.31992917194613213, 12.02644019082415738, -3.499704873216455070 ) ) ;
#10949 = CARTESIAN_POINT ( 'NONE',  ( 9.910158555493998378, -2.531067292016000003, -7.917737669614999696 ) ) ;
#10950 = EDGE_CURVE ( 'NONE', #1282, #61413, #35635, .T. ) ;
#10951 = EDGE_CURVE ( 'NONE', #59568, #20805, #35329, .T. ) ;
#10952 = ORIENTED_EDGE ( 'NONE', *, *, #37520, .T. ) ;
#10953 = ORIENTED_EDGE ( 'NONE', *, *, #38738, .T. ) ;
#10954 = CARTESIAN_POINT ( 'NONE',  ( 11.04499918239000067, 5.245459939894999479, -5.176258674916000224 ) ) ;
#10955 = CARTESIAN_POINT ( 'NONE',  ( 11.09999999999999964, 0.000000000000000000, 0.000000000000000000 ) ) ;
#10956 = CARTESIAN_POINT ( 'NONE',  ( 18.00383897971941138, -1.936685752059260190, 13.86556672038733851 ) ) ;
#10957 = EDGE_CURVE ( 'NONE', #59953, #66816, #65983, .T. ) ;
#10958 = ADVANCED_FACE ( 'NONE', ( #60819 ), #23575, .T. ) ;
#10959 = CYLINDRICAL_SURFACE ( 'NONE', #3416, 3.500000000000000000 ) ;
#10960 = CARTESIAN_POINT ( 'NONE',  ( 24.48513460874600156, 8.805438997290998770, -8.922423169716999780 ) ) ;
#10961 = CARTESIAN_POINT ( 'NONE',  ( 11.84388784977539899, 2.744254309011999737, -7.428242901739219306 ) ) ;
#10962 = CARTESIAN_POINT ( 'NONE',  ( 9.611342523874998989, 3.142972170141900001, -7.368808371628100318 ) ) ;
#10964 = CARTESIAN_POINT ( 'NONE',  ( 4.399614530587001582, 1.347590462918873522, 0.6451537652597036931 ) ) ;
#10963 = CARTESIAN_POINT ( 'NONE',  ( 10.90644474310099810, -3.106516218291800246, 7.066400461213500073 ) ) ;
#10965 = CARTESIAN_POINT ( 'NONE',  ( 4.763359839683333874, 1.310679582531388387, -0.7554284705563470981 ) ) ;
#10966 = ORIENTED_EDGE ( 'NONE', *, *, #35752, .F. ) ;
#10967 = AXIS2_PLACEMENT_3D ( 'NONE', #64081, #5706, #32635 ) ;
#10968 = CARTESIAN_POINT ( 'NONE',  ( 7.682778389973002220, -3.526905737521000006, 6.475916620580998817 ) ) ;
#10969 = CARTESIAN_POINT ( 'NONE',  ( 9.536892889968999754, -5.099406281193999746, -6.669356233738001016 ) ) ;
#10970 = CARTESIAN_POINT ( 'NONE',  ( 11.09999999999999964, 6.520421007963999926, -5.525576379744999933 ) ) ;
#10971 = CARTESIAN_POINT ( 'NONE',  ( 9.939319226872999735, -2.638101016021999978, 6.328632621050000573 ) ) ;
#10972 = CARTESIAN_POINT ( 'NONE',  ( 18.08168818186308258, 2.836704670500534764, -12.36674034546831891 ) ) ;
#10973 = DIRECTION ( 'NONE',  ( 0.000000000000000000, 0.000000000000000000, -1.000000000000000000 ) ) ;
#10974 = ADVANCED_FACE ( 'NONE', ( #66748 ), #31364, .T. ) ;
#10975 = CARTESIAN_POINT ( 'NONE',  ( 7.207719739968999839, 8.269775584676999358, -4.413073181476000251 ) ) ;
#10976 = CARTESIAN_POINT ( 'NONE',  ( 9.130088727410999638, -4.863977618062000019, -7.572461161969050281 ) ) ;
#10977 = CARTESIAN_POINT ( 'NONE',  ( 6.736818577609000158, -1.197190821580000009, 0.3103650564550000102 ) ) ;
#10978 = LINE ( 'NONE', #144, #6400 ) ;
#10979 = CARTESIAN_POINT ( 'NONE',  ( 18.20426522485155729, 2.108767964823663910, 12.42302121883312793 ) ) ;
#10980 = ORIENTED_EDGE ( 'NONE', *, *, #65651, .T. ) ;
#10981 = CARTESIAN_POINT ( 'NONE',  ( 12.18004360525213414, 0.009762034906139017282, -12.70000045436731995 ) ) ;
#10982 = CARTESIAN_POINT ( 'NONE',  ( 11.66287348028854964, 3.238044298475899918, -7.911973420841600380 ) ) ;
#10983 = CARTESIAN_POINT ( 'NONE',  ( 6.799999999999999822, -9.295462635088998837, -5.399710584805999858 ) ) ;
#10985 = CARTESIAN_POINT ( 'NONE',  ( 7.773264469372000107, 2.859518616742000141, 6.768376720750000075 ) ) ;
#10984 =( GEOMETRIC_REPRESENTATION_CONTEXT ( 3 ) GLOBAL_UNCERTAINTY_ASSIGNED_CONTEXT ( ( #21292 ) ) GLOBAL_UNIT_ASSIGNED_CONTEXT ( ( #8573, #45978, #45304 ) ) REPRESENTATION_CONTEXT ( 'NONE', 'WORKASPACE' ) );
#10986 = CARTESIAN_POINT ( 'NONE',  ( 10.28172590881818671, 3.320041345952004175, -8.679799923475062684 ) ) ;
#10987 = ORIENTED_EDGE ( 'NONE', *, *, #45316, .T. ) ;
#10988 = CARTESIAN_POINT ( 'NONE',  ( 25.52347087181200180, -11.21067381750000003, -3.136870539691000381 ) ) ;
#10989 = CARTESIAN_POINT ( 'NONE',  ( 11.11123293495519881, -4.891405920092699589, -7.464165716332529676 ) ) ;
#10990 = DIRECTION ( 'NONE',  ( -0.000000000000000000, -0.000000000000000000, 1.000000000000000000 ) ) ;
#10991 = CARTESIAN_POINT ( 'NONE',  ( 17.55505043854144276, 0.7192913403693119712, -12.57945229203838267 ) ) ;
#10992 = CARTESIAN_POINT ( 'NONE',  ( 11.49999672494999992, -11.45771900890041906, 2.434039779710992502 ) ) ;
#10993 = VECTOR ( 'NONE', #37537, 1000.000000000000000 ) ;
#10994 = CARTESIAN_POINT ( 'NONE',  ( 11.31900581613029821, 4.750686773407899466, -7.982035256002799173 ) ) ;
#10995 = VERTEX_POINT ( 'NONE', #25472 ) ;
#10996 = CARTESIAN_POINT ( 'NONE',  ( 9.242349231304000767, -5.206700957550999931, 8.808818370147001531 ) ) ;
#10997 = CARTESIAN_POINT ( 'NONE',  ( 10.90000000164000049, -2.899999999992999733, 5.160242739040000082 ) ) ;
#10998 = ORIENTED_EDGE ( 'NONE', *, *, #53176, .F. ) ;
#10999 = CARTESIAN_POINT ( 'NONE',  ( 13.31007343200417736, 11.51543253752112150, 1.765677284072383557 ) ) ;
#11000 = CARTESIAN_POINT ( 'NONE',  ( 9.176355646795000709, -2.935738482289000029, 6.259841087764999479 ) ) ;
#11001 = EDGE_CURVE ( 'NONE', #4266, #7303, #68797, .T. ) ;
#11002 = CARTESIAN_POINT ( 'NONE',  ( 8.573539158775000502, 5.361622798585000460, -7.185294144754000634 ) ) ;
#11003 = CIRCLE ( 'NONE', #13275, 0.9999999999999993339 ) ;
#11004 = ORIENTED_EDGE ( 'NONE', *, *, #49476, .T. ) ;
#11005 = CARTESIAN_POINT ( 'NONE',  ( 17.55505043854143565, 1.760845406083394682, -12.47635457398814829 ) ) ;
#11006 = CARTESIAN_POINT ( 'NONE',  ( 7.174995280405999765, 4.580689680786999674, -5.867791741075000900 ) ) ;
#11007 = EDGE_CURVE ( 'NONE', #23303, #14861, #14981, .T. ) ;
#11008 = CARTESIAN_POINT ( 'NONE',  ( 8.799469176677469306, 2.649828231765675834, -7.761613174418741323 ) ) ;
#11009 = DIRECTION ( 'NONE',  ( -1.000000000000000000, 0.000000000000000000, 0.000000000000000000 ) ) ;
#11010 = VERTEX_POINT ( 'NONE', #41553 ) ;
#11011 = CARTESIAN_POINT ( 'NONE',  ( 9.414314870535999802, -3.941041813398000304, 5.878346364186999295 ) ) ;
#11012 = DIRECTION ( 'NONE',  ( 1.000000000000000000, 0.000000000000000000, 0.000000000000000000 ) ) ;
#11013 = CARTESIAN_POINT ( 'NONE',  ( 20.75138802851920161, 0.000000000000000000, 5.760713961201000544 ) ) ;
#11014 = VERTEX_POINT ( 'NONE', #58662 ) ;
#11015 = CARTESIAN_POINT ( 'NONE',  ( 6.221693173016666023, 0.7554284705563509839, -1.310679582531386167 ) ) ;
#11016 = CARTESIAN_POINT ( 'NONE',  ( 10.08211398012999993, -4.728049789772000189, -8.793977405422999993 ) ) ;
#11017 = ORIENTED_EDGE ( 'NONE', *, *, #32606, .T. ) ;
#11018 = DIRECTION ( 'NONE',  ( 0.000000000000000000, 0.9659258262890757507, 0.2588190451024934835 ) ) ;
#11019 = CARTESIAN_POINT ( 'NONE',  ( 18.04536508902295822, 0.3876148459518023448, -13.89272660623100641 ) ) ;
#11020 = CARTESIAN_POINT ( 'NONE',  ( 4.921700572190999878, -1.028864471296000005, 0.9735824284629999159 ) ) ;
#11021 = CARTESIAN_POINT ( 'NONE',  ( 11.59999999999999787, 3.695216987067940551, -6.544326332797708368 ) ) ;
#11022 = CARTESIAN_POINT ( 'NONE',  ( 16.07476513888299863, 3.720976809451999934, 11.90233817890000090 ) ) ;
#11023 = FACE_OUTER_BOUND ( 'NONE', #46058, .T. ) ;
#11024 = DIRECTION ( 'NONE',  ( -8.952907862884936298E-11, -0.7455324205424948003, -0.6664693615763958023 ) ) ;
#11025 = EDGE_LOOP ( 'NONE', ( #42994, #23800, #17011, #34112 ) ) ;
#11026 = CARTESIAN_POINT ( 'NONE',  ( 9.299999999999998934, -4.537600397704999899, 9.154563893594000135 ) ) ;
#11027 = B_SPLINE_CURVE_WITH_KNOTS ( 'NONE', 3,
 ( #62769, #29963, #30980, #8615, #52291, #47054, #47398, #20475, #14210, #19445, #56508, #41803, #68704, #51265, #3361, #24696, #46019, #40768, #62090, #56857, #48081, #530, #10327, #10669, #27447, #49110, #11019, #26418, #6108, #53672, #32693, #64830, #58565, #1221, #48771, #31664, #879, #53330, #37930, #47745, #43178, #27107, #52984, #21844, #36908, #22194 ),
 .UNSPECIFIED., .F., .F.,
 ( 4, 2, 2, 2, 2, 2, 2, 2, 2, 2, 2, 2, 2, 2, 1, 2, 2, 2, 2, 2, 1, 2, 2, 4 ),
 ( 0.000000000000000000, 0.06247329711229584331, 0.09370994566844376150, 0.1249465942245916866, 0.1405649185026656423, 0.1561832427807396118, 0.1874198913368828046, 0.2030382156149564132, 0.2186565398930300219, 0.2264657020320668679, 0.2342748641711037416, 0.2498931884491772670, 0.2811298370053271767, 0.2889389991443658823, 0.2967481612834046989, 0.3123664855614854408, 0.3279848098395661271, 0.3436031341176468690, 0.3748397826738083527, 0.3904581069518891501, 0.4060764312299698364, 0.4373130797861328189, 0.4685497283422958015, 0.4997863768984587285 ),
 .UNSPECIFIED. ) ;
#11028 = EDGE_LOOP ( 'NONE', ( #54856, #49361, #10002, #39288, #62233, #20784 ) ) ;
#11029 = CARTESIAN_POINT ( 'NONE',  ( 9.465106464520001595, 2.290037071913000322, 6.601704384062999864 ) ) ;
#11030 = APPLICATION_CONTEXT ( 'automotive_design' ) ;
#11031 = CARTESIAN_POINT ( 'NONE',  ( 4.519598795370249888, -0.7275289865389679145, 1.350711265020586138 ) ) ;
#11032 = CARTESIAN_POINT ( 'NONE',  ( 17.71485163640869587, -12.11985299911213154, 3.159871563571859276 ) ) ;
#11033 = CARTESIAN_POINT ( 'NONE',  ( 12.27207468729462647, 2.172927540677619174, -13.73742275803506274 ) ) ;
#11034 = CARTESIAN_POINT ( 'NONE',  ( 24.57937622052195437, -12.41575245050226606, -3.011584258247195223 ) ) ;
#11035 = B_SPLINE_CURVE_WITH_KNOTS ( 'NONE', 3,
 ( #45628, #24639, #15171, #46994, #30915, #19385, #52572, #36153, #68296, #56801, #45960, #3638, #3305, #40370, #67269, #46308, #13809, #67609, #14495, #57816, #14152, #14833, #4326, #67959, #31261, #66931, #19734, #41404, #20075, #57465, #61691 ),
 .UNSPECIFIED., .F., .F.,
 ( 4, 2, 2, 1, 1, 2, 2, 2, 1, 2, 2, 2, 2, 2, 2, 2, 4 ),
 ( 0.000000000000000000, 0.06249999999998517852, 0.09374999999997776778, 0.1093749999999739375, 0.1171874999999719807, 0.1210937499999709954, 0.1249999999999700101, 0.1874999999999709677, 0.2187499999999734934, 0.2343749999999746592, 0.2499999999999758526, 0.3749999999999817368, 0.4374999999999846234, 0.4687499999999846789, 0.4999999999999847899, 0.7499999999999924505, 1.000000000000000000 ),
 .UNSPECIFIED. ) ;
#11036 = CARTESIAN_POINT ( 'NONE',  ( 7.000000000000000000, 7.526486366024999874, -3.526486366024999874 ) ) ;
#11037 = CARTESIAN_POINT ( 'NONE',  ( 18.18003636789866917, 0.02080959496299054218, 13.89999914846831963 ) ) ;
#11038 = CARTESIAN_POINT ( 'NONE',  ( 18.12515256038028255, 0.2563263766789344866, 13.89682277887403394 ) ) ;
#11039 = ORIENTED_EDGE ( 'NONE', *, *, #64174, .F. ) ;
#11040 = MECHANICAL_DESIGN_GEOMETRIC_PRESENTATION_REPRESENTATION (  '', ( #61256 ), #10984 ) ;
#11041 = CARTESIAN_POINT ( 'NONE',  ( 12.67430611818100061, -11.44505085583999993, 4.692779640757001047 ) ) ;
#11042 = EDGE_CURVE ( 'NONE', #28824, #45574, #35569, .T. ) ;
#11043 = CARTESIAN_POINT ( 'NONE',  ( 11.46118313518939935, -4.792748567750200195, 6.497569908212999401 ) ) ;
#11044 = EDGE_CURVE ( 'NONE', #31394, #21003, #55695, .T. ) ;
#11045 = CARTESIAN_POINT ( 'NONE',  ( 10.99934110471000004, -5.081022574063999819, 8.239050178861999640 ) ) ;
#11046 = CARTESIAN_POINT ( 'NONE',  ( 18.03457755495272252, -0.4008875276241527508, -13.89221989487475639 ) ) ;
#11047 = CARTESIAN_POINT ( 'NONE',  ( 9.015543146794000151, -4.175914961544999748, 5.699510287082000026 ) ) ;
#11049 = CARTESIAN_POINT ( 'NONE',  ( 18.17737860441035380, 11.15478131644621840, -3.361574628444541357 ) ) ;
#11048 = CARTESIAN_POINT ( 'NONE',  ( 9.820199962102000413, 3.883325513302000154, 6.055618835924000187 ) ) ;
#11050 = CARTESIAN_POINT ( 'NONE',  ( 10.22687885159599830, 5.132709421626000079, -7.364871923548499844 ) ) ;
#11051 = DIRECTION ( 'NONE',  ( 1.000000000000000000, 0.000000000000000000, 0.000000000000000000 ) ) ;
#11052 = CARTESIAN_POINT ( 'NONE',  ( 8.920468108405998464, 4.966402032527499344, -7.773695785133000413 ) ) ;
#11053 = B_SPLINE_CURVE_WITH_KNOTS ( 'NONE', 1,
 ( #40090, #56497 ),
 .UNSPECIFIED., .F., .F.,
 ( 2, 2 ),
 ( 0.000000000000000000, 1.000000000000000000 ),
 .UNSPECIFIED. ) ;
#11054 = CARTESIAN_POINT ( 'NONE',  ( 18.17808098948988516, 0.05063260980701757286, 12.69986973508908079 ) ) ;
#11055 = B_SPLINE_SURFACE_WITH_KNOTS ( 'NONE', 3, 3, ( 
 ( #4361, #42127, #68330, #63434 ),
 ( #20449, #67643, #30268, #35171 ),
 ( #25349, #36531, #57499, #41775 ),
 ( #36187, #14530, #9260, #56484 ),
 ( #57855, #15205, #9960, #24671 ),
 ( #56834, #8932, #51575, #25010 ),
 ( #3669, #45991, #31297, #67304 ),
 ( #8588, #52607, #46341, #40744 ),
 ( #30601, #19767, #4700, #41092 ),
 ( #26046, #62409, #35846, #9608 ) ),
 .UNSPECIFIED., .F., .F., .F.,
 ( 4, 1, 1, 1, 1, 1, 1, 4 ),
 ( 4, 4 ),
 ( 0.04183311431308000400, 0.1428571428570999946, 0.2857142857143000203, 0.4285714285713999594, 0.5714285714286000406, 0.7142857142856999797, 0.8571428571429000609, 0.9292981235707000742 ),
 ( -0.1917799910644000239, 1.191756862851000021 ),
 .UNSPECIFIED. ) ;
#11056 = CARTESIAN_POINT ( 'NONE',  ( 8.599999952505998024, -4.000000000000000000, -7.500000000000000000 ) ) ;
#11057 = DIRECTION ( 'NONE',  ( -1.000000000000000000, 0.000000000000000000, 0.000000000000000000 ) ) ;
#11058 = EDGE_LOOP ( 'NONE', ( #53324, #19136, #44323, #22552 ) ) ;
#11059 = CARTESIAN_POINT ( 'NONE',  ( 7.374102686541000651, -4.389298280625000714, 9.135255728583000945 ) ) ;
#11060 = CARTESIAN_POINT ( 'NONE',  ( 9.369139158774000720, 2.685250982074999904, -7.026194612421999608 ) ) ;
#11061 = DIRECTION ( 'NONE',  ( 0.000000000000000000, -1.000000000000000000, 0.000000000000000000 ) ) ;
#11062 = ADVANCED_FACE ( 'NONE', ( #57277, #52382 ), #42254, .F. ) ;
#11063 = CARTESIAN_POINT ( 'NONE',  ( 10.99249554219874447, 6.392256384488597121, 5.212998417364866022 ) ) ;
#11064 = CARTESIAN_POINT ( 'NONE',  ( 0.4939139796827000106, -1.072119470989999934, 3.198702759649999727 ) ) ;
#11065 = CARTESIAN_POINT ( 'NONE',  ( 10.77368717260499942, 3.460071470104900015, 6.618743573831199711 ) ) ;
#11066 = CARTESIAN_POINT ( 'NONE',  ( 10.57657334123000048, 5.344886503256999433, -7.298885378918000377 ) ) ;
#11067 = ORIENTED_EDGE ( 'NONE', *, *, #34745, .F. ) ;
#11068 = CARTESIAN_POINT ( 'NONE',  ( 7.000000000000000000, 3.640000000000000124, 3.000000000000000000 ) ) ;
#11069 = DIRECTION ( 'NONE',  ( -1.000000000000000000, 0.000000000000000000, 0.000000000000000000 ) ) ;
#11070 = CARTESIAN_POINT ( 'NONE',  ( 18.25535445515775024, 2.667446342172959728, -12.31441698789904393 ) ) ;
#11071 = CARTESIAN_POINT ( 'NONE',  ( 7.950237460432950876, -4.863279781983014693, 6.348139858574191052 ) ) ;
#11072 = CARTESIAN_POINT ( 'NONE',  ( 7.860170280410000210, 2.263558315407000254, 8.007442119518000112 ) ) ;
#11073 = ORIENTED_EDGE ( 'NONE', *, *, #22102, .T. ) ;
#11074 = CARTESIAN_POINT ( 'NONE',  ( 6.054360824503000948, -0.9021507525358000157, -1.158728426834999992 ) ) ;
#11075 = CARTESIAN_POINT ( 'NONE',  ( 7.698345280408000590, 2.727583171400000062, -8.411095346025000197 ) ) ;
#11076 = CARTESIAN_POINT ( 'NONE',  ( 8.381225618344668504, -2.869678555928259378, 8.822438359558621102 ) ) ;
#11077 = CARTESIAN_POINT ( 'NONE',  ( 9.472076168957999087, -4.649151400100800302, 6.397735581984999698 ) ) ;
#11078 = ORIENTED_EDGE ( 'NONE', *, *, #8931, .F. ) ;
#11079 = DIRECTION ( 'NONE',  ( -1.000000000000000000, 0.000000000000000000, 0.000000000000000000 ) ) ;
#11080 = B_SPLINE_CURVE_WITH_KNOTS ( 'NONE', 3,
 ( #19774, #36193, #25017, #46348, #67650, #26052, #41100, #47381, #57505, #51922 ),
 .UNSPECIFIED., .F., .F.,
 ( 4, 2, 2, 2, 4 ),
 ( 0.2509294615239107684, 0.4381970961429330624, 0.6254647307619554120, 0.8127323653809777060, 1.000000000000000000 ),
 .UNSPECIFIED. ) ;
#11081 = CARTESIAN_POINT ( 'NONE',  ( 7.000000000000000000, 0.8000000000000000444, 3.149999999999999911 ) ) ;
#11082 = ORIENTED_EDGE ( 'NONE', *, *, #51959, .T. ) ;
#11083 = CARTESIAN_POINT ( 'NONE',  ( 24.81126491645922982, 3.073463793308780279, -11.71256572910995963 ) ) ;
#11084 = DIRECTION ( 'NONE',  ( 0.000000000000000000, 0.4595926418529958646, 0.8881298348521931008 ) ) ;
#11085 = CARTESIAN_POINT ( 'NONE',  ( 18.17481363285255469, 0.08139021474669749789, -13.89968437038779570 ) ) ;
#11086 = ORIENTED_EDGE ( 'NONE', *, *, #37913, .T. ) ;
#11087 = CARTESIAN_POINT ( 'NONE',  ( 10.26947109217999810, -5.100000000000000533, -6.152188490330000370 ) ) ;
#11088 = CARTESIAN_POINT ( 'NONE',  ( 9.709999999999999076, -4.496968146123999865, -8.755198255949000696 ) ) ;
#11089 = CARTESIAN_POINT ( 'NONE',  ( 10.44125056272499918, 5.033400911533000510, -7.515315513715298934 ) ) ;
#11090 = ADVANCED_FACE ( 'NONE', ( #63557, #69151 ), #48174, .T. ) ;
#11091 = CARTESIAN_POINT ( 'NONE',  ( 11.66889198463462662, 3.216368914751021268, -11.40336763631111339 ) ) ;
#11092 = CARTESIAN_POINT ( 'NONE',  ( 11.38733729122639993, -5.277570687708000641, 7.533608309972310124 ) ) ;
#11093 = ORIENTED_EDGE ( 'NONE', *, *, #13301, .T. ) ;
#11094 = CARTESIAN_POINT ( 'NONE',  ( 7.320267219589999819, 2.466388272391000225, 6.935562100014999842 ) ) ;
#11095 = VERTEX_POINT ( 'NONE', #4477 ) ;
#11096 = CARTESIAN_POINT ( 'NONE',  ( 9.989763540183332680, -3.672815144550900524, 6.282534154164604701 ) ) ;
#11097 = CARTESIAN_POINT ( 'NONE',  ( 16.13936233968600220, -9.023335130797001113, -8.741328814538000813 ) ) ;
#11098 = CARTESIAN_POINT ( 'NONE',  ( 10.96499058814000094, 6.672045932937000323, -5.367166258627000808 ) ) ;
#11099 = ORIENTED_EDGE ( 'NONE', *, *, #12185, .T. ) ;
#11100 = CARTESIAN_POINT ( 'NONE',  ( 10.10107565221251491, -5.349884357716051753, -7.263395957186704166 ) ) ;
#11101 = FACE_OUTER_BOUND ( 'NONE', #20379, .T. ) ;
#11102 = CARTESIAN_POINT ( 'NONE',  ( 23.56666365135700403, -9.114812703071004663, 8.684180617907001576 ) ) ;
#11103 = DIRECTION ( 'NONE',  ( 0.000000000000000000, 0.000000000000000000, 1.000000000000000000 ) ) ;
#11104 = CARTESIAN_POINT ( 'NONE',  ( 12.68590879673673477, -1.797325930449588327, -13.88415075348993710 ) ) ;
#11105 = CARTESIAN_POINT ( 'NONE',  ( 10.40333997687999990, -3.786145554879500441, -6.519583185858300212 ) ) ;
#11106 = B_SPLINE_CURVE_WITH_KNOTS ( 'NONE', 3,
 ( #60021, #1989, #22953, #12474 ),
 .UNSPECIFIED., .F., .F.,
 ( 4, 4 ),
 ( 0.000000000000000000, 1.000000000000000000 ),
 .UNSPECIFIED. ) ;
#11107 = CARTESIAN_POINT ( 'NONE',  ( 24.44496356232399847, -3.224881240379999792, -12.03535804424000055 ) ) ;
#11108 = CARTESIAN_POINT ( 'NONE',  ( 18.24534165125343677, -2.701041880525442807, 12.30709158425920613 ) ) ;
#11109 = ORIENTED_EDGE ( 'NONE', *, *, #54658, .T. ) ;
#11110 =( BOUNDED_SURFACE ( )  B_SPLINE_SURFACE ( 3, 3, ( 
 ( #54329, #28470, #1895, #23555 ),
 ( #12381, #11677, #6430, #33015 ),
 ( #27780, #12033, #65855, #49090 ),
 ( #65154, #18321, #44896, #44212 ) ),
 .UNSPECIFIED., .F., .F., .T. ) 
 B_SPLINE_SURFACE_WITH_KNOTS ( ( 4, 4 ),
 ( 4, 4 ),
 ( 0.000000000000000000, 1.000000000000000000 ),
 ( 0.000000000000000000, 1.000000000000000000 ),
 .UNSPECIFIED. ) 
 GEOMETRIC_REPRESENTATION_ITEM ( )  RATIONAL_B_SPLINE_SURFACE ( (
 ( 1.512182578520000042, 1.160176301760999840, 1.160176301760999840, 1.512182578520000042),
 ( 1.111288591041000196, 0.8526025270081000196, 0.8526025270081000196, 1.111288591041000196),
 ( 1.111288591041000196, 0.8526025270081000196, 0.8526025270081000196, 1.111288591041000196),
 ( 1.512182578520000042, 1.160176301760999840, 1.160176301760999840, 1.512182578520000042) ) ) 
 REPRESENTATION_ITEM ( '' )  SURFACE ( )  );
#11111 = CARTESIAN_POINT ( 'NONE',  ( 10.51414141025500015, -3.384226587288500010, -8.596754040696000132 ) ) ;
#11112 = ORIENTED_EDGE ( 'NONE', *, *, #38625, .F. ) ;
#11113 = AXIS2_PLACEMENT_3D ( 'NONE', #9178, #10556, #42037 ) ;
#11114 = B_SPLINE_CURVE_WITH_KNOTS ( 'NONE', 3,
 ( #7241, #61074, #2685, #23324 ),
 .UNSPECIFIED., .F., .F.,
 ( 4, 4 ),
 ( 0.000000000000000000, 1.000000000000000000 ),
 .UNSPECIFIED. ) ;
#11115 = CARTESIAN_POINT ( 'NONE',  ( 25.30000327618300204, -1.393126554761421110, -11.43653827017141111 ) ) ;
#11116 = CARTESIAN_POINT ( 'NONE',  ( 4.900006121742000786, 1.947945353336632213, 0.5234957687185572972 ) ) ;
#11117 = CARTESIAN_POINT ( 'NONE',  ( 9.947724669984761903, 5.285954009497370265, 7.027653896126389910 ) ) ;
#11118 = CARTESIAN_POINT ( 'NONE',  ( 10.48735240295000004, -4.351290250877999810, -6.182246784057000788 ) ) ;
#11119 = CARTESIAN_POINT ( 'NONE',  ( 11.09999999999999964, 2.700000000000000178, -5.160242730539000178 ) ) ;
#11120 = CARTESIAN_POINT ( 'NONE',  ( 7.893560293058006216, 2.859109450078002546, -6.778905949012001386 ) ) ;
#11121 = CARTESIAN_POINT ( 'NONE',  ( 10.97864812944000157, 5.273131703456000352, 7.958028903907000462 ) ) ;
#11122 = ORIENTED_EDGE ( 'NONE', *, *, #9375, .F. ) ;
#11123 = CARTESIAN_POINT ( 'NONE',  ( 12.09999999999999964, -2.613168764257999932, 7.825000000000000178 ) ) ;
#11124 = ADVANCED_FACE ( 'NONE', ( #37001 ), #15672, .T. ) ;
#11125 = CARTESIAN_POINT ( 'NONE',  ( 10.99433665574000152, 3.697618584609999814, 5.729302299903000772 ) ) ;
#11126 = EDGE_CURVE ( 'NONE', #15766, #52017, #18864, .T. ) ;
#11127 = CARTESIAN_POINT ( 'NONE',  ( 11.79999999550100220, 3.351258778187000242, -11.15757272551999968 ) ) ;
#11128 = CARTESIAN_POINT ( 'NONE',  ( 11.64767835872009982, -4.874341053673500568, 8.051056647135798272 ) ) ;
#11129 = CARTESIAN_POINT ( 'NONE',  ( 18.24051303026600124, 3.055556278716000218, -11.39470302754000031 ) ) ;
#11130 = CARTESIAN_POINT ( 'NONE',  ( 10.86280073406000035, 9.764482209271999835, -5.701704797273999148 ) ) ;
#11131 = FACE_OUTER_BOUND ( 'NONE', #41863, .T. ) ;
#11132 = CARTESIAN_POINT ( 'NONE',  ( 24.15440335769899960, -9.221781890355002176, -9.473822549412000527 ) ) ;
#11133 = CARTESIAN_POINT ( 'NONE',  ( 10.94076550314999885, 5.140765503144999471, -6.571291218949999902 ) ) ;
#11134 = CARTESIAN_POINT ( 'NONE',  ( 23.60000000000000142, -10.96647536436334391, 8.588749203884328054 ) ) ;
#11135 = ORIENTED_EDGE ( 'NONE', *, *, #50970, .T. ) ;
#11136 = CARTESIAN_POINT ( 'NONE',  ( 6.166666667074697905, 12.50864792167083017, -2.924697251373290730 ) ) ;
#11137 = CARTESIAN_POINT ( 'NONE',  ( 7.094746981741000269, 1.094478228765999983, 0.2906167377007999875 ) ) ;
#11138 = CARTESIAN_POINT ( 'NONE',  ( 18.17921951168938932, 2.461818733276640803, 13.68145094671735329 ) ) ;
#11139 = EDGE_CURVE ( 'NONE', #65047, #52012, #43413, .T. ) ;
#11140 = CARTESIAN_POINT ( 'NONE',  ( 11.09999999999999964, -2.646159083949000124, 6.745271721726000536 ) ) ;
#11141 = CARTESIAN_POINT ( 'NONE',  ( 11.06379841651039797, -4.401637675674300532, -8.567697191971999970 ) ) ;
#11142 = ORIENTED_EDGE ( 'NONE', *, *, #57252, .T. ) ;
#11143 = CARTESIAN_POINT ( 'NONE',  ( 5.619239821438371862, -12.11503533078118622, 3.745341923022787789 ) ) ;
#11144 = EDGE_CURVE ( 'NONE', #30682, #36697, #36050, .T. ) ;
#11145 = CARTESIAN_POINT ( 'NONE',  ( 7.539232780409000689, 4.696238830159999544, 5.830273622963999536 ) ) ;
#11147 = CARTESIAN_POINT ( 'NONE',  ( 10.56819717211696741, 5.125396288431045555, -6.749639981090855834 ) ) ;
#11146 = CARTESIAN_POINT ( 'NONE',  ( 8.804445280412998898, 5.597201461420000967, -8.171008079894999554 ) ) ;
#11148 = CARTESIAN_POINT ( 'NONE',  ( 2.235213150975154495, 2.767678518585422687, -1.576253733361024256 ) ) ;
#11149 = ORIENTED_EDGE ( 'NONE', *, *, #11144, .T. ) ;
#11150 = CARTESIAN_POINT ( 'NONE',  ( 10.90638722582999875, 5.227488226180000197, 6.784465725675999259 ) ) ;
#11151 = CARTESIAN_POINT ( 'NONE',  ( 18.25665235842816259, -2.332587565413964725, -13.80433135817204793 ) ) ;
#11152 = CARTESIAN_POINT ( 'NONE',  ( 11.48641235500450009, 3.260080192309100067, 8.177841818594698609 ) ) ;
#11153 = CARTESIAN_POINT ( 'NONE',  ( 10.87148543990999983, -5.567571293949000300, 7.772413914480000408 ) ) ;
#11154 = CARTESIAN_POINT ( 'NONE',  ( 7.678995559621999867, -2.599231861044000169, 7.909347897884000389 ) ) ;
#11155 = ORIENTED_EDGE ( 'NONE', *, *, #49991, .T. ) ;
#11156 = CARTESIAN_POINT ( 'NONE',  ( 8.198726617487999135, -3.399995262767999904, 6.142473321098000483 ) ) ;
#11158 = CARTESIAN_POINT ( 'NONE',  ( 11.24323064679000161, -2.479730344050999680, -7.587230764681999418 ) ) ;
#11157 = CARTESIAN_POINT ( 'NONE',  ( 12.42828976145100128, -11.57811841779999895, 4.879106015068000346 ) ) ;
#11159 = CARTESIAN_POINT ( 'NONE',  ( 7.848601693978649152, -3.465122274420019188, 9.162632088545951348 ) ) ;
#11160 = CARTESIAN_POINT ( 'NONE',  ( 9.595487457706001422, -3.928425191288000384, 5.531324308465000783 ) ) ;
#11161 = CARTESIAN_POINT ( 'NONE',  ( 1.309336868148999855, 3.233448155534000001, 0.4075532224664999981 ) ) ;
#11162 = VERTEX_POINT ( 'NONE', #31760 ) ;
#11163 = CARTESIAN_POINT ( 'NONE',  ( 24.98032374313059023, -11.50386448131031791, -3.228640037327431767 ) ) ;
#11164 = CARTESIAN_POINT ( 'NONE',  ( 10.70641772631199906, -3.568446272909699957, 6.611684804099500212 ) ) ;
#11165 = CARTESIAN_POINT ( 'NONE',  ( 10.66579975933730040, 5.208485784810999775, 7.915786590091300035 ) ) ;
#11166 = VERTEX_POINT ( 'NONE', #20569 ) ;
#11167 = B_SPLINE_CURVE_WITH_KNOTS ( 'NONE', 3,
 ( #26851, #966, #34164, #66652 ),
 .UNSPECIFIED., .F., .F.,
 ( 4, 4 ),
 ( 0.000000000000000000, 0.2468845652704700078 ),
 .UNSPECIFIED. ) ;
#11168 = CARTESIAN_POINT ( 'NONE',  ( 8.514954719592999766, 3.207599814920999659, -6.150466394809999571 ) ) ;
#11169 = CARTESIAN_POINT ( 'NONE',  ( 8.073148997456000231, 5.167567567567999731, -6.822293592207000934 ) ) ;
#11170 = CARTESIAN_POINT ( 'NONE',  ( 10.93614141025500075, -3.450366949021700158, 6.521048559232099251 ) ) ;
#11171 = CARTESIAN_POINT ( 'NONE',  ( 9.179391679754937527, 4.176475755878279905, -8.849937275099289735 ) ) ;
#11172 = CARTESIAN_POINT ( 'NONE',  ( 18.04486049886915211, 2.888348857507973211, -13.58339007192517656 ) ) ;
#11173 = ORIENTED_EDGE ( 'NONE', *, *, #33081, .T. ) ;
#11174 = CARTESIAN_POINT ( 'NONE',  ( 8.496691940379001551, -5.198566224659999513, 8.332559954171999905 ) ) ;
#11175 = PLANE ( 'NONE',  #58078 ) ;
#11176 = VERTEX_POINT ( 'NONE', #9726 ) ;
#11177 = CARTESIAN_POINT ( 'NONE',  ( 12.30701392268165684, -3.003682976637727098, -12.23675526868967545 ) ) ;
#11178 = CARTESIAN_POINT ( 'NONE',  ( 10.38287885159599888, 4.860099138268600072, 7.602606670248799325 ) ) ;
#11179 = CARTESIAN_POINT ( 'NONE',  ( 10.62697636434999993, 3.142921793056999924, 8.668445734229999644 ) ) ;
#11180 = EDGE_CURVE ( 'NONE', #38546, #55988, #56789, .T. ) ;
#11181 = CARTESIAN_POINT ( 'NONE',  ( 10.64127413024999846, 2.258699798012000048, -6.863478635463000188 ) ) ;
#11182 = DIRECTION ( 'NONE',  ( 1.000000000000000000, 0.000000000000000000, 0.000000000000000000 ) ) ;
#11183 = CARTESIAN_POINT ( 'NONE',  ( 11.00366278039000001, -2.264082614160999984, 7.798350693290999835 ) ) ;
#11184 = B_SPLINE_CURVE_WITH_KNOTS ( 'NONE', 3,
 ( #58770, #10877, #6662, #44439, #1425, #22739, #44089, #53535, #5627, #43040 ),
 .UNSPECIFIED., .F., .F.,
 ( 4, 2, 2, 2, 4 ),
 ( 0.4999999997123694695, 0.6249999997842766719, 0.7499999998561844849, 0.8749999999280921870, 1.000000000000000000 ),
 .UNSPECIFIED. ) ;
#11185 = CARTESIAN_POINT ( 'NONE',  ( 18.08473038518646092, -0.4912829912815128153, -12.59042165808840252 ) ) ;
#11186 = CARTESIAN_POINT ( 'NONE',  ( 10.10000011340999926, -12.39999890530000037, 0.000000000000000000 ) ) ;
#11187 = CARTESIAN_POINT ( 'NONE',  ( 10.50180110216399854, -4.856393875115199599, -6.976989117212499814 ) ) ;
#11188 = CARTESIAN_POINT ( 'NONE',  ( 7.737829719589999655, 5.687206835507000235, 6.847268999608999707 ) ) ;
#11189 = VERTEX_POINT ( 'NONE', #26167 ) ;
#11190 =( NAMED_UNIT ( * ) PLANE_ANGLE_UNIT ( ) SI_UNIT ( $, .RADIAN. ) );
#11191 = DIRECTION ( 'NONE',  ( 0.000000000000000000, -0.8648648648648717963, 0.5020047465136829867 ) ) ;
#11192 = CARTESIAN_POINT ( 'NONE',  ( 9.245063355149550688, 2.690443968828802657, 7.172286089387452712 ) ) ;
#11193 = CARTESIAN_POINT ( 'NONE',  ( 7.910551708067999677, 2.874573263512000043, -6.728745899354000137 ) ) ;
#11194 = AXIS2_PLACEMENT_3D ( 'NONE', #9096, #68500, #68850 ) ;
#11195 = CARTESIAN_POINT ( 'NONE',  ( 18.27054884872053009, 2.599315299774881627, 12.32899436121337189 ) ) ;
#11196 = CARTESIAN_POINT ( 'NONE',  ( 11.12341687003999979, 6.051695911142999762, 5.270624977622000884 ) ) ;
#11197 = CARTESIAN_POINT ( 'NONE',  ( 11.06799838223999899, 8.464218156389000214, 6.698020382136999906 ) ) ;
#11198 = CARTESIAN_POINT ( 'NONE',  ( 10.71473687196862734, -4.313773474582136558, 6.683251291081091949 ) ) ;
#11199 = CARTESIAN_POINT ( 'NONE',  ( 10.09393020684899867, -2.750000000000000000, -7.500000000000000000 ) ) ;
#11200 = EDGE_CURVE ( 'NONE', #3150, #40878, #63896, .T. ) ;
#11201 = ORIENTED_EDGE ( 'NONE', *, *, #41435, .T. ) ;
#11202 = CARTESIAN_POINT ( 'NONE',  ( 12.51396835178763034, -3.139274738718787816, 12.20266202197805150 ) ) ;
#11203 = EDGE_CURVE ( 'NONE', #31672, #15110, #10764, .T. ) ;
#11204 = CARTESIAN_POINT ( 'NONE',  ( 10.00962143724499853, -3.332852462363599777, -6.749162825004299648 ) ) ;
#11205 = CARTESIAN_POINT ( 'NONE',  ( 9.374586245486254299, -4.497363021594377841, 9.030797514265954007 ) ) ;
#11206 = AXIS2_PLACEMENT_3D ( 'NONE', #59192, #54288, #32634 ) ;
#11207 = CARTESIAN_POINT ( 'NONE',  ( 8.315204322669442760, 2.904787293452365748, -6.552018845477737052 ) ) ;
#11208 = EDGE_CURVE ( 'NONE', #65259, #33492, #22289, .T. ) ;
#11209 = B_SPLINE_SURFACE_WITH_KNOTS ( 'NONE', 3, 3, ( 
 ( #29253, #19775, #46349, #29602, #24680, #40407, #62075, #13515, #35519, #45999, #41101, #34835, #67651, #3344, #35854, #35178, #50905, #51249, #51582, #61394, #24335, #13851, #34500, #51923, #39735, #30278, #67311, #18753, #62416, #67999, #66973, #57170, #56147, #9267, #50562 ),
 ( #8596, #2662, #8939, #30609, #29946, #40752, #19429, #14191, #8255, #61052, #23990, #4020, #56841, #45667, #13172, #55813, #45325, #66634, #3002, #40085, #20115, #5412, #53650, #26053, #30959, #27090, #58207, #69039, #11000, #41444, #32341, #62752, #20803, #41783, #48405 ),
 ( #14871, #20456, #5746, #63088, #53309, #42136, #36194, #31997, #42818, #52614, #15212, #31644, #64126, #52273, #37228, #4368, #48064, #10310, #26748, #52967, #36539, #57864, #25702, #47034, #63786, #68337, #58546, #57506, #167, #5063, #15897, #9615, #9968, #21484, #26400 ),
 ( #47727, #31304, #36893, #21151, #47382, #4708, #42478, #68685, #63442, #16240, #15565, #10651, #37564, #58897, #27429, #60280, #55036, #11335, #39301, #22864, #7136, #1206, #60624, #55380, #32677, #22514, #1546, #34064, #49789, #38963, #17639, #12385, #16922, #54686, #12735 ) ),
 .UNSPECIFIED., .F., .F., .F.,
 ( 4, 4 ),
 ( 4, 1, 1, 1, 1, 1, 1, 1, 1, 1, 1, 1, 1, 1, 1, 1, 1, 1, 1, 1, 1, 1, 1, 1, 1, 1, 1, 1, 1, 1, 1, 1, 4 ),
 ( -0.1039086239011999951, 1.103908623900999864 ),
 ( -0.02000000000000000042, 0.01250000000000000069, 0.04499999999999999833, 0.07749999999999999944, 0.1100000000000000006, 0.1424999999999999878, 0.1749999999999999889, 0.2074999999999999900, 0.2399999999999999911, 0.2725000000000000200, 0.3049999999999999933, 0.3375000000000000222, 0.3699999999999999956, 0.4025000000000000244, 0.4349999999999999978, 0.4675000000000000266, 0.5000000000000000000, 0.5324999999999999734, 0.5649999999999999467, 0.5975000000000000311, 0.6300000000000000044, 0.6624999999999999778, 0.6949999999999999512, 0.7275000000000000355, 0.7600000000000000089, 0.7924999999999999822, 0.8249999999999999556, 0.8575000000000000400, 0.8900000000000000133, 0.9224999999999999867, 0.9549999999999999600, 0.9875000000000000444, 1.020000000000000018 ),
 .UNSPECIFIED. ) ;
#11210 = CARTESIAN_POINT ( 'NONE',  ( 10.77256919669529900, 4.962345366016100101, -7.784327714719899483 ) ) ;
#11211 = CARTESIAN_POINT ( 'NONE',  ( 12.80505043854144276, 0.7192913403693016461, 12.57945229203838444 ) ) ;
#11212 = CARTESIAN_POINT ( 'NONE',  ( 8.470295280410999439, 4.255646040929000229, 9.114085578076998928 ) ) ;
#11213 = CARTESIAN_POINT ( 'NONE',  ( 9.575188572738724702, 5.349682312560990027, -7.676829535353270728 ) ) ;
#11214 = CARTESIAN_POINT ( 'NONE',  ( 12.21328932544278523, 2.701359397734038215, 12.40237271074985159 ) ) ;
#11215 = FACE_OUTER_BOUND ( 'NONE', #62166, .T. ) ;
#11216 = CARTESIAN_POINT ( 'NONE',  ( 11.50687348028854906, 2.996540789803000315, -8.042549288197099244 ) ) ;
#11217 = CARTESIAN_POINT ( 'NONE',  ( 8.168244718249995984, 3.088031253505000961, -6.162676582372005996 ) ) ;
#11218 = CARTESIAN_POINT ( 'NONE',  ( 11.33382334123000135, 2.642405149457999869, -7.577896731332000257 ) ) ;
#11219 = CARTESIAN_POINT ( 'NONE',  ( 9.662398456551489545, 2.649938674315804210, 7.712117850346960957 ) ) ;
#11221 = CARTESIAN_POINT ( 'NONE',  ( 18.09811783085022441, -0.3100350603877315425, 12.69492243000587983 ) ) ;
#11220 = CARTESIAN_POINT ( 'NONE',  ( 8.354426260476000010, 5.125517035499999707, 6.367235573876004473 ) ) ;
#11222 = CYLINDRICAL_SURFACE ( 'NONE', #16278, 0.5000000000000000000 ) ;
#11223 = ORIENTED_EDGE ( 'NONE', *, *, #69149, .T. ) ;
#11224 = CARTESIAN_POINT ( 'NONE',  ( 12.32101752301072572, 0.3953985757077859708, 12.69171505958679802 ) ) ;
#11225 = EDGE_CURVE ( 'NONE', #37496, #18320, #38021, .T. ) ;
#11226 = CARTESIAN_POINT ( 'NONE',  ( 23.80818154638642881, -9.703800845197944724, -9.420725050333308204 ) ) ;
#11227 = CARTESIAN_POINT ( 'NONE',  ( 11.30000000000000071, 0.000000000000000000, 0.000000000000000000 ) ) ;
#11228 = CARTESIAN_POINT ( 'NONE',  ( 17.55505043854143565, 3.199751711897561801, -12.18694338143115452 ) ) ;
#11229 = CARTESIAN_POINT ( 'NONE',  ( 12.28091743413951953, -2.013400871504821943, 13.85446832019263219 ) ) ;
#11230 = FACE_OUTER_BOUND ( 'NONE', #23479, .T. ) ;
#11231 = CARTESIAN_POINT ( 'NONE',  ( 10.90000000000000036, 0.000000000000000000, 0.000000000000000000 ) ) ;
#11232 = ORIENTED_EDGE ( 'NONE', *, *, #66802, .F. ) ;
#11233 = CARTESIAN_POINT ( 'NONE',  ( 4.159417977171999681, 0.5323169164456000857, 0.9754548401560999560 ) ) ;
#11234 = CARTESIAN_POINT ( 'NONE',  ( 18.29999999997146887, -11.00695868226778629, 3.817556993357585249 ) ) ;
#11235 = DIRECTION ( 'NONE',  ( 0.000000000000000000, 1.000000000000000000, 0.000000000000000000 ) ) ;
#11236 = CARTESIAN_POINT ( 'NONE',  ( 10.78014141025500017, -3.582647672488299850, 6.756653759087999589 ) ) ;
#11237 = TOROIDAL_SURFACE ( 'NONE', #50336, 12.20000000000000107, 0.6999999999999999556 ) ;
#11238 = CARTESIAN_POINT ( 'NONE',  ( 18.02812495262682901, 2.091428156338118960, -12.53745402072848947 ) ) ;
#11239 = CARTESIAN_POINT ( 'NONE',  ( 9.610163692916376732, -2.765799910565780895, 7.754438396796453858 ) ) ;
#11240 = CARTESIAN_POINT ( 'NONE',  ( 10.77672335273219950, 4.301522290735800169, 6.687976048055599421 ) ) ;
#11242 = CARTESIAN_POINT ( 'NONE',  ( 10.88528584683667688, -3.267379250638398069, 6.833918148925946845 ) ) ;
#11241 = CIRCLE ( 'NONE', #58161, 14.00000000000000000 ) ;
#11243 = CARTESIAN_POINT ( 'NONE',  ( 10.90246814679000131, -4.554787328265999413, -6.081873034041000103 ) ) ;
#11244 = DIRECTION ( 'NONE',  ( 0.000000000000000000, -1.000000000000000000, 0.000000000000000000 ) ) ;
#11245 = CARTESIAN_POINT ( 'NONE',  ( 11.50001544675000176, -9.368387413360784066, 8.415797411343536538 ) ) ;
#11246 = LINE ( 'NONE', #37139, #60043 ) ;
#11247 = DIRECTION ( 'NONE',  ( 0.000000000000000000, -0.8648648648648717963, 0.5020047465136829867 ) ) ;
#11248 = ORIENTED_EDGE ( 'NONE', *, *, #24620, .F. ) ;
#11249 = CARTESIAN_POINT ( 'NONE',  ( 9.591185841232000797, 2.173570076733999823, -8.023168429484000441 ) ) ;
#11250 = CARTESIAN_POINT ( 'NONE',  ( 11.74441369783139955, -4.043700988887960257, 6.634905315059499209 ) ) ;
#11251 = ORIENTED_EDGE ( 'NONE', *, *, #6090, .F. ) ;
#11252 = CARTESIAN_POINT ( 'NONE',  ( 18.14140153244920839, -2.282676164818131515, 13.71717056020691317 ) ) ;
#11253 = CARTESIAN_POINT ( 'NONE',  ( 10.96533729122639933, -5.140346530769000388, -7.470001566214039990 ) ) ;
#11254 = VERTEX_POINT ( 'NONE', #64923 ) ;
#11255 = CARTESIAN_POINT ( 'NONE',  ( 10.64902344389989963, 3.116469856398800253, 8.036199780531900316 ) ) ;
#11256 = DIRECTION ( 'NONE',  ( 0.000000000000000000, 0.8648648648648717963, 0.5020047465136829867 ) ) ;
#11257 = CARTESIAN_POINT ( 'NONE',  ( 8.734020077949999461, -4.063547279775290733, -8.378811912355599745 ) ) ;
#11258 = EDGE_CURVE ( 'NONE', #67334, #51763, #67948, .T. ) ;
#11259 = CARTESIAN_POINT ( 'NONE',  ( 13.60016906737400078, 3.366196210663000557E-13, 1.969535645684999935E-13 ) ) ;
#11260 = EDGE_CURVE ( 'NONE', #10787, #15277, #26896, .T. ) ;
#11261 = PLANE ( 'NONE',  #52243 ) ;
#11262 = CARTESIAN_POINT ( 'NONE',  ( 12.24298788029395268, 0.2740979065993932040, -13.89637745338620967 ) ) ;
#11263 = CARTESIAN_POINT ( 'NONE',  ( 23.56665676678100141, -2.935523947847999970, 13.67844066972000050 ) ) ;
#11264 = CARTESIAN_POINT ( 'NONE',  ( 10.81362580514000094, -3.876947229615999913, -9.022210119840998743 ) ) ;
#11265 = CARTESIAN_POINT ( 'NONE',  ( 12.95917414208900098, 11.49387908994000007, 1.654391991822000030 ) ) ;
#11266 = ORIENTED_EDGE ( 'NONE', *, *, #16823, .T. ) ;
#11267 = CARTESIAN_POINT ( 'NONE',  ( 8.672510841228998402, 4.686731264770999772, -8.717075579553000608 ) ) ;
#11268 = ORIENTED_EDGE ( 'NONE', *, *, #17210, .F. ) ;
#11269 = CARTESIAN_POINT ( 'NONE',  ( 10.09133754351999990, 2.216715295763999727, -8.007133643737999407 ) ) ;
#11270 = ORIENTED_EDGE ( 'NONE', *, *, #30786, .T. ) ;
#11271 = LINE ( 'NONE', #5682, #64880 ) ;
#11272 = CARTESIAN_POINT ( 'NONE',  ( 18.17545025690713345, -2.421661855460688351, -12.46948612151124358 ) ) ;
#11273 = CARTESIAN_POINT ( 'NONE',  ( 7.966901574931999797, 4.609574279519000228, -6.276317554486000816 ) ) ;
#11274 = CARTESIAN_POINT ( 'NONE',  ( 7.844724262280000637, -4.719412258162999585, 6.357657668295000342 ) ) ;
#11275 = CARTESIAN_POINT ( 'NONE',  ( 11.27765354842000001, -3.273798832483999721, 6.368296067120999382 ) ) ;
#11276 = CARTESIAN_POINT ( 'NONE',  ( 11.03776249210999971, -8.050323671732000363, -6.914613055281999543 ) ) ;
#11277 = VECTOR ( 'NONE', #9239, 1000.000000000000000 ) ;
#11278 = CARTESIAN_POINT ( 'NONE',  ( 12.21991984215965132, -0.2205930660282666711, 13.89766156610768277 ) ) ;
#11279 = ORIENTED_EDGE ( 'NONE', *, *, #32405, .F. ) ;
#11280 = CARTESIAN_POINT ( 'NONE',  ( 6.828228317543000081, 2.534482666265000184, -7.314862106114000007 ) ) ;
#11281 = EDGE_CURVE ( 'NONE', #39483, #6863, #58587, .T. ) ;
#11282 = CARTESIAN_POINT ( 'NONE',  ( 18.21407466721599988, 11.71489335541000010, -3.703722432179000101 ) ) ;
#11283 = CARTESIAN_POINT ( 'NONE',  ( 9.302887573405627109, 4.590576684156811638, 6.854437106819677439 ) ) ;
#11284 = CARTESIAN_POINT ( 'NONE',  ( 5.009753349970999636, 1.333795246837999882, 0.04609146662756000157 ) ) ;
#11285 = ADVANCED_FACE ( 'NONE', ( #16693 ), #21803, .F. ) ;
#11286 = CARTESIAN_POINT ( 'NONE',  ( 8.699089158774000907, 4.178200486578000472, -5.608493638783999202 ) ) ;
#11287 = CARTESIAN_POINT ( 'NONE',  ( 18.49969735796901205, 11.81669335334967386, -4.154069657518311587 ) ) ;
#11288 = CARTESIAN_POINT ( 'NONE',  ( 11.03407957707000087, -2.992853177526999975, -9.056567163506000995 ) ) ;
#11289 = ORIENTED_EDGE ( 'NONE', *, *, #40346, .F. ) ;
#11290 = CIRCLE ( 'NONE', #34776, 2.000000000000001332 ) ;
#11291 = CARTESIAN_POINT ( 'NONE',  ( 11.12988950457999948, 5.284594281680999650, -4.847983311486999902 ) ) ;
#11292 = LINE ( 'NONE', #32632, #38900 ) ;
#11293 = CARTESIAN_POINT ( 'NONE',  ( 18.00257402908058424, -3.100282954733041940, 13.65258486500941970 ) ) ;
#11294 = DIRECTION ( 'NONE',  ( 0.000000000000000000, 0.7071067811865474617, -0.7071067811865474617 ) ) ;
#11295 = CARTESIAN_POINT ( 'NONE',  ( 5.907109839683334584, 1.199500263597268246, 0.9218200799623752495 ) ) ;
#11296 = CARTESIAN_POINT ( 'NONE',  ( 11.67403632436368888, 3.023821283238099955, -7.272033745815799755 ) ) ;
#11297 = CARTESIAN_POINT ( 'NONE',  ( 9.280051052051998539, 4.985712601322500603, -7.692906630067099627 ) ) ;
#11299 = CARTESIAN_POINT ( 'NONE',  ( 4.399622670846948580, 1.399596316936216223, 0.4756535215918837878 ) ) ;
#11298 = CARTESIAN_POINT ( 'NONE',  ( 9.747734463322998977, -3.909687748588960066, 6.637705594503099604 ) ) ;
#11300 = DIRECTION ( 'NONE',  ( 0.000000000000000000, -0.9916377111174247139, 0.1290528957048031888 ) ) ;
#11301 = ORIENTED_EDGE ( 'NONE', *, *, #27930, .T. ) ;
#11302 = EDGE_CURVE ( 'NONE', #37325, #68067, #48559, .T. ) ;
#11303 = CARTESIAN_POINT ( 'NONE',  ( 11.17901463001529905, 4.697110652903200290, 8.616511311517999872 ) ) ;
#11304 = CLOSED_SHELL ( 'NONE', ( #30664, #35530, #45843, #30413, #59739, #52642, #56751, #64994, #41660, #7142, #20661, #44056, #66437, #53177, #51603, #22660, #31494, #41217, #14928, #13149, #3222, #8882, #50046, #21767, #39085, #59095, #55794, #58612, #45783, #51240, #26319, #26919, #54887, #11906, #11613, #58645, #26349, #40703, #22388, #7171, #9689, #9373 ) ) ;
#11305 = CARTESIAN_POINT ( 'NONE',  ( 8.164796825344000197, -3.457406484157000026, 6.165651553258999940 ) ) ;
#11306 = CARTESIAN_POINT ( 'NONE',  ( 9.304430433046999127, 2.911395389258000233, 8.171806809244198888 ) ) ;
#11307 = DIRECTION ( 'NONE',  ( 0.000000000000000000, 1.000000000000000000, 0.000000000000000000 ) ) ;
#11308 = B_SPLINE_CURVE_WITH_KNOTS ( 'NONE', 3,
 ( #52232, #35818, #40374, #56456 ),
 .UNSPECIFIED., .F., .F.,
 ( 4, 4 ),
 ( 0.000000000000000000, 1.000000000000000000 ),
 .UNSPECIFIED. ) ;
#11309 = CARTESIAN_POINT ( 'NONE',  ( 10.21608469020999976, -5.961703525007000515, 7.319668113368000384 ) ) ;
#11310 = CARTESIAN_POINT ( 'NONE',  ( 9.840770501363659051, -3.644193716302523089, 9.240192412087251839 ) ) ;
#11311 = CARTESIAN_POINT ( 'NONE',  ( 9.674373738639999942, -2.899999999999999911, -6.185493860157000867 ) ) ;
#11312 = CARTESIAN_POINT ( 'NONE',  ( 9.811963142879999822, -3.017187828228399926, -7.292822454528599785 ) ) ;
#11313 = CARTESIAN_POINT ( 'NONE',  ( 5.252930087360999423, -0.5918267827669999592, 1.016258213757999851 ) ) ;
#11314 = CARTESIAN_POINT ( 'NONE',  ( 10.97683719568448169, -3.813711395361371714, 8.354041075310609799 ) ) ;
#11315 = CARTESIAN_POINT ( 'NONE',  ( 11.49999672495000524, 4.789193247147742305, -10.68959786790916588 ) ) ;
#11316 = VERTEX_POINT ( 'NONE', #33484 ) ;
#11317 = CARTESIAN_POINT ( 'NONE',  ( 11.76902897915239876, -3.778278678798900447, 6.662660017635100296 ) ) ;
#11318 = CARTESIAN_POINT ( 'NONE',  ( 13.70003001321900271, -9.668726926528000476, -7.961868161445000425 ) ) ;
#11319 = CARTESIAN_POINT ( 'NONE',  ( 24.39664325317268734, 3.224866859135877117, -12.03536696594411914 ) ) ;
#11320 = CARTESIAN_POINT ( 'NONE',  ( 24.77999985543100081, -8.657366092043000450, 9.170186965892000330 ) ) ;
#11321 = DIRECTION ( 'NONE',  ( 0.000000000000000000, 0.01629188381079070894, -0.9998672784534433644 ) ) ;
#11322 = ORIENTED_EDGE ( 'NONE', *, *, #21785, .T. ) ;
#11323 = CARTESIAN_POINT ( 'NONE',  ( 24.87547883224999978, -11.55042359755999826, -3.247369794756999717 ) ) ;
#11324 = PRODUCT_CONTEXT ( 'NONE', #24408, 'mechanical' ) ;
#11325 = CARTESIAN_POINT ( 'NONE',  ( 10.77879632507499785, -3.576455950783300253, -8.285174533868300273 ) ) ;
#11326 = CARTESIAN_POINT ( 'NONE',  ( 18.04063798880599379, 0.3934994371746786679, 12.69179478355544255 ) ) ;
#11327 = CARTESIAN_POINT ( 'NONE',  ( 11.29996849689000271, 12.23272706294999956, 1.505586356912999912 ) ) ;
#11328 = CARTESIAN_POINT ( 'NONE',  ( 10.68360729283125465, 2.821290678667913276, 8.178873955024702269 ) ) ;
#11329 = DIRECTION ( 'NONE',  ( -1.000000000000000000, 0.000000000000000000, 0.000000000000000000 ) ) ;
#11330 = ORIENTED_EDGE ( 'NONE', *, *, #33500, .T. ) ;
#11331 = CARTESIAN_POINT ( 'NONE',  ( 10.69031285273999821, -5.903020122789000013, 7.830708506196000229 ) ) ;
#11332 = LINE ( 'NONE', #10997, #45636 ) ;
#11333 = ORIENTED_EDGE ( 'NONE', *, *, #43007, .T. ) ;
#11334 = LINE ( 'NONE', #64810, #57413 ) ;
#11335 = CARTESIAN_POINT ( 'NONE',  ( 8.289120559623999185, -4.310353212080000773, 9.459493062793997709 ) ) ;
#11336 = CARTESIAN_POINT ( 'NONE',  ( 8.142589158771000868, 5.074768364528000397, -8.296267706722000312 ) ) ;
#11337 = EDGE_CURVE ( 'NONE', #38413, #31036, #5215, .T. ) ;
#11338 = EDGE_LOOP ( 'NONE', ( #13904, #36654, #68852, #33894 ) ) ;
#11339 = CARTESIAN_POINT ( 'NONE',  ( 23.59999193302000364, -13.22318594659000013, 4.267778254689999606 ) ) ;
#11340 = ADVANCED_FACE ( 'NONE', ( #8966 ), #66662, .F. ) ;
#11341 = CIRCLE ( 'NONE', #67033, 0.4999999999999997224 ) ;
#11342 = CARTESIAN_POINT ( 'NONE',  ( 7.961735841224999000, 4.624432025063999419, -9.294334464733999823 ) ) ;
#11343 = CYLINDRICAL_SURFACE ( 'NONE', #34257, 1.250000000000000222 ) ;
#11344 = ADVANCED_FACE ( 'NONE', ( #61081, #45009 ), #8626, .T. ) ;
#11345 = CARTESIAN_POINT ( 'NONE',  ( 8.153325607601846770, -3.117005381769989647, 6.262142143703084862 ) ) ;
#11346 = ORIENTED_EDGE ( 'NONE', *, *, #6289, .F. ) ;
#11347 = CARTESIAN_POINT ( 'NONE',  ( 10.65550933554000146, -4.237674644795000667, 9.105223721671999115 ) ) ;
#11348 = EDGE_CURVE ( 'NONE', #31306, #6106, #6072, .T. ) ;
#11349 = DIRECTION ( 'NONE',  ( 0.000000000000000000, 0.000000000000000000, 1.000000000000000000 ) ) ;
#11350 = ORIENTED_EDGE ( 'NONE', *, *, #53705, .T. ) ;
#11351 = CARTESIAN_POINT ( 'NONE',  ( 6.055026506350000837, -1.500000000000000000, 0.000000000000000000 ) ) ;
#11352 = CARTESIAN_POINT ( 'NONE',  ( 11.09999999999999964, 2.899999999999999911, -4.467422426380999845 ) ) ;
#11353 = ORIENTED_EDGE ( 'NONE', *, *, #26753, .T. ) ;
#11354 = CARTESIAN_POINT ( 'NONE',  ( 9.254721904869999349, 4.875830726371099821, 7.008306153105300140 ) ) ;
#11355 = CARTESIAN_POINT ( 'NONE',  ( 17.60324462842607929, -1.762109595560080066, -12.47617631420775197 ) ) ;
#11356 = CARTESIAN_POINT ( 'NONE',  ( 4.340135294409000366, 0.2980381316198000285, 1.384766116913999978 ) ) ;
#11357 = AXIS2_PLACEMENT_3D ( 'NONE', #49458, #54358, #12063 ) ;
#11358 = CARTESIAN_POINT ( 'NONE',  ( 11.60000000000000142, 3.430179236374871099, -6.730205196242793342 ) ) ;
#11359 = CARTESIAN_POINT ( 'NONE',  ( 24.68353902991545468, 11.80738835872714176, -3.191231336988252565 ) ) ;
#11360 = CARTESIAN_POINT ( 'NONE',  ( 11.49999035076000276, -3.886252136122000156, 11.90689009355000039 ) ) ;
#11361 = DIRECTION ( 'NONE',  ( 0.000000000000000000, 0.9553735099700839672, -0.2954005017724949389 ) ) ;
#11362 = CARTESIAN_POINT ( 'NONE',  ( 13.21911358530772773, -12.38522838340864851, -1.866030466704243551 ) ) ;
#11363 = ORIENTED_EDGE ( 'NONE', *, *, #66913, .T. ) ;
#11364 = CARTESIAN_POINT ( 'NONE',  ( 10.07770645819999977, 4.622041375574999833, 5.671348593713000596 ) ) ;
#11365 = B_SPLINE_CURVE_WITH_KNOTS ( 'NONE', 3,
 ( #41200, #14965, #63186, #3776 ),
 .UNSPECIFIED., .F., .F.,
 ( 4, 4 ),
 ( 0.000000000000000000, 1.000000000000000000 ),
 .UNSPECIFIED. ) ;
#11366 = CARTESIAN_POINT ( 'NONE',  ( 17.79663207835866956, -11.53878384028511306, 4.871562533345485946 ) ) ;
#11367 = CARTESIAN_POINT ( 'NONE',  ( 12.80505043854143388, 3.124999999999999556, -13.52084414783465505 ) ) ;
#11368 = CARTESIAN_POINT ( 'NONE',  ( 9.221802827889732157, 2.874603711573444187, 6.749639981083119800 ) ) ;
#11369 = CARTESIAN_POINT ( 'NONE',  ( 10.15402496696000156, -5.267980706381999667, 5.992344456606999437 ) ) ;
#11370 = CARTESIAN_POINT ( 'NONE',  ( 17.93599053679681887, -0.4959091552601235242, 13.88809952003718351 ) ) ;
#11371 = CARTESIAN_POINT ( 'NONE',  ( 25.58980475334900362, -2.739986445787999436, 11.22452250057999912 ) ) ;
#11372 = VERTEX_POINT ( 'NONE', #44672 ) ;
#11373 = EDGE_LOOP ( 'NONE', ( #57939, #22315, #27172, #17037 ) ) ;
#11374 = CARTESIAN_POINT ( 'NONE',  ( 12.57406875486398867, 0.5808247544327472811, 13.88366201036104641 ) ) ;
#11375 = CARTESIAN_POINT ( 'NONE',  ( 12.80505043854144276, -0.6250000000000001110, -13.88107975066922428 ) ) ;
#11376 = CARTESIAN_POINT ( 'NONE',  ( 9.820206362952999868, -3.883324525498000224, 6.055606607331999847 ) ) ;
#11377 = CARTESIAN_POINT ( 'NONE',  ( 17.85613310409923216, -0.5477939754333960298, -13.88547043407233694 ) ) ;
#11378 = CARTESIAN_POINT ( 'NONE',  ( 7.149102686541000118, -4.351670788182000038, 8.977200644264000218 ) ) ;
#11379 = CARTESIAN_POINT ( 'NONE',  ( 8.751496707488000126, 4.081676005979390176, -8.356402621895700378 ) ) ;
#11381 = CARTESIAN_POINT ( 'NONE',  ( 17.74639017890714499, 11.23193386242191139, -3.094113022443028882 ) ) ;
#11380 = CARTESIAN_POINT ( 'NONE',  ( 11.07088779216199903, -2.816792857868000155, 7.073306690476799830 ) ) ;
#11382 = CARTESIAN_POINT ( 'NONE',  ( 11.50271932425157040, 3.812601581225100400, -8.764198628556998827 ) ) ;
#11383 = AXIS2_PLACEMENT_3D ( 'NONE', #17270, #29159, #7466 ) ;
#11384 = CARTESIAN_POINT ( 'NONE',  ( 12.09999999999999964, -4.831023649631406514, 7.002620348270789385 ) ) ;
#11385 = ADVANCED_FACE ( 'NONE', ( #35550 ), #40078, .T. ) ;
#11386 = DIRECTION ( 'NONE',  ( -1.000000000000000000, 0.000000000000000000, 0.000000000000000000 ) ) ;
#11387 = CARTESIAN_POINT ( 'NONE',  ( 17.57569811463524445, -0.6249994333735310326, 12.67928921956170996 ) ) ;
#11388 = CARTESIAN_POINT ( 'NONE',  ( 10.35685100253999913, -2.832432432432000269, -6.822293592207000934 ) ) ;
#11389 = EDGE_CURVE ( 'NONE', #19719, #58783, #45695, .T. ) ;
#11390 = CARTESIAN_POINT ( 'NONE',  ( 24.23233723912900217, 9.064763380006999327, 9.162364161575000665 ) ) ;
#11391 = VERTEX_POINT ( 'NONE', #24018 ) ;
#11392 = CARTESIAN_POINT ( 'NONE',  ( 9.368918146792999835, -5.618388245857000030, 7.727743016644000207 ) ) ;
#11393 = CARTESIAN_POINT ( 'NONE',  ( 8.424364158774000799, 3.292387953886000140, -6.294868737226000377 ) ) ;
#11394 = DIRECTION ( 'NONE',  ( -1.000000000000000000, 0.000000000000000000, 0.000000000000000000 ) ) ;
#11395 = CARTESIAN_POINT ( 'NONE',  ( 9.112942518363999156, -5.100000000000000533, 6.192000867487999827 ) ) ;
#11396 = AXIS2_PLACEMENT_3D ( 'NONE', #67178, #3550, #35723 ) ;
#11397 = CARTESIAN_POINT ( 'NONE',  ( 0.3871700897145999853, -0.5648807336705999882, -3.658284285490000176 ) ) ;
#11398 = CARTESIAN_POINT ( 'NONE',  ( 10.48791429142999831, 4.016993441347180394, 8.391963954669400039 ) ) ;
#11399 = AXIS2_PLACEMENT_3D ( 'NONE', #49911, #2363, #61092 ) ;
#11400 = CARTESIAN_POINT ( 'NONE',  ( 1.980200647714000173, 3.111577884474999500, -2.108416590332999885 ) ) ;
#11401 = EDGE_LOOP ( 'NONE', ( #63628, #27117, #5673, #10197 ) ) ;
#11402 = CARTESIAN_POINT ( 'NONE',  ( 12.38296014331786843, -0.5849390254007856838, -12.58641711472857772 ) ) ;
#11403 = CARTESIAN_POINT ( 'NONE',  ( 11.59999999999999964, -4.000000000000000000, -7.500000000000000000 ) ) ;
#11404 = CARTESIAN_POINT ( 'NONE',  ( 18.17205452211569749, 2.859046691836176546, -12.27135926524918474 ) ) ;
#11405 = CARTESIAN_POINT ( 'NONE',  ( 5.642739276337785270, 12.09235441392603150, 3.739144582074417578 ) ) ;
#11406 = CARTESIAN_POINT ( 'NONE',  ( 8.860767219592000643, 2.935741164366000522, 6.259844213126999790 ) ) ;
#11407 = EDGE_LOOP ( 'NONE', ( #49502, #56631, #16574, #52617 ) ) ;
#11408 = CARTESIAN_POINT ( 'NONE',  ( 6.587045118934000243, -1.528745275297999973, -0.5198780721924000092 ) ) ;
#11409 = B_SPLINE_CURVE_WITH_KNOTS ( 'NONE', 3,
 ( #7823, #29160, #7128, #66540, #44891, #60272, #28466, #65150, #12027, #49780, #23210, #66195, #60616, #18659, #65502, #39640, #44558, #1538 ),
 .UNSPECIFIED., .F., .F.,
 ( 4, 2, 2, 2, 2, 2, 2, 2, 4 ),
 ( 0.000000000000000000, 0.1250000000000000000, 0.2500000000000000000, 0.3750000000000000000, 0.5000000000000000000, 0.6250000000000000000, 0.7500000000000000000, 0.8750000000000000000, 1.000000000000000000 ),
 .UNSPECIFIED. ) ;
#11410 = CARTESIAN_POINT ( 'NONE',  ( 7.250820280410000152, 2.436157974829999961, -7.440523950196999969 ) ) ;
#11411 = CARTESIAN_POINT ( 'NONE',  ( 8.541164872330046620, -3.301241083931813591, 5.907377702369386085 ) ) ;
#11412 = CARTESIAN_POINT ( 'NONE',  ( 13.70003001321900271, 9.668726926528000476, 7.961868161445000425 ) ) ;
#11413 = ORIENTED_EDGE ( 'NONE', *, *, #43505, .T. ) ;
#11414 = CARTESIAN_POINT ( 'NONE',  ( 24.30000000000000071, 11.77655473258999841, 4.190794510628000680 ) ) ;
#11415 = CARTESIAN_POINT ( 'NONE',  ( 6.334193173016667622, 1.460959015002474048, -0.3926218265389178064 ) ) ;
#11416 = VERTEX_POINT ( 'NONE', #67338 ) ;
#11417 = CARTESIAN_POINT ( 'NONE',  ( 24.76777373405924720, 3.098484992731120435, -11.74891855520822403 ) ) ;
#11418 = CARTESIAN_POINT ( 'NONE',  ( 11.08810207955139937, 3.203462856645999945, 7.825000000000000178 ) ) ;
#11419 = CARTESIAN_POINT ( 'NONE',  ( 17.57569738523962144, -0.6249994334955764064, -13.88107975403457495 ) ) ;
#11420 = ORIENTED_EDGE ( 'NONE', *, *, #4466, .F. ) ;
#11421 = CARTESIAN_POINT ( 'NONE',  ( 15.86547101025739792, -8.701845401024742799, -7.746061882572572443 ) ) ;
#11422 = EDGE_CURVE ( 'NONE', #33943, #40655, #6958, .T. ) ;
#11423 = CARTESIAN_POINT ( 'NONE',  ( 10.98768472638000127, 7.408460511344000743, 6.159405790617999976 ) ) ;
#11424 = CARTESIAN_POINT ( 'NONE',  ( 10.73724174883999893, 3.975468761016990094, -8.391788556008700439 ) ) ;
#11425 = DIRECTION ( 'NONE',  ( 0.000000000000000000, -0.7158784314710772145, -0.6982249432342778617 ) ) ;
#11426 = EDGE_CURVE ( 'NONE', #17729, #17206, #40434, .T. ) ;
#11427 = CARTESIAN_POINT ( 'NONE',  ( 11.28887616594230003, -4.386455737425299262, 8.718182393403999697 ) ) ;
#11428 = VERTEX_POINT ( 'NONE', #51277 ) ;
#11429 = CARTESIAN_POINT ( 'NONE',  ( 9.079732780410999737, 5.421534627450999899, 6.381126373995999579 ) ) ;
#11430 = EDGE_CURVE ( 'NONE', #10178, #47578, #6567, .T. ) ;
#11431 = ORIENTED_EDGE ( 'NONE', *, *, #23060, .F. ) ;
#11432 = CARTESIAN_POINT ( 'NONE',  ( 16.09992084546400193, 8.991497430826001391, 8.719551690569000257 ) ) ;
#11433 = CARTESIAN_POINT ( 'NONE',  ( 15.45446786537200090, -9.133287421996001854, -8.216743560820999548 ) ) ;
#11434 = CARTESIAN_POINT ( 'NONE',  ( 11.07202612390000063, 6.387422431570000114, -5.354923180025000562 ) ) ;
#11435 = ORIENTED_EDGE ( 'NONE', *, *, #20125, .T. ) ;
#11436 = CARTESIAN_POINT ( 'NONE',  ( 12.37468788209173809, -2.046657606614539660, -12.54569895759545517 ) ) ;
#11437 = CARTESIAN_POINT ( 'NONE',  ( 0.4068495934470809372, -2.724938773265916492, -2.093043791803330222 ) ) ;
#11438 = CARTESIAN_POINT ( 'NONE',  ( 8.383148997457999130, 5.167567567567999731, 6.822293592207000934 ) ) ;
#11439 = DIRECTION ( 'NONE',  ( 0.000000000000000000, -0.9835907196275001096, -0.1804142351995999538 ) ) ;
#11440 = CARTESIAN_POINT ( 'NONE',  ( 12.22832816813801315, -2.961039467707567319, -13.68329631872640917 ) ) ;
#11441 = B_SPLINE_CURVE_WITH_KNOTS ( 'NONE', 3,
 ( #5865, #37344, #21943, #59352 ),
 .UNSPECIFIED., .F., .F.,
 ( 4, 4 ),
 ( 0.000000000000000000, 1.000000000000000000 ),
 .UNSPECIFIED. ) ;
#11442 = CARTESIAN_POINT ( 'NONE',  ( 10.47718582084299932, -4.656536239972400182, -6.741111985563299491 ) ) ;
#11443 = CARTESIAN_POINT ( 'NONE',  ( 5.888359839683998231, 0.7554284705563452107, 1.310679582531388609 ) ) ;
#11444 = CARTESIAN_POINT ( 'NONE',  ( 17.86958940788779771, -3.040180081688693470, 12.30916660591379674 ) ) ;
#11445 = ORIENTED_EDGE ( 'NONE', *, *, #47919, .F. ) ;
#11446 = CARTESIAN_POINT ( 'NONE',  ( 11.18412378248529926, -4.549028353065900809, -6.461285588983000316 ) ) ;
#11447 = ORIENTED_EDGE ( 'NONE', *, *, #66781, .T. ) ;
#11448 = EDGE_CURVE ( 'NONE', #1716, #16591, #7681, .T. ) ;
#11449 = VECTOR ( 'NONE', #21248, 1000.000000000000000 ) ;
#11450 = CARTESIAN_POINT ( 'NONE',  ( 11.44438160092000167, -12.37754422778999874, -1.524124373512000030 ) ) ;
#11451 = CARTESIAN_POINT ( 'NONE',  ( 8.748814158775001459, 5.251032986819000214, -6.070151079272999795 ) ) ;
#11452 = CARTESIAN_POINT ( 'NONE',  ( 10.28774346735000123, 5.077605961126000267, -5.991341245382999503 ) ) ;
#11453 = CARTESIAN_POINT ( 'NONE',  ( 0.1500002361980000143, -2.725000000000000089, 0.000000000000000000 ) ) ;
#11454 = CARTESIAN_POINT ( 'NONE',  ( 10.90000000016000037, -5.167567554889999748, 6.822293570050000255 ) ) ;
#11455 = CARTESIAN_POINT ( 'NONE',  ( 24.38452416568300052, 12.23040738833000063, 3.201157652712999901 ) ) ;
#11456 = CARTESIAN_POINT ( 'NONE',  ( 10.13049857835000012, 3.092060693447000297, 8.629378633793999498 ) ) ;
#11457 = EDGE_LOOP ( 'NONE', ( #62556, #28157, #22428, #32132 ) ) ;
#11458 = FACE_OUTER_BOUND ( 'NONE', #36302, .T. ) ;
#11459 = CARTESIAN_POINT ( 'NONE',  ( 9.538432183420001209, 5.620896541217999420, 7.423100299691999915 ) ) ;
#11460 = CARTESIAN_POINT ( 'NONE',  ( 10.07314899745999881, -5.167567567567999731, -6.822293592207000934 ) ) ;
#11461 = CARTESIAN_POINT ( 'NONE',  ( 11.68923293495519999, -5.032672437899000428, 7.541513160549049744 ) ) ;
#11462 = CARTESIAN_POINT ( 'NONE',  ( 5.500000000000000000, 12.78667792605000031, -2.345384795462000405 ) ) ;
#11463 = CARTESIAN_POINT ( 'NONE',  ( 11.19518313518939934, 3.462699341914400097, -8.179416362154199760 ) ) ;
#11464 = CARTESIAN_POINT ( 'NONE',  ( 7.100000000000168399, 3.318691773287608449, -8.707120243254404812 ) ) ;
#11465 = CARTESIAN_POINT ( 'NONE',  ( 23.95224662109200153, -9.460740396185999046, -9.410539229647000070 ) ) ;
#11466 = DIRECTION ( 'NONE',  ( 0.000000000000000000, 0.000000000000000000, -1.000000000000000000 ) ) ;
#11467 = LINE ( 'NONE', #59716, #46681 ) ;
#11468 = EDGE_CURVE ( 'NONE', #13653, #51766, #15509, .T. ) ;
#11469 = B_SPLINE_SURFACE_WITH_KNOTS ( 'NONE', 3, 3, ( 
 ( #27555, #64600, #16025, #16708, #5192, #4842, #53092, #26183, #10777, #59363, #42270, #32124, #37020, #47509, #63574, #58332, #644, #5536, #26530, #37354, #47857, #69164, #21274, #63914, #26876, #16368, #53440, #53778, #11463, #48191, #293, #64255, #21613, #39428, #2366, #65294, #7957, #55160, #6568, #7264, #17766, #60747, #17411, #43990, #13217, #28958, #55508, #18450, #1677, #28604, #23688, #12862, #29296, #34542, #50607, #45023, #64939, #2709, #43642, #39084, #55855, #17053, #33152, #1327, #38386, #39776, #49914 ),
 ( #59711, #23345, #11811, #65981, #7610, #34192, #54468, #27910, #49219, #50261, #22645, #38735, #66329, #6913, #60064, #12168, #61095, #33499, #54813, #28247, #49567, #22993, #44343, #44689, #65640, #60407, #12513, #33844, #2028, #18108, #13559, #30320, #31007, #9661, #14237, #51629, #8980, #51290, #25061, #41487, #3046, #3724, #13897, #50950, #29647, #18799, #67696, #56882, #40796, #9315, #68045, #19474, #41151, #62119, #35566, #46392, #40451, #61776, #46739, #24379, #3387, #45709, #67018, #66675, #24033, #62797, #24723 ),
 ( #19820, #19126, #34876, #14918, #57213, #46048, #62460, #67354, #35224, #20160, #14580, #35897, #30656, #51966, #4067, #25403, #36241, #57557, #45367, #40127, #56195, #56536, #8640, #52321, #61439, #8302, #29991, #20504, #32042, #31691, #26796, #32724, #43209, #5460, #26099, #10695, #15607, #47425, #53699, #64512, #58251, #53357, #4758, #63136, #16632, #37612, #5109, #48111, #26446, #31348, #563, #211, #21532, #42864, #37273, #64173, #53013, #16287, #58943, #20851, #42184, #11050, #5793, #32386, #27135, #68732, #37960 ),
 ( #63487, #48455, #15945, #36938, #47777, #59280, #11382, #10011, #4415, #21872, #25753, #10356, #69085, #47082, #68384, #41830, #15263, #36586, #57912, #52661, #21191, #42521, #63830, #58595, #65904, #34111, #22565, #33417, #49834, #27476, #48801, #33765, #23605, #7186, #18032, #23266, #61016, #18373, #54035, #39347, #39695, #6137, #60668, #17327, #910, #64860, #55430, #22223, #13134, #43560, #12782, #7521, #54735, #55081, #16971, #38303, #59632, #11726, #33068, #2287, #54384, #60326, #6485, #27834, #44264, #12434, #39008 ) ),
 .UNSPECIFIED., .F., .F., .F.,
 ( 4, 4 ),
 ( 4, 1, 1, 1, 1, 1, 1, 1, 1, 1, 1, 1, 1, 1, 1, 1, 1, 1, 1, 1, 1, 1, 1, 1, 1, 1, 1, 1, 1, 1, 1, 1, 1, 1, 1, 1, 1, 1, 1, 1, 1, 1, 1, 1, 1, 1, 1, 1, 1, 1, 1, 1, 1, 1, 1, 1, 1, 1, 1, 1, 1, 1, 1, 1, 4 ),
 ( -0.02000000000000000042, 1.020000000000000018 ),
 ( 0.008747244164287000176, 0.02453926110774999961, 0.04033127805120999970, 0.05612329499467000327, 0.07191531193812999989, 0.08770732888158999652, 0.1034993458251000087, 0.1192913627684999978, 0.1350833797120000179, 0.1508753966553999792, 0.1666674135988999994, 0.1824594305423999918, 0.1982514474858000086, 0.2140434644293000011, 0.2298354813727000179, 0.2456274983162000103, 0.2614195152596999749, 0.2772115322030999640, 0.2930035491465999842, 0.3087955660900000288, 0.3245875830334999934, 0.3403795999769999581, 0.3561716169204000026, 0.3719636338639000228, 0.3877556508073999875, 0.4035476677507999765, 0.4193396846942999967, 0.4351317016376999858, 0.4509237185811999504, 0.4667157355247000261, 0.4825077524681000152, 0.4982997694115999798, 0.5140917863550000799, 0.5298838032985000446, 0.5456758202420000092, 0.5614678371854000538, 0.5772598541289000185, 0.5930518710723000630, 0.6088438880158000277, 0.6246359049592999924, 0.6404279219027000369, 0.6562199388462000016, 0.6720119557896999662, 0.6878039727331000108, 0.7035959896765999755, 0.7193880066200000201, 0.7351800235634999847, 0.7509720405069999494, 0.7667640574504001050, 0.7825560743939000696, 0.7983480913373000032, 0.8141401082808000789, 0.8299321252243000435, 0.8457241421676999771, 0.8615161591112000528, 0.8773081760545999863, 0.8931001929981000620, 0.9088922099416000266, 0.9246842268849999602, 0.9404762438285000359, 0.9562682607720000005, 0.9720602777153999341, 0.9878522946589000098, 1.003644311601999961, 1.019436328545999970 ),
 .UNSPECIFIED. ) ;
#11470 = ORIENTED_EDGE ( 'NONE', *, *, #33144, .T. ) ;
#11471 = CARTESIAN_POINT ( 'NONE',  ( 7.100000000000000533, 12.50865771883999855, -2.924687089724999911 ) ) ;
#11472 = CARTESIAN_POINT ( 'NONE',  ( 7.360157189579999759, -0.4795858584850000161, 1.282035055333999862 ) ) ;
#11473 = CARTESIAN_POINT ( 'NONE',  ( 18.02766551172499376, 2.090896903265579976, 13.75171326662667504 ) ) ;
#11474 = CARTESIAN_POINT ( 'NONE',  ( 24.40777907822999993, 8.879621479992000133, -9.005112135964999709 ) ) ;
#11475 = B_SPLINE_CURVE_WITH_KNOTS ( 'NONE', 3,
 ( #40287, #14411, #56714, #45874, #13721, #67526, #3221, #68207, #67872, #29471, #34706, #24550, #45538, #66847, #50780, #19296 ),
 .UNSPECIFIED., .F., .F.,
 ( 4, 2, 2, 2, 2, 2, 2, 4 ),
 ( 0.1254282067584606419, 0.2190722812470546343, 0.3127163557356486545, 0.4063604302242426192, 0.5000045047128366393, 0.6872926536900242356, 0.7809367281786182557, 0.8745808026672123869 ),
 .UNSPECIFIED. ) ;
#11476 = CARTESIAN_POINT ( 'NONE',  ( 10.54272335273199879, -3.555125495332600138, -8.698083075453000745 ) ) ;
#11477 = ORIENTED_EDGE ( 'NONE', *, *, #39965, .T. ) ;
#11478 = CARTESIAN_POINT ( 'NONE',  ( 24.30000000000000071, -8.810505093353000916, 8.810505093353000916 ) ) ;
#11479 = CARTESIAN_POINT ( 'NONE',  ( 8.218892219592001780, 3.011620138462000273, 8.801434747080000065 ) ) ;
#11481 = CARTESIAN_POINT ( 'NONE',  ( 10.61094409420999973, 5.100000000000000533, -6.571291218949999902 ) ) ;
#11480 = CARTESIAN_POINT ( 'NONE',  ( 8.175739158770999992, 4.686731264770999772, -8.717075579553000608 ) ) ;
#11482 = CARTESIAN_POINT ( 'NONE',  ( 25.46373024410000241, -11.23407150414000100, 3.161076981347000103 ) ) ;
#11483 = VERTEX_POINT ( 'NONE', #67679 ) ;
#11484 = CARTESIAN_POINT ( 'NONE',  ( 11.03856029907000114, 2.974095820320000083, 8.716122353065999917 ) ) ;
#11485 = CARTESIAN_POINT ( 'NONE',  ( 18.27121482242689865, -2.402104771923907034, -13.79240553248645718 ) ) ;
#11486 = CARTESIAN_POINT ( 'NONE',  ( 10.32949413291699869, 4.912929163218899831, 7.916546720849799712 ) ) ;
#11487 = CARTESIAN_POINT ( 'NONE',  ( 10.62792628238999981, -3.100579357212000176, 8.599905962393000536 ) ) ;
#11488 = CARTESIAN_POINT ( 'NONE',  ( 7.428092358015002006, 3.524408735919001501, 6.653372890553997721 ) ) ;
#11489 = ORIENTED_EDGE ( 'NONE', *, *, #24621, .F. ) ;
#11490 = CARTESIAN_POINT ( 'NONE',  ( 24.44916829770000177, 12.41483723393999838, -3.103225306172999964 ) ) ;
#11492 = CARTESIAN_POINT ( 'NONE',  ( 11.28109314679000086, -2.660122028910999692, -6.904120269057000492 ) ) ;
#11491 = CARTESIAN_POINT ( 'NONE',  ( 12.79413755118400253, -11.93226572510000061, 3.260039893805000144 ) ) ;
#11493 = CARTESIAN_POINT ( 'NONE',  ( 7.776208646924445134, -4.986279724221044596, 8.933337815283831418 ) ) ;
#11494 = AXIS2_PLACEMENT_3D ( 'NONE', #67736, #35264, #51333 ) ;
#11495 = CARTESIAN_POINT ( 'NONE',  ( 9.442841440870999747, -2.691258483914000355, 6.269525829285999663 ) ) ;
#11496 = CARTESIAN_POINT ( 'NONE',  ( 11.84388784977539899, -5.255745690988000263, -7.428242901739219306 ) ) ;
#11497 = ORIENTED_EDGE ( 'NONE', *, *, #42141, .T. ) ;
#11498 = DIRECTION ( 'NONE',  ( -1.000000000000000000, 0.000000000000000000, 0.000000000000000000 ) ) ;
#11499 = CARTESIAN_POINT ( 'NONE',  ( 11.00180110216400031, -4.856393875115199599, 8.023010882787499298 ) ) ;
#11500 = CARTESIAN_POINT ( 'NONE',  ( 8.434803823919004628, 2.901237182992001173, 6.624660446101000133 ) ) ;
#11501 = CARTESIAN_POINT ( 'NONE',  ( 11.57656516821460890, 4.899536366368299589, 6.592171857671999646 ) ) ;
#11502 = ORIENTED_EDGE ( 'NONE', *, *, #27535, .F. ) ;
#11503 = CARTESIAN_POINT ( 'NONE',  ( 9.667489158770999680, 4.808846957865000604, -8.639578604182998944 ) ) ;
#11504 = CARTESIAN_POINT ( 'NONE',  ( 12.15953697780016540, 2.808329718129376928, -12.28305324893824668 ) ) ;
#11505 = EDGE_CURVE ( 'NONE', #66731, #41719, #46958, .T. ) ;
#11506 = CARTESIAN_POINT ( 'NONE',  ( 11.39324174884020024, -4.032306468273969990, 6.325557131097000685 ) ) ;
#11507 = EDGE_CURVE ( 'NONE', #58173, #66927, #52998, .T. ) ;
#11508 = CARTESIAN_POINT ( 'NONE',  ( 9.064883232718324635, 5.349954811645839747, -7.500006748065883855 ) ) ;
#11509 = DIRECTION ( 'NONE',  ( 1.000000000000000000, 0.000000000000000000, 0.000000000000000000 ) ) ;
#11510 = ORIENTED_EDGE ( 'NONE', *, *, #17755, .F. ) ;
#11511 = CARTESIAN_POINT ( 'NONE',  ( 9.202754440379999679, -2.542850487891999745, 7.419808283050000064 ) ) ;
#11512 = CARTESIAN_POINT ( 'NONE',  ( 9.323602683899247623, -5.219044746006709978, -7.180752970636812726 ) ) ;
#11513 = VERTEX_POINT ( 'NONE', #5094 ) ;
#11514 = CARTESIAN_POINT ( 'NONE',  ( 12.48183889708585426, -3.124385432114249461, -12.20648365185189022 ) ) ;
#11515 = CARTESIAN_POINT ( 'NONE',  ( 11.24025954179439957, 4.771812902496799680, 6.858707791728399172 ) ) ;
#11516 = DIRECTION ( 'NONE',  ( -1.000000000000000000, 0.000000000000000000, 5.204170427930416866E-14 ) ) ;
#11517 = CARTESIAN_POINT ( 'NONE',  ( 10.97216345308000029, 2.857785899823000353, -4.994019200607999309 ) ) ;
#11518 = FACE_OUTER_BOUND ( 'NONE', #30206, .T. ) ;
#11519 = CARTESIAN_POINT ( 'NONE',  ( 10.74600376124999990, -5.242711034443999552, 8.978690688221998784 ) ) ;
#11520 = CARTESIAN_POINT ( 'NONE',  ( 13.99955778315600163, 9.394084143528001363, 8.201088258230999628 ) ) ;
#11521 = CARTESIAN_POINT ( 'NONE',  ( 17.95947714806422368, 0.4766234715920644738, -12.68796191786314154 ) ) ;
#11522 = CARTESIAN_POINT ( 'NONE',  ( 12.21202437720863010, 2.301604982166983948, -12.49562318899369018 ) ) ;
#11523 = CARTESIAN_POINT ( 'NONE',  ( 10.76841504065829902, -3.085489673376300424, -6.818119527508899935 ) ) ;
#11524 = CARTESIAN_POINT ( 'NONE',  ( 7.802017219589999719, 5.638704226117999596, 8.266404648244000342 ) ) ;
#11525 = VERTEX_POINT ( 'NONE', #30993 ) ;
#11526 = VECTOR ( 'NONE', #6619, 1000.000000000000000 ) ;
#11527 = ADVANCED_FACE ( 'NONE', ( #68716 ), #30642, .F. ) ;
#11528 = AXIS2_PLACEMENT_3D ( 'NONE', #55435, #24302, #39353 ) ;
#11529 = CARTESIAN_POINT ( 'NONE',  ( 11.59999999999999787, -3.261098123302579754, -8.470724288896150256 ) ) ;
#11530 = CARTESIAN_POINT ( 'NONE',  ( 9.769471092180999960, 5.100000000000000533, -6.152188490330000370 ) ) ;
#11531 = FACE_OUTER_BOUND ( 'NONE', #45918, .T. ) ;
#11532 = ADVANCED_FACE ( 'NONE', ( #26429 ), #36570, .F. ) ;
#11533 = CARTESIAN_POINT ( 'NONE',  ( 18.24677884388063021, 2.264233918701648474, 12.39489312188808334 ) ) ;
#11534 = DIRECTION ( 'NONE',  ( 0.000000000000000000, -1.000000000000000000, 0.000000000000000000 ) ) ;
#11535 = CARTESIAN_POINT ( 'NONE',  ( 10.95622765495000195, 9.844278095421000074, 5.755901431881000008 ) ) ;
#11536 = CARTESIAN_POINT ( 'NONE',  ( 10.28414136986962646, -3.576408136849907216, 6.734426879786121312 ) ) ;
#11537 = CARTESIAN_POINT ( 'NONE',  ( 25.59997295081500113, -11.07537799752999952, 3.096069084855000320 ) ) ;
#11538 = EDGE_LOOP ( 'NONE', ( #30026, #9307 ) ) ;
#11539 = CARTESIAN_POINT ( 'NONE',  ( 12.07997135281821954, -2.506142839463719962, 12.34827158344147335 ) ) ;
#11540 = CARTESIAN_POINT ( 'NONE',  ( 9.857646554150999663, -3.513729974241599940, -8.378853663802400931 ) ) ;
#11541 = CARTESIAN_POINT ( 'NONE',  ( 9.903950872528001881, 5.205009505618999555, 6.747225973806000532 ) ) ;
#11542 = CARTESIAN_POINT ( 'NONE',  ( 8.304100344616170304, 2.916767839732335776, -6.503809950610432544 ) ) ;
#11543 = CONICAL_SURFACE ( 'NONE', #3708, 1.150084366271999725, 0.7854618604935084125 ) ;
#11544 = CARTESIAN_POINT ( 'NONE',  ( 10.87103032197929942, 4.583685623598699799, -6.683751296690399357 ) ) ;
#11545 = CARTESIAN_POINT ( 'NONE',  ( 12.13954479299509615, -0.2856017019952157288, 12.59676745213710625 ) ) ;
#11546 = AXIS2_PLACEMENT_3D ( 'NONE', #26511, #20570, #58663 ) ;
#11547 = CARTESIAN_POINT ( 'NONE',  ( 8.791232780412000736, 5.095085596809999728, 6.286981168432999922 ) ) ;
#11548 = CARTESIAN_POINT ( 'NONE',  ( 17.55505043854143565, 1.787797342887044394, 13.88538010501570952 ) ) ;
#11549 = CARTESIAN_POINT ( 'NONE',  ( 12.19026796737403195, 2.613005292445991223, 12.42452312575879070 ) ) ;
#11550 = CARTESIAN_POINT ( 'NONE',  ( 17.79999999998900151, -3.595165934733000057, -11.99793354950999991 ) ) ;
#11551 = CARTESIAN_POINT ( 'NONE',  ( 10.37457053952199892, 3.551693493661699730, -6.451042711717000167 ) ) ;
#11552 = CARTESIAN_POINT ( 'NONE',  ( 18.16427545049632286, -0.3901114995139697283, 12.59396323349878166 ) ) ;
#11553 = CARTESIAN_POINT ( 'NONE',  ( 10.50084834123000022, 4.616783736607999344, -6.288082254674000282 ) ) ;
#11554 = CARTESIAN_POINT ( 'NONE',  ( 0.000000000000000000, 2.899999999999999911, -7.500000000000000000 ) ) ;
#11556 = CARTESIAN_POINT ( 'NONE',  ( 5.000000000000000000, 0.2999999999999999889, 3.149999999999999911 ) ) ;
#11555 = FACE_OUTER_BOUND ( 'NONE', #10544, .T. ) ;
#11557 = CARTESIAN_POINT ( 'NONE',  ( 17.79999999998900151, 3.595165934733000057, 11.99793354950999991 ) ) ;
#11558 = ORIENTED_EDGE ( 'NONE', *, *, #38918, .T. ) ;
#11559 = DIRECTION ( 'NONE',  ( -1.000000000000000000, 0.000000000000000000, 0.000000000000000000 ) ) ;
#11560 = CARTESIAN_POINT ( 'NONE',  ( 23.91426698951526220, -9.509256905776609869, -9.346090767248723452 ) ) ;
#11561 = PLANE ( 'NONE',  #67541 ) ;
#11562 = CARTESIAN_POINT ( 'NONE',  ( 8.918455549952998496, 4.674761969675400586, 8.044430187461498960 ) ) ;
#11563 = B_SPLINE_CURVE_WITH_KNOTS ( 'NONE', 3,
 ( #3207, #40274, #7765, #61591, #13708, #35037, #56005, #30138, #67169, #55667 ),
 .UNSPECIFIED., .F., .F.,
 ( 4, 2, 2, 2, 4 ),
 ( 0.000000000000000000, 0.2500000000000000000, 0.5000000000000000000, 0.7500000000000000000, 1.000000000000000000 ),
 .UNSPECIFIED. ) ;
#11564 = CARTESIAN_POINT ( 'NONE',  ( 12.30643338748587468, -1.987817336848023198, 13.85816184334709433 ) ) ;
#11565 = DIRECTION ( 'NONE',  ( 1.000000000000000000, 0.000000000000000000, 0.000000000000000000 ) ) ;
#11566 = CARTESIAN_POINT ( 'NONE',  ( 24.23232808299099972, 3.402461458659999494, -12.43151225365000023 ) ) ;
#11567 = B_SPLINE_CURVE_WITH_KNOTS ( 'NONE', 3,
 ( #22492, #12362, #1522, #23537, #66182, #18302, #39626, #60947, #33693, #22842, #13408, #29146, #65834, #7805, #28805, #13061, #44542, #50116 ),
 .UNSPECIFIED., .F., .F.,
 ( 4, 2, 2, 2, 2, 2, 2, 2, 4 ),
 ( 0.000000000000000000, 0.1250000000000003331, 0.2500000000000006661, 0.3750000000000009992, 0.5000000000000013323, 0.6250000000000009992, 0.7500000000000006661, 0.8750000000000003331, 1.000000000000000000 ),
 .UNSPECIFIED. ) ;
#11568 = ORIENTED_EDGE ( 'NONE', *, *, #48217, .T. ) ;
#11569 = DIRECTION ( 'NONE',  ( 0.000000000000000000, 1.000000000000000000, 0.000000000000000000 ) ) ;
#11570 = DIRECTION ( 'NONE',  ( 1.000000000000000000, 0.000000000000000000, 0.000000000000000000 ) ) ;
#11571 = AXIS2_PLACEMENT_3D ( 'NONE', #52650, #14571, #20493 ) ;
#11572 = DIRECTION ( 'NONE',  ( 1.000000000000000000, 0.000000000000000000, 0.000000000000000000 ) ) ;
#11573 = CARTESIAN_POINT ( 'NONE',  ( 0.8468373879278999761, -2.423129934138000152, -2.873468012158999940 ) ) ;
#11574 = CARTESIAN_POINT ( 'NONE',  ( 11.79999999684100054, -3.345264396959000130, 11.86064773189999855 ) ) ;
#11575 = CARTESIAN_POINT ( 'NONE',  ( 17.60707724214342917, 1.877081947552195151, -12.57511531410870731 ) ) ;
#11576 = CARTESIAN_POINT ( 'NONE',  ( 10.51655086620999846, 4.930662802525000110, 8.573584269714999095 ) ) ;
#11577 = CARTESIAN_POINT ( 'NONE',  ( 11.36749010443639918, 4.863785690678500195, 7.435402237490909449 ) ) ;
#11578 = CARTESIAN_POINT ( 'NONE',  ( 8.616995677562000466, -4.876077402042000131, 5.996974966533000106 ) ) ;
#11579 = CARTESIAN_POINT ( 'NONE',  ( 10.92546935320999957, -5.641520548727999795, -7.883473948564999390 ) ) ;
#11580 = CARTESIAN_POINT ( 'NONE',  ( 7.933148997457998952, 5.167567567567999731, 6.822293592207000934 ) ) ;
#11581 = FACE_OUTER_BOUND ( 'NONE', #26981, .T. ) ;
#11582 = CARTESIAN_POINT ( 'NONE',  ( 24.51327040776200050, 12.11106229541000090, 3.153269560843000363 ) ) ;
#11583 = EDGE_CURVE ( 'NONE', #30840, #42489, #14398, .T. ) ;
#11584 = CARTESIAN_POINT ( 'NONE',  ( 8.810863317747999801, -3.039136629551499880, -7.500000000073117512 ) ) ;
#11585 = EDGE_CURVE ( 'NONE', #6078, #60646, #46753, .T. ) ;
#11586 = ORIENTED_EDGE ( 'NONE', *, *, #48527, .T. ) ;
#11587 = CARTESIAN_POINT ( 'NONE',  ( 7.424379198296266580, 2.348612827597222896, 8.058989540383295846 ) ) ;
#11588 = CARTESIAN_POINT ( 'NONE',  ( 11.12487750876920067, -4.543557328885200697, 6.656497609330299881 ) ) ;
#11589 = VERTEX_POINT ( 'NONE', #63121 ) ;
#11590 = CARTESIAN_POINT ( 'NONE',  ( 17.86097767714754525, -3.045104419577887800, 13.54261379197756732 ) ) ;
#11592 = CARTESIAN_POINT ( 'NONE',  ( 11.13764426047339917, -3.386171819220400003, -8.461511872390000022 ) ) ;
#11591 = B_SPLINE_CURVE_WITH_KNOTS ( 'NONE', 3,
 ( #17002, #27860, #46861, #20284 ),
 .UNSPECIFIED., .F., .F.,
 ( 4, 4 ),
 ( 0.000000000000000000, 1.000000000000000000 ),
 .UNSPECIFIED. ) ;
#11593 = ORIENTED_EDGE ( 'NONE', *, *, #10640, .T. ) ;
#11594 = CARTESIAN_POINT ( 'NONE',  ( 11.31389666366019853, 3.954123449088899900, 6.467512203247999913 ) ) ;
#11595 = CARTESIAN_POINT ( 'NONE',  ( 5.631379662966172539, 0.9049817462873084306, 0.6808242691568766602 ) ) ;
#11597 = CARTESIAN_POINT ( 'NONE',  ( 8.383148997457999130, 5.167567567567999731, 6.822293592207000934 ) ) ;
#11596 = AXIS2_PLACEMENT_3D ( 'NONE', #52991, #17216, #22110 ) ;
#11598 = CARTESIAN_POINT ( 'NONE',  ( 12.80505043854144098, -0.7302158263239267866, -13.98094363220830871 ) ) ;
#11599 = CARTESIAN_POINT ( 'NONE',  ( 7.100000000000000533, -4.000000000000000000, 7.500000000000000000 ) ) ;
#11600 = CARTESIAN_POINT ( 'NONE',  ( 9.696013540182335078, -3.000416447002272058, -6.731816600031361730 ) ) ;
#11601 = CARTESIAN_POINT ( 'NONE',  ( 11.59999999999999964, -4.447112190091930373, -6.627718330236055166 ) ) ;
#11602 = CARTESIAN_POINT ( 'NONE',  ( 10.22440803363000050, -5.317414323721999736, -8.272454209812998727 ) ) ;
#11603 = AXIS2_PLACEMENT_3D ( 'NONE', #49073, #49415, #43494 ) ;
#11604 = CARTESIAN_POINT ( 'NONE',  ( 4.000000000000000888, -1.878608423871360289, -1.082950885222729198 ) ) ;
#11605 = VERTEX_POINT ( 'NONE', #47760 ) ;
#11606 = CARTESIAN_POINT ( 'NONE',  ( 8.821685841230998193, 2.633142096252999664, -7.791134854666999843 ) ) ;
#11607 = ORIENTED_EDGE ( 'NONE', *, *, #32196, .T. ) ;
#11608 = CARTESIAN_POINT ( 'NONE',  ( 24.66708179642670373, -12.30983497500974622, 2.983163088799908103 ) ) ;
#11609 =( NAMED_UNIT ( * ) PLANE_ANGLE_UNIT ( ) SI_UNIT ( $, .RADIAN. ) );
#11610 = ORIENTED_EDGE ( 'NONE', *, *, #57045, .F. ) ;
#11611 = CARTESIAN_POINT ( 'NONE',  ( 11.09999999999999964, 5.350000000000000533, -7.500000000000000000 ) ) ;
#11612 = CARTESIAN_POINT ( 'NONE',  ( 18.14016391943236073, -2.719929439268203630, -12.39760446975600416 ) ) ;
#11613 = ADVANCED_FACE ( 'NONE', ( #21176 ), #25541, .F. ) ;
#11614 = CARTESIAN_POINT ( 'NONE',  ( 10.62452888361057113, 3.128042445605609512, 7.438521339935803667 ) ) ;
#11615 = CARTESIAN_POINT ( 'NONE',  ( 10.27934687351620724, 3.836375382625536012, -6.249999999999999112 ) ) ;
#11616 = CARTESIAN_POINT ( 'NONE',  ( 9.529346873515667227, -3.836375382625533348, -8.749999999999998224 ) ) ;
#11617 = B_SPLINE_SURFACE_WITH_KNOTS ( 'NONE', 3, 3, ( 
 ( #6423, #69029, #21142, #42468 ),
 ( #34056, #17628, #23550, #38954 ),
 ( #49779, #8166, #2235, #60615 ),
 ( #65501, #44890, #50467, #22855 ),
 ( #66194, #60960, #60271, #50131 ),
 ( #2569, #55026, #29515, #18316 ),
 ( #1890, #43848, #50818, #13075 ),
 ( #33708, #2913, #59917, #7127 ) ),
 .UNSPECIFIED., .F., .F., .F.,
 ( 4, 1, 1, 1, 1, 4 ),
 ( 4, 4 ),
 ( 0.008358950191421000986, 0.05882352941176000050, 0.1176470588234999892, 0.1764705882353000133, 0.2352941176471000095, 0.2534938933614000467 ),
 ( -0.1830994283965000080, 1.182949771275999984 ),
 .UNSPECIFIED. ) ;
#11618 = CARTESIAN_POINT ( 'NONE',  ( 9.736871746126999128, -2.742172332680000046, 6.839224809731999422 ) ) ;
#11619 = LINE ( 'NONE', #50079, #50428 ) ;
#11620 = CARTESIAN_POINT ( 'NONE',  ( 12.26342747050452076, 0.3125520594525317275, 13.89528657259775102 ) ) ;
#11621 = ORIENTED_EDGE ( 'NONE', *, *, #54695, .F. ) ;
#11622 = CARTESIAN_POINT ( 'NONE',  ( 12.83903456837200174, 11.55258133652000119, -4.939873833509000889 ) ) ;
#11623 = CARTESIAN_POINT ( 'NONE',  ( 17.57230163855200189, 11.81435006507999930, -3.324773181547000078 ) ) ;
#11624 = CARTESIAN_POINT ( 'NONE',  ( 10.21473687196862734, 3.686226525417862998, 6.683251291081091949 ) ) ;
#11625 = CARTESIAN_POINT ( 'NONE',  ( 4.633192238856000067, -0.01992358281169000211, 1.334452703055000189 ) ) ;
#11626 = VECTOR ( 'NONE', #52660, 1000.000000000000000 ) ;
#11627 = CARTESIAN_POINT ( 'NONE',  ( 9.476970280414001024, 5.511689883260999956, -7.095113581311000672 ) ) ;
#11628 = DIRECTION ( 'NONE',  ( 1.000000000000000000, 0.000000000000000000, 0.000000000000000000 ) ) ;
#11629 = CARTESIAN_POINT ( 'NONE',  ( 10.87695483801000051, -5.827068285690999438, -7.814745128155998977 ) ) ;
#11630 = VERTEX_POINT ( 'NONE', #63815 ) ;
#11631 = CARTESIAN_POINT ( 'NONE',  ( 8.085754734272050825, 5.349973530442185599, -7.853162922483586605 ) ) ;
#11632 = CARTESIAN_POINT ( 'NONE',  ( 7.000000000000000000, -11.29999999999999893, 0.000000000000000000 ) ) ;
#11633 = LINE ( 'NONE', #59537, #9838 ) ;
#11634 = CARTESIAN_POINT ( 'NONE',  ( 6.899999691988000450, 12.99045401563999924, 1.690592933733000125 ) ) ;
#11635 = CARTESIAN_POINT ( 'NONE',  ( 8.560199822370993417, -3.014874134772824732, 6.139748469567640754 ) ) ;
#11636 = CARTESIAN_POINT ( 'NONE',  ( 23.60000000000000142, -9.517611874540000017, 8.103398312166998352 ) ) ;
#11637 = CARTESIAN_POINT ( 'NONE',  ( 11.39700581613019992, 4.869652672166700391, -8.058426314824099990 ) ) ;
#11638 = CARTESIAN_POINT ( 'NONE',  ( 10.03992546752099990, 2.997990738918999920, -7.430575645513339822 ) ) ;
#11640 = CYLINDRICAL_SURFACE ( 'NONE', #4946, 1.250000000000000222 ) ;
#11639 = CARTESIAN_POINT ( 'NONE',  ( 9.395138961224001051, -3.167792625045000143, 6.937618199889199033 ) ) ;
#11641 = CONICAL_SURFACE ( 'NONE', #21673, 13.94999929345000211, 0.7853981072369679017 ) ;
#11642 = CARTESIAN_POINT ( 'NONE',  ( 7.799092354096995194, -3.518505934209000152, 6.398021147088998717 ) ) ;
#11643 = ORIENTED_EDGE ( 'NONE', *, *, #47353, .F. ) ;
#11644 = B_SPLINE_CURVE_WITH_KNOTS ( 'NONE', 3,
 ( #61929, #62940, #14726, #40603 ),
 .UNSPECIFIED., .F., .F.,
 ( 4, 4 ),
 ( 0.000000000000000000, 1.000000000000000000 ),
 .UNSPECIFIED. ) ;
#11645 = CARTESIAN_POINT ( 'NONE',  ( 10.93479632507519916, 4.557787252275099732, 6.465962698293999722 ) ) ;
#11646 = AXIS2_PLACEMENT_3D ( 'NONE', #2402, #13254, #44383 ) ;
#11647 = CARTESIAN_POINT ( 'NONE',  ( 24.67921321800200118, -8.727630028894999725, 9.158313644156001132 ) ) ;
#11648 = ADVANCED_FACE ( 'NONE', ( #57895 ), #42508, .T. ) ;
#11650 = ADVANCED_FACE ( 'NONE', ( #52645 ), #20146, .T. ) ;
#11649 = B_SPLINE_CURVE_WITH_KNOTS ( 'NONE', 3,
 ( #583, #21550, #6852, #42886 ),
 .UNSPECIFIED., .F., .F.,
 ( 4, 4 ),
 ( 0.000000000000000000, 1.000000000000000000 ),
 .UNSPECIFIED. ) ;
#11651 = CARTESIAN_POINT ( 'NONE',  ( 9.682355082327998019, 3.488994418336600400, 8.521081653687000212 ) ) ;
#11652 = DIRECTION ( 'NONE',  ( 0.000000000000000000, 0.000000000000000000, -1.000000000000000000 ) ) ;
#11653 = CARTESIAN_POINT ( 'NONE',  ( 10.59344961228999971, -5.297755890367000120, 8.474197994416998725 ) ) ;
#11654 = CARTESIAN_POINT ( 'NONE',  ( 30.60000000000000142, -2.052081084281999983E-07, 7.720759220056000238 ) ) ;
#11655 = CARTESIAN_POINT ( 'NONE',  ( 10.57101354018312023, 4.768183399968643599, 6.500416447002274722 ) ) ;
#11656 = CARTESIAN_POINT ( 'NONE',  ( 9.432025935145999185, -4.145841638824199649, -6.506233167833100239 ) ) ;
#11657 = CARTESIAN_POINT ( 'NONE',  ( 5.274803308717000760, -1.289352866216999960, -0.2932997125499000046 ) ) ;
#11658 = CARTESIAN_POINT ( 'NONE',  ( 6.553816671982000130, -1.199981415667000118, 0.9000247785775999931 ) ) ;
#11659 = CARTESIAN_POINT ( 'NONE',  ( 24.66122485234200212, -3.625879222137000202, 12.20767898207999913 ) ) ;
#11660 = CARTESIAN_POINT ( 'NONE',  ( 11.67056785386840012, -4.718624889240500053, 7.016391833292499491 ) ) ;
#11661 = CARTESIAN_POINT ( 'NONE',  ( 11.04749144726329924, 3.499163784537000055, -6.793273974143599681 ) ) ;
#11662 = DIRECTION ( 'NONE',  ( -1.000000000000000000, 0.000000000000000000, 0.000000000000000000 ) ) ;
#11663 = CARTESIAN_POINT ( 'NONE',  ( 25.57778492944800064, -8.344458803148999237, 8.014471200166999765 ) ) ;
#11664 = CARTESIAN_POINT ( 'NONE',  ( 0.9780567992084204798, 2.150913519912206695, -2.798833948393626869 ) ) ;
#11665 = ORIENTED_EDGE ( 'NONE', *, *, #68167, .T. ) ;
#11666 = CARTESIAN_POINT ( 'NONE',  ( 25.41680095681100227, -11.20712209151000138, -3.225979711303999853 ) ) ;
#11667 = APPLICATION_PROTOCOL_DEFINITION ( 'draft international standard', 'automotive_design', 1998, #26660 ) ;
#11668 = CARTESIAN_POINT ( 'NONE',  ( 10.40480513895999870, -3.220259576336399920, -7.066537524675499782 ) ) ;
#11669 = EDGE_CURVE ( 'NONE', #11391, #34244, #41166, .T. ) ;
#11670 = CYLINDRICAL_SURFACE ( 'NONE', #6898, 10.80000000000000071 ) ;
#11671 = CARTESIAN_POINT ( 'NONE',  ( 25.59994555223600088, -0.6783951095372073858, -11.19994871957819704 ) ) ;
#11672 = CARTESIAN_POINT ( 'NONE',  ( 7.000000000000000000, 10.75808151192356732, 3.620680867180093188 ) ) ;
#11673 = CARTESIAN_POINT ( 'NONE',  ( 13.18628609634500215, 12.21854424350999935, 1.979874043355999813 ) ) ;
#11674 = ORIENTED_EDGE ( 'NONE', *, *, #52036, .F. ) ;
#11675 = AXIS2_PLACEMENT_3D ( 'NONE', #15722, #52430, #63605 ) ;
#11676 = ADVANCED_FACE ( 'NONE', ( #25737 ), #15592, .T. ) ;
#11677 = CARTESIAN_POINT ( 'NONE',  ( 23.89320776801300283, 8.283889223751996767, 7.778387372934005839 ) ) ;
#11678 = CARTESIAN_POINT ( 'NONE',  ( 8.748004441081999261, -4.389076025353599420, -8.341443180570399463 ) ) ;
#11679 = ORIENTED_EDGE ( 'NONE', *, *, #57600, .F. ) ;
#11680 = CARTESIAN_POINT ( 'NONE',  ( 6.976568042970999528, -9.209912048597001188, 5.193747272324000797 ) ) ;
#11681 = CARTESIAN_POINT ( 'NONE',  ( 9.349999778958000718, -4.000000000000000000, 6.500000166194499940 ) ) ;
#11682 = CARTESIAN_POINT ( 'NONE',  ( 9.418864158773999407, 3.210851187372000037, -6.346613542714999667 ) ) ;
#11683 = EDGE_LOOP ( 'NONE', ( #45278, #5604, #47870, #12916 ) ) ;
#11684 = CARTESIAN_POINT ( 'NONE',  ( 23.76529063391505758, -13.07188707895195456, 3.759452220472195627 ) ) ;
#11685 = CARTESIAN_POINT ( 'NONE',  ( 11.13746005378019888, -2.838900981960999825, -6.879992063401499713 ) ) ;
#11686 = CARTESIAN_POINT ( 'NONE',  ( 8.011460841224998575, 3.456780951359999854, -9.320567109458000488 ) ) ;
#11687 = CARTESIAN_POINT ( 'NONE',  ( 11.50029455687000102, -11.56505190006999939, -1.404305717648999918 ) ) ;
#11688 = CARTESIAN_POINT ( 'NONE',  ( 8.155132402557608629, -3.046310786074582833, 6.333683957159311539 ) ) ;
#11689 = VERTEX_POINT ( 'NONE', #10340 ) ;
#11690 = CARTESIAN_POINT ( 'NONE',  ( 9.034116535116000435, -4.695350938297000454, 8.660677768253002284 ) ) ;
#11691 = DIRECTION ( 'NONE',  ( -1.000000000000000000, 0.000000000000000000, 0.000000000000000000 ) ) ;
#11692 = CARTESIAN_POINT ( 'NONE',  ( 6.305026506349999948, 1.500000000000000000, 0.000000000000000000 ) ) ;
#11693 = ORIENTED_EDGE ( 'NONE', *, *, #39881, .F. ) ;
#11694 = CARTESIAN_POINT ( 'NONE',  ( 6.075859839683334762, -1.460959015002473826, -0.3926218265389207485 ) ) ;
#11695 = CARTESIAN_POINT ( 'NONE',  ( 10.69015444038000062, -4.391267940138999570, -8.802346922965000431 ) ) ;
#11696 = VERTEX_POINT ( 'NONE', #31676 ) ;
#11697 = CARTESIAN_POINT ( 'NONE',  ( 9.482684229509999341, 3.291972602441000095, 8.212418068717900255 ) ) ;
#11698 = CARTESIAN_POINT ( 'NONE',  ( 17.72120476622717433, -1.779652109340960520, -12.47368672373263898 ) ) ;
#11699 = CARTESIAN_POINT ( 'NONE',  ( 4.898026823400999596, 0.7146345574896999508, 1.383890202823000237 ) ) ;
#11700 = EDGE_CURVE ( 'NONE', #50078, #11941, #43192, .T. ) ;
#11701 = CARTESIAN_POINT ( 'NONE',  ( 11.60000000000000142, 3.552887809908069627, -6.627718330236056055 ) ) ;
#11702 = CARTESIAN_POINT ( 'NONE',  ( 24.70905576447193752, 11.78230593457693942, -3.190800434545450592 ) ) ;
#11703 = CARTESIAN_POINT ( 'NONE',  ( 11.35565467195930189, 2.863826994586553987, 8.088082908809450799 ) ) ;
#11704 = CARTESIAN_POINT ( 'NONE',  ( 9.383380199233998908, 4.860242402105300563, 7.608124715612800237 ) ) ;
#11705 = CARTESIAN_POINT ( 'NONE',  ( 12.80505043854144098, 0.7302158263239095781, 13.98094363220830871 ) ) ;
#11706 = ORIENTED_EDGE ( 'NONE', *, *, #55803, .F. ) ;
#11707 = DIRECTION ( 'NONE',  ( 0.000000000000000000, 1.000000000000000000, 0.000000000000000000 ) ) ;
#11708 = CARTESIAN_POINT ( 'NONE',  ( 11.15264221959000146, 2.317063201199000222, -7.596564358366999947 ) ) ;
#11709 = DIRECTION ( 'NONE',  ( 0.000000000000000000, 0.7614089499631908620, -0.6482718649732929217 ) ) ;
#11710 = CARTESIAN_POINT ( 'NONE',  ( 12.29628962427834793, 2.863168005537269689, -13.58969864530831728 ) ) ;
#11711 = CARTESIAN_POINT ( 'NONE',  ( 10.34292546752099895, -5.276153033933000280, -7.411581555133209598 ) ) ;
#11712 = CARTESIAN_POINT ( 'NONE',  ( 25.08881765777200457, 3.215721225475999923, 11.60740081808000035 ) ) ;
#11713 = CARTESIAN_POINT ( 'NONE',  ( 18.17001922193489705, 0.1119984579798026098, 13.89939774083726576 ) ) ;
#11714 = CARTESIAN_POINT ( 'NONE',  ( 25.36466043037300011, -2.635483744749000046, 11.32507393831999920 ) ) ;
#11715 = ORIENTED_EDGE ( 'NONE', *, *, #35158, .F. ) ;
#11716 = VERTEX_POINT ( 'NONE', #43887 ) ;
#11717 = CARTESIAN_POINT ( 'NONE',  ( 9.242342830452999536, 5.206708472530999998, 8.808826521083998884 ) ) ;
#11718 = CARTESIAN_POINT ( 'NONE',  ( 12.23148617193598220, 0.2485195352681210113, 13.89701485918539170 ) ) ;
#11719 = CARTESIAN_POINT ( 'NONE',  ( 12.41700012673178044, -0.4899485148888237940, -13.88837626668755831 ) ) ;
#11720 = DIRECTION ( 'NONE',  ( -0.000000000000000000, -0.000000000000000000, 1.000000000000000000 ) ) ;
#11721 = CARTESIAN_POINT ( 'NONE',  ( 16.03314433152364771, 8.943717616153273653, 8.673217039016851260 ) ) ;
#11722 = CARTESIAN_POINT ( 'NONE',  ( 7.550620559621999739, -4.468370631666999770, 8.882152684713000568 ) ) ;
#11723 = CARTESIAN_POINT ( 'NONE',  ( 11.51053724730969918, -4.948425591258600598, 7.825000000000000178 ) ) ;
#11725 = FACE_OUTER_BOUND ( 'NONE', #63244, .T. ) ;
#11724 = CARTESIAN_POINT ( 'NONE',  ( 10.46298825978700009, -4.167373623506299474, 6.231784538167999266 ) ) ;
#11726 = CARTESIAN_POINT ( 'NONE',  ( 10.24733997687999931, 4.272363749081500295, -6.251346978035999591 ) ) ;
#11727 = B_SPLINE_CURVE_WITH_KNOTS ( 'NONE', 3,
 ( #57301, #20943, #9404, #10440 ),
 .UNSPECIFIED., .F., .F.,
 ( 4, 4 ),
 ( 0.000000000000000000, 1.000000000000000000 ),
 .UNSPECIFIED. ) ;
#11728 = CYLINDRICAL_SURFACE ( 'NONE', #22421, 1.350000000000000089 ) ;
#11729 = CARTESIAN_POINT ( 'NONE',  ( 10.34393020684899867, 2.750000000000000000, -7.500000000000000000 ) ) ;
#11730 = EDGE_CURVE ( 'NONE', #24513, #62590, #57535, .T. ) ;
#11731 = EDGE_CURVE ( 'NONE', #56474, #5840, #64496, .T. ) ;
#11732 = CARTESIAN_POINT ( 'NONE',  ( 18.01141060613106148, -0.4275228316712903487, 12.69032453495386292 ) ) ;
#11733 = CARTESIAN_POINT ( 'NONE',  ( 11.10000000000000142, -5.582818908801700175, 7.477537682244628670 ) ) ;
#11734 = CARTESIAN_POINT ( 'NONE',  ( 4.149992563291999836, 1.007210908820209028, 1.747525841223986243 ) ) ;
#11735 = EDGE_LOOP ( 'NONE', ( #7144, #4725, #36956, #66556 ) ) ;
#11736 = CARTESIAN_POINT ( 'NONE',  ( 8.481683059623998489, -2.472358291268000219, 6.234202627038999189 ) ) ;
#11737 = CARTESIAN_POINT ( 'NONE',  ( 9.550320280412000429, 2.370176859044999862, -6.912649125838000508 ) ) ;
#11738 = EDGE_CURVE ( 'NONE', #63300, #21757, #55250, .T. ) ;
#11739 = LINE ( 'NONE', #33082, #39398 ) ;
#11740 = CARTESIAN_POINT ( 'NONE',  ( 23.60205915885299888, 9.223492163361996177, -8.025915643364996299 ) ) ;
#11741 = B_SPLINE_CURVE_WITH_KNOTS ( 'NONE', 3,
 ( #6639, #37766, #17125, #22716 ),
 .UNSPECIFIED., .F., .F.,
 ( 4, 4 ),
 ( 0.000000000000000000, 1.000000000000000000 ),
 .UNSPECIFIED. ) ;
#11742 = CARTESIAN_POINT ( 'NONE',  ( 0.7079009740474999646, -3.376221432737999795, -1.056438743269999980 ) ) ;
#11743 = AXIS2_PLACEMENT_3D ( 'NONE', #9555, #25643, #30896 ) ;
#11744 = CARTESIAN_POINT ( 'NONE',  ( 11.36056039236529891, 4.891071240644300211, 7.456633480985620288 ) ) ;
#11745 = CARTESIAN_POINT ( 'NONE',  ( 10.17270667456000055, 4.650145611776999921, -8.655516756809999990 ) ) ;
#11746 = VERTEX_POINT ( 'NONE', #48783 ) ;
#11747 = CARTESIAN_POINT ( 'NONE',  ( 12.20907020345897642, -0.4097539338085484095, -12.59333942654355809 ) ) ;
#11748 = CARTESIAN_POINT ( 'NONE',  ( 24.34833211465999980, 8.895958282168665576, -8.895958282168665576 ) ) ;
#11749 = CARTESIAN_POINT ( 'NONE',  ( 18.26836321268585195, 2.610382005543650408, -12.32663954618810820 ) ) ;
#11750 = CARTESIAN_POINT ( 'NONE',  ( 5.500000000000000000, 12.22293095105000127, 3.800428736101999938 ) ) ;
#11751 = CARTESIAN_POINT ( 'NONE',  ( 8.309482780410998970, 2.905861847853000057, 8.940690431604000565 ) ) ;
#11752 = ORIENTED_EDGE ( 'NONE', *, *, #21874, .T. ) ;
#11753 = CARTESIAN_POINT ( 'NONE',  ( 6.990359675868999645, -1.019889730527999916, 1.251756626546000062 ) ) ;
#11754 = B_SPLINE_CURVE_WITH_KNOTS ( 'NONE', 3,
 ( #16319, #5491, #11415, #57946, #42554, #10386, #32757, #47811, #52693, #68763, #42898, #37648, #6166, #27508, #48834, #36970, #942, #22255 ),
 .UNSPECIFIED., .F., .F.,
 ( 4, 2, 2, 2, 2, 2, 2, 2, 4 ),
 ( 0.000000000000000000, 0.1250000000000000000, 0.2500000000000000000, 0.3750000000000000000, 0.5000000000000000000, 0.6250000000000000000, 0.7500000000000000000, 0.8750000000000000000, 1.000000000000000000 ),
 .UNSPECIFIED. ) ;
#11755 = CARTESIAN_POINT ( 'NONE',  ( 8.005554719585999734, 4.569394889178999719, -9.136182695123999054 ) ) ;
#11757 = CARTESIAN_POINT ( 'NONE',  ( 8.642077642326000841, -2.899999999999999911, 6.463854830420999953 ) ) ;
#11756 = CARTESIAN_POINT ( 'NONE',  ( 8.439910304958656795, -2.270935633533203823, 7.713963258081458996 ) ) ;
#11758 = CARTESIAN_POINT ( 'NONE',  ( 9.725367640781000134, -3.396982508013000501, 8.628164124510998789 ) ) ;
#11759 = VERTEX_POINT ( 'NONE', #27457 ) ;
#11760 = CARTESIAN_POINT ( 'NONE',  ( -15.86200481174999943, 0.8000000000000000444, 3.149999999999999911 ) ) ;
#11761 = CARTESIAN_POINT ( 'NONE',  ( 10.02314899745999988, 5.167567567567999731, -6.822293592207000934 ) ) ;
#11762 = VERTEX_POINT ( 'NONE', #42848 ) ;
#11763 = CARTESIAN_POINT ( 'NONE',  ( 11.09999999999999964, 2.274006712557999688, -7.281956340829000673 ) ) ;
#11764 = CARTESIAN_POINT ( 'NONE',  ( 25.29987654162099986, -8.533547851352999203, -7.925583806936000286 ) ) ;
#11765 = CARTESIAN_POINT ( 'NONE',  ( 17.72054635526678368, 0.7113363331415119006, -13.98191770012930135 ) ) ;
#11766 = B_SPLINE_CURVE_WITH_KNOTS ( 'NONE', 3,
 ( #2482, #7035, #28721, #33961 ),
 .UNSPECIFIED., .F., .F.,
 ( 4, 4 ),
 ( 0.000000000000000000, 1.000000000000000000 ),
 .UNSPECIFIED. ) ;
#11767 = ORIENTED_EDGE ( 'NONE', *, *, #20396, .T. ) ;
#11768 = FACE_OUTER_BOUND ( 'NONE', #36207, .T. ) ;
#11769 = CARTESIAN_POINT ( 'NONE',  ( 17.60000002773078975, -12.03387896817346281, 3.206083673428302028 ) ) ;
#11770 = CARTESIAN_POINT ( 'NONE',  ( 11.60988784977536348, 3.148894096305599799, -7.451365240271489832 ) ) ;
#11771 = CARTESIAN_POINT ( 'NONE',  ( 24.44496356299600137, 12.03536643057000077, 3.224849944858999784 ) ) ;
#11773 = AXIS2_PLACEMENT_3D ( 'NONE', #26344, #3627, #25651 ) ;
#11772 = CARTESIAN_POINT ( 'NONE',  ( 10.74733997688000109, -3.727636250918499705, 8.748653021963999521 ) ) ;
#11774 = VERTEX_POINT ( 'NONE', #27815 ) ;
#11775 = DIRECTION ( 'NONE',  ( 0.000000000000000000, 0.000000000000000000, 1.000000000000000000 ) ) ;
#11776 = CARTESIAN_POINT ( 'NONE',  ( 18.02697970389229454, -1.963589444787183558, 13.86161523094991210 ) ) ;
#11777 = CARTESIAN_POINT ( 'NONE',  ( 10.02101354018333446, -3.231816600031356845, 6.500416447002272946 ) ) ;
#11778 = AXIS2_PLACEMENT_3D ( 'NONE', #18767, #13184, #2336 ) ;
#11779 = CARTESIAN_POINT ( 'NONE',  ( 15.36385332268500115, -9.394483288005998745, -8.200629419667000874 ) ) ;
#11780 = CARTESIAN_POINT ( 'NONE',  ( 11.12484646121000154, 5.434138738817000380, -5.164717599857000074 ) ) ;
#11781 = ORIENTED_EDGE ( 'NONE', *, *, #11820, .F. ) ;
#11782 = B_SPLINE_SURFACE_WITH_KNOTS ( 'NONE', 3, 3, ( 
 ( #61972, #35408, #56734, #46584 ),
 ( #30171, #35745, #67891, #25246 ),
 ( #49639, #12934, #50335, #24452 ),
 ( #2779, #7685, #39154, #23065 ),
 ( #24105, #12585, #6988, #13627 ),
 ( #1745, #34260, #55583, #28674 ),
 ( #34952, #44414, #56266, #29027 ),
 ( #45777, #18524, #2433, #61169 ),
 ( #13290, #50683, #55232, #23761 ),
 ( #33567, #3121, #33915, #67088 ),
 ( #66750, #60822, #51021, #8376 ),
 ( #8030, #65714, #29719, #60478 ) ),
 .UNSPECIFIED., .F., .F., .F.,
 ( 4, 1, 1, 1, 1, 1, 1, 1, 1, 4 ),
 ( 4, 4 ),
 ( 0.5515740600308000063, 0.5999999999999999778, 0.6500000000000000222, 0.6999999999999999556, 0.7500000000000000000, 0.8000000000000000444, 0.8499999999999999778, 0.9000000000000000222, 0.9499999999999999556, 0.9893625964778000048 ),
 ( -0.2706692301633999986, 1.270787907492000102 ),
 .UNSPECIFIED. ) ;
#11783 = CARTESIAN_POINT ( 'NONE',  ( 12.27169925567833175, -2.173540117687664974, -12.52166307684904112 ) ) ;
#11784 = EDGE_CURVE ( 'NONE', #16879, #36918, #50863, .T. ) ;
#11785 = CARTESIAN_POINT ( 'NONE',  ( 10.84393020684979980, 2.750000000000000000, -7.500000000000000000 ) ) ;
#11786 = CARTESIAN_POINT ( 'NONE',  ( 8.286697165045001867, 5.451921732286531430, -6.342020349060414119 ) ) ;
#11787 = DIRECTION ( 'NONE',  ( 1.000000000000000000, 0.000000000000000000, 0.000000000000000000 ) ) ;
#11788 = CARTESIAN_POINT ( 'NONE',  ( 12.14431428438026472, -2.818682143830034015, -13.71332026632872036 ) ) ;
#11789 = EDGE_CURVE ( 'NONE', #30003, #25573, #19572, .T. ) ;
#11790 = CARTESIAN_POINT ( 'NONE',  ( 10.25564828895399927, -3.119330945648699949, -7.981013126389099099 ) ) ;
#11791 = CARTESIAN_POINT ( 'NONE',  ( 12.61539589083637658, -1.784264304828792058, 12.47303049908514438 ) ) ;
#11792 = CARTESIAN_POINT ( 'NONE',  ( 17.68706105916313120, -1.772767334361405211, 12.47466639265151755 ) ) ;
#11793 = ORIENTED_EDGE ( 'NONE', *, *, #44537, .T. ) ;
#11794 = CARTESIAN_POINT ( 'NONE',  ( 10.63880513895979973, -2.849548954067000039, -6.860457220153399760 ) ) ;
#11795 = EDGE_LOOP ( 'NONE', ( #24072, #55179 ) ) ;
#11796 = CARTESIAN_POINT ( 'NONE',  ( 11.68591862085600219, -12.43715917574999885, -1.778745665763999950 ) ) ;
#11797 = VECTOR ( 'NONE', #54743, 1000.000000000000000 ) ;
#11798 = CARTESIAN_POINT ( 'NONE',  ( 9.386379719595000282, 5.673443217382001080, -7.051790060464000476 ) ) ;
#11799 = CARTESIAN_POINT ( 'NONE',  ( 10.60199294549000193, 2.164976235211999889, -7.764525279724000306 ) ) ;
#11800 = CARTESIAN_POINT ( 'NONE',  ( 10.86493091395000121, -4.678465004315999209, -9.048463592221999363 ) ) ;
#11801 = VECTOR ( 'NONE', #19582, 1000.000000000000114 ) ;
#11802 = CARTESIAN_POINT ( 'NONE',  ( 10.90000000000000036, -1.199999999999999956, -9.776630298829998011 ) ) ;
#11803 = FACE_OUTER_BOUND ( 'NONE', #66462, .T. ) ;
#11804 = CARTESIAN_POINT ( 'NONE',  ( 11.08810207955139937, 3.203462856645999945, -7.174999999999999822 ) ) ;
#11805 = ORIENTED_EDGE ( 'NONE', *, *, #40874, .F. ) ;
#11806 = PLANE ( 'NONE',  #46984 ) ;
#11807 = CARTESIAN_POINT ( 'NONE',  ( 9.104014120666999332, 5.045862207587999748, 8.527865280865999154 ) ) ;
#11808 = FACE_OUTER_BOUND ( 'NONE', #34535, .T. ) ;
#11809 = CARTESIAN_POINT ( 'NONE',  ( 10.35987047770899672, 2.749999999999999556, -7.750389189149368363 ) ) ;
#11810 = CARTESIAN_POINT ( 'NONE',  ( 18.07439970769999960, 3.110573872314000177, -11.47478625844000177 ) ) ;
#11811 = CARTESIAN_POINT ( 'NONE',  ( 11.75718044953559804, 4.889766368533900120, -7.963966784336999005 ) ) ;
#11812 = CARTESIAN_POINT ( 'NONE',  ( 10.43134583106436608, 2.301117676469145223, 7.915378199131434478 ) ) ;
#11813 = CARTESIAN_POINT ( 'NONE',  ( 23.86978363481900089, -9.627977290743000793, -9.781481518887000348 ) ) ;
#11814 = EDGE_CURVE ( 'NONE', #64287, #12534, #29386, .T. ) ;
#11815 = CARTESIAN_POINT ( 'NONE',  ( 24.42275932749500100, -8.981807471221001649, 9.518608303324000985 ) ) ;
#11816 = SURFACE_STYLE_FILL_AREA ( #26880 ) ;
#11817 = VERTEX_POINT ( 'NONE', #59612 ) ;
#11818 = CARTESIAN_POINT ( 'NONE',  ( 7.000000000000000000, 0.000000000000000000, 0.000000000000000000 ) ) ;
#11819 = CARTESIAN_POINT ( 'NONE',  ( 7.293995775811000115, -1.022267936763999963, 0.4061956009805000600 ) ) ;
#11820 = EDGE_CURVE ( 'NONE', #33864, #41132, #32991, .T. ) ;
#11821 = EDGE_CURVE ( 'NONE', #36754, #68281, #4336, .T. ) ;
#11822 = CARTESIAN_POINT ( 'NONE',  ( 18.06381123663115673, 2.863168028152634825, 13.58964369048649701 ) ) ;
#11823 = CARTESIAN_POINT ( 'NONE',  ( 24.51327040776200050, 8.786342692376999608, -8.911852834221001274 ) ) ;
#11824 = CARTESIAN_POINT ( 'NONE',  ( 11.62579573085663043, -2.760622544769000264, -7.714452430741599365 ) ) ;
#11825 = ORIENTED_EDGE ( 'NONE', *, *, #21653, .T. ) ;
#11826 = CARTESIAN_POINT ( 'NONE',  ( 25.29881353977600256, 2.991656389957999984, -11.41428782199000125 ) ) ;
#11827 = CARTESIAN_POINT ( 'NONE',  ( 8.887170280412000523, 2.193665972875999959, 7.400591513898000073 ) ) ;
#11829 = CARTESIAN_POINT ( 'NONE',  ( 24.67921139482200132, 8.727627377900999406, -9.158314240160001063 ) ) ;
#11828 = CARTESIAN_POINT ( 'NONE',  ( 9.658629719592001450, 5.496789211521000418, -7.043125396300999874 ) ) ;
#11830 = CARTESIAN_POINT ( 'NONE',  ( 10.60000000000016662, 3.352395157604608933, 4.756097560975663718 ) ) ;
#11831 = ORIENTED_EDGE ( 'NONE', *, *, #41784, .F. ) ;
#11832 = CARTESIAN_POINT ( 'NONE',  ( 9.520797373037000355, 3.270552986600999912, 5.711478154812000163 ) ) ;
#11833 = CARTESIAN_POINT ( 'NONE',  ( 18.27869735329875311, -2.567871808703005243, -13.76250717860552264 ) ) ;
#11834 = CARTESIAN_POINT ( 'NONE',  ( 11.58487348028854846, 3.117292544139400157, 7.022738645480499642 ) ) ;
#11835 = CARTESIAN_POINT ( 'NONE',  ( 10.90638082498000117, -5.227498618488000126, 6.784459667733999666 ) ) ;
#11836 = CARTESIAN_POINT ( 'NONE',  ( 9.091120559621998609, -3.762710033898000184, 8.787827024292999667 ) ) ;
#11837 = ORIENTED_EDGE ( 'NONE', *, *, #38747, .T. ) ;
#11838 = CARTESIAN_POINT ( 'NONE',  ( 24.60170725920900026, 12.45697517054999892, -2.983025822496999879 ) ) ;
#11839 = B_SPLINE_CURVE_WITH_KNOTS ( 'NONE', 3,
 ( #19103, #13190, #13869, #56168, #45685 ),
 .UNSPECIFIED., .F., .F.,
 ( 4, 1, 4 ),
 ( 0.8746155046758248286, 0.9972320922596067394, 1.000000000000000000 ),
 .UNSPECIFIED. ) ;
#11840 = EDGE_CURVE ( 'NONE', #44223, #28596, #16214, .T. ) ;
#11842 = CARTESIAN_POINT ( 'NONE',  ( 11.03905685320999908, -3.855072944465999907, -9.179476187420998912 ) ) ;
#11841 = CARTESIAN_POINT ( 'NONE',  ( 11.86287780003600112, -11.93788271774999998, 3.912105503483000124 ) ) ;
#11843 = CARTESIAN_POINT ( 'NONE',  ( 7.718572254375063224, -5.707929586103706043, 7.902141240677100775 ) ) ;
#11844 = CARTESIAN_POINT ( 'NONE',  ( 10.77462219945999955, -5.575466189878000911, 8.682669263022999573 ) ) ;
#11845 = CARTESIAN_POINT ( 'NONE',  ( 23.52062801899400313, 3.100976312918000133, 13.78346562762999916 ) ) ;
#11846 = ORIENTED_EDGE ( 'NONE', *, *, #51992, .F. ) ;
#11847 = CARTESIAN_POINT ( 'NONE',  ( 24.08707339289249916, -9.231394016030909810, 9.185131054776540793 ) ) ;
#11848 = CARTESIAN_POINT ( 'NONE',  ( 11.68687482311540116, -2.942322404451000128, 7.072673169413499217 ) ) ;
#11849 = AXIS2_PLACEMENT_3D ( 'NONE', #28577, #11787, #33126 ) ;
#11850 = DIRECTION ( 'NONE',  ( -1.000000000000000000, 0.000000000000000000, 0.000000000000000000 ) ) ;
#11851 = CARTESIAN_POINT ( 'NONE',  ( 11.50271932425157040, 3.812601581225100400, 6.235801371442999397 ) ) ;
#11852 = ORIENTED_EDGE ( 'NONE', *, *, #59211, .F. ) ;
#11853 = CARTESIAN_POINT ( 'NONE',  ( 8.822164158776001130, 2.644017913812000131, -7.838184857420000817 ) ) ;
#11854 = CARTESIAN_POINT ( 'NONE',  ( 24.42400777655799970, 12.73291499258000137, -3.018588619611000112 ) ) ;
#11855 = CARTESIAN_POINT ( 'NONE',  ( 12.48129647765398076, 3.124180215534350769, -12.20653620603297362 ) ) ;
#11856 = CARTESIAN_POINT ( 'NONE',  ( 12.09966954483535773, -3.361010663344000005, 8.485927942460499196 ) ) ;
#11857 = CARTESIAN_POINT ( 'NONE',  ( 7.952954263467808538, 4.709204723604079490, -6.291795282047308646 ) ) ;
#11858 = CARTESIAN_POINT ( 'NONE',  ( 10.59184687351642751, 4.999583552997727054, -8.268183399968643599 ) ) ;
#11859 = ORIENTED_EDGE ( 'NONE', *, *, #42496, .T. ) ;
#11860 = CARTESIAN_POINT ( 'NONE',  ( 23.89320776801300283, 11.54071136943000297, 2.936967729234000402 ) ) ;
#11861 = B_SPLINE_CURVE_WITH_KNOTS ( 'NONE', 3,
 ( #13485, #8910, #51894, #14166 ),
 .UNSPECIFIED., .F., .F.,
 ( 4, 4 ),
 ( 0.000000000000000000, 1.000000000000000000 ),
 .UNSPECIFIED. ) ;
#11862 = DIRECTION ( 'NONE',  ( 1.000000000000000000, 0.000000000000000000, 0.000000000000000000 ) ) ;
#11863 = ORIENTED_EDGE ( 'NONE', *, *, #63116, .T. ) ;
#11864 = CARTESIAN_POINT ( 'NONE',  ( 9.972493632716181722, -3.822122635138222702, -9.279087650161129019 ) ) ;
#11865 = CARTESIAN_POINT ( 'NONE',  ( 10.29262282008599882, 4.451581486939200083, 6.771613406921599854 ) ) ;
#11866 = EDGE_CURVE ( 'NONE', #53988, #65371, #23248, .T. ) ;
#11867 = CARTESIAN_POINT ( 'NONE',  ( 10.49412055961999890, -2.866949708568999888, -8.960719633954001395 ) ) ;
#11868 = CARTESIAN_POINT ( 'NONE',  ( 10.60199294549000193, 2.164976235211999889, -7.764525279724000306 ) ) ;
#11869 = CARTESIAN_POINT ( 'NONE',  ( 18.26272493605000236, -11.59941211794000004, 4.057574997846999487 ) ) ;
#11870 = CARTESIAN_POINT ( 'NONE',  ( 10.41185831014999863, -2.101597930377999912, 7.856264717901999539 ) ) ;
#11871 = CARTESIAN_POINT ( 'NONE',  ( 13.55563772304700088, 9.581334502426001265, 7.839063693813000278 ) ) ;
#11872 = CARTESIAN_POINT ( 'NONE',  ( 17.91965136929538005, -0.5080407711865443376, -12.68632595416894837 ) ) ;
#11873 = ADVANCED_FACE ( 'NONE', ( #23937 ), #56440, .F. ) ;
#11874 = CYLINDRICAL_SURFACE ( 'NONE', #35253, 0.6250000000000005551 ) ;
#11875 = CARTESIAN_POINT ( 'NONE',  ( 11.55194988689359903, -3.419512757306400363, -8.638573882912000457 ) ) ;
#11876 = CARTESIAN_POINT ( 'NONE',  ( 9.021579719592999425, 2.193665972875999959, 7.400591513898000073 ) ) ;
#11877 = ORIENTED_EDGE ( 'NONE', *, *, #22358, .F. ) ;
#11878 = SURFACE_STYLE_USAGE ( .BOTH. , #5941 ) ;
#11879 = AXIS2_PLACEMENT_3D ( 'NONE', #32425, #53740, #63179 ) ;
#11880 = CARTESIAN_POINT ( 'NONE',  ( 11.60000000000000320, -4.813068503488584504, -8.037608584222631691 ) ) ;
#11881 = CARTESIAN_POINT ( 'NONE',  ( 7.100000000000000533, 4.000000000000000000, 8.849999999999999645 ) ) ;
#11882 = CARTESIAN_POINT ( 'NONE',  ( 5.700000000378000031, -0.2999999996220999443, 3.150000004979999879 ) ) ;
#11883 = AXIS2_PLACEMENT_3D ( 'NONE', #69044, #54336, #5749 ) ;
#11884 = CARTESIAN_POINT ( 'NONE',  ( 18.18389880332053465, 2.839229093938504089, 12.27596119698807620 ) ) ;
#11885 = CARTESIAN_POINT ( 'NONE',  ( 24.53429014209899961, 12.47024915613999951, 3.026245713505000268 ) ) ;
#11886 = CARTESIAN_POINT ( 'NONE',  ( 10.96578430013000016, 7.637186626153999569, 6.308908953828000321 ) ) ;
#11887 = CARTESIAN_POINT ( 'NONE',  ( 9.777558426223626142, -3.641115516887601267, 6.702043737600841489 ) ) ;
#11888 = CARTESIAN_POINT ( 'NONE',  ( 8.776575450301999481, 3.932070968445029902, 6.560591699025100532 ) ) ;
#11889 = ORIENTED_EDGE ( 'NONE', *, *, #15959, .T. ) ;
#11890 = CARTESIAN_POINT ( 'NONE',  ( 12.78084111884637331, -3.199751093817833958, 12.18694350317452724 ) ) ;
#11891 = B_SPLINE_CURVE_WITH_KNOTS ( 'NONE', 3,
 ( #33739, #18687, #28143, #23241 ),
 .UNSPECIFIED., .F., .F.,
 ( 4, 4 ),
 ( 0.000000000000000000, 1.000000000000000000 ),
 .UNSPECIFIED. ) ;
#11892 = CARTESIAN_POINT ( 'NONE',  ( 8.973138961223998677, -3.053949131563199693, -8.139313957553699908 ) ) ;
#11893 = CARTESIAN_POINT ( 'NONE',  ( 24.40777907822999993, -3.358845133677000216, -12.19253384565000076 ) ) ;
#11894 = DIRECTION ( 'NONE',  ( 0.000000000000000000, -2.657874751134998991E-08, 0.9999999999999996669 ) ) ;
#11895 = CONICAL_SURFACE ( 'NONE', #770, 12.44999944941000081, 0.7853981146832407223 ) ;
#11896 = B_SPLINE_CURVE_WITH_KNOTS ( 'NONE', 3,
 ( #65908, #18036, #60673, #12786 ),
 .UNSPECIFIED., .F., .F.,
 ( 4, 4 ),
 ( 0.000000000000000000, 1.000000000000000000 ),
 .UNSPECIFIED. ) ;
#11897 = CARTESIAN_POINT ( 'NONE',  ( 10.62487750876920067, 3.456442671114800191, -8.343502390669698343 ) ) ;
#11898 = CARTESIAN_POINT ( 'NONE',  ( 12.72146951531671455, -0.7145943380091435149, 12.57972004139935152 ) ) ;
#11899 = CARTESIAN_POINT ( 'NONE',  ( 7.464691113743000095, 4.351669901925999895, 8.977196921526999773 ) ) ;
#11900 = CARTESIAN_POINT ( 'NONE',  ( 17.55505043854143565, 1.875000000000000000, 13.78627172894481667 ) ) ;
#11901 = CARTESIAN_POINT ( 'NONE',  ( 12.78418764580518108, 3.124999405572221445, 12.28373085793388064 ) ) ;
#11902 = VERTEX_POINT ( 'NONE', #60308 ) ;
#11903 = CARTESIAN_POINT ( 'NONE',  ( 10.08477413932373246, 4.544730055193329399, -8.875862789218047055 ) ) ;
#11904 = CARTESIAN_POINT ( 'NONE',  ( 11.60533460557258323, 4.184174550317700358, -8.625775273268001087 ) ) ;
#11905 = CARTESIAN_POINT ( 'NONE',  ( 11.78192504596561996, -3.091022006579346115, 7.174999814284952926 ) ) ;
#11906 = ADVANCED_FACE ( 'NONE', ( #7503 ), #60649, .T. ) ;
#11907 = CARTESIAN_POINT ( 'NONE',  ( 8.592138961223998450, 5.059894361919000438, -8.216246114996598848 ) ) ;
#11909 = DIRECTION ( 'NONE',  ( 1.000000000000000000, 0.000000000000000000, 0.000000000000000000 ) ) ;
#11908 = CARTESIAN_POINT ( 'NONE',  ( 8.361434368299004660, 5.126350915548002263, 6.365320234831002288 ) ) ;
#11910 = CARTESIAN_POINT ( 'NONE',  ( 11.26902897915239876, -3.778278678798900447, -8.337339982364900592 ) ) ;
#11911 = CARTESIAN_POINT ( 'NONE',  ( 11.79999999684100054, 12.15995044155999949, 2.000340912084999978 ) ) ;
#11912 = VERTEX_POINT ( 'NONE', #2269 ) ;
#11913 = CARTESIAN_POINT ( 'NONE',  ( 1.691702730658999787, 2.350777309937000403, -2.257240049571999752 ) ) ;
#11914 = CARTESIAN_POINT ( 'NONE',  ( 23.72389630350670586, -9.881498421283909650, -9.454772414382880186 ) ) ;
#11915 = CARTESIAN_POINT ( 'NONE',  ( 11.90028836426309589, -11.81686663804793724, 4.153560932553760132 ) ) ;
#11916 = CARTESIAN_POINT ( 'NONE',  ( 9.121088727410999297, 3.136022381937999981, 7.427538838030949719 ) ) ;
#11917 = B_SPLINE_CURVE_WITH_KNOTS ( 'NONE', 3,
 ( #61501, #10328, #63804, #15913 ),
 .UNSPECIFIED., .F., .F.,
 ( 4, 4 ),
 ( 0.000000000000000000, 1.000000000000000000 ),
 .UNSPECIFIED. ) ;
#11918 = B_SPLINE_CURVE_WITH_KNOTS ( 'NONE', 3,
 ( #38493, #11920, #33261, #60859 ),
 .UNSPECIFIED., .F., .F.,
 ( 4, 4 ),
 ( 0.8744711836180196762, 1.000000000000000000 ),
 .UNSPECIFIED. ) ;
#11919 = CARTESIAN_POINT ( 'NONE',  ( 12.15420371307394909, -2.840396063362202295, 13.70885132993088007 ) ) ;
#11920 = CARTESIAN_POINT ( 'NONE',  ( 7.961731591766461946, 5.351349901897397565, 7.263035046629775060 ) ) ;
#11921 = CARTESIAN_POINT ( 'NONE',  ( 12.80505043854143388, 1.816864895258029522, 13.85234397965874464 ) ) ;
#11922 = CARTESIAN_POINT ( 'NONE',  ( 13.21722669115800031, -12.32379348829999977, -1.906876488274000137 ) ) ;
#11923 = ORIENTED_EDGE ( 'NONE', *, *, #43404, .F. ) ;
#11924 = EDGE_CURVE ( 'NONE', #24276, #21416, #25148, .T. ) ;
#11925 = CARTESIAN_POINT ( 'NONE',  ( 4.182224458653999832, 0.2386897511459999954, 1.109017420168999957 ) ) ;
#11926 = CARTESIAN_POINT ( 'NONE',  ( 8.603645510037566169, 4.706833859774536499, 5.918599468013309384 ) ) ;
#11927 = VECTOR ( 'NONE', #20474, 1000.000000000000000 ) ;
#11928 = CARTESIAN_POINT ( 'NONE',  ( 10.17905590578999941, 2.899999999999999911, 6.571291218949999902 ) ) ;
#11929 = CARTESIAN_POINT ( 'NONE',  ( 0.4812757755485000399, 3.010927365844000114, -1.992372462812000089 ) ) ;
#11930 = CARTESIAN_POINT ( 'NONE',  ( 11.59999999999999964, 4.000000000000000000, -7.500000000000000000 ) ) ;
#11931 = CARTESIAN_POINT ( 'NONE',  ( 18.30000103245939158, -11.66744832144745203, 3.971921730545766138 ) ) ;
#11932 = CARTESIAN_POINT ( 'NONE',  ( 10.85069631730999973, 4.478098874537000285, 6.162039661770999821 ) ) ;
#11933 = COLOUR_RGB ( '', 0.66274510, 0.83137255, 0.94901961) ;
#11934 = CARTESIAN_POINT ( 'NONE',  ( 11.56441235500451015, 3.361299021099800388, 8.085115074060599483 ) ) ;
#11935 = CARTESIAN_POINT ( 'NONE',  ( 11.09999999999999964, -2.700000000000000178, -6.461133846875999787 ) ) ;
#11936 = CARTESIAN_POINT ( 'NONE',  ( 10.88760685321000032, -5.634843745609000365, -7.088991614236999972 ) ) ;
#11937 = CIRCLE ( 'NONE', #20873, 1.250000000000000000 ) ;
#11938 = DIRECTION ( 'NONE',  ( 0.000000000000000000, -0.4595937023756062056, -0.8881292860483110951 ) ) ;
#11939 = CARTESIAN_POINT ( 'NONE',  ( 9.865041550948095761, 2.650034642413356512, -7.500002425457249267 ) ) ;
#11940 = DIRECTION ( 'NONE',  ( 8.953188301455325544E-11, 0.2714597137498098722, -0.9624498032681346738 ) ) ;
#11941 = VERTEX_POINT ( 'NONE', #28858 ) ;
#11942 = CARTESIAN_POINT ( 'NONE',  ( 7.466031583599719745, 2.286618937992697997, 7.155872792181217079 ) ) ;
#11943 = EDGE_LOOP ( 'NONE', ( #30382, #37142, #32762, #15048 ) ) ;
#11944 = AXIS2_PLACEMENT_3D ( 'NONE', #11818, #68823, #69171 ) ;
#11945 = B_SPLINE_CURVE_WITH_KNOTS ( 'NONE', 3,
 ( #10650, #31996, #16921, #21150, #58896, #42477, #15896, #58206, #31643, #33019, #10999, #48063, #52966, #27428 ),
 .UNSPECIFIED., .F., .F.,
 ( 4, 2, 2, 2, 2, 2, 4 ),
 ( 0.000000000000000000, 0.1250000000000008327, 0.2500000000000016653, 0.5000000000000029976, 0.6250000000000021094, 0.7500000000000014433, 1.000000000000000000 ),
 .UNSPECIFIED. ) ;
#11946 = CARTESIAN_POINT ( 'NONE',  ( 17.80560960443414942, -3.072671113640228491, 13.53517819557379376 ) ) ;
#11947 = CARTESIAN_POINT ( 'NONE',  ( 10.27195525820100031, -4.120672149427799802, -6.227697122196000024 ) ) ;
#11948 = VERTEX_POINT ( 'NONE', #12764 ) ;
#11949 = CARTESIAN_POINT ( 'NONE',  ( 10.64391429142989765, 4.022379549362480766, 8.674673860548999471 ) ) ;
#11950 = DIRECTION ( 'NONE',  ( -1.000000000000000000, 0.000000000000000000, 0.000000000000000000 ) ) ;
#11951 = CARTESIAN_POINT ( 'NONE',  ( 23.71151258249847871, 3.235038466978575666, -13.31088662455443128 ) ) ;
#11952 = CARTESIAN_POINT ( 'NONE',  ( 9.194604681486000075, 5.157771204918000230, 8.637848577075999401 ) ) ;
#11953 = CARTESIAN_POINT ( 'NONE',  ( 24.34832137511671135, -8.810502415987484071, -8.810502415987484071 ) ) ;
#11954 = CARTESIAN_POINT ( 'NONE',  ( 10.09393020684899867, -2.750000000000000000, -7.500000000000000000 ) ) ;
#11955 = CARTESIAN_POINT ( 'NONE',  ( 11.60581233665799950, 3.287326773434000149, -11.32699406611000015 ) ) ;
#11956 = CONICAL_SURFACE ( 'NONE', #67789, 0.9999998338055000602, 0.7853981908209605178 ) ;
#11957 = ADVANCED_FACE ( 'NONE', ( #66919 ), #68093, .F. ) ;
#11958 = CARTESIAN_POINT ( 'NONE',  ( 10.27571314244999989, -5.689440078020999714, -7.562019725378000601 ) ) ;
#11959 = CARTESIAN_POINT ( 'NONE',  ( 11.46595122972049907, -3.656201404350900130, -6.704952129760900270 ) ) ;
#11960 = ORIENTED_EDGE ( 'NONE', *, *, #10391, .T. ) ;
#11961 = CARTESIAN_POINT ( 'NONE',  ( 10.85632228256448428, -2.901817188071407205, -5.114652766790887206 ) ) ;
#11962 = ORIENTED_EDGE ( 'NONE', *, *, #67625, .T. ) ;
#11963 = CARTESIAN_POINT ( 'NONE',  ( 9.957691290288998687, 3.110563525881361535, 6.586710612921466534 ) ) ;
#11964 =( LENGTH_UNIT ( ) NAMED_UNIT ( * ) SI_UNIT ( .MILLI., .METRE. ) );
#11965 = ORIENTED_EDGE ( 'NONE', *, *, #42947, .F. ) ;
#11966 = CARTESIAN_POINT ( 'NONE',  ( 17.92207321742860415, -3.154877352415835556, -13.63994794764937701 ) ) ;
#11967 = CARTESIAN_POINT ( 'NONE',  ( 10.27152834814000215, -4.757994137332000051, 4.537574396426000689 ) ) ;
#11968 = CARTESIAN_POINT ( 'NONE',  ( 10.31652245563454073, 4.682420780414364714, 6.971781362826274808 ) ) ;
#11969 = CARTESIAN_POINT ( 'NONE',  ( 12.80505043854144276, -0.6250000000000001110, 13.88107975066923316 ) ) ;
#11970 = CARTESIAN_POINT ( 'NONE',  ( 12.34634080959761171, 2.074995934380768237, 13.75442486551246013 ) ) ;
#11971 = CARTESIAN_POINT ( 'NONE',  ( 17.71905360607588875, -1.896551502301641712, 12.57190390430904436 ) ) ;
#11972 = DIRECTION ( 'NONE',  ( -1.000000000000000000, 0.000000000000000000, 0.000000000000000000 ) ) ;
#11973 = CARTESIAN_POINT ( 'NONE',  ( 12.58447130036695327, 0.5851376999905932852, 13.88342059653409066 ) ) ;
#11974 = ORIENTED_EDGE ( 'NONE', *, *, #57682, .T. ) ;
#11975 = CARTESIAN_POINT ( 'NONE',  ( 7.243409439180999776, 5.346164515353000191, -7.398308812559000636 ) ) ;
#11976 = CARTESIAN_POINT ( 'NONE',  ( 17.56088320631100075, 12.16696388215000013, -3.135175697041999499 ) ) ;
#11977 = CARTESIAN_POINT ( 'NONE',  ( 9.328216720588626387, 4.762939826712631941, 7.071683423462644669 ) ) ;
#11978 = CARTESIAN_POINT ( 'NONE',  ( 4.927325434513999625, -0.4869043722212999525, -1.082571524400999907 ) ) ;
#11979 = VECTOR ( 'NONE', #34055, 1000.000000000000000 ) ;
#11980 = CARTESIAN_POINT ( 'NONE',  ( 8.541054719591000932, 3.807713920470999991, -9.221758713517999695 ) ) ;
#11981 = PRESENTATION_LAYER_ASSIGNMENT (  '', '', ( #35457 ) ) ;
#11982 = CARTESIAN_POINT ( 'NONE',  ( 9.854346873516623972, 2.749999999999999112, -7.663624617374463099 ) ) ;
#11983 = CARTESIAN_POINT ( 'NONE',  ( 10.11858840337999865, -3.393395892949000014, -5.921999462319999630 ) ) ;
#11984 = DIRECTION ( 'NONE',  ( 0.000000000000000000, -1.000000000000000000, 0.000000000000000000 ) ) ;
#11985 = CARTESIAN_POINT ( 'NONE',  ( 10.55101852148010266, -5.350099180695897516, -7.263329207706007651 ) ) ;
#11986 = CIRCLE ( 'NONE', #64419, 2.149999999999999911 ) ;
#11987 = FACE_OUTER_BOUND ( 'NONE', #9223, .T. ) ;
#11988 = DIRECTION ( 'NONE',  ( 0.000000000000000000, -1.000000000000000000, 0.000000000000000000 ) ) ;
#11989 = PLANE ( 'NONE',  #67047 ) ;
#11990 = CARTESIAN_POINT ( 'NONE',  ( 24.45617572362546355, 12.38364420599299898, -3.108063458830152115 ) ) ;
#11991 = EDGE_CURVE ( 'NONE', #17504, #44736, #45282, .T. ) ;
#11992 = EDGE_CURVE ( 'NONE', #10762, #22430, #28509, .T. ) ;
#11993 = CARTESIAN_POINT ( 'NONE',  ( 11.18412378248529926, 3.450971646934100079, -6.461285588983000316 ) ) ;
#11994 = CARTESIAN_POINT ( 'NONE',  ( 8.824126402770998467, 4.939810497841199854, -7.145601175474399547 ) ) ;
#11996 = FACE_OUTER_BOUND ( 'NONE', #63726, .T. ) ;
#11995 = CARTESIAN_POINT ( 'NONE',  ( 9.344480666858999030, -3.665111009453500213, 6.553061479084200336 ) ) ;
#11997 = CARTESIAN_POINT ( 'NONE',  ( 11.38351354018293904, -5.249999999999998224, 7.663624617374469317 ) ) ;
#11998 = EDGE_LOOP ( 'NONE', ( #62347, #57776, #18350, #6850, #20978, #62931, #42407, #22467, #37662, #4449, #20005 ) ) ;
#11999 = AXIS2_PLACEMENT_3D ( 'NONE', #7215, #1624, #22939 ) ;
#12000 = CARTESIAN_POINT ( 'NONE',  ( 10.56591429142999949, 4.019686495353769651, 8.533318907609000803 ) ) ;
#12001 = CARTESIAN_POINT ( 'NONE',  ( 11.27109998545999936, -5.469594811916000054, 8.504700858852999090 ) ) ;
#12002 = CARTESIAN_POINT ( 'NONE',  ( 9.403734463322997783, 4.118936914955599882, 6.364399516445999438 ) ) ;
#12003 = CARTESIAN_POINT ( 'NONE',  ( 10.65434687351636178, -2.749999999999998668, -7.336375382625537789 ) ) ;
#12004 = AXIS2_PLACEMENT_3D ( 'NONE', #27113, #47403, #37251 ) ;
#12005 = CARTESIAN_POINT ( 'NONE',  ( 9.758146639703001668, -2.901368778958000050, 6.555068849476000103 ) ) ;
#12006 = CARTESIAN_POINT ( 'NONE',  ( 9.710415594366155645, -5.733461026711495379, 7.739234121907153430 ) ) ;
#12007 = CARTESIAN_POINT ( 'NONE',  ( 10.49809687351654297, 3.672815144550898303, 6.282534154164607365 ) ) ;
#12008 = ORIENTED_EDGE ( 'NONE', *, *, #58641, .F. ) ;
#12009 = EDGE_CURVE ( 'NONE', #8238, #28950, #1009, .T. ) ;
#12010 = CARTESIAN_POINT ( 'NONE',  ( 9.457355082327998375, -4.449513475323099598, -6.601790705997299114 ) ) ;
#12011 = DIRECTION ( 'NONE',  ( -1.000000000000000000, 0.000000000000000000, 0.000000000000000000 ) ) ;
#12012 = CARTESIAN_POINT ( 'NONE',  ( 6.720013804402999114, -1.131649478240000173, 0.5631818380099999910 ) ) ;
#12013 = EDGE_CURVE ( 'NONE', #8503, #53057, #64216, .T. ) ;
#12014 = CARTESIAN_POINT ( 'NONE',  ( 6.999999999999997335, 10.71083106425634490, -3.767558118307691828 ) ) ;
#12015 = CARTESIAN_POINT ( 'NONE',  ( 24.51228084553499897, -3.325039717427999975, 12.06631758408999922 ) ) ;
#12016 = CARTESIAN_POINT ( 'NONE',  ( 12.13825819896753977, -4.851203879749700576, 7.339530235223699073 ) ) ;
#12017 = CARTESIAN_POINT ( 'NONE',  ( 11.49056651104150006, 4.085456792591960706, -6.638028001068500217 ) ) ;
#12018 = CARTESIAN_POINT ( 'NONE',  ( 12.24279999538062924, 2.226287937568673936, -13.72772666894336879 ) ) ;
#12019 = CARTESIAN_POINT ( 'NONE',  ( -15.86200481174999943, -5.599999999999999645, -6.571291218949999902 ) ) ;
#12020 = CARTESIAN_POINT ( 'NONE',  ( 12.35662541760398625, 3.053258836637784857, 12.22465729757279185 ) ) ;
#12021 = VERTEX_POINT ( 'NONE', #40029 ) ;
#12022 = CARTESIAN_POINT ( 'NONE',  ( 11.49978667957999967, -12.43119799159999950, -1.530013559959999991 ) ) ;
#12023 = AXIS2_PLACEMENT_3D ( 'NONE', #46368, #62435, #47401 ) ;
#12024 = CARTESIAN_POINT ( 'NONE',  ( 12.13954239761512177, -0.2899337805559861203, -13.99700184298317396 ) ) ;
#12025 = CARTESIAN_POINT ( 'NONE',  ( 14.03176826122700227, -8.820984799833000878, -7.691098505213000536 ) ) ;
#12026 = DIRECTION ( 'NONE',  ( 1.000000000000000000, 0.000000000000000000, 0.000000000000000000 ) ) ;
#12027 = CARTESIAN_POINT ( 'NONE',  ( 10.52934687351650389, -3.836375382625533348, -8.749999999999998224 ) ) ;
#12028 = CARTESIAN_POINT ( 'NONE',  ( 7.000000000000000000, 8.619706073299337135, 4.541782559989387735 ) ) ;
#12029 = CARTESIAN_POINT ( 'NONE',  ( 5.685751648549689286, 12.05129647863442344, -3.726325695169643737 ) ) ;
#12030 = EDGE_LOOP ( 'NONE', ( #47639, #12720, #62870, #20643, #48432, #11923, #19345, #51339, #68354, #57801, #68429, #35402 ) ) ;
#12031 = VECTOR ( 'NONE', #39209, 1000.000000000000114 ) ;
#12032 = B_SPLINE_CURVE_WITH_KNOTS ( 'NONE', 3,
 ( #11705, #38630, #33044, #1230 ),
 .UNSPECIFIED., .F., .F.,
 ( 4, 4 ),
 ( 0.000000000000000000, 1.000000000000000000 ),
 .UNSPECIFIED. ) ;
#12033 = CARTESIAN_POINT ( 'NONE',  ( 23.89320776801300283, 8.313844348291002717, 8.526065358951003148 ) ) ;
#12034 = CARTESIAN_POINT ( 'NONE',  ( 18.11747123342421162, 2.226643993407489308, -13.72766178540381077 ) ) ;
#12035 = VERTEX_POINT ( 'NONE', #55758 ) ;
#12036 = FACE_OUTER_BOUND ( 'NONE', #61477, .T. ) ;
#12037 = CARTESIAN_POINT ( 'NONE',  ( 24.73254324275212213, 8.642950426568003053, -8.588141212706347005 ) ) ;
#12038 = AXIS2_PLACEMENT_3D ( 'NONE', #48896, #58343, #63585 ) ;
#12039 = CARTESIAN_POINT ( 'NONE',  ( 9.758079719591000512, 4.905765359186999852, -8.776126235875999271 ) ) ;
#12040 = DIRECTION ( 'NONE',  ( -1.000000000000000000, 0.000000000000000000, 0.000000000000000000 ) ) ;
#12041 = CARTESIAN_POINT ( 'NONE',  ( 10.63880513895979973, -2.849548954067000039, -6.860457220153399760 ) ) ;
#12042 = CARTESIAN_POINT ( 'NONE',  ( 7.912010841225000313, 5.556101987819999977, -8.589999141415001205 ) ) ;
#12043 = DIRECTION ( 'NONE',  ( -1.000000000000000000, 0.000000000000000000, 0.000000000000000000 ) ) ;
#12044 = DIRECTION ( 'NONE',  ( 0.000000000000000000, 0.000000000000000000, 1.000000000000000000 ) ) ;
#12045 = ORIENTED_EDGE ( 'NONE', *, *, #57521, .T. ) ;
#12046 = CARTESIAN_POINT ( 'NONE',  ( 10.93728138146000006, -5.425439422033999648, 7.240583766112999697 ) ) ;
#12047 = CARTESIAN_POINT ( 'NONE',  ( 18.01235687061446455, -2.926439070453491720, -13.57366610795276962 ) ) ;
#12048 = CARTESIAN_POINT ( 'NONE',  ( 8.960616452296999768, -2.899999999999999911, 6.279946362737000243 ) ) ;
#12049 = ORIENTED_EDGE ( 'NONE', *, *, #62825, .F. ) ;
#12050 = AXIS2_PLACEMENT_3D ( 'NONE', #1111, #22424, #5313 ) ;
#12051 = CARTESIAN_POINT ( 'NONE',  ( 8.865073590557452476, 2.650142864597553327, -7.500004675916596142 ) ) ;
#12052 = CARTESIAN_POINT ( 'NONE',  ( 10.95519194037999888, -3.860335380237000180, -6.147338954930000376 ) ) ;
#12053 = EDGE_LOOP ( 'NONE', ( #10857, #28681, #44984 ) ) ;
#12054 = CARTESIAN_POINT ( 'NONE',  ( 8.646822372493998543, 3.711294259598199918, 6.555546982591299532 ) ) ;
#12055 = CARTESIAN_POINT ( 'NONE',  ( 18.27054884872056206, -2.599315299774876298, -12.32899436121337189 ) ) ;
#12056 = CARTESIAN_POINT ( 'NONE',  ( 4.590139323399000659, -1.453974671782999994, -0.5584015962769001140 ) ) ;
#12057 = CARTESIAN_POINT ( 'NONE',  ( 7.720595830382998237, 4.816914828557000483, -6.342622631669999400 ) ) ;
#12058 = CARTESIAN_POINT ( 'NONE',  ( 24.92738949723038999, 11.56001277368646640, -3.214474823069669807 ) ) ;
#12059 = FACE_OUTER_BOUND ( 'NONE', #18215, .T. ) ;
#12060 = EDGE_CURVE ( 'NONE', #19784, #12411, #20940, .T. ) ;
#12061 = VECTOR ( 'NONE', #41608, 1000.000000000000000 ) ;
#12062 = CARTESIAN_POINT ( 'NONE',  ( 8.876797255587998592, 4.866234952405400271, 7.536673658251589636 ) ) ;
#12063 = DIRECTION ( 'NONE',  ( 0.000000000000000000, -0.9999808993455937545, -0.006180691221632959691 ) ) ;
#12064 = EDGE_LOOP ( 'NONE', ( #1935, #64152, #33425, #33405, #21171, #68057, #40777, #45987 ) ) ;
#12065 = LINE ( 'NONE', #18010, #21375 ) ;
#12066 = CARTESIAN_POINT ( 'NONE',  ( 10.25880778041000063, 2.491777456852000139, -7.289938575364999451 ) ) ;
#12067 = CARTESIAN_POINT ( 'NONE',  ( 18.31644260632910814, -11.66217921385985079, 4.569092474540076054 ) ) ;
#12068 = CARTESIAN_POINT ( 'NONE',  ( 12.18824001706381210, 2.602861674270835923, -13.65112526288234029 ) ) ;
#12069 = CARTESIAN_POINT ( 'NONE',  ( 9.887000818240000655, -5.131870447930000800, -8.096031607030200306 ) ) ;
#12070 = CARTESIAN_POINT ( 'NONE',  ( 10.89874164595999950, -2.834836218627000193, 9.088455567997000273 ) ) ;
#12071 = CARTESIAN_POINT ( 'NONE',  ( 18.25578913467702336, -0.1888260363403085340, 13.99874504378992590 ) ) ;
#12072 = CYLINDRICAL_SURFACE ( 'NONE', #63172, 1.350000000000000533 ) ;
#12073 = ORIENTED_EDGE ( 'NONE', *, *, #40020, .F. ) ;
#12074 = ORIENTED_EDGE ( 'NONE', *, *, #25835, .F. ) ;
#12075 = CARTESIAN_POINT ( 'NONE',  ( 9.345514158774999913, 5.775964236216999836, -8.174909295649001706 ) ) ;
#12076 = CARTESIAN_POINT ( 'NONE',  ( 12.29062815680005549, -0.3550741891739155331, 13.89389891666938226 ) ) ;
#12077 = CARTESIAN_POINT ( 'NONE',  ( 10.62426357027499968, -2.745128867668000350, 7.257895958275299542 ) ) ;
#12078 = CARTESIAN_POINT ( 'NONE',  ( 7.309012197735174965, -3.319721303298527104, 6.319100263144195928 ) ) ;
#12079 = LINE ( 'NONE', #50179, #61842 ) ;
#12080 = EDGE_CURVE ( 'NONE', #42842, #5840, #41001, .T. ) ;
#12081 = ADVANCED_FACE ( 'NONE', ( #28503 ), #30223, .T. ) ;
#12082 = CARTESIAN_POINT ( 'NONE',  ( 8.090519353209000286, -5.342173944271999986, 8.432314172168000610 ) ) ;
#12083 = CARTESIAN_POINT ( 'NONE',  ( 24.84547362285450234, 8.580307739459316352, -9.011481308573959126 ) ) ;
#12085 = CARTESIAN_POINT ( 'NONE',  ( 11.01817738136000102, -6.612169668047999771, 5.428883362029000459 ) ) ;
#12084 = CARTESIAN_POINT ( 'NONE',  ( 10.26035508232799920, -4.572497688003699601, 8.643954013369999245 ) ) ;
#12086 = CARTESIAN_POINT ( 'NONE',  ( 9.258115045126002585, -5.097433850589000670, -6.601368032590999135 ) ) ;
#12087 = EDGE_CURVE ( 'NONE', #49898, #2068, #38524, .T. ) ;
#12088 = CYLINDRICAL_SURFACE ( 'NONE', #16828, 0.4999999999999998335 ) ;
#12089 = CARTESIAN_POINT ( 'NONE',  ( 10.40537527825904007, 5.100000000000000533, -6.445686799541589629 ) ) ;
#12090 = CARTESIAN_POINT ( 'NONE',  ( 18.17981518646734784, 0.01996654564806146087, 12.69998441237379083 ) ) ;
#12091 = CARTESIAN_POINT ( 'NONE',  ( 8.316694573732000606, -2.898380360490000029, 6.611503418275999522 ) ) ;
#12092 = CIRCLE ( 'NONE', #47833, 0.2000000000000004274 ) ;
#12093 = CARTESIAN_POINT ( 'NONE',  ( 18.13624051180335783, -2.730018211839375208, -12.39499564932253328 ) ) ;
#12094 = ORIENTED_EDGE ( 'NONE', *, *, #6260, .T. ) ;
#12096 = CARTESIAN_POINT ( 'NONE',  ( 17.91920925550502020, 10.80976535600978572, -4.345114692431126358 ) ) ;
#12095 = CARTESIAN_POINT ( 'NONE',  ( 9.059370559623998176, -4.192917962110999319, 5.525484568403999930 ) ) ;
#12097 = CARTESIAN_POINT ( 'NONE',  ( 9.798945280410000791, 5.639765292528999829, -8.059103558718000215 ) ) ;
#12098 = DIRECTION ( 'NONE',  ( 1.000000000000000000, 0.000000000000000000, 0.000000000000000000 ) ) ;
#12099 = CARTESIAN_POINT ( 'NONE',  ( 4.400000000000000355, 0.5526513453421999511, 1.394480724316999876 ) ) ;
#12100 = AXIS2_PLACEMENT_3D ( 'NONE', #30961, #46697, #10312 ) ;
#12101 = CARTESIAN_POINT ( 'NONE',  ( 13.49980696793000057, -9.514462421839999351, -7.834836582454001608 ) ) ;
#12102 = EDGE_CURVE ( 'NONE', #28877, #29433, #46824, .T. ) ;
#12103 = CARTESIAN_POINT ( 'NONE',  ( 3.999999173945999686, 1.825000327749000117, 0.000000000000000000 ) ) ;
#12104 = CARTESIAN_POINT ( 'NONE',  ( 2.023109259092000567, 1.242860124574000080, -3.147067557564999785 ) ) ;
#12105 = ORIENTED_EDGE ( 'NONE', *, *, #60303, .T. ) ;
#12106 = AXIS2_PLACEMENT_3D ( 'NONE', #35111, #66214, #18336 ) ;
#12107 = CARTESIAN_POINT ( 'NONE',  ( 12.08612546794235421, 0.09367178904473767720, -12.59965724591066660 ) ) ;
#12108 = CARTESIAN_POINT ( 'NONE',  ( 24.39664737804999817, 8.853227125957333854, -8.853227125957333854 ) ) ;
#12109 = CARTESIAN_POINT ( 'NONE',  ( 18.08628618592427273, 2.970581112497161502, -12.24483314193592776 ) ) ;
#12110 = CARTESIAN_POINT ( 'NONE',  ( 8.477766462057999775, 2.899999999999999911, -6.558719934578999933 ) ) ;
#12111 = CARTESIAN_POINT ( 'NONE',  ( 8.604017219593000476, 5.165497731316000873, 8.645531386060000045 ) ) ;
#12112 = ORIENTED_EDGE ( 'NONE', *, *, #15139, .T. ) ;
#12113 = CARTESIAN_POINT ( 'NONE',  ( 6.234144881615000244, 0.9190761964769998960, -1.327642370976000130 ) ) ;
#12114 = CARTESIAN_POINT ( 'NONE',  ( 7.309404719586999555, 4.580689680786999674, -5.867791741075000900 ) ) ;
#12115 = B_SPLINE_CURVE_WITH_KNOTS ( 'NONE', 3,
 ( #28011, #65043, #59124, #33258 ),
 .UNSPECIFIED., .F., .F.,
 ( 4, 4 ),
 ( 0.000000000000000000, 1.000000000000000000 ),
 .UNSPECIFIED. ) ;
#12117 = CARTESIAN_POINT ( 'NONE',  ( 10.96876099447000108, 2.333339469804000199, 6.524055942683999021 ) ) ;
#12116 = FACE_OUTER_BOUND ( 'NONE', #35621, .T. ) ;
#12118 = CARTESIAN_POINT ( 'NONE',  ( 11.51145123989532948, 4.605239108938600445, -8.668865425277999748 ) ) ;
#12119 = VERTEX_POINT ( 'NONE', #41728 ) ;
#12120 = LINE ( 'NONE', #39040, #9854 ) ;
#12121 = CARTESIAN_POINT ( 'NONE',  ( 10.05083014070727820, 5.349869709803526163, -7.263173528791787348 ) ) ;
#12122 = ORIENTED_EDGE ( 'NONE', *, *, #6555, .T. ) ;
#12123 = CARTESIAN_POINT ( 'NONE',  ( 12.70675980919426173, 3.199682200193715520, -12.18696163212671024 ) ) ;
#12124 = CARTESIAN_POINT ( 'NONE',  ( 16.31144947526900069, 3.254927130315000028, 11.33654363332999893 ) ) ;
#12125 = CARTESIAN_POINT ( 'NONE',  ( 18.14018103492323419, -0.2205930660282629796, -13.89766156610767034 ) ) ;
#12126 = ORIENTED_EDGE ( 'NONE', *, *, #21237, .F. ) ;
#12127 = CARTESIAN_POINT ( 'NONE',  ( 16.01451879247663967, -8.585242134254837509, -7.875498515381707421 ) ) ;
#12128 = DIRECTION ( 'NONE',  ( -1.000000000000000000, 0.000000000000000000, 0.000000000000000000 ) ) ;
#12129 = B_SPLINE_CURVE_WITH_KNOTS ( 'NONE', 3,
 ( #3566, #56030, #9158, #39609 ),
 .UNSPECIFIED., .F., .F.,
 ( 4, 4 ),
 ( 0.000000000000000000, 1.000000000000000000 ),
 .UNSPECIFIED. ) ;
#12130 = CARTESIAN_POINT ( 'NONE',  ( 10.48791429142999831, 4.016993441347180394, -6.608036045330599961 ) ) ;
#12131 = DIRECTION ( 'NONE',  ( -1.000000000000000000, 0.000000000000000000, 0.000000000000000000 ) ) ;
#12132 = CARTESIAN_POINT ( 'NONE',  ( 5.227606837614000135, -0.3108367803229999948, 1.065889863396000115 ) ) ;
#12133 = ORIENTED_EDGE ( 'NONE', *, *, #61833, .F. ) ;
#12134 = CARTESIAN_POINT ( 'NONE',  ( 9.026926658770998202, 4.852728889087999598, 8.683917172082999514 ) ) ;
#12135 = CARTESIAN_POINT ( 'NONE',  ( 12.28991563251189945, -2.854049639552650675, -13.59191281878594992 ) ) ;
#12136 = CARTESIAN_POINT ( 'NONE',  ( 10.06819717211483578, 5.125396288440276393, -6.749639981106758668 ) ) ;
#12137 = CARTESIAN_POINT ( 'NONE',  ( 17.65223863462161802, 0.7192245859873318548, 12.57945610904469724 ) ) ;
#12138 = VERTEX_POINT ( 'NONE', #20064 ) ;
#12139 = CARTESIAN_POINT ( 'NONE',  ( 12.58248715490569047, -1.915879699765342892, -12.56863216566091168 ) ) ;
#12140 = AXIS2_PLACEMENT_3D ( 'NONE', #52196, #32264, #26323 ) ;
#12141 = CARTESIAN_POINT ( 'NONE',  ( 10.63559687351579974, 5.092232985442826099, -6.870476274536379435 ) ) ;
#12142 = CARTESIAN_POINT ( 'NONE',  ( 7.242472165043829513, 4.622497589504547477, -5.750277660584385053 ) ) ;
#12143 = EDGE_CURVE ( 'NONE', #39483, #61665, #30751, .T. ) ;
#12144 = DIRECTION ( 'NONE',  ( 1.000000000000000000, 0.000000000000000000, 0.000000000000000000 ) ) ;
#12145 = CARTESIAN_POINT ( 'NONE',  ( 12.70945613931270124, -1.793774045999469102, -13.88460948128834360 ) ) ;
#12146 = EDGE_CURVE ( 'NONE', #14135, #47477, #34103, .T. ) ;
#12147 = AXIS2_PLACEMENT_3D ( 'NONE', #39883, #29402, #61882 ) ;
#12148 = CARTESIAN_POINT ( 'NONE',  ( 10.42795525820099911, -4.094749303624469761, -6.501013802764199490 ) ) ;
#12149 = CARTESIAN_POINT ( 'NONE',  ( 10.34393020684899867, 2.750000000000000000, 7.500000000000000000 ) ) ;
#12150 = CARTESIAN_POINT ( 'NONE',  ( 17.92103372721324561, -3.006741473881710647, 12.31895748915803424 ) ) ;
#12151 = ORIENTED_EDGE ( 'NONE', *, *, #47373, .T. ) ;
#12152 = CARTESIAN_POINT ( 'NONE',  ( 11.59966954483535773, -3.361010663344000005, -6.514072057539499916 ) ) ;
#12153 = ORIENTED_EDGE ( 'NONE', *, *, #10897, .F. ) ;
#12154 = CARTESIAN_POINT ( 'NONE',  ( 25.29989727901499919, -2.078227429405999693, -11.31065739696999906 ) ) ;
#12155 = CARTESIAN_POINT ( 'NONE',  ( 9.210288521113000115, -4.352953559891299840, 6.715449042252499723 ) ) ;
#12156 = CARTESIAN_POINT ( 'NONE',  ( 2.670826577536000279, -1.894280328234999811, -2.798560188998999720 ) ) ;
#12157 = CARTESIAN_POINT ( 'NONE',  ( 10.26368921839999970, -4.794141574281000295, -8.804455889106000299 ) ) ;
#12158 = DIRECTION ( 'NONE',  ( -0.9999999999995587974, -4.522743910995809051E-07, -8.233165796359658046E-07 ) ) ;
#12159 = CARTESIAN_POINT ( 'NONE',  ( 5.700000000172999570, 0.5292307618289999738, 2.083846155904000241 ) ) ;
#12160 = CARTESIAN_POINT ( 'NONE',  ( 8.749283493600000128, 4.089987329977850194, -8.350279134800100422 ) ) ;
#12161 = ORIENTED_EDGE ( 'NONE', *, *, #24662, .F. ) ;
#12162 = DIRECTION ( 'NONE',  ( -1.000000000000000000, 0.000000000000000000, 0.000000000000000000 ) ) ;
#12163 = CARTESIAN_POINT ( 'NONE',  ( 11.10026222744819790, -4.774534945026900346, 6.861998062869400172 ) ) ;
#12164 = CARTESIAN_POINT ( 'NONE',  ( 9.124700695083998170, 4.778663323155000420, 8.799742559280000265 ) ) ;
#12165 = DIRECTION ( 'NONE',  ( 0.000000000000000000, -0.9549051095262108824, 0.2969111513580035000 ) ) ;
#12166 = CARTESIAN_POINT ( 'NONE',  ( 10.79399293566600093, -3.453258297007899991, 6.829299525004299376 ) ) ;
#12167 = CARTESIAN_POINT ( 'NONE',  ( 18.35192688406300121, 2.803631260452999818, -11.45923525916999886 ) ) ;
#12168 = CARTESIAN_POINT ( 'NONE',  ( 11.43718179236249988, 3.790319673775199849, -6.518682001772900136 ) ) ;
#12169 = EDGE_CURVE ( 'NONE', #16567, #62492, #57453, .T. ) ;
#12170 = B_SPLINE_CURVE_WITH_KNOTS ( 'NONE', 3,
 ( #10324, #15230, #26068, #68701, #20472, #36210, #15577 ),
 .UNSPECIFIED., .F., .F.,
 ( 4, 1, 1, 1, 4 ),
 ( 0.000000000000000000, 0.2500000039167279420, 0.5000000015353956995, 0.7499999991540633459, 1.000000000000000000 ),
 .UNSPECIFIED. ) ;
#12171 = CARTESIAN_POINT ( 'NONE',  ( 10.29264778178926321, 4.710327358940427089, 9.125082257938260000 ) ) ;
#12172 = CARTESIAN_POINT ( 'NONE',  ( 9.479721904869998994, 4.995641764568400589, -8.058956102599799109 ) ) ;
#12173 = CARTESIAN_POINT ( 'NONE',  ( 23.54905859008200153, -10.40163749118999981, -9.427750568795000063 ) ) ;
#12174 = DIRECTION ( 'NONE',  ( -1.000000000000000000, 0.000000000000000000, 0.000000000000000000 ) ) ;
#12175 = CARTESIAN_POINT ( 'NONE',  ( 24.57788509281051148, 3.600249671649326189, -12.25995025209595646 ) ) ;
#12176 = ORIENTED_EDGE ( 'NONE', *, *, #23041, .T. ) ;
#12177 = CARTESIAN_POINT ( 'NONE',  ( 8.592629440379999650, -3.856773448568000084, 5.521258396339000285 ) ) ;
#12178 = CARTESIAN_POINT ( 'NONE',  ( 9.531727112333999941, -4.010297355695000121, -9.208122400763999238 ) ) ;
#12179 = CARTESIAN_POINT ( 'NONE',  ( 18.01397738364135392, 2.075598766708242060, 13.75431519107023526 ) ) ;
#12180 = CARTESIAN_POINT ( 'NONE',  ( 23.60205915885299888, -2.338900754078999444, 12.00073634674999212 ) ) ;
#12181 = CARTESIAN_POINT ( 'NONE',  ( 11.47810404293059960, -4.563346034752700398, -8.647151967355000579 ) ) ;
#12182 = VERTEX_POINT ( 'NONE', #63033 ) ;
#12183 = CARTESIAN_POINT ( 'NONE',  ( 24.30001697071400457, -8.938702858184001343, 8.938676113071998941 ) ) ;
#12184 = CARTESIAN_POINT ( 'NONE',  ( 9.234510841229999656, 5.964723767581000757, 7.776480083716999836 ) ) ;
#12185 = EDGE_CURVE ( 'NONE', #4475, #55227, #62699, .T. ) ;
#12187 = CARTESIAN_POINT ( 'NONE',  ( 11.46989666366029859, 3.941571897678119996, 6.185029684353999357 ) ) ;
#12186 = CARTESIAN_POINT ( 'NONE',  ( 9.392285841233000809, 5.775964236216999836, -8.174909295649001706 ) ) ;
#12188 = CARTESIAN_POINT ( 'NONE',  ( 10.71093936450548156, 3.092590697381819798, 4.810214324148986087 ) ) ;
#12189 = EDGE_LOOP ( 'NONE', ( #7887, #32701, #55199, #22501 ) ) ;
#12190 = CARTESIAN_POINT ( 'NONE',  ( 10.94796973825000030, 2.864322365205000054, 8.846249469408000721 ) ) ;
#12192 = CARTESIAN_POINT ( 'NONE',  ( 18.10325613414707746, -2.040025360435032464, -13.85057320474804854 ) ) ;
#12191 = VECTOR ( 'NONE', #16719, 1000.000000000000000 ) ;
#12193 = CARTESIAN_POINT ( 'NONE',  ( 10.89564560330029863, 4.307504762655200103, 8.455191956516999952 ) ) ;
#12194 = CARTESIAN_POINT ( 'NONE',  ( 10.07771285905000092, -4.622037501707999319, 5.671359981946999973 ) ) ;
#12195 = CARTESIAN_POINT ( 'NONE',  ( 7.656866975822993915, 3.528150633380001899, 6.493493947281997691 ) ) ;
#12196 = EDGE_LOOP ( 'NONE', ( #65186, #56702, #63964, #42047 ) ) ;
#12197 = CARTESIAN_POINT ( 'NONE',  ( 24.50399615158200106, 12.34862307823000016, -3.085465605547000223 ) ) ;
#12199 = CARTESIAN_POINT ( 'NONE',  ( 10.86460564679000029, -3.843601288168000174, -5.985268170611000471 ) ) ;
#12198 = CARTESIAN_POINT ( 'NONE',  ( 12.40355051044899959, -11.78614875273999907, 3.442261952866000119 ) ) ;
#12200 = CARTESIAN_POINT ( 'NONE',  ( 7.732099726745981449, -5.601557586365069952, 8.181612574483722256 ) ) ;
#12201 = CARTESIAN_POINT ( 'NONE',  ( 9.318721994369999706, -2.755032632138999737, 8.795122807847999269 ) ) ;
#12202 = FACE_OUTER_BOUND ( 'NONE', #22794, .T. ) ;
#12203 = CARTESIAN_POINT ( 'NONE',  ( 10.15797570133299921, -3.162316589966200020, 6.724099908144899551 ) ) ;
#12204 = ORIENTED_EDGE ( 'NONE', *, *, #45645, .T. ) ;
#12205 = CARTESIAN_POINT ( 'NONE',  ( 23.91319624006256461, -9.510189266786756690, 9.347864195410048538 ) ) ;
#12206 = CARTESIAN_POINT ( 'NONE',  ( 12.00271932425157040, -4.187398418774900044, 6.235801371442999397 ) ) ;
#12207 = ORIENTED_EDGE ( 'NONE', *, *, #33620, .T. ) ;
#12208 = CARTESIAN_POINT ( 'NONE',  ( 8.221179504219003675, 3.443168248977001245, 6.131664885159996636 ) ) ;
#12209 = VERTEX_POINT ( 'NONE', #67949 ) ;
#12210 = B_SPLINE_SURFACE_WITH_KNOTS ( 'NONE', 3, 3, ( 
 ( #37914, #54687, #58899, #59581, #21486, #16242, #43515, #11682, #49095, #17640, #38964, #27785, #64127, #37565, #1207, #60281, #43858, #6785, #59928, #49791, #33720, #21828, #64813, #42819, #11002, #17281, #43160, #1547, #12386, #55037, #38607, #59234, #33372, #11336, #32678 ),
 ( #6093, #7138, #12039, #65159, #48753, #858, #22175, #33022, #54334, #28123, #6436, #45244, #39302, #8176, #40001, #19349, #2580, #12736, #62002, #61314, #13770, #23908, #13085, #13435, #35103, #66894, #56765, #40671, #2923, #14115, #35439, #55732, #7834, #3270, #1900 ),
 ( #29525, #29170, #8862, #34416, #61656, #51174, #7476, #29866, #56415, #50142, #50478, #23221, #66551, #60972, #50827, #18669, #30200, #8518, #23560, #24601, #45921, #34756, #44568, #24251, #45589, #56066, #19006, #40333, #67233, #65860, #17983, #60625, #34066, #55382, #28831 ),
 ( #2247, #44901, #66204, #18326, #39649, #15138, #46957, #20725, #47302, #68606, #42053, #36459, #62342, #20381, #4634, #58469, #41708, #62677, #21070, #42401, #63359, #10232, #3945, #15821, #68957, #19700, #25973, #63709, #52886, #57778, #14459, #9889, #51505, #68260, #67575 ) ),
 .UNSPECIFIED., .F., .F., .F.,
 ( 4, 4 ),
 ( 4, 1, 1, 1, 1, 1, 1, 1, 1, 1, 1, 1, 1, 1, 1, 1, 1, 1, 1, 1, 1, 1, 1, 1, 1, 1, 1, 1, 1, 1, 1, 1, 4 ),
 ( -0.1039370721279000015, 1.103937072127999963 ),
 ( -0.02000000000000000042, 0.01250000000000000069, 0.04499999999999999833, 0.07749999999999999944, 0.1100000000000000006, 0.1424999999999999878, 0.1749999999999999889, 0.2074999999999999900, 0.2399999999999999911, 0.2725000000000000200, 0.3049999999999999933, 0.3375000000000000222, 0.3699999999999999956, 0.4025000000000000244, 0.4349999999999999978, 0.4675000000000000266, 0.5000000000000000000, 0.5324999999999999734, 0.5649999999999999467, 0.5975000000000000311, 0.6300000000000000044, 0.6624999999999999778, 0.6949999999999999512, 0.7275000000000000355, 0.7600000000000000089, 0.7924999999999999822, 0.8249999999999999556, 0.8575000000000000400, 0.8900000000000000133, 0.9224999999999999867, 0.9549999999999999600, 0.9875000000000000444, 1.020000000000000018 ),
 .UNSPECIFIED. ) ;
#12211 = CARTESIAN_POINT ( 'NONE',  ( 8.863029719594999634, 2.990001567622999623, -8.695425648791999862 ) ) ;
#12212 = CARTESIAN_POINT ( 'NONE',  ( 23.64843174477000076, 13.35727533436999792, -3.864837375578999978 ) ) ;
#12213 = CARTESIAN_POINT ( 'NONE',  ( 12.13935791461255675, 2.765884558748026301, -12.29268093925658434 ) ) ;
#12214 = CARTESIAN_POINT ( 'NONE',  ( 11.98011496860029901, -3.080230834057799960, 7.971338736265699332 ) ) ;
#12215 = DIRECTION ( 'NONE',  ( 0.000000000000000000, -0.8648648648648720183, -0.5020047465136825426 ) ) ;
#12216 = DIRECTION ( 'NONE',  ( 0.000000000000000000, 0.1807154286440004198, 0.9835354258236025382 ) ) ;
#12218 = EDGE_LOOP ( 'NONE', ( #21708, #38159, #51344, #60225, #30055, #36340 ) ) ;
#12217 = B_SPLINE_CURVE_WITH_KNOTS ( 'NONE', 3,
 ( #35235, #46751, #24391, #68056, #24734, #46061 ),
 .UNSPECIFIED., .F., .F.,
 ( 4, 2, 4 ),
 ( 0.000000000000000000, 0.5000000000000004441, 1.000000000000000000 ),
 .UNSPECIFIED. ) ;
#12219 = DIRECTION ( 'NONE',  ( -1.000000000000000000, 0.000000000000000000, 0.000000000000000000 ) ) ;
#12220 = DIRECTION ( 'NONE',  ( 0.7071067388045961799, 0.7071068235684964121, -1.176037761303994353E-10 ) ) ;
#12221 = EDGE_LOOP ( 'NONE', ( #46801, #27514, #18755, #4206, #8894, #33158, #45747, #49226, #766, #19830 ) ) ;
#12222 = B_SPLINE_SURFACE_WITH_KNOTS ( 'NONE', 3, 3, ( 
 ( #46399, #56541, #51295, #29653 ),
 ( #3391, #56199, #66680, #51634 ),
 ( #62124, #28962, #45373, #8645 ),
 ( #8984, #19827, #40455, #45028 ),
 ( #14243, #18803, #41158, #50267 ),
 ( #2370, #67358, #56887, #19132 ) ),
 .UNSPECIFIED., .F., .F., .F.,
 ( 4, 1, 1, 4 ),
 ( 4, 4 ),
 ( 0.1423941366080999915, 0.3333333333333000081, 0.6666666666667000474, 0.8219462302419999755 ),
 ( -0.1256563615234000120, 1.125656361508000192 ),
 .UNSPECIFIED. ) ;
#12223 = CARTESIAN_POINT ( 'NONE',  ( 10.15102996164048932, -2.740893273674518849, -6.282207469075709483 ) ) ;
#12224 = CARTESIAN_POINT ( 'NONE',  ( 10.30487885159599770, 4.996404279947399552, 7.618867373350600047 ) ) ;
#12225 = CARTESIAN_POINT ( 'NONE',  ( 10.15335805961999860, -3.144986649008000068, -5.860958514434000399 ) ) ;
#12226 = CARTESIAN_POINT ( 'NONE',  ( 11.13711610230999938, 2.663427511852999974, -5.178750069089000263 ) ) ;
#12227 = FACE_OUTER_BOUND ( 'NONE', #31742, .T. ) ;
#12228 = ADVANCED_FACE ( 'NONE', ( #52560 ), #51870, .F. ) ;
#12229 = CARTESIAN_POINT ( 'NONE',  ( 11.02445830383999947, -3.404091099119999519, 5.822494319281999786 ) ) ;
#12230 = CARTESIAN_POINT ( 'NONE',  ( 12.72201428491567121, -3.119809216722634115, -13.52222099568139413 ) ) ;
#12231 = ADVANCED_FACE ( 'NONE', ( #51531 ), #40695, .T. ) ;
#12232 = CARTESIAN_POINT ( 'NONE',  ( 18.14710087547455331, -0.2005123242923291527, -12.69787478206145259 ) ) ;
#12233 = CARTESIAN_POINT ( 'NONE',  ( 0.000000000000000000, -5.100000000000000533, 7.500000000000000000 ) ) ;
#12234 = CARTESIAN_POINT ( 'NONE',  ( 11.45348876160960039, -4.885820101980599794, -8.421216112044099589 ) ) ;
#12235 = EDGE_CURVE ( 'NONE', #33712, #39743, #13533, .T. ) ;
#12236 = EDGE_CURVE ( 'NONE', #14587, #13866, #51945, .T. ) ;
#12237 = CARTESIAN_POINT ( 'NONE',  ( 8.379704719592000473, 4.283000592898000392, 9.286795422009001655 ) ) ;
#12238 = ORIENTED_EDGE ( 'NONE', *, *, #22304, .F. ) ;
#12239 = CARTESIAN_POINT ( 'NONE',  ( 10.71685100253999856, 2.832432432432000269, 6.822293592207000934 ) ) ;
#12240 = CARTESIAN_POINT ( 'NONE',  ( 5.399999746777999654, -13.10000000000000142, 0.000000000000000000 ) ) ;
#12241 = CARTESIAN_POINT ( 'NONE',  ( 7.866682853741001402, 2.870179227930000021, -6.741414558537999646 ) ) ;
#12242 = CARTESIAN_POINT ( 'NONE',  ( 10.40878363256000050, 3.093886843363999883, -6.480781753756000185 ) ) ;
#12243 = CARTESIAN_POINT ( 'NONE',  ( 18.06564745257664129, 2.991132176950368482, 12.23981809347030847 ) ) ;
#12244 = CARTESIAN_POINT ( 'NONE',  ( 18.44496314779700086, 2.860815007322000447, -12.13831535021000008 ) ) ;
#12245 = CARTESIAN_POINT ( 'NONE',  ( 9.843732751558000871, 4.115124343450999866, 9.466620196856998959 ) ) ;
#12246 = CARTESIAN_POINT ( 'NONE',  ( 10.13216648677562759, -4.862862160676565182, 7.355082228165340297 ) ) ;
#12247 = FACE_OUTER_BOUND ( 'NONE', #64405, .T. ) ;
#12248 = ORIENTED_EDGE ( 'NONE', *, *, #30483, .F. ) ;
#12249 = CARTESIAN_POINT ( 'NONE',  ( 12.10442723766657025, -2.667336250084669125, 12.31445622895738978 ) ) ;
#12250 = CARTESIAN_POINT ( 'NONE',  ( 9.429063610504998749, -3.531653260805799999, -8.541338455964998744 ) ) ;
#12251 = FACE_OUTER_BOUND ( 'NONE', #42973, .T. ) ;
#12252 = DIRECTION ( 'NONE',  ( -1.000000000000000000, 0.000000000000000000, 0.000000000000000000 ) ) ;
#12253 = CARTESIAN_POINT ( 'NONE',  ( 10.28026357027499849, 4.985299147223100746, -7.690095141806899903 ) ) ;
#12254 = VERTEX_POINT ( 'NONE', #52911 ) ;
#12255 = CARTESIAN_POINT ( 'NONE',  ( 12.15201606283211788, -0.3124912280145362153, 12.59612551846059780 ) ) ;
#12256 = CARTESIAN_POINT ( 'NONE',  ( 8.753448341231001351, 2.876288091423999660, 6.568897128359000526 ) ) ;
#12257 = CARTESIAN_POINT ( 'NONE',  ( 10.65050915380999896, 5.200037120669999346, 5.937706951697999891 ) ) ;
#12258 = CARTESIAN_POINT ( 'NONE',  ( 12.43906710990142628, 3.006741445058540574, 12.31893827218670445 ) ) ;
#12259 = VERTEX_POINT ( 'NONE', #56790 ) ;
#12260 = CARTESIAN_POINT ( 'NONE',  ( 9.842764158772000727, 5.798263352390999437, -8.113145944980999502 ) ) ;
#12261 = CARTESIAN_POINT ( 'NONE',  ( 10.71503032197929883, 4.743378537856500543, -6.460430507351999196 ) ) ;
#12262 = CARTESIAN_POINT ( 'NONE',  ( 8.541480666858999982, 4.426512626096299918, -8.706015266875999359 ) ) ;
#12264 = CARTESIAN_POINT ( 'NONE',  ( 18.02801395638694260, -0.4085932595162927727, 12.69115266611978043 ) ) ;
#12263 = CARTESIAN_POINT ( 'NONE',  ( 7.690241772926001751, 4.592291064388997590, 6.438923047733998928 ) ) ;
#12265 = CARTESIAN_POINT ( 'NONE',  ( 9.478113844317999082, -3.781046324972699768, 8.338908357746399602 ) ) ;
#12266 = AXIS2_PLACEMENT_3D ( 'NONE', #58631, #5832, #27170 ) ;
#12267 = CARTESIAN_POINT ( 'NONE',  ( 10.89979975933730039, -3.180925410802600162, -7.218192605361100078 ) ) ;
#12268 = LINE ( 'NONE', #27311, #1764 ) ;
#12269 = ORIENTED_EDGE ( 'NONE', *, *, #26043, .F. ) ;
#12270 = B_SPLINE_CURVE_WITH_KNOTS ( 'NONE', 3,
 ( #65490, #39281, #33000, #1527 ),
 .UNSPECIFIED., .F., .F.,
 ( 4, 4 ),
 ( 0.000000000000000000, 1.000000000000000000 ),
 .UNSPECIFIED. ) ;
#12271 = CARTESIAN_POINT ( 'NONE',  ( 1.305473797069999886, 3.048238319583999711, -1.563029678068999839 ) ) ;
#12272 = CARTESIAN_POINT ( 'NONE',  ( 7.000000000000000000, 0.5415384615382000666, 2.132307692307999769 ) ) ;
#12273 = EDGE_CURVE ( 'NONE', #31943, #63357, #58638, .T. ) ;
#12274 = DIRECTION ( 'NONE',  ( 0.000000000000000000, 0.000000000000000000, 1.000000000000000000 ) ) ;
#12275 = CARTESIAN_POINT ( 'NONE',  ( 9.171747021775997766, 3.348327362764200288, 6.928134003122899287 ) ) ;
#12276 = CARTESIAN_POINT ( 'NONE',  ( 10.56577346846700038, 5.100000000000000533, 6.304440313576233024 ) ) ;
#12277 = EDGE_CURVE ( 'NONE', #2331, #53988, #42422, .T. ) ;
#12278 = CARTESIAN_POINT ( 'NONE',  ( 12.50306195774383333, -1.853743832531306701, 13.87673314481786058 ) ) ;
#12279 = CARTESIAN_POINT ( 'NONE',  ( 11.13509627278000025, 2.662095878336999899, 5.086083211022000228 ) ) ;
#12280 = CARTESIAN_POINT ( 'NONE',  ( 24.25968945202800242, 3.166454503780999907, -12.13789061559999993 ) ) ;
#12281 = CARTESIAN_POINT ( 'NONE',  ( 12.99284288850700086, -12.22216846288000092, -1.954503247608000205 ) ) ;
#12282 = VERTEX_POINT ( 'NONE', #27034 ) ;
#12283 = CARTESIAN_POINT ( 'NONE',  ( 7.437916666664375676, 3.170361928033863297, -6.420449762762457269 ) ) ;
#12284 = CARTESIAN_POINT ( 'NONE',  ( 6.899999438051000133, 1.266765207443000030, 0.8033093483900000109 ) ) ;
#12285 = CARTESIAN_POINT ( 'NONE',  ( 8.590472024761092840, 4.653241489312755164, 5.916299078424504643 ) ) ;
#12286 = LINE ( 'NONE', #65050, #27980 ) ;
#12287 = CARTESIAN_POINT ( 'NONE',  ( 0.6990182015430999041, 1.892658550137999995, 3.053125390820000007 ) ) ;
#12288 = DIRECTION ( 'NONE',  ( 0.000000000000000000, 0.000000000000000000, 1.000000000000000000 ) ) ;
#12289 = CARTESIAN_POINT ( 'NONE',  ( 17.84375123822102438, 1.945578272181329504, -12.56362807389522374 ) ) ;
#12290 = CARTESIAN_POINT ( 'NONE',  ( 9.696006702408610067, -3.000394487162608925, 8.268211173249310875 ) ) ;
#12291 = CARTESIAN_POINT ( 'NONE',  ( 11.85159063708299954, 4.825025306051200502, 7.268038553423699533 ) ) ;
#12292 = CARTESIAN_POINT ( 'NONE',  ( 15.83777337640987781, 9.021763928136897093, 8.400065602738665760 ) ) ;
#12293 = CARTESIAN_POINT ( 'NONE',  ( 10.59956814679000026, -4.438148200474000937, -8.958389257466000899 ) ) ;
#12294 = CARTESIAN_POINT ( 'NONE',  ( 17.78891907839554420, -0.6928235585744062508, -13.98285841810580443 ) ) ;
#12295 = LINE ( 'NONE', #23121, #26564 ) ;
#12296 = CARTESIAN_POINT ( 'NONE',  ( 12.76376210869972105, -3.125000000000000444, 12.28374662615010671 ) ) ;
#12297 = EDGE_LOOP ( 'NONE', ( #48229, #59762, #60515, #6361, #31195 ) ) ;
#12298 = CARTESIAN_POINT ( 'NONE',  ( 11.09999999999999964, -5.299316147296000423, 5.124965750789000296 ) ) ;
#12299 = EDGE_LOOP ( 'NONE', ( #15496, #10987, #67445, #66971, #39826 ) ) ;
#12300 = CARTESIAN_POINT ( 'NONE',  ( 18.11136953712603059, -2.785023373216928277, 13.60886753798840765 ) ) ;
#12301 = DIRECTION ( 'NONE',  ( 0.7071058810607747658, -0.7071076813111745185, 3.975037112901852268E-09 ) ) ;
#12302 = ORIENTED_EDGE ( 'NONE', *, *, #25080, .F. ) ;
#12303 = CARTESIAN_POINT ( 'NONE',  ( 11.27745123989519982, 4.410212499603100689, 6.707778874960499849 ) ) ;
#12304 = CARTESIAN_POINT ( 'NONE',  ( 5.922234340208202497, -0.4543021360680231102, -1.037812024122457544 ) ) ;
#12305 = CARTESIAN_POINT ( 'NONE',  ( 9.113217775048997993, -8.654438058834999836, 6.112263052845000821 ) ) ;
#12306 = CYLINDRICAL_SURFACE ( 'NONE', #56611, 1.350000000000000089 ) ;
#12307 = CARTESIAN_POINT ( 'NONE',  ( 12.56925896339910764, -1.825837054118446323, -13.88044190432301406 ) ) ;
#12308 = CARTESIAN_POINT ( 'NONE',  ( 10.68559687351583420, -2.907767014557174790, 8.129523725463618788 ) ) ;
#12309 = CARTESIAN_POINT ( 'NONE',  ( 11.74274107869599959, 3.315287298500999569, -11.22371330986000082 ) ) ;
#12310 = CARTESIAN_POINT ( 'NONE',  ( 10.95551720753999980, -4.744041807741999683, -9.198129812222999746 ) ) ;
#12311 = CARTESIAN_POINT ( 'NONE',  ( 13.49994651945300284, -12.07042783918999795, -2.492331243371999960 ) ) ;
#12312 = ADVANCED_FACE ( 'NONE', ( #28069, #64069 ), #6379, .F. ) ;
#12313 = EDGE_CURVE ( 'NONE', #56577, #39090, #61071, .T. ) ;
#12314 = CARTESIAN_POINT ( 'NONE',  ( 5.000000000000000000, 0.05000000000000000278, -9.776630298829998011 ) ) ;
#12315 = ORIENTED_EDGE ( 'NONE', *, *, #33538, .T. ) ;
#12316 = CONICAL_SURFACE ( 'NONE', #64742, 11.74991359182999950, 0.7853990805437361944 ) ;
#12317 = CARTESIAN_POINT ( 'NONE',  ( 8.936337454063531638, 3.131903168333550536, -6.831783586538417552 ) ) ;
#12318 = VERTEX_POINT ( 'NONE', #29117 ) ;
#12319 = DIRECTION ( 'NONE',  ( 0.000000000000000000, -0.7916053084224905501, -0.6110327615417471270 ) ) ;
#12320 = CARTESIAN_POINT ( 'NONE',  ( 10.70976172572000173, -5.125515269697999976, 5.002993350055000121 ) ) ;
#12321 = CARTESIAN_POINT ( 'NONE',  ( 10.61517041231343761, -2.962049961264340947, 5.046074788812947354 ) ) ;
#12322 = CARTESIAN_POINT ( 'NONE',  ( 23.59999462723899910, 13.22316330987000121, -4.267799687262000319 ) ) ;
#12323 = CARTESIAN_POINT ( 'NONE',  ( 12.21968270649327870, 2.719953125373911096, 13.62430835208223101 ) ) ;
#12324 = CARTESIAN_POINT ( 'NONE',  ( 10.87148543990999983, -5.567571293949000300, 7.772413914480000408 ) ) ;
#12325 = ORIENTED_EDGE ( 'NONE', *, *, #1674, .F. ) ;
#12326 = CARTESIAN_POINT ( 'NONE',  ( 10.01293113571299997, 5.100000000000000533, 6.444141223344916014 ) ) ;
#12327 = CARTESIAN_POINT ( 'NONE',  ( 12.15456646199064217, 0.3226776716457197547, 13.99628514671256241 ) ) ;
#12328 = ORIENTED_EDGE ( 'NONE', *, *, #45011, .F. ) ;
#12329 = CARTESIAN_POINT ( 'NONE',  ( 7.184909439180999335, 5.017953588770000195, -6.429833855306000601 ) ) ;
#12330 = CARTESIAN_POINT ( 'NONE',  ( 17.60750054167100132, 12.16746880438999945, -3.133263442192999904 ) ) ;
#12331 = ADVANCED_FACE ( 'NONE', ( #34704 ), #35, .F. ) ;
#12332 = CARTESIAN_POINT ( 'NONE',  ( 9.049596101582626062, 3.436622489763541122, 8.169431139013614285 ) ) ;
#12333 = CARTESIAN_POINT ( 'NONE',  ( 5.088708767848000747, 1.186311595762999938, 0.04099492891103999337 ) ) ;
#12334 = CARTESIAN_POINT ( 'NONE',  ( 9.974220280410998285, 5.496789211521000418, -7.043125396300999874 ) ) ;
#12335 = DIRECTION ( 'NONE',  ( 1.000000000000000000, 0.000000000000000000, 0.000000000000000000 ) ) ;
#12336 = CARTESIAN_POINT ( 'NONE',  ( 10.00074484908000194, -2.373896846742000299, -7.962434077545999855 ) ) ;
#12337 = DIRECTION ( 'NONE',  ( 1.000000000000000000, 0.000000000000000000, 0.000000000000000000 ) ) ;
#12338 = CARTESIAN_POINT ( 'NONE',  ( 11.08757144985999865, -2.712428550139000194, 6.571291218949999902 ) ) ;
#12339 =( NAMED_UNIT ( * ) PLANE_ANGLE_UNIT ( ) SI_UNIT ( $, .RADIAN. ) );
#12340 = CARTESIAN_POINT ( 'NONE',  ( 9.746744136172999617, -5.062748727288000516, -8.618689820632001286 ) ) ;
#12341 = DIRECTION ( 'NONE',  ( 0.000000000000000000, 1.000000000000000000, 0.000000000000000000 ) ) ;
#12342 = DIRECTION ( 'NONE',  ( -1.000000000000000000, 0.000000000000000000, 0.000000000000000000 ) ) ;
#12343 = CARTESIAN_POINT ( 'NONE',  ( 10.93479632507519916, 4.557787252275099732, -8.534037301706000278 ) ) ;
#12344 = CARTESIAN_POINT ( 'NONE',  ( 10.09058376188599837, 3.152987476450699766, -8.039825975318500184 ) ) ;
#12346 = CARTESIAN_POINT ( 'NONE',  ( 10.90000000000000036, -8.618205959414002137, -7.308661029293999967 ) ) ;
#12345 = CARTESIAN_POINT ( 'NONE',  ( 9.874380199233998567, -3.139757597894699881, 7.608124715612800237 ) ) ;
#12347 = FACE_OUTER_BOUND ( 'NONE', #31139, .T. ) ;
#12348 = VERTEX_POINT ( 'NONE', #3551 ) ;
#12349 = VECTOR ( 'NONE', #53513, 1000.000000000000000 ) ;
#12350 = CARTESIAN_POINT ( 'NONE',  ( 11.10101463001529964, 4.622233839778099984, 8.496586578655598743 ) ) ;
#12351 = CARTESIAN_POINT ( 'NONE',  ( 10.21608469020999976, -5.961703525007000515, 7.319668113368000384 ) ) ;
#12352 = CARTESIAN_POINT ( 'NONE',  ( 9.884988259786998910, 3.850604015305000072, 6.368003848175999515 ) ) ;
#12353 = CARTESIAN_POINT ( 'NONE',  ( 9.834799664234624927, 4.795722374051563541, -7.863810627050381363 ) ) ;
#12354 = CARTESIAN_POINT ( 'NONE',  ( 9.848732933287999813, -2.769734897491000325, 6.441850735262000249 ) ) ;
#12355 = EDGE_CURVE ( 'NONE', #2906, #40590, #12652, .T. ) ;
#12356 = CARTESIAN_POINT ( 'NONE',  ( 11.10000000009000054, -5.300000000088999741, -6.571291220400000022 ) ) ;
#12357 = CARTESIAN_POINT ( 'NONE',  ( 10.53976354018315753, 4.327184855449099921, 6.282534154164603812 ) ) ;
#12358 = ORIENTED_EDGE ( 'NONE', *, *, #18673, .F. ) ;
#12359 = APPLICATION_CONTEXT ( 'automotive_design' ) ;
#12360 = CONICAL_SURFACE ( 'NONE', #51439, 0.8999999994071996579, 0.7853981633972997312 ) ;
#12361 = CARTESIAN_POINT ( 'NONE',  ( 8.722809814040999754, -3.385590752329799891, -8.294571108394100278 ) ) ;
#12362 = CARTESIAN_POINT ( 'NONE',  ( 9.604346873516666605, -2.749999999999998224, -7.336375382625535124 ) ) ;
#12363 = DIRECTION ( 'NONE',  ( 0.000000000000000000, 0.8304044637635152881, -0.5571610418556101063 ) ) ;
#12364 = B_SPLINE_SURFACE_WITH_KNOTS ( 'NONE', 3, 3, ( 
 ( #22132, #64770, #16884, #38211, #6391, #49054, #40625, #24204, #8477, #2535, #61957, #56721, #34024, #23863, #2881, #35395, #13040, #8816, #55337, #56024, #14071, #30160, #1853, #45547, #60582, #8131, #3229, #23171, #44520, #35055, #66852, #65813, #7786, #50432, #17938, #29821, #23515, #61610, #18966, #34370, #66164, #39257, #24556, #61273, #45879, #40292, #13726, #39956, #56373, #45200, #66505, #18283, #12687, #7433, #28784, #51126, #29126, #67189, #19301, #50095, #2204, #39602, #50786, #44857, #60928, #55689, #18627 ),
 ( #13390, #34712, #29477, #57052, #67532, #51802, #35734, #57730, #68559, #9151, #3560, #3900, #42360, #25235, #15440, #4245, #63661, #63312, #4936, #14753, #46569, #62964, #26276, #62299, #20680, #30489, #10189, #41661, #36765, #20332, #67878, #21026, #37107, #58422, #52491, #40975, #9841, #52841, #10527, #24895, #58086, #25925, #46224, #57386, #30832, #51463, #31519, #19998, #42011, #47255, #36070, #41322, #19654, #47601, #15092, #68909, #4588, #15777, #36416, #14417, #52142, #25584, #62628, #9490, #46911, #68214, #31186 ),
 ( #1080, #37445, #43, #53185, #21363, #11904, #65030, #21700, #16798, #11216, #54205, #5623, #27653, #38126, #58766, #47943, #32217, #16119, #59453, #48974, #10873, #5282, #53531, #22737, #26964, #17147, #53865, #44086, #43732, #54563, #64340, #48278, #43390, #6660, #42693, #22395, #384, #59802, #22043, #38479, #731, #43036, #16457, #64001, #37789, #6306, #59110, #33242, #60157, #28001, #64690, #49310, #65385, #38829, #1422, #11551, #17506, #32552, #31867, #26624, #5966, #27304, #48628, #32894, #2456, #13312, #40215 ),
 ( #29046, #60845, #45460, #56291, #7707, #33590, #2799, #66077, #65733, #7010, #55605, #29740, #49661, #29392, #13646, #28342, #34973, #55256, #61532, #45117, #39174, #7352, #23781, #17856, #54907, #34284, #50356, #8395, #51043, #19219, #3144, #50702, #24125, #66772, #28697, #66424, #24473, #8049, #12261, #12957, #50011, #18890, #18545, #39872, #61191, #18198, #33937, #34634, #12606, #67110, #45797, #1770, #40545, #2121, #60497, #23438, #23088, #44436, #44777, #39520, #55946, #68474, #62550, #52755, #47517, #24816, #14673 ) ),
 .UNSPECIFIED., .F., .F., .F.,
 ( 4, 4 ),
 ( 4, 1, 1, 1, 1, 1, 1, 1, 1, 1, 1, 1, 1, 1, 1, 1, 1, 1, 1, 1, 1, 1, 1, 1, 1, 1, 1, 1, 1, 1, 1, 1, 1, 1, 1, 1, 1, 1, 1, 1, 1, 1, 1, 1, 1, 1, 1, 1, 1, 1, 1, 1, 1, 1, 1, 1, 1, 1, 1, 1, 1, 1, 1, 1, 4 ),
 ( -0.02000000000000000042, 1.020000000000000018 ),
 ( 0.008747244164287000176, 0.02453926110774999961, 0.04033127805120999970, 0.05612329499467000327, 0.07191531193812999989, 0.08770732888158999652, 0.1034993458251000087, 0.1192913627684999978, 0.1350833797120000179, 0.1508753966553999792, 0.1666674135988999994, 0.1824594305423999918, 0.1982514474858000086, 0.2140434644293000011, 0.2298354813727000179, 0.2456274983162000103, 0.2614195152596999749, 0.2772115322030999640, 0.2930035491465999842, 0.3087955660900000288, 0.3245875830334999934, 0.3403795999769999581, 0.3561716169204000026, 0.3719636338639000228, 0.3877556508073999875, 0.4035476677507999765, 0.4193396846942999967, 0.4351317016376999858, 0.4509237185811999504, 0.4667157355247000261, 0.4825077524681000152, 0.4982997694115999798, 0.5140917863550000799, 0.5298838032985000446, 0.5456758202420000092, 0.5614678371854000538, 0.5772598541289000185, 0.5930518710723000630, 0.6088438880158000277, 0.6246359049592999924, 0.6404279219027000369, 0.6562199388462000016, 0.6720119557896999662, 0.6878039727331000108, 0.7035959896765999755, 0.7193880066200000201, 0.7351800235634999847, 0.7509720405069999494, 0.7667640574504001050, 0.7825560743939000696, 0.7983480913373000032, 0.8141401082808000789, 0.8299321252243000435, 0.8457241421676999771, 0.8615161591112000528, 0.8773081760545999863, 0.8931001929981000620, 0.9088922099416000266, 0.9246842268849999602, 0.9404762438285000359, 0.9562682607720000005, 0.9720602777153999341, 0.9878522946589000098, 1.003644311601999961, 1.019436328545999970 ),
 .UNSPECIFIED. ) ;
#12365 = CARTESIAN_POINT ( 'NONE',  ( 6.899999691988000450, 12.20988339176000004, 3.111064831550000243 ) ) ;
#12366 = CARTESIAN_POINT ( 'NONE',  ( 24.35145719007200071, -3.377064811435000369, 12.26055847765000095 ) ) ;
#12367 = CARTESIAN_POINT ( 'NONE',  ( 11.94133594839949986, -3.430493414882899827, 8.152656755002400502 ) ) ;
#12368 = CARTESIAN_POINT ( 'NONE',  ( 10.35826357027499789, 4.850513154668600002, -7.664090691848299386 ) ) ;
#12369 = CARTESIAN_POINT ( 'NONE',  ( 12.19329716805284036, 2.371658047258630830, -13.69984404026345004 ) ) ;
#12370 = CARTESIAN_POINT ( 'NONE',  ( 25.37703487173499894, -8.494994160653000392, 7.921071945508999512 ) ) ;
#12371 = DIRECTION ( 'NONE',  ( 1.000000000000000000, 0.000000000000000000, 0.000000000000000000 ) ) ;
#12372 = EDGE_LOOP ( 'NONE', ( #1647, #54672, #440, #55697 ) ) ;
#12373 = CARTESIAN_POINT ( 'NONE',  ( 0.000000000000000000, -1.460905701137619417, -2.533699434756940594 ) ) ;
#12374 = CARTESIAN_POINT ( 'NONE',  ( 12.50529577747503929, -0.6653129401483898198, -13.98418548573915743 ) ) ;
#12375 = CARTESIAN_POINT ( 'NONE',  ( 17.55505043854147118, -1.875000000000000000, 13.78631952119024895 ) ) ;
#12376 = CARTESIAN_POINT ( 'NONE',  ( 7.100000000000000533, -13.94845324556000143, 4.312847325879000770 ) ) ;
#12377 = CARTESIAN_POINT ( 'NONE',  ( 4.900006121741999898, 1.747572776708514519, -1.007237960741801386 ) ) ;
#12378 = CARTESIAN_POINT ( 'NONE',  ( 6.999999999999999112, 9.962435980213809827, 4.520115016280596976 ) ) ;
#12379 = CARTESIAN_POINT ( 'NONE',  ( 5.641095281750911461, 12.09393047400991783, -3.739612655151742793 ) ) ;
#12380 = VERTEX_POINT ( 'NONE', #4580 ) ;
#12381 = CARTESIAN_POINT ( 'NONE',  ( 24.35365242081700288, 8.326148686889998984, 7.789520173161003314 ) ) ;
#12382 = CARTESIAN_POINT ( 'NONE',  ( 17.74765434492527660, 1.905326452124538550, -13.78174529102851231 ) ) ;
#12383 = ORIENTED_EDGE ( 'NONE', *, *, #43570, .F. ) ;
#12384 = CARTESIAN_POINT ( 'NONE',  ( 8.576923877145999242, 3.399999999999999911, 5.924121105096999962 ) ) ;
#12385 = CARTESIAN_POINT ( 'NONE',  ( 9.187745559622999991, -5.964711531933999389, 7.776478361891000723 ) ) ;
#12386 = CARTESIAN_POINT ( 'NONE',  ( 8.374639158773000247, 2.721111233225000259, -6.936528696292000085 ) ) ;
#12387 = CARTESIAN_POINT ( 'NONE',  ( 11.10000000000000142, -2.264799782219416802, -7.479379319469428467 ) ) ;
#12388 = CARTESIAN_POINT ( 'NONE',  ( 10.92968717260509948, -4.687649763627899979, -8.622362941748999532 ) ) ;
#12389 = CARTESIAN_POINT ( 'NONE',  ( 9.258050732556000639, -4.895927245463000510, -6.008721945297999412 ) ) ;
#12390 = AXIS2_PLACEMENT_3D ( 'NONE', #21027, #8306, #13220 ) ;
#12391 = CARTESIAN_POINT ( 'NONE',  ( 10.94166666666863996, -5.229667600279077178, 8.191470186739737258 ) ) ;
#12392 = ORIENTED_EDGE ( 'NONE', *, *, #37275, .T. ) ;
#12393 = FACE_OUTER_BOUND ( 'NONE', #22356, .T. ) ;
#12394 = ADVANCED_FACE ( 'NONE', ( #25577 ), #67523, .F. ) ;
#12395 = ADVANCED_FACE ( 'NONE', ( #41312 ), #24546, .T. ) ;
#12396 = CARTESIAN_POINT ( 'NONE',  ( 18.12992444764572042, -2.745380825951750037, -13.61829546699563664 ) ) ;
#12397 = CARTESIAN_POINT ( 'NONE',  ( 6.800000000000000711, 5.221516520829000640, -8.074802043613001246 ) ) ;
#12398 = VERTEX_POINT ( 'NONE', #35725 ) ;
#12399 = CARTESIAN_POINT ( 'NONE',  ( 10.88015784977000067, 2.793131772868000073, -6.864962922767000819 ) ) ;
#12400 = B_SPLINE_CURVE_WITH_KNOTS ( 'NONE', 3,
 ( #22518, #55039, #23223, #48756 ),
 .UNSPECIFIED., .F., .F.,
 ( 4, 4 ),
 ( 0.000000000000000000, 1.000000000000000000 ),
 .UNSPECIFIED. ) ;
#12401 = LINE ( 'NONE', #34079, #35405 ) ;
#12402 = ORIENTED_EDGE ( 'NONE', *, *, #28727, .F. ) ;
#12403 = CARTESIAN_POINT ( 'NONE',  ( 8.824126402770998467, 4.939810497841199854, 7.854398824525599565 ) ) ;
#12404 = CARTESIAN_POINT ( 'NONE',  ( 18.28006803703877026, -2.506146490485266387, -12.34827083869107156 ) ) ;
#12405 = CIRCLE ( 'NONE', #24678, 11.84999999999999964 ) ;
#12406 = CARTESIAN_POINT ( 'NONE',  ( 11.09999803709000155, 0.4999945937327000545, 9.776630298829998011 ) ) ;
#12407 = CARTESIAN_POINT ( 'NONE',  ( 16.39955778315600199, 3.526114926816000139, 11.96132012103000086 ) ) ;
#12408 = CARTESIAN_POINT ( 'NONE',  ( 11.01356641589999974, 2.786433584103999994, 6.253463831328000211 ) ) ;
#12409 = CARTESIAN_POINT ( 'NONE',  ( 9.459367640780998343, 4.408706755790200660, 8.264635032075899446 ) ) ;
#12410 = CARTESIAN_POINT ( 'NONE',  ( 6.869678056658000465, -9.249704301540999651, -5.114242507410000194 ) ) ;
#12411 = VERTEX_POINT ( 'NONE', #25226 ) ;
#12412 = CARTESIAN_POINT ( 'NONE',  ( 5.499988390671900262, -12.65264562523000080, 3.063511175100999573 ) ) ;
#12413 = CARTESIAN_POINT ( 'NONE',  ( 10.08211611373999972, 4.728047954991999369, -8.793974144431000894 ) ) ;
#12414 = EDGE_CURVE ( 'NONE', #55891, #55934, #8809, .T. ) ;
#12415 = DIRECTION ( 'NONE',  ( 0.000000000000000000, 0.8514543052404082157, -0.5244287998266055073 ) ) ;
#12416 = CARTESIAN_POINT ( 'NONE',  ( 12.27908368890581947, 2.837770472453523318, -13.59599796867854238 ) ) ;
#12417 = CARTESIAN_POINT ( 'NONE',  ( 11.17726354018259727, -3.370476274536371442, 8.592232985442818105 ) ) ;
#12418 = EDGE_CURVE ( 'NONE', #48090, #64727, #63530, .T. ) ;
#12419 = CARTESIAN_POINT ( 'NONE',  ( 9.347248564704999652, -4.028326926800000152, 9.469437404464001062 ) ) ;
#12420 = CARTESIAN_POINT ( 'NONE',  ( 17.77532102045679352, 0.5849891190461627977, 13.88342664904964430 ) ) ;
#12421 = CLOSED_SHELL ( 'NONE', ( #40063, #58778, #43315, #51872, #17329, #31614, #16716, #43088, #34693, #29427, #24268, #2244, #3678, #11527, #64603, #50377, #7738, #32322, #59900, #23877, #10480, #8318, #15225, #48138, #53350, #36841, #64256, #68246, #1139, #17803, #3771, #48969, #49165, #63986, #63758, #63845, #8661, #65816, #37193, #51559, #42860, #52169, #407, #67864, #14746, #22247, #10218, #52128, #64853, #11648, #48611, #42663, #43841, #34773, #41128, #51329, #44724, #3269, #27277, #66911, #49792, #51104, #15698, #57455, #64451, #21209, #20448, #56753, #16643, #30073, #17077, #34610, #24457, #49883, #8757, #68809, #43003, #65500, #3853, #7279, #9801, #69087, #65421, #46139, #33899, #66232, #8409, #13024, #42054, #48010, #18626, #41152, #60241, #28256, #22079, #36222, #42319, #8051, #34335, #15582, #2013, #47935, #25335, #15078, #24185, #10782, #38855, #10249, #39786, #215, #41931, #58000, #10082, #4562, #21728, #24577, #28494, #61320, #21544, #40877, #45720, #54378, #58955, #5983, #47070, #35934, #7989, #42881, #33872, #36616, #64418, #32911, #51365, #19539, #4600, #9518, #1010, #29285, #47185, #61650, #43106, #5727, #14057, #9545, #56272, #30576, #54207, #12936, #19672, #40267, #25537, #67467, #38793, #18591, #4272, #16945, #45786, #43131, #37782, #55401, #17174, #23356, #13498, #32051, #20087, #44929, #53255, #40566, #16338, #30107, #29854, #19928, #18398, #35988, #19968, #9690, #66092, #33647, #54049, #35714, #8695, #24389, #47129, #63697, #65160, #11650, #38658, #49960, #54714, #44924, #49879, #12617, #34065, #25951, #1145, #62448, #64630, #59821, #28013, #48185, #37475, #57379, #68727, #16003, #14311, #53819, #30614, #8298, #25007, #45487, #59275, #56400, #18814, #30537, #9252, #25789, #64477, #44759, #33847, #31263, #23747, #55883, #49247, #47703, #5949, #14225, #18089, #48839, #66953, #65982, #16, #3568, #46921, #38459, #14366, #29775, #46965, #43795, #21682, #42415, #7704, #60137, #34357, #20230, #49001, #621, #5119, #25256, #55713, #32937, #41740, #928, #16334, #12395, #60301, #20663, #65705, #60139, #31489, #12987, #35387, #63024, #49195, #31930, #4894, #13197, #9461, #64602, #133, #66444, #53227, #43489, #13022, #41463, #67626, #19565, #24326, #2106, #35331, #25875, #63864, #6149, #3379, #45192, #37663, #24146, #53896, #29852, #14555, #18668, #33672, #58088, #63420, #24920, #9209, #60363 ) ) ;
#12422 = CARTESIAN_POINT ( 'NONE',  ( 24.48565841925800157, -3.324180655266999906, 12.08642999707000065 ) ) ;
#12423 = ORIENTED_EDGE ( 'NONE', *, *, #31740, .T. ) ;
#12424 = ORIENTED_EDGE ( 'NONE', *, *, #63602, .T. ) ;
#12425 = CARTESIAN_POINT ( 'NONE',  ( 9.137754719594999742, 2.319062457810000311, -7.919229449146000022 ) ) ;
#12426 = CARTESIAN_POINT ( 'NONE',  ( 12.44874774240861903, -0.5136130429876892833, 13.88722741725485221 ) ) ;
#12427 = CARTESIAN_POINT ( 'NONE',  ( 10.55862282008599884, -3.333723918618700210, 6.425317846273999933 ) ) ;
#12428 = CARTESIAN_POINT ( 'NONE',  ( 10.56492304196000021, -4.212244324161999565, 8.933470634735002136 ) ) ;
#12429 = CARTESIAN_POINT ( 'NONE',  ( 23.63861704028150612, 3.356905873913091920, -13.53849385471555244 ) ) ;
#12430 = CARTESIAN_POINT ( 'NONE',  ( 7.614808059621999803, -3.326257819185999942, 8.794522506294001118 ) ) ;
#12431 = CARTESIAN_POINT ( 'NONE',  ( 5.452606837613999780, -0.4199405305951999789, 1.440017343911000003 ) ) ;
#12433 = CARTESIAN_POINT ( 'NONE',  ( 11.07204542438999972, -5.775934056910999814, 5.099638290457999545 ) ) ;
#12432 = CARTESIAN_POINT ( 'NONE',  ( 10.61496314287999887, -2.748296264808000267, 7.763860089407599752 ) ) ;
#12434 = CARTESIAN_POINT ( 'NONE',  ( 10.05862282008599884, 4.666276081381299790, -8.574682153725998290 ) ) ;
#12435 = CARTESIAN_POINT ( 'NONE',  ( 24.72545694048200104, -8.702406706990998941, -9.187175443698999189 ) ) ;
#12436 = CARTESIAN_POINT ( 'NONE',  ( 8.893126402770997530, 4.811247217215600003, -7.194081880505399873 ) ) ;
#12437 = CARTESIAN_POINT ( 'NONE',  ( 18.06356912472852727, 0.3639343692979884470, 12.69299665021504531 ) ) ;
#12438 = CARTESIAN_POINT ( 'NONE',  ( 8.266851002545999805, 2.832432432432000269, 6.822293592207000934 ) ) ;
#12439 = CARTESIAN_POINT ( 'NONE',  ( 17.96110074834193426, -2.975239710472639132, -12.32804434199374377 ) ) ;
#12440 = EDGE_LOOP ( 'NONE', ( #67367, #40747, #66301, #61940, #60768, #24333 ) ) ;
#12442 = CARTESIAN_POINT ( 'NONE',  ( 10.87068169682078178, 4.873909797778569697, 7.519268307021759412 ) ) ;
#12441 = CARTESIAN_POINT ( 'NONE',  ( 24.32155146060084050, -3.683040365894125756, 12.56970734039675008 ) ) ;
#12443 = CARTESIAN_POINT ( 'NONE',  ( 8.664129719593997692, 5.524776413195999325, -7.147585171405999915 ) ) ;
#12444 = CARTESIAN_POINT ( 'NONE',  ( 12.52583694058618136, -1.940453150098577106, 13.77633667721135780 ) ) ;
#12445 = CARTESIAN_POINT ( 'NONE',  ( 24.35365242081700288, 8.326148686863003689, -7.789520173261992753 ) ) ;
#12446 = CARTESIAN_POINT ( 'NONE',  ( 10.86272200990529946, 2.793294545435000220, 7.920925559347199219 ) ) ;
#12447 = CARTESIAN_POINT ( 'NONE',  ( 17.80000000005199823, -3.345268251980999974, -11.86064071431999878 ) ) ;
#12448 = CARTESIAN_POINT ( 'NONE',  ( 2.929066298468999463, -2.590989723220999519, -2.488095879762999729 ) ) ;
#12449 = PRODUCT_RELATED_PRODUCT_CATEGORY ( 'part', '', ( #35538 ) ) ;
#12450 = ORIENTED_EDGE ( 'NONE', *, *, #25572, .T. ) ;
#12451 = CARTESIAN_POINT ( 'NONE',  ( 12.21591953885793735, -0.4193891200559257126, -12.59302195412780456 ) ) ;
#12453 = VECTOR ( 'NONE', #51529, 1000.000000000000114 ) ;
#12452 = CARTESIAN_POINT ( 'NONE',  ( 7.805869834195655166, -3.184795896352067501, 6.408392962140504245 ) ) ;
#12454 = CARTESIAN_POINT ( 'NONE',  ( 12.80505043854144276, 0.7192913403693124152, -12.57945229203838267 ) ) ;
#12455 = CARTESIAN_POINT ( 'NONE',  ( 7.149100552923999707, 4.351669901925999895, 8.977196921526999773 ) ) ;
#12456 = EDGE_LOOP ( 'NONE', ( #62442, #10262, #41957, #57369, #4690, #22882, #46440, #23227, #4909, #52255, #45650 ) ) ;
#12457 = CARTESIAN_POINT ( 'NONE',  ( 5.931658963912999738, 0.08722338096739000457, 1.612367018429999854 ) ) ;
#12458 = B_SPLINE_CURVE_WITH_KNOTS ( 'NONE', 3,
 ( #17627, #60614, #66883, #29512 ),
 .UNSPECIFIED., .F., .F.,
 ( 4, 4 ),
 ( 0.8155233265773513818, 1.000000000000000000 ),
 .UNSPECIFIED. ) ;
#12459 = CARTESIAN_POINT ( 'NONE',  ( 8.335910841226001011, 2.603157881926999817, -7.543458285860999979 ) ) ;
#12461 = DIRECTION ( 'NONE',  ( -0.000000000000000000, 1.000000000000000000, 0.000000000000000000 ) ) ;
#12460 = CARTESIAN_POINT ( 'NONE',  ( 8.586687454835056243, -4.265569429095399379, 5.778312903272157186 ) ) ;
#12462 = CARTESIAN_POINT ( 'NONE',  ( 10.55068303964747578, -4.571908710946855692, -6.838932659516637536 ) ) ;
#12463 = EDGE_LOOP ( 'NONE', ( #23014, #322, #45433, #19466 ) ) ;
#12464 = CARTESIAN_POINT ( 'NONE',  ( 9.792562654643999664, -3.463427761954999795, 6.184385360914999907 ) ) ;
#12465 = ORIENTED_EDGE ( 'NONE', *, *, #60785, .F. ) ;
#12466 = DIRECTION ( 'NONE',  ( 1.000000000000000000, 0.000000000000000000, 0.000000000000000000 ) ) ;
#12467 = CARTESIAN_POINT ( 'NONE',  ( 15.86222979673600264, 3.623677739266000231, 11.32125985288999992 ) ) ;
#12468 = AXIS2_PLACEMENT_3D ( 'NONE', #875, #16601, #38619 ) ;
#12469 = CARTESIAN_POINT ( 'NONE',  ( 18.17180502197784975, 0.1017048024284007979, -13.89950429703524293 ) ) ;
#12470 = VERTEX_POINT ( 'NONE', #61946 ) ;
#12471 = CARTESIAN_POINT ( 'NONE',  ( 10.94809868027465960, 9.167339311643493360, -6.329225113183299278 ) ) ;
#12472 = DIRECTION ( 'NONE',  ( 0.000000000000000000, 1.000000000000000000, 0.000000000000000000 ) ) ;
#12473 = CARTESIAN_POINT ( 'NONE',  ( 10.32309687351666838, -5.217465845835395299, 7.827184855449101697 ) ) ;
#12474 = CARTESIAN_POINT ( 'NONE',  ( 8.817462135714999150, -5.100000000000000533, 6.571291218949999902 ) ) ;
#12475 = CARTESIAN_POINT ( 'NONE',  ( 9.179055905797000037, -2.899999999999999911, 6.571291218949999902 ) ) ;
#12476 = EDGE_LOOP ( 'NONE', ( #40734, #15506, #58824, #18949 ) ) ;
#12477 = CARTESIAN_POINT ( 'NONE',  ( 8.898551658772998252, 5.146726419831999522, 6.597424767138000412 ) ) ;
#12478 = EDGE_CURVE ( 'NONE', #45907, #40201, #35199, .T. ) ;
#12479 = EDGE_CURVE ( 'NONE', #23086, #53057, #50173, .T. ) ;
#12480 = CARTESIAN_POINT ( 'NONE',  ( 23.58435508815700032, -13.25843894756000019, -4.303664095111000343 ) ) ;
#12481 = SURFACE_STYLE_FILL_AREA ( #27524 ) ;
#12482 = PLANE ( 'NONE',  #22536 ) ;
#12483 = ORIENTED_EDGE ( 'NONE', *, *, #18706, .F. ) ;
#12484 = CARTESIAN_POINT ( 'NONE',  ( 23.75090057454168146, 13.09200471557739220, -3.783062315943054088 ) ) ;
#12485 = CARTESIAN_POINT ( 'NONE',  ( 10.99664311227126312, 4.444039568019539033, -8.706333095531745059 ) ) ;
#12486 = CARTESIAN_POINT ( 'NONE',  ( 8.336422165046002419, 5.855021065977306982, -7.410170379902396576 ) ) ;
#12487 = DIRECTION ( 'NONE',  ( 1.000000000000000000, 1.507841142982000116E-09, 1.100586469722000106E-11 ) ) ;
#12488 = CARTESIAN_POINT ( 'NONE',  ( 24.30001680106099826, 12.21047197645999915, -3.271805488357999891 ) ) ;
#12489 = DIRECTION ( 'NONE',  ( -1.000000000000000000, 0.000000000000000000, 1.554312234491000161E-14 ) ) ;
#12490 = CARTESIAN_POINT ( 'NONE',  ( 17.65148079338498022, -1.767134912084536325, 12.47546541983269286 ) ) ;
#12491 = EDGE_LOOP ( 'NONE', ( #2936, #61573, #19048 ) ) ;
#12492 = CARTESIAN_POINT ( 'NONE',  ( 11.76588784977539781, -5.120865761890000201, -7.435950347916509884 ) ) ;
#12493 = VERTEX_POINT ( 'NONE', #8685 ) ;
#12494 = B_SPLINE_CURVE_WITH_KNOTS ( 'NONE', 3,
 ( #15543, #26380, #69016, #38146, #56656, #2479 ),
 .UNSPECIFIED., .F., .F.,
 ( 4, 1, 1, 4 ),
 ( 0.000000000000000000, 0.3333333333333000081, 0.6666666666667000474, 1.000000000000000000 ),
 .UNSPECIFIED. ) ;
#12495 = CARTESIAN_POINT ( 'NONE',  ( 0.1499942179680000265, 2.678379783547567339, 0.7197945678028357941 ) ) ;
#12496 = CARTESIAN_POINT ( 'NONE',  ( 10.03280471959000231, 3.987760651117999711, -9.123263301387000368 ) ) ;
#12497 = CIRCLE ( 'NONE', #41532, 12.39999890530000037 ) ;
#12498 = CARTESIAN_POINT ( 'NONE',  ( 3.467248883606000032, 0.03946336865253999987, 3.379145356818000323 ) ) ;
#12499 = EDGE_CURVE ( 'NONE', #51109, #1148, #39688, .T. ) ;
#12500 = CARTESIAN_POINT ( 'NONE',  ( 10.01597818573999987, -4.792673671522000411, -6.390249203106999509 ) ) ;
#12501 = CARTESIAN_POINT ( 'NONE',  ( 11.50009108335969898, -2.881106418324590468, 7.402342568044064208 ) ) ;
#12502 = CARTESIAN_POINT ( 'NONE',  ( 24.33639490202200406, 12.30598233413000031, 3.219714224404999658 ) ) ;
#12503 = DIRECTION ( 'NONE',  ( 1.000000000000000000, 0.000000000000000000, 0.000000000000000000 ) ) ;
#12504 = VERTEX_POINT ( 'NONE', #33889 ) ;
#12505 = DIRECTION ( 'NONE',  ( 1.000000000000000000, 0.000000000000000000, 0.000000000000000000 ) ) ;
#12506 = CARTESIAN_POINT ( 'NONE',  ( 10.92795525820100089, -4.094749303624469761, 8.498986197235801399 ) ) ;
#12507 = CARTESIAN_POINT ( 'NONE',  ( 9.447841622600000377, 5.447457912891000120, 7.431328695644999982 ) ) ;
#12508 = B_SPLINE_CURVE_WITH_KNOTS ( 'NONE', 3,
 ( #13164, #34492, #7906, #18745 ),
 .UNSPECIFIED., .F., .F.,
 ( 4, 4 ),
 ( 0.000000000000000000, 1.000000000000000000 ),
 .UNSPECIFIED. ) ;
#12509 = CARTESIAN_POINT ( 'NONE',  ( 25.46372189163300348, -2.879475976718999686, 11.30953721564000070 ) ) ;
#12510 = CARTESIAN_POINT ( 'NONE',  ( 10.36409408021999923, -3.399999909169000301, -4.954046131279000065 ) ) ;
#12511 = DIRECTION ( 'NONE',  ( 1.000000000000000000, 0.000000000000000000, 0.000000000000000000 ) ) ;
#12512 = AXIS2_PLACEMENT_3D ( 'NONE', #29123, #50092, #39599 ) ;
#12513 = CARTESIAN_POINT ( 'NONE',  ( 11.16641369783139837, 3.949373449607799902, -8.502191501283999031 ) ) ;
#12514 = CARTESIAN_POINT ( 'NONE',  ( 10.43950453984525417, 2.266522852357361728, 7.738844268769847545 ) ) ;
#12515 = VECTOR ( 'NONE', #37427, 1000.000000000000227 ) ;
#12516 = B_SPLINE_CURVE_WITH_KNOTS ( 'NONE', 3,
 ( #37391, #20973, #63611, #16405, #26221, #10818, #16061, #54154, #59061, #63259, #32498, #53476, #15727, #679, #15386, #62003, #16744, #58369 ),
 .UNSPECIFIED., .F., .F.,
 ( 4, 2, 2, 2, 2, 2, 2, 2, 4 ),
 ( 0.000000000000000000, 0.1250000000000000000, 0.2500000000000000000, 0.3750000000000000000, 0.5000000000000000000, 0.6250000000000000000, 0.7500000000000000000, 0.8750000000000000000, 1.000000000000000000 ),
 .UNSPECIFIED. ) ;
#12517 = CARTESIAN_POINT ( 'NONE',  ( 9.910317406968998100, 4.212364169857599983, -8.621889436328999068 ) ) ;
#12518 = CARTESIAN_POINT ( 'NONE',  ( 23.55356531116300189, -10.33133730171999964, 9.496498206886998972 ) ) ;
#12519 = CARTESIAN_POINT ( 'NONE',  ( 8.129547907574799837, 4.951600119927478616, -6.344532045157325939 ) ) ;
#12520 = ORIENTED_EDGE ( 'NONE', *, *, #8853, .F. ) ;
#12521 = CARTESIAN_POINT ( 'NONE',  ( 7.437254440376999121, -2.216884807317999861, 8.370075800106999253 ) ) ;
#12522 = CARTESIAN_POINT ( 'NONE',  ( 10.15291672334000062, -4.949038487346999915, -8.498994087616001281 ) ) ;
#12523 = CARTESIAN_POINT ( 'NONE',  ( 18.18532329594571095, 2.156378744708868922, 13.83294935661368541 ) ) ;
#12524 = CARTESIAN_POINT ( 'NONE',  ( 15.90018573812068325, -5.468217585226445188, -10.55609518975756345 ) ) ;
#12525 = CARTESIAN_POINT ( 'NONE',  ( 11.30579707368350029, -4.634832087857400751, -6.390809033205999690 ) ) ;
#12526 = ORIENTED_EDGE ( 'NONE', *, *, #6571, .F. ) ;
#12527 = B_SPLINE_CURVE_WITH_KNOTS ( 'NONE', 3,
 ( #17463, #3357, #40419, #3015, #32853, #27957, #18766 ),
 .UNSPECIFIED., .F., .F.,
 ( 4, 1, 1, 1, 4 ),
 ( 0.000000000000000000, 0.2500000143192999680, 0.5000000056314000130, 0.7499999969435999780, 1.000000000000000000 ),
 .UNSPECIFIED. ) ;
#12528 = CARTESIAN_POINT ( 'NONE',  ( 24.48566039390000171, 3.324180779519999795, -12.08642902895999782 ) ) ;
#12529 = CARTESIAN_POINT ( 'NONE',  ( 7.191892219589999691, 3.501518846194999757, 9.055971388486000251 ) ) ;
#12531 = CARTESIAN_POINT ( 'NONE',  ( 11.05435090131019926, 5.119447121461000449, 6.807613609764599616 ) ) ;
#12530 = CARTESIAN_POINT ( 'NONE',  ( 8.323770280408998801, 5.332332124071999857, -8.487089944253000340 ) ) ;
#12532 = CARTESIAN_POINT ( 'NONE',  ( 10.72128915877000033, 4.673511966357999370, -5.778393480304000462 ) ) ;
#12533 = ADVANCED_FACE ( 'NONE', ( #29000 ), #38576, .T. ) ;
#12534 = VERTEX_POINT ( 'NONE', #55554 ) ;
#12535 = ADVANCED_FACE ( 'NONE', ( #30033 ), #2408, .T. ) ;
#12536 = CARTESIAN_POINT ( 'NONE',  ( 10.50244247011999832, 2.268911387573000038, 7.824865741583000300 ) ) ;
#12537 = CARTESIAN_POINT ( 'NONE',  ( 18.03607885879101147, -1.971554139641146230, -13.86048489721954624 ) ) ;
#12538 = CARTESIAN_POINT ( 'NONE',  ( 10.71918447801630059, 5.140463864104999558, 7.525145395936648995 ) ) ;
#12539 = CARTESIAN_POINT ( 'NONE',  ( 9.576494682405000347, -4.593972507100000158, 5.662052676321000177 ) ) ;
#12540 = EDGE_LOOP ( 'NONE', ( #6595, #50957, #19934, #44009 ) ) ;
#12541 = CARTESIAN_POINT ( 'NONE',  ( 24.70770306079000278, 12.32897093721000026, -2.948671852896999734 ) ) ;
#12543 = CARTESIAN_POINT ( 'NONE',  ( 10.84160444037999937, -2.641264320582999758, -7.444904971031999885 ) ) ;
#12542 = CARTESIAN_POINT ( 'NONE',  ( 12.01716035628400192, -11.91307312420999942, 3.686993282830000052 ) ) ;
#12544 = CARTESIAN_POINT ( 'NONE',  ( 8.058954703304616274, -3.652055520346594975, 5.795450222806093343 ) ) ;
#12545 = CARTESIAN_POINT ( 'NONE',  ( 10.68403590588000007, -5.436611040123999317, 8.578433628717998971 ) ) ;
#12546 = CARTESIAN_POINT ( 'NONE',  ( 10.10331918378244431, -3.090221196180537699, 8.647993508352264769 ) ) ;
#12547 = CARTESIAN_POINT ( 'NONE',  ( 10.03132996542199962, -4.793057006135000186, 6.678540912152799436 ) ) ;
#12548 = ORIENTED_EDGE ( 'NONE', *, *, #27146, .F. ) ;
#12550 = CARTESIAN_POINT ( 'NONE',  ( 24.17844123396919542, -9.099783653359832414, 9.084867597324226551 ) ) ;
#12549 = CIRCLE ( 'NONE', #18141, 2.100000000000000533 ) ;
#12551 = CARTESIAN_POINT ( 'NONE',  ( 10.82533997688000049, -3.756890902898200046, 8.614534918052999757 ) ) ;
#12552 = ORIENTED_EDGE ( 'NONE', *, *, #16472, .T. ) ;
#12553 = CARTESIAN_POINT ( 'NONE',  ( 12.80000000000000071, 11.23412379136000006, -3.084957477885999833 ) ) ;
#12554 = ORIENTED_EDGE ( 'NONE', *, *, #16578, .T. ) ;
#12555 = CARTESIAN_POINT ( 'NONE',  ( 9.342560841233000346, 5.835196551504000517, -7.008466539623000813 ) ) ;
#12556 = CARTESIAN_POINT ( 'NONE',  ( 17.55505043854143565, 1.875000000000000000, 12.57541666120756041 ) ) ;
#12557 = CARTESIAN_POINT ( 'NONE',  ( 8.268352065779833282, 5.042535165667102248, 6.407252835108709021 ) ) ;
#12558 = CARTESIAN_POINT ( 'NONE',  ( 12.51396835178759659, 3.139274738718781599, -12.20266202197804972 ) ) ;
#12559 = CARTESIAN_POINT ( 'NONE',  ( 11.52812378248509795, -4.416893162838900544, 8.288725998710999576 ) ) ;
#12560 = EDGE_CURVE ( 'NONE', #44978, #36556, #18497, .T. ) ;
#12561 = CARTESIAN_POINT ( 'NONE',  ( 9.304437359457891077, 2.650065539925081204, -7.676779421619798427 ) ) ;
#12562 = CIRCLE ( 'NONE', #44961, 1.600000000000000089 ) ;
#12563 = EDGE_CURVE ( 'NONE', #8116, #32306, #16847, .T. ) ;
#12564 = ORIENTED_EDGE ( 'NONE', *, *, #47132, .F. ) ;
#12565 = CARTESIAN_POINT ( 'NONE',  ( 8.047379440378000126, -4.468370631666999770, 8.882152684713000568 ) ) ;
#12566 = CARTESIAN_POINT ( 'NONE',  ( 24.11585380241538701, 9.189141416228876480, 9.154356187537644018 ) ) ;
#12567 = EDGE_LOOP ( 'NONE', ( #29757, #36518, #56031, #32286, #36477 ) ) ;
#12568 = CARTESIAN_POINT ( 'NONE',  ( 12.08013217067794720, -2.460179751193595887, -12.35749396829501023 ) ) ;
#12569 = CARTESIAN_POINT ( 'NONE',  ( 11.21149010443640037, 5.137564434800999891, 7.414927836855409460 ) ) ;
#12570 = AXIS2_PLACEMENT_3D ( 'NONE', #39081, #49563, #7261 ) ;
#12571 = CARTESIAN_POINT ( 'NONE',  ( 24.35365242081699932, 3.253466243134998326, -12.21167519469000240 ) ) ;
#12572 = CARTESIAN_POINT ( 'NONE',  ( 10.91624242361999997, 5.459834480072999874, -8.642877574935999618 ) ) ;
#12573 = CARTESIAN_POINT ( 'NONE',  ( 18.10229711294200072, -11.55827859785000022, 4.675888931126000791 ) ) ;
#12574 = CARTESIAN_POINT ( 'NONE',  ( 8.142152878612618494, -3.293758513149224854, 8.705677052449603437 ) ) ;
#12575 = CARTESIAN_POINT ( 'NONE',  ( 12.49024380163862169, -3.040024005673539254, -13.54391858567109885 ) ) ;
#12576 = CARTESIAN_POINT ( 'NONE',  ( 18.18005727183074782, -0.009762034906138482987, -12.70000045436731995 ) ) ;
#12577 = CARTESIAN_POINT ( 'NONE',  ( 17.55505043854143565, 1.875000000000000000, -13.78631952119025073 ) ) ;
#12578 = CARTESIAN_POINT ( 'NONE',  ( 11.01456785386839954, -4.946394603182100447, -8.136888821800198457 ) ) ;
#12579 = DIRECTION ( 'NONE',  ( 1.000000000000000000, 0.000000000000000000, 0.000000000000000000 ) ) ;
#12580 = EDGE_LOOP ( 'NONE', ( #22524, #37938, #3917, #66367, #65335, #45485, #51328 ) ) ;
#12581 = SURFACE_STYLE_USAGE ( .BOTH. , #27975 ) ;
#12582 = FACE_OUTER_BOUND ( 'NONE', #42536, .T. ) ;
#12583 = DIRECTION ( 'NONE',  ( 0.000000000000000000, 0.000000000000000000, -1.000000000000000000 ) ) ;
#12584 = CARTESIAN_POINT ( 'NONE',  ( 10.90638722582999875, 5.227488226180000197, 6.784465725675999259 ) ) ;
#12585 = CARTESIAN_POINT ( 'NONE',  ( 23.66588336739700082, -3.239807211238000306, 13.42507355106999967 ) ) ;
#12586 = ADVANCED_FACE ( 'NONE', ( #35266 ), #34584, .F. ) ;
#12587 = CARTESIAN_POINT ( 'NONE',  ( 18.08809746899275694, 2.173637705205955228, 12.52162896472547082 ) ) ;
#12588 = CARTESIAN_POINT ( 'NONE',  ( 18.35309808591700076, 2.844562563850999926, -12.04738788559999918 ) ) ;
#12589 = CARTESIAN_POINT ( 'NONE',  ( 10.40227026081000083, 2.765684886876999649, 9.035354958280999327 ) ) ;
#12590 = CARTESIAN_POINT ( 'NONE',  ( 10.53743284169262573, -4.454886069780877200, 8.247402791297171021 ) ) ;
#12591 = B_SPLINE_CURVE_WITH_KNOTS ( 'NONE', 3,
 ( #53781, #5877, #27216, #43177 ),
 .UNSPECIFIED., .F., .F.,
 ( 4, 4 ),
 ( 0.000000000000000000, 1.000000000000000000 ),
 .UNSPECIFIED. ) ;
#12592 = CARTESIAN_POINT ( 'NONE',  ( 2.286817272374999543, 2.922173510531999696, 1.340674101542000063 ) ) ;
#12593 = EDGE_LOOP ( 'NONE', ( #49950, #20767, #11073, #41099, #26352 ) ) ;
#12594 = CARTESIAN_POINT ( 'NONE',  ( 12.43939714311205336, -3.101706251878837861, 12.21226669259267439 ) ) ;
#12595 = CARTESIAN_POINT ( 'NONE',  ( 8.971126402771000485, -3.060189502158800146, -7.145601175474399547 ) ) ;
#12596 = FACE_OUTER_BOUND ( 'NONE', #12064, .T. ) ;
#12597 = B_SPLINE_CURVE_WITH_KNOTS ( 'NONE', 3,
 ( #1983, #44645, #39382, #27867 ),
 .UNSPECIFIED., .F., .F.,
 ( 4, 4 ),
 ( 0.000000000000000000, 1.000000000000000000 ),
 .UNSPECIFIED. ) ;
#12598 = CARTESIAN_POINT ( 'NONE',  ( 9.262620115046999558, 3.343122245339613663, 8.575407073603340535 ) ) ;
#12599 = CARTESIAN_POINT ( 'NONE',  ( 11.01041369783139956, 3.935522326596939902, -8.776385133971000840 ) ) ;
#12600 = CARTESIAN_POINT ( 'NONE',  ( 12.36315700431396714, -0.5707228546306997163, 12.58707662888204304 ) ) ;
#12601 = CARTESIAN_POINT ( 'NONE',  ( 8.175760841228999709, 2.599243720295000060, 7.909344432242998657 ) ) ;
#12602 = CARTESIAN_POINT ( 'NONE',  ( 10.89874804681000064, 2.834828962328999502, 9.088465460431999432 ) ) ;
#12603 = CARTESIAN_POINT ( 'NONE',  ( 12.51734955435997598, 3.054939157457059906, 12.30478592156021378 ) ) ;
#12604 = VERTEX_POINT ( 'NONE', #61483 ) ;
#12605 = CARTESIAN_POINT ( 'NONE',  ( 9.635004719593998956, 2.334550724494000029, -7.977056617806000283 ) ) ;
#12606 = CARTESIAN_POINT ( 'NONE',  ( 10.46887750876899936, 3.307728619566300043, -8.574279626736998949 ) ) ;
#12607 = PLANE ( 'NONE',  #38286 ) ;
#12609 = CARTESIAN_POINT ( 'NONE',  ( 18.02496081276520101, -0.4121104631841241983, 12.69099970360672458 ) ) ;
#12608 = CARTESIAN_POINT ( 'NONE',  ( 8.817629440380001071, -3.894643656844000379, 6.044452984962999764 ) ) ;
#12610 = CARTESIAN_POINT ( 'NONE',  ( 10.03334252387499959, -4.992846242613000030, 7.651982363644999730 ) ) ;
#12611 = CARTESIAN_POINT ( 'NONE',  ( 10.62903166480609940, -4.864052766304100217, -7.560921321260908989 ) ) ;
#12612 = ORIENTED_EDGE ( 'NONE', *, *, #40874, .T. ) ;
#12613 = CARTESIAN_POINT ( 'NONE',  ( 2.168522225066999987, 1.603576596796000064, -2.837084241009999896 ) ) ;
#12614 = CARTESIAN_POINT ( 'NONE',  ( 6.841180590298025166, -0.9745722302259033354, 0.7309630519589359610 ) ) ;
#12615 = CARTESIAN_POINT ( 'NONE',  ( 9.383506238772769237, -3.863849893416519521, 8.533506295447228496 ) ) ;
#12616 = CARTESIAN_POINT ( 'NONE',  ( 18.05125194753120965, -2.880159329997852069, 13.58544989777342415 ) ) ;
#12617 = ADVANCED_FACE ( 'NONE', ( #34235 ), #8346, .T. ) ;
#12618 = ADVANCED_FACE ( 'NONE', ( #8004, #29340 ), #50652, .T. ) ;
#12619 = DIRECTION ( 'NONE',  ( 0.000000000000000000, -0.8707944170444857912, 0.4916473159126918957 ) ) ;
#12620 = CARTESIAN_POINT ( 'NONE',  ( 12.75683046442385482, -1.789027279909009227, 13.88522190323555350 ) ) ;
#12621 = CARTESIAN_POINT ( 'NONE',  ( 11.05669207475000171, 2.810775113057000230, 4.849214660961000511 ) ) ;
#12622 = DIRECTION ( 'NONE',  ( -1.000000000000000000, 0.000000000000000000, 0.000000000000000000 ) ) ;
#12623 = CARTESIAN_POINT ( 'NONE',  ( 17.55505043854143565, 3.125000000000000000, -13.52084414783465682 ) ) ;
#12624 = VERTEX_POINT ( 'NONE', #66722 ) ;
#12625 = ADVANCED_FACE ( 'NONE', ( #18842 ), #47798, .F. ) ;
#12626 = LINE ( 'NONE', #60863, #22978 ) ;
#12627 = CARTESIAN_POINT ( 'NONE',  ( 11.59213512191444018, 3.196550831395155168, -7.174950736703190834 ) ) ;
#12628 = CARTESIAN_POINT ( 'NONE',  ( 7.424682295424686274, -2.345875091448395455, 8.038402344753549755 ) ) ;
#12629 = CARTESIAN_POINT ( 'NONE',  ( 10.76947109217999810, 5.100000000000000533, -6.152188490330000370 ) ) ;
#12630 = CARTESIAN_POINT ( 'NONE',  ( 1.275974932895000080, -3.758001540264999996, 0.07616889274500000806 ) ) ;
#12631 = ORIENTED_EDGE ( 'NONE', *, *, #1799, .T. ) ;
#12632 = DIRECTION ( 'NONE',  ( 0.000000000000000000, -1.000000000000000000, 0.000000000000000000 ) ) ;
#12633 = CARTESIAN_POINT ( 'NONE',  ( 17.71905360607584967, 1.896551502301641934, -12.57190390430904436 ) ) ;
#12634 = CARTESIAN_POINT ( 'NONE',  ( 10.79500540879000070, 3.503955365545999623, 6.168588659884999714 ) ) ;
#12635 = CARTESIAN_POINT ( 'NONE',  ( 10.92026088462129962, 4.002135146349410810, 8.503467136482999678 ) ) ;
#12636 = CARTESIAN_POINT ( 'NONE',  ( 18.50001572531400384, 0.9783175634148698618, 12.52499999877128722 ) ) ;
#12637 = CARTESIAN_POINT ( 'NONE',  ( 9.406851002546000373, -2.832432432432000269, -6.822293592207000934 ) ) ;
#12638 = CARTESIAN_POINT ( 'NONE',  ( 18.28019269455629114, 0.1906559479335279972, -14.00000681886699105 ) ) ;
#12639 = CARTESIAN_POINT ( 'NONE',  ( 0.5000220334827000235, 2.806761118207999672, -2.090954811877999919 ) ) ;
#12640 = CARTESIAN_POINT ( 'NONE',  ( 12.64175205087593490, -3.104634757607365625, 12.28992885563596360 ) ) ;
#12641 = VERTEX_POINT ( 'NONE', #34923 ) ;
#12642 = CARTESIAN_POINT ( 'NONE',  ( 7.327778877203178887, 3.954478523966745040, 9.238305800967093973 ) ) ;
#12643 = ORIENTED_EDGE ( 'NONE', *, *, #19486, .T. ) ;
#12644 = AXIS2_PLACEMENT_3D ( 'NONE', #64268, #52416, #58347 ) ;
#12645 = B_SPLINE_CURVE_WITH_KNOTS ( 'NONE', 3,
 ( #46321, #51893, #62048, #62388, #47005, #51219, #30928, #67281, #19399, #57141, #56812, #20426, #51552, #3991, #41755, #25327 ),
 .UNSPECIFIED., .F., .F.,
 ( 4, 2, 2, 1, 1, 2, 2, 2, 4 ),
 ( 0.000000000000000000, 0.2499999999999812372, 0.3749999999999744094, 0.4374999999999678035, 0.4687499999999645284, 0.4843749999999643618, 0.4999999999999642508, 0.7499999999999821254, 1.000000000000000000 ),
 .UNSPECIFIED. ) ;
#12646 = CARTESIAN_POINT ( 'NONE',  ( 18.06424752491737706, -2.862976204506491484, 13.58975765073224906 ) ) ;
#12647 = DIRECTION ( 'NONE',  ( 1.000000000000000000, 0.000000000000000000, 0.000000000000000000 ) ) ;
#12648 = ORIENTED_EDGE ( 'NONE', *, *, #68468, .F. ) ;
#12649 = CARTESIAN_POINT ( 'NONE',  ( 10.32169598648999909, 4.766524664146899681, 7.043598424555200133 ) ) ;
#12650 = CARTESIAN_POINT ( 'NONE',  ( 6.503943694692421396, 0.6532722510427437790, -0.9258527769090765247 ) ) ;
#12651 = CARTESIAN_POINT ( 'NONE',  ( 23.63923232067427094, 13.40729140062978075, -3.856841352120893074 ) ) ;
#12652 = B_SPLINE_CURVE_WITH_KNOTS ( 'NONE', 3,
 ( #36061, #52483, #3219, #14408, #57377, #9480, #24886, #46562, #30823, #51794, #62290, #46903, #56709, #67868, #31179, #30480, #3891, #40967 ),
 .UNSPECIFIED., .F., .F.,
 ( 4, 2, 2, 2, 2, 2, 2, 2, 4 ),
 ( 0.000000000000000000, 0.1250000000000003331, 0.2500000000000006661, 0.3750000000000009992, 0.5000000000000013323, 0.6250000000000009992, 0.7500000000000006661, 0.8750000000000003331, 1.000000000000000000 ),
 .UNSPECIFIED. ) ;
#12653 = CARTESIAN_POINT ( 'NONE',  ( 10.96080777006000062, 2.054568739078000306, 7.810084630238000258 ) ) ;
#12654 = CARTESIAN_POINT ( 'NONE',  ( 12.43754357087991202, -3.154646014561297562, -13.64000194807119826 ) ) ;
#12655 = CARTESIAN_POINT ( 'NONE',  ( 10.69601354018253581, -3.000416447002272058, 8.268183399968641822 ) ) ;
#12656 = CARTESIAN_POINT ( 'NONE',  ( 11.56631965465000178, 3.502676170607000206, -11.07146920481999963 ) ) ;
#12657 = CARTESIAN_POINT ( 'NONE',  ( 11.06133683778999988, -2.503914237677999921, -6.712780725818999983 ) ) ;
#12658 = CARTESIAN_POINT ( 'NONE',  ( 10.97807333593999957, 5.235090452703000885, -6.783100406990000053 ) ) ;
#12659 = CARTESIAN_POINT ( 'NONE',  ( -15.86200481174999943, 2.399999999999999911, -6.571291218949999902 ) ) ;
#12660 = ORIENTED_EDGE ( 'NONE', *, *, #63508, .F. ) ;
#12661 = CARTESIAN_POINT ( 'NONE',  ( 24.30000000000000071, 2.078227429405999693, -11.31065739696999906 ) ) ;
#12662 =( NAMED_UNIT ( * ) SI_UNIT ( $, .STERADIAN. ) SOLID_ANGLE_UNIT ( ) );
#12663 = DIRECTION ( 'NONE',  ( 1.000000000000000000, -1.157371756828000031E-14, -5.786858784138000079E-14 ) ) ;
#12664 = CARTESIAN_POINT ( 'NONE',  ( 10.27635097765000083, -4.738769859112000660, 4.693832200104000485 ) ) ;
#12665 = ADVANCED_FACE ( 'NONE', ( #29692 ), #50993, .T. ) ;
#12666 = CIRCLE ( 'NONE', #24938, 14.00000000000000533 ) ;
#12667 = PLANE ( 'NONE',  #46233 ) ;
#12668 = CARTESIAN_POINT ( 'NONE',  ( 9.143927823787139531, 5.249988444743198812, 7.500000155056751439 ) ) ;
#12669 = CARTESIAN_POINT ( 'NONE',  ( 12.52647507922620562, 1.940423270478297102, 13.77628945559399121 ) ) ;
#12670 = CARTESIAN_POINT ( 'NONE',  ( 9.889844610056000462, -4.052276314598000084, 9.260527932809999641 ) ) ;
#12671 = ORIENTED_EDGE ( 'NONE', *, *, #37497, .F. ) ;
#12672 = EDGE_CURVE ( 'NONE', #25788, #17060, #13940, .T. ) ;
#12673 = CARTESIAN_POINT ( 'NONE',  ( 24.35365242081699932, -8.948887819794997256, -8.923422014253004519 ) ) ;
#12674 = CARTESIAN_POINT ( 'NONE',  ( 12.09164601416806306, 0.1306247939804469627, 13.99939550958098522 ) ) ;
#12675 = VERTEX_POINT ( 'NONE', #62162 ) ;
#12676 = CARTESIAN_POINT ( 'NONE',  ( 7.313271682458000633, 2.788803157567000035, -8.345558963038001821 ) ) ;
#12677 = CARTESIAN_POINT ( 'NONE',  ( 8.893038976302710452, 2.713248994154062732, -7.026754482570071403 ) ) ;
#12678 = CARTESIAN_POINT ( 'NONE',  ( 23.58437025649000063, -2.901519131754999758, -13.63407372122000005 ) ) ;
#12679 = CARTESIAN_POINT ( 'NONE',  ( 4.599999999999999645, -1.875000000000000000, 13.78631952119025073 ) ) ;
#12680 = CARTESIAN_POINT ( 'NONE',  ( 9.576420280414000175, 4.861259245430999520, -8.806664389576001284 ) ) ;
#12681 = CARTESIAN_POINT ( 'NONE',  ( 9.989763540182750035, 4.327184855449099921, -8.717465845835395299 ) ) ;
#12682 = DIRECTION ( 'NONE',  ( 0.000000000000000000, 0.7180578485451756254, 0.6959834237556764558 ) ) ;
#12683 = CARTESIAN_POINT ( 'NONE',  ( 5.500000000000000000, 12.78667792605000031, -2.345384795462000405 ) ) ;
#12684 = DIRECTION ( 'NONE',  ( 1.000000000000000000, 0.000000000000000000, 0.000000000000000000 ) ) ;
#12685 = SURFACE_SIDE_STYLE ('',( #54990 ) ) ;
#12686 = CARTESIAN_POINT ( 'NONE',  ( 9.526735624254000001, -3.423478821957000040, -6.068694811299999436 ) ) ;
#12687 = CARTESIAN_POINT ( 'NONE',  ( 10.60441638348510018, 3.158410350011299883, -7.294998899090099798 ) ) ;
#12688 = CARTESIAN_POINT ( 'NONE',  ( 10.90000000162999960, 2.899999999992999733, -5.160242739096000619 ) ) ;
#12689 = CARTESIAN_POINT ( 'NONE',  ( 10.51925056272499859, 5.174767082365999471, -7.517410630436119234 ) ) ;
#12690 = CARTESIAN_POINT ( 'NONE',  ( 8.748138961223999033, 4.832207374954999857, -8.062381800110799190 ) ) ;
#12692 = CARTESIAN_POINT ( 'NONE',  ( 10.57189201149000191, -2.801299163661999714, 4.692232677100000693 ) ) ;
#12691 = CARTESIAN_POINT ( 'NONE',  ( 9.319151519676999840, -3.978278301382419890, 6.495824366094999469 ) ) ;
#12693 = CARTESIAN_POINT ( 'NONE',  ( 11.35226354018294792, -5.092232985442820770, 8.129523725463624118 ) ) ;
#12694 = VERTEX_POINT ( 'NONE', #25104 ) ;
#12695 = AXIS2_PLACEMENT_3D ( 'NONE', #51443, #45860, #34694 ) ;
#12696 = CARTESIAN_POINT ( 'NONE',  ( 11.35545123989519922, 4.475221369382300196, 6.582230774881299595 ) ) ;
#12697 = CARTESIAN_POINT ( 'NONE',  ( 9.476374593785998002, -5.098398394707999159, 6.305533045879999854 ) ) ;
#12698 = CARTESIAN_POINT ( 'NONE',  ( 9.631696787963999640, 4.196076320588900010, 8.624850445389000697 ) ) ;
#12699 = CARTESIAN_POINT ( 'NONE',  ( 10.18940772478662637, 3.446387339840331965, -8.177528816364860731 ) ) ;
#12700 = ADVANCED_FACE ( 'NONE', ( #9022 ), #5612, .F. ) ;
#12701 = CARTESIAN_POINT ( 'NONE',  ( 9.290195424034999760, -2.377814350880000038, 7.540992175424999999 ) ) ;
#12702 = LINE ( 'NONE', #27756, #50883 ) ;
#12704 = UNCERTAINTY_MEASURE_WITH_UNIT (LENGTH_MEASURE( 1.000000000000000082E-05 ), #872, 'distance_accuracy_value', 'NONE');
#12703 = CARTESIAN_POINT ( 'NONE',  ( 10.52934687351650389, 4.163624617374466652, 6.250000000000000000 ) ) ;
#12705 = VERTEX_POINT ( 'NONE', #52863 ) ;
#12706 = EDGE_CURVE ( 'NONE', #6018, #64952, #5988, .T. ) ;
#12707 = ADVANCED_FACE ( 'NONE', ( #406 ), #20997, .T. ) ;
#12708 = AXIS2_PLACEMENT_3D ( 'NONE', #11081, #58628, #63862 ) ;
#12709 = CARTESIAN_POINT ( 'NONE',  ( 8.655265421554998895, -4.188500707411799695, -8.475084258675400051 ) ) ;
#12710 = DIRECTION ( 'NONE',  ( 0.000000000000000000, -0.001485959642859940649, 0.9999988959613604900 ) ) ;
#12711 = CARTESIAN_POINT ( 'NONE',  ( 5.419378390662999756, 1.024801514603000063, 1.247845015360000032 ) ) ;
#12712 = CARTESIAN_POINT ( 'NONE',  ( 9.258104461123007667, -2.902565898239000131, -6.601372212749001100 ) ) ;
#12713 = AXIS2_PLACEMENT_3D ( 'NONE', #13381, #8123, #45535 ) ;
#12714 = CARTESIAN_POINT ( 'NONE',  ( 11.49999672495000169, 7.851643750443685121, -8.692270414123809630 ) ) ;
#12715 = CARTESIAN_POINT ( 'NONE',  ( 11.49826088462129903, -3.998156935320088756, 8.366195817038299509 ) ) ;
#12716 = CARTESIAN_POINT ( 'NONE',  ( 11.77359063708300013, 4.955772084214699724, -7.768721787835699999 ) ) ;
#12717 = CARTESIAN_POINT ( 'NONE',  ( 8.576923877145999242, -3.399999999999999911, 5.924121105096999962 ) ) ;
#12718 = CARTESIAN_POINT ( 'NONE',  ( 9.524152735436000938, -4.911674715448000050, -6.466751564808000730 ) ) ;
#12719 = CARTESIAN_POINT ( 'NONE',  ( 25.57778554945400273, 11.11296393906000013, 3.219278657787000064 ) ) ;
#12720 = ORIENTED_EDGE ( 'NONE', *, *, #38370, .T. ) ;
#12721 = CARTESIAN_POINT ( 'NONE',  ( 8.960616452296999768, -2.899999999999999911, 6.279946362737000243 ) ) ;
#12722 = B_SPLINE_CURVE_WITH_KNOTS ( 'NONE', 3,
 ( #29259, #35862, #2329, #9273 ),
 .UNSPECIFIED., .F., .F.,
 ( 4, 4 ),
 ( 0.000000000000000000, 1.000000000000000000 ),
 .UNSPECIFIED. ) ;
#12723 = CARTESIAN_POINT ( 'NONE',  ( 12.14435534536353600, -0.3008963210925020837, -13.99677033988233354 ) ) ;
#12724 = CARTESIAN_POINT ( 'NONE',  ( 14.04832727683000115, -8.838110522795000534, -7.948685794524999793 ) ) ;
#12725 = DIRECTION ( 'NONE',  ( -1.000000000000000000, 0.000000000000000000, 0.000000000000000000 ) ) ;
#12726 = ADVANCED_FACE ( 'NONE', ( #21722 ), #62, .F. ) ;
#12727 = CARTESIAN_POINT ( 'NONE',  ( 18.18005044212792143, 2.500000099754956739, -13.67345740034994250 ) ) ;
#12728 = CARTESIAN_POINT ( 'NONE',  ( 0.7000000000000000666, 0.000000000000000000, 0.000000000000000000 ) ) ;
#12729 = CARTESIAN_POINT ( 'NONE',  ( 5.699999545467999695, 12.03770622561999915, -3.722046322334000124 ) ) ;
#12730 = VERTEX_POINT ( 'NONE', #31893 ) ;
#12731 =( LENGTH_UNIT ( ) NAMED_UNIT ( * ) SI_UNIT ( .MILLI., .METRE. ) );
#12732 = CARTESIAN_POINT ( 'NONE',  ( 18.17918265292642488, 2.461360938835027934, -13.68159685767606781 ) ) ;
#12733 = ORIENTED_EDGE ( 'NONE', *, *, #57227, .F. ) ;
#12734 = DIRECTION ( 'NONE',  ( 0.000000000000000000, 0.1623203401144080182, -0.9867381147929490393 ) ) ;
#12735 = CARTESIAN_POINT ( 'NONE',  ( 9.316120559621998254, -3.677416446733000388, 9.250734868033999803 ) ) ;
#12736 = CARTESIAN_POINT ( 'NONE',  ( 9.012204719595001023, 3.161445734422999809, -6.178649910536000434 ) ) ;
#12737 = CARTESIAN_POINT ( 'NONE',  ( 11.10000000000000142, -2.373997543953228373, -7.952634597122376192 ) ) ;
#12738 = CARTESIAN_POINT ( 'NONE',  ( 17.78989870834643483, 1.827084948615273818, -13.88026577095109815 ) ) ;
#12739 = B_SPLINE_CURVE_WITH_KNOTS ( 'NONE', 3,
 ( #23561, #1901, #61657, #61316 ),
 .UNSPECIFIED., .F., .F.,
 ( 4, 4 ),
 ( 0.000000000000000000, 0.1494581667962507632 ),
 .UNSPECIFIED. ) ;
#12740 = PLANE ( 'NONE',  #58252 ) ;
#12741 = CARTESIAN_POINT ( 'NONE',  ( 10.37309687351566723, -5.217465845835394411, 7.827184855449101697 ) ) ;
#12742 = EDGE_LOOP ( 'NONE', ( #48617, #41212, #26507, #46648 ) ) ;
#12743 = CARTESIAN_POINT ( 'NONE',  ( 9.447848023450999833, -5.447470167531999863, 7.431328114251999573 ) ) ;
#12744 = DIRECTION ( 'NONE',  ( 0.000000000000000000, -0.1333333333333049375, -0.9910712498212375099 ) ) ;
#12745 = CARTESIAN_POINT ( 'NONE',  ( 18.09739622856945118, -2.188708726578779906, 13.73458559203602469 ) ) ;
#12746 = VERTEX_POINT ( 'NONE', #43416 ) ;
#12747 = CARTESIAN_POINT ( 'NONE',  ( 10.10656234570999956, 4.887646627408000377, -6.257286147482000516 ) ) ;
#12748 =( LENGTH_UNIT ( ) NAMED_UNIT ( * ) SI_UNIT ( .MILLI., .METRE. ) );
#12749 = VERTEX_POINT ( 'NONE', #37465 ) ;
#12750 = CARTESIAN_POINT ( 'NONE',  ( 8.655265421554998895, 3.811499292588199861, 6.524915741324599949 ) ) ;
#12751 = CARTESIAN_POINT ( 'NONE',  ( 18.26225755805772977, -2.321011060852003371, -12.38438709824086459 ) ) ;
#12752 = B_SPLINE_CURVE_WITH_KNOTS ( 'NONE', 3,
 ( #51287, #56191, #4064, #30317 ),
 .UNSPECIFIED., .F., .F.,
 ( 4, 4 ),
 ( 0.4999999894681322887, 1.000000000000000000 ),
 .UNSPECIFIED. ) ;
#12753 = CARTESIAN_POINT ( 'NONE',  ( 24.51105662686868669, -3.208409238885217896, 11.97394890221126751 ) ) ;
#12754 = CYLINDRICAL_SURFACE ( 'NONE', #43910, 14.00000000000000000 ) ;
#12755 = CARTESIAN_POINT ( 'NONE',  ( 24.35365242081700288, 2.582848009905001074, 11.10541636514000174 ) ) ;
#12756 = EDGE_CURVE ( 'NONE', #9405, #14271, #32241, .T. ) ;
#12757 = CARTESIAN_POINT ( 'NONE',  ( 10.25944474310099785, 4.893483781708200198, 7.066400461213500073 ) ) ;
#12758 = CARTESIAN_POINT ( 'NONE',  ( 6.789185465859000068, -9.291930834867999422, -5.322879461504999909 ) ) ;
#12759 = ORIENTED_EDGE ( 'NONE', *, *, #55009, .T. ) ;
#12760 = CARTESIAN_POINT ( 'NONE',  ( 5.599959403262399604, 11.06886219213000011, -1.536526853569999851 ) ) ;
#12761 = CARTESIAN_POINT ( 'NONE',  ( 10.92546721959000067, 5.641524285727999910, -7.883474821562000301 ) ) ;
#12762 = B_SPLINE_CURVE_WITH_KNOTS ( 'NONE', 3,
 ( #30657, #68047, #41488, #25755 ),
 .UNSPECIFIED., .F., .F.,
 ( 4, 4 ),
 ( 0.000000000000000000, 1.000000000000000000 ),
 .UNSPECIFIED. ) ;
#12763 = AXIS2_PLACEMENT_3D ( 'NONE', #34764, #66902, #8870 ) ;
#12764 = CARTESIAN_POINT ( 'NONE',  ( 12.09999999999999964, -4.883784007588900522, 7.174999999999999822 ) ) ;
#12765 = CARTESIAN_POINT ( 'NONE',  ( 12.29779067500859568, 1.996199619003542258, -13.85695719179637031 ) ) ;
#12766 = CARTESIAN_POINT ( 'NONE',  ( 11.10434687351569494, -2.749999999999998224, 7.663624617374462211 ) ) ;
#12767 = CARTESIAN_POINT ( 'NONE',  ( 9.566960887370999700, -5.215923019114000247, 6.177729435798999802 ) ) ;
#12768 = CARTESIAN_POINT ( 'NONE',  ( 17.81326568215976636, 0.5695321295966297992, 13.88429381145915542 ) ) ;
#12769 = AXIS2_PLACEMENT_3D ( 'NONE', #33370, #54685, #33718 ) ;
#12770 = CARTESIAN_POINT ( 'NONE',  ( 24.69899731016300137, -3.637719133123000326, 12.18533670124999979 ) ) ;
#12771 = VERTEX_POINT ( 'NONE', #16143 ) ;
#12772 = ORIENTED_EDGE ( 'NONE', *, *, #48128, .F. ) ;
#12773 = CARTESIAN_POINT ( 'NONE',  ( 9.444964158775000840, 3.920043641733999884, -9.398198753036000497 ) ) ;
#12774 = CARTESIAN_POINT ( 'NONE',  ( 12.19608251854004166, 0.1421750971580202361, 13.89904149565881575 ) ) ;
#12775 = VECTOR ( 'NONE', #45320, 1000.000000000000114 ) ;
#12776 = CARTESIAN_POINT ( 'NONE',  ( 12.18865263574115509, -2.603587051922128914, 13.65094575296205903 ) ) ;
#12777 = CARTESIAN_POINT ( 'NONE',  ( 10.93769906941999892, 2.936877991120999898, -4.920829195977000303 ) ) ;
#12778 = CARTESIAN_POINT ( 'NONE',  ( 8.218894353209000414, -3.011617647609999615, 8.801438026873999121 ) ) ;
#12779 = CARTESIAN_POINT ( 'NONE',  ( 6.999999691988000095, -13.87069231928999891, 4.225386915259999654 ) ) ;
#12781 = CARTESIAN_POINT ( 'NONE',  ( 11.12438586031000121, -6.497919266103000524, 5.557820251765999586 ) ) ;
#12780 = CARTESIAN_POINT ( 'NONE',  ( 10.43765911260399903, -4.555852086785099786, 6.347865960448999090 ) ) ;
#12782 = CARTESIAN_POINT ( 'NONE',  ( 10.41964694612699915, 2.813019656517000477, -7.973702485506099613 ) ) ;
#12783 = ORIENTED_EDGE ( 'NONE', *, *, #61091, .T. ) ;
#12784 = FACE_OUTER_BOUND ( 'NONE', #8921, .T. ) ;
#12785 = CARTESIAN_POINT ( 'NONE',  ( 10.42374681322000107, -3.188261102799000213, -5.025588318470999738 ) ) ;
#12786 = CARTESIAN_POINT ( 'NONE',  ( 7.871384581343000342, 5.129340811002999878, 6.740051537885999977 ) ) ;
#12787 = B_SPLINE_SURFACE_WITH_KNOTS ( 'NONE', 3, 3, ( 
 ( #4411, #25750, #47079, #61772, #18795, #3721, #19123, #25058, #35562, #61436, #13556, #29644, #13893, #8637, #24720, #67693, #46044, #56878, #37270, #208, #47773, #42518, #20501, #32719, #21869, #48452, #32382, #57909, #36935, #20848, #43206, #15260, #36583, #10692, #47421 ),
 ( #10007, #31345, #54031, #53696, #58248, #4754, #16284, #16629, #27472, #10352, #5106, #21528, #68729, #37955, #15603, #69082, #6133, #64509, #42861, #58592, #63827, #21187, #26443, #5789, #15941, #32039, #52658, #59276, #53354, #11047, #5457, #31688, #26792, #27132, #64170 ),
 ( #53009, #11378, #48108, #42181, #68380, #41826, #63134, #26096, #37609, #58940, #560, #63484, #22219, #48797, #66247, #6831, #12082, #16967, #12778, #39004, #906, #28163, #38649, #7182, #22906, #7873, #55426, #1247, #7517, #28872, #59972, #13130, #28519, #49830, #18369 ),
 ( #17679, #33413, #39691, #61012, #44606, #50180, #22561, #34458, #60321, #11722, #12430, #44260, #2283, #55076, #33064, #33761, #17323, #43903, #55771, #1943, #23262, #23601, #65899, #43555, #18027, #64856, #39342, #60663, #44942, #54730, #49479, #34107, #38298, #59628, #54380 ) ),
 .UNSPECIFIED., .F., .F., .F.,
 ( 4, 4 ),
 ( 4, 1, 1, 1, 1, 1, 1, 1, 1, 1, 1, 1, 1, 1, 1, 1, 1, 1, 1, 1, 1, 1, 1, 1, 1, 1, 1, 1, 1, 1, 1, 1, 4 ),
 ( -0.1039086239011999951, 1.103908623900999864 ),
 ( -0.02000000000000000042, 0.01250000000000000069, 0.04499999999999999833, 0.07749999999999999944, 0.1100000000000000006, 0.1424999999999999878, 0.1749999999999999889, 0.2074999999999999900, 0.2399999999999999911, 0.2725000000000000200, 0.3049999999999999933, 0.3375000000000000222, 0.3699999999999999956, 0.4025000000000000244, 0.4349999999999999978, 0.4675000000000000266, 0.5000000000000000000, 0.5324999999999999734, 0.5649999999999999467, 0.5975000000000000311, 0.6300000000000000044, 0.6624999999999999778, 0.6949999999999999512, 0.7275000000000000355, 0.7600000000000000089, 0.7924999999999999822, 0.8249999999999999556, 0.8575000000000000400, 0.8900000000000000133, 0.9224999999999999867, 0.9549999999999999600, 0.9875000000000000444, 1.020000000000000018 ),
 .UNSPECIFIED. ) ;
#12788 = CARTESIAN_POINT ( 'NONE',  ( 12.49451986944247217, -0.5425047576885997369, 12.68440192076777961 ) ) ;
#12789 = CARTESIAN_POINT ( 'NONE',  ( 4.149992563292000725, 2.000000000000000000, 0.000000000000000000 ) ) ;
#12790 = VERTEX_POINT ( 'NONE', #47624 ) ;
#12792 = CARTESIAN_POINT ( 'NONE',  ( 9.587317385018980787, 5.286614015217494078, -7.026982148269482309 ) ) ;
#12791 = CARTESIAN_POINT ( 'NONE',  ( 11.61486084871780022, -2.792989229543000107, 7.825000000000000178 ) ) ;
#12793 = CARTESIAN_POINT ( 'NONE',  ( 9.260829719593999698, 4.861259245430999520, -8.806664389576001284 ) ) ;
#12794 = EDGE_CURVE ( 'NONE', #1019, #10847, #5946, .T. ) ;
#12795 = CARTESIAN_POINT ( 'NONE',  ( 12.43812277102956010, -1.993632728549934230, 13.76791003216514575 ) ) ;
#12796 = CARTESIAN_POINT ( 'NONE',  ( 10.24733997687999931, 4.272363749081500295, 8.748653021963999521 ) ) ;
#12797 = AXIS2_PLACEMENT_3D ( 'NONE', #68069, #3415, #67384 ) ;
#12798 = CARTESIAN_POINT ( 'NONE',  ( 13.70005190196300227, -9.005348107749998832, -7.391036106496999381 ) ) ;
#12799 = B_SPLINE_SURFACE_WITH_KNOTS ( 'NONE', 1, 3, ( 
 ( #11211, #32547, #62959, #63656, #58415, #64333, #378, #27299, #16452, #53525, #37438, #5615, #10184, #26617, #59105, #16112, #20326, #21020, #47596, #15086, #20674, #63994, #10520, #26267, #42005, #47937, #63307, #5960, #26958, #31181, #48623, #31513, #25919, #47249, #52486, #68904, #53175, #4582, #42686, #37781, #53860, #41653, #15772, #36411, #48272, #15434, #52835, #4931, #65378, #43383, #65726, #726, #1414, #27995, #64683, #48966, #44429, #17500, #6653, #22387, #28335, #1074, #55598, #33928, #38121, #7699, #38473, #6300, #27646, #11545, #49302, #12255, #32889, #1763, #18192, #44771, #23432, #22730, #39513, #33584, #54199, #49655, #60491, #38823, #16793, #39168, #59448, #12600, #17140, #23082, #43726, #7002, #2115, #54901, #59794, #44080, #34278, #65024, #60149, #17850, #22037, #55249, #7346, #28691, #50004, #33236, #11898, #29040, #66071, #60837, #12950, #54556 ),
 ( #24466, #66766, #2450, #61185, #62543, #24810, #56283, #35651, #46135, #14328, #50350, #18881, #30072, #23775, #56963, #14664, #8389, #29732, #51375, #35308, #46478, #41233, #45109, #35980, #66417, #67440, #30404, #57298, #8730, #18536, #19212, #67786, #51036, #19908, #39865, #9400, #19563, #61525, #9065, #40209, #2793, #34627, #13305, #50696, #13640, #34966, #51716, #55940, #8042, #29385, #3136, #67104, #3808, #25147, #24118, #45452, #40885, #62206, #45791, #40538, #56626, #61862, #13983, #3473, #10780, #37699, #32125, #69165, #47859, #21276, #47165, #15690, #294, #26531, #30743, #31432, #57997, #25494, #9748, #5193, #47511, #36678, #52403, #58333, #31096, #16370, #63915, #68129, #59029, #68466, #36327, #57642, #41571, #10098, #42272, #62881, #31777, #48192, #5538, #53441, #52749, #21614, #63576, #15001, #10437, #42604, #26185, #4154, #16027, #46823, #37356, #20589 ) ),
 .UNSPECIFIED., .F., .F., .F.,
 ( 2, 2 ),
 ( 4, 2, 2, 2, 2, 2, 2, 2, 2, 2, 2, 2, 2, 2, 2, 2, 2, 2, 2, 2, 2, 2, 2, 2, 2, 2, 2, 2, 2, 2, 2, 2, 2, 2, 2, 2, 2, 2, 2, 2, 2, 2, 2, 2, 2, 2, 2, 2, 2, 2, 2, 2, 2, 2, 2, 4 ),
 ( 0.000000000000000000, 1.000000000000000000 ),
 ( 0.000000000000000000, 7.083325941644275862E-05, 0.0001416665188328855172, 0.0002124997782493282623, 0.0002479164079575496213, 0.0002833330376657710345, 0.0003187496673739924477, 0.0003541662970822138067, 0.0004249995564986565246, 0.0004604161862068778836, 0.0004781245010609885631, 0.0004958328159150992426, 0.0005312494456233207100, 0.0005666660753315420690, 0.0006374993347479848953, 0.0006729159644562062543, 0.0007083325941644276133, 0.0007437492238726489723, 0.0007791658535808703313, 0.0008145824832890916902, 0.0008499991129973130492, 0.0008854157427055344082, 0.0009208323724137557672, 0.0009562490021219771262, 0.0009916656318301984852, 0.001027082261538419953, 0.001062498891246641420, 0.001133332150663084138, 0.001168748780371305605, 0.001204165410079526856, 0.001239582039787748323, 0.001274998669495969791, 0.001345831928912412509, 0.001381248558620633976, 0.001416665188328855227, 0.001452081818037076477, 0.001469790132891187102, 0.001487498447745297945, 0.001558331707161740663, 0.001629164966578183380, 0.001664581596286404848, 0.001699998225994626098, 0.001735414855702847349, 0.001770831485411068816, 0.001841664744827511534, 0.001877081374535732785, 0.001912498004243954252, 0.001947914633952175720, 0.001983331263660396970, 0.002018747893368618221, 0.002054164523076839905, 0.002124997782493282840, 0.002160414412201504090, 0.002195831041909725341, 0.002231247671617946592, 0.002266664301326168276 ),
 .UNSPECIFIED. ) ;
#12800 = DIRECTION ( 'NONE',  ( 1.000000000000000000, 0.000000000000000000, 0.000000000000000000 ) ) ;
#12801 = CARTESIAN_POINT ( 'NONE',  ( 3.215157995114000133, 1.238879411953999865, 3.371798807325999903 ) ) ;
#12802 = ORIENTED_EDGE ( 'NONE', *, *, #12143, .T. ) ;
#12803 = CARTESIAN_POINT ( 'NONE',  ( 12.21516876105738092, 0.4188397444781323808, -12.59305179380755035 ) ) ;
#12804 = CARTESIAN_POINT ( 'NONE',  ( 5.399998535875000449, 2.451372438371999805E-13, 6.461498003317998333E-14 ) ) ;
#12805 = CARTESIAN_POINT ( 'NONE',  ( 24.16198515854589246, -12.44540882913624635, -3.348940053833783015 ) ) ;
#12806 = CARTESIAN_POINT ( 'NONE',  ( 8.347267219593000220, 2.741641653469999884, 6.457329666915000210 ) ) ;
#12807 = ORIENTED_EDGE ( 'NONE', *, *, #30229, .T. ) ;
#12808 = CARTESIAN_POINT ( 'NONE',  ( 5.824162447775000473, -0.7240778834237999728, 1.106429931180000104 ) ) ;
#12809 = CARTESIAN_POINT ( 'NONE',  ( 10.95457883563474155, 9.034768305091144924, 6.398572458980741118 ) ) ;
#12810 = EDGE_CURVE ( 'NONE', #3072, #33524, #63395, .T. ) ;
#12812 = CARTESIAN_POINT ( 'NONE',  ( 10.67956456102485951, 4.176706786694609264, -8.849774126559262655 ) ) ;
#12811 = FACE_OUTER_BOUND ( 'NONE', #57862, .T. ) ;
#12813 = AXIS2_PLACEMENT_3D ( 'NONE', #3291, #9561, #52214 ) ;
#12814 = CARTESIAN_POINT ( 'NONE',  ( 11.03776249210999971, -8.050323671732000363, -6.914613055281999543 ) ) ;
#12815 = VERTEX_POINT ( 'NONE', #10896 ) ;
#12816 = CARTESIAN_POINT ( 'NONE',  ( 11.09999999999999964, -4.000000000000000000, 7.500000000000000000 ) ) ;
#12817 = EDGE_LOOP ( 'NONE', ( #32319, #19812, #56249, #2815 ) ) ;
#12818 = EDGE_CURVE ( 'NONE', #54214, #42540, #6822, .T. ) ;
#12819 = CARTESIAN_POINT ( 'NONE',  ( 9.489492991957288126, -4.926916480655023634, 8.481281896443434221 ) ) ;
#12820 = FACE_OUTER_BOUND ( 'NONE', #39149, .T. ) ;
#12821 = AXIS2_PLACEMENT_3D ( 'NONE', #36818, #5332, #26326 ) ;
#12822 = CARTESIAN_POINT ( 'NONE',  ( 18.26841422636659118, -0.1308528744652316944, -13.99939340647621222 ) ) ;
#12823 = VERTEX_POINT ( 'NONE', #11574 ) ;
#12824 = CARTESIAN_POINT ( 'NONE',  ( 10.92934437010315740, 9.489520708315478004, -6.090896311640516814 ) ) ;
#12825 = CARTESIAN_POINT ( 'NONE',  ( 18.30003129332100187, 2.732683818840999646, 11.53064095373000164 ) ) ;
#12826 = DIRECTION ( 'NONE',  ( -1.000000000000000000, 1.776356839322000196E-14, -1.776356839322000196E-14 ) ) ;
#12827 = CARTESIAN_POINT ( 'NONE',  ( 9.906851002540999929, 2.832432432432000269, -6.822293592207000934 ) ) ;
#12828 = CARTESIAN_POINT ( 'NONE',  ( 18.15150620825778205, -2.686947401731335283, 12.40607332096686655 ) ) ;
#12829 = ORIENTED_EDGE ( 'NONE', *, *, #48885, .F. ) ;
#12830 = CARTESIAN_POINT ( 'NONE',  ( 8.577614158774000686, 3.981661882377999895, 8.959227447876999761 ) ) ;
#12831 = CARTESIAN_POINT ( 'NONE',  ( 12.47184101605662931, -3.029124285173875997, -13.54683579967691998 ) ) ;
#12832 = DIRECTION ( 'NONE',  ( -1.000000000000000000, 0.000000000000000000, 0.000000000000000000 ) ) ;
#12833 = CARTESIAN_POINT ( 'NONE',  ( 17.55505043854147118, -1.875000000000000000, 12.57545641911172396 ) ) ;
#12834 = ORIENTED_EDGE ( 'NONE', *, *, #25050, .F. ) ;
#12835 = CARTESIAN_POINT ( 'NONE',  ( 10.70259541447426344, -2.712334124290769921, 7.031803886929559155 ) ) ;
#12836 = DIRECTION ( 'NONE',  ( 0.000000000000000000, -1.000000000000000000, 0.000000000000000000 ) ) ;
#12837 = CARTESIAN_POINT ( 'NONE',  ( 5.700000000000000178, 11.06886219213000011, 1.536526853569999851 ) ) ;
#12838 = CARTESIAN_POINT ( 'NONE',  ( 23.71897770753286849, -3.252386419300755893, -13.29323848889808701 ) ) ;
#12839 = CARTESIAN_POINT ( 'NONE',  ( 24.59999999957999961, 2.749830087550999854E-09, -4.999999999859999988 ) ) ;
#12840 = EDGE_CURVE ( 'NONE', #37115, #28639, #40143, .T. ) ;
#12841 = LINE ( 'NONE', #60036, #52052 ) ;
#12842 = CARTESIAN_POINT ( 'NONE',  ( 17.72806902343761948, -3.100663240735258341, 12.29112607895899068 ) ) ;
#12843 = ORIENTED_EDGE ( 'NONE', *, *, #2139, .T. ) ;
#12844 = CARTESIAN_POINT ( 'NONE',  ( 11.11123293495519881, -4.891405920092699589, -7.464165716332529676 ) ) ;
#12845 = ORIENTED_EDGE ( 'NONE', *, *, #13767, .T. ) ;
#12846 = CARTESIAN_POINT ( 'NONE',  ( 6.999999691988000095, -1.332267629549999942E-14, 1.576516694967999966E-14 ) ) ;
#12847 = CARTESIAN_POINT ( 'NONE',  ( 7.169256274120943573, 0.2499999999999997224, -3.082564036157278586 ) ) ;
#12848 = CARTESIAN_POINT ( 'NONE',  ( 3.167073505399999878, 1.530628728318999876, -2.827318827580999727 ) ) ;
#12849 = CARTESIAN_POINT ( 'NONE',  ( 10.90421209872000041, -3.863781031729999871, -9.185081053980001187 ) ) ;
#12850 = CARTESIAN_POINT ( 'NONE',  ( 11.50000000000000000, -3.008232475376599879, 7.825000000000000178 ) ) ;
#12851 = AXIS2_PLACEMENT_3D ( 'NONE', #15329, #58316, #42253 ) ;
#12852 = LINE ( 'NONE', #2016, #22731 ) ;
#12853 = CARTESIAN_POINT ( 'NONE',  ( 11.42394752546313441, 3.297753801639562443, 6.396140797112706444 ) ) ;
#12854 = ORIENTED_EDGE ( 'NONE', *, *, #35325, .T. ) ;
#12855 = CARTESIAN_POINT ( 'NONE',  ( 18.02410434383600091, 3.285250940561000199, 11.23276246309000115 ) ) ;
#12856 = CARTESIAN_POINT ( 'NONE',  ( 11.69102897915239936, -3.743141152489600110, 6.529961657816500065 ) ) ;
#12857 = CARTESIAN_POINT ( 'NONE',  ( 10.50285691784999997, 5.158890929072000198, 8.369954994793999958 ) ) ;
#12858 = LINE ( 'NONE', #50946, #50494 ) ;
#12859 = CARTESIAN_POINT ( 'NONE',  ( 8.736413463905998711, -3.915843685459630574, -8.382409559052598880 ) ) ;
#12861 = B_SPLINE_CURVE_WITH_KNOTS ( 'NONE', 3,
 ( #58921, #63462, #20824, #42161, #15585, #537, #43184, #26423, #42840, #63809, #64150, #31668, #64488, #16610, #52990, #5086, #47749, #69064, #37935, #31324, #5435, #21170, #15918, #10675, #32022, #26775, #66442, #18214, #29063, #38852, #28018 ),
 .UNSPECIFIED., .F., .F.,
 ( 4, 2, 2, 1, 1, 2, 2, 2, 1, 2, 2, 2, 2, 2, 2, 2, 4 ),
 ( 0.000000000000000000, 0.06250000000001527944, 0.09375000000002210732, 0.1093750000000244527, 0.1171875000000244943, 0.1210937500000246470, 0.1250000000000247857, 0.1875000000000223710, 0.2187500000000211775, 0.2343750000000196232, 0.2500000000000180966, 0.3750000000000170974, 0.4375000000000169309, 0.4687500000000165978, 0.5000000000000163203, 0.7500000000000081046, 1.000000000000000000 ),
 .UNSPECIFIED. ) ;
#12860 = CYLINDRICAL_SURFACE ( 'NONE', #10535, 0.4999999999999998335 ) ;
#12862 = CARTESIAN_POINT ( 'NONE',  ( 10.62903166480609940, 3.135947233695900227, -7.560921321260908989 ) ) ;
#12863 = CARTESIAN_POINT ( 'NONE',  ( 10.99161758052705196, 2.805470275078409514, -6.623309719462226575 ) ) ;
#12864 = AXIS2_PLACEMENT_3D ( 'NONE', #24271, #6806, #56085 ) ;
#12865 = CARTESIAN_POINT ( 'NONE',  ( 9.986304848515999311, 5.038423216181000086, -7.974775391194199869 ) ) ;
#12866 = CARTESIAN_POINT ( 'NONE',  ( 23.61807764069600069, -10.28177138180000050, 9.268757862392000391 ) ) ;
#12867 = B_SPLINE_CURVE_WITH_KNOTS ( 'NONE', 3,
 ( #68341, #35857, #63092, #52970 ),
 .UNSPECIFIED., .F., .F.,
 ( 4, 4 ),
 ( 0.000000000000000000, 1.000000000000000000 ),
 .UNSPECIFIED. ) ;
#12868 = CARTESIAN_POINT ( 'NONE',  ( 0.8957314031238002849, 0.8639796672389500332, -3.414949893371867606 ) ) ;
#12869 = CARTESIAN_POINT ( 'NONE',  ( 10.52384528040999889, 5.441915759804999198, -7.989632847918000103 ) ) ;
#12870 = ORIENTED_EDGE ( 'NONE', *, *, #16275, .F. ) ;
#12871 = CARTESIAN_POINT ( 'NONE',  ( 8.143316940379001778, -5.061720701958000390, 5.824087910811999613 ) ) ;
#12872 = ADVANCED_FACE ( 'NONE', ( #32917 ), #49333, .F. ) ;
#12873 = EDGE_CURVE ( 'NONE', #25668, #38871, #31848, .T. ) ;
#12874 = CARTESIAN_POINT ( 'NONE',  ( 17.65774109649147050, 3.116847231231422821, 13.52303903038508182 ) ) ;
#12875 = CARTESIAN_POINT ( 'NONE',  ( 23.60205915885299888, -2.171992490524999209, 12.06370038613999718 ) ) ;
#12876 = CARTESIAN_POINT ( 'NONE',  ( 10.39503166480599994, -5.274847857784000560, -7.589885038193400213 ) ) ;
#12877 = ORIENTED_EDGE ( 'NONE', *, *, #42020, .T. ) ;
#12878 = EDGE_CURVE ( 'NONE', #25292, #48209, #11766, .T. ) ;
#12879 = CARTESIAN_POINT ( 'NONE',  ( 9.091114158770999154, 3.762712042852999872, 8.787816121229999666 ) ) ;
#12881 = CARTESIAN_POINT ( 'NONE',  ( 0.6354672858397831803, 1.708930379032600699, 3.099689759355926277 ) ) ;
#12880 = CARTESIAN_POINT ( 'NONE',  ( 10.24457120343299898, -4.042028078047379402, -8.365991721916298474 ) ) ;
#12882 = CARTESIAN_POINT ( 'NONE',  ( 10.00190165877000048, 2.729646201450000031, -8.843033333815998986 ) ) ;
#12883 = ORIENTED_EDGE ( 'NONE', *, *, #8830, .F. ) ;
#12884 = CARTESIAN_POINT ( 'NONE',  ( 10.74599736040000053, 5.242718773683000322, 8.978699897073999736 ) ) ;
#12885 = CARTESIAN_POINT ( 'NONE',  ( 17.96944589180085572, -3.117220005880608547, -13.64855254614797531 ) ) ;
#12886 = CARTESIAN_POINT ( 'NONE',  ( 10.39918582084299992, 3.253651555277099927, 8.362701637490498996 ) ) ;
#12887 = CARTESIAN_POINT ( 'NONE',  ( 10.72520823780999955, -5.521647200017000934, 6.612992938078999572 ) ) ;
#12888 = CARTESIAN_POINT ( 'NONE',  ( 8.513433059625000965, -5.040796345420999636, 8.522966281393001609 ) ) ;
#12889 = EDGE_LOOP ( 'NONE', ( #30341, #52691, #45642, #10308 ) ) ;
#12890 = PLANE ( 'NONE',  #41094 ) ;
#12891 = CARTESIAN_POINT ( 'NONE',  ( 1.355140132541249764, -0.9161175952574772685, -3.408904368339104707 ) ) ;
#12892 = EDGE_CURVE ( 'NONE', #12470, #60343, #44112, .T. ) ;
#12893 = CARTESIAN_POINT ( 'NONE',  ( 7.944408677273556485, -2.261289390559563905, 7.612513792833588866 ) ) ;
#12894 = CARTESIAN_POINT ( 'NONE',  ( 10.65550933554000146, -4.237674644795000667, 9.105223721671999115 ) ) ;
#12895 = CARTESIAN_POINT ( 'NONE',  ( 11.67766954483535891, -3.284117569315500251, -6.395429936871999566 ) ) ;
#12896 = CARTESIAN_POINT ( 'NONE',  ( 9.778038493599000347, -3.173653894988100355, 8.287963554181398962 ) ) ;
#12897 = ORIENTED_EDGE ( 'NONE', *, *, #52393, .F. ) ;
#12898 = CARTESIAN_POINT ( 'NONE',  ( 24.74119899597345551, -11.75041001041740429, -3.191107525484343732 ) ) ;
#12899 = CARTESIAN_POINT ( 'NONE',  ( 11.48579841651039857, -4.449968941611500028, 6.303820944768999901 ) ) ;
#12900 = ORIENTED_EDGE ( 'NONE', *, *, #40069, .T. ) ;
#12901 = EDGE_CURVE ( 'NONE', #10058, #53044, #8078, .T. ) ;
#12902 = CARTESIAN_POINT ( 'NONE',  ( 18.36651216305132905, -2.877244130631001262, -12.05316132863760181 ) ) ;
#12903 = ORIENTED_EDGE ( 'NONE', *, *, #4121, .T. ) ;
#12904 = CARTESIAN_POINT ( 'NONE',  ( 9.839739029020998728, -5.130141620686999637, -6.219151643305999677 ) ) ;
#12905 = CARTESIAN_POINT ( 'NONE',  ( 9.740360841231000322, 4.047146749018000200, -5.600703114891000034 ) ) ;
#12906 = CARTESIAN_POINT ( 'NONE',  ( 10.72191429142990060, 4.025072603369280522, -6.183971186511000084 ) ) ;
#12907 = CARTESIAN_POINT ( 'NONE',  ( 24.30000000000000071, 2.204728229456999866, -11.99913219504999873 ) ) ;
#12908 = CARTESIAN_POINT ( 'NONE',  ( 12.50301483199531916, 3.134404823497599413, -12.20391382861247287 ) ) ;
#12909 = CARTESIAN_POINT ( 'NONE',  ( 11.42026088462129962, -3.997864853650589634, 8.503467136482999678 ) ) ;
#12910 = CARTESIAN_POINT ( 'NONE',  ( 11.69434208742519843, -4.478858766422799675, 6.747282993577999655 ) ) ;
#12911 = ORIENTED_EDGE ( 'NONE', *, *, #19425, .T. ) ;
#12912 = CARTESIAN_POINT ( 'NONE',  ( 5.070886616771334232, -1.393043258182025568, 0.6426200619446649220 ) ) ;
#12913 = VERTEX_POINT ( 'NONE', #40239 ) ;
#12914 = CARTESIAN_POINT ( 'NONE',  ( 8.508081853209001011, -2.202816532622999812, 7.706987678916999762 ) ) ;
#12915 = CARTESIAN_POINT ( 'NONE',  ( 17.74278521987943336, 0.7069209314886554241, 13.98214394338196165 ) ) ;
#12916 = ORIENTED_EDGE ( 'NONE', *, *, #30125, .T. ) ;
#12917 = CARTESIAN_POINT ( 'NONE',  ( 12.11850681454236245, -2.712075317534410335, -12.30466467946555653 ) ) ;
#12919 = CARTESIAN_POINT ( 'NONE',  ( 10.47718582084299932, 3.343463760027599818, 8.258888014436699621 ) ) ;
#12918 = CIRCLE ( 'NONE', #54218, 12.20000000000000107 ) ;
#12920 = CARTESIAN_POINT ( 'NONE',  ( 23.60205915885299888, 2.171992490524999209, -12.06370038613999718 ) ) ;
#12921 = CARTESIAN_POINT ( 'NONE',  ( 9.268025422169147376, 5.100000000000000533, 6.452077467066149374 ) ) ;
#12922 = B_SPLINE_CURVE_WITH_KNOTS ( 'NONE', 3,
 ( #55981, #66811, #7388, #65767 ),
 .UNSPECIFIED., .F., .F.,
 ( 4, 4 ),
 ( 0.000000000000000000, 1.000000000000000000 ),
 .UNSPECIFIED. ) ;
#12923 = CARTESIAN_POINT ( 'NONE',  ( 18.14133394217200390, -11.74923367482999836, 3.582907174652000037 ) ) ;
#12924 = CARTESIAN_POINT ( 'NONE',  ( 8.183771503764621258, -2.796787595787157521, 8.203896902613195152 ) ) ;
#12925 = CARTESIAN_POINT ( 'NONE',  ( 12.39904396558118016, -2.975276281382168264, -13.56103672317925124 ) ) ;
#12926 = CARTESIAN_POINT ( 'NONE',  ( 18.17808098948988516, -0.05063260980701731612, -12.69986973508909323 ) ) ;
#12927 = CARTESIAN_POINT ( 'NONE',  ( 11.12133729122639991, -4.865898216891100247, -7.477221318588949117 ) ) ;
#12928 = CARTESIAN_POINT ( 'NONE',  ( 10.86687616594229944, -4.344946439135400240, -6.412662853391999818 ) ) ;
#12929 = CARTESIAN_POINT ( 'NONE',  ( 9.342517219591000455, 5.057081813675999626, 8.967637988488998957 ) ) ;
#12930 = ORIENTED_EDGE ( 'NONE', *, *, #37092, .T. ) ;
#12931 = FILL_AREA_STYLE_COLOUR ( '', #41035 ) ;
#12932 = CARTESIAN_POINT ( 'NONE',  ( 24.63002439619599926, 0.000000000000000000, 0.000000000000000000 ) ) ;
#12933 = DIRECTION ( 'NONE',  ( 1.000000000000000000, 0.000000000000000000, 0.000000000000000000 ) ) ;
#12934 = CARTESIAN_POINT ( 'NONE',  ( 23.58682091624699950, -3.020374421963000433, 13.60611292239000036 ) ) ;
#12935 = CARTESIAN_POINT ( 'NONE',  ( 17.74796797082749578, 1.905496177146738690, 12.57037238745254726 ) ) ;
#12936 = ADVANCED_FACE ( 'NONE', ( #55283 ), #44469, .F. ) ;
#12937 = CARTESIAN_POINT ( 'NONE',  ( 11.07074944260999949, 5.433295094434000383, 5.078291584939999659 ) ) ;
#12938 = EDGE_CURVE ( 'NONE', #3039, #2005, #36793, .T. ) ;
#12939 = CARTESIAN_POINT ( 'NONE',  ( 10.18756025349000005, 5.387489739490000318, 8.640945789268998922 ) ) ;
#12940 = B_SPLINE_CURVE_WITH_KNOTS ( 'NONE', 1,
 ( #34302, #33610 ),
 .UNSPECIFIED., .F., .F.,
 ( 2, 2 ),
 ( 0.000000000000000000, 1.000000000000000000 ),
 .UNSPECIFIED. ) ;
#12941 = CARTESIAN_POINT ( 'NONE',  ( 9.600254395947626307, -4.850975458930337325, 7.703403631282998099 ) ) ;
#12942 = CARTESIAN_POINT ( 'NONE',  ( 8.749283493600000128, 4.089987329977850194, 6.649720865199900466 ) ) ;
#12943 = ORIENTED_EDGE ( 'NONE', *, *, #34508, .T. ) ;
#12944 = CARTESIAN_POINT ( 'NONE',  ( 12.27200335545532894, -2.173637791136410424, 12.52166559990193662 ) ) ;
#12945 = CARTESIAN_POINT ( 'NONE',  ( 9.047113844317999920, -3.746347404385800051, -6.528144732449299603 ) ) ;
#12946 = CARTESIAN_POINT ( 'NONE',  ( 9.569805421428000614, 4.064052243276000453, 8.919241792616000808 ) ) ;
#12947 = CARTESIAN_POINT ( 'NONE',  ( 9.301820635884373800, -3.939853377893446584, 6.549596649571864937 ) ) ;
#12948 = VECTOR ( 'NONE', #8104, 1000.000000000000000 ) ;
#12949 = CARTESIAN_POINT ( 'NONE',  ( 11.62579573085663043, 5.239377455231000624, -7.714452430741599365 ) ) ;
#12950 = CARTESIAN_POINT ( 'NONE',  ( 12.79307474260548538, -0.7192913015564696977, 12.57945229205062709 ) ) ;
#12951 = AXIS2_PLACEMENT_3D ( 'NONE', #35064, #19307, #29827 ) ;
#12952 = CARTESIAN_POINT ( 'NONE',  ( 8.866801658774001282, 2.550580605805000012, 8.854682662413999594 ) ) ;
#12953 = CARTESIAN_POINT ( 'NONE',  ( 10.09197164456000095, 3.841384681542000301, 5.536408945990000774 ) ) ;
#12954 = LINE ( 'NONE', #46138, #14345 ) ;
#12955 = VERTEX_POINT ( 'NONE', #54587 ) ;
#12956 = CARTESIAN_POINT ( 'NONE',  ( 9.246064158776000852, 5.200883864107000321, -6.027780766890000308 ) ) ;
#12957 = CARTESIAN_POINT ( 'NONE',  ( 10.69041504065829962, 5.024558373595999328, -6.736065107693399945 ) ) ;
#12958 = SHAPE_REPRESENTATION ( 'O Ring Seal 3', ( #9676 ), #806 ) ;
#12959 = ADVANCED_FACE ( 'NONE', ( #65759 ), #38865, .F. ) ;
#12960 = ADVANCED_FACE ( 'NONE', ( #33615 ), #67892, .T. ) ;
#12961 = CARTESIAN_POINT ( 'NONE',  ( 5.440308476675333793, -0.1973919536007288644, 1.504917372998084923 ) ) ;
#12963 = CARTESIAN_POINT ( 'NONE',  ( 25.09890003032761641, 11.37374245467410461, 3.274683916523300375 ) ) ;
#12962 = CARTESIAN_POINT ( 'NONE',  ( 8.368316940379001423, -4.780993534312999671, 6.267212032957000467 ) ) ;
#12964 = CARTESIAN_POINT ( 'NONE',  ( 9.706076168957999073, -4.439974903344300117, 6.752918994396699404 ) ) ;
#12965 = CARTESIAN_POINT ( 'NONE',  ( 11.61364291764652812, -4.859654669415900408, -7.393734108507599601 ) ) ;
#12966 = ORIENTED_EDGE ( 'NONE', *, *, #56357, .F. ) ;
#12967 = CONICAL_SURFACE ( 'NONE', #29698, 12.47499939740000130, 0.7853981102588313279 ) ;
#12968 = EDGE_CURVE ( 'NONE', #56572, #26364, #54473, .T. ) ;
#12969 = CARTESIAN_POINT ( 'NONE',  ( 1.214883236251000032, 2.900008637959000435, -1.487022697228999935 ) ) ;
#12970 = CARTESIAN_POINT ( 'NONE',  ( 12.62607976188088799, 11.85836615252178916, -3.313854784738079484 ) ) ;
#12971 = CIRCLE ( 'NONE', #21876, 1.000000000000000000 ) ;
#12972 = CARTESIAN_POINT ( 'NONE',  ( 5.700000000000000178, -13.94845324556000143, -4.312847325879000770 ) ) ;
#12973 = CARTESIAN_POINT ( 'NONE',  ( 11.09999999999999964, -4.000000000000000000, -7.500000000000000000 ) ) ;
#12974 = CARTESIAN_POINT ( 'NONE',  ( 7.721047347516135417, 2.916517638618118635, 6.666908946472835495 ) ) ;
#12975 = CARTESIAN_POINT ( 'NONE',  ( 12.47175297079834699, -3.166474622353419921, 13.63720910406326858 ) ) ;
#12976 = CARTESIAN_POINT ( 'NONE',  ( 24.30001697352500045, -3.271769158411000245, -12.21048181092999840 ) ) ;
#12977 = CARTESIAN_POINT ( 'NONE',  ( 9.411512147430608266, -5.333029039908475433, 7.282975621311138070 ) ) ;
#12978 = CARTESIAN_POINT ( 'NONE',  ( 13.26944243593800010, -12.10482456369999937, -2.110592202804000284 ) ) ;
#12979 = ORIENTED_EDGE ( 'NONE', *, *, #14606, .F. ) ;
#12980 = DIRECTION ( 'NONE',  ( 1.000000000000000000, 0.000000000000000000, -1.776356839484000040E-14 ) ) ;
#12981 = CARTESIAN_POINT ( 'NONE',  ( 10.85939066991000068, 5.063022199667999601, 5.180095919022000395 ) ) ;
#12982 = CARTESIAN_POINT ( 'NONE',  ( 7.430335179696497150, -2.310327096630513832, 7.914026420381109261 ) ) ;
#12983 = CARTESIAN_POINT ( 'NONE',  ( 17.75510503588994737, -0.5924680672155933081, 13.88300198247031503 ) ) ;
#12984 = CARTESIAN_POINT ( 'NONE',  ( 1.466702730658999920, 2.711246897165000114, -2.603366577799000048 ) ) ;
#12985 = ORIENTED_EDGE ( 'NONE', *, *, #37473, .T. ) ;
#12986 = CARTESIAN_POINT ( 'NONE',  ( 0.07497316781761000082, 0.000000000000000000, 0.000000000000000000 ) ) ;
#12987 = ADVANCED_FACE ( 'NONE', ( #35001 ), #9434, .F. ) ;
#12988 = DIRECTION ( 'NONE',  ( -1.000000000000000000, 0.000000000000000000, 0.000000000000000000 ) ) ;
#12989 = CYLINDRICAL_SURFACE ( 'NONE', #3061, 0.5000000000000028866 ) ;
#12990 = CARTESIAN_POINT ( 'NONE',  ( 11.31410538575739899, 4.975963290822400076, 7.733337754805098996 ) ) ;
#12991 = DIRECTION ( 'NONE',  ( -1.000000000000000000, 0.000000000000000000, 2.886579864060000134E-14 ) ) ;
#12992 = CARTESIAN_POINT ( 'NONE',  ( 10.42511694037999881, -3.371058793856000158, -6.294333763729999198 ) ) ;
#12993 = CARTESIAN_POINT ( 'NONE',  ( 15.89979320884932967, -8.154023814690269489, -9.295983641917322515 ) ) ;
#12994 = CARTESIAN_POINT ( 'NONE',  ( 0.4921978635424994475, 2.476206882760971340, -2.521572608111618319 ) ) ;
#12995 = CARTESIAN_POINT ( 'NONE',  ( 12.22895615649426482, -2.742396662243991035, 12.39180484751770095 ) ) ;
#12996 = VERTEX_POINT ( 'NONE', #57675 ) ;
#12998 = CARTESIAN_POINT ( 'NONE',  ( 8.338298982574256613, 3.701651498039506549, 9.235001345112676674 ) ) ;
#12997 = B_SPLINE_CURVE_WITH_KNOTS ( 'NONE', 3,
 ( #63275, #3862, #47218, #42325 ),
 .UNSPECIFIED., .F., .F.,
 ( 4, 4 ),
 ( 0.000000000000000000, 1.000000000000000000 ),
 .UNSPECIFIED. ) ;
#12999 = ORIENTED_EDGE ( 'NONE', *, *, #47460, .T. ) ;
#13000 = CARTESIAN_POINT ( 'NONE',  ( 17.67504841906449897, -3.238437383711913586, 13.62029908313571980 ) ) ;
#13001 = CARTESIAN_POINT ( 'NONE',  ( 10.17349413291699811, -2.837298848764000514, -6.969488574374499201 ) ) ;
#13002 = ORIENTED_EDGE ( 'NONE', *, *, #13050, .T. ) ;
#13003 = CARTESIAN_POINT ( 'NONE',  ( 8.971881080173746525, -5.348857519615915379, 7.441217429712126297 ) ) ;
#13004 = DIRECTION ( 'NONE',  ( -0.000000000000000000, -0.000000000000000000, 1.000000000000000000 ) ) ;
#13005 = CARTESIAN_POINT ( 'NONE',  ( 9.677263540183332680, 4.629523725463628558, -6.407767014557180119 ) ) ;
#13006 = FACE_OUTER_BOUND ( 'NONE', #43824, .T. ) ;
#13007 = CIRCLE ( 'NONE', #20821, 11.35000000000000675 ) ;
#13008 = CARTESIAN_POINT ( 'NONE',  ( 10.27815081430999911, 5.521603098753999461, 8.751228458888000716 ) ) ;
#13009 = CARTESIAN_POINT ( 'NONE',  ( 6.999999085428000534, 11.95749330617000084, -3.642574904853999929 ) ) ;
#13010 = CYLINDRICAL_SURFACE ( 'NONE', #39514, 1.999999999999999778 ) ;
#13011 = CARTESIAN_POINT ( 'NONE',  ( 4.000000000000000000, 0.000000000000000000, 0.000000000000000000 ) ) ;
#13012 = CARTESIAN_POINT ( 'NONE',  ( 10.30297040315999979, -4.081263557776000361, -9.025012210052000938 ) ) ;
#13013 = CARTESIAN_POINT ( 'NONE',  ( 4.000000000000000000, -2.149963194832000379, -0.1424560705006995553 ) ) ;
#13014 = CARTESIAN_POINT ( 'NONE',  ( 23.56664309646999911, -10.37807348783000094, 9.381504613656002078 ) ) ;
#13015 = ORIENTED_EDGE ( 'NONE', *, *, #7740, .T. ) ;
#13016 = CIRCLE ( 'NONE', #724, 12.20000000000000639 ) ;
#13017 = CARTESIAN_POINT ( 'NONE',  ( 11.01870451217999936, -2.731005928090000090, -4.994859145087000130 ) ) ;
#13018 = CYLINDRICAL_SURFACE ( 'NONE', #7965, 1.350000000000000089 ) ;
#13019 = CARTESIAN_POINT ( 'NONE',  ( 10.42440867506999957, -5.011664035303000198, 4.759074316248999459 ) ) ;
#13020 = DIRECTION ( 'NONE',  ( 0.000000000000000000, -1.000000000000000000, 0.000000000000000000 ) ) ;
#13021 = CARTESIAN_POINT ( 'NONE',  ( 11.09999999999999964, -4.000000000000000000, 7.500000000000000000 ) ) ;
#13022 = ADVANCED_FACE ( 'NONE', ( #24501, #14014 ), #67134, .F. ) ;
#13023 = CARTESIAN_POINT ( 'NONE',  ( 12.78089176142232475, 3.248146600645739124, 13.61798599873023363 ) ) ;
#13024 = ADVANCED_FACE ( 'NONE', ( #36016 ), #32185, .F. ) ;
#13025 = CARTESIAN_POINT ( 'NONE',  ( 10.11260824411999870, -3.359889198679999911, 5.859131457670000209 ) ) ;
#13026 = VERTEX_POINT ( 'NONE', #56316 ) ;
#13027 = CARTESIAN_POINT ( 'NONE',  ( 23.60205915885299888, -9.361474752776006270, -7.912850866691996998 ) ) ;
#13028 = CARTESIAN_POINT ( 'NONE',  ( 12.42135566322309614, 0.6200266137005038258, 13.98626978124057807 ) ) ;
#13029 = ORIENTED_EDGE ( 'NONE', *, *, #3223, .F. ) ;
#13030 = DIRECTION ( 'NONE',  ( 0.000000000000000000, 1.000000000000000000, 0.000000000000000000 ) ) ;
#13031 = CARTESIAN_POINT ( 'NONE',  ( 17.60604090556100232, 11.93226446383000017, -3.260045347513999658 ) ) ;
#13032 = CARTESIAN_POINT ( 'NONE',  ( 23.74222155833099990, -3.207124327041000367, -13.21279906398999948 ) ) ;
#13033 = FACE_OUTER_BOUND ( 'NONE', #40396, .T. ) ;
#13034 = FACE_OUTER_BOUND ( 'NONE', #31437, .T. ) ;
#13035 = CARTESIAN_POINT ( 'NONE',  ( 11.06794248424000138, 8.472325439733999985, -6.697655630924000292 ) ) ;
#13036 = CARTESIAN_POINT ( 'NONE',  ( 8.242030379543560770, 3.170592169292434370, -8.579047363641327806 ) ) ;
#13037 = CARTESIAN_POINT ( 'NONE',  ( 8.679055905797000037, 2.899999999999999911, 6.571291218949999902 ) ) ;
#13038 = CARTESIAN_POINT ( 'NONE',  ( 24.30000000000000071, 12.80696435099000041, 50.50083396221000243 ) ) ;
#13039 = CARTESIAN_POINT ( 'NONE',  ( 9.218723707566001124, -5.383415012847999392, -8.183490493635000362 ) ) ;
#13040 = CARTESIAN_POINT ( 'NONE',  ( 11.49056651104150006, 4.085456792591960706, -6.638028001068500217 ) ) ;
#13041 = CARTESIAN_POINT ( 'NONE',  ( 12.70786224245961904, -0.7192245859873329650, 12.57945610904470080 ) ) ;
#13042 = B_SPLINE_CURVE_WITH_KNOTS ( 'NONE', 3,
 ( #42559, #14024, #8772, #4795 ),
 .UNSPECIFIED., .F., .F.,
 ( 4, 4 ),
 ( 0.000000000000000000, 1.000000000000000000 ),
 .UNSPECIFIED. ) ;
#13043 = CARTESIAN_POINT ( 'NONE',  ( 10.48791429142999831, 4.016993441347180394, -6.608036045330599961 ) ) ;
#13044 = CARTESIAN_POINT ( 'NONE',  ( 9.303367640780999537, 4.538247246588100303, -6.493012239633999982 ) ) ;
#13046 = CARTESIAN_POINT ( 'NONE',  ( 8.281163468719425325, -9.408291950837329054, -6.292115732828485797 ) ) ;
#13045 = CARTESIAN_POINT ( 'NONE',  ( 9.215822372493999382, -4.249211653873900651, 6.684745346084599582 ) ) ;
#13047 = CARTESIAN_POINT ( 'NONE',  ( 23.57423432650097084, -13.35627592009906550, 4.153587462749816162 ) ) ;
#13048 = ORIENTED_EDGE ( 'NONE', *, *, #27470, .F. ) ;
#13049 = AXIS2_PLACEMENT_3D ( 'NONE', #45496, #8773, #52094 ) ;
#13050 = EDGE_CURVE ( 'NONE', #29684, #9641, #25020, .T. ) ;
#13051 = B_SPLINE_CURVE_WITH_KNOTS ( 'NONE', 3,
 ( #59595, #64478, #26766, #10665 ),
 .UNSPECIFIED., .F., .F.,
 ( 4, 4 ),
 ( 0.000000000000000000, 1.000000000000000000 ),
 .UNSPECIFIED. ) ;
#13052 = CARTESIAN_POINT ( 'NONE',  ( 10.60235971519489873, 4.605301262871499546, 8.506961598696999971 ) ) ;
#13053 = AXIS2_PLACEMENT_3D ( 'NONE', #66821, #45165, #23827 ) ;
#13054 = CARTESIAN_POINT ( 'NONE',  ( 10.93227479887999998, -2.539880901735999785, 6.453614191797999666 ) ) ;
#13055 = CARTESIAN_POINT ( 'NONE',  ( 8.947809814040999399, 4.698458605182900705, 6.596733927440100231 ) ) ;
#13056 = CARTESIAN_POINT ( 'NONE',  ( 10.85226354018294792, -5.092232985442820770, -6.870476274536370553 ) ) ;
#13057 = CARTESIAN_POINT ( 'NONE',  ( 9.013429960698999821, -4.933961117404000341, 8.417889755737999025 ) ) ;
#13058 = CARTESIAN_POINT ( 'NONE',  ( 12.47184101605659912, 3.029124285173875997, 13.54683579967692530 ) ) ;
#13059 = EDGE_LOOP ( 'NONE', ( #57594, #61899, #33203, #50772 ) ) ;
#13060 = CARTESIAN_POINT ( 'NONE',  ( 8.644809814040998575, -3.301541394817099739, -8.403266072559899769 ) ) ;
#13061 = CARTESIAN_POINT ( 'NONE',  ( 9.823096873516664829, -5.217465845835395299, -7.172815144550894750 ) ) ;
#13062 = CARTESIAN_POINT ( 'NONE',  ( 5.973935906450000388, 0.003195320017092000316, 1.614721372341000105 ) ) ;
#13063 = EDGE_CURVE ( 'NONE', #1602, #37026, #68161, .T. ) ;
#13064 = CARTESIAN_POINT ( 'NONE',  ( 8.525643369680000916, -2.918411554970002708, -6.570687780412999501 ) ) ;
#13065 = CARTESIAN_POINT ( 'NONE',  ( 9.099999931440999390, 5.250000000000000000, 7.500000000000000000 ) ) ;
#13066 = CARTESIAN_POINT ( 'NONE',  ( 10.45672469555900008, 4.433465011431599656, -6.750062220519700062 ) ) ;
#13068 = VECTOR ( 'NONE', #47290, 1000.000000000000000 ) ;
#13067 = CARTESIAN_POINT ( 'NONE',  ( 10.93769906950999982, 5.063122007744000008, 4.920829195600999739 ) ) ;
#13069 = CARTESIAN_POINT ( 'NONE',  ( 9.793328727373999953, -5.651611919872999934, -7.935921913274999184 ) ) ;
#13070 = PLANE ( 'NONE',  #67244 ) ;
#13071 = ORIENTED_EDGE ( 'NONE', *, *, #26837, .T. ) ;
#13072 = CARTESIAN_POINT ( 'NONE',  ( 24.56665282559600172, -12.04830931903000035, -3.140565848678999572 ) ) ;
#13073 = CARTESIAN_POINT ( 'NONE',  ( 12.58477985662609022, 0.5849891190461610213, -13.88342664904962831 ) ) ;
#13074 = CARTESIAN_POINT ( 'NONE',  ( 11.59999999999999964, -4.000000000000000000, -7.500000000000000000 ) ) ;
#13075 = CARTESIAN_POINT ( 'NONE',  ( 25.57798315594400052, -8.344602483709998353, -8.013942396659000877 ) ) ;
#13076 = CARTESIAN_POINT ( 'NONE',  ( 4.900006121741999898, 0.2617993877991493523, -1.999999999999999556 ) ) ;
#13077 = CARTESIAN_POINT ( 'NONE',  ( 9.418864158773999407, 3.210851187372000037, -6.346613542714999667 ) ) ;
#13078 = CARTESIAN_POINT ( 'NONE',  ( 10.25313817995482779, 2.714785337465412951, 7.027193780659266586 ) ) ;
#13079 = ORIENTED_EDGE ( 'NONE', *, *, #47917, .F. ) ;
#13080 = DIRECTION ( 'NONE',  ( -1.000000000000000000, 3.717264591378875951E-14, -3.221629312528359368E-14 ) ) ;
#13081 = CARTESIAN_POINT ( 'NONE',  ( 17.86981019193746079, 1.959656554206103962, -13.77332550900839969 ) ) ;
#13082 = VERTEX_POINT ( 'NONE', #31134 ) ;
#13083 = DIRECTION ( 'NONE',  ( -1.000000000000000000, 0.000000000000000000, 0.000000000000000000 ) ) ;
#13084 = CARTESIAN_POINT ( 'NONE',  ( 2.686390132544208331, -0.4581489286485234680, 3.499999999999998668 ) ) ;
#13085 = CARTESIAN_POINT ( 'NONE',  ( 8.763579719593998618, 4.815598936798999752, -8.835641302565999666 ) ) ;
#13086 = CARTESIAN_POINT ( 'NONE',  ( 24.13227431101038434, -12.49511235236459861, 3.369163575088180984 ) ) ;
#13087 = CARTESIAN_POINT ( 'NONE',  ( 8.832537864289999874, 2.899999999999999911, 6.571291218949999902 ) ) ;
#13088 = CARTESIAN_POINT ( 'NONE',  ( 17.72542258366203072, 0.6019459914113660659, -12.68079480699871020 ) ) ;
#13089 = CARTESIAN_POINT ( 'NONE',  ( 11.09999999999999964, -2.646159083949000124, 6.745271721726000536 ) ) ;
#13090 = ORIENTED_EDGE ( 'NONE', *, *, #17398, .F. ) ;
#13091 = CARTESIAN_POINT ( 'NONE',  ( 10.00638553269999953, -5.119272496996000399, 8.420388242270998802 ) ) ;
#13092 = CARTESIAN_POINT ( 'NONE',  ( 18.14119057082517017, -2.717377330333714536, -13.62490400537736512 ) ) ;
#13093 = CARTESIAN_POINT ( 'NONE',  ( 9.047164158776000775, 2.156584729807999867, -7.959751745006000689 ) ) ;
#13094 = ORIENTED_EDGE ( 'NONE', *, *, #19883, .T. ) ;
#13095 = CIRCLE ( 'NONE', #48814, 7.720759220056002903 ) ;
#13096 = CARTESIAN_POINT ( 'NONE',  ( 10.53865537815000053, 3.647234352455999584, -6.014129666051999834 ) ) ;
#13097 =( LENGTH_UNIT ( ) NAMED_UNIT ( * ) SI_UNIT ( .MILLI., .METRE. ) );
#13098 = B_SPLINE_CURVE_WITH_KNOTS ( 'NONE', 3,
 ( #11395, #32734, #15956, #57927 ),
 .UNSPECIFIED., .F., .F.,
 ( 4, 4 ),
 ( 0.000000000000000000, 1.000000000000000000 ),
 .UNSPECIFIED. ) ;
#13099 = ORIENTED_EDGE ( 'NONE', *, *, #13213, .T. ) ;
#13100 = CARTESIAN_POINT ( 'NONE',  ( 9.809950584426999853, 4.453199839589800035, 8.548019252390998801 ) ) ;
#13101 = CARTESIAN_POINT ( 'NONE',  ( 18.20792762907820972, -2.166426970554230724, -12.41237440719186580 ) ) ;
#13102 = CARTESIAN_POINT ( 'NONE',  ( 11.89975833414730033, -3.203462856645999945, 7.825000000000000178 ) ) ;
#13103 = CARTESIAN_POINT ( 'NONE',  ( 9.152446624286001864, 2.899999999999999911, -6.169193161299999950 ) ) ;
#13104 = CARTESIAN_POINT ( 'NONE',  ( 11.56566386073000174, -11.72961781202000076, -1.923363593971999963 ) ) ;
#13105 = EDGE_CURVE ( 'NONE', #60343, #29839, #52436, .T. ) ;
#13106 = EDGE_CURVE ( 'NONE', #44723, #62212, #48426, .T. ) ;
#13107 = AXIS2_PLACEMENT_3D ( 'NONE', #6998, #29038, #23430 ) ;
#13108 = CARTESIAN_POINT ( 'NONE',  ( 8.826138961223998436, 4.718363881473300658, 7.014550357332099750 ) ) ;
#13109 = EDGE_CURVE ( 'NONE', #64314, #6549, #12516, .T. ) ;
#13110 = EDGE_CURVE ( 'NONE', #65247, #27371, #5084, .T. ) ;
#13111 = CARTESIAN_POINT ( 'NONE',  ( 9.354368786244091183, -3.362065969394026688, 9.118206140364792489 ) ) ;
#13112 = ORIENTED_EDGE ( 'NONE', *, *, #54444, .T. ) ;
#13113 = CARTESIAN_POINT ( 'NONE',  ( 8.331682137624000006, -5.101289325373999262, 6.607176193198000647 ) ) ;
#13114 = CARTESIAN_POINT ( 'NONE',  ( 10.09249221959000131, 2.841614569232000065, -8.724659027040001291 ) ) ;
#13115 = CARTESIAN_POINT ( 'NONE',  ( 11.13500449003999826, -5.334503170127000260, -5.174025948961000765 ) ) ;
#13116 = AXIS2_PLACEMENT_3D ( 'NONE', #33169, #37375, #27233 ) ;
#13117 = CARTESIAN_POINT ( 'NONE',  ( 12.23619509269997430, 2.970722878206525142, -13.68118758531137935 ) ) ;
#13118 = CARTESIAN_POINT ( 'NONE',  ( 10.46957120343300041, -4.062009413492949861, -8.777708647662999297 ) ) ;
#13119 = CARTESIAN_POINT ( 'NONE',  ( 9.877259503622999759, -2.207992199716000137, 7.624813542847999059 ) ) ;
#13120 = CARTESIAN_POINT ( 'NONE',  ( 17.91845017417215757, -0.6323113780857052557, 13.98571806661952976 ) ) ;
#13121 = CARTESIAN_POINT ( 'NONE',  ( 2.000973465872999846, 3.500000000000000000, 0.000000000000000000 ) ) ;
#13122 = ORIENTED_EDGE ( 'NONE', *, *, #2602, .T. ) ;
#13123 = ORIENTED_EDGE ( 'NONE', *, *, #45151, .F. ) ;
#13124 = AXIS2_PLACEMENT_3D ( 'NONE', #46260, #21394, #16834 ) ;
#13125 = CARTESIAN_POINT ( 'NONE',  ( 9.187479719595000205, 2.391443348526999912, -6.856688371964000162 ) ) ;
#13126 = CARTESIAN_POINT ( 'NONE',  ( 7.307500000000000107, -0.2999999999999999889, 3.149999999999999911 ) ) ;
#13127 = CARTESIAN_POINT ( 'NONE',  ( 12.30534114217652686, -2.122480415427712597, 13.74636906787141477 ) ) ;
#13128 = CARTESIAN_POINT ( 'NONE',  ( 9.143006881379495354, -5.327771165987038593, 6.363180085552491150 ) ) ;
#13129 = ADVANCED_FACE ( 'NONE', ( #36714 ), #21311, .T. ) ;
#13130 = CARTESIAN_POINT ( 'NONE',  ( 9.053331853208000268, -5.618388245857000030, 7.727743016644000207 ) ) ;
#13131 = CARTESIAN_POINT ( 'NONE',  ( 15.90007192502618238, -3.569777767583313111, -11.29792192708077181 ) ) ;
#13133 = CARTESIAN_POINT ( 'NONE',  ( 2.550973465877000024, 3.500000000000000000, 0.000000000000000000 ) ) ;
#13132 = CARTESIAN_POINT ( 'NONE',  ( 9.458265421554999719, -4.240073379563900069, 6.258138488953999712 ) ) ;
#13134 = CARTESIAN_POINT ( 'NONE',  ( 10.46887750876899936, 3.307728619566300043, -8.574279626736998949 ) ) ;
#13135 = ORIENTED_EDGE ( 'NONE', *, *, #68169, .T. ) ;
#13136 = CARTESIAN_POINT ( 'NONE',  ( 10.98768538770000092, -2.700669876604000041, 4.945210823433001224 ) ) ;
#13137 = FACE_OUTER_BOUND ( 'NONE', #45392, .T. ) ;
#13138 = CARTESIAN_POINT ( 'NONE',  ( 18.13658048666561484, 0.2292434675627118279, 12.69722039463304775 ) ) ;
#13139 = CARTESIAN_POINT ( 'NONE',  ( 12.18105077442922379, 0.04081512046595160009, 12.69993297814735733 ) ) ;
#13140 = CARTESIAN_POINT ( 'NONE',  ( 4.149992563291998948, 1.229060429538527899, 1.599290730647371150 ) ) ;
#13141 = ORIENTED_EDGE ( 'NONE', *, *, #10897, .T. ) ;
#13143 = CARTESIAN_POINT ( 'NONE',  ( 7.946129465983998941, 3.388696841564000195, -6.288310469962000049 ) ) ;
#13142 = CARTESIAN_POINT ( 'NONE',  ( 11.82299956498189886, -5.207010770456999893, 7.825000000000000178 ) ) ;
#13144 = CARTESIAN_POINT ( 'NONE',  ( 8.804445280412998898, 5.597201461420000967, -8.171008079894999554 ) ) ;
#13145 = FACE_OUTER_BOUND ( 'NONE', #66573, .T. ) ;
#13146 = CARTESIAN_POINT ( 'NONE',  ( 7.954655249370001791, -5.133340916889001626, 6.761736834907998706 ) ) ;
#13147 = AXIS2_PLACEMENT_3D ( 'NONE', #45577, #61304, #7817 ) ;
#13148 = CARTESIAN_POINT ( 'NONE',  ( 24.39664803272433247, -3.240506204277676883, -12.09373379660224757 ) ) ;
#13149 = ADVANCED_FACE ( 'NONE', ( #58714 ), #19896, .F. ) ;
#13150 = MECHANICAL_DESIGN_GEOMETRIC_PRESENTATION_REPRESENTATION (  '', ( #18731 ), #39947 ) ;
#13151 = DIRECTION ( 'NONE',  ( 1.000000000000000000, 0.000000000000000000, 0.000000000000000000 ) ) ;
#13152 = CARTESIAN_POINT ( 'NONE',  ( 2.733565162642999979, 3.260648250327000230, 1.050234076676999972 ) ) ;
#13153 = VERTEX_POINT ( 'NONE', #6252 ) ;
#13154 = CARTESIAN_POINT ( 'NONE',  ( 12.34976886901036508, -0.5598083480993675254, -12.58755849294668394 ) ) ;
#13155 = CARTESIAN_POINT ( 'NONE',  ( 7.810165831303219619, -3.098200876999478215, 6.455848190766955597 ) ) ;
#13156 = EDGE_CURVE ( 'NONE', #31293, #50878, #45954, .T. ) ;
#13157 = CARTESIAN_POINT ( 'NONE',  ( 11.01356641589999974, -2.786433584103999994, 6.253463831328000211 ) ) ;
#13159 = CARTESIAN_POINT ( 'NONE',  ( 8.385051658773999606, 4.977909614887999545, 6.416776202806000029 ) ) ;
#13158 = VECTOR ( 'NONE', #64865, 1000.000000000000114 ) ;
#13160 = CARTESIAN_POINT ( 'NONE',  ( 6.294818532647999849E-06, 2.999993704296999741, 7.007529276254001127E-10 ) ) ;
#13161 = ORIENTED_EDGE ( 'NONE', *, *, #57825, .F. ) ;
#13162 = CARTESIAN_POINT ( 'NONE',  ( 6.580377242028999873, 0.8081923938199999657, -1.046566182397999922 ) ) ;
#13163 = CARTESIAN_POINT ( 'NONE',  ( 10.93804669887601833, 9.350510991039678643, 6.206837107818420129 ) ) ;
#13165 = CYLINDRICAL_SURFACE ( 'NONE', #37697, 0.5999999999999999778 ) ;
#13164 = CARTESIAN_POINT ( 'NONE',  ( 9.472537864290000442, -2.899999999999999911, -6.571291218949999902 ) ) ;
#13166 = CARTESIAN_POINT ( 'NONE',  ( 10.73964560330029983, 4.391636236366600166, 8.716526793355999558 ) ) ;
#13167 = CARTESIAN_POINT ( 'NONE',  ( 10.74760529021567734, -3.959614718189205185, -8.373188771871163283 ) ) ;
#13168 = ORIENTED_EDGE ( 'NONE', *, *, #40961, .F. ) ;
#13169 = PRESENTATION_STYLE_ASSIGNMENT (( #55461 ) ) ;
#13170 = ORIENTED_EDGE ( 'NONE', *, *, #44118, .F. ) ;
#13171 = FACE_OUTER_BOUND ( 'NONE', #51502, .T. ) ;
#13172 = CARTESIAN_POINT ( 'NONE',  ( 8.277730646792999636, -4.874569256861000177, 6.119503992241999590 ) ) ;
#13173 = CARTESIAN_POINT ( 'NONE',  ( 18.17070062201314684, -0.3858260082455376994, -13.99468631105251681 ) ) ;
#13174 = EDGE_LOOP ( 'NONE', ( #14217, #32445, #61697, #2127, #52827, #24405 ) ) ;
#13175 = CARTESIAN_POINT ( 'NONE',  ( 9.091609899095999481, -8.664388034093999380, 6.180722816477000059 ) ) ;
#13176 = LINE ( 'NONE', #7919, #37160 ) ;
#13177 = VECTOR ( 'NONE', #68361, 1000.000000000000227 ) ;
#13178 = CARTESIAN_POINT ( 'NONE',  ( 7.789414158769000451, 2.892522941075999832, -8.352379580902999479 ) ) ;
#13179 = CARTESIAN_POINT ( 'NONE',  ( 9.883148997457000817, -5.167567567567999731, 6.822293592207000934 ) ) ;
#13180 = CARTESIAN_POINT ( 'NONE',  ( 18.29983863916000075, -2.861762957209999847, 11.98830831200999825 ) ) ;
#13181 = ORIENTED_EDGE ( 'NONE', *, *, #42841, .F. ) ;
#13182 = FACE_OUTER_BOUND ( 'NONE', #21226, .T. ) ;
#13183 = CARTESIAN_POINT ( 'NONE',  ( 23.58699641938800085, -13.29334148118999970, -4.186654201655000129 ) ) ;
#13184 = DIRECTION ( 'NONE',  ( 1.000000000000000000, 0.000000000000000000, 0.000000000000000000 ) ) ;
#13185 = CARTESIAN_POINT ( 'NONE',  ( 9.753242276648833808, -2.714773723612734724, 7.027402982326762526 ) ) ;
#13186 = ORIENTED_EDGE ( 'NONE', *, *, #52748, .F. ) ;
#13187 = PRODUCT_DEFINITION_SHAPE ( 'NONE', 'NONE',  #16698 ) ;
#13188 = CARTESIAN_POINT ( 'NONE',  ( 25.39410316732910289, 2.774859191736423369, 11.32590268944005629 ) ) ;
#13189 = CARTESIAN_POINT ( 'NONE',  ( 10.95677425385773951, -2.827156737707505751, -6.689562958348049371 ) ) ;
#13190 = CARTESIAN_POINT ( 'NONE',  ( 10.68864630996109533, 2.651251715426289568, 7.268672106620575946 ) ) ;
#13191 = CARTESIAN_POINT ( 'NONE',  ( 24.62620337094597645, 12.35920179424943832, -2.996409964572606555 ) ) ;
#13192 = CARTESIAN_POINT ( 'NONE',  ( 5.500000000000000000, 0.000000000000000000, 0.000000000000000000 ) ) ;
#13193 = CARTESIAN_POINT ( 'NONE',  ( 12.26342747050452608, -0.3125520594525371676, -13.89528657259774391 ) ) ;
#13195 = EDGE_CURVE ( 'NONE', #57519, #49507, #60784, .T. ) ;
#13194 = AXIS2_PLACEMENT_3D ( 'NONE', #66390, #46105, #67411 ) ;
#13197 = ADVANCED_FACE ( 'NONE', ( #43677 ), #31031, .T. ) ;
#13196 = CARTESIAN_POINT ( 'NONE',  ( 18.11622138774307444, -2.775899412256286780, 12.38303361670990910 ) ) ;
#13198 = EDGE_LOOP ( 'NONE', ( #36900, #42485, #39870, #64051 ) ) ;
#13199 = CARTESIAN_POINT ( 'NONE',  ( 11.56322412107030928, -3.945399343424460525, -6.467939235001000320 ) ) ;
#13200 = ORIENTED_EDGE ( 'NONE', *, *, #55258, .T. ) ;
#13201 = CARTESIAN_POINT ( 'NONE',  ( 17.88292281839158093, 1.943028894538316065, 13.77656085490136206 ) ) ;
#13202 = CARTESIAN_POINT ( 'NONE',  ( 9.228345280414000484, 2.481540185810000132, -7.878707153279001396 ) ) ;
#13203 = CARTESIAN_POINT ( 'NONE',  ( 2.251656942761999680, 1.317797921594999755, -2.945325209437999803 ) ) ;
#13204 = CARTESIAN_POINT ( 'NONE',  ( 9.976697000975999430, -4.172225768856000272, -6.147144998063999388 ) ) ;
#13205 = VECTOR ( 'NONE', #2135, 999.9999999999998863 ) ;
#13206 = DIRECTION ( 'NONE',  ( -0.9999999999751629787, 5.691912101169789703E-06, -4.156456140529849248E-06 ) ) ;
#13207 = CARTESIAN_POINT ( 'NONE',  ( 23.51521036156700006, 13.45800259219000061, 4.320073176091000278 ) ) ;
#13208 = ORIENTED_EDGE ( 'NONE', *, *, #33395, .T. ) ;
#13209 = CIRCLE ( 'NONE', #5395, 1.350000000000000533 ) ;
#13210 = CARTESIAN_POINT ( 'NONE',  ( 11.74025954179439957, -3.228187097503200320, 6.858707791728399172 ) ) ;
#13211 = CARTESIAN_POINT ( 'NONE',  ( 10.93727498060999892, 5.425427353909999972, 7.240585962396000497 ) ) ;
#13212 = CARTESIAN_POINT ( 'NONE',  ( 10.61503919148196218, -5.349978903665073560, -7.499997722305344006 ) ) ;
#13213 = EDGE_CURVE ( 'NONE', #55008, #2543, #55636, .T. ) ;
#13214 = DIRECTION ( 'NONE',  ( -1.000000000000000000, 9.912705577010336396E-15, 5.699805706780943546E-14 ) ) ;
#13215 = CARTESIAN_POINT ( 'NONE',  ( 9.148115446195712153, 3.223534912153761756, 8.615607170735332332 ) ) ;
#13216 = VECTOR ( 'NONE', #24924, 1000.000000000000114 ) ;
#13217 = CARTESIAN_POINT ( 'NONE',  ( 10.80133863405319872, 4.534404523786000674, -8.181696703306599261 ) ) ;
#13218 = DIRECTION ( 'NONE',  ( 0.000000000000000000, -1.000000000000000000, 0.000000000000000000 ) ) ;
#13219 = CARTESIAN_POINT ( 'NONE',  ( 10.31357120343299982, 3.951311476804090006, -8.503230697164999796 ) ) ;
#13220 = DIRECTION ( 'NONE',  ( 0.000000000000000000, -1.000000000000000000, 0.000000000000000000 ) ) ;
#13221 = FACE_OUTER_BOUND ( 'NONE', #44299, .T. ) ;
#13222 = AXIS2_PLACEMENT_3D ( 'NONE', #32075, #4789, #58978 ) ;
#13223 = LINE ( 'NONE', #34549, #64519 ) ;
#13224 = CARTESIAN_POINT ( 'NONE',  ( 10.67529528041000120, 3.066676902634999813, -8.703232886886000941 ) ) ;
#13225 = VERTEX_POINT ( 'NONE', #44721 ) ;
#13226 = CARTESIAN_POINT ( 'NONE',  ( 8.079129440378000737, -3.524751762020000179, 5.573845465339999805 ) ) ;
#13227 = CARTESIAN_POINT ( 'NONE',  ( 18.17146957700709464, 2.902473988487531464, 13.69582979195751271 ) ) ;
#13228 = CARTESIAN_POINT ( 'NONE',  ( 23.89320776801300283, -3.226867021032998828, 11.46303308821000044 ) ) ;
#13229 = CARTESIAN_POINT ( 'NONE',  ( 6.999999691988000095, 12.36734761319999798, -2.759114534468000368 ) ) ;
#13230 = ORIENTED_EDGE ( 'NONE', *, *, #3397, .T. ) ;
#13231 = B_SPLINE_CURVE_WITH_KNOTS ( 'NONE', 3,
 ( #48056, #849, #64117, #10643 ),
 .UNSPECIFIED., .F., .F.,
 ( 4, 4 ),
 ( 0.000000000000000000, 1.000000000000000000 ),
 .UNSPECIFIED. ) ;
#13232 = CARTESIAN_POINT ( 'NONE',  ( 8.924954719592001595, 4.158911560497999815, 5.873540104660999184 ) ) ;
#13234 = CARTESIAN_POINT ( 'NONE',  ( 9.205449068729999240, -4.363978735910500006, 6.712833982956899703 ) ) ;
#13233 = CARTESIAN_POINT ( 'NONE',  ( 10.11792546752099931, -4.864937374655599278, -7.440072690703440017 ) ) ;
#13235 = CARTESIAN_POINT ( 'NONE',  ( 3.475528029604590952, -2.564910051950582748, 1.888346443232108207 ) ) ;
#13236 = EDGE_LOOP ( 'NONE', ( #52465, #38425, #1806 ) ) ;
#13237 = CARTESIAN_POINT ( 'NONE',  ( 9.799251915619999309, 4.057329420971000467, 9.430703183047999261 ) ) ;
#13238 = CARTESIAN_POINT ( 'NONE',  ( 18.18357137170428928, -2.882057337525668839, -13.70014066609292058 ) ) ;
#13239 = CARTESIAN_POINT ( 'NONE',  ( 11.70379573085659786, 5.106255642043000087, 7.308581953418300081 ) ) ;
#13240 = EDGE_CURVE ( 'NONE', #21338, #7236, #31084, .T. ) ;
#13241 = CARTESIAN_POINT ( 'NONE',  ( 10.05691733561000056, -2.453480799114999833, 6.657106310117000270 ) ) ;
#13242 = DIRECTION ( 'NONE',  ( 0.8660254037844296038, 3.108624468950434369E-15, -0.5000000000000157652 ) ) ;
#13243 = ORIENTED_EDGE ( 'NONE', *, *, #54837, .T. ) ;
#13244 = DIRECTION ( 'NONE',  ( 0.8843050097021329936, 0.1786785991674020024, -0.4313682974156600181 ) ) ;
#13245 = CARTESIAN_POINT ( 'NONE',  ( 11.33381694038000020, -2.642393655627000015, -7.577897390831000557 ) ) ;
#13246 = CARTESIAN_POINT ( 'NONE',  ( 7.933496154964543301, -2.297183234189244860, 7.856070056283313008 ) ) ;
#13247 = CARTESIAN_POINT ( 'NONE',  ( 9.228135700785001561, -2.875364528161000077, 8.669943154892999715 ) ) ;
#13248 = CARTESIAN_POINT ( 'NONE',  ( 10.97635090131019986, -3.000792947412299849, -8.118017011233499503 ) ) ;
#13249 = CARTESIAN_POINT ( 'NONE',  ( 10.51258376188599897, -4.962881317320600338, 6.886327436977599525 ) ) ;
#13250 = ORIENTED_EDGE ( 'NONE', *, *, #41274, .F. ) ;
#13251 = DIRECTION ( 'NONE',  ( 8.953094821930460994E-11, -0.2714597137497840040, 0.9624498032681421122 ) ) ;
#13252 = CARTESIAN_POINT ( 'NONE',  ( 11.19456919669529960, -2.906008650422999828, 7.176777099639999768 ) ) ;
#13253 = ORIENTED_EDGE ( 'NONE', *, *, #42791, .T. ) ;
#13254 = DIRECTION ( 'NONE',  ( 1.000000000000000000, 0.000000000000000000, 0.000000000000000000 ) ) ;
#13255 = EDGE_LOOP ( 'NONE', ( #58476, #52391, #20925, #29133 ) ) ;
#13256 = CARTESIAN_POINT ( 'NONE',  ( 9.930325322607000516, -5.020908168068000776, -6.342951604057000203 ) ) ;
#13257 = CARTESIAN_POINT ( 'NONE',  ( 9.351420280414000530, 4.953415418491999844, -8.946479654552000227 ) ) ;
#13258 = VECTOR ( 'NONE', #16467, 1000.000000000000000 ) ;
#13259 = CARTESIAN_POINT ( 'NONE',  ( 7.399999923048000028, 0.9999997023190999590, 0.000000000000000000 ) ) ;
#13260 = CARTESIAN_POINT ( 'NONE',  ( 8.307732882202806479, 5.093561060909792104, 6.540202441368732522 ) ) ;
#13261 = CARTESIAN_POINT ( 'NONE',  ( 12.22227632225710359, 2.273941840405718562, -12.50139599066423202 ) ) ;
#13262 = CARTESIAN_POINT ( 'NONE',  ( 11.83872066707849946, -3.141388196630700236, 8.019361746728900897 ) ) ;
#13263 = CARTESIAN_POINT ( 'NONE',  ( 11.27368717260499942, -4.539928529895099985, 6.618743573831199711 ) ) ;
#13264 = VERTEX_POINT ( 'NONE', #22683 ) ;
#13265 = CARTESIAN_POINT ( 'NONE',  ( 7.597040668823413334, 4.060223358062168053, 8.863603326158687068 ) ) ;
#13266 = AXIS2_PLACEMENT_3D ( 'NONE', #66469, #45508, #49705 ) ;
#13267 = VERTEX_POINT ( 'NONE', #23723 ) ;
#13268 = CARTESIAN_POINT ( 'NONE',  ( 7.764230646791999924, -4.628942671846000501, 5.991663889842000046 ) ) ;
#13269 = CARTESIAN_POINT ( 'NONE',  ( 17.78891907840798225, 0.6928235585691923104, 13.98285841810605135 ) ) ;
#13270 = ORIENTED_EDGE ( 'NONE', *, *, #28343, .T. ) ;
#13271 = CARTESIAN_POINT ( 'NONE',  ( 12.08977223171471493, -2.598917558143528872, -12.32906181315049032 ) ) ;
#13272 = CARTESIAN_POINT ( 'NONE',  ( 10.98995257254739855, 2.904643075091000171, 7.181435527216799564 ) ) ;
#13273 = CARTESIAN_POINT ( 'NONE',  ( 9.888320559623000605, -5.105186397454999359, -8.895598708036001057 ) ) ;
#13274 = CARTESIAN_POINT ( 'NONE',  ( 10.73976354018279977, 3.672815144550903632, 8.717465845835395299 ) ) ;
#13275 = AXIS2_PLACEMENT_3D ( 'NONE', #42488, #16599, #27441 ) ;
#13276 = CARTESIAN_POINT ( 'NONE',  ( 18.04814306103499888, -11.49796191965999981, 4.570681980344999396 ) ) ;
#13277 = CARTESIAN_POINT ( 'NONE',  ( 9.880016419786366910, 5.547192302291032107, -8.349494629669511170 ) ) ;
#13278 = CARTESIAN_POINT ( 'NONE',  ( 12.17999522571492399, -2.481546339243234200, -13.67732359575999013 ) ) ;
#13279 = CARTESIAN_POINT ( 'NONE',  ( 18.13628167719502216, 0.2299973361971401897, -12.69720198919504739 ) ) ;
#13280 = CARTESIAN_POINT ( 'NONE',  ( 11.26902897915239876, -3.778278678798900447, -8.337339982364900592 ) ) ;
#13281 = FACE_OUTER_BOUND ( 'NONE', #27340, .T. ) ;
#13282 = EDGE_CURVE ( 'NONE', #34641, #39483, #4261, .T. ) ;
#13284 = EDGE_CURVE ( 'NONE', #37826, #13517, #39812, .T. ) ;
#13283 = CARTESIAN_POINT ( 'NONE',  ( 8.893204719592999297, 3.977267228909999730, 9.308925224542001331 ) ) ;
#13285 = ORIENTED_EDGE ( 'NONE', *, *, #59704, .F. ) ;
#13286 = AXIS2_PLACEMENT_3D ( 'NONE', #48520, #43276, #6896 ) ;
#13287 = SHAPE_REPRESENTATION_RELATIONSHIP ( 'NONE' , 'NONE' ,  #60856, #42763 ) ;
#13288 = DIRECTION ( 'NONE',  ( 0.7071067306621966475, 0.09464344911259944815, 0.7007443820625967046 ) ) ;
#13289 = CARTESIAN_POINT ( 'NONE',  ( 18.12992444769444234, 2.745380825832320681, 13.61829546702431948 ) ) ;
#13290 = CARTESIAN_POINT ( 'NONE',  ( 24.02106019941100357, -3.259132549667000056, 12.61348568738999987 ) ) ;
#13291 = CARTESIAN_POINT ( 'NONE',  ( 17.91340230256478350, 1.987833194700777240, 12.55624649895498202 ) ) ;
#13292 = CARTESIAN_POINT ( 'NONE',  ( 11.12376201898999994, 5.751928413374999494, 5.182603196608999596 ) ) ;
#13293 = B_SPLINE_CURVE_WITH_KNOTS ( 'NONE', 3,
 ( #6848, #18389, #7204, #34815, #7540, #1612, #43923, #65229, #17342, #66612, #55445, #66267, #28540, #38671, #28184 ),
 .UNSPECIFIED., .F., .F.,
 ( 4, 2, 1, 2, 2, 2, 2, 4 ),
 ( 0.000000000000000000, 0.1250000000000000833, 0.2500000000000001665, 0.3750000000000002220, 0.5000000000000003331, 0.6250000000000004441, 0.7500000000000004441, 1.000000000000000000 ),
 .UNSPECIFIED. ) ;
#13294 = CARTESIAN_POINT ( 'NONE',  ( 9.691082467489000152, 5.335647408863999352, 8.701220655673999715 ) ) ;
#13295 = CARTESIAN_POINT ( 'NONE',  ( 9.372292071306626227, -3.125836066416603387, 7.537009346329285542 ) ) ;
#13296 = CARTESIAN_POINT ( 'NONE',  ( 12.80505043854144276, 0.7192913403693124152, -12.57945229203838267 ) ) ;
#13297 = ORIENTED_EDGE ( 'NONE', *, *, #12060, .F. ) ;
#13298 = CARTESIAN_POINT ( 'NONE',  ( 12.28024293382675403, -2.160546425968632445, 12.52422939561507675 ) ) ;
#13299 = CARTESIAN_POINT ( 'NONE',  ( 9.830304848515998728, -3.211495113978299898, -7.860510733857099197 ) ) ;
#13300 = CARTESIAN_POINT ( 'NONE',  ( 9.924742128742000347, 5.060458431729999873, 8.686130311522999747 ) ) ;
#13301 = EDGE_CURVE ( 'NONE', #57489, #20902, #882, .T. ) ;
#13302 = DIRECTION ( 'NONE',  ( 0.000000000000000000, -1.000000000000000000, 0.000000000000000000 ) ) ;
#13303 = ADVANCED_FACE ( 'NONE', ( #29682 ), #62489, .F. ) ;
#13304 = CARTESIAN_POINT ( 'NONE',  ( 11.47810404293059960, 3.436653965247300047, -8.647151967355000579 ) ) ;
#13305 = CARTESIAN_POINT ( 'NONE',  ( 12.22015141286114215, 0.2205037192104031540, 12.69742880170239019 ) ) ;
#13306 = CARTESIAN_POINT ( 'NONE',  ( 7.737829719589999655, 5.687206835507000235, 6.847268999608999707 ) ) ;
#13307 = CARTESIAN_POINT ( 'NONE',  ( 9.013423559847998590, 4.933953210258000155, 8.417881984655998906 ) ) ;
#13308 = AXIS2_PLACEMENT_3D ( 'NONE', #45958, #66587, #67267 ) ;
#13309 = CARTESIAN_POINT ( 'NONE',  ( 12.18370898482671727, 2.431702807279747525, 12.46721300078355554 ) ) ;
#13310 = ORIENTED_EDGE ( 'NONE', *, *, #37918, .T. ) ;
#13311 = CARTESIAN_POINT ( 'NONE',  ( 8.848264158775000610, 5.751585344281000545, -8.235867044345999588 ) ) ;
#13312 = CARTESIAN_POINT ( 'NONE',  ( 10.13662282008599824, 4.594711216567399781, -8.459250300176799797 ) ) ;
#13313 = CARTESIAN_POINT ( 'NONE',  ( 10.76375265279853366, -5.207958528999011349, 8.762692967157324375 ) ) ;
#13315 = CARTESIAN_POINT ( 'NONE',  ( 3.261349571466417352, -3.499999999999999556, -0.4563649592517093900 ) ) ;
#13314 = CARTESIAN_POINT ( 'NONE',  ( 8.149355646792999508, -2.583664704444999849, 6.684748541034000624 ) ) ;
#13316 = CARTESIAN_POINT ( 'NONE',  ( 9.655417874594000693, -4.797903641662700558, 7.160798403412399260 ) ) ;
#13317 = CARTESIAN_POINT ( 'NONE',  ( 11.58487348028854846, -4.882707455860599843, -7.977261354519500358 ) ) ;
#13318 = ORIENTED_EDGE ( 'NONE', *, *, #11507, .T. ) ;
#13319 = CARTESIAN_POINT ( 'NONE',  ( 0.7809723532208000529, 2.290033430544000215, -2.273164938691999648 ) ) ;
#13320 = CARTESIAN_POINT ( 'NONE',  ( 18.11727294771828412, -0.2737714781793354479, -12.69604447594146812 ) ) ;
#13321 = CARTESIAN_POINT ( 'NONE',  ( 11.09999999999999964, -2.700469802787999640, -5.124965750789000296 ) ) ;
#13322 = LINE ( 'NONE', #17869, #13476 ) ;
#13323 = FACE_OUTER_BOUND ( 'NONE', #22532, .T. ) ;
#13324 = CARTESIAN_POINT ( 'NONE',  ( 4.900006121742000786, -1.747572776708519404, -1.007237960741793170 ) ) ;
#13325 = DIRECTION ( 'NONE',  ( 0.000000000000000000, -0.9840640631525201520, -0.1778142840487031695 ) ) ;
#13326 = CARTESIAN_POINT ( 'NONE',  ( 20.07256264693999981, 0.000000000000000000, 0.000000000000000000 ) ) ;
#13327 = CARTESIAN_POINT ( 'NONE',  ( 13.50830001818700055, -12.29143783039000049, -2.111693202397000313 ) ) ;
#13328 = ORIENTED_EDGE ( 'NONE', *, *, #17525, .F. ) ;
#13329 = CARTESIAN_POINT ( 'NONE',  ( 8.662857780412000608, 2.741641653469999884, 6.457329666915000210 ) ) ;
#13330 = CARTESIAN_POINT ( 'NONE',  ( 10.89212518207000002, 5.053080421413000067, 5.013248928177000074 ) ) ;
#13331 = CARTESIAN_POINT ( 'NONE',  ( 7.421943355951564847, -2.366001551502044720, 8.097493604183329197 ) ) ;
#13332 = CARTESIAN_POINT ( 'NONE',  ( 17.69809243807087995, -0.6087680664141890130, 13.88205110007296028 ) ) ;
#13333 = CARTESIAN_POINT ( 'NONE',  ( 2.029339447824000331, -2.164574875407999865, -2.655056891479000036 ) ) ;
#13334 = EDGE_LOOP ( 'NONE', ( #28713, #7793, #32259, #39296 ) ) ;
#13335 = CARTESIAN_POINT ( 'NONE',  ( 1.803056799206332883, -2.798833948393629978, -2.150913519912204031 ) ) ;
#13336 = CARTESIAN_POINT ( 'NONE',  ( 27.64127793187000037, -3.399999999999999911, -4.505338571134999803 ) ) ;
#13337 = CARTESIAN_POINT ( 'NONE',  ( 10.59303303094000093, 2.436236667456999960, 7.793464546548000804 ) ) ;
#13338 = CARTESIAN_POINT ( 'NONE',  ( 11.06795257254739973, 3.036453385827900142, 7.219770138693499817 ) ) ;
#13339 = ADVANCED_FACE ( 'NONE', ( #51326 ), #53064, .F. ) ;
#13340 = CARTESIAN_POINT ( 'NONE',  ( 10.38314899745999931, -5.167567567567999731, 6.822293592207000934 ) ) ;
#13341 = CARTESIAN_POINT ( 'NONE',  ( 11.10664194037999941, -5.324199331986000594, -7.809344861333999965 ) ) ;
#13342 = CARTESIAN_POINT ( 'NONE',  ( 4.615443173015708389, -1.500000000000000222, -0.1963495408493622085 ) ) ;
#13343 = CARTESIAN_POINT ( 'NONE',  ( 0.4609011837824754654, 0.5355237950841763572, -3.460879404214840527 ) ) ;
#13344 = CARTESIAN_POINT ( 'NONE',  ( 12.18102902120000053, -2.459609776866888087, 12.46092926277264645 ) ) ;
#13345 = CARTESIAN_POINT ( 'NONE',  ( 8.360176255943175150, 3.240365764118005032, 9.085589947929626931 ) ) ;
#13346 = ORIENTED_EDGE ( 'NONE', *, *, #61315, .F. ) ;
#13347 = CARTESIAN_POINT ( 'NONE',  ( 17.93785022694517295, -2.005837716635007428, 13.76593133495255472 ) ) ;
#13348 = CARTESIAN_POINT ( 'NONE',  ( 10.05041772631199848, -3.450375740502100275, -8.631352948887998977 ) ) ;
#13349 = VERTEX_POINT ( 'NONE', #40159 ) ;
#13350 = EDGE_LOOP ( 'NONE', ( #2650, #587, #4432, #35133 ) ) ;
#13351 = CARTESIAN_POINT ( 'NONE',  ( 24.72252647404960513, -3.121154203591807175, -11.78764156663662099 ) ) ;
#13352 = DIRECTION ( 'NONE',  ( -1.000000000000000000, 0.000000000000000000, 0.000000000000000000 ) ) ;
#13353 = CARTESIAN_POINT ( 'NONE',  ( 8.691343736187999269, -4.374232398910099739, -8.309341309902798400 ) ) ;
#13354 = CARTESIAN_POINT ( 'NONE',  ( 10.46432998405999903, 2.042755206296999582, 7.723699495214000343 ) ) ;
#13355 = CARTESIAN_POINT ( 'NONE',  ( 9.937409415358999354, 3.510662261693000108, -6.227052446266999830 ) ) ;
#13356 = CARTESIAN_POINT ( 'NONE',  ( 10.90000000000000036, -8.263403946409999534, -6.953859016290999229 ) ) ;
#13357 = CARTESIAN_POINT ( 'NONE',  ( 10.48164908029000131, -4.022873587130999518, 9.090901241422999490 ) ) ;
#13358 = CARTESIAN_POINT ( 'NONE',  ( 17.57900174287143358, 0.7192906882580965000, -12.57945229568000656 ) ) ;
#13359 = CARTESIAN_POINT ( 'NONE',  ( 25.44994642811800034, -1.261213355973999610E-13, 4.884981308350999274E-14 ) ) ;
#13360 = CARTESIAN_POINT ( 'NONE',  ( 11.12133729122639991, -4.865898216891100247, -7.477221318588949117 ) ) ;
#13361 = EDGE_CURVE ( 'NONE', #852, #39266, #7563, .T. ) ;
#13363 = EDGE_CURVE ( 'NONE', #69034, #61732, #1747, .T. ) ;
#13362 = CARTESIAN_POINT ( 'NONE',  ( 4.599999999999999645, -13.17499999999999893, -1.613472157876637865E-15 ) ) ;
#13364 = ORIENTED_EDGE ( 'NONE', *, *, #26188, .T. ) ;
#13365 = CARTESIAN_POINT ( 'NONE',  ( 10.38937479142535913, -8.258793008140132841, 6.886170040595600561 ) ) ;
#13366 = EDGE_CURVE ( 'NONE', #65484, #29598, #52278, .T. ) ;
#13367 = CARTESIAN_POINT ( 'NONE',  ( 10.59999999999999964, 3.399999999999999911, -4.756097560976000338 ) ) ;
#13368 = B_SPLINE_CURVE_WITH_KNOTS ( 'NONE', 3,
 ( #5551, #67801, #58692, #57314, #26201, #46496, #41246, #58014, #9414, #31791, #47180 ),
 .UNSPECIFIED., .F., .F.,
 ( 4, 1, 1, 1, 1, 1, 1, 1, 4 ),
 ( 0.000000000000000000, 0.06984075817144648479, 0.2122522371145511844, 0.3546637160571506908, 0.4970751950002550990, 0.6394866739433597846, 0.7818981528859593189, 0.9243096318290640045, 1.000000000000000000 ),
 .UNSPECIFIED. ) ;
#13369 = FACE_OUTER_BOUND ( 'NONE', #6376, .T. ) ;
#13370 = CARTESIAN_POINT ( 'NONE',  ( 10.39358376188600097, 2.921249888908000081, -8.187519150726398465 ) ) ;
#13371 = CARTESIAN_POINT ( 'NONE',  ( 12.20052126010791405, 2.341019711503390610, 13.70584597024487827 ) ) ;
#13372 = CARTESIAN_POINT ( 'NONE',  ( 11.14993998249000029, -2.627133311863999676, 6.696092388640000337 ) ) ;
#13373 = ORIENTED_EDGE ( 'NONE', *, *, #42467, .F. ) ;
#13374 = CARTESIAN_POINT ( 'NONE',  ( 12.39790242452336244, 0.4743817203469002375, -12.68807659223303475 ) ) ;
#13375 = CARTESIAN_POINT ( 'NONE',  ( 12.21516724099300077, 0.4251989115648853179, 13.99355557726514476 ) ) ;
#13376 = ORIENTED_EDGE ( 'NONE', *, *, #2792, .T. ) ;
#13377 = DIRECTION ( 'NONE',  ( 0.000000000000000000, 0.000000000000000000, -1.000000000000000000 ) ) ;
#13378 = CYLINDRICAL_SURFACE ( 'NONE', #10304, 0.5000000000000002220 ) ;
#13379 = AXIS2_PLACEMENT_3D ( 'NONE', #69023, #15548, #9954 ) ;
#13380 = CARTESIAN_POINT ( 'NONE',  ( 8.922950365671626471, 4.680938325111460685, 8.049413566043876145 ) ) ;
#13381 = CARTESIAN_POINT ( 'NONE',  ( 5.200000000000000178, -1.199999999999999956, -9.776630298829998011 ) ) ;
#13382 = B_SPLINE_SURFACE_WITH_KNOTS ( 'NONE', 3, 3, ( 
 ( #34303, #14009, #35338, #12981 ),
 ( #7375, #39893, #7725, #50033 ),
 ( #23460, #44796, #66099, #39543 ),
 ( #50378, #61213, #55967, #13330 ),
 ( #34654, #8072, #26216, #51744 ),
 ( #14693, #47543, #62236, #9428 ) ),
 .UNSPECIFIED., .F., .F., .F.,
 ( 4, 1, 1, 4 ),
 ( 4, 4 ),
 ( -0.007877443071734000282, 0.000000000000000000, 0.07142857142856999519, 0.1006819380563999944 ),
 ( -0.1835627106809000209, 1.183562710543999863 ),
 .UNSPECIFIED. ) ;
#13383 = EDGE_CURVE ( 'NONE', #65964, #2231, #4444, .T. ) ;
#13384 = CYLINDRICAL_SURFACE ( 'NONE', #23530, 0.4999999999999998335 ) ;
#13385 = CARTESIAN_POINT ( 'NONE',  ( 11.12486385074000061, 7.229995578275999257, -6.290807116501000884 ) ) ;
#13386 = CARTESIAN_POINT ( 'NONE',  ( 0.05492698531792999939, 3.485378829570000114, 1.246872170512999922 ) ) ;
#13387 = CYLINDRICAL_SURFACE ( 'NONE', #59408, 0.6250000000000005551 ) ;
#13388 = CARTESIAN_POINT ( 'NONE',  ( 12.35197574246970298, 3.042005152232404086, 12.22727356655694386 ) ) ;
#13389 = CARTESIAN_POINT ( 'NONE',  ( 9.617321917839001699, -3.361793157411000266, -5.915550373431999631 ) ) ;
#13390 = CARTESIAN_POINT ( 'NONE',  ( 11.78179573085659904, 4.973133828855400118, -7.668383662421899061 ) ) ;
#13391 = CARTESIAN_POINT ( 'NONE',  ( 12.61463924704883510, -0.7003689475845866763, 12.58057160030299393 ) ) ;
#13392 = B_SPLINE_CURVE_WITH_KNOTS ( 'NONE', 3,
 ( #15439, #36069, #4244, #57385 ),
 .UNSPECIFIED., .F., .F.,
 ( 4, 4 ),
 ( 0.000000000000000000, 1.000000000000000000 ),
 .UNSPECIFIED. ) ;
#13393 = CARTESIAN_POINT ( 'NONE',  ( 10.91060165877000188, 4.702351492776999820, -9.210043641106000933 ) ) ;
#13394 = CARTESIAN_POINT ( 'NONE',  ( 9.759292290062999697, 4.987433183662999703, -6.926667499798199401 ) ) ;
#13396 = CARTESIAN_POINT ( 'NONE',  ( 10.26390484475999898, -3.364655826309999931, 4.688340142401999699 ) ) ;
#13395 = CARTESIAN_POINT ( 'NONE',  ( 15.98722619340700213, -8.633165116997000510, -7.765565731395999372 ) ) ;
#13397 = CARTESIAN_POINT ( 'NONE',  ( 24.30000000000000071, -11.85420044612000012, 3.901016762742000488 ) ) ;
#13398 = ORIENTED_EDGE ( 'NONE', *, *, #38453, .F. ) ;
#13399 = CARTESIAN_POINT ( 'NONE',  ( 9.860095611463300713, -4.592594002674506015, -8.996708106635217916 ) ) ;
#13400 = CARTESIAN_POINT ( 'NONE',  ( 10.37373728961999930, -2.215269876326000364, 7.703982265807999497 ) ) ;
#13401 = CARTESIAN_POINT ( 'NONE',  ( 10.11093802597399893, 3.477805217445600228, 8.357994702431799539 ) ) ;
#13402 = CARTESIAN_POINT ( 'NONE',  ( 10.08809113605762597, 3.189914598996232975, -7.169403702379763210 ) ) ;
#13403 = CARTESIAN_POINT ( 'NONE',  ( 24.67921569845699992, 12.29514839105000057, -2.979196030862000022 ) ) ;
#13404 = DIRECTION ( 'NONE',  ( 0.000000000000000000, 0.000000000000000000, -1.000000000000000000 ) ) ;
#13405 = UNCERTAINTY_MEASURE_WITH_UNIT (LENGTH_MEASURE( 1.000000000000000082E-05 ), #59088, 'distance_accuracy_value', 'NONE');
#13406 = EDGE_LOOP ( 'NONE', ( #27074, #60718, #41051, #23880 ) ) ;
#13407 = CARTESIAN_POINT ( 'NONE',  ( 9.556659112603998807, -4.496147888241900148, -8.528383061402999843 ) ) ;
#13408 = CARTESIAN_POINT ( 'NONE',  ( 9.739763540183334456, -4.327184855449098144, -6.282534154164605589 ) ) ;
#13409 = B_SPLINE_CURVE_WITH_KNOTS ( 'NONE', 3,
 ( #30789, #61914, #29782, #2839 ),
 .UNSPECIFIED., .F., .F.,
 ( 4, 4 ),
 ( 0.000000000000000000, 1.000000000000000000 ),
 .UNSPECIFIED. ) ;
#13410 = CARTESIAN_POINT ( 'NONE',  ( 18.06303038656657733, 1.966720487694622932, -12.44556484937419150 ) ) ;
#13411 = DIRECTION ( 'NONE',  ( -1.000000000000000000, -4.212899870229393166E-14, 3.717264591378875951E-14 ) ) ;
#13412 = DIRECTION ( 'NONE',  ( 0.000000000000000000, -1.000000000000000000, 0.000000000000000000 ) ) ;
#13413 = EDGE_CURVE ( 'NONE', #16052, #18161, #15454, .T. ) ;
#13415 = EDGE_CURVE ( 'NONE', #16591, #49775, #48946, .T. ) ;
#13414 = B_SPLINE_CURVE_WITH_KNOTS ( 'NONE', 3,
 ( #28899, #13500, #39718, #18050 ),
 .UNSPECIFIED., .F., .F.,
 ( 4, 4 ),
 ( 0.000000000000000000, 1.000000000000000000 ),
 .UNSPECIFIED. ) ;
#13416 = CARTESIAN_POINT ( 'NONE',  ( 11.38795122972049967, 4.398282450130399646, -6.578956058177199751 ) ) ;
#13417 = CARTESIAN_POINT ( 'NONE',  ( 12.23612747308697379, 2.758947143663601498, -13.61512400666043376 ) ) ;
#13418 = CARTESIAN_POINT ( 'NONE',  ( 9.971918425727000823, -4.365624317997999881, -9.242254741729000855 ) ) ;
#13419 = CARTESIAN_POINT ( 'NONE',  ( 0.8426401325419167199, -3.058252359239902685, -1.762666431298148595 ) ) ;
#13420 = EDGE_LOOP ( 'NONE', ( #58138, #44129, #26416, #50068 ) ) ;
#13421 = CARTESIAN_POINT ( 'NONE',  ( 18.00257402911388738, 3.100282954702140881, -13.65258486501627466 ) ) ;
#13422 = CARTESIAN_POINT ( 'NONE',  ( 12.57519714614618600, 0.5812901181791684246, -13.88363587338389493 ) ) ;
#13423 = CARTESIAN_POINT ( 'NONE',  ( 10.59999999999999964, 3.399999999999999911, 4.756097560976000338 ) ) ;
#13424 = CARTESIAN_POINT ( 'NONE',  ( 17.88292281824755747, -1.943028894393611372, -13.77656085492286486 ) ) ;
#13425 = CARTESIAN_POINT ( 'NONE',  ( 2.258651541363375426, -3.500000000000000000, -0.3376993977123544100 ) ) ;
#13426 = AXIS2_PLACEMENT_3D ( 'NONE', #53733, #36974, #26135 ) ;
#13427 = CARTESIAN_POINT ( 'NONE',  ( 9.658629719592001450, 5.496789211521000418, -7.043125396300999874 ) ) ;
#13428 = CARTESIAN_POINT ( 'NONE',  ( 6.785263095641375308, 1.476230154961222452, -0.3823247283369876626 ) ) ;
#13429 = ORIENTED_EDGE ( 'NONE', *, *, #18454, .T. ) ;
#13430 = DIRECTION ( 'NONE',  ( 0.000000000000000000, 0.001239076634196941687, -0.9999992323442525866 ) ) ;
#13431 = CARTESIAN_POINT ( 'NONE',  ( 18.06505946208161362, 2.138585121884149398, -13.74350169411782652 ) ) ;
#13432 = VERTEX_POINT ( 'NONE', #26825 ) ;
#13433 = CARTESIAN_POINT ( 'NONE',  ( 25.27003374619006948, -8.359947296913826875, -8.486664668671879852 ) ) ;
#13434 = CARTESIAN_POINT ( 'NONE',  ( 24.66906608026770442, 3.147934860013589464, 11.83339566522958464 ) ) ;
#13435 = CARTESIAN_POINT ( 'NONE',  ( 8.713854719593998155, 5.442817578555000146, -8.106149115450000053 ) ) ;
#13436 = CARTESIAN_POINT ( 'NONE',  ( 23.98816733236458276, -12.73143379325068025, 3.487225215969183889 ) ) ;
#13437 = CARTESIAN_POINT ( 'NONE',  ( 10.68546886766499959, -4.566506264294200257, -6.470713638631999665 ) ) ;
#13438 = DIRECTION ( 'NONE',  ( -1.000000000000000000, 0.000000000000000000, 0.000000000000000000 ) ) ;
#13439 = CARTESIAN_POINT ( 'NONE',  ( 10.35226354018232975, -5.092232985442820770, 8.129523725463624118 ) ) ;
#13440 = ORIENTED_EDGE ( 'NONE', *, *, #16306, .T. ) ;
#13441 = CARTESIAN_POINT ( 'NONE',  ( 7.675811484805873164, 4.984677974768257691, -8.445524128177581247 ) ) ;
#13442 = CARTESIAN_POINT ( 'NONE',  ( 10.79184687351566829, -4.999583552997724389, 8.268183399968647151 ) ) ;
#13444 = EDGE_CURVE ( 'NONE', #33492, #7350, #23421, .T. ) ;
#13443 = CARTESIAN_POINT ( 'NONE',  ( 9.693589158772999426, 4.047146749018000200, -5.600703114891000034 ) ) ;
#13445 = VERTEX_POINT ( 'NONE', #37987 ) ;
#13446 = CARTESIAN_POINT ( 'NONE',  ( 10.01597178489000051, 4.792666960550000077, -6.390258598531999290 ) ) ;
#13447 = CARTESIAN_POINT ( 'NONE',  ( 3.999999855301999752, 0.000000000000000000, 0.000000000000000000 ) ) ;
#13448 = EDGE_CURVE ( 'NONE', #8401, #19244, #930, .T. ) ;
#13449 = ORIENTED_EDGE ( 'NONE', *, *, #11430, .F. ) ;
#13450 = CARTESIAN_POINT ( 'NONE',  ( 9.404684229509999938, 3.195116560491999991, 8.309874741421300115 ) ) ;
#13451 = CARTESIAN_POINT ( 'NONE',  ( 18.13206058706451174, -2.916601882134804313, -12.25780480496326419 ) ) ;
#13452 = CARTESIAN_POINT ( 'NONE',  ( 10.99335825053592330, 6.355322062518198756, -5.175304492146106661 ) ) ;
#13453 = CARTESIAN_POINT ( 'NONE',  ( 7.936333771302000351, 5.123034328734999754, 6.721303713258000023 ) ) ;
#13454 = DIRECTION ( 'NONE',  ( -1.000000000000000000, 0.000000000000000000, 0.000000000000000000 ) ) ;
#13455 = CARTESIAN_POINT ( 'NONE',  ( 9.402626378948871988, -2.553903598434096089, 8.467682852844752972 ) ) ;
#13456 = ORIENTED_EDGE ( 'NONE', *, *, #28287, .F. ) ;
#13457 = CARTESIAN_POINT ( 'NONE',  ( 10.47253786429000044, 2.899999999999999911, -6.571291218949999902 ) ) ;
#13458 = CARTESIAN_POINT ( 'NONE',  ( 10.37239528041000014, 3.992345698584000235, -5.977238432995000572 ) ) ;
#13459 = CARTESIAN_POINT ( 'NONE',  ( 12.80505043854143388, 3.248109929747637015, -13.61799478206225444 ) ) ;
#13460 = CARTESIAN_POINT ( 'NONE',  ( 12.15420371307391356, 2.840396063362191192, -13.70885132993087652 ) ) ;
#13461 = CARTESIAN_POINT ( 'NONE',  ( 9.633709346416999608, -2.844451673749999632, -6.951281079990299538 ) ) ;
#13462 = CARTESIAN_POINT ( 'NONE',  ( 10.24961784311999935, -4.184221496660999406, 9.286877953065999947 ) ) ;
#13463 = ADVANCED_FACE ( 'NONE', ( #47457 ), #42453, .F. ) ;
#13464 = AXIS2_PLACEMENT_3D ( 'NONE', #16527, #21091, #36830 ) ;
#13465 = CARTESIAN_POINT ( 'NONE',  ( 17.97798355280614047, -0.5935699150349393882, 13.98741755999925118 ) ) ;
#13466 = CARTESIAN_POINT ( 'NONE',  ( 7.836101299556240463, 4.962718242113793643, 6.493661227056148455 ) ) ;
#13467 = VERTEX_POINT ( 'NONE', #27863 ) ;
#13468 = VERTEX_POINT ( 'NONE', #27506 ) ;
#13469 = CARTESIAN_POINT ( 'NONE',  ( 9.146614158775999925, 2.981992329588000423, -5.895876591910999664 ) ) ;
#13470 = CARTESIAN_POINT ( 'NONE',  ( 9.137136214451835770, 5.220014052224821732, 6.249519307007754598 ) ) ;
#13471 = B_SPLINE_CURVE_WITH_KNOTS ( 'NONE', 3,
 ( #58304, #37328, #53413, #43266, #68788, #32097 ),
 .UNSPECIFIED., .F., .F.,
 ( 4, 2, 4 ),
 ( 0.000000000000000000, 0.5000000000000000000, 1.000000000000000000 ),
 .UNSPECIFIED. ) ;
#13472 = CARTESIAN_POINT ( 'NONE',  ( 12.18791262562190525, -2.399397798184976782, 13.69429647073317113 ) ) ;
#13473 = CARTESIAN_POINT ( 'NONE',  ( 1.700000000000000178, 0.000000000000000000, 0.000000000000000000 ) ) ;
#13474 = CARTESIAN_POINT ( 'NONE',  ( 24.15420991129199990, 9.222014324292000964, -9.473961295084999179 ) ) ;
#13476 = VECTOR ( 'NONE', #60855, 1000.000000000000114 ) ;
#13475 = CARTESIAN_POINT ( 'NONE',  ( 17.79229341877100268, -3.377812583009999869, -11.11021646535000151 ) ) ;
#13478 = CARTESIAN_POINT ( 'NONE',  ( 11.07206039417999932, -6.376288328743000555, 5.346922539581000500 ) ) ;
#13477 = CARTESIAN_POINT ( 'NONE',  ( 9.675772138681999479, -4.424886761933599644, 8.559813987224998755 ) ) ;
#13479 = CARTESIAN_POINT ( 'NONE',  ( 0.5929091678463546122, 3.086677832968792501, -1.352473734835327290 ) ) ;
#13480 = EDGE_LOOP ( 'NONE', ( #21464, #66860, #35336, #3263 ) ) ;
#13481 = DIRECTION ( 'NONE',  ( 0.000000000000000000, -0.8648648648648717963, -0.5020047465136829867 ) ) ;
#13482 = CARTESIAN_POINT ( 'NONE',  ( 23.60205915885299888, -11.53346724329999873, -4.150849519424002487 ) ) ;
#13483 = CARTESIAN_POINT ( 'NONE',  ( 18.14024703743437072, 0.2197131112048714974, 12.69744725510431493 ) ) ;
#13484 = CARTESIAN_POINT ( 'NONE',  ( 12.18394763204575248, -0.08111188042542251397, 12.69973954613695177 ) ) ;
#13485 = CARTESIAN_POINT ( 'NONE',  ( 11.79999999550100220, 11.52577121388000059, 1.696750555870000010 ) ) ;
#13486 = EDGE_LOOP ( 'NONE', ( #60676, #38256, #12733, #55704 ) ) ;
#13488 = CARTESIAN_POINT ( 'NONE',  ( 12.15805955563557461, -2.854826764565363106, -12.27308055912475204 ) ) ;
#13487 = CARTESIAN_POINT ( 'NONE',  ( 11.03766149047999967, -5.246943569709999977, -5.025196799498999667 ) ) ;
#13489 = CARTESIAN_POINT ( 'NONE',  ( 44.24148000000000280, 2.258942858049999725, -12.29419282279000036 ) ) ;
#13490 = DIRECTION ( 'NONE',  ( 1.000000000000000000, 0.000000000000000000, 0.000000000000000000 ) ) ;
#13491 = CARTESIAN_POINT ( 'NONE',  ( 10.39503166480599994, 2.725152142215999884, 7.410114961806599787 ) ) ;
#13492 = B_SPLINE_CURVE_WITH_KNOTS ( 'NONE', 3,
 ( #52158, #20349, #4262, #41673 ),
 .UNSPECIFIED., .F., .F.,
 ( 4, 4 ),
 ( 0.000000000000000000, 1.000000000000000000 ),
 .UNSPECIFIED. ) ;
#13493 = CARTESIAN_POINT ( 'NONE',  ( 5.699996624164000103, -12.50864642754000045, -2.924703664565999617 ) ) ;
#13494 = DIRECTION ( 'NONE',  ( 0.000000000000000000, 0.000000000000000000, -1.000000000000000000 ) ) ;
#13495 = CARTESIAN_POINT ( 'NONE',  ( 3.124567434295000279, 1.296329916925999859, 3.528159097347999928 ) ) ;
#13496 = EDGE_LOOP ( 'NONE', ( #46532, #45250, #61999, #10490 ) ) ;
#13497 = ADVANCED_FACE ( 'NONE', ( #54419 ), #17361, .T. ) ;
#13498 = ADVANCED_FACE ( 'NONE', ( #35093 ), #44296, .T. ) ;
#13499 = CARTESIAN_POINT ( 'NONE',  ( 12.26373771493048181, -0.3125877143166542749, -12.69482668528969604 ) ) ;
#13500 = CARTESIAN_POINT ( 'NONE',  ( 10.94911764820105482, -2.860072064609847864, 5.104013334854830219 ) ) ;
#13501 = CARTESIAN_POINT ( 'NONE',  ( 20.10000000000000142, 0.000000000000000000, 0.000000000000000000 ) ) ;
#13502 = DIRECTION ( 'NONE',  ( -1.000000000000000000, 0.000000000000000000, 0.000000000000000000 ) ) ;
#13503 = CARTESIAN_POINT ( 'NONE',  ( 18.23980063339601898, -2.972525812591876093, -11.47315805767759755 ) ) ;
#13504 = VERTEX_POINT ( 'NONE', #65245 ) ;
#13505 = CARTESIAN_POINT ( 'NONE',  ( 6.350178865300000197, -1.113463867511000238, -0.3786539577593999728 ) ) ;
#13506 = EDGE_CURVE ( 'NONE', #13445, #20297, #12120, .T. ) ;
#13507 = CARTESIAN_POINT ( 'NONE',  ( 8.485085841226998937, 4.376386084436000523, -6.154119786874999498 ) ) ;
#13508 = DIRECTION ( 'NONE',  ( -1.000000000000000000, 0.000000000000000000, 0.000000000000000000 ) ) ;
#13509 = CARTESIAN_POINT ( 'NONE',  ( 7.773264469372000107, 2.859518616742000141, 6.768376720750000075 ) ) ;
#13510 = CARTESIAN_POINT ( 'NONE',  ( 11.64633327354034797, 3.135095881599500256, -6.934277916748599502 ) ) ;
#13511 = ORIENTED_EDGE ( 'NONE', *, *, #48532, .F. ) ;
#13512 = CARTESIAN_POINT ( 'NONE',  ( 9.388626433405999450, -4.079401915682999480, 9.259353168384000909 ) ) ;
#13513 = ORIENTED_EDGE ( 'NONE', *, *, #43279, .T. ) ;
#13514 = CARTESIAN_POINT ( 'NONE',  ( 25.60000000000000142, 0.000000000000000000, 10.75000000000000000 ) ) ;
#13515 = CARTESIAN_POINT ( 'NONE',  ( 7.919004440377000797, -5.361050935357000391, 6.973449182446000094 ) ) ;
#13516 = CARTESIAN_POINT ( 'NONE',  ( 18.18333308066189247, 0.3651687365794590856, -13.99525266148724079 ) ) ;
#13517 = VERTEX_POINT ( 'NONE', #67223 ) ;
#13518 = CARTESIAN_POINT ( 'NONE',  ( 10.98911330520352791, 7.751816412315136517, -6.410483435660403018 ) ) ;
#13519 = CARTESIAN_POINT ( 'NONE',  ( 8.266851002545999805, 2.832432432432000269, 6.822293592207000934 ) ) ;
#13520 = VECTOR ( 'NONE', #52581, 1000.000000000000000 ) ;
#13521 = DIRECTION ( 'NONE',  ( 1.000000000000000000, 0.000000000000000000, 0.000000000000000000 ) ) ;
#13522 = CARTESIAN_POINT ( 'NONE',  ( 25.46372676430900128, 8.354609436172999892, -8.148458316574000548 ) ) ;
#13523 = CARTESIAN_POINT ( 'NONE',  ( 18.16726790532722191, -2.625885335051481029, 12.42137433334730723 ) ) ;
#13524 = ORIENTED_EDGE ( 'NONE', *, *, #15796, .T. ) ;
#13525 = CARTESIAN_POINT ( 'NONE',  ( 10.58844302970999962, -3.754658547780000521, 5.545362468768000319 ) ) ;
#13526 = B_SPLINE_CURVE_WITH_KNOTS ( 'NONE', 3,
 ( #49798, #44906, #2584, #38968, #12391, #7483, #6791, #65516, #49100, #18674, #17286, #29175, #28836, #17988, #23226, #55041, #28480, #13089 ),
 .UNSPECIFIED., .F., .F.,
 ( 4, 2, 2, 2, 2, 2, 2, 2, 4 ),
 ( 0.000000000000000000, 0.1250000000000001110, 0.2500000000000002220, 0.3750000000000003331, 0.5000000000000004441, 0.6250000000000003331, 0.7500000000000002220, 0.8750000000000001110, 1.000000000000000000 ),
 .UNSPECIFIED. ) ;
#13527 = CARTESIAN_POINT ( 'NONE',  ( 23.61341120619100309, -13.29072902885999952, -4.053938077286999508 ) ) ;
#13528 = CARTESIAN_POINT ( 'NONE',  ( 10.52934687351650389, 4.163624617374466652, -8.749999999999998224 ) ) ;
#13529 = CARTESIAN_POINT ( 'NONE',  ( 12.61470515270720405, -1.811791595467374671, 13.88227300399886666 ) ) ;
#13530 = ORIENTED_EDGE ( 'NONE', *, *, #3726, .F. ) ;
#13531 = DIRECTION ( 'NONE',  ( 1.000000000000000000, 0.000000000000000000, 0.000000000000000000 ) ) ;
#13532 = CARTESIAN_POINT ( 'NONE',  ( 8.903317944506804693, -4.274905112035349397, -6.473766235688636073 ) ) ;
#13533 = B_SPLINE_CURVE_WITH_KNOTS ( 'NONE', 3,
 ( #9217, #31251, #14819, #19722, #35466, #57116, #30555, #41045, #9562, #52215, #10255, #4657, #14138, #25996, #4316, #36480, #15160, #9913 ),
 .UNSPECIFIED., .F., .F.,
 ( 4, 2, 2, 2, 2, 2, 2, 2, 4 ),
 ( 0.1253528645472067604, 0.2189972814376893728, 0.3126416983281720130, 0.4062861152186546532, 0.4999305321091372933, 0.5935749489996199335, 0.6872193658901024627, 0.7808637827805851028, 0.8745081996710677430 ),
 .UNSPECIFIED. ) ;
#13534 = CARTESIAN_POINT ( 'NONE',  ( 3.500000000000000000, 3.491196775144654207, 0.2719696052742964221 ) ) ;
#13535 = CARTESIAN_POINT ( 'NONE',  ( 9.925810748568999031, -5.172583146916751140, -8.000243450341617546 ) ) ;
#13536 = DIRECTION ( 'NONE',  ( 0.000000000000000000, 0.7071067811865475727, -0.7071067811865475727 ) ) ;
#13537 = CARTESIAN_POINT ( 'NONE',  ( 12.37769783401832768, 0.4561791668615491901, -13.88992602861184089 ) ) ;
#13538 = CARTESIAN_POINT ( 'NONE',  ( 18.11306383842994450, -2.218305400803588512, 12.51277866499342650 ) ) ;
#13539 = ORIENTED_EDGE ( 'NONE', *, *, #63133, .T. ) ;
#13540 = CARTESIAN_POINT ( 'NONE',  ( 11.27745123989519982, -3.589787500396900199, -8.292221125039500151 ) ) ;
#13541 = EDGE_LOOP ( 'NONE', ( #53020, #68405, #8598, #54103, #41563, #59655, #11004, #19528 ) ) ;
#13542 = CARTESIAN_POINT ( 'NONE',  ( 21.60000000000000142, 0.000000000000000000, 0.000000000000000000 ) ) ;
#13543 = CARTESIAN_POINT ( 'NONE',  ( 9.088029719595001055, 2.881930053949999682, -8.823338183322999129 ) ) ;
#13544 = CARTESIAN_POINT ( 'NONE',  ( 3.376658322786999733, 0.03754434462908000369, 3.214824333363999642 ) ) ;
#13545 = CARTESIAN_POINT ( 'NONE',  ( 10.95551720753999980, -4.744041807741999683, -9.198129812222999746 ) ) ;
#13546 = EDGE_CURVE ( 'NONE', #57286, #63228, #1283, .T. ) ;
#13547 = DIRECTION ( 'NONE',  ( 0.000000000000000000, -0.7071067811865475727, 0.7071067811865475727 ) ) ;
#13548 = CARTESIAN_POINT ( 'NONE',  ( 23.55654991076200133, 13.49867770468999950, 4.025919757528999554 ) ) ;
#13549 = B_SPLINE_CURVE_WITH_KNOTS ( 'NONE', 3,
 ( #60405, #65979, #54811, #45021 ),
 .UNSPECIFIED., .F., .F.,
 ( 4, 4 ),
 ( 0.8746029590009303245, 1.000000000000000000 ),
 .UNSPECIFIED. ) ;
#13550 = ORIENTED_EDGE ( 'NONE', *, *, #26487, .F. ) ;
#13551 = EDGE_CURVE ( 'NONE', #49429, #34400, #56731, .T. ) ;
#13552 = CIRCLE ( 'NONE', #12390, 11.84999999999999964 ) ;
#13553 = CARTESIAN_POINT ( 'NONE',  ( 11.63764426047339917, -3.386171819220400003, 6.538488127609999978 ) ) ;
#13554 = CARTESIAN_POINT ( 'NONE',  ( 9.910790522921001156, 3.869345236050000025, 5.882548872612999524 ) ) ;
#13555 = DIRECTION ( 'NONE',  ( 2.887756364190019784E-10, 0.06432770287658050312, 0.9979288284455070102 ) ) ;
#13556 = CARTESIAN_POINT ( 'NONE',  ( 7.886566940378000545, -3.084082018960999871, 9.259837032825000591 ) ) ;
#13558 = CARTESIAN_POINT ( 'NONE',  ( 9.218548476234555977, 2.654500937185336973, 7.609826956513907170 ) ) ;
#13557 = CARTESIAN_POINT ( 'NONE',  ( 10.87021720923999979, 2.226038107033000202, 7.782753921296999167 ) ) ;
#13559 = CARTESIAN_POINT ( 'NONE',  ( 11.06795257254739973, 3.036453385827900142, -7.780229861306499295 ) ) ;
#13560 = DIRECTION ( 'NONE',  ( 0.000000000000000000, -1.000000000000000000, 0.000000000000000000 ) ) ;
#13561 = CARTESIAN_POINT ( 'NONE',  ( 8.973138961223998677, 4.946050868436800307, -8.139313957553699908 ) ) ;
#13562 = CARTESIAN_POINT ( 'NONE',  ( 18.18883553772844408, -0.3494793053307401753, 12.59515668824706580 ) ) ;
#13563 = CYLINDRICAL_SURFACE ( 'NONE', #8203, 0.6999999999999992895 ) ;
#13564 = CARTESIAN_POINT ( 'NONE',  ( 0.7871629501879499058, -3.165274489958428195, -1.545762285366434563 ) ) ;
#13565 = CARTESIAN_POINT ( 'NONE',  ( 11.30000000000000071, -4.368599826607999503, -15.48886178036999972 ) ) ;
#13566 = ORIENTED_EDGE ( 'NONE', *, *, #57395, .T. ) ;
#13567 = CARTESIAN_POINT ( 'NONE',  ( 9.341483607044001047, -4.148132978932999926, 9.337467253566000380 ) ) ;
#13568 = CARTESIAN_POINT ( 'NONE',  ( 18.24660850951283919, 2.298559566806791299, 13.81002375772540880 ) ) ;
#13569 = CARTESIAN_POINT ( 'NONE',  ( 25.60000000000000142, 11.77655473258999841, -4.190794510628000680 ) ) ;
#13570 = FACE_OUTER_BOUND ( 'NONE', #32910, .T. ) ;
#13571 = ORIENTED_EDGE ( 'NONE', *, *, #6885, .F. ) ;
#13572 = CARTESIAN_POINT ( 'NONE',  ( 8.256676658772999389, 2.876288091423999660, 6.568897128359000526 ) ) ;
#13574 = CARTESIAN_POINT ( 'NONE',  ( 11.71922412107039868, 4.069539071394910223, 8.814426450544999625 ) ) ;
#13573 = CARTESIAN_POINT ( 'NONE',  ( 8.646410841231000788, 2.261390688294000029, -6.733978371730000134 ) ) ;
#13575 = AXIS2_PLACEMENT_3D ( 'NONE', #55989, #8094, #29438 ) ;
#13576 = CARTESIAN_POINT ( 'NONE',  ( 10.60770165877000082, 2.392327800351000011, -6.587345916039000215 ) ) ;
#13577 = ORIENTED_EDGE ( 'NONE', *, *, #58007, .F. ) ;
#13578 = ADVANCED_FACE ( 'NONE', ( #49515 ), #941, .T. ) ;
#13579 = CARTESIAN_POINT ( 'NONE',  ( 5.127943173016667799, -0.9218200799623714747, -1.199500263597270466 ) ) ;
#13580 = CARTESIAN_POINT ( 'NONE',  ( 17.97915611674150327, -3.110288500502089715, -13.65013405122915913 ) ) ;
#13581 = CARTESIAN_POINT ( 'NONE',  ( 10.54687750876899877, 3.382085645339300228, 6.541108991297599928 ) ) ;
#13582 = CARTESIAN_POINT ( 'NONE',  ( 10.00122642709000154, -2.274091010763000131, 7.851325450887000734 ) ) ;
#13583 = DIRECTION ( 'NONE',  ( 1.000000000000000000, 0.000000000000000000, 0.000000000000000000 ) ) ;
#13584 = ORIENTED_EDGE ( 'NONE', *, *, #45806, .F. ) ;
#13585 = CARTESIAN_POINT ( 'NONE',  ( 6.999999691988000095, -11.00717859340000082, 1.432487142323000118 ) ) ;
#13586 = EDGE_CURVE ( 'NONE', #10719, #56062, #42104, .T. ) ;
#13587 = EDGE_CURVE ( 'NONE', #35879, #49285, #64434, .T. ) ;
#13588 = CARTESIAN_POINT ( 'NONE',  ( 1.500973465873999935, 3.500000000000000000, 0.000000000000000000 ) ) ;
#13589 = CARTESIAN_POINT ( 'NONE',  ( 8.026781271869193546, -2.988395543640873786, 6.057288563851790819 ) ) ;
#13590 = CARTESIAN_POINT ( 'NONE',  ( 10.93227479887999998, -2.539880901735999785, 6.453614191797999666 ) ) ;
#13591 = CARTESIAN_POINT ( 'NONE',  ( 10.43614141025499897, -3.450366949021700158, -8.478951440767898973 ) ) ;
#13592 = CARTESIAN_POINT ( 'NONE',  ( 10.33527973160900082, -3.897539901865500145, 8.637205511891998810 ) ) ;
#13593 = ORIENTED_EDGE ( 'NONE', *, *, #54123, .T. ) ;
#13594 = CARTESIAN_POINT ( 'NONE',  ( 11.03703505992000089, -5.149240112441999528, -5.120435640197999128 ) ) ;
#13595 = CARTESIAN_POINT ( 'NONE',  ( 11.46118313518939935, -4.792748567750200195, 6.497569908212999401 ) ) ;
#13596 = ORIENTED_EDGE ( 'NONE', *, *, #54129, .F. ) ;
#13597 = CARTESIAN_POINT ( 'NONE',  ( 16.32027728219714291, -3.351613101375973791, -11.15747237328656460 ) ) ;
#13598 = ORIENTED_EDGE ( 'NONE', *, *, #63478, .T. ) ;
#13599 = CARTESIAN_POINT ( 'NONE',  ( 9.842321917838999568, -3.423478821957000040, -6.068694811299999436 ) ) ;
#13600 = CARTESIAN_POINT ( 'NONE',  ( 8.944760841233000193, 4.990139824845000405, -9.121472988377998803 ) ) ;
#13601 = CARTESIAN_POINT ( 'NONE',  ( 11.51145123989532948, 4.605239108938600445, -8.668865425277999748 ) ) ;
#13602 = DIRECTION ( 'NONE',  ( 0.000000000000000000, 0.000000000000000000, -1.000000000000000000 ) ) ;
#13603 = CARTESIAN_POINT ( 'NONE',  ( 12.23131043852896305, 2.748092942712452746, -12.39032383288960482 ) ) ;
#13604 = CARTESIAN_POINT ( 'NONE',  ( 12.20379573085659963, -2.893744357957000357, 7.308581953418300081 ) ) ;
#13605 = CARTESIAN_POINT ( 'NONE',  ( 11.23724174883999893, -4.024531238983009906, 6.608211443991299561 ) ) ;
#13606 = EDGE_CURVE ( 'NONE', #54965, #65525, #50817, .T. ) ;
#13607 = VERTEX_POINT ( 'NONE', #2912 ) ;
#13608 = CARTESIAN_POINT ( 'NONE',  ( 29.60000000000000142, 0.000000000000000000, 0.000000000000000000 ) ) ;
#13609 = CARTESIAN_POINT ( 'NONE',  ( 8.791230646795000325, -5.095088356574999366, 6.286978111459999852 ) ) ;
#13610 = CARTESIAN_POINT ( 'NONE',  ( 17.92010247869879791, 0.6380582630082767270, 13.98550026811474467 ) ) ;
#13611 = VERTEX_POINT ( 'NONE', #43941 ) ;
#13612 = CARTESIAN_POINT ( 'NONE',  ( 12.17424305300937526, -2.124765750614182824, -12.41957393385126807 ) ) ;
#13613 = CARTESIAN_POINT ( 'NONE',  ( 11.65456516821461008, 4.802916961510000249, 6.689681884064299311 ) ) ;
#13614 = CARTESIAN_POINT ( 'NONE',  ( 11.26847231345999845, -2.565616654150999931, -7.116622328138999976 ) ) ;
#13615 = CARTESIAN_POINT ( 'NONE',  ( 6.315443173016669576, 1.499999999999999778, 0.1963495408493654004 ) ) ;
#13616 = CARTESIAN_POINT ( 'NONE',  ( 17.61439135794200084, -11.93243341766000043, 3.259310185281999672 ) ) ;
#13617 = CARTESIAN_POINT ( 'NONE',  ( 9.041999884715581359, 3.843103124197280618, -8.691999950321772417 ) ) ;
#13618 = CARTESIAN_POINT ( 'NONE',  ( 12.33367687689871062, -2.910531109056639920, -13.57771726184491712 ) ) ;
#13619 = CARTESIAN_POINT ( 'NONE',  ( 5.103285156735999806, -1.342354185336999794, -0.7898986551783000465 ) ) ;
#13620 = FACE_OUTER_BOUND ( 'NONE', #20535, .T. ) ;
#13621 = CARTESIAN_POINT ( 'NONE',  ( 10.93656785386839836, -5.060279460151999587, -8.213529149347399638 ) ) ;
#13622 = DIRECTION ( 'NONE',  ( -1.000000000000000000, 0.000000000000000000, 0.000000000000000000 ) ) ;
#13623 = ORIENTED_EDGE ( 'NONE', *, *, #35828, .T. ) ;
#13624 = VERTEX_POINT ( 'NONE', #28200 ) ;
#13625 = DIRECTION ( 'NONE',  ( -1.000000000000000000, 0.000000000000000000, 0.000000000000000000 ) ) ;
#13626 = CARTESIAN_POINT ( 'NONE',  ( 18.11165249899354635, 2.784436927422415664, 13.60895423188022058 ) ) ;
#13627 = CARTESIAN_POINT ( 'NONE',  ( 23.63098035122899887, -3.423374544452999935, 13.57524279781000054 ) ) ;
#13628 = CARTESIAN_POINT ( 'NONE',  ( 13.43979992210466889, 11.65095899958523340, 2.173573044049638359 ) ) ;
#13629 = CARTESIAN_POINT ( 'NONE',  ( 17.93835418254524328, 2.006228213506225710, 12.55298903047910208 ) ) ;
#13630 = CARTESIAN_POINT ( 'NONE',  ( 21.72233714749290101, -5.999764115230404649, 0.05320302240984180892 ) ) ;
#13631 = CARTESIAN_POINT ( 'NONE',  ( 9.414312736919001168, 3.941041961981000430, 5.878350450964999752 ) ) ;
#13632 = EDGE_CURVE ( 'NONE', #31558, #61812, #67602, .T. ) ;
#13633 = CARTESIAN_POINT ( 'NONE',  ( 10.98768472633000037, -5.449702618601000026, 4.945212061625999134 ) ) ;
#13634 = ORIENTED_EDGE ( 'NONE', *, *, #8445, .T. ) ;
#13635 = CARTESIAN_POINT ( 'NONE',  ( 12.72249460523640963, -1.880133632676047384, 12.57461455596142663 ) ) ;
#13636 = CARTESIAN_POINT ( 'NONE',  ( 10.15958376188599921, -4.731143729777899765, -7.965979387614599894 ) ) ;
#13637 = CARTESIAN_POINT ( 'NONE',  ( 9.889842476439000052, 4.052276433608000161, 9.260531940735001299 ) ) ;
#13638 = CARTESIAN_POINT ( 'NONE',  ( 9.295853127542962113, -3.970210778477946345, 6.554146822010631368 ) ) ;
#13639 = CARTESIAN_POINT ( 'NONE',  ( 11.40425819896749893, 2.744109752373000255, -7.736761623643599428 ) ) ;
#13640 = CARTESIAN_POINT ( 'NONE',  ( 12.21006921427117398, 0.1916424759571752623, 12.69805926625132209 ) ) ;
#13641 = CARTESIAN_POINT ( 'NONE',  ( 8.443892219592001425, 2.905861847853000057, 8.940690431604000565 ) ) ;
#13642 = CARTESIAN_POINT ( 'NONE',  ( 9.414312736919001168, 3.941041961981000430, 5.878350450964999752 ) ) ;
#13643 = CARTESIAN_POINT ( 'NONE',  ( 12.75302363333805644, 1.877081947669209328, 12.57507557223850903 ) ) ;
#13644 = ORIENTED_EDGE ( 'NONE', *, *, #43008, .T. ) ;
#13645 = CARTESIAN_POINT ( 'NONE',  ( 8.997439158776000312, 2.773858540272000184, -8.951250717848999727 ) ) ;
#13646 = CARTESIAN_POINT ( 'NONE',  ( 11.30579707368350029, 3.365167912142600137, -6.390809033205999690 ) ) ;
#13647 = B_SPLINE_CURVE_WITH_KNOTS ( 'NONE', 3,
 ( #46703, #68007, #19783, #19436, #41452 ),
 .UNSPECIFIED., .F., .F.,
 ( 4, 1, 4 ),
 ( 0.000000000000000000, 0.006423492687020981168, 0.1253905405517105054 ),
 .UNSPECIFIED. ) ;
#13648 = CARTESIAN_POINT ( 'NONE',  ( 10.82095911837782154, -4.087393693045735077, 9.237492157467196208 ) ) ;
#13650 = CARTESIAN_POINT ( 'NONE',  ( 3.333982310585333231, -1.775032085411882177, -3.050824490492882735 ) ) ;
#13649 = CARTESIAN_POINT ( 'NONE',  ( 8.689254440380000943, -2.550228841911000188, 7.666975032000999946 ) ) ;
#13651 = CARTESIAN_POINT ( 'NONE',  ( 10.26130484851599967, -3.086535948898899928, 7.082356937474298952 ) ) ;
#13652 = CARTESIAN_POINT ( 'NONE',  ( 10.77256919669529900, -3.037654633983899899, -7.784327714719899483 ) ) ;
#13653 = VERTEX_POINT ( 'NONE', #17717 ) ;
#13654 = VECTOR ( 'NONE', #41711, 1000.000000000000000 ) ;
#13655 = CARTESIAN_POINT ( 'NONE',  ( 1.491428256769000038, 2.689776413290000168, 2.380956047316999946 ) ) ;
#13656 = CARTESIAN_POINT ( 'NONE',  ( 18.06967961652323496, -0.3547743934310131353, -12.69333341030272067 ) ) ;
#13657 = CARTESIAN_POINT ( 'NONE',  ( 0.8933122983452270738, 3.086673542548771021, -1.352482486230435210 ) ) ;
#13658 = CARTESIAN_POINT ( 'NONE',  ( 18.07075314650775155, -2.853223032316301033, 13.59217294861099035 ) ) ;
#13659 = CARTESIAN_POINT ( 'NONE',  ( 9.957462135714001406, 5.100000000000000533, -6.571291218949999902 ) ) ;
#13660 = CARTESIAN_POINT ( 'NONE',  ( 12.32491409494626211, -3.065531103753984077, 13.66026219579215351 ) ) ;
#13661 = DIRECTION ( 'NONE',  ( 0.000000000000000000, -0.9421243786071880066, 0.3352635608502960163 ) ) ;
#13662 = CYLINDRICAL_SURFACE ( 'NONE', #912, 1.500000000000000000 ) ;
#13663 = CARTESIAN_POINT ( 'NONE',  ( 7.795980646793000624, -3.164807285701999984, 9.104732190648000767 ) ) ;
#13664 = ORIENTED_EDGE ( 'NONE', *, *, #33962, .F. ) ;
#13665 = CARTESIAN_POINT ( 'NONE',  ( 8.946010841230998878, 5.458692773671000253, 7.456452194274000078 ) ) ;
#13666 = EDGE_CURVE ( 'NONE', #20140, #63182, #35917, .T. ) ;
#13667 = LINE ( 'NONE', #23803, #36240 ) ;
#13668 = CARTESIAN_POINT ( 'NONE',  ( 7.437825695874983545, -2.276412617413176687, 7.746772493203951448 ) ) ;
#13669 = AXIS2_PLACEMENT_3D ( 'NONE', #2201, #7088, #44517 ) ;
#13670 = CARTESIAN_POINT ( 'NONE',  ( 17.86532676363442107, -0.5429298016068462296, 13.88573085157524112 ) ) ;
#13671 = CARTESIAN_POINT ( 'NONE',  ( 1.218746307330000000, 3.398721108301999916, 0.4283847067656000318 ) ) ;
#13672 = VERTEX_POINT ( 'NONE', #51495 ) ;
#13673 = DIRECTION ( 'NONE',  ( 0.000000000000000000, 0.000000000000000000, -1.000000000000000000 ) ) ;
#13674 = CARTESIAN_POINT ( 'NONE',  ( 21.54999911806000057, 1.172395514003999961E-13, -2.486899575159999765E-14 ) ) ;
#13675 = CARTESIAN_POINT ( 'NONE',  ( 10.11260611051000069, 3.359887741436999864, 5.859127722154000573 ) ) ;
#13676 = CARTESIAN_POINT ( 'NONE',  ( 11.75718044953559804, 4.889766368533900120, 7.036033215662999218 ) ) ;
#13677 = AXIS2_PLACEMENT_3D ( 'NONE', #22029, #59098, #27638 ) ;
#13678 = CARTESIAN_POINT ( 'NONE',  ( 23.66004879239100234, -9.998911572074998588, 9.691526907171001071 ) ) ;
#13679 = CARTESIAN_POINT ( 'NONE',  ( 11.35905860703999970, -2.719090443614000208, -7.157642341559000698 ) ) ;
#13680 = CARTESIAN_POINT ( 'NONE',  ( 15.89994436294300151, -8.847904542234999781, -8.580301953175000662 ) ) ;
#13681 = CARTESIAN_POINT ( 'NONE',  ( 11.08810207955139937, 3.203462856645999945, 7.825000000000000178 ) ) ;
#13682 = CARTESIAN_POINT ( 'NONE',  ( 12.18526316314726365, -2.581188759560296919, 12.43231204081571661 ) ) ;
#13683 = EDGE_CURVE ( 'NONE', #46774, #15621, #36800, .T. ) ;
#13684 = CARTESIAN_POINT ( 'NONE',  ( 8.435568070370525362, 2.274764478101395149, 7.822608341263479481 ) ) ;
#13685 = ORIENTED_EDGE ( 'NONE', *, *, #33147, .T. ) ;
#13686 = CARTESIAN_POINT ( 'NONE',  ( 17.81260085050724129, -3.200899519495056023, 13.62917211583034671 ) ) ;
#13687 = CARTESIAN_POINT ( 'NONE',  ( 17.71839800377850338, 3.104623491297676452, -13.52646211264892706 ) ) ;
#13688 = ORIENTED_EDGE ( 'NONE', *, *, #39332, .F. ) ;
#13689 = DIRECTION ( 'NONE',  ( -1.000000000000000000, 0.000000000000000000, 0.000000000000000000 ) ) ;
#13690 = EDGE_CURVE ( 'NONE', #18862, #39042, #52127, .T. ) ;
#13691 = CARTESIAN_POINT ( 'NONE',  ( 10.65413259636999932, 3.216622244594500302, 7.073141822156699732 ) ) ;
#13692 = CARTESIAN_POINT ( 'NONE',  ( 5.243573426643169277, -0.5273870646426602748, 1.002916043689504377 ) ) ;
#13693 = CARTESIAN_POINT ( 'NONE',  ( 23.56665676678100141, 1.192379528446999839E-13, -4.982680934517999418E-13 ) ) ;
#13694 = CARTESIAN_POINT ( 'NONE',  ( 10.99433665574000152, 3.697618584609999814, 5.729302299903000772 ) ) ;
#13695 = CARTESIAN_POINT ( 'NONE',  ( 11.01002959534999981, 3.180718072098000171, -6.283812549199000230 ) ) ;
#13696 = CARTESIAN_POINT ( 'NONE',  ( 9.378875014952626543, -3.131883468830893857, -7.390885577342253931 ) ) ;
#13697 = CARTESIAN_POINT ( 'NONE',  ( 9.813358178091998951, -5.349400659402999914, 6.657024270273000255 ) ) ;
#13698 = CARTESIAN_POINT ( 'NONE',  ( 18.27397540914052598, -0.09367178904474234014, -12.59965724591066660 ) ) ;
#13699 = CARTESIAN_POINT ( 'NONE',  ( 23.59999445750599989, -13.22316420035999940, -4.267800004853000040 ) ) ;
#13700 = CARTESIAN_POINT ( 'NONE',  ( 10.43210941423799909, -3.358814833524500276, -6.917608226833099394 ) ) ;
#13701 = DIRECTION ( 'NONE',  ( 0.000000000000000000, 0.000000000000000000, 1.000000000000000000 ) ) ;
#13702 = ORIENTED_EDGE ( 'NONE', *, *, #58517, .F. ) ;
#13703 =( REPRESENTATION_RELATIONSHIP ('NONE','NONE', #10823, #8579 ) REPRESENTATION_RELATIONSHIP_WITH_TRANSFORMATION ( #54322 )SHAPE_REPRESENTATION_RELATIONSHIP( ) );
#13704 = CARTESIAN_POINT ( 'NONE',  ( 11.12439163055999991, -6.498888995361999932, -5.558825371164000551 ) ) ;
#13705 = AXIS2_PLACEMENT_3D ( 'NONE', #6482, #23263, #27473 ) ;
#13706 =( LENGTH_UNIT ( ) NAMED_UNIT ( * ) SI_UNIT ( .MILLI., .METRE. ) );
#13707 = CARTESIAN_POINT ( 'NONE',  ( 10.63652412148805659, 3.218092512488175849, -4.773914205603903227 ) ) ;
#13708 = CARTESIAN_POINT ( 'NONE',  ( 8.978248830702483474, 4.955089878105851220, 6.882626671536596241 ) ) ;
#13709 = CARTESIAN_POINT ( 'NONE',  ( 9.127126402770999292, 5.196937059091999878, -7.048639765412399782 ) ) ;
#13710 = CARTESIAN_POINT ( 'NONE',  ( 12.32516769934781209, 3.065409648700728074, 13.66028300215598890 ) ) ;
#13711 = CARTESIAN_POINT ( 'NONE',  ( 10.22399006116000031, -5.507891002176999784, 6.589804341508000540 ) ) ;
#13712 = ORIENTED_EDGE ( 'NONE', *, *, #40786, .F. ) ;
#13713 = CARTESIAN_POINT ( 'NONE',  ( 12.24298814206631825, -0.2740984088879005465, -12.69603503204707096 ) ) ;
#13714 = CARTESIAN_POINT ( 'NONE',  ( 12.14435534536354844, 0.3008963210924944232, 13.99677033988233354 ) ) ;
#13715 = ORIENTED_EDGE ( 'NONE', *, *, #6686, .T. ) ;
#13716 = DIRECTION ( 'NONE',  ( -1.000000000000000000, 0.000000000000000000, 0.000000000000000000 ) ) ;
#13717 = DIRECTION ( 'NONE',  ( 1.000000000000000000, -1.776356839420000071E-14, 1.776356839420000071E-14 ) ) ;
#13718 = CARTESIAN_POINT ( 'NONE',  ( 23.64690940319799850, -3.329270756416000232, -13.50285105039000122 ) ) ;
#13719 = FACE_OUTER_BOUND ( 'NONE', #58914, .T. ) ;
#13720 = AXIS2_PLACEMENT_3D ( 'NONE', #14022, #51415, #23470 ) ;
#13721 = CARTESIAN_POINT ( 'NONE',  ( 8.667306314937334832, 5.079264019707368405, -8.329425799205553815 ) ) ;
#13722 = CARTESIAN_POINT ( 'NONE',  ( 0.1043854016219000064, 3.484641797009000008, -0.6100991035018999975 ) ) ;
#13723 = CARTESIAN_POINT ( 'NONE',  ( -15.86200481174999943, 2.399999999999999911, -6.571291218949999902 ) ) ;
#13724 = CARTESIAN_POINT ( 'NONE',  ( 12.48183889708581695, 3.124385432114247685, 12.20648365185189377 ) ) ;
#13725 = CARTESIAN_POINT ( 'NONE',  ( 9.436149330669000079, -3.485164486501000081, -6.221839249167999242 ) ) ;
#13726 = CARTESIAN_POINT ( 'NONE',  ( 10.75210807141120029, 4.040019166404060336, -8.365272822098500427 ) ) ;
#13727 = CARTESIAN_POINT ( 'NONE',  ( 18.29995268966800026, 2.861739928647000220, 11.98821236628000086 ) ) ;
#13728 = DIRECTION ( 'NONE',  ( 0.000000000000000000, 0.000000000000000000, -1.000000000000000000 ) ) ;
#13729 = CARTESIAN_POINT ( 'NONE',  ( 9.480671671056999372, 2.873958896683999953, -7.689118697196099639 ) ) ;
#13731 = CARTESIAN_POINT ( 'NONE',  ( 12.21194436378594972, 2.301855881723279040, 12.49553541603377838 ) ) ;
#13730 = CARTESIAN_POINT ( 'NONE',  ( 17.55505043854143565, 3.125000000000000000, -25.00000000000000000 ) ) ;
#13732 = LINE ( 'NONE', #51132, #65379 ) ;
#13733 = ORIENTED_EDGE ( 'NONE', *, *, #64064, .F. ) ;
#13734 = CARTESIAN_POINT ( 'NONE',  ( 11.31900581613029821, 4.750686773407899466, 7.017964743997199939 ) ) ;
#13735 = CARTESIAN_POINT ( 'NONE',  ( 9.786673210037999837, -2.381198102024000285, 7.612749732462000374 ) ) ;
#13736 = CARTESIAN_POINT ( 'NONE',  ( 9.401721904869997815, 4.875830726371099821, 7.008306153105300140 ) ) ;
#13737 = CARTESIAN_POINT ( 'NONE',  ( 9.074925248765625341, 3.255423617190434271, -7.040502144637257764 ) ) ;
#13738 = CARTESIAN_POINT ( 'NONE',  ( 7.100000000000000533, -13.04986661130000059, 1.811520473896000016 ) ) ;
#13739 = CARTESIAN_POINT ( 'NONE',  ( 12.39223264510076561, 2.969378069107369011, 13.56257646889492818 ) ) ;
#13740 = CARTESIAN_POINT ( 'NONE',  ( 11.59999999999999964, -4.000000000000000000, -7.500000000000000000 ) ) ;
#13741 = ORIENTED_EDGE ( 'NONE', *, *, #38169, .F. ) ;
#13742 = ADVANCED_FACE ( 'NONE', ( #67913 ), #20029, .F. ) ;
#13743 = EDGE_CURVE ( 'NONE', #59745, #6314, #41734, .T. ) ;
#13744 = CARTESIAN_POINT ( 'NONE',  ( 8.771455549952998254, -3.111370763671500228, -6.783011486330899231 ) ) ;
#13745 = TOROIDAL_SURFACE ( 'NONE', #51661, 13.79999999999999893, 0.2000000000000000111 ) ;
#13746 = CARTESIAN_POINT ( 'NONE',  ( 8.668612063652194166, 4.202134689404237733, 5.871184905935877829 ) ) ;
#13747 = PRODUCT ( 'O Ring Seal 3', 'O Ring Seal 3', '', ( #40742 ) ) ;
#13748 = CARTESIAN_POINT ( 'NONE',  ( 18.07990072965510464, 1.983698511703259948, -12.44287000959587175 ) ) ;
#13749 = CARTESIAN_POINT ( 'NONE',  ( 10.88829480895999957, -2.943348573720999894, 5.042864669073000350 ) ) ;
#13750 = CARTESIAN_POINT ( 'NONE',  ( 21.72233714749290101, 5.000000000000000000, 0.000000000000000000 ) ) ;
#13751 = CARTESIAN_POINT ( 'NONE',  ( 12.29688428856856852, 2.864514977098406856, -13.58937626179519143 ) ) ;
#13752 = CARTESIAN_POINT ( 'NONE',  ( 9.707908211423999845, -3.300107492866999781, -5.762405935562999737 ) ) ;
#13753 = CARTESIAN_POINT ( 'NONE',  ( 0.8843067992085332785, -1.762666431298145930, -3.058252359239904905 ) ) ;
#13754 = ORIENTED_EDGE ( 'NONE', *, *, #68169, .F. ) ;
#13755 = CARTESIAN_POINT ( 'NONE',  ( 0.000000000000000000, -0.3800960799355100894, -2.899897457380500310 ) ) ;
#13756 = CARTESIAN_POINT ( 'NONE',  ( 11.04678944127999962, -5.235596213805000509, -5.039805523473999571 ) ) ;
#13757 = CARTESIAN_POINT ( 'NONE',  ( 24.30000000000000071, -8.810505093353000916, -8.810505093353000916 ) ) ;
#13758 = DIRECTION ( 'NONE',  ( 0.000000000000000000, 1.000000000000000000, 0.000000000000000000 ) ) ;
#13759 = DIRECTION ( 'NONE',  ( 0.000000000000000000, 0.9989394889204477046, 0.04604234437292184512 ) ) ;
#13760 = CARTESIAN_POINT ( 'NONE',  ( 18.29058462261052753, -11.07487261139573143, 3.615341608536529083 ) ) ;
#13762 = CIRCLE ( 'NONE', #52833, 1.625000000000000000 ) ;
#13761 = CARTESIAN_POINT ( 'NONE',  ( 12.35979573085659844, -3.159987984332300215, 7.354650721737899133 ) ) ;
#13763 = ORIENTED_EDGE ( 'NONE', *, *, #22466, .T. ) ;
#13764 = CARTESIAN_POINT ( 'NONE',  ( 9.125465313390733968, -5.349725526283760857, -7.676666018642554157 ) ) ;
#13765 = CARTESIAN_POINT ( 'NONE',  ( 17.88876975676773640, 1.869670916578580533, -13.87459417580158316 ) ) ;
#13766 = ORIENTED_EDGE ( 'NONE', *, *, #39815, .T. ) ;
#13767 = EDGE_CURVE ( 'NONE', #40775, #20272, #25892, .T. ) ;
#13768 = CARTESIAN_POINT ( 'NONE',  ( 9.908709346416999963, -3.216804796119200116, 7.871904849557299855 ) ) ;
#13770 = CARTESIAN_POINT ( 'NONE',  ( 8.863029719594999634, 2.990001567622999623, -8.695425648791999862 ) ) ;
#13769 = VECTOR ( 'NONE', #29186, 1000.000000000000114 ) ;
#13771 = CARTESIAN_POINT ( 'NONE',  ( 7.931011803055000975, 3.387313518888000363, -6.297038610257000180 ) ) ;
#13772 = CARTESIAN_POINT ( 'NONE',  ( 10.81524174883999834, -4.028418853626810403, -8.533115712456000423 ) ) ;
#13773 = CARTESIAN_POINT ( 'NONE',  ( 18.05195279581856127, 0.3792326063240399336, -12.69238213822339567 ) ) ;
#13774 = CARTESIAN_POINT ( 'NONE',  ( 11.03775575519999919, -8.050335494570999728, 6.914609630061999468 ) ) ;
#13775 = VERTEX_POINT ( 'NONE', #4283 ) ;
#13776 = CARTESIAN_POINT ( 'NONE',  ( 8.002383708823000319, 5.117451078405999887, -6.702236199791999915 ) ) ;
#13777 =( BOUNDED_SURFACE ( )  B_SPLINE_SURFACE ( 3, 3, ( 
 ( #1185, #1525, #44544, #22494, #17962, #39280, #12712, #23540 ),
 ( #39628, #60949, #13064, #7808, #14438, #19325, #29845, #35759 ),
 ( #19678, #25260, #45902, #8497, #20361, #36097, #3582, #14778 ),
 ( #46599, #51486, #57074, #61983, #56745, #34733, #46937, #57412 ) ),
 .UNSPECIFIED., .F., .F., .F. ) 
 B_SPLINE_SURFACE_WITH_KNOTS ( ( 4, 4 ),
 ( 4, 1, 1, 1, 1, 4 ),
 ( 0.000000000000000000, 1.000000000000000000 ),
 ( 0.8111870735734000304, 0.8462787474214000794, 0.8943647847192999212, 0.9442642648822999751, 1.000000000000000000, 1.006078322774000000 ),
 .UNSPECIFIED. ) 
 GEOMETRIC_REPRESENTATION_ITEM ( )  RATIONAL_B_SPLINE_SURFACE ( (
 ( 1.221012505305000051, 1.221012505305000051, 1.221012505305000051, 1.221012505305000051, 1.221012505305000051, 1.221012505305000051, 1.221012505305000051, 1.221012505305000051),
 ( 0.9263291648981999415, 0.9263291648981999415, 0.9263291648981999415, 0.9263291648981999415, 0.9263291648981999415, 0.9263291648981999415, 0.9263291648981999415, 0.9263291648981999415),
 ( 0.9263291648981999415, 0.9263291648981999415, 0.9263291648981999415, 0.9263291648981999415, 0.9263291648981999415, 0.9263291648981999415, 0.9263291648981999415, 0.9263291648981999415),
 ( 1.221012505305000051, 1.221012505305000051, 1.221012505305000051, 1.221012505305000051, 1.221012505305000051, 1.221012505305000051, 1.221012505305000051, 1.221012505305000051) ) ) 
 REPRESENTATION_ITEM ( '' )  SURFACE ( )  );
#13778 = CARTESIAN_POINT ( 'NONE',  ( 17.59614113504008159, -3.125000000000000888, -13.52078631348664217 ) ) ;
#13779 = CARTESIAN_POINT ( 'NONE',  ( 8.500189158773000742, 2.724453559418999582, -8.908010318766001134 ) ) ;
#13780 = ORIENTED_EDGE ( 'NONE', *, *, #5676, .T. ) ;
#13781 = CARTESIAN_POINT ( 'NONE',  ( 10.46009300862000124, 2.565654508827999614, -6.975684004278000394 ) ) ;
#13782 = CARTESIAN_POINT ( 'NONE',  ( 10.99600480934999958, -8.065001534460998656, 6.834777879866000383 ) ) ;
#13783 = VERTEX_POINT ( 'NONE', #10222 ) ;
#13784 = CARTESIAN_POINT ( 'NONE',  ( 9.227380199234000102, 5.132898093246000215, 7.642395078236999595 ) ) ;
#13785 = B_SPLINE_CURVE_WITH_KNOTS ( 'NONE', 3,
 ( #57448, #30551, #3963, #9558, #4311, #46976, #68280, #20400, #64063, #33311 ),
 .UNSPECIFIED., .F., .F.,
 ( 4, 2, 2, 2, 4 ),
 ( 0.000000000000000000, 0.2500000000000003331, 0.5000000000000006661, 0.7500000000000003331, 1.000000000000000000 ),
 .UNSPECIFIED. ) ;
#13786 = CARTESIAN_POINT ( 'NONE',  ( 17.65794081825379180, -1.883184384514173360, -12.57407373858317534 ) ) ;
#13787 = LINE ( 'NONE', #19716, #17341 ) ;
#13788 = B_SPLINE_CURVE_WITH_KNOTS ( 'NONE', 3,
 ( #36723, #68172, #30445, #9793, #20289, #31144, #67144, #62250, #4201, #40582 ),
 .UNSPECIFIED., .F., .F.,
 ( 4, 2, 2, 2, 4 ),
 ( 0.000000000000000000, 0.2500000000000002220, 0.5000000000000004441, 0.7500000000000002220, 1.000000000000000000 ),
 .UNSPECIFIED. ) ;
#13789 = DIRECTION ( 'NONE',  ( 0.9999999999976796339, 1.847154591387964169E-06, 1.108402172101977569E-06 ) ) ;
#13790 = CARTESIAN_POINT ( 'NONE',  ( 9.446897644051269083, -2.250365900417164777, 7.566722005472066748 ) ) ;
#13791 = VERTEX_POINT ( 'NONE', #31554 ) ;
#13792 = CARTESIAN_POINT ( 'NONE',  ( 11.59999999999999964, 3.186931496511417272, 6.962391415777370973 ) ) ;
#13793 = CIRCLE ( 'NONE', #65115, 2.000000000000000444 ) ;
#13794 = CARTESIAN_POINT ( 'NONE',  ( 9.865944350586199008, -5.673398084260703023, -8.064521635305629488 ) ) ;
#13795 = CARTESIAN_POINT ( 'NONE',  ( 24.30001685126999789, 8.938702716825000394, -8.938676159935001309 ) ) ;
#13796 = CARTESIAN_POINT ( 'NONE',  ( 12.11714050632479100, 2.287289704013984792, -13.81189467606769306 ) ) ;
#13797 = VECTOR ( 'NONE', #59284, 1000.000000000000227 ) ;
#13798 = CARTESIAN_POINT ( 'NONE',  ( 9.986304848515999311, -2.961576783819000358, -7.974775391194199869 ) ) ;
#13799 = CARTESIAN_POINT ( 'NONE',  ( 10.71756905878999966, -3.040221764047000175, 8.808455607108001573 ) ) ;
#13800 = CARTESIAN_POINT ( 'NONE',  ( 17.55505043854147118, -3.125000000000000000, -12.28373071562070074 ) ) ;
#13801 = CARTESIAN_POINT ( 'NONE',  ( 10.97571094393200042, -2.824289056067999848, 6.306988371318333897 ) ) ;
#13802 = EDGE_CURVE ( 'NONE', #1219, #43427, #60066, .T. ) ;
#13803 = EDGE_CURVE ( 'NONE', #24516, #11716, #3346, .T. ) ;
#13804 = ORIENTED_EDGE ( 'NONE', *, *, #10722, .F. ) ;
#13805 = ORIENTED_EDGE ( 'NONE', *, *, #37169, .F. ) ;
#13806 = CARTESIAN_POINT ( 'NONE',  ( 10.11453584122999949, 5.322769172805999816, -7.951018786192998178 ) ) ;
#13807 = CARTESIAN_POINT ( 'NONE',  ( 7.307500000000000107, 0.2999999999999999889, 3.149999999999999911 ) ) ;
#13808 = CARTESIAN_POINT ( 'NONE',  ( 10.41164068750946825, 2.873222873834231805, -6.752018918838227357 ) ) ;
#13809 = CARTESIAN_POINT ( 'NONE',  ( 24.00946664458725266, 3.345587221009647561, 12.72975888196361893 ) ) ;
#13810 = CARTESIAN_POINT ( 'NONE',  ( 23.83637295000900025, 9.655512588674998398, -9.482097233574000583 ) ) ;
#13811 = CARTESIAN_POINT ( 'NONE',  ( 18.53573769406200356, -2.787008136214999876, -11.27235516822999983 ) ) ;
#13813 = LINE ( 'NONE', #46998, #16127 ) ;
#13812 = CARTESIAN_POINT ( 'NONE',  ( 9.500480666858999612, -3.573487373903700082, 6.293984733123999753 ) ) ;
#13814 = AXIS2_PLACEMENT_3D ( 'NONE', #36378, #52806, #14715 ) ;
#13815 = CARTESIAN_POINT ( 'NONE',  ( 4.565443173016666911, -1.500000000000000222, -0.1963495408493622363 ) ) ;
#13816 = ORIENTED_EDGE ( 'NONE', *, *, #3302, .T. ) ;
#13817 = CARTESIAN_POINT ( 'NONE',  ( 10.42702554439000195, -2.952854773874999950, 4.671719621119999388 ) ) ;
#13818 = AXIS2_PLACEMENT_3D ( 'NONE', #40526, #61852, #62195 ) ;
#13819 = CARTESIAN_POINT ( 'NONE',  ( 10.59654005035000068, -3.014401618106000047, -5.075934621078999953 ) ) ;
#13820 = CARTESIAN_POINT ( 'NONE',  ( 9.666315108303999537, -3.197530835772000035, -8.817973615970998935 ) ) ;
#13821 = CARTESIAN_POINT ( 'NONE',  ( 18.11574795581002562, 0.2761699508452412077, 12.69595998167824114 ) ) ;
#13822 = PLANE ( 'NONE',  #10887 ) ;
#13823 = CARTESIAN_POINT ( 'NONE',  ( 8.573148997459998810, 5.167567567567999731, -6.822293592207000934 ) ) ;
#13824 = CARTESIAN_POINT ( 'NONE',  ( 9.491735841231999871, 3.920043641733999884, -9.398198753036000497 ) ) ;
#13825 = EDGE_CURVE ( 'NONE', #6251, #60622, #51837, .T. ) ;
#13826 = CARTESIAN_POINT ( 'NONE',  ( 10.93656785386839836, 2.939720539848000413, 6.786470850652599474 ) ) ;
#13827 = EDGE_CURVE ( 'NONE', #46698, #35849, #14104, .T. ) ;
#13828 = B_SPLINE_CURVE_WITH_KNOTS ( 'NONE', 3,
 ( #10983, #32323, #48738, #20788, #59565 ),
 .UNSPECIFIED., .F., .F.,
 ( 4, 1, 4 ),
 ( 0.000000000000000000, 0.5000000000000000000, 1.000000000000000000 ),
 .UNSPECIFIED. ) ;
#13829 = DIRECTION ( 'NONE',  ( 1.000000000000000000, 0.000000000000000000, 0.000000000000000000 ) ) ;
#13830 = DIRECTION ( 'NONE',  ( 0.000000000000000000, 0.000000000000000000, -1.000000000000000000 ) ) ;
#13831 = CARTESIAN_POINT ( 'NONE',  ( 9.343930206849998754, 2.750000000000000000, 7.500000000000000000 ) ) ;
#13832 = ORIENTED_EDGE ( 'NONE', *, *, #52080, .F. ) ;
#13833 = CARTESIAN_POINT ( 'NONE',  ( 12.72146951531671633, 0.7145943380091474006, -12.57972004139935152 ) ) ;
#13834 = CARTESIAN_POINT ( 'NONE',  ( 12.02531641787287597, -4.339035680702311382, 8.308706962315561384 ) ) ;
#13835 = CARTESIAN_POINT ( 'NONE',  ( 13.49994651945300284, 12.07042783918999795, 2.492331243371999960 ) ) ;
#13836 = CARTESIAN_POINT ( 'NONE',  ( 7.100000000000000533, -12.35000000006999876, 0.000000000000000000 ) ) ;
#13837 = CARTESIAN_POINT ( 'NONE',  ( 10.12947109217999930, -5.100000000000000533, 6.152188490330000370 ) ) ;
#13838 = ORIENTED_EDGE ( 'NONE', *, *, #1173, .F. ) ;
#13839 = CARTESIAN_POINT ( 'NONE',  ( 5.924991087009000346, -1.272350122907000003, -0.3600015818555999947 ) ) ;
#13840 = CIRCLE ( 'NONE', #53388, 0.3000000000000004330 ) ;
#13841 = CARTESIAN_POINT ( 'NONE',  ( 10.96031085658187720, 8.907343134533192597, 6.453647402135471722 ) ) ;
#13842 = LINE ( 'NONE', #34493, #60006 ) ;
#13843 = CARTESIAN_POINT ( 'NONE',  ( 1.605140132540249898, 0.9161175952574701631, 3.408904368339106927 ) ) ;
#13844 = CARTESIAN_POINT ( 'NONE',  ( 11.18923293495519822, 2.967327562101000016, -7.458486839450950256 ) ) ;
#13845 = ORIENTED_EDGE ( 'NONE', *, *, #56376, .T. ) ;
#13846 = VECTOR ( 'NONE', #46382, 1000.000000000000000 ) ;
#13847 = CARTESIAN_POINT ( 'NONE',  ( 9.590594544025000445, -2.445960766574000189, 7.841185849078001091 ) ) ;
#13848 = ORIENTED_EDGE ( 'NONE', *, *, #4865, .T. ) ;
#13849 = ADVANCED_FACE ( 'NONE', ( #62999 ), #15128, .F. ) ;
#13850 = CARTESIAN_POINT ( 'NONE',  ( 8.507041456382204103, -3.224154684601456822, 6.000520319185582707 ) ) ;
#13851 = CARTESIAN_POINT ( 'NONE',  ( 8.817629440380001071, -3.894643656844000379, 6.044452984962999764 ) ) ;
#13852 = CARTESIAN_POINT ( 'NONE',  ( 18.13088524799817947, 0.4443071882833261599, -13.99296005428181466 ) ) ;
#13853 = ORIENTED_EDGE ( 'NONE', *, *, #14414, .T. ) ;
#13854 = CARTESIAN_POINT ( 'NONE',  ( 10.94310967158117798, 9.262160174352873199, -6.269908194909642241 ) ) ;
#13855 = CARTESIAN_POINT ( 'NONE',  ( 11.07503769033554342, -4.268003910456493522, -9.025037683630598551 ) ) ;
#13856 = CARTESIAN_POINT ( 'NONE',  ( 10.27101354018333446, -4.768183399968641822, 8.499583552997725278 ) ) ;
#13857 = CARTESIAN_POINT ( 'NONE',  ( 25.34046362424712839, 8.480593820237956493, -7.990867062144727306 ) ) ;
#13858 = CARTESIAN_POINT ( 'NONE',  ( 18.06426550930201458, -2.862542805000389823, 12.35969564690757316 ) ) ;
#13859 = ORIENTED_EDGE ( 'NONE', *, *, #8835, .F. ) ;
#13860 = CARTESIAN_POINT ( 'NONE',  ( 10.83668192271000130, -4.288535286065000562, 9.448729895547000268 ) ) ;
#13861 = CARTESIAN_POINT ( 'NONE',  ( 11.60000000000000142, 4.813860086966100127, 8.315594847681079926 ) ) ;
#13862 = DIRECTION ( 'NONE',  ( 0.000000000000000000, -1.000000000000000000, 0.000000000000000000 ) ) ;
#13863 = CARTESIAN_POINT ( 'NONE',  ( 9.821013540182335078, 3.231816600031359510, 8.499583552997727054 ) ) ;
#13864 = PRESENTATION_LAYER_ASSIGNMENT (  '', '', ( #6002 ) ) ;
#13865 = DIRECTION ( 'NONE',  ( -0.7071067811865474617, -0.7071067811865474617, -9.650793108809640698E-10 ) ) ;
#13866 = VERTEX_POINT ( 'NONE', #20715 ) ;
#13867 = CARTESIAN_POINT ( 'NONE',  ( 23.67741368841328864, 13.18816119140440257, -3.924050752104807138 ) ) ;
#13868 = CARTESIAN_POINT ( 'NONE',  ( 10.91620964606000044, -2.818413279081999789, -6.814156272943999504 ) ) ;
#13869 = CARTESIAN_POINT ( 'NONE',  ( 10.70259330317452751, 2.712330661039021429, 7.031802534341066391 ) ) ;
#13870 = CARTESIAN_POINT ( 'NONE',  ( 24.03543971961891401, -3.344494741195767062, -12.68172832290301777 ) ) ;
#13871 = CARTESIAN_POINT ( 'NONE',  ( 3.073890132543958043, 2.150913519912194705, 2.798833948393636639 ) ) ;
#13872 = AXIS2_PLACEMENT_3D ( 'NONE', #18648, #35083, #24580 ) ;
#13873 = CARTESIAN_POINT ( 'NONE',  ( 12.19004662364084091, -0.1118032413084504434, -13.89939982891984904 ) ) ;
#13874 = CARTESIAN_POINT ( 'NONE',  ( 18.16983287387829549, -2.613005487247105574, 12.42455217891717467 ) ) ;
#13875 = EDGE_LOOP ( 'NONE', ( #30473, #2066, #68028, #37823 ) ) ;
#13876 = CARTESIAN_POINT ( 'NONE',  ( 11.02301463001509774, -3.452642973349600464, -6.623338154204899908 ) ) ;
#13877 = ORIENTED_EDGE ( 'NONE', *, *, #40286, .F. ) ;
#13878 = CARTESIAN_POINT ( 'NONE',  ( 9.903950872528001881, 5.205009505618999555, 6.747225973806000532 ) ) ;
#13879 = CARTESIAN_POINT ( 'NONE',  ( 25.39940339878695852, -11.19882859648231666, 3.252360728051921335 ) ) ;
#13880 = CARTESIAN_POINT ( 'NONE',  ( 9.816185841232000442, 2.656512020013999997, -7.884832994446999699 ) ) ;
#13881 = B_SPLINE_CURVE_WITH_KNOTS ( 'NONE', 3,
 ( #36371, #10483, #4542, #4890 ),
 .UNSPECIFIED., .F., .F.,
 ( 4, 4 ),
 ( 0.000000000000000000, 1.000000000000000000 ),
 .UNSPECIFIED. ) ;
#13882 = CARTESIAN_POINT ( 'NONE',  ( 3.187343406994000095, -1.703486777756999970, 3.293594259118999723 ) ) ;
#13883 = CARTESIAN_POINT ( 'NONE',  ( 10.91623602276999883, -5.459825388708999583, -8.642870457474998602 ) ) ;
#13884 = CARTESIAN_POINT ( 'NONE',  ( 15.89994436294300151, 8.847904542234999781, 8.580301953175000662 ) ) ;
#13885 = CARTESIAN_POINT ( 'NONE',  ( 9.618481599739016730, -2.362941927002724096, -6.884006425641727489 ) ) ;
#13886 = EDGE_CURVE ( 'NONE', #46546, #47653, #3727, .T. ) ;
#13887 = EDGE_CURVE ( 'NONE', #17344, #32816, #57985, .T. ) ;
#13888 = ORIENTED_EDGE ( 'NONE', *, *, #26214, .T. ) ;
#13889 = ADVANCED_FACE ( 'NONE', ( #68592, #3590 ), #9526, .F. ) ;
#13890 = CARTESIAN_POINT ( 'NONE',  ( 11.02226222744799955, -4.880489021643899861, 6.774721295617600170 ) ) ;
#13891 = CARTESIAN_POINT ( 'NONE',  ( 10.81315553411000074, 3.756074350075000012, 6.071610008629000355 ) ) ;
#13892 = CARTESIAN_POINT ( 'NONE',  ( 15.86005557146100209, 8.873324881979000267, 8.501367972259000538 ) ) ;
#13893 = CARTESIAN_POINT ( 'NONE',  ( 8.014941940377999785, -2.280579276705999803, 6.510290672242000198 ) ) ;
#13895 = CARTESIAN_POINT ( 'NONE',  ( 10.98333333333433082, 4.339018939181010559, 8.912414555068393085 ) ) ;
#13894 = CARTESIAN_POINT ( 'NONE',  ( 9.442843574488000158, 2.691255504502000129, 6.269523028052000235 ) ) ;
#13896 = CIRCLE ( 'NONE', #61896, 11.84999999999999964 ) ;
#13897 = CARTESIAN_POINT ( 'NONE',  ( 10.77256919669529900, 4.962345366016100101, -7.784327714719899483 ) ) ;
#13898 = CARTESIAN_POINT ( 'NONE',  ( 24.59232958921100121, -12.25045686045999993, 3.053350357284999816 ) ) ;
#13899 = CARTESIAN_POINT ( 'NONE',  ( 10.23758376188599861, 3.152987476450699766, -8.039825975318500184 ) ) ;
#13900 = CARTESIAN_POINT ( 'NONE',  ( 18.12277215905344363, -0.4475098806653837746, 12.59205372277267898 ) ) ;
#13901 = CARTESIAN_POINT ( 'NONE',  ( 25.49994615398131614, -10.64595569433734390, 3.788460569392772648 ) ) ;
#13902 = CARTESIAN_POINT ( 'NONE',  ( 0.8504945477338626825, -1.107043943361407212, -3.344068980614735231 ) ) ;
#13903 = CARTESIAN_POINT ( 'NONE',  ( 23.66479333458100243, 10.00924341248000005, 9.518029705864998746 ) ) ;
#13904 = ORIENTED_EDGE ( 'NONE', *, *, #22304, .T. ) ;
#13905 = CARTESIAN_POINT ( 'NONE',  ( 7.037120559622001004, -4.623636604834999275, 8.651469651195000665 ) ) ;
#13906 = CARTESIAN_POINT ( 'NONE',  ( 18.24298441323063003, 2.287290078788467351, 13.81189461436434307 ) ) ;
#13907 = CARTESIAN_POINT ( 'NONE',  ( 9.057169810767971896, 4.203513387681364399, 6.292830123317686208 ) ) ;
#13908 = CARTESIAN_POINT ( 'NONE',  ( 10.27195525820100031, -4.120672149427799802, -6.227697122196000024 ) ) ;
#13909 = ORIENTED_EDGE ( 'NONE', *, *, #27306, .F. ) ;
#13910 = AXIS2_PLACEMENT_3D ( 'NONE', #33715, #23215, #38601 ) ;
#13911 = CARTESIAN_POINT ( 'NONE',  ( 8.064114158772998309, 4.228291488957999888, 8.941375734143997889 ) ) ;
#13912 = AXIS2_PLACEMENT_3D ( 'NONE', #34607, #2428, #55920 ) ;
#13914 = CARTESIAN_POINT ( 'NONE',  ( 11.27234208742519783, 3.445253572379500362, 6.627995351445298944 ) ) ;
#13913 = CARTESIAN_POINT ( 'NONE',  ( 8.927455549952998837, -3.325238030324599858, -6.955569812538500152 ) ) ;
#13915 = FACE_OUTER_BOUND ( 'NONE', #65509, .T. ) ;
#13916 = VERTEX_POINT ( 'NONE', #63695 ) ;
#13917 = CARTESIAN_POINT ( 'NONE',  ( 23.59999176271200128, 13.22318677037999812, 4.267778497637999102 ) ) ;
#13918 = CARTESIAN_POINT ( 'NONE',  ( 18.13115538416117900, -2.961380457613815409, -13.68321312766444997 ) ) ;
#13919 = CARTESIAN_POINT ( 'NONE',  ( 11.16225954179439839, 4.877394611789299894, 6.770980925167799036 ) ) ;
#13920 = DIRECTION ( 'NONE',  ( 0.9999999999938153916, 3.516990153967770421E-06, 1.152484550329258267E-11 ) ) ;
#13921 = LINE ( 'NONE', #4094, #23186 ) ;
#13922 = ORIENTED_EDGE ( 'NONE', *, *, #33931, .T. ) ;
#13923 = CARTESIAN_POINT ( 'NONE',  ( 11.48381255716000027, -3.703723199601000271, 11.90766076753999947 ) ) ;
#13924 = CARTESIAN_POINT ( 'NONE',  ( 11.37167944038000122, -2.803484087760999888, -6.967877228197000505 ) ) ;
#13925 = CIRCLE ( 'NONE', #49651, 11.50000000000000000 ) ;
#13926 = CARTESIAN_POINT ( 'NONE',  ( 8.069163351475221901, -3.878260955912923080, 5.763835643759676941 ) ) ;
#13927 = CARTESIAN_POINT ( 'NONE',  ( 10.97124174884019965, -4.036194082918090231, -8.815770025351000072 ) ) ;
#13928 = CARTESIAN_POINT ( 'NONE',  ( 9.144809814041000351, -3.301541394817099739, 6.596733927440100231 ) ) ;
#13929 = ORIENTED_EDGE ( 'NONE', *, *, #25310, .F. ) ;
#13930 = CARTESIAN_POINT ( 'NONE',  ( 10.39968959185000053, -4.894615431365999747, -4.742639820717000632 ) ) ;
#13931 = CARTESIAN_POINT ( 'NONE',  ( 11.36272200990529946, -5.206705454565000224, 7.920925559347199219 ) ) ;
#13932 = ORIENTED_EDGE ( 'NONE', *, *, #6857, .T. ) ;
#13933 = ADVANCED_FACE ( 'NONE', ( #38158 ), #43426, .T. ) ;
#13934 = CARTESIAN_POINT ( 'NONE',  ( 11.09999999999999964, 4.000000000000000000, -9.049999999997968558 ) ) ;
#13935 = EDGE_LOOP ( 'NONE', ( #45723, #48071, #38961, #44433 ) ) ;
#13936 = CARTESIAN_POINT ( 'NONE',  ( 9.353137413980999071, -5.679455740088000582, -8.329752476417999318 ) ) ;
#13937 = B_SPLINE_CURVE_WITH_KNOTS ( 'NONE', 3,
 ( #2506, #23830, #39570, #60204, #18248, #1470, #32943, #6707, #59502, #33641, #60894, #65077 ),
 .UNSPECIFIED., .F., .F.,
 ( 4, 1, 1, 1, 1, 1, 1, 1, 1, 4 ),
 ( 0.000000000000000000, 0.1111111144503000026, 0.2222222250406999944, 0.3333333356311999895, 0.4444444462216000091, 0.5555555568119999732, 0.6666666674023999928, 0.7777777779927999013, 0.8888888885832000319, 1.000000000000000000 ),
 .UNSPECIFIED. ) ;
#13938 = CARTESIAN_POINT ( 'NONE',  ( 12.80000000000000071, 10.78295181803999903, -4.410266442048000002 ) ) ;
#13939 = DIRECTION ( 'NONE',  ( -1.000000000000000000, 0.000000000000000000, 0.000000000000000000 ) ) ;
#13940 = LINE ( 'NONE', #56583, #6459 ) ;
#13941 = CARTESIAN_POINT ( 'NONE',  ( 12.38992078601020630, 2.032669449810693862, -12.54828005421690307 ) ) ;
#13942 = CARTESIAN_POINT ( 'NONE',  ( 12.12994988689360021, -3.481863023525599843, 6.483720595741000459 ) ) ;
#13943 = CARTESIAN_POINT ( 'NONE',  ( 15.20000000000000107, 11.47055000429999971, -4.757693469806000053 ) ) ;
#13944 = ORIENTED_EDGE ( 'NONE', *, *, #18793, .T. ) ;
#13945 = DIRECTION ( 'NONE',  ( 1.000000000000000000, 0.000000000000000000, 0.000000000000000000 ) ) ;
#13946 = VECTOR ( 'NONE', #52779, 1000.000000000000000 ) ;
#13947 = CARTESIAN_POINT ( 'NONE',  ( 8.983793146794999629, -3.979464503892999439, 9.134080454305001595 ) ) ;
#13948 = CARTESIAN_POINT ( 'NONE',  ( 29.91622776601699840, 0.000000000000000000, 0.000000000000000000 ) ) ;
#13949 = ORIENTED_EDGE ( 'NONE', *, *, #7962, .F. ) ;
#13950 = B_SPLINE_SURFACE_WITH_KNOTS ( 'NONE', 3, 3, ( 
 ( #43897, #57291, #25489, #46817, #59967, #23947, #55420, #7513, #33755, #50514, #54725, #12773, #17318, #12075, #39338, #34100, #44938, #13469, #34790, #23595, #39686, #65892, #28868, #1584, #49825, #44255, #61005, #18022, #55767, #22901, #6825, #38643, #24288, #56101, #60316 ),
 ( #33408, #2957, #2615, #7174, #8210, #28158, #29559, #50176, #7869, #65551, #66243, #18364, #40037, #55071, #2279, #49472, #17674, #38997, #13125, #12425, #1938, #34453, #28512, #23257, #44601, #50861, #61350, #29205, #60658, #45279, #66586, #18704, #45623, #24972, #29900 ),
 ( #68292, #45957, #61688, #19382, #51539, #46305, #30910, #30564, #19038, #3974, #20072, #41738, #3635, #24636, #51206, #66928, #67606, #56797, #25313, #67266, #41400, #9224, #15168, #25658, #46991, #8895, #31258, #62032, #14148, #57462, #40367, #4664, #14828, #4323, #30232 ),
 ( #20412, #40706, #52569, #13806, #19730, #51878, #35135, #41054, #9570, #26003, #62375, #35477, #63041, #14491, #56448, #8553, #35810, #57126, #36150, #46650, #52225, #3300, #67956, #62707, #36491, #57813, #9922, #37519, #48709, #461, #59189, #16196, #48355, #26701, #21435 ) ),
 .UNSPECIFIED., .F., .F., .F.,
 ( 4, 4 ),
 ( 4, 1, 1, 1, 1, 1, 1, 1, 1, 1, 1, 1, 1, 1, 1, 1, 1, 1, 1, 1, 1, 1, 1, 1, 1, 1, 1, 1, 1, 1, 1, 1, 4 ),
 ( -0.1039370721279000015, 1.103937072127999963 ),
 ( -0.02000000000000000042, 0.01250000000000000069, 0.04499999999999999833, 0.07749999999999999944, 0.1100000000000000006, 0.1424999999999999878, 0.1749999999999999889, 0.2074999999999999900, 0.2399999999999999911, 0.2725000000000000200, 0.3049999999999999933, 0.3375000000000000222, 0.3699999999999999956, 0.4025000000000000244, 0.4349999999999999978, 0.4675000000000000266, 0.5000000000000000000, 0.5324999999999999734, 0.5649999999999999467, 0.5975000000000000311, 0.6300000000000000044, 0.6624999999999999778, 0.6949999999999999512, 0.7275000000000000355, 0.7600000000000000089, 0.7924999999999999822, 0.8249999999999999556, 0.8575000000000000400, 0.8900000000000000133, 0.9224999999999999867, 0.9549999999999999600, 0.9875000000000000444, 1.020000000000000018 ),
 .UNSPECIFIED. ) ;
#13951 = CARTESIAN_POINT ( 'NONE',  ( 12.08128888832030512, -2.529854562579159527, -12.34343511423995743 ) ) ;
#13952 = CARTESIAN_POINT ( 'NONE',  ( 11.45348876160960039, 3.114179898019400206, 6.578783887955899523 ) ) ;
#13953 = CARTESIAN_POINT ( 'NONE',  ( 10.39539435320999949, -5.667179153637999178, -7.250689665673000661 ) ) ;
#13954 = CARTESIAN_POINT ( 'NONE',  ( 15.40000000001299973, 8.815237407733999220, 7.616696375847999967 ) ) ;
#13955 = FACE_OUTER_BOUND ( 'NONE', #58143, .T. ) ;
#13956 = CARTESIAN_POINT ( 'NONE',  ( 24.31006797093800031, -8.914161086992001160, 8.860056389909999552 ) ) ;
#13957 = CARTESIAN_POINT ( 'NONE',  ( 12.54499921992993094, -1.931577877770960239, -13.77766407476416077 ) ) ;
#13958 = CARTESIAN_POINT ( 'NONE',  ( 11.83518044953559922, -3.231951024059400268, -7.900497508315099893 ) ) ;
#13959 = CARTESIAN_POINT ( 'NONE',  ( 10.41964694612699915, -5.186980343482999523, -7.973702485506099613 ) ) ;
#13960 = CARTESIAN_POINT ( 'NONE',  ( 8.550568453843245820, -5.068330482988463004, 6.313212389168451288 ) ) ;
#13961 = ORIENTED_EDGE ( 'NONE', *, *, #44983, .T. ) ;
#13962 = ORIENTED_EDGE ( 'NONE', *, *, #54552, .T. ) ;
#13963 = CARTESIAN_POINT ( 'NONE',  ( 10.31498017945866685, 2.650031506806222570, -7.499998780888569527 ) ) ;
#13964 = CARTESIAN_POINT ( 'NONE',  ( 18.08141525684210649, 2.837131573407952523, 13.59610056795573740 ) ) ;
#13965 = CARTESIAN_POINT ( 'NONE',  ( 10.98277660187000215, 2.518725482848000130, -8.314790074023999722 ) ) ;
#13966 = CARTESIAN_POINT ( 'NONE',  ( 4.599999999999999645, 0.000000000000000000, 0.000000000000000000 ) ) ;
#13967 = AXIS2_PLACEMENT_3D ( 'NONE', #2290, #2630, #56113 ) ;
#13968 = CARTESIAN_POINT ( 'NONE',  ( 17.75808086271924324, 3.091459143609192495, 12.29388367502514257 ) ) ;
#13969 = FACE_OUTER_BOUND ( 'NONE', #16692, .T. ) ;
#13970 = ADVANCED_FACE ( 'NONE', ( #27690 ), #15810, .T. ) ;
#13972 = EDGE_CURVE ( 'NONE', #24517, #29064, #9556, .T. ) ;
#13971 = CARTESIAN_POINT ( 'NONE',  ( 9.166073843917999397, 4.023333628930999772, 9.122276991855001071 ) ) ;
#13973 = CARTESIAN_POINT ( 'NONE',  ( 10.21921441925097973, -4.353287638977898055, -8.814644987550590116 ) ) ;
#13974 = EDGE_CURVE ( 'NONE', #65063, #50859, #65533, .T. ) ;
#13975 = EDGE_CURVE ( 'NONE', #58018, #32077, #58864, .T. ) ;
#13976 = ORIENTED_EDGE ( 'NONE', *, *, #31365, .T. ) ;
#13977 = CARTESIAN_POINT ( 'NONE',  ( 12.42174667009962086, -2.006228232438482362, 12.55302761990816052 ) ) ;
#13978 = CARTESIAN_POINT ( 'NONE',  ( 9.553696787962998371, -3.827518619249500098, -6.510508982544899403 ) ) ;
#13979 = CARTESIAN_POINT ( 'NONE',  ( 9.442087588264000075, 4.742492734433000123, 8.809983635807000724 ) ) ;
#13980 = CARTESIAN_POINT ( 'NONE',  ( 11.47635090131019986, -3.000792947412299849, 6.881982988766500497 ) ) ;
#13981 = CARTESIAN_POINT ( 'NONE',  ( 8.839404719593998649, 5.140767546012999567, -6.196177269779999719 ) ) ;
#13982 = CARTESIAN_POINT ( 'NONE',  ( 11.23195122972050086, 4.507250159094099651, -6.326963915009999440 ) ) ;
#13983 = CARTESIAN_POINT ( 'NONE',  ( 12.19004707749462924, -0.1118057330073182615, 12.69934308675516377 ) ) ;
#13984 = CARTESIAN_POINT ( 'NONE',  ( 8.829017219593000121, 5.290207928847999064, 8.768105151414001597 ) ) ;
#13985 = CARTESIAN_POINT ( 'NONE',  ( 10.18756025349000005, 5.387489739490000318, 8.640945789268998922 ) ) ;
#13986 = CARTESIAN_POINT ( 'NONE',  ( 12.20003344249112409, 2.341920628070001342, 12.48700265052702107 ) ) ;
#13987 = ORIENTED_EDGE ( 'NONE', *, *, #8133, .F. ) ;
#13988 = CARTESIAN_POINT ( 'NONE',  ( 10.16426084122999995, 4.808846957865000604, -8.639578604182998944 ) ) ;
#13989 = CARTESIAN_POINT ( 'NONE',  ( 7.307500000000000107, 0.2500000000000000000, 3.149999999999999911 ) ) ;
#13990 = EDGE_CURVE ( 'NONE', #64554, #59745, #39669, .T. ) ;
#13991 = CARTESIAN_POINT ( 'NONE',  ( 5.305026506349999948, 1.500000000000000000, 0.000000000000000000 ) ) ;
#13993 = DIRECTION ( 'NONE',  ( -1.000000000000000000, 0.000000000000000000, 0.000000000000000000 ) ) ;
#13992 = CARTESIAN_POINT ( 'NONE',  ( 9.202754440379999679, -2.542850487891999745, 7.419808283050000064 ) ) ;
#13994 = CARTESIAN_POINT ( 'NONE',  ( 12.09999999999999964, -3.927017550833199699, 8.552611010855411422 ) ) ;
#13995 = CARTESIAN_POINT ( 'NONE',  ( 10.55103166480599874, -5.000984463463999496, -7.570575893572789816 ) ) ;
#13996 = VERTEX_POINT ( 'NONE', #31902 ) ;
#13997 = CARTESIAN_POINT ( 'NONE',  ( 1.248245171504000162, -3.558193753575999985, 1.211459191638999844 ) ) ;
#13998 = CARTESIAN_POINT ( 'NONE',  ( 17.59562594683476178, -0.6249999999999998890, -12.67928921589118829 ) ) ;
#14000 = CARTESIAN_POINT ( 'NONE',  ( 10.60226354018307937, 5.092232985442822546, 6.870476274536374106 ) ) ;
#13999 = CARTESIAN_POINT ( 'NONE',  ( 9.645836745965350900, 5.376058781240163675, 6.376281615445395623 ) ) ;
#14001 = FACE_OUTER_BOUND ( 'NONE', #26776, .T. ) ;
#14002 = CARTESIAN_POINT ( 'NONE',  ( 10.29378723213999969, 3.483632952461999999, 6.176337842045999338 ) ) ;
#14003 = CARTESIAN_POINT ( 'NONE',  ( 16.09997386696500143, 8.350085070477001992, 8.123950967096998710 ) ) ;
#14004 = CARTESIAN_POINT ( 'NONE',  ( 8.060840674114750470, -9.103590313266890277, 5.835422151730303320 ) ) ;
#14005 = CARTESIAN_POINT ( 'NONE',  ( 5.700000000000000178, 0.000000000000000000, 0.000000000000000000 ) ) ;
#14006 = CARTESIAN_POINT ( 'NONE',  ( 9.170316940378999249, -5.558929022707999046, 6.272984818914999927 ) ) ;
#14007 = ORIENTED_EDGE ( 'NONE', *, *, #68985, .F. ) ;
#14008 = CARTESIAN_POINT ( 'NONE',  ( 7.352704719590999360, 4.773081973066999772, 8.927402469597002010 ) ) ;
#14009 = CARTESIAN_POINT ( 'NONE',  ( 11.04467482866999894, 5.245201221631999644, 5.185341696387000709 ) ) ;
#14010 = CARTESIAN_POINT ( 'NONE',  ( 7.450458831010640992, -2.261073438131606217, 7.470018516072758352 ) ) ;
#14011 = PLANE ( 'NONE',  #41492 ) ;
#14012 = CARTESIAN_POINT ( 'NONE',  ( 2.077021397264999791, -0.2901351235585999944, -3.413359411422000278 ) ) ;
#14013 = ORIENTED_EDGE ( 'NONE', *, *, #56232, .F. ) ;
#14014 = FACE_OUTER_BOUND ( 'NONE', #5319, .T. ) ;
#14015 = CARTESIAN_POINT ( 'NONE',  ( 10.98133997688000107, -3.815400206859000054, 8.346298710230199092 ) ) ;
#14016 = CARTESIAN_POINT ( 'NONE',  ( 10.27427156480999848, -4.600000212792999754, 4.944156960788000710 ) ) ;
#14017 = CARTESIAN_POINT ( 'NONE',  ( 10.20319667131999886, 3.421760346951000287, 6.017732782098999422 ) ) ;
#14018 = VECTOR ( 'NONE', #67119, 1000.000000000000000 ) ;
#14019 = EDGE_CURVE ( 'NONE', #60421, #62492, #59143, .T. ) ;
#14020 = CARTESIAN_POINT ( 'NONE',  ( 10.96949144726329806, 3.419793223320000131, 8.318725197575499664 ) ) ;
#14021 = CARTESIAN_POINT ( 'NONE',  ( 8.682949004128220238, -5.079917234190865827, 6.251799941949381711 ) ) ;
#14022 = CARTESIAN_POINT ( 'NONE',  ( 12.09999999999999964, -4.000000000000000000, 7.500000000000000000 ) ) ;
#14023 = EDGE_CURVE ( 'NONE', #46365, #46842, #46602, .T. ) ;
#14024 = CARTESIAN_POINT ( 'NONE',  ( 7.990055090139000171, 4.541015240501000250, -6.262949957254000388 ) ) ;
#14025 = CARTESIAN_POINT ( 'NONE',  ( 9.470944094206000585, 5.100000000000000533, 6.571291218949999902 ) ) ;
#14026 = CARTESIAN_POINT ( 'NONE',  ( 23.66004879239100234, -3.393652723963000106, -13.50507488346000073 ) ) ;
#14027 = CARTESIAN_POINT ( 'NONE',  ( 7.528897780153962493, 3.013532217265934676, 6.036466769713773495 ) ) ;
#14028 = ORIENTED_EDGE ( 'NONE', *, *, #33873, .F. ) ;
#14029 = CARTESIAN_POINT ( 'NONE',  ( 18.17163261364645876, -2.902690589304653290, 13.69579465584391542 ) ) ;
#14030 = CARTESIAN_POINT ( 'NONE',  ( 19.94999927679900154, 0.000000000000000000, 5.040412531797999279E-14 ) ) ;
#14031 = ORIENTED_EDGE ( 'NONE', *, *, #57016, .T. ) ;
#14032 = DIRECTION ( 'NONE',  ( 0.000000000000000000, 0.000000000000000000, -1.000000000000000000 ) ) ;
#14033 = CARTESIAN_POINT ( 'NONE',  ( 11.06967835872019812, 3.245266201729799960, 7.975673736933100777 ) ) ;
#14034 = DIRECTION ( 'NONE',  ( 0.8480635683784220058, 0.000000000000000000, 0.5298945026977139872 ) ) ;
#14035 = CARTESIAN_POINT ( 'NONE',  ( 11.53979707368350027, 3.569730287184500472, 8.251775607861899786 ) ) ;
#14036 = CARTESIAN_POINT ( 'NONE',  ( 10.53138775541999905, 5.607751175212000838, 7.280102404048999887 ) ) ;
#14037 = CARTESIAN_POINT ( 'NONE',  ( 10.52662718686000076, 4.933722097448000277, -6.506013113666999637 ) ) ;
#14038 = CARTESIAN_POINT ( 'NONE',  ( 9.226900131858625898, -4.185762427694958987, -8.354999759870066711 ) ) ;
#14039 = CARTESIAN_POINT ( 'NONE',  ( 10.57223537388000167, -4.020426196685999543, 8.920680607665000039 ) ) ;
#14040 = CARTESIAN_POINT ( 'NONE',  ( 18.22023691865392081, 0.2863297863804545318, -12.59675086341328232 ) ) ;
#14041 = LINE ( 'NONE', #35368, #67615 ) ;
#14042 = CARTESIAN_POINT ( 'NONE',  ( 11.78179573085659904, -3.026866171144600326, -7.668383662421899061 ) ) ;
#14043 = CARTESIAN_POINT ( 'NONE',  ( 8.179999999999999716, 4.924138593003999809, -8.484107647018999998 ) ) ;
#14044 = ORIENTED_EDGE ( 'NONE', *, *, #26756, .F. ) ;
#14045 = AXIS2_PLACEMENT_3D ( 'NONE', #19625, #30132, #18939 ) ;
#14046 = DIRECTION ( 'NONE',  ( -1.000000000000000000, 0.000000000000000000, 0.000000000000000000 ) ) ;
#14047 = CARTESIAN_POINT ( 'NONE',  ( 24.87151402923947430, 8.583161980870569252, 8.460101252743749356 ) ) ;
#14048 = CONICAL_SURFACE ( 'NONE', #53110, 12.37499919541000004, 0.7853980884875938484 ) ;
#14049 = CARTESIAN_POINT ( 'NONE',  ( 9.099999999999999645, -11.84999999999999964, 0.000000000000000000 ) ) ;
#14050 = CARTESIAN_POINT ( 'NONE',  ( 9.557721904870000174, 5.115452802765999785, -8.126218358304999612 ) ) ;
#14051 = CARTESIAN_POINT ( 'NONE',  ( 12.10457356466339895, 2.707610175640967842, 13.73569711802853099 ) ) ;
#14052 = CARTESIAN_POINT ( 'NONE',  ( 11.49999672495000169, 3.632761979779000061, -11.06912554803999882 ) ) ;
#14053 = VERTEX_POINT ( 'NONE', #53561 ) ;
#14054 = CARTESIAN_POINT ( 'NONE',  ( 12.49451986919435953, 0.5425047575455477222, -12.68440192077494011 ) ) ;
#14055 = EDGE_CURVE ( 'NONE', #64129, #20386, #47975, .T. ) ;
#14056 = CARTESIAN_POINT ( 'NONE',  ( 25.00275116957158161, 8.478815136465241764, 8.837059051057721604 ) ) ;
#14057 = ADVANCED_FACE ( 'NONE', ( #65062 ), #32252, .F. ) ;
#14058 = ORIENTED_EDGE ( 'NONE', *, *, #55663, .F. ) ;
#14059 = FACE_BOUND ( 'NONE', #15695, .T. ) ;
#14060 = CARTESIAN_POINT ( 'NONE',  ( 10.93769853197999886, 5.063116524846000388, -4.920828787216999345 ) ) ;
#14061 = CARTESIAN_POINT ( 'NONE',  ( 8.331682176603999679, 5.101289360622999425, 6.607176324693000424 ) ) ;
#14062 = PLANE ( 'NONE',  #17141 ) ;
#14063 = VECTOR ( 'NONE', #24127, 1000.000000000000000 ) ;
#14064 = AXIS2_PLACEMENT_3D ( 'NONE', #64660, #1733, #60811 ) ;
#14065 = CARTESIAN_POINT ( 'NONE',  ( 15.90018573812399971, -8.493548356068000516, -8.263529029821000904 ) ) ;
#14066 = CARTESIAN_POINT ( 'NONE',  ( 0.1371912743484000052, 0.7117304887930000490, 3.632629627798000360 ) ) ;
#14067 = B_SPLINE_CURVE_WITH_KNOTS ( 'NONE', 3,
 ( #25065, #67700, #13901, #67023 ),
 .UNSPECIFIED., .F., .F.,
 ( 4, 4 ),
 ( 0.000000000000000000, 1.000000000000000000 ),
 .UNSPECIFIED. ) ;
#14068 = CARTESIAN_POINT ( 'NONE',  ( 8.164556123749363792, 2.650750344902805811, 7.676799495578948473 ) ) ;
#14069 = CARTESIAN_POINT ( 'NONE',  ( 12.56995090575619578, 3.160862399908558551, 12.19708787818174400 ) ) ;
#14070 = CARTESIAN_POINT ( 'NONE',  ( 9.311892889969000109, -5.494586520014999920, -6.370782351137999733 ) ) ;
#14071 = CARTESIAN_POINT ( 'NONE',  ( 11.39210538575740017, 4.842454415653899780, -7.298582155985900322 ) ) ;
#14072 = CARTESIAN_POINT ( 'NONE',  ( 18.23777342769928467, 3.105166803968430145, 11.92942855515249967 ) ) ;
#14073 = CARTESIAN_POINT ( 'NONE',  ( 10.75915165876999957, 5.387277012365999873, -6.278112168454999420 ) ) ;
#14074 = EDGE_CURVE ( 'NONE', #18862, #50564, #18651, .T. ) ;
#14075 = CARTESIAN_POINT ( 'NONE',  ( 10.11390035061499937, 4.304339077956200299, -8.600505223349999895 ) ) ;
#14077 = PLANE ( 'NONE',  #48469 ) ;
#14076 = DIRECTION ( 'NONE',  ( 0.000000000000000000, 0.000000000000000000, -1.000000000000000000 ) ) ;
#14078 = CARTESIAN_POINT ( 'NONE',  ( 23.60815875000115582, -13.39692513168543364, 3.962568340425848490 ) ) ;
#14079 = ORIENTED_EDGE ( 'NONE', *, *, #55875, .F. ) ;
#14080 = DIRECTION ( 'NONE',  ( 0.000000000000000000, 0.000000000000000000, -1.000000000000000000 ) ) ;
#14081 = CARTESIAN_POINT ( 'NONE',  ( 9.228135700785001561, -2.875364528161000077, 8.669943154892999715 ) ) ;
#14082 = CARTESIAN_POINT ( 'NONE',  ( 10.18692546752099837, 2.997990738918999920, 7.569424354486659290 ) ) ;
#14083 = CARTESIAN_POINT ( 'NONE',  ( 8.772923981633081070, 4.310454296184184741, -8.314671747086004316 ) ) ;
#14084 = CARTESIAN_POINT ( 'NONE',  ( 23.89320776801300283, 10.75689324691000337, -4.023240149132002230 ) ) ;
#14085 = CYLINDRICAL_SURFACE ( 'NONE', #65392, 1.350000000000000089 ) ;
#14086 = CARTESIAN_POINT ( 'NONE',  ( 7.044509995414057535, -0.8324003622799491797, -1.084551266798225333 ) ) ;
#14087 = ORIENTED_EDGE ( 'NONE', *, *, #56664, .F. ) ;
#14088 = CARTESIAN_POINT ( 'NONE',  ( 10.10344474310099905, -2.862064370975999861, -8.052229793103100164 ) ) ;
#14089 = CYLINDRICAL_SURFACE ( 'NONE', #56655, 0.5000000000000004441 ) ;
#14090 = CARTESIAN_POINT ( 'NONE',  ( 11.27368717260499942, -4.539928529895099985, 6.618743573831199711 ) ) ;
#14091 = B_SPLINE_CURVE_WITH_KNOTS ( 'NONE', 3,
 ( #37541, #64791, #32317, #63764, #27066, #47704, #69014, #42454, #15875, #37206, #58524, #10630, #17615, #38939, #34394, #32999, #66527, #65838, #1877, #44192, #44879, #12014, #55360 ),
 .UNSPECIFIED., .F., .F.,
 ( 4, 2, 2, 2, 2, 2, 2, 2, 1, 2, 2, 4 ),
 ( 0.000000000000000000, 0.06249999999999983347, 0.1249999999999996669, 0.2499999999999977796, 0.3749999999999958922, 0.4374999999999949485, 0.4999999999999940048, 0.6249999999999936717, 0.6874999999999940048, 0.7187499999999945599, 0.7499999999999951150, 1.000000000000000000 ),
 .UNSPECIFIED. ) ;
#14092 = CARTESIAN_POINT ( 'NONE',  ( 17.63759097916651442, 3.119868145639166812, -12.28530842955782099 ) ) ;
#14093 = CARTESIAN_POINT ( 'NONE',  ( 2.615556799209333594, 0.4581489286485002088, 3.500000000000001776 ) ) ;
#14094 = AXIS2_PLACEMENT_3D ( 'NONE', #15472, #763, #48310 ) ;
#14095 = CARTESIAN_POINT ( 'NONE',  ( 24.62774583285499830, -3.462210234181999802, 12.08748376425999993 ) ) ;
#14096 = CARTESIAN_POINT ( 'NONE',  ( 12.24478949867863165, 2.777190625918491307, -13.61075457645665665 ) ) ;
#14097 = CARTESIAN_POINT ( 'NONE',  ( 9.866664898013999263, -4.626219091573998909, -9.027249334595000008 ) ) ;
#14098 = CARTESIAN_POINT ( 'NONE',  ( 8.099999999999999645, 12.35000000006999876, 0.000000000000000000 ) ) ;
#14099 = EDGE_CURVE ( 'NONE', #8229, #24046, #68892, .T. ) ;
#14100 = ORIENTED_EDGE ( 'NONE', *, *, #46481, .T. ) ;
#14101 = DIRECTION ( 'NONE',  ( 0.000000000000000000, 1.000000000000000000, 0.000000000000000000 ) ) ;
#14102 = CARTESIAN_POINT ( 'NONE',  ( 12.54953656384602390, 0.6834693007276639865, -13.98330741474946315 ) ) ;
#14103 = CARTESIAN_POINT ( 'NONE',  ( 23.60345044734545183, 13.39469792596697673, 3.980595414305586388 ) ) ;
#14104 = LINE ( 'NONE', #24927, #62210 ) ;
#14105 = CARTESIAN_POINT ( 'NONE',  ( 3.009306799211332262, 3.058252359239904905, -1.762666431298142600 ) ) ;
#14106 = CARTESIAN_POINT ( 'NONE',  ( 17.66658663920539851, -11.23412379136108719, 3.084957477882974253 ) ) ;
#14107 = CARTESIAN_POINT ( 'NONE',  ( 6.699036861725389258, 0.3526192069364459392, -1.483084712358169854 ) ) ;
#14108 = ORIENTED_EDGE ( 'NONE', *, *, #50455, .T. ) ;
#14109 = VECTOR ( 'NONE', #8753, 1000.000000000000000 ) ;
#14110 = CARTESIAN_POINT ( 'NONE',  ( 4.000000000000000888, 2.040156275101110417, 0.6926574996740214596 ) ) ;
#14111 = CARTESIAN_POINT ( 'NONE',  ( 18.27457017588618271, 2.425781798817260082, -13.78826143416240768 ) ) ;
#14112 = ORIENTED_EDGE ( 'NONE', *, *, #956, .F. ) ;
#14113 = DIRECTION ( 'NONE',  ( 0.000000000000000000, -0.9565994702956990281, -0.2914059941558995726 ) ) ;
#14114 = CARTESIAN_POINT ( 'NONE',  ( 2.550973465877000024, 3.500000000000000000, 0.000000000000000000 ) ) ;
#14115 = CARTESIAN_POINT ( 'NONE',  ( 8.415504719592000527, 2.469361196073999842, -7.826019481986000059 ) ) ;
#14116 = CARTESIAN_POINT ( 'NONE',  ( 18.30003129334700063, 2.732683817159999862, -11.53064095410000078 ) ) ;
#14117 = CARTESIAN_POINT ( 'NONE',  ( 10.69057802013490033, -5.033226574983999946, -7.475947032624040034 ) ) ;
#14118 = CARTESIAN_POINT ( 'NONE',  ( 11.59999999999999964, -2.912667852269566815, -6.982348652072319695 ) ) ;
#14119 = CARTESIAN_POINT ( 'NONE',  ( 5.055026506350000837, -1.500000000000000000, 0.000000000000000000 ) ) ;
#14120 = ORIENTED_EDGE ( 'NONE', *, *, #56579, .T. ) ;
#14121 = DIRECTION ( 'NONE',  ( 1.000000000000000000, 0.000000000000000000, 0.000000000000000000 ) ) ;
#14122 = CARTESIAN_POINT ( 'NONE',  ( 10.84393020684900044, -5.250000000000000000, 7.500000000000000000 ) ) ;
#14123 = CARTESIAN_POINT ( 'NONE',  ( 8.839404719593998649, 5.140767546012999567, -6.196177269779999719 ) ) ;
#14124 = ORIENTED_EDGE ( 'NONE', *, *, #54128, .T. ) ;
#14125 = CARTESIAN_POINT ( 'NONE',  ( 11.06133897141000055, 2.503910831767000023, -6.712778933675999760 ) ) ;
#14126 = FILL_AREA_STYLE_COLOUR ( '', #26515 ) ;
#14127 = VERTEX_POINT ( 'NONE', #22081 ) ;
#14128 = CARTESIAN_POINT ( 'NONE',  ( 9.480671671056999372, 2.873958896683999953, 7.310881302803900361 ) ) ;
#14129 = CARTESIAN_POINT ( 'NONE',  ( 17.88942345255914645, -3.118753088769716797, -12.20792418036210591 ) ) ;
#14130 = CARTESIAN_POINT ( 'NONE',  ( 8.733215486276282746, -3.972057587790281730, -8.383215533252753815 ) ) ;
#14131 = CARTESIAN_POINT ( 'NONE',  ( 19.99999987597299977, -12.42499880353999941, 0.000000000000000000 ) ) ;
#14132 = ADVANCED_FACE ( 'NONE', ( #64720 ), #30929, .F. ) ;
#14133 = CARTESIAN_POINT ( 'NONE',  ( 23.60000000000000142, 11.85420044612000012, 3.901016762742000488 ) ) ;
#14134 = EDGE_CURVE ( 'NONE', #19777, #26667, #12922, .T. ) ;
#14135 = VERTEX_POINT ( 'NONE', #54944 ) ;
#14136 = CARTESIAN_POINT ( 'NONE',  ( 24.57788509278314493, -3.600249671654212058, 12.25995025212536227 ) ) ;
#14137 = CARTESIAN_POINT ( 'NONE',  ( 10.34939834122999969, 2.653159779809000085, -7.312415497503999440 ) ) ;
#14138 = CARTESIAN_POINT ( 'NONE',  ( 7.997739111735391759, -4.828320830117715623, 8.578514095141958506 ) ) ;
#14139 = CARTESIAN_POINT ( 'NONE',  ( 12.54773036592020574, 3.200672309338199462, -13.62922281487128728 ) ) ;
#14140 = CIRCLE ( 'NONE', #55460, 2.999989272562999965 ) ;
#14141 = CARTESIAN_POINT ( 'NONE',  ( 9.380417874594000338, -5.177249570814000279, -8.000467616829000761 ) ) ;
#14142 = CARTESIAN_POINT ( 'NONE',  ( 18.27393099755800421, 0.09542514088231059122, 13.99967976774382272 ) ) ;
#14143 = STYLED_ITEM ( 'NONE', ( #19361 ), #23576 ) ;
#14144 = CARTESIAN_POINT ( 'NONE',  ( 17.82346232393702223, 11.54140747413759449, -4.865347213226944412 ) ) ;
#14145 = CARTESIAN_POINT ( 'NONE',  ( 10.80160188108999897, -2.805072368922999715, -8.157282064671999677 ) ) ;
#14146 = ORIENTED_EDGE ( 'NONE', *, *, #7818, .T. ) ;
#14147 = VERTEX_POINT ( 'NONE', #17541 ) ;
#14148 = CARTESIAN_POINT ( 'NONE',  ( 8.780820280412001466, 2.567871051582000241, -6.869011921437000012 ) ) ;
#14149 = AXIS2_PLACEMENT_3D ( 'NONE', #4693, #27412, #42118 ) ;
#14150 = CARTESIAN_POINT ( 'NONE',  ( 9.229641524935605190, 5.653351949750144989, 8.124846574879386552 ) ) ;
#14151 = CARTESIAN_POINT ( 'NONE',  ( 12.19221373221769156, -2.622703612849026644, 13.64666901003217703 ) ) ;
#14152 = CARTESIAN_POINT ( 'NONE',  ( 23.85842818131158793, 3.325647356525735621, 13.01563238088372643 ) ) ;
#14153 = CARTESIAN_POINT ( 'NONE',  ( 23.61708153891300199, 10.26225109528000168, -9.295033282810001296 ) ) ;
#14154 = EDGE_CURVE ( 'NONE', #57647, #58563, #30501, .T. ) ;
#14155 = CARTESIAN_POINT ( 'NONE',  ( 11.49977531252999974, 12.43119799159999950, 1.530013559959999991 ) ) ;
#14157 = LINE ( 'NONE', #26013, #41779 ) ;
#14156 = CARTESIAN_POINT ( 'NONE',  ( 9.751759580228998914, -5.110528875107000601, 7.765443149353999708 ) ) ;
#14158 = CARTESIAN_POINT ( 'NONE',  ( 8.755016320410998532, -4.513710855956997392, -6.314259950256001730 ) ) ;
#14159 = ORIENTED_EDGE ( 'NONE', *, *, #9293, .F. ) ;
#14160 = AXIS2_PLACEMENT_3D ( 'NONE', #63510, #52340, #15285 ) ;
#14161 = EDGE_CURVE ( 'NONE', #62789, #33960, #7512, .T. ) ;
#14162 = CARTESIAN_POINT ( 'NONE',  ( 6.999999691988000095, -13.87069231928999891, -4.225386915259999654 ) ) ;
#14163 = CARTESIAN_POINT ( 'NONE',  ( 11.07605693148000015, -2.665626082328999669, -4.951852240693000340 ) ) ;
#14164 = CARTESIAN_POINT ( 'NONE',  ( 9.485142521132999605, -3.025808284870999731, -9.100010361367001366 ) ) ;
#14165 = CARTESIAN_POINT ( 'NONE',  ( 12.80505043854143388, 3.207098164520926886, 13.58558594083658910 ) ) ;
#14166 = CARTESIAN_POINT ( 'NONE',  ( 11.79999999471800010, 11.69117318561000118, 1.923227876431999883 ) ) ;
#14167 = LINE ( 'NONE', #45974, #20736 ) ;
#14168 = CARTESIAN_POINT ( 'NONE',  ( 8.397785841227999981, 5.616457598545999907, -8.245813000738998255 ) ) ;
#14169 = DIRECTION ( 'NONE',  ( -1.000000000000000000, 0.000000000000000000, 1.665334536957000056E-14 ) ) ;
#14170 = CARTESIAN_POINT ( 'NONE',  ( 11.13459739833729856, 3.176841881612200158, 7.174999999999999822 ) ) ;
#14171 = CARTESIAN_POINT ( 'NONE',  ( 0.1691085717929338428, 1.946941735042009070, -2.534826368309772260 ) ) ;
#14172 = CARTESIAN_POINT ( 'NONE',  ( 3.258066606493000172, 2.789036351275000047, 1.988993390707999964 ) ) ;
#14173 = ORIENTED_EDGE ( 'NONE', *, *, #67260, .T. ) ;
#14174 = CARTESIAN_POINT ( 'NONE',  ( 12.68606859785048258, 0.7096370184368562262, -12.58000072970462924 ) ) ;
#14175 = CARTESIAN_POINT ( 'NONE',  ( 12.21429833793744812, -2.704300905630751206, -12.40162098802949942 ) ) ;
#14176 = CARTESIAN_POINT ( 'NONE',  ( 27.64127793187000037, 2.399999999999999911, 6.571291218949999902 ) ) ;
#14177 = CARTESIAN_POINT ( 'NONE',  ( 17.55505043854144276, 0.7302158263239086899, 13.98094363220831049 ) ) ;
#14178 = FILL_AREA_STYLE_COLOUR ( '', #64036 ) ;
#14179 = ORIENTED_EDGE ( 'NONE', *, *, #20126, .T. ) ;
#14180 = CARTESIAN_POINT ( 'NONE',  ( 6.177062685093000383, 1.262548346495000029, 0.3929982786279000440 ) ) ;
#14181 = PRODUCT_CONTEXT ( 'NONE', #47174, 'mechanical' ) ;
#14182 = CARTESIAN_POINT ( 'NONE',  ( 0.7509734658760000015, -3.500000000000000000, 0.000000000000000000 ) ) ;
#14183 = LINE ( 'NONE', #30950, #33217 ) ;
#14184 = CARTESIAN_POINT ( 'NONE',  ( 10.39503166480599994, 2.725152142215999884, 7.410114961806599787 ) ) ;
#14185 = CARTESIAN_POINT ( 'NONE',  ( 11.14256920625030034, 4.042230905578960254, -6.325872106312999676 ) ) ;
#14186 = ORIENTED_EDGE ( 'NONE', *, *, #66296, .T. ) ;
#14187 = AXIS2_PLACEMENT_3D ( 'NONE', #17934, #60577, #34018 ) ;
#14188 = CARTESIAN_POINT ( 'NONE',  ( 10.68361719090999884, -2.603550124652000086, 7.762065570229999878 ) ) ;
#14189 = ORIENTED_EDGE ( 'NONE', *, *, #17611, .T. ) ;
#14190 = CARTESIAN_POINT ( 'NONE',  ( 9.269471092183000138, 5.100000000000000533, -6.152188490330000370 ) ) ;
#14191 = CARTESIAN_POINT ( 'NONE',  ( 7.828418146791999099, -5.524126964933000927, 6.910359834012999691 ) ) ;
#14192 =( GEOMETRIC_REPRESENTATION_CONTEXT ( 3 ) GLOBAL_UNCERTAINTY_ASSIGNED_CONTEXT ( ( #44874 ) ) GLOBAL_UNIT_ASSIGNED_CONTEXT ( ( #66138, #8455, #12662 ) ) REPRESENTATION_CONTEXT ( 'NONE', 'WORKASPACE' ) );
#14193 = CARTESIAN_POINT ( 'NONE',  ( 18.05935379312179734, -0.5247499651446981828, -13.99016470477802443 ) ) ;
#14194 = EDGE_CURVE ( 'NONE', #57302, #63258, #13788, .T. ) ;
#14195 = EDGE_CURVE ( 'NONE', #7001, #65623, #62923, .T. ) ;
#14196 = ORIENTED_EDGE ( 'NONE', *, *, #53122, .T. ) ;
#14197 = CARTESIAN_POINT ( 'NONE',  ( 8.558761214560396624, 2.378033399648631363, -8.172933946829649798 ) ) ;
#14198 = DIRECTION ( 'NONE',  ( 0.000000000000000000, 0.9553735099700839672, -0.2954005017724949389 ) ) ;
#14199 = CARTESIAN_POINT ( 'NONE',  ( 6.894364158771001172, 2.898440551356999961, -6.639986657414999272 ) ) ;
#14200 = CIRCLE ( 'NONE', #9685, 1.449999999999999956 ) ;
#14201 = CARTESIAN_POINT ( 'NONE',  ( 10.90454231406000041, -5.099691312770999296, -5.130383474399000221 ) ) ;
#14202 = CARTESIAN_POINT ( 'NONE',  ( 3.452384183491000069, 1.140396268832999827, -3.309002319436000317 ) ) ;
#14203 = EDGE_LOOP ( 'NONE', ( #63737, #38614, #47062, #33196 ) ) ;
#14204 = CARTESIAN_POINT ( 'NONE',  ( 9.347248564704999652, -4.028326926800000152, 9.469437404464001062 ) ) ;
#14205 = CARTESIAN_POINT ( 'NONE',  ( 12.20052776709553299, -2.340020608624143517, -13.70605490525081827 ) ) ;
#14206 = CARTESIAN_POINT ( 'NONE',  ( 8.599999999999999645, 4.000000000000000000, -7.500000000000000000 ) ) ;
#14207 = CARTESIAN_POINT ( 'NONE',  ( 10.01597818573999987, -4.792673671522000411, -6.390249203106999509 ) ) ;
#14208 = CARTESIAN_POINT ( 'NONE',  ( 8.256966361271000920, 2.896784447077999758, 6.628744947585000880 ) ) ;
#14209 = ORIENTED_EDGE ( 'NONE', *, *, #26188, .F. ) ;
#14210 = CARTESIAN_POINT ( 'NONE',  ( 17.81163219999022829, 0.5699871459077878733, -13.88426688812565324 ) ) ;
#14211 = DIRECTION ( 'NONE',  ( 0.000000000000000000, 0.000000000000000000, -1.000000000000000000 ) ) ;
#14212 = CARTESIAN_POINT ( 'NONE',  ( 23.67317840412032837, -3.197506257295965604, -13.39107809300776708 ) ) ;
#14213 = DIRECTION ( 'NONE',  ( 0.000000000000000000, 1.000000000000000000, 0.000000000000000000 ) ) ;
#14214 = AXIS2_PLACEMENT_3D ( 'NONE', #49529, #1297, #11775 ) ;
#14215 = CARTESIAN_POINT ( 'NONE',  ( 12.19008165514798847, 0.1119984579798066066, -13.89939774083725688 ) ) ;
#14216 = CARTESIAN_POINT ( 'NONE',  ( 17.92245882712031246, -1.993980507605455310, 12.55520606452098775 ) ) ;
#14217 = ORIENTED_EDGE ( 'NONE', *, *, #58349, .F. ) ;
#14218 = EDGE_CURVE ( 'NONE', #52300, #30607, #28778, .T. ) ;
#14219 = CARTESIAN_POINT ( 'NONE',  ( 10.44125056272499918, -2.966599088466999934, -7.515315513715298934 ) ) ;
#14220 = EDGE_CURVE ( 'NONE', #64705, #13225, #41269, .T. ) ;
#14221 = ORIENTED_EDGE ( 'NONE', *, *, #4743, .F. ) ;
#14222 = CARTESIAN_POINT ( 'NONE',  ( 9.813360311708999362, 5.349397258738000538, 6.657026394682000081 ) ) ;
#14223 = CARTESIAN_POINT ( 'NONE',  ( 18.10163077481653104, 2.185641740716382841, 13.73537224937479451 ) ) ;
#14224 = CARTESIAN_POINT ( 'NONE',  ( 10.07367028041000090, 4.905765359186999852, -8.776126235875999271 ) ) ;
#14225 = ADVANCED_FACE ( 'NONE', ( #52095 ), #25880, .T. ) ;
#14226 = CARTESIAN_POINT ( 'NONE',  ( 3.522679114812999668, 3.707222910410999717, -0.07828546188973999065 ) ) ;
#14227 = CARTESIAN_POINT ( 'NONE',  ( 10.71983009893999927, -3.571743996388999864, -5.696159701115999674 ) ) ;
#14228 = CARTESIAN_POINT ( 'NONE',  ( 12.80505043854146940, -1.875000000000000444, -25.00000000000000000 ) ) ;
#14229 = CARTESIAN_POINT ( 'NONE',  ( 8.991740795306689904, -5.328224142454163648, 7.781282113468042994 ) ) ;
#14230 = ORIENTED_EDGE ( 'NONE', *, *, #28580, .F. ) ;
#14231 = CARTESIAN_POINT ( 'NONE',  ( 11.78533594839949927, -3.249987070165300196, 8.359517726022600570 ) ) ;
#14232 = CARTESIAN_POINT ( 'NONE',  ( 12.80505043854144276, 0.6249999999999994449, 13.88107975066923316 ) ) ;
#14233 = CARTESIAN_POINT ( 'NONE',  ( 16.00156003475500199, 9.132520755637999699, 8.493756974768999157 ) ) ;
#14234 = CARTESIAN_POINT ( 'NONE',  ( 5.500000000000000000, -9.503509090790997936E-14, 3.419486915844999993E-14 ) ) ;
#14236 = CARTESIAN_POINT ( 'NONE',  ( 23.60205915885299888, -2.338900754103997670, -12.00073634675999834 ) ) ;
#14235 = CARTESIAN_POINT ( 'NONE',  ( 10.49785886974000171, 3.776281431161999880, 5.717632172928999168 ) ) ;
#14237 = CARTESIAN_POINT ( 'NONE',  ( 10.96949144726329806, 3.419793223320000131, -6.681274802424499448 ) ) ;
#14238 = AXIS2_PLACEMENT_3D ( 'NONE', #57420, #67563, #25960 ) ;
#14239 = EDGE_CURVE ( 'NONE', #30450, #16931, #3514, .T. ) ;
#14240 = CARTESIAN_POINT ( 'NONE',  ( 6.999999691988000095, 12.11716380430000051, -3.069905306952000146 ) ) ;
#14241 = CARTESIAN_POINT ( 'NONE',  ( 9.325734463322998380, 4.104624583183299258, -8.498947444525299488 ) ) ;
#14242 = CARTESIAN_POINT ( 'NONE',  ( 18.08473038518645382, 0.4912829912815083744, 12.59042165808839897 ) ) ;
#14243 = CARTESIAN_POINT ( 'NONE',  ( 24.26733149983100191, 3.229785797570000394, 12.20153234936999986 ) ) ;
#14244 = CARTESIAN_POINT ( 'NONE',  ( 10.59725056272499977, 5.316133253199000208, 7.480494252843770120 ) ) ;
#14245 =( GEOMETRIC_REPRESENTATION_CONTEXT ( 3 ) GLOBAL_UNCERTAINTY_ASSIGNED_CONTEXT ( ( #36694 ) ) GLOBAL_UNIT_ASSIGNED_CONTEXT ( ( #64163, #10684, #48098 ) ) REPRESENTATION_CONTEXT ( 'NONE', 'WORKASPACE' ) );
#14246 = CARTESIAN_POINT ( 'NONE',  ( 24.63002439619599926, 0.000000000000000000, 0.000000000000000000 ) ) ;
#14247 = EDGE_LOOP ( 'NONE', ( #14678, #37191, #13250, #48075 ) ) ;
#14248 = CARTESIAN_POINT ( 'NONE',  ( 9.181706853207000307, -3.734278838175999482, 8.942129638874000364 ) ) ;
#14249 = FACE_OUTER_BOUND ( 'NONE', #14804, .T. ) ;
#14250 = CARTESIAN_POINT ( 'NONE',  ( 6.943877770042311326, -0.7023778695283228179, 1.314805733899347739 ) ) ;
#14251 = CARTESIAN_POINT ( 'NONE',  ( 10.14325461470300027, 3.159754091322399816, 7.286236678332599581 ) ) ;
#14252 = VERTEX_POINT ( 'NONE', #9107 ) ;
#14253 = AXIS2_PLACEMENT_3D ( 'NONE', #6659, #17505, #5281 ) ;
#14254 = CARTESIAN_POINT ( 'NONE',  ( 17.76900185986900027, 3.411877013825000304, 11.89794217324999970 ) ) ;
#14256 = CARTESIAN_POINT ( 'NONE',  ( 10.52799293566599914, 4.806678152079100208, 6.510429574318199464 ) ) ;
#14255 = CARTESIAN_POINT ( 'NONE',  ( 9.611342523874998989, -4.857027829858100887, -7.368808371628100318 ) ) ;
#14257 = CARTESIAN_POINT ( 'NONE',  ( 10.62256721958999961, 2.471460423959999986, -8.210789473540000216 ) ) ;
#14258 = ORIENTED_EDGE ( 'NONE', *, *, #41187, .F. ) ;
#14259 = CARTESIAN_POINT ( 'NONE',  ( 11.53443712336079763, -2.942831166283299105, 7.824978679112010838 ) ) ;
#14260 = VECTOR ( 'NONE', #18431, 1000.000000000000000 ) ;
#14261 = PLANE ( 'NONE',  #58808 ) ;
#14262 = CARTESIAN_POINT ( 'NONE',  ( 10.86272200990529946, 2.793294545435000220, 7.920925559347199219 ) ) ;
#14263 = CARTESIAN_POINT ( 'NONE',  ( 11.00589466765999802, -3.012766713855000056, 5.961506477028999385 ) ) ;
#14264 = FACE_OUTER_BOUND ( 'NONE', #55737, .T. ) ;
#14265 = ORIENTED_EDGE ( 'NONE', *, *, #35615, .T. ) ;
#14266 = CARTESIAN_POINT ( 'NONE',  ( 11.74249537357300177, -3.528133194209999601, 11.96072866431000037 ) ) ;
#14267 = CARTESIAN_POINT ( 'NONE',  ( 7.815514158766998953, 5.899700469177000528, -7.473738753146999869 ) ) ;
#14268 = CARTESIAN_POINT ( 'NONE',  ( 8.254953780971833410, -5.339409724223009412, 8.610099718891319753 ) ) ;
#14269 = CARTESIAN_POINT ( 'NONE',  ( 10.52799293566599914, -3.193321847920899792, -8.489570425681801424 ) ) ;
#14270 = CARTESIAN_POINT ( 'NONE',  ( 10.15596314287999924, -2.748296264808000267, 7.763860089407599752 ) ) ;
#14271 = VERTEX_POINT ( 'NONE', #41961 ) ;
#14272 = CARTESIAN_POINT ( 'NONE',  ( 11.03280546629000014, -5.245089378378999356, -5.027159640631999160 ) ) ;
#14273 = B_SPLINE_CURVE_WITH_KNOTS ( 'NONE', 3,
 ( #6536, #32430, #53747, #38005 ),
 .UNSPECIFIED., .F., .F.,
 ( 4, 4 ),
 ( 0.000000000000000000, 1.000000000000000000 ),
 .UNSPECIFIED. ) ;
#14274 = CARTESIAN_POINT ( 'NONE',  ( 10.55862282008599884, -3.333723918618700210, 6.425317846273999933 ) ) ;
#14275 = EDGE_LOOP ( 'NONE', ( #24337, #22211, #65251, #48026 ) ) ;
#14276 = CYLINDRICAL_SURFACE ( 'NONE', #8273, 11.50000000000000000 ) ;
#14277 = ORIENTED_EDGE ( 'NONE', *, *, #4466, .T. ) ;
#14278 = ADVANCED_FACE ( 'NONE', ( #30115 ), #58649, .F. ) ;
#14279 = ADVANCED_FACE ( 'NONE', ( #67064 ), #46439, .T. ) ;
#14280 = CARTESIAN_POINT ( 'NONE',  ( 9.925159544971000614, -4.365624317997999881, -9.242254741729000855 ) ) ;
#14281 = CARTESIAN_POINT ( 'NONE',  ( 17.60000001072100062, -11.41073498373000028, 4.623967591968000335 ) ) ;
#14282 = CARTESIAN_POINT ( 'NONE',  ( 11.67766954483535891, 4.715882430684499305, -6.395429936871999566 ) ) ;
#14283 = CARTESIAN_POINT ( 'NONE',  ( 12.30233327354039830, -5.101536739857000846, 8.220500279733599314 ) ) ;
#14284 = CARTESIAN_POINT ( 'NONE',  ( 12.17998194132759870, 2.482033040872618113, -12.45578191469033236 ) ) ;
#14285 = AXIS2_PLACEMENT_3D ( 'NONE', #26499, #37327, #48164 ) ;
#14286 = CARTESIAN_POINT ( 'NONE',  ( 11.02226222744799955, -4.880489021643899861, 6.774721295617600170 ) ) ;
#14287 = CARTESIAN_POINT ( 'NONE',  ( 8.181107780410998842, 5.485785046334999748, 8.532070739720001740 ) ) ;
#14288 = ORIENTED_EDGE ( 'NONE', *, *, #6731, .F. ) ;
#14289 = CARTESIAN_POINT ( 'NONE',  ( 9.573096873516668381, 5.217465845835396188, -7.827184855449103473 ) ) ;
#14290 = CARTESIAN_POINT ( 'NONE',  ( 9.587879440377001572, -3.762710033898000184, 8.787827024292999667 ) ) ;
#14291 = DIRECTION ( 'NONE',  ( -1.000000000000000000, 0.000000000000000000, 2.893429392025000534E-14 ) ) ;
#14292 = ORIENTED_EDGE ( 'NONE', *, *, #68079, .T. ) ;
#14293 = CARTESIAN_POINT ( 'NONE',  ( 12.68485691281878225, -1.770762539963705695, -12.47495103249912241 ) ) ;
#14294 = CARTESIAN_POINT ( 'NONE',  ( 11.01041369783139956, 3.935522326596939902, 6.223614866029000048 ) ) ;
#14295 = AXIS2_PLACEMENT_3D ( 'NONE', #66441, #66095, #18213 ) ;
#14296 = CARTESIAN_POINT ( 'NONE',  ( 11.28109314679000086, -2.660122028910999692, -6.904120269057000492 ) ) ;
#14297 = CARTESIAN_POINT ( 'NONE',  ( 10.80226354018299872, 2.907767014557178786, 8.129523725463625894 ) ) ;
#14298 = CARTESIAN_POINT ( 'NONE',  ( 18.23590051321700400, -3.219096189435000088, -11.95421454054999977 ) ) ;
#14299 = CARTESIAN_POINT ( 'NONE',  ( 10.90000000296000060, 2.899999999990999999, 5.160242730682999657 ) ) ;
#14300 = CARTESIAN_POINT ( 'NONE',  ( 12.68504826104526551, -3.238474326485687449, -13.62029029943391478 ) ) ;
#14301 = VECTOR ( 'NONE', #32047, 1000.000000000000000 ) ;
#14302 = CARTESIAN_POINT ( 'NONE',  ( 11.17056785386839834, -4.718624889240500053, -7.983608166707499620 ) ) ;
#14303 = CARTESIAN_POINT ( 'NONE',  ( 10.12426357027499790, -2.745128867668000350, -7.742104041724699570 ) ) ;
#14304 = CARTESIAN_POINT ( 'NONE',  ( 0.07500022993665000914, 0.000000000000000000, 0.000000000000000000 ) ) ;
#14305 = ORIENTED_EDGE ( 'NONE', *, *, #5648, .F. ) ;
#14306 = ORIENTED_EDGE ( 'NONE', *, *, #42020, .F. ) ;
#14307 = DIRECTION ( 'NONE',  ( 0.000000000000000000, 1.000000000000000000, 1.348567142399000110E-14 ) ) ;
#14308 = AXIS2_PLACEMENT_3D ( 'NONE', #52602, #51571, #46339 ) ;
#14309 = DIRECTION ( 'NONE',  ( 0.000000000000000000, 0.2588190451024934835, -0.9659258262890757507 ) ) ;
#14310 = CARTESIAN_POINT ( 'NONE',  ( 18.15125492461094936, 2.687770500147851571, 13.63179079428598151 ) ) ;
#14311 = ADVANCED_FACE ( 'NONE', ( #25450 ), #57484, .F. ) ;
#14312 = CARTESIAN_POINT ( 'NONE',  ( 10.02799997617999850, 3.452028386838999818, -6.074524158096999749 ) ) ;
#14313 = DIRECTION ( 'NONE',  ( -1.000000000000000000, 0.000000000000000000, 0.000000000000000000 ) ) ;
#14314 = CARTESIAN_POINT ( 'NONE',  ( 8.828674827949001269, -4.601003974012999542, -6.242416087727000296 ) ) ;
#14315 = CARTESIAN_POINT ( 'NONE',  ( 23.52015599135700086, -13.48676572944000185, 4.209850081331000027 ) ) ;
#14316 = CARTESIAN_POINT ( 'NONE',  ( 10.03490996941999924, 5.615906393494999982, 7.351455918368999143 ) ) ;
#14317 = AXIS2_PLACEMENT_3D ( 'NONE', #6682, #60182, #12288 ) ;
#14318 = CARTESIAN_POINT ( 'NONE',  ( 10.34423739839155409, -2.685214518266378469, -7.853261023685102593 ) ) ;
#14319 = ORIENTED_EDGE ( 'NONE', *, *, #29731, .F. ) ;
#14320 = CARTESIAN_POINT ( 'NONE',  ( 12.18833199825129654, -2.603395164171334653, 12.42692484756187810 ) ) ;
#14321 = CARTESIAN_POINT ( 'NONE',  ( 9.095759580228998331, -4.843256805554699618, -7.298441312785299395 ) ) ;
#14322 = CARTESIAN_POINT ( 'NONE',  ( 10.73931450027999901, 2.763002390638999994, 6.801034082888999244 ) ) ;
#14323 = CARTESIAN_POINT ( 'NONE',  ( 11.64256920625030034, -3.957769094421040190, 8.674127893687000324 ) ) ;
#14324 = CARTESIAN_POINT ( 'NONE',  ( 9.418385841233000377, 3.251172436837000301, -6.320036569851000152 ) ) ;
#14325 = PRODUCT_DEFINITION_SHAPE ( 'NONE', 'NONE',  #7317 ) ;
#14326 = CARTESIAN_POINT ( 'NONE',  ( 10.37041638348499895, 2.758294858530000226, -7.197535585171899619 ) ) ;
#14327 = EDGE_CURVE ( 'NONE', #27153, #42702, #33464, .T. ) ;
#14328 = CARTESIAN_POINT ( 'NONE',  ( 12.58477481432937672, 0.5849872192492359124, 12.68185863724641216 ) ) ;
#14329 = CARTESIAN_POINT ( 'NONE',  ( 8.379704719592000473, 4.283000592898000392, 9.286795422009001655 ) ) ;
#14330 = CARTESIAN_POINT ( 'NONE',  ( 9.910790522921001156, 3.869345236050000025, 5.882548872612999524 ) ) ;
#14331 = CARTESIAN_POINT ( 'NONE',  ( 11.35620373058000077, -3.594096350588000366, 11.23428177897000069 ) ) ;
#14332 = VERTEX_POINT ( 'NONE', #55127 ) ;
#14333 = CARTESIAN_POINT ( 'NONE',  ( 9.336654719594999818, 5.095038542659000136, -6.157541456184000062 ) ) ;
#14334 = CARTESIAN_POINT ( 'NONE',  ( 0.000000000000000000, -1.781768641235091488, 2.319305672483670477 ) ) ;
#14335 = DIRECTION ( 'NONE',  ( 1.000000000000000000, 0.000000000000000000, 0.000000000000000000 ) ) ;
#14336 = PLANE ( 'NONE',  #1660 ) ;
#14337 = CARTESIAN_POINT ( 'NONE',  ( 3.400000000000000355, -1.000000000000000000, 0.000000000000000000 ) ) ;
#14338 = CARTESIAN_POINT ( 'NONE',  ( 11.36333594839950045, -3.340240242524600056, -6.743912759487099784 ) ) ;
#14339 = ORIENTED_EDGE ( 'NONE', *, *, #36484, .F. ) ;
#14340 = CARTESIAN_POINT ( 'NONE',  ( 1.157654610683999996, -3.400502393318999950, 1.157769971473999959 ) ) ;
#14341 = CARTESIAN_POINT ( 'NONE',  ( 18.08681263786920468, -0.3285869676541873230, -12.69428288850341957 ) ) ;
#14343 = DIRECTION ( 'NONE',  ( 0.000000000000000000, 0.8514543052404082157, -0.5244287998266055073 ) ) ;
#14342 = CARTESIAN_POINT ( 'NONE',  ( 10.02052890782000105, 2.899999999999999911, 6.152188490330000370 ) ) ;
#14344 = CARTESIAN_POINT ( 'NONE',  ( 6.999999691988000095, 12.49999909016000110, -4.772673758002000880E-10 ) ) ;
#14346 = CARTESIAN_POINT ( 'NONE',  ( 12.63927634677111733, -3.229167277941582093, 13.62249984660984303 ) ) ;
#14345 = VECTOR ( 'NONE', #29043, 1000.000000000000000 ) ;
#14347 = DIRECTION ( 'NONE',  ( 1.000000000000000000, 0.000000000000000000, 0.000000000000000000 ) ) ;
#14348 = DIRECTION ( 'NONE',  ( 1.000000000000000000, 3.552713678802000396E-14, 5.329070518202999332E-14 ) ) ;
#14349 = CARTESIAN_POINT ( 'NONE',  ( 8.694605646795000808, -5.290204991635000020, 8.768102264518001121 ) ) ;
#14350 = ORIENTED_EDGE ( 'NONE', *, *, #29964, .T. ) ;
#14351 = CARTESIAN_POINT ( 'NONE',  ( 8.855420280411999912, 5.633477595780999714, 7.451234169193000412 ) ) ;
#14353 = CARTESIAN_POINT ( 'NONE',  ( 10.22908305962000064, -4.838492992840000007, -5.852445959518000507 ) ) ;
#14352 = CARTESIAN_POINT ( 'NONE',  ( 5.851234045860000066, 0.8358542970315000487, -1.207425004536999857 ) ) ;
#14354 = CARTESIAN_POINT ( 'NONE',  ( 7.641402119058184894, -5.301423981906861371, 6.346217268197262840 ) ) ;
#14355 = AXIS2_PLACEMENT_3D ( 'NONE', #36379, #31483, #63277 ) ;
#14356 = FACE_OUTER_BOUND ( 'NONE', #38566, .T. ) ;
#14357 = CARTESIAN_POINT ( 'NONE',  ( 1.838611650060999914, -0.2083462584559999942, 3.419270530009000275 ) ) ;
#14358 = VERTEX_POINT ( 'NONE', #33811 ) ;
#14359 = CARTESIAN_POINT ( 'NONE',  ( 1.810868395215021298, 2.997604546769242706, 1.386667885582162141 ) ) ;
#14360 = B_SPLINE_CURVE_WITH_KNOTS ( 'NONE', 3,
 ( #3393, #57567, #29997, #25760 ),
 .UNSPECIFIED., .F., .F.,
 ( 4, 4 ),
 ( 0.000000000000000000, 1.000000000000000000 ),
 .UNSPECIFIED. ) ;
#14361 = CARTESIAN_POINT ( 'NONE',  ( 11.20287750876920008, -4.469200303112399908, 6.771886227364699806 ) ) ;
#14362 = CARTESIAN_POINT ( 'NONE',  ( 11.00350689643929947, -3.174004326299003420, -9.060806138410798738 ) ) ;
#14363 = CARTESIAN_POINT ( 'NONE',  ( 10.39106065309000115, 4.025321035224999733, 9.261125884460000179 ) ) ;
#14364 = CARTESIAN_POINT ( 'NONE',  ( 11.11302897915239818, 4.291996373817799970, 6.397263297997000109 ) ) ;
#14365 = STYLED_ITEM ( 'NONE', ( #33298 ), #8079 ) ;
#14366 = ADVANCED_FACE ( 'NONE', ( #7231, #54777 ), #55475, .T. ) ;
#14367 = ADVANCED_FACE ( 'NONE', ( #33117 ), #64905, .F. ) ;
#14368 = CARTESIAN_POINT ( 'NONE',  ( 24.07540675168254651, -3.340246503750487150, 12.60851480763457388 ) ) ;
#14369 = EDGE_CURVE ( 'NONE', #22433, #25113, #28749, .T. ) ;
#14370 = EDGE_CURVE ( 'NONE', #9331, #23104, #37178, .T. ) ;
#14371 = CARTESIAN_POINT ( 'NONE',  ( 24.44496356299600137, 12.03536643057000077, 3.224849944858999784 ) ) ;
#14372 = CARTESIAN_POINT ( 'NONE',  ( 23.73953425137737483, -3.508700594862699695, -13.37373074045048682 ) ) ;
#14373 = CARTESIAN_POINT ( 'NONE',  ( 8.150787273753783424, 5.419866027665010577, 6.461055956173178849 ) ) ;
#14374 = ORIENTED_EDGE ( 'NONE', *, *, #58247, .T. ) ;
#14375 = CARTESIAN_POINT ( 'NONE',  ( 17.59651827076220343, -1.876037923068245794, 13.78616466676677987 ) ) ;
#14376 = FACE_BOUND ( 'NONE', #11538, .T. ) ;
#14377 = ORIENTED_EDGE ( 'NONE', *, *, #15221, .T. ) ;
#14378 = ORIENTED_EDGE ( 'NONE', *, *, #7004, .T. ) ;
#14379 = CARTESIAN_POINT ( 'NONE',  ( 10.67905590578999941, -2.899999999999999911, 6.571291218949999902 ) ) ;
#14380 = CARTESIAN_POINT ( 'NONE',  ( 8.460990129357115919, 3.502203120029797390, 5.991055485590817575 ) ) ;
#14381 = CARTESIAN_POINT ( 'NONE',  ( 11.36749010443639918, 4.863785690678500195, 7.435402237490909449 ) ) ;
#14382 = CARTESIAN_POINT ( 'NONE',  ( 10.84168637167000071, 2.681011538858999899, 6.554754637093000547 ) ) ;
#14383 = CARTESIAN_POINT ( 'NONE',  ( 10.73506130198999919, 5.202496273738000276, -8.441412224440000500 ) ) ;
#14384 = CARTESIAN_POINT ( 'NONE',  ( 9.758812222687625493, -3.837269700090108593, -8.359680823568968577 ) ) ;
#14385 = CARTESIAN_POINT ( 'NONE',  ( 9.442085454646999665, -4.742494605615999781, 8.809986937145000141 ) ) ;
#14386 = CARTESIAN_POINT ( 'NONE',  ( 18.27044763842724251, 0.1172743548790672746, -12.59945959730644205 ) ) ;
#14387 = CARTESIAN_POINT ( 'NONE',  ( 10.83767365324000131, -5.758089526411000136, -6.911472812823999945 ) ) ;
#14388 = CARTESIAN_POINT ( 'NONE',  ( 10.62903166480609940, -4.864052766304100217, -7.560921321260908989 ) ) ;
#14389 = DIRECTION ( 'NONE',  ( 0.000000000000000000, 1.000000000000000000, 0.000000000000000000 ) ) ;
#14391 = ORIENTED_EDGE ( 'NONE', *, *, #21765, .F. ) ;
#14390 = B_SPLINE_CURVE_WITH_KNOTS ( 'NONE', 3,
 ( #13774, #36121, #2927, #41713 ),
 .UNSPECIFIED., .F., .F.,
 ( 4, 4 ),
 ( 0.000000000000000000, 1.000000000000000000 ),
 .UNSPECIFIED. ) ;
#14392 = CARTESIAN_POINT ( 'NONE',  ( 11.01665874711000015, -6.699714419246999952, -5.516646458005999953 ) ) ;
#14393 = CARTESIAN_POINT ( 'NONE',  ( 24.94498381146992116, 11.54147255574495823, -3.218772431449972604 ) ) ;
#14394 = CARTESIAN_POINT ( 'NONE',  ( 11.10000000011000054, 5.340540509194999785, -6.721892583407999666 ) ) ;
#14395 = CIRCLE ( 'NONE', #52307, 12.32510602165000613 ) ;
#14396 = CARTESIAN_POINT ( 'NONE',  ( 17.77313190797694986, 1.794191980291843347, 12.47160287655520428 ) ) ;
#14397 = CARTESIAN_POINT ( 'NONE',  ( 9.583051052052001140, 5.255397705012999410, -7.745684736446600382 ) ) ;
#14398 = B_SPLINE_CURVE_WITH_KNOTS ( 'NONE', 3,
 ( #3709, #20489, #31333, #62782, #62445, #25046, #68030, #52302, #4051, #46378 ),
 .UNSPECIFIED., .F., .F.,
 ( 4, 2, 2, 2, 4 ),
 ( 0.000000000000000000, 0.2500000000000003331, 0.5000000000000006661, 0.7500000000000003331, 1.000000000000000000 ),
 .UNSPECIFIED. ) ;
#14399 = CARTESIAN_POINT ( 'NONE',  ( 12.21346991607042298, 2.095738610141147706, 13.84225324474580354 ) ) ;
#14400 = CYLINDRICAL_SURFACE ( 'NONE', #33350, 1.350000000000000533 ) ;
#14401 = ORIENTED_EDGE ( 'NONE', *, *, #50136, .T. ) ;
#14402 = AXIS2_PLACEMENT_3D ( 'NONE', #8234, #66266, #61031 ) ;
#14403 = CARTESIAN_POINT ( 'NONE',  ( 12.43800415093376621, 0.5060493093079869720, -12.68643001349182597 ) ) ;
#14404 = CARTESIAN_POINT ( 'NONE',  ( 12.08006676141316049, -0.02431279293010735545, 13.99999914078079932 ) ) ;
#14405 = EDGE_LOOP ( 'NONE', ( #21632, #45822, #40347, #65632 ) ) ;
#14406 = DIRECTION ( 'NONE',  ( 0.000000000000000000, 0.000000000000000000, 1.000000000000000000 ) ) ;
#14407 = DIRECTION ( 'NONE',  ( -0.7071069136393470789, 0.000000000000000000, -0.7071066487337230866 ) ) ;
#14408 = CARTESIAN_POINT ( 'NONE',  ( 10.63559687351579974, -2.907767014557175678, -6.870476274536380323 ) ) ;
#14409 = CARTESIAN_POINT ( 'NONE',  ( 11.10441638348510018, -4.841589649988700117, 7.705001100909899314 ) ) ;
#14410 = EDGE_CURVE ( 'NONE', #13783, #66620, #34156, .T. ) ;
#14411 = CARTESIAN_POINT ( 'NONE',  ( 8.625655602088629692, 5.349651844363364717, -7.676783314127475499 ) ) ;
#14412 = DIRECTION ( 'NONE',  ( -1.000000000000000000, 0.000000000000000000, 0.000000000000000000 ) ) ;
#14413 = CARTESIAN_POINT ( 'NONE',  ( 11.13220574173981170, 5.136173005413450454, 8.088082908809449023 ) ) ;
#14414 = EDGE_CURVE ( 'NONE', #64893, #33797, #47956, .T. ) ;
#14415 = CARTESIAN_POINT ( 'NONE',  ( 10.37581074856900187, -5.172583146916752028, -8.000243450341619322 ) ) ;
#14416 = CARTESIAN_POINT ( 'NONE',  ( 9.707908211423999845, -3.300107492866999781, -5.762405935562999737 ) ) ;
#14417 = CARTESIAN_POINT ( 'NONE',  ( 10.35410941423799791, 4.742797679580299963, -6.825313060354999628 ) ) ;
#14418 = DIRECTION ( 'NONE',  ( 1.000000000000000000, 0.000000000000000000, 0.000000000000000000 ) ) ;
#14419 = CARTESIAN_POINT ( 'NONE',  ( 11.23589666366019912, 3.960399224793059947, -8.391246537305399045 ) ) ;
#14420 = CARTESIAN_POINT ( 'NONE',  ( 10.16455864497999961, 4.898932057185599653, -8.204026508301600629 ) ) ;
#14422 = CARTESIAN_POINT ( 'NONE',  ( 12.27188044047571402, 2.173264662094914090, 12.52171693736594271 ) ) ;
#14421 = CARTESIAN_POINT ( 'NONE',  ( 15.56012107570600023, -8.822147194309000184, -7.967418575816001436 ) ) ;
#14423 = CARTESIAN_POINT ( 'NONE',  ( 23.50387503050299998, 14.00000000000000000, 0.000000000000000000 ) ) ;
#14424 = ORIENTED_EDGE ( 'NONE', *, *, #68875, .F. ) ;
#14425 = CARTESIAN_POINT ( 'NONE',  ( 10.99999689388000057, 1.243449787579999883E-13, 0.000000000000000000 ) ) ;
#14426 = CARTESIAN_POINT ( 'NONE',  ( 9.302064839073725722, 5.580009628946752898, -6.689794082201894199 ) ) ;
#14427 = CARTESIAN_POINT ( 'NONE',  ( 9.021784697134998865, 4.545051930576500254, 8.343659109631099469 ) ) ;
#14428 = CARTESIAN_POINT ( 'NONE',  ( 9.201570984676626708, 3.555997837402618877, -8.253919324947762703 ) ) ;
#14429 = CARTESIAN_POINT ( 'NONE',  ( 24.35365242081699932, 12.20235406293000935, -3.288253180433003298 ) ) ;
#14430 = CARTESIAN_POINT ( 'NONE',  ( 12.40004937879930047, 2.976133613074172679, 13.56081502232355795 ) ) ;
#14431 = CARTESIAN_POINT ( 'NONE',  ( 10.12947109217999930, -5.100000000000000533, 6.152188490330000370 ) ) ;
#14432 = VERTEX_POINT ( 'NONE', #2332 ) ;
#14433 = CARTESIAN_POINT ( 'NONE',  ( 9.024747021775999301, -4.858221690000700477, -8.253120162257399528 ) ) ;
#14434 = B_SPLINE_CURVE_WITH_KNOTS ( 'NONE', 3,
 ( #64464, #42817, #37563, #15564, #27783 ),
 .UNSPECIFIED., .F., .F.,
 ( 4, 1, 4 ),
 ( 0.000000000000000000, 0.5000000000000000000, 1.000000000000000000 ),
 .UNSPECIFIED. ) ;
#14435 = LINE ( 'NONE', #36093, #47722 ) ;
#14436 = CARTESIAN_POINT ( 'NONE',  ( 11.43990547754509990, -2.967013601007999934, 7.467215766047949899 ) ) ;
#14437 = CARTESIAN_POINT ( 'NONE',  ( 17.55505043854143565, 1.760845406083387354, -12.47635457398815362 ) ) ;
#14438 = CARTESIAN_POINT ( 'NONE',  ( 8.848090123393001605, -2.900413175355999851, -6.422155424834999238 ) ) ;
#14439 = DIRECTION ( 'NONE',  ( 1.000000000000000000, 0.000000000000000000, 0.000000000000000000 ) ) ;
#14440 = EDGE_CURVE ( 'NONE', #54722, #68545, #18419, .T. ) ;
#14441 = CARTESIAN_POINT ( 'NONE',  ( 12.19818565359414819, 2.649653948234573786, -13.64057837091597669 ) ) ;
#14442 = DIRECTION ( 'NONE',  ( -0.8987684456439055669, 0.000000000000000000, 0.4384236320214022764 ) ) ;
#14443 = CARTESIAN_POINT ( 'NONE',  ( 12.80505043854146940, -1.760910691117821614, -12.47634535983622683 ) ) ;
#14444 = CARTESIAN_POINT ( 'NONE',  ( 9.683745612763230426, -2.796157461453096182, 8.204744624355374327 ) ) ;
#14445 = EDGE_CURVE ( 'NONE', #28970, #15559, #14652, .T. ) ;
#14446 = CARTESIAN_POINT ( 'NONE',  ( 12.14438218221664378, 0.3016537271415140609, -13.99676704218776813 ) ) ;
#14447 = ADVANCED_FACE ( 'NONE', ( #13182 ), #11956, .T. ) ;
#14448 = CARTESIAN_POINT ( 'NONE',  ( 13.64649313145500109, -9.010717346174999420, -7.468773375841999851 ) ) ;
#14449 = CARTESIAN_POINT ( 'NONE',  ( 11.09999998388999920, 9.505740268506999158, 6.352095299649000104 ) ) ;
#14450 = CARTESIAN_POINT ( 'NONE',  ( 10.91620964606000044, -2.818413279081999789, -6.814156272943999504 ) ) ;
#14451 = CARTESIAN_POINT ( 'NONE',  ( 8.871889158775999817, 2.702406276695999754, -6.981052078638000147 ) ) ;
#14452 = CARTESIAN_POINT ( 'NONE',  ( 12.33518044953559922, -3.231951024059400268, 7.099502491684900107 ) ) ;
#14453 = VERTEX_POINT ( 'NONE', #8606 ) ;
#14454 = CARTESIAN_POINT ( 'NONE',  ( 8.528661480133219897, -4.352698949119082172, 8.815590613233990069 ) ) ;
#14455 = CARTESIAN_POINT ( 'NONE',  ( 18.06209397514826165, 1.995989992690354153, -13.85698731868970590 ) ) ;
#14456 = ORIENTED_EDGE ( 'NONE', *, *, #38309, .F. ) ;
#14457 = CARTESIAN_POINT ( 'NONE',  ( 10.46595058442700044, -3.655872208659600275, 8.295791434820300125 ) ) ;
#14458 = CARTESIAN_POINT ( 'NONE',  ( 2.696806799210917038, -0.9161175952574931447, 3.408904368339101598 ) ) ;
#14459 = CARTESIAN_POINT ( 'NONE',  ( 8.546960841229999772, 2.724453559418999582, -8.908010318766001134 ) ) ;
#14460 = CARTESIAN_POINT ( 'NONE',  ( 13.49980696793000057, 9.514462421839999351, 7.834836582454001608 ) ) ;
#14461 = CARTESIAN_POINT ( 'NONE',  ( 11.48011496860029901, -3.080230834057799960, -7.028661263734299780 ) ) ;
#14462 = CARTESIAN_POINT ( 'NONE',  ( 11.60000000000000142, -3.195619894033323583, -6.677026092743741259 ) ) ;
#14463 = B_SPLINE_CURVE_WITH_KNOTS ( 'NONE', 3,
 ( #61402, #13857, #40091, #13522 ),
 .UNSPECIFIED., .F., .F.,
 ( 4, 4 ),
 ( 0.000000000000000000, 1.000000000000000000 ),
 .UNSPECIFIED. ) ;
#14464 = PLANE ( 'NONE',  #63036 ) ;
#14465 = ORIENTED_EDGE ( 'NONE', *, *, #10336, .T. ) ;
#14466 = DIRECTION ( 'NONE',  ( 0.7071067811866525998, 0.000000000000000000, -0.7071067811864425456 ) ) ;
#14467 = CARTESIAN_POINT ( 'NONE',  ( 10.80226354018233259, -5.092232985442821658, 8.129523725463625894 ) ) ;
#14468 = CARTESIAN_POINT ( 'NONE',  ( 8.590779719591999708, 2.836879604150999601, -8.783908972046001296 ) ) ;
#14469 = ORIENTED_EDGE ( 'NONE', *, *, #47992, .F. ) ;
#14470 = EDGE_CURVE ( 'NONE', #21511, #67420, #2151, .T. ) ;
#14471 = B_SPLINE_CURVE_WITH_KNOTS ( 'NONE', 3,
 ( #34855, #60034, #49893, #50239, #56170 ),
 .UNSPECIFIED., .F., .F.,
 ( 4, 1, 4 ),
 ( 0.000000000000000000, 0.5000000000000000000, 1.000000000000000000 ),
 .UNSPECIFIED. ) ;
#14472 = CARTESIAN_POINT ( 'NONE',  ( 10.64127413024999846, 2.258699798012000048, -6.863478635463000188 ) ) ;
#14473 = EDGE_LOOP ( 'NONE', ( #29970, #6552, #24755, #4462 ) ) ;
#14474 = CARTESIAN_POINT ( 'NONE',  ( 10.03590035061499997, 4.340961869598300105, 6.267064942904999825 ) ) ;
#14475 = CARTESIAN_POINT ( 'NONE',  ( 18.15975285618101154, -2.341680162859185010, -12.48703895936062480 ) ) ;
#14476 = CARTESIAN_POINT ( 'NONE',  ( 9.599999931441001166, -4.000000000000000000, 7.500000000000000000 ) ) ;
#14477 = PRODUCT_DEFINITION_SHAPE ( 'NONE', 'NONE',  #69205 ) ;
#14478 = B_SPLINE_CURVE_WITH_KNOTS ( 'NONE', 3,
 ( #19778, #31307, #15216, #57174, #47385, #26404 ),
 .UNSPECIFIED., .F., .F.,
 ( 4, 2, 4 ),
 ( 0.000000000000000000, 0.5000000000000000000, 1.000000000000000000 ),
 .UNSPECIFIED. ) ;
#14479 = CARTESIAN_POINT ( 'NONE',  ( 4.400035872229480560, -1.058819220088977886, 0.8053076396761240652 ) ) ;
#14480 = CARTESIAN_POINT ( 'NONE',  ( 10.48632761434999949, -8.229716073962000777, -6.713145785397999887 ) ) ;
#14481 = ORIENTED_EDGE ( 'NONE', *, *, #65878, .T. ) ;
#14482 = CARTESIAN_POINT ( 'NONE',  ( 24.53429011008099891, 3.614318944477000084, -12.31267538233000103 ) ) ;
#14483 = CARTESIAN_POINT ( 'NONE',  ( 11.29596084123000210, 2.828872990872000059, -8.191118698770999629 ) ) ;
#14484 = DIRECTION ( 'NONE',  ( 0.9999999999990064614, -1.235604879081008633E-06, 6.784100806884041873E-07 ) ) ;
#14485 = CARTESIAN_POINT ( 'NONE',  ( 12.68593947922891552, 3.238585582162118115, -13.62026383368923454 ) ) ;
#14486 = CARTESIAN_POINT ( 'NONE',  ( 18.17070062201315039, 0.3858260082455215456, 13.99468631105251859 ) ) ;
#14487 = CARTESIAN_POINT ( 'NONE',  ( 17.90328515628180384, 11.55107739452601834, -4.842351092693065517 ) ) ;
#14488 = CARTESIAN_POINT ( 'NONE',  ( 10.47094409420000005, -5.100000000000000533, 6.571291218949999902 ) ) ;
#14489 = ORIENTED_EDGE ( 'NONE', *, *, #46396, .T. ) ;
#14490 = ORIENTED_EDGE ( 'NONE', *, *, #60574, .T. ) ;
#14491 = CARTESIAN_POINT ( 'NONE',  ( 9.617285841233000454, 5.306366356490000769, -7.996450761531000317 ) ) ;
#14492 = EDGE_CURVE ( 'NONE', #53681, #22879, #9624, .T. ) ;
#14493 = CARTESIAN_POINT ( 'NONE',  ( 10.61503919148293740, 5.349978903665603802, -7.499997722305280945 ) ) ;
#14494 = CARTESIAN_POINT ( 'NONE',  ( 1.061390132541624842, 3.499999999999999112, 0.4581489286485193602 ) ) ;
#14495 = CARTESIAN_POINT ( 'NONE',  ( 23.95413520383817740, 3.345971697916644949, 12.83256498468845841 ) ) ;
#14496 = CARTESIAN_POINT ( 'NONE',  ( 24.51040282428800055, 8.845021705915000254, -9.169845360568999126 ) ) ;
#14497 = CARTESIAN_POINT ( 'NONE',  ( 11.29998578400000042, -3.824193979571000046, 11.71675423233000046 ) ) ;
#14499 = CARTESIAN_POINT ( 'NONE',  ( 7.844724277266999835, 4.719412473309000156, 6.357657803787000184 ) ) ;
#14498 = CARTESIAN_POINT ( 'NONE',  ( 10.71426717315700117, -4.869050473540199597, 8.240598219300300897 ) ) ;
#14500 = CARTESIAN_POINT ( 'NONE',  ( 8.468724635341004614, -4.797383707087001348, -6.431807026291995300 ) ) ;
#14501 = ORIENTED_EDGE ( 'NONE', *, *, #19446, .F. ) ;
#14502 = LINE ( 'NONE', #9932, #13520 ) ;
#14503 = DIRECTION ( 'NONE',  ( -1.000000000000000000, 0.000000000000000000, 0.000000000000000000 ) ) ;
#14504 = CARTESIAN_POINT ( 'NONE',  ( 9.221132306829000314, -4.645169647889000331, -5.840816811670999975 ) ) ;
#14505 = DIRECTION ( 'NONE',  ( -0.7071058580588949205, 0.7071077043129949669, -4.007463041294969893E-09 ) ) ;
#14506 = CARTESIAN_POINT ( 'NONE',  ( 11.04384236319999957, -7.396937235950000300, 6.274987567768999241 ) ) ;
#14507 = DIRECTION ( 'NONE',  ( 0.000000000000000000, 1.000000000000000000, 0.000000000000000000 ) ) ;
#14508 = CARTESIAN_POINT ( 'NONE',  ( 8.596685841231000325, 2.141799395716999843, -7.895788736628000848 ) ) ;
#14509 = B_SPLINE_CURVE_WITH_KNOTS ( 'NONE', 3,
 ( #55828, #60719, #12835, #34162, #1997 ),
 .UNSPECIFIED., .F., .F.,
 ( 4, 1, 4 ),
 ( 0.000000000000000000, 0.002767885366475097975, 0.1253844953241992632 ),
 .UNSPECIFIED. ) ;
#14510 = CARTESIAN_POINT ( 'NONE',  ( 13.80679720086500062, 8.861764092194999165, 7.504495031742999700 ) ) ;
#14511 = TOROIDAL_SURFACE ( 'NONE', #56928, 12.35000000006999876, 0.5000000000000000000 ) ;
#14512 = CARTESIAN_POINT ( 'NONE',  ( 9.050000000000000711, 0.000000000000000000, 4.000000000000000000 ) ) ;
#14513 = B_SPLINE_CURVE_WITH_KNOTS ( 'NONE', 3,
 ( #33496, #8976, #30651, #62455 ),
 .UNSPECIFIED., .F., .F.,
 ( 4, 4 ),
 ( 0.000000000000000000, 1.000000000000000000 ),
 .UNSPECIFIED. ) ;
#14514 = CARTESIAN_POINT ( 'NONE',  ( 6.059559201232000092, 1.111956540095999868, -0.3830577677631999967 ) ) ;
#14515 = B_SPLINE_SURFACE_WITH_KNOTS ( 'NONE', 3, 3, ( 
 ( #3388, #40797, #13898, #28959 ),
 ( #19475, #62121, #50262, #8981 ),
 ( #3725, #67697, #45025, #18452 ),
 ( #47084, #52322, #57913, #10012 ),
 ( #31350, #63833, #21193, #48112 ),
 ( #10358, #58254, #31692, #57559 ),
 ( #10697, #36939, #41153, #41831 ),
 ( #35898, #20161, #15608, #52663 ) ),
 .UNSPECIFIED., .F., .F., .F.,
 ( 4, 1, 1, 1, 1, 4 ),
 ( 4, 4 ),
 ( 0.008355503774731999275, 0.05882352941176000050, 0.1176470588234999892, 0.1764705882353000133, 0.2352941176471000095, 0.2534843214274999923 ),
 ( -0.1830816817365999993, 1.182949857538000193 ),
 .UNSPECIFIED. ) ;
#14516 = FACE_OUTER_BOUND ( 'NONE', #27415, .T. ) ;
#14517 = CARTESIAN_POINT ( 'NONE',  ( 2.220184363877999889, 1.697856089507000066, -2.629976706909999518 ) ) ;
#14518 = ORIENTED_EDGE ( 'NONE', *, *, #25818, .F. ) ;
#14519 = CARTESIAN_POINT ( 'NONE',  ( 12.51941477301789973, -0.5560043133243457447, -12.68361349193355103 ) ) ;
#14520 = CARTESIAN_POINT ( 'NONE',  ( 12.18869345026739737, -2.603827955476766043, -12.42676989087486206 ) ) ;
#14521 = CARTESIAN_POINT ( 'NONE',  ( 16.09997386696500143, 5.375854662731813782, 10.37779375783400937 ) ) ;
#14522 = CARTESIAN_POINT ( 'NONE',  ( 8.898551658772998252, 5.146726419831999522, 6.597424767138000412 ) ) ;
#14523 = CARTESIAN_POINT ( 'NONE',  ( 7.225322421146570306, -2.650264760010439868, 7.500018091723870128 ) ) ;
#14524 = EDGE_LOOP ( 'NONE', ( #50174, #56739, #4696, #6432, #21543 ) ) ;
#14525 = LINE ( 'NONE', #36880, #16533 ) ;
#14526 = EDGE_CURVE ( 'NONE', #2005, #25280, #25407, .T. ) ;
#14527 = SHAPE_DEFINITION_REPRESENTATION ( #66764, #60729 ) ;
#14528 = ADVANCED_FACE ( 'NONE', ( #52283 ), #6187, .T. ) ;
#14529 = CARTESIAN_POINT ( 'NONE',  ( 0.5211625230349857807, 3.419518492017623146, 0.8791808744453025737 ) ) ;
#14530 = CARTESIAN_POINT ( 'NONE',  ( 13.60429364930200080, -11.50682694388999927, -2.143319390578000139 ) ) ;
#14531 = CARTESIAN_POINT ( 'NONE',  ( 7.806464712881202139, 3.011078243462636639, 6.531313835357527964 ) ) ;
#14532 = CARTESIAN_POINT ( 'NONE',  ( 10.55569598648999907, 5.130952141044000214, -8.173387776112500447 ) ) ;
#14533 = ORIENTED_EDGE ( 'NONE', *, *, #36662, .F. ) ;
#14534 = CARTESIAN_POINT ( 'NONE',  ( 10.25888544622000076, -4.512389816463000081, 5.993697694029000544 ) ) ;
#14535 = ORIENTED_EDGE ( 'NONE', *, *, #19571, .T. ) ;
#14536 = CARTESIAN_POINT ( 'NONE',  ( 9.449367199446873755, 4.457171844012795425, 8.907134314554838284 ) ) ;
#14537 = CARTESIAN_POINT ( 'NONE',  ( 15.86376629110799996, 3.753680978508000088, 11.28125155222999787 ) ) ;
#14538 = CARTESIAN_POINT ( 'NONE',  ( 15.98722619340700213, 8.633165116997000510, 7.765565731395999372 ) ) ;
#14539 = EDGE_LOOP ( 'NONE', ( #22256, #25053, #41176 ) ) ;
#14540 = CARTESIAN_POINT ( 'NONE',  ( -0.000000000000000000, 2.319407620233877587, -1.781870588985297932 ) ) ;
#14541 = CARTESIAN_POINT ( 'NONE',  ( 4.649999478197480052, 2.033928581112999763E-13, -2.806643806251999915E-13 ) ) ;
#14542 = CARTESIAN_POINT ( 'NONE',  ( 7.979454719588000344, 2.702884610408000210, -6.624425519483001068 ) ) ;
#14543 = DIRECTION ( 'NONE',  ( -0.7071067811866525998, 0.000000000000000000, -0.7071067811864425456 ) ) ;
#14544 = CARTESIAN_POINT ( 'NONE',  ( 24.67921311619700120, 3.567517360056999820, 12.13750603036999998 ) ) ;
#14545 = ORIENTED_EDGE ( 'NONE', *, *, #54577, .F. ) ;
#14546 = CARTESIAN_POINT ( 'NONE',  ( 9.194602547868999665, -5.157768569202000108, 8.637845986715998237 ) ) ;
#14547 = CARTESIAN_POINT ( 'NONE',  ( 12.22895947710367359, -2.742405092547198553, -13.61899867098736472 ) ) ;
#14548 = PLANE ( 'NONE',  #45033 ) ;
#14549 = ORIENTED_EDGE ( 'NONE', *, *, #33456, .F. ) ;
#14550 = EDGE_CURVE ( 'NONE', #53746, #21776, #1937, .T. ) ;
#14551 = CARTESIAN_POINT ( 'NONE',  ( 10.90000000000000036, -8.263403946409999534, -6.953859016290999229 ) ) ;
#14552 = CARTESIAN_POINT ( 'NONE',  ( 9.299999999999998934, -4.537600397704999899, 9.154563893594000135 ) ) ;
#14553 = ORIENTED_EDGE ( 'NONE', *, *, #61485, .T. ) ;
#14554 = CARTESIAN_POINT ( 'NONE',  ( 10.70959604073516225, 5.759191062913065373, 7.715212687030478023 ) ) ;
#14555 = ADVANCED_FACE ( 'NONE', ( #12393 ), #7485, .T. ) ;
#14556 = DIRECTION ( 'NONE',  ( -1.000000000000000000, 0.000000000000000000, 0.000000000000000000 ) ) ;
#14557 = DIRECTION ( 'NONE',  ( 1.000000000000000000, 0.000000000000000000, 0.000000000000000000 ) ) ;
#14558 = FACE_OUTER_BOUND ( 'NONE', #32501, .T. ) ;
#14559 = CARTESIAN_POINT ( 'NONE',  ( 12.58447130036695150, -0.5851376999905949505, -13.88342059653408533 ) ) ;
#14560 = CARTESIAN_POINT ( 'NONE',  ( 18.17889124921894961, -2.543048589645668489, 12.44148151073661523 ) ) ;
#14561 = ORIENTED_EDGE ( 'NONE', *, *, #10477, .T. ) ;
#14562 = CARTESIAN_POINT ( 'NONE',  ( 8.354417780085995560, -5.125509315120996057, 6.367236178909004174 ) ) ;
#14563 = VERTEX_POINT ( 'NONE', #1214 ) ;
#14564 = CARTESIAN_POINT ( 'NONE',  ( 10.18240541510999897, 2.607737086676999994, 7.783408568367999436 ) ) ;
#14565 = AXIS2_PLACEMENT_3D ( 'NONE', #53283, #47699, #4344 ) ;
#14566 = DIRECTION ( 'NONE',  ( 1.000000000000000000, 0.000000000000000000, 0.000000000000000000 ) ) ;
#14567 = CARTESIAN_POINT ( 'NONE',  ( 9.675870280412999236, 3.031907308384000022, -8.729608011560001657 ) ) ;
#14568 = B_SPLINE_CURVE_WITH_KNOTS ( 'NONE', 3,
 ( #1530, #54317, #55715, #49076 ),
 .UNSPECIFIED., .F., .F.,
 ( 4, 4 ),
 ( 0.000000000000000000, 1.000000000000000000 ),
 .UNSPECIFIED. ) ;
#14569 = CARTESIAN_POINT ( 'NONE',  ( 2.635666247922999972, -2.915774638497000026, 2.013997748395000009 ) ) ;
#14570 = LINE ( 'NONE', #46381, #42143 ) ;
#14571 = DIRECTION ( 'NONE',  ( -1.000000000000000000, 0.000000000000000000, 0.000000000000000000 ) ) ;
#14572 = CARTESIAN_POINT ( 'NONE',  ( 9.038117261819090587, -4.950750304293762838, 8.458219317142523508 ) ) ;
#14573 = ORIENTED_EDGE ( 'NONE', *, *, #42168, .F. ) ;
#14574 = CARTESIAN_POINT ( 'NONE',  ( 11.46533729122639933, -5.140346530769000388, 7.529998433785960010 ) ) ;
#14575 = CARTESIAN_POINT ( 'NONE',  ( 3.123890132544374421, 2.150913519912194261, 2.798833948393636195 ) ) ;
#14576 = CARTESIAN_POINT ( 'NONE',  ( -0.2999999999999999889, 1.154700538379000108, 0.000000000000000000 ) ) ;
#14577 = DIRECTION ( 'NONE',  ( -0.000000000000000000, -0.000000000000000000, 1.000000000000000000 ) ) ;
#14579 = CARTESIAN_POINT ( 'NONE',  ( 12.70933660601936133, 3.243304671732729183, -13.61914346456424951 ) ) ;
#14578 = CARTESIAN_POINT ( 'NONE',  ( 10.31167969999000000, 2.874476822401000220, 8.900029516786000627 ) ) ;
#14580 = CARTESIAN_POINT ( 'NONE',  ( 11.48225819896749833, 2.879005208331999910, -7.711331004020999913 ) ) ;
#14581 = CARTESIAN_POINT ( 'NONE',  ( 11.33570505509991655, -3.091015088729731186, -7.175001305235313431 ) ) ;
#14582 = CARTESIAN_POINT ( 'NONE',  ( 9.629684229509999582, 3.291972602441000095, -6.787581931282099745 ) ) ;
#14583 = CARTESIAN_POINT ( 'NONE',  ( 17.56702613447739481, 0.7192913015564668111, 12.57945229205062709 ) ) ;
#14584 = CARTESIAN_POINT ( 'NONE',  ( 11.00000000000000000, 5.079754677601000523, -7.825000000000000178 ) ) ;
#14585 = CARTESIAN_POINT ( 'NONE',  ( 11.64122412107036908, 4.062069863985690255, 8.673243607771999208 ) ) ;
#14586 = CARTESIAN_POINT ( 'NONE',  ( 23.58305362212199796, 10.33301849453000010, 9.360217489553999570 ) ) ;
#14587 = VERTEX_POINT ( 'NONE', #22525 ) ;
#14588 = CARTESIAN_POINT ( 'NONE',  ( 8.128308059623998716, -3.117370956513999758, 8.662188901935000018 ) ) ;
#14589 = CARTESIAN_POINT ( 'NONE',  ( 24.30000000000000071, 11.85420044612000012, -3.901016762742000488 ) ) ;
#14590 = FACE_BOUND ( 'NONE', #27199, .T. ) ;
#14591 = B_SPLINE_CURVE_WITH_KNOTS ( 'NONE', 3,
 ( #63592, #68147, #3828, #30424, #57661, #20610 ),
 .UNSPECIFIED., .F., .F.,
 ( 4, 2, 4 ),
 ( 0.000000000000000000, 0.5000000000000000000, 1.000000000000000000 ),
 .UNSPECIFIED. ) ;
#14592 = ORIENTED_EDGE ( 'NONE', *, *, #44371, .T. ) ;
#14593 = CARTESIAN_POINT ( 'NONE',  ( 10.72180282789423522, 2.874603711610002055, 6.749639981020137292 ) ) ;
#14594 = AXIS2_PLACEMENT_3D ( 'NONE', #23164, #55331, #50425 ) ;
#14595 = CARTESIAN_POINT ( 'NONE',  ( 11.64633327354034797, 3.135095881599500256, 8.065722083251399610 ) ) ;
#14596 = CARTESIAN_POINT ( 'NONE',  ( 10.86460778041000097, 3.843601682313000367, -5.985271987931999327 ) ) ;
#14597 = VERTEX_POINT ( 'NONE', #33379 ) ;
#14598 = CARTESIAN_POINT ( 'NONE',  ( 8.636611612198999310, 5.100000000000000533, -6.496831119766667051 ) ) ;
#14600 = AXIS2_PLACEMENT_3D ( 'NONE', #27136, #37613, #64513 ) ;
#14599 = CARTESIAN_POINT ( 'NONE',  ( 17.92356899877518472, -1.853474162636749467, 12.46298541230695456 ) ) ;
#14601 = CARTESIAN_POINT ( 'NONE',  ( 10.54272335273199879, 4.444874504667400750, 6.301916924546999255 ) ) ;
#14602 = CARTESIAN_POINT ( 'NONE',  ( 13.70003001321900271, -9.668726926528000476, -7.961868161445000425 ) ) ;
#14603 = CARTESIAN_POINT ( 'NONE',  ( 14.46666666233133469, 9.187454791078208061, 8.213178404136472821 ) ) ;
#14604 = ORIENTED_EDGE ( 'NONE', *, *, #43257, .F. ) ;
#14605 = CARTESIAN_POINT ( 'NONE',  ( 11.53898808224000128, -3.920528549154999709, 11.93545759853000021 ) ) ;
#14606 = EDGE_CURVE ( 'NONE', #18530, #45160, #58842, .T. ) ;
#14607 = EDGE_CURVE ( 'NONE', #32433, #26116, #54640, .T. ) ;
#14608 = CARTESIAN_POINT ( 'NONE',  ( 7.765789158767000266, 5.525377065333000104, -6.367402836891999485 ) ) ;
#14609 = AXIS2_PLACEMENT_3D ( 'NONE', #17879, #33268, #28024 ) ;
#14610 = CARTESIAN_POINT ( 'NONE',  ( 8.284908184216730476, -4.822684648958374787, 9.032360259545255232 ) ) ;
#14611 = CARTESIAN_POINT ( 'NONE',  ( 9.094151519677000195, -3.975306837623020062, 6.358456126310000123 ) ) ;
#14612 = ORIENTED_EDGE ( 'NONE', *, *, #41907, .T. ) ;
#14613 = CARTESIAN_POINT ( 'NONE',  ( 10.92233852386999970, -5.248250142883000180, -4.977516224977000192 ) ) ;
#14614 = CARTESIAN_POINT ( 'NONE',  ( 11.33810672858430024, -5.021298157087000114, 8.268288002587098617 ) ) ;
#14615 = EDGE_LOOP ( 'NONE', ( #64374, #5158, #2943, #6349 ) ) ;
#14616 = LINE ( 'NONE', #41864, #51826 ) ;
#14617 = VERTEX_POINT ( 'NONE', #50148 ) ;
#14618 = CARTESIAN_POINT ( 'NONE',  ( 10.02091161619000026, -4.911674715448000050, -6.466751564808000730 ) ) ;
#14619 = CARTESIAN_POINT ( 'NONE',  ( 2.353056799209541250, -2.798833948393629534, -2.150913519912204031 ) ) ;
#14620 = CARTESIAN_POINT ( 'NONE',  ( 10.81524174883999834, 3.971581146373189597, -8.533115712456000423 ) ) ;
#14621 = CARTESIAN_POINT ( 'NONE',  ( 11.97500581613029880, -3.011381429075500105, 6.865182626353099948 ) ) ;
#14622 = CARTESIAN_POINT ( 'NONE',  ( 12.29460735697731444, 2.139198256859471403, -12.52837235904283908 ) ) ;
#14623 = CARTESIAN_POINT ( 'NONE',  ( 11.04687750876899877, -4.617914354660699772, 6.541108991297599928 ) ) ;
#14624 = CARTESIAN_POINT ( 'NONE',  ( 7.282482780409000434, 3.448180532882000104, 9.222462917385000125 ) ) ;
#14625 = ORIENTED_EDGE ( 'NONE', *, *, #19134, .F. ) ;
#14626 = CARTESIAN_POINT ( 'NONE',  ( 9.447682302133417309, 5.285671839984114939, 7.027659275301406439 ) ) ;
#14627 = CARTESIAN_POINT ( 'NONE',  ( 8.032370559622998840, -3.524751762020000179, 5.573845465339999805 ) ) ;
#14628 = CARTESIAN_POINT ( 'NONE',  ( 1.700000000000000178, 1.500000000000000000, 0.000000000000000000 ) ) ;
#14629 = EDGE_LOOP ( 'NONE', ( #41244, #13181, #40432, #63949 ) ) ;
#14630 = CARTESIAN_POINT ( 'NONE',  ( 12.70218814580029232, -3.116819717849789839, -12.28621950321772616 ) ) ;
#14631 = EDGE_CURVE ( 'NONE', #69130, #12504, #2253, .T. ) ;
#14632 = CARTESIAN_POINT ( 'NONE',  ( 10.25149413291699929, 5.037815157227999663, 7.973529073237199505 ) ) ;
#14633 = CARTESIAN_POINT ( 'NONE',  ( 10.22094314679000071, -2.563075248996000255, -8.004105227364998854 ) ) ;
#14634 = CARTESIAN_POINT ( 'NONE',  ( 6.897224497904996809, 9.172783816707005045, -5.180261716721994425 ) ) ;
#14635 = CARTESIAN_POINT ( 'NONE',  ( 17.86531638133300248, -3.412592442238999713, -11.89775222658999887 ) ) ;
#14636 = CARTESIAN_POINT ( 'NONE',  ( 24.54688887196200042, -8.860350057919001543, 9.344992028423000363 ) ) ;
#14637 = CARTESIAN_POINT ( 'NONE',  ( 12.31340688242393355, -2.113974262928781656, -13.74774419251637880 ) ) ;
#14638 = CARTESIAN_POINT ( 'NONE',  ( 10.40749413291699987, -3.211956830789300277, -7.140435631538599281 ) ) ;
#14639 = CARTESIAN_POINT ( 'NONE',  ( 10.32118582084299874, -4.836160649475099937, -6.533484739457099622 ) ) ;
#14640 = CONICAL_SURFACE ( 'NONE', #53710, 1.449999999965999375, 0.7853981633972997312 ) ;
#14641 = CARTESIAN_POINT ( 'NONE',  ( 11.59999999999999964, -4.000000000000000000, -7.500000000000000000 ) ) ;
#14642 = VERTEX_POINT ( 'NONE', #8868 ) ;
#14643 = B_SPLINE_CURVE_WITH_KNOTS ( 'NONE', 3,
 ( #56325, #8429, #39554, #34665 ),
 .UNSPECIFIED., .F., .F.,
 ( 4, 4 ),
 ( 0.000000000000000000, 1.000000000000000000 ),
 .UNSPECIFIED. ) ;
#14644 = VERTEX_POINT ( 'NONE', #50484 ) ;
#14645 = CARTESIAN_POINT ( 'NONE',  ( 12.80505043854144276, 0.7302158263239216796, -13.98094363220830871 ) ) ;
#14646 = DIRECTION ( 'NONE',  ( 0.000000000000000000, -0.2461538461538895772, 0.9692307692307582379 ) ) ;
#14647 = CARTESIAN_POINT ( 'NONE',  ( 10.90000000000000036, -1.315736040608999957, -10.71955403322999878 ) ) ;
#14648 = CARTESIAN_POINT ( 'NONE',  ( 10.05525296965999971, 5.223856410664000194, -6.898317050646999959 ) ) ;
#14649 = DIRECTION ( 'NONE',  ( -1.000000000000000000, 0.000000000000000000, 0.000000000000000000 ) ) ;
#14650 = CARTESIAN_POINT ( 'NONE',  ( 18.17997390458972262, 2.522451123844924759, 12.44632513475228208 ) ) ;
#14651 = CARTESIAN_POINT ( 'NONE',  ( 17.79408754209099897, 3.298114924730999764, -11.83441383768999877 ) ) ;
#14652 = B_SPLINE_CURVE_WITH_KNOTS ( 'NONE', 3,
 ( #22957, #23999, #39053, #34511 ),
 .UNSPECIFIED., .F., .F.,
 ( 4, 4 ),
 ( 0.000000000000000000, 1.000000000000000000 ),
 .UNSPECIFIED. ) ;
#14653 = CARTESIAN_POINT ( 'NONE',  ( 10.93227693248999977, 2.539877577705000000, 6.453611809651000009 ) ) ;
#14654 = VECTOR ( 'NONE', #7428, 1000.000000000000000 ) ;
#14655 = CARTESIAN_POINT ( 'NONE',  ( 11.41544519387737289, -3.267573604823260869, -7.017892448335746103 ) ) ;
#14656 = ORIENTED_EDGE ( 'NONE', *, *, #57050, .F. ) ;
#14657 = CARTESIAN_POINT ( 'NONE',  ( 12.39106450428433703, -2.968342857027795656, 12.33004038639663413 ) ) ;
#14658 = CARTESIAN_POINT ( 'NONE',  ( 23.61748067083564351, -10.10092716189297235, -9.643545208109760125 ) ) ;
#14659 = CARTESIAN_POINT ( 'NONE',  ( 10.98286939055999945, 3.998514186275999638, 9.091062412789998604 ) ) ;
#14660 = CARTESIAN_POINT ( 'NONE',  ( 11.18035971519489813, -3.321859513918399731, 8.628134814664999652 ) ) ;
#14661 = CARTESIAN_POINT ( 'NONE',  ( 9.915635841230999503, 3.210851187372000037, -6.346613542714999667 ) ) ;
#14662 = CARTESIAN_POINT ( 'NONE',  ( 11.12483609420999997, 7.237683487921999337, -6.298805210297000912 ) ) ;
#14663 = CARTESIAN_POINT ( 'NONE',  ( 25.19966511448500057, 8.371114574844000344, 8.687417344736999780 ) ) ;
#14664 = CARTESIAN_POINT ( 'NONE',  ( 12.49249186488743035, 0.5416145769730058568, 12.68445494689096087 ) ) ;
#14665 = EDGE_CURVE ( 'NONE', #7917, #28326, #57101, .T. ) ;
#14666 = EDGE_CURVE ( 'NONE', #68105, #33345, #61335, .T. ) ;
#14667 = CARTESIAN_POINT ( 'NONE',  ( 6.999999691988000095, -12.36734761319999798, -2.759114534468000368 ) ) ;
#14668 = B_SPLINE_CURVE_WITH_KNOTS ( 'NONE', 3,
 ( #49353, #16505, #37833, #33290 ),
 .UNSPECIFIED., .F., .F.,
 ( 4, 4 ),
 ( 0.000000000000000000, 1.000000000000000000 ),
 .UNSPECIFIED. ) ;
#14669 = CARTESIAN_POINT ( 'NONE',  ( 10.46932803217000085, 4.988495740890000363, 6.213106455073000411 ) ) ;
#14670 = DIRECTION ( 'NONE',  ( 0.000000000000000000, 0.000000000000000000, -1.000000000000000000 ) ) ;
#14671 = ORIENTED_EDGE ( 'NONE', *, *, #53652, .T. ) ;
#14672 = CARTESIAN_POINT ( 'NONE',  ( 9.626145280412998773, 3.934138271021000222, -9.063586117809000697 ) ) ;
#14673 = CARTESIAN_POINT ( 'NONE',  ( 10.05041772631199848, 4.549624259497900169, -8.631352948887998977 ) ) ;
#14674 = CARTESIAN_POINT ( 'NONE',  ( 24.53429010005800137, -12.47024913742999885, 3.026245653581999928 ) ) ;
#14675 = CARTESIAN_POINT ( 'NONE',  ( 10.19809687351566474, 4.327184855449106138, 8.717465845835393523 ) ) ;
#14676 = CARTESIAN_POINT ( 'NONE',  ( 10.72510394928502286, 2.650147065043140238, 7.500007457243191844 ) ) ;
#14677 = CARTESIAN_POINT ( 'NONE',  ( 10.92026088462129962, -3.997864853650589634, -6.496532863517000322 ) ) ;
#14678 = ORIENTED_EDGE ( 'NONE', *, *, #5842, .T. ) ;
#14679 = CARTESIAN_POINT ( 'NONE',  ( 1.109972661243999958, -2.155162080922000012, 2.873869168568000010 ) ) ;
#14680 = CARTESIAN_POINT ( 'NONE',  ( 18.18005043824376443, -1.329523415562850021E-10, -12.70000000088146486 ) ) ;
#14682 = CARTESIAN_POINT ( 'NONE',  ( 11.44792571093000255, 3.801678398496999733, -11.87711516161999903 ) ) ;
#14681 = CARTESIAN_POINT ( 'NONE',  ( 9.717214158771000143, 3.990126737362999609, -8.809457313313998839 ) ) ;
#14683 = DIRECTION ( 'NONE',  ( 0.000000000000000000, 1.000000000000000000, 0.000000000000000000 ) ) ;
#14684 = CARTESIAN_POINT ( 'NONE',  ( 8.849999778957998942, 4.000000000000000000, 7.500000000000000000 ) ) ;
#14685 = CARTESIAN_POINT ( 'NONE',  ( 17.96899650538952997, -2.968713945236787666, -13.56275387600713067 ) ) ;
#14686 = CARTESIAN_POINT ( 'NONE',  ( 11.46595122972049907, 4.343798595649099425, 8.295047870239098842 ) ) ;
#14687 = DIRECTION ( 'NONE',  ( 0.000000000000000000, -0.8648648648648717963, 0.5020047465136829867 ) ) ;
#14688 = CARTESIAN_POINT ( 'NONE',  ( 8.014941940377999785, -2.280579276705999803, 6.510290672242000198 ) ) ;
#14689 = ORIENTED_EDGE ( 'NONE', *, *, #32281, .T. ) ;
#14690 = CARTESIAN_POINT ( 'NONE',  ( 7.374100552923999352, 4.389299166881000858, 9.135259451319999613 ) ) ;
#14691 = EDGE_CURVE ( 'NONE', #7034, #32067, #23139, .T. ) ;
#14693 = CARTESIAN_POINT ( 'NONE',  ( 11.12916632831999841, 5.271622498040000160, 4.814907817406999690 ) ) ;
#14692 = CARTESIAN_POINT ( 'NONE',  ( 5.246262210455999941, -0.9612325616298000863, -1.110208802542000051 ) ) ;
#14694 = CARTESIAN_POINT ( 'NONE',  ( 7.637790262712637279, -5.247290350387737945, 6.287244541376254325 ) ) ;
#14695 = CARTESIAN_POINT ( 'NONE',  ( 7.932045726517200634, -5.134137217805110787, 6.756605349134713556 ) ) ;
#14696 = CARTESIAN_POINT ( 'NONE',  ( 0.7530474580061000678, 2.610614231003999919, -1.727479700733000056 ) ) ;
#14697 = ORIENTED_EDGE ( 'NONE', *, *, #40108, .T. ) ;
#14698 = CARTESIAN_POINT ( 'NONE',  ( 2.204555053273437704, 1.932598637109171014, -2.448717497070831417 ) ) ;
#14699 = EDGE_CURVE ( 'NONE', #55522, #8893, #34763, .T. ) ;
#14700 = CARTESIAN_POINT ( 'NONE',  ( 11.86333594839950045, -3.340240242524600056, 8.256087240512899328 ) ) ;
#14701 = CARTESIAN_POINT ( 'NONE',  ( 10.27815081430999911, 5.521603098753999461, 8.751228458888000716 ) ) ;
#14702 = CARTESIAN_POINT ( 'NONE',  ( 11.18706938844999854, 3.186790175674999670, 6.232702730851999995 ) ) ;
#14703 = CARTESIAN_POINT ( 'NONE',  ( 11.08841369783139896, 3.942447888101379583, 6.360711682373000109 ) ) ;
#14704 = CIRCLE ( 'NONE', #59300, 11.79499999999999993 ) ;
#14705 = DIRECTION ( 'NONE',  ( 6.943145065999975329E-10, 0.7071067809470975574, -0.7071067814259974771 ) ) ;
#14706 = CARTESIAN_POINT ( 'NONE',  ( 18.22497476944389661, 3.457026130725855850, -12.03849088744170004 ) ) ;
#14707 = CARTESIAN_POINT ( 'NONE',  ( 10.98358762163081259, -5.203662202021275718, 6.699115767914069153 ) ) ;
#14708 = CARTESIAN_POINT ( 'NONE',  ( 24.69847986554200148, -3.637895343793999814, -12.18598392984999990 ) ) ;
#14709 = CARTESIAN_POINT ( 'NONE',  ( 17.97988082628308959, -1.926206752467417127, 13.86685907515736638 ) ) ;
#14710 = CARTESIAN_POINT ( 'NONE',  ( 23.60001133530950668, -1.983597864821140026E-14, -13.89477126879791058 ) ) ;
#14711 = EDGE_LOOP ( 'NONE', ( #60294, #50037, #44579, #59836 ) ) ;
#14712 = CARTESIAN_POINT ( 'NONE',  ( 8.647350449577999143, -5.160012848592001156, -6.809278868592000933 ) ) ;
#14713 = CARTESIAN_POINT ( 'NONE',  ( 10.63706886433642573, -2.899999999999999911, 6.444141223494331605 ) ) ;
#14714 = VERTEX_POINT ( 'NONE', #62009 ) ;
#14715 = DIRECTION ( 'NONE',  ( 1.000000000000000000, 0.000000000000000000, 0.000000000000000000 ) ) ;
#14716 = EDGE_CURVE ( 'NONE', #60364, #44668, #45491, .T. ) ;
#14717 = CARTESIAN_POINT ( 'NONE',  ( 10.82595391537419971, 4.716560378569699452, 7.013338090450799811 ) ) ;
#14718 = AXIS2_PLACEMENT_3D ( 'NONE', #49887, #8613, #28571 ) ;
#14719 = CARTESIAN_POINT ( 'NONE',  ( 9.939321360490000146, 2.638097915594000309, 6.328629954376999933 ) ) ;
#14720 = CARTESIAN_POINT ( 'NONE',  ( 10.65649893244999902, 5.448184228579000532, -7.015214795518000201 ) ) ;
#14721 = CARTESIAN_POINT ( 'NONE',  ( 10.21473687196862734, -4.313773474582136558, -8.316748708918906274 ) ) ;
#14722 = CARTESIAN_POINT ( 'NONE',  ( 10.79499900793999956, -3.503951165873000040, 6.168577387731000172 ) ) ;
#14723 = CARTESIAN_POINT ( 'NONE',  ( 18.24522866045827740, 0.2205548374446872906, -12.59807454672508165 ) ) ;
#14724 = CARTESIAN_POINT ( 'NONE',  ( 5.700000001242999659, 1.249999998757000075, -1.883720587326999896E-09 ) ) ;
#14725 = CARTESIAN_POINT ( 'NONE',  ( 10.30903300763299946, -3.402282662142699809, -8.126922218169600143 ) ) ;
#14726 = CARTESIAN_POINT ( 'NONE',  ( 12.80505043854146940, -1.798896937388929640, 12.50938852236267529 ) ) ;
#14727 = EDGE_LOOP ( 'NONE', ( #23666, #16891, #57922, #43953, #6796, #34502 ) ) ;
#14728 = B_SPLINE_CURVE_WITH_KNOTS ( 'NONE', 3,
 ( #52804, #4897, #57345, #25887, #10489, #26236, #40936, #41622 ),
 .UNSPECIFIED., .F., .F.,
 ( 4, 2, 2, 4 ),
 ( 0.000000000000000000, 0.5000000000000026645, 0.7500000000000013323, 1.000000000000000000 ),
 .UNSPECIFIED. ) ;
#14729 = CARTESIAN_POINT ( 'NONE',  ( 11.07127482541000063, -6.556071284744000138, -5.494407061017000160 ) ) ;
#14730 = CARTESIAN_POINT ( 'NONE',  ( 11.83570505509991833, -3.091015088729731186, 7.824998694764690121 ) ) ;
#14731 = CARTESIAN_POINT ( 'NONE',  ( 3.999999855301999752, -2.524999655449999825, 0.000000000000000000 ) ) ;
#14732 = CARTESIAN_POINT ( 'NONE',  ( 10.16476354018241501, -2.782534154164604256, -7.172815144550905408 ) ) ;
#14733 = CARTESIAN_POINT ( 'NONE',  ( 17.81303847540707963, 1.807878129530184896, 12.46962684194071791 ) ) ;
#14734 = CARTESIAN_POINT ( 'NONE',  ( 12.11816748453748538, 2.752694035764603253, 13.72673318081622895 ) ) ;
#14735 = CARTESIAN_POINT ( 'NONE',  ( 10.90000000000000036, 2.899999999999999911, 6.414037451299000381 ) ) ;
#14736 = ORIENTED_EDGE ( 'NONE', *, *, #54577, .T. ) ;
#14737 = CARTESIAN_POINT ( 'NONE',  ( 12.18105077442090334, -0.04081512033874237777, -12.69993297814843558 ) ) ;
#14738 = FACE_OUTER_BOUND ( 'NONE', #52187, .T. ) ;
#14739 = ORIENTED_EDGE ( 'NONE', *, *, #31098, .T. ) ;
#14740 = CARTESIAN_POINT ( 'NONE',  ( 12.48133867187399915, -1.836397482308033346, 12.46545911376216687 ) ) ;
#14741 = CARTESIAN_POINT ( 'NONE',  ( 11.79999999471800010, 11.69117318561000118, 1.923227876431999883 ) ) ;
#14742 = CARTESIAN_POINT ( 'NONE',  ( 16.08259915475489521, 9.118254932978883787, 8.587227412616197597 ) ) ;
#14743 = CARTESIAN_POINT ( 'NONE',  ( 12.11364291764652990, -4.859654669415900408, 7.606265891492399511 ) ) ;
#14744 = AXIS2_PLACEMENT_3D ( 'NONE', #50992, #13939, #28999 ) ;
#14745 = CARTESIAN_POINT ( 'NONE',  ( 20.75138802851920161, 0.000000000000000000, 0.000000000000000000 ) ) ;
#14746 = ADVANCED_FACE ( 'NONE', ( #56772 ), #25290, .F. ) ;
#14747 = EDGE_CURVE ( 'NONE', #67420, #44775, #51292, .T. ) ;
#14748 = DIRECTION ( 'NONE',  ( 0.000000000000000000, 0.9659258262890756397, -0.2588190451024932059 ) ) ;
#14749 = CARTESIAN_POINT ( 'NONE',  ( 11.32299956498189886, 2.792989229543000107, -7.174999999999999822 ) ) ;
#14750 = CARTESIAN_POINT ( 'NONE',  ( 12.08198123077151287, 2.425144973324804276, 12.36441727636090704 ) ) ;
#14751 = CARTESIAN_POINT ( 'NONE',  ( 9.839913318575998602, -5.792391408692000532, -6.955579396894000510 ) ) ;
#14752 = EDGE_CURVE ( 'NONE', #8013, #33506, #63788, .T. ) ;
#14753 = CARTESIAN_POINT ( 'NONE',  ( 11.33872066707849768, 4.858611803369300652, -6.980638253271099103 ) ) ;
#14754 = CARTESIAN_POINT ( 'NONE',  ( 24.30000000000000071, 0.000000000000000000, 0.000000000000000000 ) ) ;
#14755 = CARTESIAN_POINT ( 'NONE',  ( 11.24323278040999874, 2.479734175328000223, -7.587230544849999703 ) ) ;
#14756 = CARTESIAN_POINT ( 'NONE',  ( 9.630633995698000049, 5.271405458160000279, -7.641111829547599932 ) ) ;
#14758 = CYLINDRICAL_SURFACE ( 'NONE', #55210, 0.5000000000000004441 ) ;
#14757 = CARTESIAN_POINT ( 'NONE',  ( 10.17500046684965120, 2.650307855385062972, 7.500001770945063484 ) ) ;
#14759 = CARTESIAN_POINT ( 'NONE',  ( 10.33253786428999987, -2.899999999999999911, 6.571291218949999902 ) ) ;
#14760 = EDGE_LOOP ( 'NONE', ( #6475, #47201, #61149, #54519 ) ) ;
#14761 = AXIS2_PLACEMENT_3D ( 'NONE', #57721, #68900, #58411 ) ;
#14762 = CARTESIAN_POINT ( 'NONE',  ( 12.39790242569448075, -0.4743817213088754592, 12.68807659218376571 ) ) ;
#14763 = LINE ( 'NONE', #7794, #4298 ) ;
#14764 = VECTOR ( 'NONE', #199, 1000.000000000000114 ) ;
#14765 = CARTESIAN_POINT ( 'NONE',  ( 9.579111560609650411, 2.241182798226359463, -7.748722518521907965 ) ) ;
#14766 = CARTESIAN_POINT ( 'NONE',  ( 9.653000818238998804, 3.232852935619000334, 7.096028062709999418 ) ) ;
#14767 = CARTESIAN_POINT ( 'NONE',  ( 8.846962924124625260, 4.841836872161519700, -7.738417548727159812 ) ) ;
#14768 = FACE_BOUND ( 'NONE', #2294, .T. ) ;
#14769 = CARTESIAN_POINT ( 'NONE',  ( 12.55463174185022091, -3.072731264995193001, 13.53516186994627013 ) ) ;
#14770 = CARTESIAN_POINT ( 'NONE',  ( 12.24260983038582395, 2.772891244655266263, 13.61173698548887501 ) ) ;
#14771 = CARTESIAN_POINT ( 'NONE',  ( 23.61276350013500291, 3.132797279252000244, -13.53855344537999983 ) ) ;
#14772 = ORIENTED_EDGE ( 'NONE', *, *, #30234, .T. ) ;
#14773 = CARTESIAN_POINT ( 'NONE',  ( 4.455902236433000319, 0.09694544799576999827, -1.130268743893000138 ) ) ;
#14774 = CARTESIAN_POINT ( 'NONE',  ( 9.655963142879999239, -2.748296264808000267, -7.236139910592400248 ) ) ;
#14775 = CARTESIAN_POINT ( 'NONE',  ( 10.61815932168150312, -5.019094019303483201, -5.036897186739046184 ) ) ;
#14776 = CARTESIAN_POINT ( 'NONE',  ( 12.09603632436369125, -4.842640371965599932, 7.696781148700499564 ) ) ;
#14777 = CARTESIAN_POINT ( 'NONE',  ( 18.27458182272986775, 2.390008000232564545, -12.37125705564431577 ) ) ;
#14778 = CARTESIAN_POINT ( 'NONE',  ( 8.894507664004006386, -3.102842363045003271, -6.153768356943001727 ) ) ;
#14779 = CARTESIAN_POINT ( 'NONE',  ( 18.11161644830704986, 2.784507902010840308, 12.38071508488312844 ) ) ;
#14780 = CARTESIAN_POINT ( 'NONE',  ( 5.699999545467999695, -12.03770622561999915, 3.722046322334000124 ) ) ;
#14781 = CARTESIAN_POINT ( 'NONE',  ( 9.575903104272999400, -2.330665094450000030, -8.349943402163999551 ) ) ;
#14782 = CARTESIAN_POINT ( 'NONE',  ( 10.91060805961999947, -4.702347118766000200, -9.210032991522000501 ) ) ;
#14783 = CARTESIAN_POINT ( 'NONE',  ( 9.558834163536323203, -4.704973616088924615, 8.704082162066264061 ) ) ;
#14784 = CARTESIAN_POINT ( 'NONE',  ( 12.44248702983404442, 0.6327954766588935742, -13.98569611075749464 ) ) ;
#14785 = CARTESIAN_POINT ( 'NONE',  ( 13.46376629110800138, -9.221173139870998625, -7.505113150216000228 ) ) ;
#14786 = CARTESIAN_POINT ( 'NONE',  ( 21.10000033274619824, -12.52499966719000035, -3.709625656131999791E-10 ) ) ;
#14787 = CARTESIAN_POINT ( 'NONE',  ( 18.14123990138214992, 2.282196115480399801, 12.49965818828386155 ) ) ;
#14788 = CARTESIAN_POINT ( 'NONE',  ( 8.903895280414001689, 3.867331042029999999, -9.227339949050001877 ) ) ;
#14789 = DIRECTION ( 'NONE',  ( -1.000000000000000000, 0.000000000000000000, 0.000000000000000000 ) ) ;
#14790 = VERTEX_POINT ( 'NONE', #13776 ) ;
#14791 = CONICAL_SURFACE ( 'NONE', #13705, 2.649999808707999893, 0.7853980705567794596 ) ;
#14792 = CARTESIAN_POINT ( 'NONE',  ( 8.424688440789097399, -5.350083765069893360, 7.500019236172019710 ) ) ;
#14793 = CARTESIAN_POINT ( 'NONE',  ( 18.07784313215196903, 3.023931901684152823, -13.66952493495815801 ) ) ;
#14794 = ORIENTED_EDGE ( 'NONE', *, *, #31061, .F. ) ;
#14795 = CARTESIAN_POINT ( 'NONE',  ( 10.23798825978600036, -4.113440707072600233, 6.640442468193600511 ) ) ;
#14796 = CARTESIAN_POINT ( 'NONE',  ( 11.76077869730539938, 3.404661623424200201, 8.673950353177000139 ) ) ;
#14797 = EDGE_CURVE ( 'NONE', #62021, #12694, #7084, .T. ) ;
#14798 = CARTESIAN_POINT ( 'NONE',  ( 17.98087424866222506, 3.330341796646840713, -11.16384340189072333 ) ) ;
#14799 = CARTESIAN_POINT ( 'NONE',  ( 12.80505043854146940, -3.125000000000000000, -25.00000000000000000 ) ) ;
#14800 = CARTESIAN_POINT ( 'NONE',  ( 11.22567835872029995, -4.993948309075300074, -6.873560442659099046 ) ) ;
#14801 = CARTESIAN_POINT ( 'NONE',  ( 8.928197172114701985, 5.125396288430382086, 6.749639981089713636 ) ) ;
#14802 = EDGE_CURVE ( 'NONE', #47324, #37325, #37858, .T. ) ;
#14803 = CARTESIAN_POINT ( 'NONE',  ( 8.929547492598356229, -3.266100554355691354, -8.304419251562590532 ) ) ;
#14804 = EDGE_LOOP ( 'NONE', ( #8722, #22956, #68350, #41810, #47489 ) ) ;
#14805 = DIRECTION ( 'NONE',  ( 0.000000000000000000, -1.000000000000000000, 0.000000000000000000 ) ) ;
#14806 = CARTESIAN_POINT ( 'NONE',  ( 8.458179719589999479, 5.332332124071999857, -8.487089944253000340 ) ) ;
#14807 = ORIENTED_EDGE ( 'NONE', *, *, #34831, .T. ) ;
#14808 = CIRCLE ( 'NONE', #56124, 9.250000000000000000 ) ;
#14809 = CARTESIAN_POINT ( 'NONE',  ( 10.86493304757000011, 4.678466548873998931, -9.048467117372998914 ) ) ;
#14810 = VERTEX_POINT ( 'NONE', #3611 ) ;
#14811 = CARTESIAN_POINT ( 'NONE',  ( 9.352013376692999813, 2.859607053196999704, 8.079558723821699928 ) ) ;
#14812 = CARTESIAN_POINT ( 'NONE',  ( 17.92180752009631561, -1.993817408553323789, -12.55519104945816622 ) ) ;
#14813 = CARTESIAN_POINT ( 'NONE',  ( 25.60000000000000142, 2.258942858049999725, 12.29419282279000036 ) ) ;
#14814 = CARTESIAN_POINT ( 'NONE',  ( 24.35146665670700017, -12.30647607894000117, -3.205652257177999953 ) ) ;
#14815 = CARTESIAN_POINT ( 'NONE',  ( 8.567745549749458789, 3.352117218477321359, 5.929420214889738361 ) ) ;
#14816 = ORIENTED_EDGE ( 'NONE', *, *, #45922, .T. ) ;
#14817 = CARTESIAN_POINT ( 'NONE',  ( 10.16052890781999984, 2.899999999999999911, -6.152188490330000370 ) ) ;
#14818 = CARTESIAN_POINT ( 'NONE',  ( 10.76588584123000025, 3.166544027818999574, -8.574484964885998650 ) ) ;
#14819 = CARTESIAN_POINT ( 'NONE',  ( 8.154130060498479438, -2.684642961096272096, 7.853228170896902505 ) ) ;
#14820 = FACE_OUTER_BOUND ( 'NONE', #19568, .T. ) ;
#14821 = B_SPLINE_CURVE_WITH_KNOTS ( 'NONE', 3,
 ( #25745, #42515, #53349, #31684 ),
 .UNSPECIFIED., .F., .F.,
 ( 4, 4 ),
 ( 0.000000000000000000, 1.000000000000000000 ),
 .UNSPECIFIED. ) ;
#14822 = CARTESIAN_POINT ( 'NONE',  ( 18.14440149583522199, 0.4259565731506576580, 13.99353270933017335 ) ) ;
#14823 = CARTESIAN_POINT ( 'NONE',  ( 17.88018231457700224, 3.314507696643999690, 11.22393832560999982 ) ) ;
#14824 = CARTESIAN_POINT ( 'NONE',  ( 11.02205565301999890, -2.309485172892000282, -7.515673712097999726 ) ) ;
#14825 = EDGE_CURVE ( 'NONE', #65344, #42751, #58139, .T. ) ;
#14826 = VERTEX_POINT ( 'NONE', #36820 ) ;
#14827 = ORIENTED_EDGE ( 'NONE', *, *, #12560, .F. ) ;
#14828 = CARTESIAN_POINT ( 'NONE',  ( 8.581920280410001212, 4.769017407621999993, -8.862909124839001507 ) ) ;
#14829 = FACE_OUTER_BOUND ( 'NONE', #8119, .T. ) ;
#14830 = EDGE_CURVE ( 'NONE', #66075, #4878, #9496, .T. ) ;
#14831 = ADVANCED_FACE ( 'NONE', ( #36465 ), #6761, .F. ) ;
#14832 = CARTESIAN_POINT ( 'NONE',  ( 1.196806799207750238, -0.9161175952574931447, 3.408904368339101598 ) ) ;
#14833 = CARTESIAN_POINT ( 'NONE',  ( 23.84129534145970553, 3.319672314572660987, 13.04905549722290381 ) ) ;
#14834 = CARTESIAN_POINT ( 'NONE',  ( 23.74313043943600121, 9.836954956339999612, -9.383370562020999728 ) ) ;
#14835 = CARTESIAN_POINT ( 'NONE',  ( 9.712659112603999390, 3.623260508844300176, -8.280881105104999307 ) ) ;
#14837 = CARTESIAN_POINT ( 'NONE',  ( 3.400000000000000355, 0.000000000000000000, 0.000000000000000000 ) ) ;
#14836 = CARTESIAN_POINT ( 'NONE',  ( 10.35764655415099966, -3.513729974241599940, 6.621146336197599958 ) ) ;
#14838 = CARTESIAN_POINT ( 'NONE',  ( 8.205380712518003605, -3.106081630192000009, 6.107045428706002532 ) ) ;
#14839 = ORIENTED_EDGE ( 'NONE', *, *, #31021, .F. ) ;
#14840 = CARTESIAN_POINT ( 'NONE',  ( 9.758513540182331525, 4.163624617374472869, -6.250000000000000888 ) ) ;
#14841 = CARTESIAN_POINT ( 'NONE',  ( 10.37169758536000153, -3.424645824523000037, -5.010422874381999847 ) ) ;
#14842 = CARTESIAN_POINT ( 'NONE',  ( 9.580894592352999339, -5.371875912611999482, -7.370590366721999409 ) ) ;
#14843 = CARTESIAN_POINT ( 'NONE',  ( 11.79999999771000141, -12.39026187696000036, -1.832249219479999969 ) ) ;
#14844 = DIRECTION ( 'NONE',  ( 0.000000000000000000, -0.7071067811865475727, 0.7071067811865475727 ) ) ;
#14845 = CARTESIAN_POINT ( 'NONE',  ( 10.99827931143999926, -5.289657308675000280, -4.962166337294999785 ) ) ;
#14846 = DIRECTION ( 'NONE',  ( 0.000000000000000000, -1.000000000000000000, 0.000000000000000000 ) ) ;
#14847 = ADVANCED_FACE ( 'NONE', ( #41715 ), #4301, .F. ) ;
#14848 = CARTESIAN_POINT ( 'NONE',  ( 5.000000001445999764, 1.799999998554000058, -4.283815592157999860E-09 ) ) ;
#14849 = CARTESIAN_POINT ( 'NONE',  ( 7.935252636294002571, -4.895109672515001620, 6.296391117214003685 ) ) ;
#14850 = VECTOR ( 'NONE', #56581, 1000.000000000000000 ) ;
#14851 = CARTESIAN_POINT ( 'NONE',  ( 11.14393020684970104, -2.750000000000000000, 7.500000000000000000 ) ) ;
#14852 = CARTESIAN_POINT ( 'NONE',  ( 0.1889203238210994673, 2.786086813067528034, -1.606789352532954629 ) ) ;
#14853 = CYLINDRICAL_SURFACE ( 'NONE', #1586, 1.000000000000001332 ) ;
#14854 = CARTESIAN_POINT ( 'NONE',  ( 2.538064026817000052, -3.226256590673000080, 0.4610373736932000255 ) ) ;
#14855 = VERTEX_POINT ( 'NONE', #16765 ) ;
#14856 = CARTESIAN_POINT ( 'NONE',  ( 12.33502333850778676, -0.4124490627810476484, -12.69099791225217366 ) ) ;
#14857 = CARTESIAN_POINT ( 'NONE',  ( 12.20626853909968546, -2.679149498323847300, -12.40801937966050161 ) ) ;
#14858 = DIRECTION ( 'NONE',  ( 0.000000000000000000, 0.8648648648648717963, 0.5020047465136829867 ) ) ;
#14859 = CARTESIAN_POINT ( 'NONE',  ( 6.899999692186000289, 12.99045401582999837, -1.690592930688000095 ) ) ;
#14860 = CARTESIAN_POINT ( 'NONE',  ( 10.35465597998896214, 2.649863840852023422, -7.676734101936348864 ) ) ;
#14861 = VERTEX_POINT ( 'NONE', #1052 ) ;
#14862 = DIRECTION ( 'NONE',  ( 1.000000000000000000, 1.776356839496000193E-14, -1.776356839496000193E-14 ) ) ;
#14863 = CARTESIAN_POINT ( 'NONE',  ( 0.7094218594409307244, -3.054526701543303524, 1.768616831485774865 ) ) ;
#14864 = CARTESIAN_POINT ( 'NONE',  ( 10.36476354018324741, -5.217465845835395299, 7.172815144550902744 ) ) ;
#14865 = CARTESIAN_POINT ( 'NONE',  ( 10.27195525820100031, 3.879327850572200198, 8.772302877803999976 ) ) ;
#14866 = CARTESIAN_POINT ( 'NONE',  ( 10.56080513895999928, 5.026880838510000338, -6.929150654994399083 ) ) ;
#14867 = ORIENTED_EDGE ( 'NONE', *, *, #27224, .T. ) ;
#14868 = CARTESIAN_POINT ( 'NONE',  ( 10.92717634842000152, -5.023656093247000243, 8.718039182945998888 ) ) ;
#14869 = EDGE_LOOP ( 'NONE', ( #26643, #63699, #15990, #2305 ) ) ;
#14870 = CARTESIAN_POINT ( 'NONE',  ( 11.96550210169813688, -4.058074521742473628, 6.192987292895718809 ) ) ;
#14871 = CARTESIAN_POINT ( 'NONE',  ( 7.352706853207999771, -4.773080213113000347, 8.927399220053999329 ) ) ;
#14872 = EDGE_CURVE ( 'NONE', #35486, #13916, #41003, .T. ) ;
#14873 = CARTESIAN_POINT ( 'NONE',  ( 15.76715644869600119, 8.722854347492999594, 8.080426068599999567 ) ) ;
#14874 = EDGE_LOOP ( 'NONE', ( #27464, #57537, #68746, #57737, #20496, #23779 ) ) ;
#14875 = CARTESIAN_POINT ( 'NONE',  ( 25.29986734212600297, -2.258942858049999725, 11.29419282279013004 ) ) ;
#14876 = CARTESIAN_POINT ( 'NONE',  ( 8.020125753392001400, 4.498951069075999953, -6.245588651729999441 ) ) ;
#14877 = CARTESIAN_POINT ( 'NONE',  ( 8.277804719590999838, 4.529523339102000890, -8.867457431226998921 ) ) ;
#14878 = ADVANCED_FACE ( 'NONE', ( #20387 ), #38096, .F. ) ;
#14879 = DIRECTION ( 'NONE',  ( 1.000000000000000000, 0.000000000000000000, 0.000000000000000000 ) ) ;
#14880 = CARTESIAN_POINT ( 'NONE',  ( 12.80000000000000071, 50.14170351282000127, -17.06962823869000090 ) ) ;
#14881 = EDGE_LOOP ( 'NONE', ( #48197, #8170, #4106, #1723, #9826 ) ) ;
#14882 = CARTESIAN_POINT ( 'NONE',  ( 9.905786073958001481, -2.698967003257000119, 8.979227319929000473 ) ) ;
#14883 = AXIS2_PLACEMENT_3D ( 'NONE', #38786, #40096, #56158 ) ;
#14884 = CARTESIAN_POINT ( 'NONE',  ( 12.20843209901191884, -2.686266380820965693, -13.63213492619998135 ) ) ;
#14885 = CARTESIAN_POINT ( 'NONE',  ( 11.09999999999999964, 4.000000000000000000, 7.500000000000000000 ) ) ;
#14886 = EDGE_LOOP ( 'NONE', ( #527, #21062, #55765, #161, #31287, #16843, #5784, #18521, #16076, #54341, #54404 ) ) ;
#14887 = CARTESIAN_POINT ( 'NONE',  ( 9.937415816209998809, -3.510658118802999716, -6.227041669085999764 ) ) ;
#14888 = AXIS2_PLACEMENT_3D ( 'NONE', #17056, #12174, #11466 ) ;
#14889 = CARTESIAN_POINT ( 'NONE',  ( 10.90000000016000037, -5.167567554889999748, 6.822293570050000255 ) ) ;
#14890 = ORIENTED_EDGE ( 'NONE', *, *, #67603, .T. ) ;
#14891 = CARTESIAN_POINT ( 'NONE',  ( 11.79999999771000141, 12.39026187696000036, 1.832249219479999969 ) ) ;
#14892 = CARTESIAN_POINT ( 'NONE',  ( 23.84018977933850891, 12.96271613198936734, -3.649568246013530803 ) ) ;
#14893 = CARTESIAN_POINT ( 'NONE',  ( 7.100000000000000533, 0.000000000000000000, 0.000000000000000000 ) ) ;
#14894 = CARTESIAN_POINT ( 'NONE',  ( 8.737804660583998739, 4.491756428607999396, -5.831236541471000123 ) ) ;
#14895 = FACE_OUTER_BOUND ( 'NONE', #65505, .T. ) ;
#14896 = CARTESIAN_POINT ( 'NONE',  ( 7.936333720142999759, -5.123034382927999175, 6.721303993095999907 ) ) ;
#14897 = CARTESIAN_POINT ( 'NONE',  ( 12.32706758141025993, 2.902815230603663199, 13.57967619870183640 ) ) ;
#14898 = CARTESIAN_POINT ( 'NONE',  ( 21.60000000000000142, 12.52500000000000036, 0.000000000000000000 ) ) ;
#14899 = EDGE_LOOP ( 'NONE', ( #6304, #60484, #52994, #42147, #60597 ) ) ;
#14900 = CARTESIAN_POINT ( 'NONE',  ( 10.98656920625009903, -3.967932847735990531, -6.608450613814399688 ) ) ;
#14901 = ORIENTED_EDGE ( 'NONE', *, *, #3138, .T. ) ;
#14902 = CARTESIAN_POINT ( 'NONE',  ( 11.01776904286000125, 4.914120883409999863, 8.587704221454000475 ) ) ;
#14903 = AXIS2_PLACEMENT_3D ( 'NONE', #16759, #1383, #16077 ) ;
#14904 = DIRECTION ( 'NONE',  ( -1.000000000000000000, 0.000000000000000000, 0.000000000000000000 ) ) ;
#14905 = CARTESIAN_POINT ( 'NONE',  ( 12.33243540359735313, 2.090896859126741614, -13.75176201293517586 ) ) ;
#14906 = CARTESIAN_POINT ( 'NONE',  ( 2.558588954831999995, 3.370261330116000043, 1.546253863582000010 ) ) ;
#14907 = CARTESIAN_POINT ( 'NONE',  ( 10.15786958814999963, -4.213496663054999480, -5.822956951053000374 ) ) ;
#14908 = DIRECTION ( 'NONE',  ( -0.000000000000000000, -0.000000000000000000, 1.000000000000000000 ) ) ;
#14909 = DIRECTION ( 'NONE',  ( 0.000000000000000000, 1.000000000000000000, 0.000000000000000000 ) ) ;
#14910 = ORIENTED_EDGE ( 'NONE', *, *, #14161, .F. ) ;
#14911 = CARTESIAN_POINT ( 'NONE',  ( 11.04272335273199879, -3.555125495332600138, 6.301916924546999255 ) ) ;
#14912 = DIRECTION ( 'NONE',  ( 1.000000000000000000, 0.000000000000000000, 0.000000000000000000 ) ) ;
#14913 = ADVANCED_FACE ( 'NONE', ( #63015 ), #54177, .T. ) ;
#14914 = CARTESIAN_POINT ( 'NONE',  ( 15.39046541331000029, 9.526477069417000010, 8.190982836632000996 ) ) ;
#14915 = CARTESIAN_POINT ( 'NONE',  ( 24.32158589636341262, 9.044138011824934154, 9.474428460952893261 ) ) ;
#14917 = CARTESIAN_POINT ( 'NONE',  ( 1.700000811628999964, 0.000000000000000000, 0.000000000000000000 ) ) ;
#14916 = CARTESIAN_POINT ( 'NONE',  ( 10.87521525736000072, 4.831064930369000088, 6.312796576761000367 ) ) ;
#14918 = CARTESIAN_POINT ( 'NONE',  ( 11.65456516821461008, 4.802916961510000249, -8.310318115935698913 ) ) ;
#14919 = CARTESIAN_POINT ( 'NONE',  ( 17.55505043854147118, -3.125000000000000000, -13.52078605991414761 ) ) ;
#14920 = CARTESIAN_POINT ( 'NONE',  ( 9.197076168957998732, 3.560025096655699883, -8.247081005603298820 ) ) ;
#14921 = CARTESIAN_POINT ( 'NONE',  ( 18.02437627528317421, 0.5483668826291584475, 12.58806376549905082 ) ) ;
#14922 = CARTESIAN_POINT ( 'NONE',  ( 7.206237632408999616, 0.06715535307188000291, 1.130410956850999904 ) ) ;
#14923 = CARTESIAN_POINT ( 'NONE',  ( 11.83003632436370012, 2.756744593645999775, 7.790336465152099876 ) ) ;
#14924 = DIRECTION ( 'NONE',  ( 0.000000000000000000, -0.9466492601157001641, 0.3222656952305000266 ) ) ;
#14925 = ORIENTED_EDGE ( 'NONE', *, *, #5349, .F. ) ;
#14926 = CARTESIAN_POINT ( 'NONE',  ( 7.641206853206999661, -4.524489047957000132, 9.047757046927999980 ) ) ;
#14927 = CARTESIAN_POINT ( 'NONE',  ( 17.65063036598052548, 3.242172222319704034, 13.61940987276824622 ) ) ;
#14928 = ADVANCED_FACE ( 'NONE', ( #61500 ), #49629, .F. ) ;
#14929 = DIRECTION ( 'NONE',  ( 1.000000000000000000, 0.000000000000000000, 0.000000000000000000 ) ) ;
#14930 = EDGE_LOOP ( 'NONE', ( #46721, #49864, #9627, #33810 ) ) ;
#14931 = EDGE_CURVE ( 'NONE', #56519, #39559, #52176, .T. ) ;
#14932 = CARTESIAN_POINT ( 'NONE',  ( 17.95534550153200115, 3.277905616156999713, 11.84067279748999901 ) ) ;
#14933 = CARTESIAN_POINT ( 'NONE',  ( 10.44999293566599974, 4.720032669050099550, 6.616719557880299085 ) ) ;
#14934 = CARTESIAN_POINT ( 'NONE',  ( 10.71315778041000044, 2.619207518211999819, -8.142085279690999045 ) ) ;
#14935 = ORIENTED_EDGE ( 'NONE', *, *, #57884, .F. ) ;
#14936 = CARTESIAN_POINT ( 'NONE',  ( 17.55505043854143565, 1.875000000000000000, 13.78627172894481667 ) ) ;
#14937 = CARTESIAN_POINT ( 'NONE',  ( 24.67921321800200118, -8.727630028894999725, 9.158313644156001132 ) ) ;
#14938 = CARTESIAN_POINT ( 'NONE',  ( 11.28118179236249929, 3.732952383914999839, 8.749800764654999341 ) ) ;
#14939 = FACE_OUTER_BOUND ( 'NONE', #40026, .T. ) ;
#14940 = LINE ( 'NONE', #53722, #20050 ) ;
#14941 = ORIENTED_EDGE ( 'NONE', *, *, #55875, .T. ) ;
#14942 = CARTESIAN_POINT ( 'NONE',  ( 11.50001496184999894, 8.431319371474298663, -9.354420476537780971 ) ) ;
#14943 = CARTESIAN_POINT ( 'NONE',  ( 8.064139158768000470, 2.101036793381999779, -7.559080181511999896 ) ) ;
#14944 = CARTESIAN_POINT ( 'NONE',  ( 8.279953265935446893, -4.917462069712163597, 8.978228541670741691 ) ) ;
#14945 = AXIS2_PLACEMENT_3D ( 'NONE', #6934, #49589, #1696 ) ;
#14946 = CARTESIAN_POINT ( 'NONE',  ( 10.13063399569800005, -2.728594541839999721, 7.358888170452400068 ) ) ;
#14947 = VERTEX_POINT ( 'NONE', #28306 ) ;
#14948 = CARTESIAN_POINT ( 'NONE',  ( 2.834306799209666661, -1.762666431298145708, -3.058252359239904461 ) ) ;
#14949 = B_SPLINE_CURVE_WITH_KNOTS ( 'NONE', 3,
 ( #47895, #22251, #52788, #25532, #4882, #52439 ),
 .UNSPECIFIED., .F., .F.,
 ( 4, 2, 4 ),
 ( 0.000000000000000000, 0.5000000000000000000, 1.000000000000000000 ),
 .UNSPECIFIED. ) ;
#14950 = DIRECTION ( 'NONE',  ( 0.000000000000000000, 0.5393449376833056030, -0.8420849352621094797 ) ) ;
#14951 = ORIENTED_EDGE ( 'NONE', *, *, #10819, .T. ) ;
#14952 = DIRECTION ( 'NONE',  ( -1.000000000000000000, 0.000000000000000000, 0.000000000000000000 ) ) ;
#14953 = ORIENTED_EDGE ( 'NONE', *, *, #39541, .T. ) ;
#14954 = CARTESIAN_POINT ( 'NONE',  ( 18.30000103245939158, -11.66744832144745203, 3.971921730545766138 ) ) ;
#14955 = CARTESIAN_POINT ( 'NONE',  ( 2.467640132543333475, 1.762666431298152148, -3.058252359239900908 ) ) ;
#14956 = CARTESIAN_POINT ( 'NONE',  ( 11.26723293495529887, 2.826061044294000180, -7.452807962566580180 ) ) ;
#14957 = EDGE_CURVE ( 'NONE', #65610, #37496, #39925, .T. ) ;
#14958 = CARTESIAN_POINT ( 'NONE',  ( 11.35168717260510007, -4.613789146762799831, 6.498190316041999814 ) ) ;
#14959 = CARTESIAN_POINT ( 'NONE',  ( 12.54473519888576050, 3.068232154748442575, -12.30085162971233537 ) ) ;
#14960 = CARTESIAN_POINT ( 'NONE',  ( 11.36687616594229944, -4.344946439135400240, 8.587337146608000182 ) ) ;
#14961 = CARTESIAN_POINT ( 'NONE',  ( 8.977760841230999489, 2.019067547072999957, 7.390982789861999969 ) ) ;
#14962 = ORIENTED_EDGE ( 'NONE', *, *, #50264, .F. ) ;
#14963 = CARTESIAN_POINT ( 'NONE',  ( 7.000000000000000000, 0.2708497377871000311, 3.000000000000000000 ) ) ;
#14964 = CARTESIAN_POINT ( 'NONE',  ( 8.883148997460001084, 5.167567567567999731, 6.822293592207000934 ) ) ;
#14965 = CARTESIAN_POINT ( 'NONE',  ( 15.90000000000000036, -8.611670352360746961, -8.369116320314965662 ) ) ;
#14966 = VERTEX_POINT ( 'NONE', #17826 ) ;
#14967 = CARTESIAN_POINT ( 'NONE',  ( 12.58060354176266493, -1.796139714418076849, -12.47132288122299570 ) ) ;
#14968 = CARTESIAN_POINT ( 'NONE',  ( 10.22687885159599830, 5.132709421626000079, 7.635128076451499268 ) ) ;
#14969 = CARTESIAN_POINT ( 'NONE',  ( 10.35753185321000025, -5.367809014988999650, -6.514738374536999999 ) ) ;
#14970 = CARTESIAN_POINT ( 'NONE',  ( 7.294908919857999052, 10.77487787641000239, -3.564476421554995778 ) ) ;
#14971 = CARTESIAN_POINT ( 'NONE',  ( 2.490019101166500270, 3.500000000000001332, -0.4817981237446227194 ) ) ;
#14972 = CARTESIAN_POINT ( 'NONE',  ( 8.433148997460000018, 5.167567567567999731, 6.822293592207000934 ) ) ;
#14973 = CARTESIAN_POINT ( 'NONE',  ( 12.51733672169667422, -1.945066915100360783, -13.77556489992940847 ) ) ;
#14974 = CARTESIAN_POINT ( 'NONE',  ( 11.43718179236249988, -4.209680326224799707, -6.518682001772900136 ) ) ;
#14975 = CARTESIAN_POINT ( 'NONE',  ( 24.39664237488266707, -3.224866622838412411, -12.03536608415421050 ) ) ;
#14976 = CARTESIAN_POINT ( 'NONE',  ( 17.67439832720113557, -3.190335184669550461, 12.18941280901077917 ) ) ;
#14977 = ORIENTED_EDGE ( 'NONE', *, *, #56578, .F. ) ;
#14978 = ORIENTED_EDGE ( 'NONE', *, *, #45151, .T. ) ;
#14979 = CYLINDRICAL_SURFACE ( 'NONE', #28331, 10.75000000000000000 ) ;
#14980 = DIRECTION ( 'NONE',  ( 1.000000000000000000, 0.000000000000000000, 0.000000000000000000 ) ) ;
#14981 = LINE ( 'NONE', #20918, #19079 ) ;
#14982 = DIRECTION ( 'NONE',  ( 0.000000000000000000, 0.5000000000000169864, -0.8660254037844288266 ) ) ;
#14983 = CARTESIAN_POINT ( 'NONE',  ( 11.02205778663999958, 2.309481324353999554, -7.515673747780000191 ) ) ;
#14984 = FACE_BOUND ( 'NONE', #29924, .T. ) ;
#14985 = CARTESIAN_POINT ( 'NONE',  ( 17.92152980461522560, 3.006687145500352543, 12.31895938800958490 ) ) ;
#14986 = CARTESIAN_POINT ( 'NONE',  ( 17.76396973669300294, 3.526704268670000086, -11.96114524401999901 ) ) ;
#14987 = CARTESIAN_POINT ( 'NONE',  ( 9.261662452849000360, 2.944259351255000379, 6.507396354981000108 ) ) ;
#14988 = ORIENTED_EDGE ( 'NONE', *, *, #7441, .F. ) ;
#14989 = CARTESIAN_POINT ( 'NONE',  ( 10.97462572286999993, -5.299102401333000145, -4.938840653320999863 ) ) ;
#14990 = ADVANCED_FACE ( 'NONE', ( #60467 ), #17380, .T. ) ;
#14991 = VERTEX_POINT ( 'NONE', #49199 ) ;
#14992 = CARTESIAN_POINT ( 'NONE',  ( 12.60202002655574205, -3.091459147703856214, 12.29390037902082078 ) ) ;
#14993 = EDGE_CURVE ( 'NONE', #31587, #35662, #11114, .T. ) ;
#14994 = CARTESIAN_POINT ( 'NONE',  ( 9.501025935145998247, -4.125890936441000356, -6.642177514500700042 ) ) ;
#14995 = CARTESIAN_POINT ( 'NONE',  ( 10.69030645188999884, 5.903031974240000146, 7.830710565751001440 ) ) ;
#14996 = CARTESIAN_POINT ( 'NONE',  ( 11.93345123989529988, -3.459769760840400110, 6.456682674800999777 ) ) ;
#14997 = LINE ( 'NONE', #9744, #31706 ) ;
#14998 = VECTOR ( 'NONE', #18559, 1000.000000000000000 ) ;
#14999 = CARTESIAN_POINT ( 'NONE',  ( 9.317462135714000837, 5.100000000000000533, 6.571291218949999902 ) ) ;
#15000 = CARTESIAN_POINT ( 'NONE',  ( 10.61656919669529842, 5.225637333137999718, -7.862118085997298778 ) ) ;
#15001 = CARTESIAN_POINT ( 'NONE',  ( 12.69240093715870010, -0.6148490057825437560, 12.67995724530759816 ) ) ;
#15002 = CIRCLE ( 'NONE', #477, 10.75000000000000000 ) ;
#15003 = CARTESIAN_POINT ( 'NONE',  ( 5.619729929257407441, -12.11456185543947228, -3.745214083256774629 ) ) ;
#15004 = CARTESIAN_POINT ( 'NONE',  ( 18.36663043076582724, -2.717294527786511704, -11.46570543779412787 ) ) ;
#15005 = CARTESIAN_POINT ( 'NONE',  ( 11.42387073792000152, -3.325692027085000113, 11.41083924281000073 ) ) ;
#15006 = VERTEX_POINT ( 'NONE', #1652 ) ;
#15007 = CARTESIAN_POINT ( 'NONE',  ( 9.675870280412999236, 3.031907308384000022, -8.729608011560001657 ) ) ;
#15008 = FACE_OUTER_BOUND ( 'NONE', #12218, .T. ) ;
#15009 = CARTESIAN_POINT ( 'NONE',  ( 11.59999999999999964, 4.000000000000000000, 7.500000000000000000 ) ) ;
#15010 = LINE ( 'NONE', #6496, #10585 ) ;
#15011 = EDGE_CURVE ( 'NONE', #37580, #47653, #5310, .T. ) ;
#15012 = CARTESIAN_POINT ( 'NONE',  ( 12.10000000000000142, -4.304783012932057673, 8.455673667202290744 ) ) ;
#15013 = CARTESIAN_POINT ( 'NONE',  ( 11.21149010443640037, -2.862435565199000109, -7.585072163144589652 ) ) ;
#15014 = ORIENTED_EDGE ( 'NONE', *, *, #54531, .F. ) ;
#15015 = CARTESIAN_POINT ( 'NONE',  ( 2.011156362556000055, 3.707157770482000014, -0.6207725330884000803 ) ) ;
#15016 = EDGE_CURVE ( 'NONE', #32203, #64186, #33823, .T. ) ;
#15017 = CARTESIAN_POINT ( 'NONE',  ( 7.758198341228000672, 5.797099724369999763, 8.340484548805999765 ) ) ;
#15020 = UNCERTAINTY_MEASURE_WITH_UNIT (LENGTH_MEASURE( 1.000000000000000082E-05 ), #39578, 'distance_accuracy_value', 'NONE');
#15019 = CARTESIAN_POINT ( 'NONE',  ( 13.87269624719400163, -9.544758557629000606, -8.169753052074002042 ) ) ;
#15018 = CARTESIAN_POINT ( 'NONE',  ( 9.906784761384550109, 2.482585475679351728, 8.418381271750890349 ) ) ;
#15021 = CARTESIAN_POINT ( 'NONE',  ( 18.15932194375241338, -2.660757699944335197, 13.63806486313331945 ) ) ;
#15022 = EDGE_LOOP ( 'NONE', ( #56827, #36196, #19110, #22253, #26765, #22266, #24431, #59334 ) ) ;
#15023 = CARTESIAN_POINT ( 'NONE',  ( 12.07299956498157023, -2.792989229543000107, 7.174999999999999822 ) ) ;
#15024 = CARTESIAN_POINT ( 'NONE',  ( 18.09841665128862331, -2.190490658128016577, -13.73421521058128114 ) ) ;
#15025 = CARTESIAN_POINT ( 'NONE',  ( 11.07210672858429845, 3.307795442047700263, 8.020722037455799480 ) ) ;
#15026 = CYLINDRICAL_SURFACE ( 'NONE', #26571, 0.5000000000000002220 ) ;
#15027 = CARTESIAN_POINT ( 'NONE',  ( 9.106129440379998385, -4.192917962110999319, 5.525484568403999930 ) ) ;
#15028 = VERTEX_POINT ( 'NONE', #65958 ) ;
#15029 = CARTESIAN_POINT ( 'NONE',  ( 7.326301658771000369, 3.394842219570000097, 9.388954446285000088 ) ) ;
#15031 = CARTESIAN_POINT ( 'NONE',  ( 10.83488305961999920, -5.800181157098999840, -7.920538492179999501 ) ) ;
#15030 = CARTESIAN_POINT ( 'NONE',  ( 10.01721296880960033, -5.205658458020572255, 8.206277775804004193 ) ) ;
#15032 = CARTESIAN_POINT ( 'NONE',  ( 7.595706369369626287, -4.453886063348286406, 5.820683931063973304 ) ) ;
#15033 = CYLINDRICAL_SURFACE ( 'NONE', #63686, 0.6999999999999992895 ) ;
#15034 = CARTESIAN_POINT ( 'NONE',  ( 1.786156362557000055, 3.214278412021000175, -0.5382386926684999962 ) ) ;
#15035 = ORIENTED_EDGE ( 'NONE', *, *, #32625, .F. ) ;
#15036 = CARTESIAN_POINT ( 'NONE',  ( 2.182545538860289458, 1.234472752153680020, -2.960455995469124524 ) ) ;
#15037 = CARTESIAN_POINT ( 'NONE',  ( 11.98641235500450009, -4.739919807690899489, 8.177841818594698609 ) ) ;
#15038 = CARTESIAN_POINT ( 'NONE',  ( 9.967852198058999136, 2.034774058634999605, 7.636878205663998997 ) ) ;
#15039 = CARTESIAN_POINT ( 'NONE',  ( 9.409415556003999370, 2.113395950889999764, 7.914199712930999553 ) ) ;
#15040 = CARTESIAN_POINT ( 'NONE',  ( 10.21462282008599942, 4.523146351753199568, 6.656181553372300108 ) ) ;
#15041 = DIRECTION ( 'NONE',  ( -1.000000000000000000, 0.000000000000000000, 0.000000000000000000 ) ) ;
#15042 = CARTESIAN_POINT ( 'NONE',  ( 10.34920446230533564, 2.899999999999999911, -6.662590550568722847 ) ) ;
#15043 = CARTESIAN_POINT ( 'NONE',  ( 11.04384236319999957, 1.600341926351999788, 5.035088906224999938 ) ) ;
#15044 = FACE_OUTER_BOUND ( 'NONE', #5071, .T. ) ;
#15045 = AXIS2_PLACEMENT_3D ( 'NONE', #41389, #8887, #30221 ) ;
#15046 = DIRECTION ( 'NONE',  ( 0.000000000000000000, 1.000000000000000000, 0.000000000000000000 ) ) ;
#15047 = CARTESIAN_POINT ( 'NONE',  ( 17.88876225154221089, 3.028809290940018162, -13.54697662062381802 ) ) ;
#15048 = ORIENTED_EDGE ( 'NONE', *, *, #33666, .F. ) ;
#15049 = CARTESIAN_POINT ( 'NONE',  ( 10.84393020684979980, 2.750000000000000000, 7.500000000000000000 ) ) ;
#15050 = CARTESIAN_POINT ( 'NONE',  ( 10.52052890781999928, -2.899999999999999911, 6.152188490330000370 ) ) ;
#15051 = VERTEX_POINT ( 'NONE', #61418 ) ;
#15052 = CARTESIAN_POINT ( 'NONE',  ( 10.42702345793999896, -5.047055844931000124, 4.671718569916000874 ) ) ;
#15054 = CARTESIAN_POINT ( 'NONE',  ( 11.68748876160954886, 3.399618311400500303, 6.875627981711399883 ) ) ;
#15053 = CIRCLE ( 'NONE', #54121, 13.10000000000000320 ) ;
#15055 = EDGE_CURVE ( 'NONE', #61133, #49162, #32129, .T. ) ;
#15056 = CARTESIAN_POINT ( 'NONE',  ( 10.18756025349000005, 5.387489739490000318, 8.640945789268998922 ) ) ;
#15057 = EDGE_CURVE ( 'NONE', #68067, #7298, #19842, .T. ) ;
#15058 = CARTESIAN_POINT ( 'NONE',  ( 10.23643409129999959, 5.517148499152000340, -6.754126239302999934 ) ) ;
#15059 = CARTESIAN_POINT ( 'NONE',  ( 9.252229279041625176, -3.908861085869333785, -8.370187317335780364 ) ) ;
#15060 = CARTESIAN_POINT ( 'NONE',  ( 9.854949224988001077, -2.800315695760000168, 9.013807298610000629 ) ) ;
#15061 = CARTESIAN_POINT ( 'NONE',  ( 18.28003407448208151, 0.02395120399003647718, -12.59999907117299855 ) ) ;
#15062 = CARTESIAN_POINT ( 'NONE',  ( 9.020069425496542337, 5.146911715855399194, 8.214611775107460545 ) ) ;
#15063 = CARTESIAN_POINT ( 'NONE',  ( 11.55610404293055993, -4.502836909561000134, -8.523936114709998790 ) ) ;
#15064 = DIRECTION ( 'NONE',  ( 1.000000000000000000, 0.000000000000000000, 0.000000000000000000 ) ) ;
#15065 = ORIENTED_EDGE ( 'NONE', *, *, #16001, .F. ) ;
#15066 = AXIS2_PLACEMENT_3D ( 'NONE', #67066, #2078, #40845 ) ;
#15067 = DIRECTION ( 'NONE',  ( 0.000000000000000000, 1.000000000000000000, 0.000000000000000000 ) ) ;
#15068 = DIRECTION ( 'NONE',  ( 0.7071060218675898623, -0.7071075405046897133, 8.464214322710876718E-10 ) ) ;
#15069 = CARTESIAN_POINT ( 'NONE',  ( 24.95273178630209898, 8.555918886037284565, 8.377715515261876078 ) ) ;
#15070 = CARTESIAN_POINT ( 'NONE',  ( 21.05000000000000426, 0.000000000000000000, 0.000000000000000000 ) ) ;
#15071 = CARTESIAN_POINT ( 'NONE',  ( 12.30764200008706766, 3.049303773002893791, 13.66388724637008778 ) ) ;
#15072 = CARTESIAN_POINT ( 'NONE',  ( 11.11504459742000073, -3.456612073675000119, 5.970342812640000218 ) ) ;
#15073 = CARTESIAN_POINT ( 'NONE',  ( 12.31853785136292956, -0.3923495137057630422, -12.69184251825842757 ) ) ;
#15074 = CARTESIAN_POINT ( 'NONE',  ( 12.19581923677613489, -0.3960277493246582847, 13.99440111282555499 ) ) ;
#15075 = EDGE_CURVE ( 'NONE', #53746, #40911, #14471, .T. ) ;
#15076 = EDGE_LOOP ( 'NONE', ( #28274, #57582 ) ) ;
#15077 = CARTESIAN_POINT ( 'NONE',  ( 24.30857393632600250, 8.915481952665000875, 8.861377372684998477 ) ) ;
#15078 = ADVANCED_FACE ( 'NONE', ( #65271 ), #45346, .T. ) ;
#15079 = CARTESIAN_POINT ( 'NONE',  ( 13.99999999379500082, -8.815218614167999789, -7.616697584347000394 ) ) ;
#15080 = CARTESIAN_POINT ( 'NONE',  ( 9.662553763536999796, -4.094830574823999925, 9.119950378356000087 ) ) ;
#15081 = CARTESIAN_POINT ( 'NONE',  ( 15.92727146503378499, 9.312591611299771088, 8.375703117199133629 ) ) ;
#15082 = CARTESIAN_POINT ( 'NONE',  ( 11.35056919669530018, -3.169300617545700138, 7.254567470917099747 ) ) ;
#15083 = EDGE_CURVE ( 'NONE', #6863, #42044, #56194, .T. ) ;
#15084 = B_SPLINE_CURVE_WITH_KNOTS ( 'NONE', 3,
 ( #43815, #54286, #7089, #59880, #16541, #49742, #38209, #1851, #23169, #33325 ),
 .UNSPECIFIED., .F., .F.,
 ( 4, 2, 2, 2, 4 ),
 ( 0.000000000000000000, 0.2500000000000001110, 0.5000000000000001110, 0.7500000000000001110, 1.000000000000000000 ),
 .UNSPECIFIED. ) ;
#15085 = B_SPLINE_SURFACE_WITH_KNOTS ( 'NONE', 1, 3, ( 
 ( #854, #10307, #43511, #48401, #32674, #69036, #32338, #53647, #5409, #21148, #33016, #42475, #54330, #6431, #21480, #63782, #15894, #508, #53987, #64808, #27426, #16919, #53306, #5743, #16237, #43854, #21823, #52964, #10648, #38250, #42815, #26745, #5060, #43156, #49091, #164, #22511, #64462, #16585, #18664, #60277, #45240, #50137, #61310, #12732, #44897, #34061, #39298, #44563, #39996, #1543, #2576, #65508, #54683, #12034, #2242, #60966, #66546, #45584, #65856, #13431, #33716, #50474, #6781, #55377, #66200, #18322, #22861, #7830, #39645, #34752, #56061, #23556, #50823, #13081, #38960, #23904, #34411, #44213, #55728, #17635, #29165, #12382, #28119, #38602, #8172, #49431, #29521, #33368, #2918 ),
 ( #24247, #55033, #17277, #7133, #59923, #28471, #49786, #1896, #23216, #17979, #60621, #7472, #28826, #9189, #57775, #46614, #36456, #8514, #29862, #51170, #67229, #3265, #3941, #14793, #24597, #19002, #19344, #9885, #20378, #4289, #61998, #25970, #9532, #41702, #30195, #40666, #61652, #66890, #36112, #35775, #67570, #56411, #19696, #57089, #30530, #14111, #35435, #45917, #56761, #8858, #63006, #30877, #40329, #52189, #51843, #62673, #51501, #41016, #62338, #3598, #24934, #15135, #46268, #31227, #52534, #14455, #25279, #67919, #20035, #41364, #25625, #57426, #46953, #68257, #4631, #13765, #35099, #5153, #28478, #65163, #49795, #12738, #6787, #66206, #60974, #38259, #28125, #7140, #39652, #17283 ) ),
 .UNSPECIFIED., .F., .F., .F.,
 ( 2, 2 ),
 ( 4, 2, 2, 2, 2, 2, 2, 2, 2, 2, 2, 2, 2, 2, 2, 2, 2, 2, 2, 2, 2, 2, 2, 2, 2, 2, 2, 2, 2, 2, 2, 2, 2, 2, 2, 2, 2, 2, 2, 2, 2, 2, 2, 2, 4 ),
 ( 0.000000000000000000, 1.000000000000000000 ),
 ( 0.000000000000000000, 7.142752612018008851E-05, 0.0001428550522403601770, 0.0002142825783605402791, 0.0002857101044807203540, 0.0003214238675408103915, 0.0003571376306009004832, 0.0003928513936609905207, 0.0004285651567210805582, 0.0004999926828412606331, 0.0005357064459013507248, 0.0005714202089614407081, 0.0006071339720215306913, 0.0006428477350816207830, 0.0007142752612018009664, 0.0007857027873219810414, 0.0008214165503820710246, 0.0008571303134421611163, 0.0009285578395623411913, 0.0009999853656825212662, 0.001071412891802701450, 0.001142840417922881416, 0.001214267944043061383, 0.001285695470163241566, 0.001321409233223331658, 0.001357122996283421749, 0.001428550522403601933, 0.001499978048523782116, 0.001535691811583872208, 0.001571405574643962083, 0.001607119337704051958, 0.001642833100764142049, 0.001714260626884322233, 0.001749974389944412324, 0.001785688153004502416, 0.001821401916064592508, 0.001857115679124682383, 0.001928543205244862349, 0.001964256968304952441, 0.001999970731365042532, 0.002035684494425132624, 0.002071398257485222716, 0.002142825783605402899, 0.002214253309725583083, 0.002285680835845762832 ),
 .UNSPECIFIED. ) ;
#15086 = CARTESIAN_POINT ( 'NONE',  ( 12.36861573454711127, 0.5743932053697951012, 12.58690132123599525 ) ) ;
#15087 = PRESENTATION_LAYER_ASSIGNMENT (  '', '', ( #6139 ) ) ;
#15088 = CARTESIAN_POINT ( 'NONE',  ( 9.056630296855326279, 5.100000000000000533, 6.328714934328742103 ) ) ;
#15089 = CARTESIAN_POINT ( 'NONE',  ( 8.060295491240845323, 3.823126980273178432, 8.848192560902505832 ) ) ;
#15090 = CARTESIAN_POINT ( 'NONE',  ( 12.50259176966688379, 1.826373719304920540, 12.46693171540044531 ) ) ;
#15091 = CARTESIAN_POINT ( 'NONE',  ( 9.619904806657000762, -2.133039813254999917, -7.346564890486999566 ) ) ;
#15092 = CARTESIAN_POINT ( 'NONE',  ( 10.47718582084299932, 3.343463760027599818, -6.741111985563299491 ) ) ;
#15093 = CARTESIAN_POINT ( 'NONE',  ( 12.25964841771339309, 11.59985379594652599, -4.724415456179380968 ) ) ;
#15094 = CARTESIAN_POINT ( 'NONE',  ( 11.19050471959000070, 2.516756593394000152, -6.840361808223000217 ) ) ;
#15095 = CARTESIAN_POINT ( 'NONE',  ( 10.11188779216199940, 5.183207142131999845, -7.926693309523199282 ) ) ;
#15097 = CARTESIAN_POINT ( 'NONE',  ( 12.24249432807752314, 2.226917153349847300, 12.51101585363617730 ) ) ;
#15096 = CARTESIAN_POINT ( 'NONE',  ( 9.928731151682097078, 5.349829198379457473, 7.563678851448849549 ) ) ;
#15098 = CARTESIAN_POINT ( 'NONE',  ( 8.975133055567869889, 5.349981391149201571, 7.499992565666659949 ) ) ;
#15099 = ORIENTED_EDGE ( 'NONE', *, *, #6571, .T. ) ;
#15100 = CARTESIAN_POINT ( 'NONE',  ( 12.31443506033308921, -0.3873604453481457877, 12.69205253627869823 ) ) ;
#15101 = EDGE_CURVE ( 'NONE', #45349, #36624, #34384, .T. ) ;
#15102 = DIRECTION ( 'NONE',  ( -1.000000000000000000, 0.000000000000000000, 0.000000000000000000 ) ) ;
#15103 = VECTOR ( 'NONE', #27137, 1000.000000000000000 ) ;
#15104 = CARTESIAN_POINT ( 'NONE',  ( 8.856793857978997764, 5.100000000000000533, -6.339888365514000590 ) ) ;
#15105 = CARTESIAN_POINT ( 'NONE',  ( 9.425038493598998812, 4.627468580434300094, 8.098323595618600379 ) ) ;
#15106 = CARTESIAN_POINT ( 'NONE',  ( 23.59433343020063845, -3.211148892941130928, -13.60463507072412703 ) ) ;
#15107 = CARTESIAN_POINT ( 'NONE',  ( 12.33386765766683624, -2.911124516513512894, 13.57763168322026459 ) ) ;
#15108 = CARTESIAN_POINT ( 'NONE',  ( 12.19290954920418635, 2.626136293140859390, 13.64584403818151337 ) ) ;
#15109 = CARTESIAN_POINT ( 'NONE',  ( 8.168183350545964672, 2.950618456246918875, 6.463661575758196776 ) ) ;
#15110 = VERTEX_POINT ( 'NONE', #18083 ) ;
#15111 = B_SPLINE_CURVE_WITH_KNOTS ( 'NONE', 3,
 ( #3612, #29532, #18902, #12974, #2132, #60510 ),
 .UNSPECIFIED., .F., .F.,
 ( 4, 2, 4 ),
 ( 0.000000000000000000, 0.5000000000000000000, 1.000000000000000000 ),
 .UNSPECIFIED. ) ;
#15112 = B_SPLINE_CURVE_WITH_KNOTS ( 'NONE', 3,
 ( #50367, #61202, #13657, #50712 ),
 .UNSPECIFIED., .F., .F.,
 ( 4, 4 ),
 ( 0.000000000000000000, 1.000000000000000000 ),
 .UNSPECIFIED. ) ;
#15113 = CARTESIAN_POINT ( 'NONE',  ( 4.569067376532999880, 0.6287086875568000943, -1.109729982504999990 ) ) ;
#15114 = CARTESIAN_POINT ( 'NONE',  ( 9.681292290062998518, -2.893743561734000380, -6.857675253263499471 ) ) ;
#15115 = DIRECTION ( 'NONE',  ( 0.4682208595141937879, -0.4682208595141937879, 0.7493586947727897130 ) ) ;
#15117 = B_SPLINE_CURVE_WITH_KNOTS ( 'NONE', 3,
 ( #66865, #61624, #51476, #29834 ),
 .UNSPECIFIED., .F., .F.,
 ( 4, 4 ),
 ( 0.000000000000000000, 1.000000000000000000 ),
 .UNSPECIFIED. ) ;
#15116 = CARTESIAN_POINT ( 'NONE',  ( 11.22702344389999851, -5.004394439171999664, 8.109550315577399360 ) ) ;
#15118 = CARTESIAN_POINT ( 'NONE',  ( 17.93339585188538976, 2.997500062648085883, -12.32163866699053401 ) ) ;
#15119 = CARTESIAN_POINT ( 'NONE',  ( 9.742292592096250203, -4.365494583328262124, 8.705986097797767442 ) ) ;
#15120 = CARTESIAN_POINT ( 'NONE',  ( 18.10295792974228490, 2.800845227017174643, 12.37636719702360288 ) ) ;
#15121 = CARTESIAN_POINT ( 'NONE',  ( 7.415011787918005304, 3.233093659812002585, 6.479723185591006462 ) ) ;
#15122 = CARTESIAN_POINT ( 'NONE',  ( 11.13491264576000006, -2.665455753003000527, -5.170164771427000261 ) ) ;
#15123 = CARTESIAN_POINT ( 'NONE',  ( 9.970944094204998720, -5.100000000000000533, 6.571291218949999902 ) ) ;
#15124 = CARTESIAN_POINT ( 'NONE',  ( 24.14474055218938986, 3.678932468831995539, -12.80134587320634054 ) ) ;
#15125 = AXIS2_PLACEMENT_3D ( 'NONE', #3292, #45947, #12415 ) ;
#15126 = CARTESIAN_POINT ( 'NONE',  ( 12.21569938124765820, 0.4259565731506669839, -13.99353270933016979 ) ) ;
#15127 = CARTESIAN_POINT ( 'NONE',  ( 11.07299956498199833, -2.792989229543000107, -7.825000000000000178 ) ) ;
#15128 = CYLINDRICAL_SURFACE ( 'NONE', #43250, 1.999999999999999556 ) ;
#15129 = CARTESIAN_POINT ( 'NONE',  ( 9.074999999999999289, -4.417172942406000224, 8.783926296998000538 ) ) ;
#15130 = VERTEX_POINT ( 'NONE', #60725 ) ;
#15131 = CARTESIAN_POINT ( 'NONE',  ( 9.211104719594999324, 5.462898983065000102, -8.055936939571999744 ) ) ;
#15132 = CARTESIAN_POINT ( 'NONE',  ( 11.25210807141120029, -3.959980833595939664, 6.634727177901499573 ) ) ;
#15133 = VERTEX_POINT ( 'NONE', #28225 ) ;
#15134 = FACE_OUTER_BOUND ( 'NONE', #31248, .T. ) ;
#15135 = CARTESIAN_POINT ( 'NONE',  ( 18.13255570286229101, 2.076448383791616781, -13.84516006853289127 ) ) ;
#15136 = ORIENTED_EDGE ( 'NONE', *, *, #1656, .F. ) ;
#15137 = CARTESIAN_POINT ( 'NONE',  ( 11.55300581613033906, 5.107584469683000172, 6.788791567531699656 ) ) ;
#15138 = CARTESIAN_POINT ( 'NONE',  ( 9.790085841230000696, 5.149303692842000402, -5.987168472229000393 ) ) ;
#15139 = EDGE_CURVE ( 'NONE', #47642, #25573, #33662, .T. ) ;
#15140 = DIRECTION ( 'NONE',  ( 0.000000000000000000, -0.9466492601157000530, 0.3222656952305000266 ) ) ;
#15141 = EDGE_CURVE ( 'NONE', #54978, #63863, #23662, .T. ) ;
#15142 = CARTESIAN_POINT ( 'NONE',  ( 9.378359312499400247, -5.126777126185184663, 6.752018918871678821 ) ) ;
#15143 = CARTESIAN_POINT ( 'NONE',  ( 8.933148997457999840, 5.167567567567999731, 6.822293592207000934 ) ) ;
#15144 = CARTESIAN_POINT ( 'NONE',  ( 10.99999999997000089, -4.000000000000000000, -7.500000000000000000 ) ) ;
#15145 = ORIENTED_EDGE ( 'NONE', *, *, #64812, .T. ) ;
#15146 = CARTESIAN_POINT ( 'NONE',  ( 13.75930817923600102, 9.623971528738000103, 8.076134841847999013 ) ) ;
#15147 = CARTESIAN_POINT ( 'NONE',  ( 9.883629719592001095, 5.656948148960999845, -6.994239053114000626 ) ) ;
#15148 = ORIENTED_EDGE ( 'NONE', *, *, #27354, .T. ) ;
#15149 = CARTESIAN_POINT ( 'NONE',  ( 10.74708949327000163, 5.603142351927999698, -6.963341971584000589 ) ) ;
#15150 = VERTEX_POINT ( 'NONE', #39754 ) ;
#15151 = CARTESIAN_POINT ( 'NONE',  ( 8.997405316140000053, 3.728406863338599830, 6.249951378708000327 ) ) ;
#15152 = CARTESIAN_POINT ( 'NONE',  ( 17.97018005872497426, -2.032669421145251842, -12.54824173908127882 ) ) ;
#15153 = CIRCLE ( 'NONE', #20741, 14.00000000000000000 ) ;
#15154 = DIRECTION ( 'NONE',  ( 0.000000000000000000, 0.8514543052404082157, -0.5244287998266055073 ) ) ;
#15155 = CARTESIAN_POINT ( 'NONE',  ( 18.17512443070437200, -2.418970859208086743, -12.47009038069303521 ) ) ;
#15156 = CARTESIAN_POINT ( 'NONE',  ( 24.34832161043337351, -3.224867767510426919, 12.03537035604409056 ) ) ;
#15157 = VERTEX_POINT ( 'NONE', #17742 ) ;
#15158 = CARTESIAN_POINT ( 'NONE',  ( 12.42828976145100128, 11.57811841779999895, -4.879106015068000346 ) ) ;
#15159 = CARTESIAN_POINT ( 'NONE',  ( 17.73161317130500336, 12.16650445177999984, -3.137092607272999878 ) ) ;
#15160 = CARTESIAN_POINT ( 'NONE',  ( 7.935182732229959512, -5.348502701843340645, 7.676951299079880719 ) ) ;
#15161 = CARTESIAN_POINT ( 'NONE',  ( 12.61614725291585160, 3.223296771745986167, -13.62389115065822054 ) ) ;
#15162 = EDGE_CURVE ( 'NONE', #51247, #23850, #56689, .T. ) ;
#15163 = CARTESIAN_POINT ( 'NONE',  ( 8.997439158776000312, 2.773858540272000184, -8.951250717848999727 ) ) ;
#15164 = CARTESIAN_POINT ( 'NONE',  ( 17.85728973496400229, 3.190139087762999814, 11.45065787240999988 ) ) ;
#15165 = CARTESIAN_POINT ( 'NONE',  ( 9.988720925027999797, -2.842024021884000273, -6.504330542082999322 ) ) ;
#15166 = EDGE_LOOP ( 'NONE', ( #35586, #53992, #2975, #36225, #49061, #54756 ) ) ;
#15167 = ORIENTED_EDGE ( 'NONE', *, *, #39616, .T. ) ;
#15168 = CARTESIAN_POINT ( 'NONE',  ( 9.079170280414000871, 4.815598936798999752, -8.835641302565999666 ) ) ;
#15169 = CARTESIAN_POINT ( 'NONE',  ( 10.92799928938507925, -5.127999289385079429, -6.526892970155856233 ) ) ;
#15170 = CARTESIAN_POINT ( 'NONE',  ( 1.123890132541374820, 2.150913519912194261, 2.798833948393636195 ) ) ;
#15171 = CARTESIAN_POINT ( 'NONE',  ( 24.23036338817854585, 3.301121323903743576, 12.33133795113440456 ) ) ;
#15172 = CARTESIAN_POINT ( 'NONE',  ( 10.63880513895979973, 5.150451045932999961, -6.860457220153399760 ) ) ;
#15173 = CARTESIAN_POINT ( 'NONE',  ( 8.876797255587998592, 4.866234952405400271, -7.463326341748410364 ) ) ;
#15175 = CARTESIAN_POINT ( 'NONE',  ( 8.667968151675525590, 5.621194584483597545, 6.797889474695828049 ) ) ;
#15174 = CARTESIAN_POINT ( 'NONE',  ( 10.33231740696899870, -3.813190776280700245, 6.513113677132300161 ) ) ;
#15176 = CARTESIAN_POINT ( 'NONE',  ( 4.638359839683334762, -0.7554284705563483193, -1.310679582531387721 ) ) ;
#15177 = ORIENTED_EDGE ( 'NONE', *, *, #7679, .T. ) ;
#15178 = CARTESIAN_POINT ( 'NONE',  ( 11.85979573085659844, -3.159987984332300215, -7.645349278262099979 ) ) ;
#15179 = EDGE_CURVE ( 'NONE', #4537, #59620, #20276, .T. ) ;
#15180 = CONICAL_SURFACE ( 'NONE', #54251, 1.150081673463000165, 0.7854598275718697176 ) ;
#15181 = CARTESIAN_POINT ( 'NONE',  ( 8.046990059540997109, -3.146252403201002856, 6.173090499042001689 ) ) ;
#15182 = CARTESIAN_POINT ( 'NONE',  ( 9.709696787963999043, 4.219671260427300119, 8.760209873321999297 ) ) ;
#15183 = CARTESIAN_POINT ( 'NONE',  ( 11.09999999999999964, -2.649999999999999911, -7.500000000000000000 ) ) ;
#15184 = CARTESIAN_POINT ( 'NONE',  ( 9.815199780373001559, -2.813634733202999616, 8.848854270764999086 ) ) ;
#15185 = CARTESIAN_POINT ( 'NONE',  ( 0.1500001228197999914, 2.250000122783999856, -5.253495588359999773E-10 ) ) ;
#15186 = CARTESIAN_POINT ( 'NONE',  ( 25.29987931604000195, 11.13052921044000065, -3.427478701325000099 ) ) ;
#15187 = CARTESIAN_POINT ( 'NONE',  ( 13.73763077846600034, 8.978479145825000174, 7.363267546620999582 ) ) ;
#15188 = DIRECTION ( 'NONE',  ( -1.000000000000000000, 0.000000000000000000, 0.000000000000000000 ) ) ;
#15189 = VECTOR ( 'NONE', #18212, 999.9999999999998863 ) ;
#15190 = CARTESIAN_POINT ( 'NONE',  ( 11.10226354018308115, -2.907767014557176566, 6.870476274536374106 ) ) ;
#15191 = AXIS2_PLACEMENT_3D ( 'NONE', #66992, #63807, #15237 ) ;
#15192 = DIRECTION ( 'NONE',  ( 1.000000000000000000, 0.000000000000000000, 0.000000000000000000 ) ) ;
#15193 = CARTESIAN_POINT ( 'NONE',  ( 0.1499942179680000265, -1.384928887584815804, -2.402872127494067644 ) ) ;
#15194 = CARTESIAN_POINT ( 'NONE',  ( 3.639522202018000030, 2.080217348686999923, -2.466622738429000261 ) ) ;
#15195 = ORIENTED_EDGE ( 'NONE', *, *, #28667, .F. ) ;
#15196 = CARTESIAN_POINT ( 'NONE',  ( 12.21300000160833577, 0.2005123242923269322, -12.69787478206145259 ) ) ;
#15197 = CARTESIAN_POINT ( 'NONE',  ( 12.29671722858996041, -2.864281468071980807, -12.35920955626405515 ) ) ;
#15198 = DIRECTION ( 'NONE',  ( -1.000000000000000000, 0.000000000000000000, 0.000000000000000000 ) ) ;
#15199 = CARTESIAN_POINT ( 'NONE',  ( 12.80505043854146940, -1.875000000000000444, 13.78631952119025605 ) ) ;
#15200 = CARTESIAN_POINT ( 'NONE',  ( 3.500000000000001332, -0.7367456077618940169, 3.179724234113067372 ) ) ;
#15201 = VERTEX_POINT ( 'NONE', #40103 ) ;
#15202 = CARTESIAN_POINT ( 'NONE',  ( 5.694792710280000669, 0.06352927768877000836, 1.174369886990999978 ) ) ;
#15203 = APPLICATION_PROTOCOL_DEFINITION ( 'draft international standard', 'automotive_design', 1998, #65948 ) ;
#15204 = CARTESIAN_POINT ( 'NONE',  ( 17.55505043854144276, 0.6250000000000001110, 12.67928921589117586 ) ) ;
#15205 = CARTESIAN_POINT ( 'NONE',  ( 13.51386961183700031, -11.53357255609999932, -1.992589078083000009 ) ) ;
#15206 = CARTESIAN_POINT ( 'NONE',  ( 7.564999999998999414, 5.349999999999999645, -7.500000000000000000 ) ) ;
#15207 = CARTESIAN_POINT ( 'NONE',  ( 13.05446786537200232, 12.11615129267999968, 2.032410325197000045 ) ) ;
#15208 = VERTEX_POINT ( 'NONE', #12488 ) ;
#15209 = CARTESIAN_POINT ( 'NONE',  ( 10.27968096967000022, -5.739708848514999850, 7.774962785835000112 ) ) ;
#15210 = ORIENTED_EDGE ( 'NONE', *, *, #26802, .T. ) ;
#15211 = DIRECTION ( 'NONE',  ( 1.000000000000000000, 0.000000000000000000, 0.000000000000000000 ) ) ;
#15212 = CARTESIAN_POINT ( 'NONE',  ( 7.930394353207000258, -3.164807285701999984, 9.104732190648000767 ) ) ;
#15213 = DIRECTION ( 'NONE',  ( 0.000000000000000000, -1.000000000000000000, 0.000000000000000000 ) ) ;
#15214 = EDGE_CURVE ( 'NONE', #68576, #19063, #27636, .T. ) ;
#15215 = ORIENTED_EDGE ( 'NONE', *, *, #29338, .F. ) ;
#15216 = CARTESIAN_POINT ( 'NONE',  ( 8.267894473231022445, 3.183914367779229870, -6.154702421054330408 ) ) ;
#15217 = ADVANCED_FACE ( 'NONE', ( #14558 ), #3364, .F. ) ;
#15218 = DIRECTION ( 'NONE',  ( 0.000000000000000000, -1.000000000000000000, 0.000000000000000000 ) ) ;
#15219 = CARTESIAN_POINT ( 'NONE',  ( 7.233579719589999790, 5.250007070404999254, -8.441605882928000071 ) ) ;
#15220 = DIRECTION ( 'NONE',  ( 1.000000000000000000, 0.000000000000000000, 0.000000000000000000 ) ) ;
#15221 = EDGE_CURVE ( 'NONE', #1019, #55375, #36126, .T. ) ;
#15222 = LINE ( 'NONE', #36547, #6110 ) ;
#15223 = ORIENTED_EDGE ( 'NONE', *, *, #61317, .T. ) ;
#15224 = CARTESIAN_POINT ( 'NONE',  ( 9.629020610622001541, -5.794331084664000819, 7.414872097535999629 ) ) ;
#15225 = ADVANCED_FACE ( 'NONE', ( #9290 ), #8278, .F. ) ;
#15226 = CARTESIAN_POINT ( 'NONE',  ( 12.80505043854146940, -1.875000000000000444, -13.78627172894481667 ) ) ;
#15227 = CARTESIAN_POINT ( 'NONE',  ( 11.25740844561608611, 5.045781347359230118, -7.175000373111195984 ) ) ;
#15228 = ORIENTED_EDGE ( 'NONE', *, *, #47320, .F. ) ;
#15229 = CARTESIAN_POINT ( 'NONE',  ( 9.101497196731600070, 2.899999999999999911, 6.350512455778112297 ) ) ;
#15230 = CARTESIAN_POINT ( 'NONE',  ( 10.98956486188259341, -5.568313880529865756, -4.946129200245233726 ) ) ;
#15231 = ORIENTED_EDGE ( 'NONE', *, *, #5613, .F. ) ;
#15232 = CARTESIAN_POINT ( 'NONE',  ( 24.30000000000000071, -50.50083396221999976, -14.25635100356000073 ) ) ;
#15233 = CARTESIAN_POINT ( 'NONE',  ( 24.04053420818027575, 12.64669712376688793, -3.439809266941736166 ) ) ;
#15234 = CARTESIAN_POINT ( 'NONE',  ( 10.93769906941999892, 2.936877991120999898, -4.920829195977000303 ) ) ;
#15235 = AXIS2_PLACEMENT_3D ( 'NONE', #1636, #65600, #48150 ) ;
#15236 = CARTESIAN_POINT ( 'NONE',  ( 6.999999691988000095, -12.89129024452999950, 1.677687644161999891 ) ) ;
#15237 = DIRECTION ( 'NONE',  ( 0.000000000000000000, 1.000000000000000000, 0.000000000000000000 ) ) ;
#15238 = CARTESIAN_POINT ( 'NONE',  ( 0.000000000000000000, 0.000000000000000000, 0.000000000000000000 ) ) ;
#15239 = CARTESIAN_POINT ( 'NONE',  ( 12.29585337184155946, 2.862976231886636302, 13.58970269765488048 ) ) ;
#15240 = CARTESIAN_POINT ( 'NONE',  ( 4.149992563292000725, 2.000000000000000000, 0.000000000000000000 ) ) ;
#15241 = ORIENTED_EDGE ( 'NONE', *, *, #6401, .F. ) ;
#15242 = CARTESIAN_POINT ( 'NONE',  ( 7.696680409794002919, -4.865376733307997803, 6.399695646141002392 ) ) ;
#15243 = B_SPLINE_CURVE_WITH_KNOTS ( 'NONE', 3,
 ( #45986, #61718, #56135, #13837 ),
 .UNSPECIFIED., .F., .F.,
 ( 4, 4 ),
 ( 0.000000000000000000, 1.000000000000000000 ),
 .UNSPECIFIED. ) ;
#15244 = B_SPLINE_CURVE_WITH_KNOTS ( 'NONE', 3,
 ( #6443, #18330, #39654, #27791, #34424, #1212, #22523, #54692, #45928, #29529, #30885, #24255, #9540, #57099, #24943, #30205, #35443, #14119 ),
 .UNSPECIFIED., .F., .F.,
 ( 4, 2, 2, 2, 2, 2, 2, 2, 4 ),
 ( 0.000000000000000000, 0.1249999999999999722, 0.2499999999999999445, 0.3749999999999998890, 0.4999999999999998890, 0.6249999999999998890, 0.7499999999999997780, 0.8749999999999998890, 1.000000000000000000 ),
 .UNSPECIFIED. ) ;
#15245 = ORIENTED_EDGE ( 'NONE', *, *, #63909, .F. ) ;
#15246 = CARTESIAN_POINT ( 'NONE',  ( 9.520797373037000355, 3.270552986600999912, 5.711478154812000163 ) ) ;
#15247 = EDGE_CURVE ( 'NONE', #11010, #15130, #47751, .T. ) ;
#15248 = DIRECTION ( 'NONE',  ( 0.000000000000000000, 1.000000000000000000, 0.000000000000000000 ) ) ;
#15249 = VECTOR ( 'NONE', #31032, 1000.000000000000000 ) ;
#15250 = CYLINDRICAL_SURFACE ( 'NONE', #29403, 0.4999999999999998335 ) ;
#15251 = CARTESIAN_POINT ( 'NONE',  ( 2.768173772219000295, -3.696853176092000481, 0.2879355096300999506 ) ) ;
#15252 = DIRECTION ( 'NONE',  ( 0.000000000000000000, 1.000000000000000000, 0.000000000000000000 ) ) ;
#15253 = CARTESIAN_POINT ( 'NONE',  ( 25.30000327618300204, 10.83443035398000021, -3.855530949778000149 ) ) ;
#15254 = LINE ( 'NONE', #550, #46205 ) ;
#15255 = ORIENTED_EDGE ( 'NONE', *, *, #63339, .T. ) ;
#15256 = CARTESIAN_POINT ( 'NONE',  ( 12.78268972790800184, -11.49710380946999955, 4.820178426657999005 ) ) ;
#15257 = CARTESIAN_POINT ( 'NONE',  ( 10.89503166480599994, -5.274847857784000560, 7.410114961806599787 ) ) ;
#15258 = CARTESIAN_POINT ( 'NONE',  ( 10.43243243692329081, 4.711781382511952998, -9.127213014442659755 ) ) ;
#15259 = PLANE ( 'NONE',  #21485 ) ;
#15260 = CARTESIAN_POINT ( 'NONE',  ( 9.234504440379000201, -5.964711531933999389, 7.776478361891000723 ) ) ;
#15262 = CARTESIAN_POINT ( 'NONE',  ( 23.60205915885299888, -2.504446818062000535, -12.27382285989999566 ) ) ;
#15261 = CARTESIAN_POINT ( 'NONE',  ( 10.68903608760000168, 2.568976842941999905, 7.728092503410000091 ) ) ;
#15263 = CARTESIAN_POINT ( 'NONE',  ( 11.25656651104150008, 4.126085365637900182, -6.228222165170999247 ) ) ;
#15264 = DIRECTION ( 'NONE',  ( 0.000000000000000000, 0.000000000000000000, -1.000000000000000000 ) ) ;
#15265 = EDGE_CURVE ( 'NONE', #43864, #62706, #36562, .T. ) ;
#15266 = CARTESIAN_POINT ( 'NONE',  ( 10.00760887879199856, 3.803658216258800184, -6.655513263298900029 ) ) ;
#15267 = CARTESIAN_POINT ( 'NONE',  ( 17.85474174040770023, 0.6550687562476208425, 12.58296113213902245 ) ) ;
#15268 = CARTESIAN_POINT ( 'NONE',  ( 6.706645871493999600, -1.006228542663000214, 0.7393869427924999460 ) ) ;
#15269 = CARTESIAN_POINT ( 'NONE',  ( 10.97124174884019965, 3.963805917081910213, 6.184229974648999928 ) ) ;
#15270 = EDGE_CURVE ( 'NONE', #53716, #60760, #43689, .T. ) ;
#15271 = CARTESIAN_POINT ( 'NONE',  ( 12.10000000000000142, 50.14170351282000127, -17.06962823869000090 ) ) ;
#15272 = ORIENTED_EDGE ( 'NONE', *, *, #35410, .F. ) ;
#15273 = CARTESIAN_POINT ( 'NONE',  ( 8.636456853209999451, -3.869396851328000153, 5.695656592546999519 ) ) ;
#15274 = CARTESIAN_POINT ( 'NONE',  ( 8.475644353210000759, -5.095088356574999366, 6.286978111459999852 ) ) ;
#15275 = CARTESIAN_POINT ( 'NONE',  ( 17.60315097558330777, 3.246934396132593825, 13.61827533163851101 ) ) ;
#15276 = DIRECTION ( 'NONE',  ( 2.887756364190075102E-10, -0.5897878662160149776, -0.8075582163933199276 ) ) ;
#15277 = VERTEX_POINT ( 'NONE', #63110 ) ;
#15278 = AXIS2_PLACEMENT_3D ( 'NONE', #57872, #26058, #47387 ) ;
#15279 = CARTESIAN_POINT ( 'NONE',  ( 0.4855877078939999647, -3.136585174263000209, 0.6804425983637999442 ) ) ;
#15280 = VECTOR ( 'NONE', #55218, 1000.000000000000000 ) ;
#15281 = CARTESIAN_POINT ( 'NONE',  ( 10.84657802013509986, 2.684088780794000151, 7.530633716161349689 ) ) ;
#15282 = CARTESIAN_POINT ( 'NONE',  ( 10.77401721959000014, 3.826866801954999620, -5.823193568970000733 ) ) ;
#15283 = ORIENTED_EDGE ( 'NONE', *, *, #25080, .T. ) ;
#15284 = CARTESIAN_POINT ( 'NONE',  ( 8.869959105252339882, 2.899999999999999911, 6.481052078534832006 ) ) ;
#15285 = DIRECTION ( 'NONE',  ( 0.000000000000000000, 0.8648648648648717963, -0.5020047465136829867 ) ) ;
#15286 = CARTESIAN_POINT ( 'NONE',  ( 11.18272066707849888, 5.093522884867000222, 8.161456030935699602 ) ) ;
#15287 = CARTESIAN_POINT ( 'NONE',  ( 17.60000000714711277, -11.20147114780081843, 4.552742043578180464 ) ) ;
#15289 = CARTESIAN_POINT ( 'NONE',  ( 8.079135841228998416, 3.524748802314000340, 5.573833469815000718 ) ) ;
#15288 = VECTOR ( 'NONE', #34486, 1000.000000000000114 ) ;
#15290 = ORIENTED_EDGE ( 'NONE', *, *, #3351, .T. ) ;
#15291 = CARTESIAN_POINT ( 'NONE',  ( 11.09999999999999964, -5.449702618175999547, 5.124965750789000296 ) ) ;
#15292 = CARTESIAN_POINT ( 'NONE',  ( 7.019914158769999801, 2.417988323708999854, -8.552044326954000297 ) ) ;
#15293 = CARTESIAN_POINT ( 'NONE',  ( 8.288447824096289551, -4.754611573949904191, 9.066990413095210144 ) ) ;
#15294 = CARTESIAN_POINT ( 'NONE',  ( 9.953329965422000214, -4.888489908445900589, 6.579690231462300254 ) ) ;
#15295 = ORIENTED_EDGE ( 'NONE', *, *, #45316, .F. ) ;
#15296 = CARTESIAN_POINT ( 'NONE',  ( 2.896806799209917127, 0.9161175952574848180, -3.408904368339103819 ) ) ;
#15297 = CARTESIAN_POINT ( 'NONE',  ( 7.204898016025000018, -0.2500000000000000000, -3.099950251719000072 ) ) ;
#15298 = VERTEX_POINT ( 'NONE', #41124 ) ;
#15299 = DIRECTION ( 'NONE',  ( 1.000000000000000000, 0.000000000000000000, 0.000000000000000000 ) ) ;
#15300 = CYLINDRICAL_SURFACE ( 'NONE', #13426, 0.4999999999999998335 ) ;
#15301 = ORIENTED_EDGE ( 'NONE', *, *, #21955, .T. ) ;
#15302 = CARTESIAN_POINT ( 'NONE',  ( 18.13658220607008786, 0.2292390942789236941, -13.89746050377129905 ) ) ;
#15303 = CARTESIAN_POINT ( 'NONE',  ( 7.726789014911999764, -2.853537667309000270, 6.781794374791000557 ) ) ;
#15304 = CARTESIAN_POINT ( 'NONE',  ( 2.311390132542709086, -3.500000000000000888, -0.4581489286485119217 ) ) ;
#15305 = AXIS2_PLACEMENT_3D ( 'NONE', #54239, #6341, #60536 ) ;
#15306 = CARTESIAN_POINT ( 'NONE',  ( 10.76857802013509868, 2.825431102905000103, -7.472656658230009796 ) ) ;
#15307 = CARTESIAN_POINT ( 'NONE',  ( 11.76723293495529887, -5.173938955706000264, 7.547192037433419820 ) ) ;
#15308 = CARTESIAN_POINT ( 'NONE',  ( 12.58270105247233417, 3.084473834238323331, -12.29599965897950220 ) ) ;
#15309 = EDGE_CURVE ( 'NONE', #51764, #61432, #61121, .T. ) ;
#15310 = CARTESIAN_POINT ( 'NONE',  ( 11.53918313518939875, -4.707599264529200411, 6.605241151424599444 ) ) ;
#15311 = CARTESIAN_POINT ( 'NONE',  ( 7.448642219589999947, 4.628941086829000184, 5.991667691044999522 ) ) ;
#15312 = EDGE_CURVE ( 'NONE', #8614, #2551, #31193, .T. ) ;
#15313 = ORIENTED_EDGE ( 'NONE', *, *, #69149, .F. ) ;
#15314 = CARTESIAN_POINT ( 'NONE',  ( -0.2999999999999999889, 1.154700538379000108, 0.000000000000000000 ) ) ;
#15315 = CARTESIAN_POINT ( 'NONE',  ( 11.56914347478616634, -3.251273819902354312, -8.529874251157636422 ) ) ;
#15316 = CARTESIAN_POINT ( 'NONE',  ( 12.80505043854143388, 1.760845406083386688, -12.47635457398814829 ) ) ;
#15317 = ORIENTED_EDGE ( 'NONE', *, *, #69042, .T. ) ;
#15318 = CARTESIAN_POINT ( 'NONE',  ( 12.19649458927093555, -2.642789655208612754, -12.41715525233005479 ) ) ;
#15319 = CARTESIAN_POINT ( 'NONE',  ( 9.840759809372002564, 7.661537722051988908, -5.619389075507000619 ) ) ;
#15320 = CYLINDRICAL_SURFACE ( 'NONE', #31579, 0.5000000000000004441 ) ;
#15321 = CYLINDRICAL_SURFACE ( 'NONE', #28592, 9.250000000000000000 ) ;
#15322 = CARTESIAN_POINT ( 'NONE',  ( 12.36790649065927283, -2.053195086250958479, -13.75808315936462023 ) ) ;
#15323 = CARTESIAN_POINT ( 'NONE',  ( 10.99826088462129903, -3.998156935320088756, -6.633804182961699603 ) ) ;
#15324 = CARTESIAN_POINT ( 'NONE',  ( 17.97784399489228946, 3.574258648614753398, 12.00418160090821473 ) ) ;
#15325 = CARTESIAN_POINT ( 'NONE',  ( 18.13174941159754283, -2.917101476509666114, 12.25768593326185396 ) ) ;
#15326 = VERTEX_POINT ( 'NONE', #62437 ) ;
#15327 = ORIENTED_EDGE ( 'NONE', *, *, #15016, .T. ) ;
#15328 = EDGE_CURVE ( 'NONE', #29598, #57705, #47059, .T. ) ;
#15329 = CARTESIAN_POINT ( 'NONE',  ( 0.000000000000000000, 0.000000000000000000, 0.000000000000000000 ) ) ;
#15330 = DIRECTION ( 'NONE',  ( -1.000000000000000000, 0.000000000000000000, 0.000000000000000000 ) ) ;
#15331 = CARTESIAN_POINT ( 'NONE',  ( 4.900006121741999010, -2.000000000000000000, 0.000000000000000000 ) ) ;
#15332 = CARTESIAN_POINT ( 'NONE',  ( 10.93146722582000052, 2.472885155055999817, -7.514158739122999364 ) ) ;
#15333 = CARTESIAN_POINT ( 'NONE',  ( 10.64447714202000128, -5.073836261934999925, -8.340686666652999293 ) ) ;
#15334 = MECHANICAL_DESIGN_GEOMETRIC_PRESENTATION_REPRESENTATION (  '', ( #30960 ), #34312 ) ;
#15335 = CARTESIAN_POINT ( 'NONE',  ( 18.17921332558106329, 2.461874964459677795, 12.46038192087330643 ) ) ;
#15336 = CARTESIAN_POINT ( 'NONE',  ( 16.13895793972310599, 3.268072512451278389, 11.38828084065380608 ) ) ;
#15337 = CARTESIAN_POINT ( 'NONE',  ( 10.93727498060999892, 5.425427353909999972, 7.240585962396000497 ) ) ;
#15338 = B_SPLINE_CURVE_WITH_KNOTS ( 'NONE', 3,
 ( #68945, #42040, #63346, #47634 ),
 .UNSPECIFIED., .F., .F.,
 ( 4, 4 ),
 ( 0.8745081996710677430, 1.000000000000000000 ),
 .UNSPECIFIED. ) ;
#15339 = ORIENTED_EDGE ( 'NONE', *, *, #34102, .F. ) ;
#15340 = CARTESIAN_POINT ( 'NONE',  ( 8.781951181944481988, 5.320239682019779259, -6.310370185644361918 ) ) ;
#15341 = ORIENTED_EDGE ( 'NONE', *, *, #41232, .T. ) ;
#15342 = CARTESIAN_POINT ( 'NONE',  ( 18.29991931957795259, -1.031823913341759950E-13, -12.32514597914127563 ) ) ;
#15343 = CARTESIAN_POINT ( 'NONE',  ( 23.60754984838813186, -10.12980629292501078, -9.622309725513526146 ) ) ;
#15344 = CARTESIAN_POINT ( 'NONE',  ( 9.465106464520001595, 2.290037071913000322, 6.601704384062999864 ) ) ;
#15345 = CARTESIAN_POINT ( 'NONE',  ( 11.13880513895979973, -2.849548954067000039, 8.139542779846600240 ) ) ;
#15346 = CARTESIAN_POINT ( 'NONE',  ( 8.771960841230001193, 3.061731693614000438, -8.535706278603999664 ) ) ;
#15347 = AXIS2_PLACEMENT_3D ( 'NONE', #6776, #28114, #49425 ) ;
#15348 = CARTESIAN_POINT ( 'NONE',  ( 10.85467598778999943, 9.827440234331000113, -5.589530524231999919 ) ) ;
#15349 = CARTESIAN_POINT ( 'NONE',  ( 24.37899127803200372, 8.840620920327999954, 8.761547301204000604 ) ) ;
#15350 = CARTESIAN_POINT ( 'NONE',  ( 10.83837003704316615, 5.765189909578217531, -7.466044055516256606 ) ) ;
#15351 = CARTESIAN_POINT ( 'NONE',  ( 11.60000000000000320, 4.738901876697420690, -8.470724288896152032 ) ) ;
#15352 = CARTESIAN_POINT ( 'NONE',  ( 10.44079719460000000, 5.435719122931000236, 7.303631812894000319 ) ) ;
#15353 = AXIS2_PLACEMENT_3D ( 'NONE', #68266, #43360, #6631 ) ;
#15354 = LINE ( 'NONE', #5196, #60107 ) ;
#15355 = EDGE_CURVE ( 'NONE', #8263, #39811, #48635, .T. ) ;
#15356 = ORIENTED_EDGE ( 'NONE', *, *, #61114, .T. ) ;
#15357 = CARTESIAN_POINT ( 'NONE',  ( 8.581920280410001212, 4.769017407621999993, -8.862909124839001507 ) ) ;
#15358 = CARTESIAN_POINT ( 'NONE',  ( 3.799999782336999754, 0.000000000000000000, 0.000000000000000000 ) ) ;
#15359 = FACE_OUTER_BOUND ( 'NONE', #29763, .T. ) ;
#15360 = CARTESIAN_POINT ( 'NONE',  ( 3.479247788823166321, 3.398203023142295720, -0.9541934759467685101 ) ) ;
#15361 = CARTESIAN_POINT ( 'NONE',  ( 24.67921580255100267, 8.727633792449999817, 9.158312800479000870 ) ) ;
#15362 = CARTESIAN_POINT ( 'NONE',  ( 11.62994988689359843, -3.481863023525599843, -8.516279404258998653 ) ) ;
#15363 = ORIENTED_EDGE ( 'NONE', *, *, #50107, .T. ) ;
#15364 = CARTESIAN_POINT ( 'NONE',  ( 4.500000000000000000, -3.200000000000000178, 0.000000000000000000 ) ) ;
#15365 = CARTESIAN_POINT ( 'NONE',  ( 13.99999999379500082, 8.815218614167999789, 7.616697584347000394 ) ) ;
#15367 = CARTESIAN_POINT ( 'NONE',  ( 7.614999999996999946, 5.349999999999999645, -7.500000000000000000 ) ) ;
#15366 = CARTESIAN_POINT ( 'NONE',  ( 9.021064158776001207, 4.883347899767999323, -6.417062834774999835 ) ) ;
#15368 = CARTESIAN_POINT ( 'NONE',  ( 18.16732611103527617, -2.625479214373699133, 13.64604457671237014 ) ) ;
#15369 = ORIENTED_EDGE ( 'NONE', *, *, #43595, .F. ) ;
#15370 = CARTESIAN_POINT ( 'NONE',  ( 10.57224177473000104, 4.020426023752999178, 8.920668579831000145 ) ) ;
#15371 = CARTESIAN_POINT ( 'NONE',  ( 17.98404385246625381, -2.954974373217228667, -13.56632247660221324 ) ) ;
#15372 = CARTESIAN_POINT ( 'NONE',  ( 10.65364694612719809, 3.195501139158400061, 7.178938988280099132 ) ) ;
#15373 = CARTESIAN_POINT ( 'NONE',  ( 11.09392659058396724, -2.706073409412732111, 6.603326177236545469 ) ) ;
#15374 = CARTESIAN_POINT ( 'NONE',  ( 8.796581853210000190, -2.368260286481999710, 7.410200011629000549 ) ) ;
#15375 = ORIENTED_EDGE ( 'NONE', *, *, #26608, .F. ) ;
#15376 = CARTESIAN_POINT ( 'NONE',  ( 9.342517219591000455, 5.057081813675999626, 8.967637988488998957 ) ) ;
#15377 = AXIS2_PLACEMENT_3D ( 'NONE', #21583, #37670, #64226 ) ;
#15378 = B_SPLINE_CURVE_WITH_KNOTS ( 'NONE', 3,
 ( #50812, #40654, #3254, #61637 ),
 .UNSPECIFIED., .F., .F.,
 ( 4, 4 ),
 ( 0.8745717919976516708, 1.000000000000000000 ),
 .UNSPECIFIED. ) ;
#15380 = CARTESIAN_POINT ( 'NONE',  ( 10.55478570706233299, -2.868293641868291388, -8.113400509224881318 ) ) ;
#15379 = CARTESIAN_POINT ( 'NONE',  ( 10.20448674122262211, -2.648429362731085757, 7.853061647121137412 ) ) ;
#15381 = CARTESIAN_POINT ( 'NONE',  ( 7.485254293485687604, -2.429645980366736957, 6.751440798236062690 ) ) ;
#15382 = TOROIDAL_SURFACE ( 'NONE', #3098, 10.75000000000000000, 1.500000000000000000 ) ;
#15383 = CARTESIAN_POINT ( 'NONE',  ( 18.18005043853800373, -0.02024535602757234626, 13.89999992471014245 ) ) ;
#15384 = CARTESIAN_POINT ( 'NONE',  ( 24.22085374770700028, 3.760945907258999465, 12.77833517530000051 ) ) ;
#15385 = ORIENTED_EDGE ( 'NONE', *, *, #22188, .F. ) ;
#15386 = CARTESIAN_POINT ( 'NONE',  ( 9.435596873515667227, 2.907767014557176566, -8.129523725463622341 ) ) ;
#15387 = CARTESIAN_POINT ( 'NONE',  ( 11.22749279009020107, -4.225282629687599822, 6.663611138821799784 ) ) ;
#15388 = CARTESIAN_POINT ( 'NONE',  ( 10.02991192131000098, 2.506457833269999824, 6.215406506815000398 ) ) ;
#15389 = CARTESIAN_POINT ( 'NONE',  ( 11.09647882763000126, 3.099775370665000196, 6.097099813297999660 ) ) ;
#15390 = AXIS2_PLACEMENT_3D ( 'NONE', #41164, #51303, #57571 ) ;
#15391 = CARTESIAN_POINT ( 'NONE',  ( 10.49764694612699856, 2.940513484064000149, 7.077178005756699974 ) ) ;
#15392 = ORIENTED_EDGE ( 'NONE', *, *, #26124, .F. ) ;
#15393 = CARTESIAN_POINT ( 'NONE',  ( 10.92799928937301246, 5.127999289373012637, -6.526892970107653014 ) ) ;
#15394 = VECTOR ( 'NONE', #24651, 1000.000000000000000 ) ;
#15395 = CARTESIAN_POINT ( 'NONE',  ( 24.39664803136666649, 12.09373379607674082, 3.240506204136868185 ) ) ;
#15396 = EDGE_CURVE ( 'NONE', #36962, #64274, #4217, .T. ) ;
#15397 = CARTESIAN_POINT ( 'NONE',  ( 12.47602583993311498, -1.943637617989338651, 12.56471729223352085 ) ) ;
#15398 = EDGE_CURVE ( 'NONE', #61732, #9405, #23619, .T. ) ;
#15399 = CARTESIAN_POINT ( 'NONE',  ( 25.29574788798400320, -2.995621132715000190, -11.41693952213999985 ) ) ;
#15400 = AXIS2_PLACEMENT_3D ( 'NONE', #62148, #55882, #50290 ) ;
#15401 = CARTESIAN_POINT ( 'NONE',  ( 18.05353730554815428, -1.987694103345771568, 13.85817950142401855 ) ) ;
#15402 = CARTESIAN_POINT ( 'NONE',  ( 10.37902717885611636, -2.650237472149363338, -7.263327126957014990 ) ) ;
#15403 = EDGE_LOOP ( 'NONE', ( #43688, #24286, #40641, #27438 ) ) ;
#15404 = DIRECTION ( 'NONE',  ( 1.000000000000000000, 0.000000000000000000, 0.000000000000000000 ) ) ;
#15405 = CARTESIAN_POINT ( 'NONE',  ( 9.272783876522375124, -4.789858247946766845, -6.518107589053542483 ) ) ;
#15406 = EDGE_LOOP ( 'NONE', ( #52543, #40066, #51720, #18654, #29518 ) ) ;
#15407 = CARTESIAN_POINT ( 'NONE',  ( 15.90018573812067260, 7.083264066697978478, 9.547770387690125204 ) ) ;
#15408 = CARTESIAN_POINT ( 'NONE',  ( 10.93727498060999892, 5.425427353909999972, 7.240585962396000497 ) ) ;
#15409 = CARTESIAN_POINT ( 'NONE',  ( 10.07930935222999835, 2.718121894972999719, -6.397795030233000446 ) ) ;
#15410 = CARTESIAN_POINT ( 'NONE',  ( 8.500383147356993518, 5.097359707274998541, 6.605634423517003029 ) ) ;
#15411 = CARTESIAN_POINT ( 'NONE',  ( 9.889844610056000462, -4.052276314598000084, 9.260527932809999641 ) ) ;
#15412 = CARTESIAN_POINT ( 'NONE',  ( 17.57898592363196855, -0.7189971323194248587, -12.57946912511937754 ) ) ;
#15413 = CARTESIAN_POINT ( 'NONE',  ( 12.28979759248826298, 2.853877291412238559, -12.36206589979061832 ) ) ;
#15414 = CARTESIAN_POINT ( 'NONE',  ( 11.60533460557258323, -3.815825449682300086, -8.625775273268001087 ) ) ;
#15415 = CARTESIAN_POINT ( 'NONE',  ( 7.443295280410000103, 4.698356649019999942, 8.789431186081998248 ) ) ;
#15416 = ORIENTED_EDGE ( 'NONE', *, *, #23182, .F. ) ;
#15417 = EDGE_CURVE ( 'NONE', #7173, #17632, #4731, .T. ) ;
#15418 = CARTESIAN_POINT ( 'NONE',  ( 25.29986734212600297, -2.596989636639000398, 11.35306351421000137 ) ) ;
#15419 = LINE ( 'NONE', #33565, #4813 ) ;
#15420 = CARTESIAN_POINT ( 'NONE',  ( 8.477766462057999775, 2.899999999999999911, -6.558719934578999933 ) ) ;
#15421 = EDGE_CURVE ( 'NONE', #7028, #33691, #43298, .T. ) ;
#15422 = CARTESIAN_POINT ( 'NONE',  ( 9.825984992304002574, 8.538414651508006159, 6.566328153291997261 ) ) ;
#15423 = CARTESIAN_POINT ( 'NONE',  ( 12.57019395242807036, 1.827067495629551841, 13.88026806835660842 ) ) ;
#15424 = CARTESIAN_POINT ( 'NONE',  ( 9.353731048338000065, -2.823575173856999410, 9.032043499493001448 ) ) ;
#15425 = CARTESIAN_POINT ( 'NONE',  ( 10.90000037895999796, 0.2999996193951000034, 9.776630289319001577 ) ) ;
#15426 = CARTESIAN_POINT ( 'NONE',  ( 25.46373154986600085, 8.354608910739999672, 8.148450287869000164 ) ) ;
#15427 = ORIENTED_EDGE ( 'NONE', *, *, #49837, .F. ) ;
#15428 = CARTESIAN_POINT ( 'NONE',  ( 12.41909388474796216, -1.871095411850187018, 12.46029856231474930 ) ) ;
#15429 = CARTESIAN_POINT ( 'NONE',  ( 9.076468108405999047, -2.769196120524999749, -7.848577323721800170 ) ) ;
#15430 = DIRECTION ( 'NONE',  ( -0.7071067811865474617, -0.7071067811865474617, 6.440236212535425163E-09 ) ) ;
#15431 = CARTESIAN_POINT ( 'NONE',  ( 9.414314870535999802, -3.941041813398000304, 5.878346364186999295 ) ) ;
#15432 = CARTESIAN_POINT ( 'NONE',  ( 11.64595257254739913, -4.831736303435800295, 7.258104750172799768 ) ) ;
#15433 = B_SPLINE_CURVE_WITH_KNOTS ( 'NONE', 3,
 ( #33354, #34397, #23890, #65493 ),
 .UNSPECIFIED., .F., .F.,
 ( 4, 4 ),
 ( 0.000000000000000000, 1.000000000000000000 ),
 .UNSPECIFIED. ) ;
#15434 = CARTESIAN_POINT ( 'NONE',  ( 12.10797143991212010, 0.1980440493285337555, 12.59844852634975787 ) ) ;
#15435 = CARTESIAN_POINT ( 'NONE',  ( 7.533885841228999958, 4.623631324973000112, 8.651459902566999816 ) ) ;
#15436 = CARTESIAN_POINT ( 'NONE',  ( 9.616863785686895483, 5.079232767740477605, -8.329457163983990498 ) ) ;
#15437 = VECTOR ( 'NONE', #50613, 1000.000000000000114 ) ;
#15438 = CARTESIAN_POINT ( 'NONE',  ( 12.12868457208159789, 2.220738826795316090, 12.40275942113247964 ) ) ;
#15439 = CARTESIAN_POINT ( 'NONE',  ( 11.09999999999999964, 2.700000000000000178, -5.160242730539000178 ) ) ;
#15440 = CARTESIAN_POINT ( 'NONE',  ( 11.46179707368349909, 3.501542828836900156, -6.629085939160999530 ) ) ;
#15441 = CARTESIAN_POINT ( 'NONE',  ( 12.41307909110098429, 11.56466389787666493, -4.809819853923482214 ) ) ;
#15442 = CARTESIAN_POINT ( 'NONE',  ( 9.888314158772001150, 5.105193280231000053, -8.895607399415000671 ) ) ;
#15443 = CARTESIAN_POINT ( 'NONE',  ( 8.921417874593998931, 2.822750429186000165, -8.000467616829000761 ) ) ;
#15445 = CARTESIAN_POINT ( 'NONE',  ( 12.19222608798534502, 2.622765415552483770, 12.42211422047175517 ) ) ;
#15444 = CARTESIAN_POINT ( 'NONE',  ( 9.951050468514374359, 5.324162572649938419, 7.941948203265592809 ) ) ;
#15446 = CARTESIAN_POINT ( 'NONE',  ( 8.082873386424997975, 5.111739203374999541, -6.679001318365999751 ) ) ;
#15447 = ORIENTED_EDGE ( 'NONE', *, *, #22783, .T. ) ;
#15448 = VECTOR ( 'NONE', #24237, 1000.000000000000114 ) ;
#15449 = CARTESIAN_POINT ( 'NONE',  ( 12.64261153913240499, 0.6049396497608361400, 12.68060203380711570 ) ) ;
#15450 = CARTESIAN_POINT ( 'NONE',  ( 10.18559687351583243, 5.092232985442825210, 8.129523725463618788 ) ) ;
#15451 = CARTESIAN_POINT ( 'NONE',  ( 10.25462442569999943, -2.860634389522000109, 6.604605425112000994 ) ) ;
#15452 = PRODUCT_RELATED_PRODUCT_CATEGORY ( 'part', '', ( #8728 ) ) ;
#15453 = CARTESIAN_POINT ( 'NONE',  ( 9.577013376692997682, 3.227076647348800176, 7.892807122431200639 ) ) ;
#15454 = CIRCLE ( 'NONE', #57870, 12.35000000006999876 ) ;
#15455 = PLANE ( 'NONE',  #66740 ) ;
#15456 = CARTESIAN_POINT ( 'NONE',  ( 12.27362767355647222, -2.829117748835542567, 13.59812893905842479 ) ) ;
#15457 = CARTESIAN_POINT ( 'NONE',  ( 12.20843209895684645, 2.686266380639721785, 13.63213492624170264 ) ) ;
#15458 = CARTESIAN_POINT ( 'NONE',  ( 8.154195026538843649, 3.087577394105698758, 6.292719520537814581 ) ) ;
#15459 = ORIENTED_EDGE ( 'NONE', *, *, #22950, .F. ) ;
#15460 = CARTESIAN_POINT ( 'NONE',  ( 4.671696543201000473, 1.240591757068000067, 0.2961542510987000276 ) ) ;
#15461 = CARTESIAN_POINT ( 'NONE',  ( 8.592138961223998450, -2.940105638081000006, -8.216246114996598848 ) ) ;
#15462 = DIRECTION ( 'NONE',  ( 1.000000000000000000, 1.776356839548999970E-14, 0.000000000000000000 ) ) ;
#15463 = CARTESIAN_POINT ( 'NONE',  ( 10.97769598648999967, -2.990523684589000197, 6.898940957443399746 ) ) ;
#15464 = CARTESIAN_POINT ( 'NONE',  ( 17.98432920965424131, 2.954704375608638411, -12.33394473884602149 ) ) ;
#15465 = CARTESIAN_POINT ( 'NONE',  ( 8.587232097456750424, 5.014137595553737725, 6.171797112031566002 ) ) ;
#15466 = CARTESIAN_POINT ( 'NONE',  ( 17.81530815051377203, 3.068584091763893795, 12.30073186569319610 ) ) ;
#15467 = CARTESIAN_POINT ( 'NONE',  ( 17.65076761721691057, 3.243341803239792487, 13.61913462217096260 ) ) ;
#15469 = CARTESIAN_POINT ( 'NONE',  ( 9.663906509039998483, -2.491831134779999957, -6.388915175267000812 ) ) ;
#15468 = B_SPLINE_CURVE_WITH_KNOTS ( 'NONE', 3,
 ( #47261, #47608, #42017, #5289 ),
 .UNSPECIFIED., .F., .F.,
 ( 4, 4 ),
 ( 0.8163836489557156906, 1.000000000000000000 ),
 .UNSPECIFIED. ) ;
#15470 = CARTESIAN_POINT ( 'NONE',  ( 10.60770805961999841, -2.392337812398999564, -6.587351599745000286 ) ) ;
#15471 = DIRECTION ( 'NONE',  ( 1.000000000000000000, 0.000000000000000000, 0.000000000000000000 ) ) ;
#15472 = CARTESIAN_POINT ( 'NONE',  ( 0.07500022993665000914, 0.000000000000000000, 0.000000000000000000 ) ) ;
#15473 = CARTESIAN_POINT ( 'NONE',  ( 24.01983374632887092, 9.335054998824150019, -9.252342060729551676 ) ) ;
#15474 = EDGE_CURVE ( 'NONE', #55934, #2412, #52847, .T. ) ;
#15475 = CARTESIAN_POINT ( 'NONE',  ( 24.30000000000000071, -8.810505093353000916, 8.810505093353000916 ) ) ;
#15476 = ADVANCED_FACE ( 'NONE', ( #42501 ), #10331, .T. ) ;
#15477 = FACE_OUTER_BOUND ( 'NONE', #58993, .T. ) ;
#15478 = VERTEX_POINT ( 'NONE', #32361 ) ;
#15479 = CARTESIAN_POINT ( 'NONE',  ( 8.863029719594999634, 2.990001567622999623, -8.695425648791999862 ) ) ;
#15480 = CARTESIAN_POINT ( 'NONE',  ( 10.79262282008599882, -3.548418513060800361, 6.771613406921599854 ) ) ;
#15481 = ORIENTED_EDGE ( 'NONE', *, *, #26841, .T. ) ;
#15482 = DIRECTION ( 'NONE',  ( 0.000000000000000000, -0.8648648648648717963, 0.5020047465136829867 ) ) ;
#15483 = CARTESIAN_POINT ( 'NONE',  ( 11.30579707368350029, -4.634832087857400751, -6.390809033205999690 ) ) ;
#15484 = ORIENTED_EDGE ( 'NONE', *, *, #4642, .F. ) ;
#15485 = CARTESIAN_POINT ( 'NONE',  ( 11.18412378248529926, 3.450971646934100079, 8.538714411016998795 ) ) ;
#15486 = DIRECTION ( 'NONE',  ( 0.000000000000000000, -1.000000000000000000, 0.000000000000000000 ) ) ;
#15487 = CYLINDRICAL_SURFACE ( 'NONE', #4085, 0.6999999999999992895 ) ;
#15488 = CARTESIAN_POINT ( 'NONE',  ( 10.39969598649000027, -3.111999510220800236, -8.028730309000598808 ) ) ;
#15489 = CARTESIAN_POINT ( 'NONE',  ( 12.41737190959485382, 0.4903666734152603013, -13.88835870177955378 ) ) ;
#15490 = CARTESIAN_POINT ( 'NONE',  ( 18.18005044388380043, 2.499999700417821380, 12.45156116530496604 ) ) ;
#15491 = CIRCLE ( 'NONE', #54559, 2.200000000000001066 ) ;
#15492 = CARTESIAN_POINT ( 'NONE',  ( 8.099999999999999645, 11.84999999999999964, 0.000000000000000000 ) ) ;
#15493 = ORIENTED_EDGE ( 'NONE', *, *, #36840, .T. ) ;
#15494 = CARTESIAN_POINT ( 'NONE',  ( 13.94794651623100101, 9.527030574842997979, 8.190375113092999371 ) ) ;
#15495 = CARTESIAN_POINT ( 'NONE',  ( 9.626145280412998773, 3.934138271021000222, -9.063586117809000697 ) ) ;
#15496 = ORIENTED_EDGE ( 'NONE', *, *, #38032, .F. ) ;
#15497 = CARTESIAN_POINT ( 'NONE',  ( 10.47212119989999835, 2.640756834784999896, -8.505248851866998194 ) ) ;
#15498 = ORIENTED_EDGE ( 'NONE', *, *, #20682, .T. ) ;
#15499 = CARTESIAN_POINT ( 'NONE',  ( 9.200038493598999167, 4.925784867300699865, 8.382783533462799141 ) ) ;
#15500 = CARTESIAN_POINT ( 'NONE',  ( 18.17921332558109881, -2.461874964459676907, -12.46038192087330820 ) ) ;
#15501 = EDGE_CURVE ( 'NONE', #4646, #12348, #37588, .T. ) ;
#15502 = LINE ( 'NONE', #31584, #42996 ) ;
#15503 = B_SPLINE_SURFACE_WITH_KNOTS ( 'NONE', 3, 3, ( 
 ( #60766, #34896, #49934, #66001, #13574, #8321, #19145, #40466, #24397, #45727, #12187, #33516, #54832, #6931, #1693, #44360, #18125, #2045, #65660, #39101, #12531, #33862, #55177, #39445, #57574, #15281, #25077, #4086, #30006, #52336, #63152, #40813, #56555, #14256, #46411 ),
 ( #56897, #62473, #67712, #26114, #20174, #9329, #19838, #35583, #41501, #68397, #62137, #36604, #62814, #9677, #8996, #68059, #10027, #31027, #4430, #25768, #25422, #47442, #57930, #41168, #35914, #30674, #3742, #31366, #52677, #47097, #20520, #30338, #57229, #14933, #4772 ),
 ( #41846, #68748, #14595, #51645, #36257, #20865, #67371, #8659, #51980, #46756, #61797, #13914, #35241, #51308, #3405, #24739, #46066, #19496, #64875, #32399, #43575, #64528, #54054, #11065, #43223, #21546, #16302, #63504, #6502, #16987, #22237, #6151, #31708, #10711, #63847 ),
 ( #64189, #15623, #42203, #37973, #53029, #925, #59645, #11744, #59295, #58268, #27492, #5125, #21205, #37627, #53374, #33086, #26811, #42882, #38317, #32058, #48125, #16647, #48472, #49154, #27847, #53714, #48817, #1266, #11398, #54402, #579, #10370, #26462, #230, #58610 ) ),
 .UNSPECIFIED., .F., .F., .F.,
 ( 4, 4 ),
 ( 4, 1, 1, 1, 1, 1, 1, 1, 1, 1, 1, 1, 1, 1, 1, 1, 1, 1, 1, 1, 1, 1, 1, 1, 1, 1, 1, 1, 1, 1, 1, 1, 4 ),
 ( -0.02000000000000000042, 1.020000000000000018 ),
 ( 0.1633025096610999927, 0.1899619885200000136, 0.2166214673788000034, 0.2432809462376999965, 0.2699404250964999585, 0.2965999039553000038, 0.3232593828141999692, 0.3499188616730000145, 0.3765783405318000043, 0.4032378193906999697, 0.4298972982494999595, 0.4565567771083000048, 0.4832162559671999702, 0.5098757348260000155, 0.5365352136848999809, 0.5631946925437000262, 0.5898541714025000715, 0.6165136502614000369, 0.6431731291201999712, 0.6698326079790000165, 0.6964920868378999819, 0.7231515656967000272, 0.7498110445554999615, 0.7764705234143999268, 0.8031300022731999722, 0.8297894811320000175, 0.8564489599908999828, 0.8831084388497000282, 0.9097679177085999935, 0.9364273965674000388, 0.9630868754261999731, 0.9897463542851000495, 1.016405833144000015 ),
 .UNSPECIFIED. ) ;
#15504 = CARTESIAN_POINT ( 'NONE',  ( 3.799999782336999754, 0.000000000000000000, 0.000000000000000000 ) ) ;
#15505 = CARTESIAN_POINT ( 'NONE',  ( 13.86904166957592999, -8.833215535550223763, -7.896538540699776121 ) ) ;
#15506 = ORIENTED_EDGE ( 'NONE', *, *, #38048, .T. ) ;
#15507 = CARTESIAN_POINT ( 'NONE',  ( 12.32697677577000128, 11.50538345640999971, -4.553133914476999777 ) ) ;
#15508 = CARTESIAN_POINT ( 'NONE',  ( 17.75588107601699761, 11.55446208650999829, -4.935524324464999779 ) ) ;
#15509 = CIRCLE ( 'NONE', #54583, 12.50000000000000000 ) ;
#15510 = DIRECTION ( 'NONE',  ( 1.000000000000000000, 0.000000000000000000, 0.000000000000000000 ) ) ;
#15511 = CARTESIAN_POINT ( 'NONE',  ( 8.883506238772763908, 4.136150106583479591, 8.533506295447224943 ) ) ;
#15512 = CARTESIAN_POINT ( 'NONE',  ( 9.933354719590999693, 5.639765292528999829, -8.059103558718000215 ) ) ;
#15513 = CARTESIAN_POINT ( 'NONE',  ( 18.44330693167099966, -2.998553466420000202, 12.10578145104000036 ) ) ;
#15514 = CARTESIAN_POINT ( 'NONE',  ( 10.05525937050999907, -5.223866772223000332, -6.898311956607000361 ) ) ;
#15515 = ORIENTED_EDGE ( 'NONE', *, *, #54614, .T. ) ;
#15516 = ORIENTED_EDGE ( 'NONE', *, *, #26439, .F. ) ;
#15517 = CARTESIAN_POINT ( 'NONE',  ( 10.91165258067000110, 5.022850734190000388, -4.913708377245000314 ) ) ;
#15518 = CARTESIAN_POINT ( 'NONE',  ( 25.60000000000000142, -8.131727983644998048, 8.131727983644998048 ) ) ;
#15519 = CARTESIAN_POINT ( 'NONE',  ( 5.805026506351000037, 1.500000000000000000, 0.000000000000000000 ) ) ;
#15520 = CARTESIAN_POINT ( 'NONE',  ( 6.094609839683333696, -1.500000000000000888, 0.1963495408493559080 ) ) ;
#15521 = CARTESIAN_POINT ( 'NONE',  ( 11.68277869730536977, 3.468607053297499743, -6.452143920160000157 ) ) ;
#15522 = CARTESIAN_POINT ( 'NONE',  ( 8.902126402770997871, 4.811247217215600003, -7.194081880505399873 ) ) ;
#15524 = CARTESIAN_POINT ( 'NONE',  ( 4.399720353966697139, 0.5971468265269567199, -1.134349138418559999 ) ) ;
#15523 = CARTESIAN_POINT ( 'NONE',  ( 10.68692546752099837, -5.002009261081000524, 7.569424354486659290 ) ) ;
#15525 = CARTESIAN_POINT ( 'NONE',  ( 4.700859839683333874, 0.3926218265389221362, -1.460959015002473160 ) ) ;
#15526 = ORIENTED_EDGE ( 'NONE', *, *, #8629, .F. ) ;
#15527 = CARTESIAN_POINT ( 'NONE',  ( 25.00275061277693567, -11.89252591243665869, 2.924339798584659977 ) ) ;
#15528 = CARTESIAN_POINT ( 'NONE',  ( 10.35303240674999969, -3.419511749372000420, -4.861886959447999423 ) ) ;
#15529 = EDGE_CURVE ( 'NONE', #64582, #52126, #33225, .T. ) ;
#15530 = EDGE_CURVE ( 'NONE', #28381, #10297, #51096, .T. ) ;
#15531 = CARTESIAN_POINT ( 'NONE',  ( 10.46957120343300041, 3.937990586507050139, 6.222291352336999815 ) ) ;
#15532 = PLANE ( 'NONE',  #39193 ) ;
#15533 = CIRCLE ( 'NONE', #19984, 0.3000000000000000444 ) ;
#15534 = CARTESIAN_POINT ( 'NONE',  ( 9.566960887370999700, -5.215923019114000247, 6.177729435798999802 ) ) ;
#15535 = CARTESIAN_POINT ( 'NONE',  ( 18.14658900067671965, 2.701839613031566500, -12.40227423856772582 ) ) ;
#15536 = FACE_OUTER_BOUND ( 'NONE', #30790, .T. ) ;
#15537 = CARTESIAN_POINT ( 'NONE',  ( 15.79991751193277416, -9.060349897821465603, -8.357793075677504291 ) ) ;
#15538 = CARTESIAN_POINT ( 'NONE',  ( 7.945634795641004722, 2.916734013644262991, -6.617471303626205170 ) ) ;
#15539 = CARTESIAN_POINT ( 'NONE',  ( 10.21722949779699974, -3.442773960835399993, -8.335668797826500054 ) ) ;
#15540 = DIRECTION ( 'NONE',  ( 0.000000000000000000, 0.000000000000000000, -1.000000000000000000 ) ) ;
#15541 = CARTESIAN_POINT ( 'NONE',  ( 10.83103907547008227, -3.225837863097585689, 7.100484084056944312 ) ) ;
#15542 = CARTESIAN_POINT ( 'NONE',  ( 5.644459969794759502, 12.96885562310360029, -2.321858018549519453 ) ) ;
#15543 = CARTESIAN_POINT ( 'NONE',  ( 7.744301838472999577, -3.130384865731000055, 6.467396727560999814 ) ) ;
#15544 = ORIENTED_EDGE ( 'NONE', *, *, #4163, .T. ) ;
#15545 = CARTESIAN_POINT ( 'NONE',  ( 12.19636936301369978, -0.1422617729927582730, -12.69893308522357422 ) ) ;
#15546 = CARTESIAN_POINT ( 'NONE',  ( 5.200000000000000178, -1.376649746192999846, -11.21582968292000082 ) ) ;
#15547 = CARTESIAN_POINT ( 'NONE',  ( 5.399999746777999654, -12.99045401563999924, 1.690592933733000125 ) ) ;
#15548 = DIRECTION ( 'NONE',  ( -1.000000000000000000, 0.000000000000000000, 0.000000000000000000 ) ) ;
#15549 = CARTESIAN_POINT ( 'NONE',  ( 11.09999999999999964, -2.649999999999999911, 7.500000000000000000 ) ) ;
#15550 = ORIENTED_EDGE ( 'NONE', *, *, #8958, .T. ) ;
#15551 = FACE_OUTER_BOUND ( 'NONE', #48447, .T. ) ;
#15552 = DIRECTION ( 'NONE',  ( 0.000000000000000000, 0.000000000000000000, 1.000000000000000000 ) ) ;
#15553 = CARTESIAN_POINT ( 'NONE',  ( 10.80502344389999791, -5.125258734743999511, -6.817099149379099110 ) ) ;
#15554 = EDGE_CURVE ( 'NONE', #20236, #36843, #12861, .T. ) ;
#15555 = CARTESIAN_POINT ( 'NONE',  ( 24.30001680216799897, -3.271769318036999774, 12.21048166890999909 ) ) ;
#15556 = CARTESIAN_POINT ( 'NONE',  ( 17.55505043854144276, 0.6250000000000001110, -12.67928921589118474 ) ) ;
#15557 = CARTESIAN_POINT ( 'NONE',  ( 11.49999672494999636, -10.70720904779669524, 4.749689352253898988 ) ) ;
#15558 = CARTESIAN_POINT ( 'NONE',  ( 11.59603632436369125, 3.157359628034400068, -7.303218851299499548 ) ) ;
#15559 = VERTEX_POINT ( 'NONE', #22755 ) ;
#15560 = EDGE_CURVE ( 'NONE', #60354, #46704, #66216, .T. ) ;
#15561 = B_SPLINE_CURVE_WITH_KNOTS ( 'NONE', 3,
 ( #8833, #30174, #56389, #61975, #33430 ),
 .UNSPECIFIED., .F., .F.,
 ( 4, 1, 4 ),
 ( 0.000000000000000000, 0.5000000000000000000, 1.000000000000000000 ),
 .UNSPECIFIED. ) ;
#15562 = CARTESIAN_POINT ( 'NONE',  ( 10.11260824411999870, -3.359889198679999911, 5.859131457670000209 ) ) ;
#15563 = EDGE_LOOP ( 'NONE', ( #55049, #54617, #31300, #7131, #18405, #43010, #8824, #43981 ) ) ;
#15564 = CARTESIAN_POINT ( 'NONE',  ( 11.03879883359000047, -2.753595124514999881, 5.027017047203000466 ) ) ;
#15565 = CARTESIAN_POINT ( 'NONE',  ( 7.839808059622000336, -3.084082018960999871, 9.259837032825000591 ) ) ;
#15566 = DIRECTION ( 'NONE',  ( -1.000000000000000000, 0.000000000000000000, 0.000000000000000000 ) ) ;
#15567 = EDGE_LOOP ( 'NONE', ( #61818, #30775, #47169, #3101, #37045 ) ) ;
#15568 = CARTESIAN_POINT ( 'NONE',  ( 8.514905693275615306, 2.973706675831895740, -8.924953531459744127 ) ) ;
#15569 = CARTESIAN_POINT ( 'NONE',  ( 7.093264158770000272, 5.397217548590999669, -7.528974776547999959 ) ) ;
#15570 = CARTESIAN_POINT ( 'NONE',  ( 18.50003594170800270, 2.686563649653999963, -11.33603604535000109 ) ) ;
#15571 = CARTESIAN_POINT ( 'NONE',  ( 9.477173644534087060, 5.064627895235314980, 8.332423391400503476 ) ) ;
#15572 = ORIENTED_EDGE ( 'NONE', *, *, #7426, .F. ) ;
#15573 = CARTESIAN_POINT ( 'NONE',  ( 9.815199780373001559, -2.813634733202999616, 8.848854270764999086 ) ) ;
#15574 = CARTESIAN_POINT ( 'NONE',  ( 10.86123236735334530, 5.100000000000000533, -6.348362623949493688 ) ) ;
#15575 = CARTESIAN_POINT ( 'NONE',  ( 9.551300837857858994, -2.809882456706737308, 7.276433888703319752 ) ) ;
#15576 = ORIENTED_EDGE ( 'NONE', *, *, #21563, .F. ) ;
#15577 = CARTESIAN_POINT ( 'NONE',  ( 10.98768472633000037, -6.720753151621999599, -5.471698430863999540 ) ) ;
#15578 = ORIENTED_EDGE ( 'NONE', *, *, #61407, .T. ) ;
#15579 = CARTESIAN_POINT ( 'NONE',  ( 5.002606837613999602, -0.4199405305951999789, 1.440017343911000003 ) ) ;
#15580 = CARTESIAN_POINT ( 'NONE',  ( 10.64551289531389777, 5.370173726513001178, 6.373339187755826529 ) ) ;
#15581 = DIRECTION ( 'NONE',  ( -1.000000000000000000, 0.000000000000000000, 0.000000000000000000 ) ) ;
#15582 = ADVANCED_FACE ( 'NONE', ( #48034 ), #55623, .T. ) ;
#15583 = DIRECTION ( 'NONE',  ( 0.000000000000000000, -1.000000000000000000, 0.000000000000000000 ) ) ;
#15584 = LINE ( 'NONE', #46716, #57611 ) ;
#15585 = CARTESIAN_POINT ( 'NONE',  ( 24.17844067670218777, 12.41761889074214587, 3.338210367410554991 ) ) ;
#15586 = CARTESIAN_POINT ( 'NONE',  ( 9.414763540182331525, -5.217465845835395299, -7.827184855449099921 ) ) ;
#15587 = VERTEX_POINT ( 'NONE', #2473 ) ;
#15588 = CARTESIAN_POINT ( 'NONE',  ( 10.40480513895999870, -3.220259576336399920, -7.066537524675499782 ) ) ;
#15589 = ORIENTED_EDGE ( 'NONE', *, *, #68553, .F. ) ;
#15590 = CARTESIAN_POINT ( 'NONE',  ( 9.388624299788999039, 4.079402096444999515, 9.259357173634999327 ) ) ;
#15591 = CARTESIAN_POINT ( 'NONE',  ( 11.07691721959000120, 3.101894630379999906, -8.926552937604000704 ) ) ;
#15592 = PLANE ( 'NONE',  #7292 ) ;
#15593 = CARTESIAN_POINT ( 'NONE',  ( 12.32580140628882681, 2.098690126660239130, -13.75042779764526735 ) ) ;
#15594 = DIRECTION ( 'NONE',  ( -0.1218403629891999795, -1.031102291695999760E-07, 0.9925497095595008368 ) ) ;
#15595 = FACE_OUTER_BOUND ( 'NONE', #3081, .T. ) ;
#15596 = CARTESIAN_POINT ( 'NONE',  ( 18.14706097348721414, 0.2014071429975164695, 13.89805485625563541 ) ) ;
#15597 = CARTESIAN_POINT ( 'NONE',  ( 18.17614081693745121, 0.08113699202310993563, 13.89976078941035631 ) ) ;
#15598 = ORIENTED_EDGE ( 'NONE', *, *, #36861, .F. ) ;
#15599 = CARTESIAN_POINT ( 'NONE',  ( 5.000000000000000000, 1.800000000000000044, 0.000000000000000000 ) ) ;
#15600 = CARTESIAN_POINT ( 'NONE',  ( 11.14118447801630118, -2.722297859592000435, 7.528171279442569919 ) ) ;
#15601 = DIRECTION ( 'NONE',  ( 1.000000000000000000, 0.000000000000000000, 1.736057635219000097E-14 ) ) ;
#15602 = CARTESIAN_POINT ( 'NONE',  ( 7.100000000000000533, -13.17499999999999893, -1.613472157876637865E-15 ) ) ;
#15603 = CARTESIAN_POINT ( 'NONE',  ( 8.052730646792999991, -4.968144979409999884, 5.971795951526999602 ) ) ;
#15604 = CIRCLE ( 'NONE', #21188, 1.000000000000000000 ) ;
#15606 = CARTESIAN_POINT ( 'NONE',  ( 12.56936319533972757, 3.210092459268786946, -13.62701963584631848 ) ) ;
#15605 = CARTESIAN_POINT ( 'NONE',  ( 10.44079719460000000, 5.435719122931000236, 7.303631812894000319 ) ) ;
#15607 = CARTESIAN_POINT ( 'NONE',  ( 10.84226088462129844, 4.002427228022017225, -6.359261544073000039 ) ) ;
#15608 = CARTESIAN_POINT ( 'NONE',  ( 25.48313768079200159, -11.09944635839999982, 3.317483465242999863 ) ) ;
#15609 = CARTESIAN_POINT ( 'NONE',  ( 9.551684229509998403, 3.388828644390000200, -6.885038603985500494 ) ) ;
#15610 = ADVANCED_FACE ( 'NONE', ( #34300 ), #65376, .F. ) ;
#15611 = EDGE_CURVE ( 'NONE', #47809, #16477, #16187, .T. ) ;
#15612 = CARTESIAN_POINT ( 'NONE',  ( 18.27048529734872773, 0.1170514037749867675, 12.59946170170351643 ) ) ;
#15613 = CARTESIAN_POINT ( 'NONE',  ( 7.173029500063999642, 0.5195473280092000046, 1.006186743336999978 ) ) ;
#15614 = CARTESIAN_POINT ( 'NONE',  ( 23.86819263930300394, 9.630286858308998887, 9.781782771855001002 ) ) ;
#15615 = VERTEX_POINT ( 'NONE', #2136 ) ;
#15616 = CARTESIAN_POINT ( 'NONE',  ( 7.583058059622000080, -4.763531818439999732, 5.668890958491999754 ) ) ;
#15617 = CARTESIAN_POINT ( 'NONE',  ( 9.708354719591000048, 5.481267232667000222, -8.005061172455999241 ) ) ;
#15618 = EDGE_CURVE ( 'NONE', #33463, #56577, #24496, .T. ) ;
#15619 = CARTESIAN_POINT ( 'NONE',  ( 6.899999691988000450, -13.87069231928999891, -4.225386915259999654 ) ) ;
#15620 = LINE ( 'NONE', #21886, #36750 ) ;
#15621 = VERTEX_POINT ( 'NONE', #55275 ) ;
#15622 = CARTESIAN_POINT ( 'NONE',  ( 10.70920446231090040, 2.899999999999999911, 6.662590550528270761 ) ) ;
#15623 = CARTESIAN_POINT ( 'NONE',  ( 11.59603632436369125, 3.157359628034400068, 7.696781148700499564 ) ) ;
#15624 = CARTESIAN_POINT ( 'NONE',  ( 10.80374834123000127, 2.766954612461999918, -8.073381085840999560 ) ) ;
#15625 = VERTEX_POINT ( 'NONE', #18906 ) ;
#15626 = CARTESIAN_POINT ( 'NONE',  ( 9.143927823787141307, 5.249988444743199700, -7.499999844943244121 ) ) ;
#15627 = CARTESIAN_POINT ( 'NONE',  ( 17.65093748390281547, -3.195004315082954793, 12.18819265947264263 ) ) ;
#15628 = CARTESIAN_POINT ( 'NONE',  ( 10.98579841651039857, 3.550031058388499972, 6.303820944768999901 ) ) ;
#15629 = CARTESIAN_POINT ( 'NONE',  ( 7.152687255306670266, -3.171513860283114994, 8.579150755730465150 ) ) ;
#15630 = CARTESIAN_POINT ( 'NONE',  ( 8.464260841230998977, 2.029098103856999735, 7.726995416028000108 ) ) ;
#15631 = ORIENTED_EDGE ( 'NONE', *, *, #23684, .T. ) ;
#15632 = CARTESIAN_POINT ( 'NONE',  ( 17.55505043854144276, -0.7192913403693006469, 12.57945229203838444 ) ) ;
#15633 = CARTESIAN_POINT ( 'NONE',  ( 8.486229719590999920, 4.901484321470999994, -8.891682961388999829 ) ) ;
#15634 = CARTESIAN_POINT ( 'NONE',  ( 8.229919888127584571, -5.613417466181594762, 8.151383774938032900 ) ) ;
#15635 = CARTESIAN_POINT ( 'NONE',  ( 13.99999999485600277, 9.471999751521998689, 8.194948195317001804 ) ) ;
#15636 = ORIENTED_EDGE ( 'NONE', *, *, #1431, .F. ) ;
#15637 = DIRECTION ( 'NONE',  ( -1.000000000000000000, 0.000000000000000000, 0.000000000000000000 ) ) ;
#15638 = DIRECTION ( 'NONE',  ( 1.000000000000000000, 3.552713678493000424E-14, 8.881784196233999896E-14 ) ) ;
#15639 = ORIENTED_EDGE ( 'NONE', *, *, #60871, .T. ) ;
#15640 = CARTESIAN_POINT ( 'NONE',  ( 11.00000000000000000, 5.079754677601000523, -7.825000000000000178 ) ) ;
#15641 = CARTESIAN_POINT ( 'NONE',  ( 6.916495184453999912, 12.19460085780000114, 3.104235911784000379 ) ) ;
#15642 = CARTESIAN_POINT ( 'NONE',  ( 18.11581248800845145, 0.2761834754990897256, -13.89631168292871344 ) ) ;
#15643 = CARTESIAN_POINT ( 'NONE',  ( 7.744883055160999952, -2.855944972365000112, 6.776570926616000357 ) ) ;
#15644 = CARTESIAN_POINT ( 'NONE',  ( 8.470944094208999076, -5.100000000000000533, 6.571291218949999902 ) ) ;
#15645 = CARTESIAN_POINT ( 'NONE',  ( 11.51656039236534923, 5.173498198882000132, -7.557111631074219460 ) ) ;
#15646 = CARTESIAN_POINT ( 'NONE',  ( 11.80367835872029936, -5.113555564477999305, 8.201822467543799178 ) ) ;
#15647 = CARTESIAN_POINT ( 'NONE',  ( 8.801828814214612606, -4.497542371825409724, 9.205821706225451706 ) ) ;
#15648 = CARTESIAN_POINT ( 'NONE',  ( 10.94426222744800015, -4.986443098259000450, 6.687444528363699625 ) ) ;
#15649 = ORIENTED_EDGE ( 'NONE', *, *, #44195, .T. ) ;
#15650 = CARTESIAN_POINT ( 'NONE',  ( 7.165489158771000788, 2.688365364125000045, 8.140015608605001063 ) ) ;
#15651 = EDGE_LOOP ( 'NONE', ( #62014, #25194, #45476, #20957 ) ) ;
#15652 = AXIS2_PLACEMENT_3D ( 'NONE', #13948, #23045, #17817 ) ;
#15653 = DIRECTION ( 'NONE',  ( 0.000000000000000000, 0.000000000000000000, 1.000000000000000000 ) ) ;
#15654 = CARTESIAN_POINT ( 'NONE',  ( 9.085769353209000698, -2.821866379289000193, 6.127148604720000336 ) ) ;
#15655 = CARTESIAN_POINT ( 'NONE',  ( 9.885596873516499627, 2.907767014557175678, 6.870476274536375882 ) ) ;
#15656 = ORIENTED_EDGE ( 'NONE', *, *, #36636, .F. ) ;
#15657 = B_SPLINE_SURFACE_WITH_KNOTS ( 'NONE', 3, 3, ( 
 ( #54346, #50152, #12399, #34077, #18680, #8186, #2590, #35114, #1558, #28844, #45256, #23921, #40013, #44230, #66561, #66217, #55393, #56077, #29180, #39660, #39315, #61327, #34767, #34430, #13446, #40344, #23233, #49804, #7490, #56425, #28135, #65870, #33731, #55047, #7150 ),
 ( #65523, #22880, #55743, #60636, #17651, #50838, #50489, #24263, #28486, #45601, #7845, #38974, #1912, #13096, #66905, #13781, #49449, #60292, #29536, #44578, #19019, #2934, #61667, #17994, #12747, #18340, #2257, #23571, #44913, #60983, #30211, #68271, #52204, #4305, #3281 ),
 ( #36127, #57442, #14125, #20391, #9548, #4645, #25985, #14809, #42065, #20051, #15149, #30890, #25639, #20737, #3616, #51515, #35789, #15497, #36824, #46282, #35452, #56778, #8874, #19360, #47312, #45934, #24611, #46968, #41031, #67245, #31241, #41718, #68618, #62013, #63372 ),
 ( #67586, #36469, #41378, #52547, #3955, #63019, #57790, #8530, #9902, #29878, #24950, #51186, #19710, #62353, #40684, #14472, #67934, #57104, #9202, #30545, #51858, #25293, #46628, #62686, #37844, #16516, #59167, #63718, #48683, #11269, #54263, #6364, #64395, #22447, #441 ) ),
 .UNSPECIFIED., .F., .F., .F.,
 ( 4, 4 ),
 ( 4, 1, 1, 1, 1, 1, 1, 1, 1, 1, 1, 1, 1, 1, 1, 1, 1, 1, 1, 1, 1, 1, 1, 1, 1, 1, 1, 1, 1, 1, 1, 1, 4 ),
 ( -0.1039370721279000015, 1.103937072127999963 ),
 ( 0.1942321073450000157, 0.2199060843169000079, 0.2455800612886999967, 0.2712540382605999612, 0.2969280152323999777, 0.3226019922043000254, 0.3482759691761000420, 0.3739499461479999787, 0.3996239231197999953, 0.4252979000916999874, 0.4509718770635000040, 0.4766458540353999962, 0.5023198310072000128, 0.5279938079791000050, 0.5536677849509000771, 0.5793417619227999582, 0.6050157388945999193, 0.6306897158665000225, 0.6563636928382999836, 0.6820376698101999757, 0.7077116467820000478, 0.7333856237539000400, 0.7590596007256998901, 0.7847335776975999933, 0.8104075546693999543, 0.8360815316413000575, 0.8617555086131000186, 0.8874294855850000108, 0.9131034625568000829, 0.9387774395286999640, 0.9644514165004999251, 0.9901253934722999972, 1.015799370444000038 ),
 .UNSPECIFIED. ) ;
#15658 = CARTESIAN_POINT ( 'NONE',  ( 12.18852176789205188, -2.603049415106243547, -12.42696357550859965 ) ) ;
#15659 = ADVANCED_FACE ( 'NONE', ( #40231 ), #30708, .T. ) ;
#15660 = CARTESIAN_POINT ( 'NONE',  ( 11.40138360751001834, 9.883546562558999327, -5.506038862248998633 ) ) ;
#15661 = CARTESIAN_POINT ( 'NONE',  ( 9.003209435578913400, 2.902877702504753632, 6.186420784426521990 ) ) ;
#15662 = CARTESIAN_POINT ( 'NONE',  ( 10.75851354018298522, 4.163624617374472869, 8.749999999999996447 ) ) ;
#15663 = CARTESIAN_POINT ( 'NONE',  ( 12.11707904423856164, -2.286486548259630158, -13.81204227851269195 ) ) ;
#15664 = B_SPLINE_CURVE_WITH_KNOTS ( 'NONE', 3,
 ( #63562, #15676, #37005, #58321, #10423, #37687, #53082, #5181, #26516, #47846, #42592, #63900, #16015, #17753 ),
 .UNSPECIFIED., .F., .F.,
 ( 4, 2, 2, 2, 2, 2, 4 ),
 ( 0.000000000000000000, 0.2492980987600019183, 0.3739471481400044595, 0.4051094104850044286, 0.4362716728300042868, 0.4674339351750042004, 0.4985961975200040586 ),
 .UNSPECIFIED. ) ;
#15665 = EDGE_CURVE ( 'NONE', #11372, #57947, #68940, .T. ) ;
#15666 = CARTESIAN_POINT ( 'NONE',  ( 10.80133863405319872, -3.465595476214000215, -8.181696703306599261 ) ) ;
#15667 = DIRECTION ( 'NONE',  ( -1.000000000000000000, 0.000000000000000000, 0.000000000000000000 ) ) ;
#15668 = CARTESIAN_POINT ( 'NONE',  ( 18.23564136049840201, -2.231667926091398080, 12.40079771041856027 ) ) ;
#15669 = EDGE_LOOP ( 'NONE', ( #581, #58969, #46029, #26329 ) ) ;
#15670 = ORIENTED_EDGE ( 'NONE', *, *, #19336, .T. ) ;
#15671 = DIRECTION ( 'NONE',  ( 1.000000000000000000, 0.000000000000000000, 0.000000000000000000 ) ) ;
#15672 = CYLINDRICAL_SURFACE ( 'NONE', #4315, 1.250000000000000222 ) ;
#15673 = CARTESIAN_POINT ( 'NONE',  ( 4.900006121741999898, -1.747572776708515407, 1.007237960741799387 ) ) ;
#15674 = CARTESIAN_POINT ( 'NONE',  ( 11.17811698873999937, 2.762452057009999962, -6.187198315927000536 ) ) ;
#15675 = LINE ( 'NONE', #47150, #53260 ) ;
#15676 = CARTESIAN_POINT ( 'NONE',  ( 17.72043029662046010, 1.875000000000000444, -12.57545629021512212 ) ) ;
#15677 = CARTESIAN_POINT ( 'NONE',  ( 7.733151861820001471, 2.920631402299000534, -6.523085346364998038 ) ) ;
#15678 = CARTESIAN_POINT ( 'NONE',  ( 10.37873747135000002, 4.882725050998000249, 6.350806206758999650 ) ) ;
#15679 = EDGE_LOOP ( 'NONE', ( #60078, #1953, #54089, #53951 ) ) ;
#15680 = CARTESIAN_POINT ( 'NONE',  ( 10.39191562140000080, -4.919949601728999866, -4.654593006246000364 ) ) ;
#15681 = CARTESIAN_POINT ( 'NONE',  ( 9.967852198058999136, 2.034774058634999605, 7.636878205663998997 ) ) ;
#15682 = CARTESIAN_POINT ( 'NONE',  ( 9.374380199233998567, -3.139757597894699881, -7.391875284387199763 ) ) ;
#15683 = CARTESIAN_POINT ( 'NONE',  ( 11.00366064676999933, 2.264078662261999941, 7.798351372501000078 ) ) ;
#15684 = CARTESIAN_POINT ( 'NONE',  ( 11.07102344389999971, -4.762665848028800220, 7.962849245488699879 ) ) ;
#15685 = CARTESIAN_POINT ( 'NONE',  ( 9.120035841232999374, 5.288433695693000480, -8.041290150997999930 ) ) ;
#15686 = LINE ( 'NONE', #48539, #37488 ) ;
#15687 = B_SPLINE_CURVE_WITH_KNOTS ( 'NONE', 3,
 ( #32154, #20620, #15030, #53123, #5224, #4526, #25862, #68497, #15379, #58027 ),
 .UNSPECIFIED., .F., .F.,
 ( 4, 2, 2, 2, 4 ),
 ( 0.1254469995254103021, 0.3127557518398033087, 0.5000645041541962321, 0.6873732564685889335, 0.8746820087829817458 ),
 .UNSPECIFIED. ) ;
#15688 = CARTESIAN_POINT ( 'NONE',  ( 10.41964694612699915, 2.813019656517000477, -7.973702485506099613 ) ) ;
#15689 = AXIS2_PLACEMENT_3D ( 'NONE', #5787, #54376, #27130 ) ;
#15690 = CARTESIAN_POINT ( 'NONE',  ( 12.24208977126479070, -0.2715269968477702078, 12.69609476950840943 ) ) ;
#15691 = CARTESIAN_POINT ( 'NONE',  ( 5.614176421966211805, -12.11993299477413366, -3.746642824815739292 ) ) ;
#15692 = ADVANCED_FACE ( 'NONE', ( #28981 ), #22326, .T. ) ;
#15693 = CARTESIAN_POINT ( 'NONE',  ( 8.136848617591816435, 5.311482524923382798, -7.867489542080182474 ) ) ;
#15694 = DIRECTION ( 'NONE',  ( -0.7071175914358266423, 0.000000000000000000, -0.7070959707719987053 ) ) ;
#15695 = EDGE_LOOP ( 'NONE', ( #38598, #56424 ) ) ;
#15696 = CARTESIAN_POINT ( 'NONE',  ( 9.020585841232000135, 4.920236664407999783, -6.448229650796999834 ) ) ;
#15697 = CARTESIAN_POINT ( 'NONE',  ( 6.995122584706000346, 0.6190876222846001253, -0.9481936368762999834 ) ) ;
#15698 = ADVANCED_FACE ( 'NONE', ( #23372 ), #65621, .F. ) ;
#15699 = ADVANCED_FACE ( 'NONE', ( #45734 ), #34567, .T. ) ;
#15700 = CARTESIAN_POINT ( 'NONE',  ( 11.50000000000000000, -2.920245322398999921, 7.174999999999999822 ) ) ;
#15701 = CARTESIAN_POINT ( 'NONE',  ( 19.39373726536100051, 0.000000000000000000, 0.000000000000000000 ) ) ;
#15702 = CARTESIAN_POINT ( 'NONE',  ( 10.60000000000016662, 4.646670285053247085, 4.756097560975664607 ) ) ;
#15703 = CARTESIAN_POINT ( 'NONE',  ( 11.70379573085659786, -2.893744357957000357, -7.691418046581699919 ) ) ;
#15704 = ORIENTED_EDGE ( 'NONE', *, *, #22214, .F. ) ;
#15705 = CARTESIAN_POINT ( 'NONE',  ( 24.44496412535000118, -8.810486166165000910, -8.810507954003998776 ) ) ;
#15706 = CARTESIAN_POINT ( 'NONE',  ( 9.332537864288001472, -2.899999999999999911, 6.571291218949999902 ) ) ;
#15709 = CARTESIAN_POINT ( 'NONE',  ( 11.53898808224000128, 3.920528549154999709, -11.93545759853000021 ) ) ;
#15708 = CARTESIAN_POINT ( 'NONE',  ( 8.962479719595000560, 2.546924812613000189, -6.918870225297999887 ) ) ;
#15707 = PRODUCT_DEFINITION_CONTEXT ( 'detailed design', #65019, 'design' ) ;
#15710 = CARTESIAN_POINT ( 'NONE',  ( 18.18005044212796051, -2.500000099754955851, 13.67345740034994783 ) ) ;
#15711 = ORIENTED_EDGE ( 'NONE', *, *, #386, .T. ) ;
#15712 = CARTESIAN_POINT ( 'NONE',  ( 11.14994211610999919, 2.627136771666999771, 6.696094414592000277 ) ) ;
#15713 = CARTESIAN_POINT ( 'NONE',  ( 18.11617320663398445, -2.776000138870932776, -13.61099849375431958 ) ) ;
#15714 = CARTESIAN_POINT ( 'NONE',  ( 11.85159063708299954, 4.825025306051200502, 7.268038553423699533 ) ) ;
#15715 = CARTESIAN_POINT ( 'NONE',  ( 4.599999999999999645, -0.7302158263239199032, -13.98094363220830871 ) ) ;
#15716 = CARTESIAN_POINT ( 'NONE',  ( 7.422245559621999611, -5.361050935357000391, 6.973449182446000094 ) ) ;
#15717 = VERTEX_POINT ( 'NONE', #67043 ) ;
#15718 = CARTESIAN_POINT ( 'NONE',  ( 8.315517219592001297, 5.485785046334999748, 8.532070739720001740 ) ) ;
#15719 = B_SPLINE_CURVE_WITH_KNOTS ( 'NONE', 1,
 ( #53604, #21778 ),
 .UNSPECIFIED., .F., .F.,
 ( 2, 2 ),
 ( 0.000000000000000000, 1.000000000000000000 ),
 .UNSPECIFIED. ) ;
#15720 = EDGE_CURVE ( 'NONE', #523, #54836, #16488, .T. ) ;
#15722 = CARTESIAN_POINT ( 'NONE',  ( 13.59982064663300072, -2.380318164795999883E-13, -1.474376176701999879E-13 ) ) ;
#15721 = CARTESIAN_POINT ( 'NONE',  ( 10.84606641549978256, 4.838299037060044938, -7.747677868960886727 ) ) ;
#15723 = CARTESIAN_POINT ( 'NONE',  ( 7.482900004268410399, -2.407370889025786997, 6.799601156578478189 ) ) ;
#15724 = CARTESIAN_POINT ( 'NONE',  ( 8.406851002545000284, 2.832432432432000269, -6.822293592207000934 ) ) ;
#15725 = CARTESIAN_POINT ( 'NONE',  ( 1.929202210879999990, -0.1982148001128000159, 3.252998300308999724 ) ) ;
#15726 = ORIENTED_EDGE ( 'NONE', *, *, #57706, .T. ) ;
#15727 = CARTESIAN_POINT ( 'NONE',  ( 9.466846873515667227, 3.231816600031355069, -8.499583552997723501 ) ) ;
#15728 = CARTESIAN_POINT ( 'NONE',  ( 10.97718582084299932, -4.656536239972400182, 8.258888014436699621 ) ) ;
#15729 = CARTESIAN_POINT ( 'NONE',  ( 10.80168826891999956, 3.998196217194999846, 9.431555066626000183 ) ) ;
#15730 = CARTESIAN_POINT ( 'NONE',  ( 11.43302763632549990, 2.964209339073000216, 7.977941233841399971 ) ) ;
#15731 = ORIENTED_EDGE ( 'NONE', *, *, #66773, .F. ) ;
#15732 = SHAPE_REPRESENTATION ( 'Negative Post', ( #9676 ), #67766 ) ;
#15733 = CARTESIAN_POINT ( 'NONE',  ( 24.09351851543715384, -3.337598052541425719, 12.57555534302550448 ) ) ;
#15734 = AXIS2_PLACEMENT_3D ( 'NONE', #18377, #39699, #45972 ) ;
#15735 = CARTESIAN_POINT ( 'NONE',  ( 12.19613275390595319, 2.089545048426563856, -12.42553124896410566 ) ) ;
#15736 = CARTESIAN_POINT ( 'NONE',  ( 11.60101463001529964, -3.377766160221900016, 8.496586578655598743 ) ) ;
#15737 = CARTESIAN_POINT ( 'NONE',  ( 25.08881450776800293, -3.215722343401999694, -11.60740445141000166 ) ) ;
#15738 = CARTESIAN_POINT ( 'NONE',  ( 18.25313429507010099, -2.320711718358091424, 13.80631856085855169 ) ) ;
#15739 = CARTESIAN_POINT ( 'NONE',  ( 25.39940292809759370, -8.416043265628282199, -8.072286559073248213 ) ) ;
#15740 = ORIENTED_EDGE ( 'NONE', *, *, #62988, .F. ) ;
#15741 = CARTESIAN_POINT ( 'NONE',  ( 8.803927344482000095, -5.129996464381000543, -6.743586268849999676 ) ) ;
#15742 = FACE_OUTER_BOUND ( 'NONE', #53142, .T. ) ;
#15744 = ORIENTED_EDGE ( 'NONE', *, *, #55596, .T. ) ;
#15743 = CIRCLE ( 'NONE', #44802, 14.00000000000000533 ) ;
#15745 = LINE ( 'NONE', #30454, #50637 ) ;
#15746 = CARTESIAN_POINT ( 'NONE',  ( 11.04333729122639873, 2.996877626170000308, 7.526388557597149642 ) ) ;
#15747 = CARTESIAN_POINT ( 'NONE',  ( 11.09999999999999964, 7.281355511280001025, -6.286510895624999762 ) ) ;
#15748 = CARTESIAN_POINT ( 'NONE',  ( 9.949437606643998677, 2.508497579857000392, -7.171862210735000076 ) ) ;
#15749 = CARTESIAN_POINT ( 'NONE',  ( 7.800985831153996131, 4.602212482482000766, 6.372454311207003563 ) ) ;
#15750 = CARTESIAN_POINT ( 'NONE',  ( 9.743567407955000093, -5.287392049455999832, 8.939957179821000466 ) ) ;
#15751 = CARTESIAN_POINT ( 'NONE',  ( 17.72055336043788998, -0.7006927685645097936, -12.58050281163331796 ) ) ;
#15752 = EDGE_CURVE ( 'NONE', #58126, #32166, #65341, .T. ) ;
#15753 = CARTESIAN_POINT ( 'NONE',  ( 12.76376210871183403, 3.124999999999998224, -12.28374662615010848 ) ) ;
#15754 = CARTESIAN_POINT ( 'NONE',  ( 11.65456516821461008, -3.197083038490000195, -8.310318115935698913 ) ) ;
#15755 = CARTESIAN_POINT ( 'NONE',  ( 7.673642219589999591, 4.696238830159999544, 5.830273622963999536 ) ) ;
#15756 = ORIENTED_EDGE ( 'NONE', *, *, #28063, .T. ) ;
#15757 = CARTESIAN_POINT ( 'NONE',  ( 11.59999999999999964, -4.883784007588900522, -7.825000000000000178 ) ) ;
#15758 = DIRECTION ( 'NONE',  ( 0.000000000000000000, 1.000000000000000000, 0.000000000000000000 ) ) ;
#15759 = CARTESIAN_POINT ( 'NONE',  ( 8.628315327349485031, 2.973711298499293942, -6.169547619358109358 ) ) ;
#15760 = DIRECTION ( 'NONE',  ( -0.7071067718169923300, -0.7071067905560921574, -1.210975589615986548E-07 ) ) ;
#15761 = AXIS2_PLACEMENT_3D ( 'NONE', #19958, #36375, #68519 ) ;
#15762 = CARTESIAN_POINT ( 'NONE',  ( 10.96506373917000055, 6.669401756511000201, 5.364506396814999967 ) ) ;
#15763 = CARTESIAN_POINT ( 'NONE',  ( 10.95087180411999839, 9.916154023254000194, 5.627633586593999482 ) ) ;
#15764 = CARTESIAN_POINT ( 'NONE',  ( 12.52212199933416237, -0.5573870965680521872, -12.68353347974201384 ) ) ;
#15765 = CARTESIAN_POINT ( 'NONE',  ( 9.864763540183249191, -5.217465845835395299, -7.827184855449096368 ) ) ;
#15766 = VERTEX_POINT ( 'NONE', #45391 ) ;
#15767 = CARTESIAN_POINT ( 'NONE',  ( 12.35083548769878625, -1.919332845685027822, 12.45296032288162813 ) ) ;
#15768 = CARTESIAN_POINT ( 'NONE',  ( 10.26492546752099955, -5.139081147506999514, -7.421078600323300023 ) ) ;
#15769 = CARTESIAN_POINT ( 'NONE',  ( 8.828853474160295534, 2.650682855974121122, -7.263274753612249945 ) ) ;
#15770 = CARTESIAN_POINT ( 'NONE',  ( 10.62698276521000196, -3.142914536759000121, 8.668455626664998803 ) ) ;
#15771 = CARTESIAN_POINT ( 'NONE',  ( 11.91672066707849886, -3.258843737379200078, 7.948314604624900248 ) ) ;
#15772 = CARTESIAN_POINT ( 'NONE',  ( 12.12656756701886707, 0.2537702651956291744, 12.59744904646397679 ) ) ;
#15773 = CARTESIAN_POINT ( 'NONE',  ( 0.2033022342298000107, 1.141789477572999978, -2.999605631121999849 ) ) ;
#15774 = CARTESIAN_POINT ( 'NONE',  ( 7.739033623444901089, -2.652152912377775174, 7.263328590673341800 ) ) ;
#15775 = CARTESIAN_POINT ( 'NONE',  ( 12.09179812036142110, 2.610377073672085046, 12.32664058968472176 ) ) ;
#15776 = CARTESIAN_POINT ( 'NONE',  ( 9.201101285863998669, 3.264788442324599860, -6.626387721327399838 ) ) ;
#15777 = CARTESIAN_POINT ( 'NONE',  ( 10.40333997687999990, 4.213854445120500003, -6.519583185858300212 ) ) ;
#15778 = CARTESIAN_POINT ( 'NONE',  ( 12.35268573731032227, 12.09127048605807353, -3.267865047144104640 ) ) ;
#15779 = EDGE_CURVE ( 'NONE', #10880, #39380, #46165, .T. ) ;
#15780 = CARTESIAN_POINT ( 'NONE',  ( 10.47111721959000086, 5.170640285885000687, -8.712953516124999354 ) ) ;
#15781 = CARTESIAN_POINT ( 'NONE',  ( 9.301355082327999568, 3.427502311996299955, -6.356045986629998978 ) ) ;
#15783 = CARTESIAN_POINT ( 'NONE',  ( 18.18005043824377154, 1.329526366183796371E-10, 12.70000000088145420 ) ) ;
#15782 = CARTESIAN_POINT ( 'NONE',  ( 18.30000786429387816, -11.69700901162388185, 3.885059408455575625 ) ) ;
#15784 = CARTESIAN_POINT ( 'NONE',  ( 8.967236468531000426, 5.342667293695661179, 7.360013885755487983 ) ) ;
#15785 = ORIENTED_EDGE ( 'NONE', *, *, #50292, .T. ) ;
#15786 = CARTESIAN_POINT ( 'NONE',  ( 12.18827089114435758, 0.1029087316592282725, 12.69945830692958566 ) ) ;
#15787 = CYLINDRICAL_SURFACE ( 'NONE', #5452, 11.35000000000000142 ) ;
#15788 = CARTESIAN_POINT ( 'NONE',  ( 9.660528907822998335, 2.899999999999999911, -6.152188490330000370 ) ) ;
#15789 = CARTESIAN_POINT ( 'NONE',  ( 9.376392757686998536, 4.677963304775400566, 6.758914271013199304 ) ) ;
#15790 = CARTESIAN_POINT ( 'NONE',  ( 8.999999001754000361, 3.268496584495999908E-13, -12.49999978039651083 ) ) ;
#15791 = CARTESIAN_POINT ( 'NONE',  ( 12.23000334607949036, -2.254948878044617633, 13.72238900567161402 ) ) ;
#15792 = CARTESIAN_POINT ( 'NONE',  ( 12.22437278964929064, 2.731306219223309295, 13.62162349210572820 ) ) ;
#15793 = CARTESIAN_POINT ( 'NONE',  ( 23.54908214757200113, 2.962708511087999597, -13.72216420026999906 ) ) ;
#15794 = B_SPLINE_CURVE_WITH_KNOTS ( 'NONE', 3,
 ( #65487, #1875, #57408, #3920 ),
 .UNSPECIFIED., .F., .F.,
 ( 4, 4 ),
 ( 0.000000000000000000, 1.000000000000000000 ),
 .UNSPECIFIED. ) ;
#15795 = ORIENTED_EDGE ( 'NONE', *, *, #12892, .F. ) ;
#15796 = EDGE_CURVE ( 'NONE', #18020, #52078, #61804, .T. ) ;
#15797 = CARTESIAN_POINT ( 'NONE',  ( 4.363809043199000648, -1.123505578223999990, 0.6037476609470000533 ) ) ;
#15798 = CARTESIAN_POINT ( 'NONE',  ( 9.605304848515999083, -2.836617618740000069, -8.031907719862799055 ) ) ;
#15799 = CARTESIAN_POINT ( 'NONE',  ( 9.679514975094384965, -4.176630006209533619, -8.850146613061715684 ) ) ;
#15800 = CARTESIAN_POINT ( 'NONE',  ( 10.98768472639999949, 5.139096889661000311, -4.945212061661000469 ) ) ;
#15801 = EDGE_CURVE ( 'NONE', #53841, #11010, #13921, .T. ) ;
#15802 = CARTESIAN_POINT ( 'NONE',  ( 18.17519250343466908, 2.421563205337720959, -12.46952409297816544 ) ) ;
#15803 = CARTESIAN_POINT ( 'NONE',  ( 13.99999999347100044, -9.187456302440001110, -8.213201953411001455 ) ) ;
#15804 = CARTESIAN_POINT ( 'NONE',  ( 18.12908148756949700, 2.747269642044513294, 12.39050915966048017 ) ) ;
#15805 = CARTESIAN_POINT ( 'NONE',  ( 10.86330120046000047, -2.934641216426999932, -5.167266016126999872 ) ) ;
#15806 = CARTESIAN_POINT ( 'NONE',  ( 10.49412055961999890, -2.866949708568999888, -8.960719633954001395 ) ) ;
#15807 = CARTESIAN_POINT ( 'NONE',  ( 12.70654069052307555, 3.248070099070885064, 13.61800428248618466 ) ) ;
#15808 = CARTESIAN_POINT ( 'NONE',  ( 9.771640687503566625, 2.873222873816650313, 6.752018918868516018 ) ) ;
#15809 = CARTESIAN_POINT ( 'NONE',  ( 4.599999999999999645, 1.760845406083394682, -12.47635457398814829 ) ) ;
#15810 = CYLINDRICAL_SURFACE ( 'NONE', #10854, 0.4999999999999998335 ) ;
#15811 = CARTESIAN_POINT ( 'NONE',  ( 11.39393020684959978, -5.250000000000000000, 7.500000000000000000 ) ) ;
#15812 = ORIENTED_EDGE ( 'NONE', *, *, #58862, .T. ) ;
#15813 = CARTESIAN_POINT ( 'NONE',  ( 8.854170280414001226, 4.902869380824999901, -8.978557145469999057 ) ) ;
#15814 = CARTESIAN_POINT ( 'NONE',  ( 11.10441638348510018, -4.841589649988700117, 7.705001100909899314 ) ) ;
#15815 = ORIENTED_EDGE ( 'NONE', *, *, #14327, .T. ) ;
#15816 = DIRECTION ( 'NONE',  ( -0.000000000000000000, 0.2588190451024934280, 0.9659258262890756397 ) ) ;
#15818 = CARTESIAN_POINT ( 'NONE',  ( 10.76841504065829902, -3.085489673376300424, -6.818119527508899935 ) ) ;
#15817 = B_SPLINE_CURVE_WITH_KNOTS ( 'NONE', 3,
 ( #25949, #5990, #26650, #5645, #63688, #4966 ),
 .UNSPECIFIED., .F., .F.,
 ( 4, 2, 4 ),
 ( 0.000000000000000000, 0.5000000000000000000, 1.000000000000000000 ),
 .UNSPECIFIED. ) ;
#15819 = VERTEX_POINT ( 'NONE', #41175 ) ;
#15820 = CARTESIAN_POINT ( 'NONE',  ( 11.09590547754519996, 5.315605332491999846, 7.458246194669389872 ) ) ;
#15821 = CARTESIAN_POINT ( 'NONE',  ( 8.895035841232999729, 5.751585344281000545, -8.235867044345999588 ) ) ;
#15822 = CARTESIAN_POINT ( 'NONE',  ( 18.02410434383600091, -3.285250940561000199, 11.23276246309000115 ) ) ;
#15823 = FACE_OUTER_BOUND ( 'NONE', #22350, .T. ) ;
#15824 = CARTESIAN_POINT ( 'NONE',  ( 9.810596873515665450, -4.629523725463621453, -6.407767014557176566 ) ) ;
#15825 = CARTESIAN_POINT ( 'NONE',  ( 7.000000000000000000, -7.526486366024999874, -3.526486366024999874 ) ) ;
#15826 = CARTESIAN_POINT ( 'NONE',  ( 17.55505043854147118, -3.125000000000000000, -25.00000000000000000 ) ) ;
#15827 = ORIENTED_EDGE ( 'NONE', *, *, #13825, .F. ) ;
#15828 = CARTESIAN_POINT ( 'NONE',  ( 8.684028039623227002, 2.794631556210644074, 8.206409581471232784 ) ) ;
#15829 = ORIENTED_EDGE ( 'NONE', *, *, #38738, .F. ) ;
#15830 = LINE ( 'NONE', #10242, #187 ) ;
#15831 =( NAMED_UNIT ( * ) SI_UNIT ( $, .STERADIAN. ) SOLID_ANGLE_UNIT ( ) );
#15832 = VERTEX_POINT ( 'NONE', #62482 ) ;
#15833 = CARTESIAN_POINT ( 'NONE',  ( 9.174709346416998201, 5.155548326249999924, 8.048718920009699573 ) ) ;
#15834 = CARTESIAN_POINT ( 'NONE',  ( 17.75808086271927522, -3.091459143609192495, -12.29388367502514612 ) ) ;
#15835 = CARTESIAN_POINT ( 'NONE',  ( 10.21684687351595677, 4.768183399968648040, -6.500416447002277387 ) ) ;
#15836 = CYLINDRICAL_SURFACE ( 'NONE', #13464, 0.9499999999999999556 ) ;
#15837 = CARTESIAN_POINT ( 'NONE',  ( 12.23133660942382583, 0.2481576080865451894, 13.89702325994033671 ) ) ;
#15838 = VERTEX_POINT ( 'NONE', #2733 ) ;
#15839 = CARTESIAN_POINT ( 'NONE',  ( 12.56257882282300109, 11.80639483233000142, -3.358960109135999961 ) ) ;
#15840 = CARTESIAN_POINT ( 'NONE',  ( 18.54135782960599954, 11.85700164854999983, -4.150661879143999755 ) ) ;
#15841 = CARTESIAN_POINT ( 'NONE',  ( 9.429533309317625012, 4.633212041316643770, 8.103800281262431682 ) ) ;
#15842 = CARTESIAN_POINT ( 'NONE',  ( 23.56664322114200161, -2.935586410151000081, -13.67842711829000102 ) ) ;
#15843 = CIRCLE ( 'NONE', #11396, 12.49999909016000110 ) ;
#15844 = FACE_OUTER_BOUND ( 'NONE', #31717, .T. ) ;
#15845 = CARTESIAN_POINT ( 'NONE',  ( 17.79173234077999766, -3.528207283916999781, 11.96069632439000152 ) ) ;
#15846 = AXIS2_PLACEMENT_3D ( 'NONE', #48786, #26085, #22206 ) ;
#15847 = CARTESIAN_POINT ( 'NONE',  ( 10.53865751177000121, -3.647233463439000012, -6.014125921456000334 ) ) ;
#15848 = VERTEX_POINT ( 'NONE', #35248 ) ;
#15849 = VERTEX_POINT ( 'NONE', #3412 ) ;
#15850 = CARTESIAN_POINT ( 'NONE',  ( 11.04471440281000127, 5.245236777044000043, -5.184237567191000373 ) ) ;
#15851 = CARTESIAN_POINT ( 'NONE',  ( 5.700000000000000178, -1.300000000000000044, -9.662944685757000940 ) ) ;
#15852 = CARTESIAN_POINT ( 'NONE',  ( 11.29996849689000271, 12.23272706294999956, 1.505586356912999912 ) ) ;
#15853 = CARTESIAN_POINT ( 'NONE',  ( 0.1499942179679999987, 2.750000000000000000, 0.000000000000000000 ) ) ;
#15854 = EDGE_CURVE ( 'NONE', #57059, #44304, #49364, .T. ) ;
#15855 = ADVANCED_FACE ( 'NONE', ( #3749 ), #19153, .F. ) ;
#15856 = CARTESIAN_POINT ( 'NONE',  ( 11.03776785110999903, 5.237767851104999650, 6.571291218949999902 ) ) ;
#15857 = CARTESIAN_POINT ( 'NONE',  ( 9.079430433046999482, 3.262177192690499883, -7.044669955395099770 ) ) ;
#15859 = CARTESIAN_POINT ( 'NONE',  ( 8.453116750410908153, 5.099910069830336568, -6.561598178278856608 ) ) ;
#15858 = CARTESIAN_POINT ( 'NONE',  ( 10.88955864498000103, -3.209241371122599773, 6.880692865553299953 ) ) ;
#15860 = CARTESIAN_POINT ( 'NONE',  ( 8.500486250726996929, -2.902641158998001458, 6.605591905707999700 ) ) ;
#15861 = ORIENTED_EDGE ( 'NONE', *, *, #39805, .T. ) ;
#15862 = CARTESIAN_POINT ( 'NONE',  ( 9.873096873515667227, 2.782534154164606921, -7.172815144550898303 ) ) ;
#15863 = CARTESIAN_POINT ( 'NONE',  ( 7.790168786842999182, -2.923571394339999685, 6.474157094959999803 ) ) ;
#15864 = CARTESIAN_POINT ( 'NONE',  ( 9.431076168958000494, 3.350848599899200142, 6.397735581984999698 ) ) ;
#15865 = DIRECTION ( 'NONE',  ( 0.000000000000000000, 0.000000000000000000, -1.000000000000000000 ) ) ;
#15866 = CARTESIAN_POINT ( 'NONE',  ( 9.285188841453999586, -5.269672295101000437, 8.747824102203999530 ) ) ;
#15867 = CARTESIAN_POINT ( 'NONE',  ( 18.14127614488628382, 2.717147700443817815, -12.39835379074819954 ) ) ;
#15868 = CARTESIAN_POINT ( 'NONE',  ( 16.39956681845000119, -3.250692199830000018, -11.33777344299000056 ) ) ;
#15869 = CARTESIAN_POINT ( 'NONE',  ( 15.89998535262538581, -8.893549080881243185, -8.534693534631728085 ) ) ;
#15870 = LINE ( 'NONE', #65752, #2079 ) ;
#15871 = CARTESIAN_POINT ( 'NONE',  ( 10.24255864497999902, -3.209241371122599773, -8.119307134446700047 ) ) ;
#15872 = CIRCLE ( 'NONE', #262, 12.35000000006999876 ) ;
#15873 = CARTESIAN_POINT ( 'NONE',  ( 6.535161299140999525, 1.240385862733000000, 0.4581726639353000397 ) ) ;
#15874 = EDGE_CURVE ( 'NONE', #45907, #15819, #22741, .T. ) ;
#15875 = CARTESIAN_POINT ( 'NONE',  ( 6.999999999999999112, 9.168025982482129521, -4.705522764150024351 ) ) ;
#15876 = CARTESIAN_POINT ( 'NONE',  ( 44.24148000000000280, 9.517611874540000017, -8.103398312166000039 ) ) ;
#15877 = VERTEX_POINT ( 'NONE', #40475 ) ;
#15878 = CARTESIAN_POINT ( 'NONE',  ( 12.18528753443599477, 0.08139242733401171048, -12.69965452654168026 ) ) ;
#15879 = CARTESIAN_POINT ( 'NONE',  ( 23.60000000000000497, 10.96672402886443187, 8.588474120523409638 ) ) ;
#15880 = CARTESIAN_POINT ( 'NONE',  ( 6.899999692059999745, 12.99045401434999825, 1.690592943097000145 ) ) ;
#15881 = FACE_OUTER_BOUND ( 'NONE', #38018, .T. ) ;
#15882 = CARTESIAN_POINT ( 'NONE',  ( 1.655140132541082831, 0.9161175952574702741, 3.408904368339106927 ) ) ;
#15883 = EDGE_LOOP ( 'NONE', ( #22172, #2589, #7008, #68335, #8947 ) ) ;
#15884 = CARTESIAN_POINT ( 'NONE',  ( 18.30017264560542145, -0.9191760160195996399, -11.85014035451979630 ) ) ;
#15885 = CONTEXT_DEPENDENT_SHAPE_REPRESENTATION ( #13703, #27168 ) ;
#15886 = CARTESIAN_POINT ( 'NONE',  ( 11.27234208742519783, -4.554746427620499638, -8.372004648554700168 ) ) ;
#15887 = DIRECTION ( 'NONE',  ( -0.7071067783004970631, -0.7071067840725973053, 3.040673725924991281E-08 ) ) ;
#15888 = DIRECTION ( 'NONE',  ( 0.000000000000000000, 0.000000000000000000, -1.000000000000000000 ) ) ;
#15889 = DIRECTION ( 'NONE',  ( 1.000000000000000000, 0.000000000000000000, 0.000000000000000000 ) ) ;
#15891 = AXIS2_PLACEMENT_3D ( 'NONE', #6542, #23322, #44998 ) ;
#15890 = CARTESIAN_POINT ( 'NONE',  ( 10.39969598649000027, 4.888000489779200208, -8.028730309000598808 ) ) ;
#15892 = ORIENTED_EDGE ( 'NONE', *, *, #58391, .F. ) ;
#15893 = CARTESIAN_POINT ( 'NONE',  ( 10.46754921866999943, -2.318350880468999620, 6.549783596838000044 ) ) ;
#15894 = CARTESIAN_POINT ( 'NONE',  ( 17.89590342297354297, 3.023973030522680627, -13.54825986461598752 ) ) ;
#15895 = ORIENTED_EDGE ( 'NONE', *, *, #38255, .T. ) ;
#15896 = CARTESIAN_POINT ( 'NONE',  ( 13.56457200098428117, 11.48338024779088862, 1.964390585080378226 ) ) ;
#15897 = CARTESIAN_POINT ( 'NONE',  ( 9.214144353209000826, -5.421531391267000011, 6.381128921159999301 ) ) ;
#15898 = CARTESIAN_POINT ( 'NONE',  ( 17.67321579093595219, -0.7208442004938210301, -13.98143072948223953 ) ) ;
#15899 = ORIENTED_EDGE ( 'NONE', *, *, #47275, .T. ) ;
#15900 = CARTESIAN_POINT ( 'NONE',  ( 11.41486084871699802, 2.792989229543000107, 7.174999999999999822 ) ) ;
#15901 = CARTESIAN_POINT ( 'NONE',  ( 7.663385841224000572, 2.462963193532999640, -6.383277393009000100 ) ) ;
#15902 = DIRECTION ( 'NONE',  ( 1.000000000000000000, 0.000000000000000000, 0.000000000000000000 ) ) ;
#15903 = CARTESIAN_POINT ( 'NONE',  ( 7.364999999998000035, 2.649999999999999911, -7.500000000000000000 ) ) ;
#15904 = VERTEX_POINT ( 'NONE', #56562 ) ;
#15905 = CARTESIAN_POINT ( 'NONE',  ( 9.352255147285999826, -2.817754448466000206, 6.388456890282999900 ) ) ;
#15906 = CARTESIAN_POINT ( 'NONE',  ( 11.59999999999999964, 3.182579051151299687, 7.825000000000000178 ) ) ;
#15907 = SURFACE_SIDE_STYLE ('',( #10662 ) ) ;
#15908 = ORIENTED_EDGE ( 'NONE', *, *, #46883, .T. ) ;
#15909 = CARTESIAN_POINT ( 'NONE',  ( 7.307500000000000107, -0.2999999999999999889, -3.149999999999999911 ) ) ;
#15910 = ORIENTED_EDGE ( 'NONE', *, *, #40021, .F. ) ;
#15911 = CARTESIAN_POINT ( 'NONE',  ( 4.867324867288667534, 1.499999999999999778, 0.2318186422567637128 ) ) ;
#15912 = CARTESIAN_POINT ( 'NONE',  ( 17.67442079356968065, -1.770331164897447573, -12.47501301698789611 ) ) ;
#15913 = CARTESIAN_POINT ( 'NONE',  ( 18.29983863916000075, 2.861762957209999847, -11.98830831200999825 ) ) ;
#15914 = LINE ( 'NONE', #5768, #36953 ) ;
#15915 = ADVANCED_FACE ( 'NONE', ( #66702, #14264 ), #61464, .T. ) ;
#15916 = CARTESIAN_POINT ( 'NONE',  ( 44.24148000000000280, -9.517611874540000017, -8.103398312166000039 ) ) ;
#15917 = CARTESIAN_POINT ( 'NONE',  ( 7.171515396205728088, 4.321096043748422488, -8.846445178760147243 ) ) ;
#15918 = CARTESIAN_POINT ( 'NONE',  ( 23.81728141243367602, 12.99649529944050030, 3.682154768044699988 ) ) ;
#15919 = EDGE_CURVE ( 'NONE', #26552, #7028, #55587, .T. ) ;
#15920 = B_SPLINE_SURFACE_WITH_KNOTS ( 'NONE', 3, 3, ( 
 ( #23484, #33639, #54606, #49354, #60202, #2502, #44824, #7057, #39568, #29442, #50748, #65432, #2845, #39920, #60892, #65777, #28392, #13008, #34334, #24172, #13354, #33291, #59847, #55652, #29094, #1816, #1468, #44486, #12653, #50403, #22784, #23135, #44133, #34680, #17554 ),
 ( #11952, #61238, #55994, #8098, #17903, #38880, #54955, #39220, #60546, #30127, #67155, #45844, #35023, #14719, #3867, #57019, #25550, #15056, #35702, #57350, #9119, #30456, #19963, #56684, #8783, #62933, #9806, #25201, #51430, #36034, #13694, #40258, #57696, #67500, #68525 ),
 ( #9454, #51091, #29789, #31155, #4212, #40940, #41287, #62261, #19267, #36380, #30796, #52109, #46875, #46536, #40596, #62595, #61578, #61921, #3526, #24862, #68183, #41627, #20301, #52457, #14036, #4552, #51769, #3194, #67842, #14382, #25893, #35362, #46190, #47222, #56338 ),
 ( #8441, #24521, #19618, #26588, #37075, #48243, #42998, #32860, #43356, #63278, #54173, #26929, #16424, #58386, #64306, #27612, #32516, #696, #10493, #7, #37753, #5929, #4901, #53149, #20647, #59079, #53832, #11179, #48940, #6271, #41972, #27271, #15408, #36734, #48594 ) ),
 .UNSPECIFIED., .F., .F., .F.,
 ( 4, 4 ),
 ( 4, 1, 1, 1, 1, 1, 1, 1, 1, 1, 1, 1, 1, 1, 1, 1, 1, 1, 1, 1, 1, 1, 1, 1, 1, 1, 1, 1, 1, 1, 1, 1, 4 ),
 ( -0.1039370721279000015, 1.103937072127999963 ),
 ( -0.01933701211302999920, 0.01208563257065999909, 0.04350827725433999843, 0.07493092193802000645, 0.1063535666217000075, 0.1377762113054000204, 0.1691988559891000055, 0.2006215006727000150, 0.2320441453564000001, 0.2634667900400999851, 0.2948894347238000258, 0.3263120794074999553, 0.3577347240911999959, 0.3891573687748000054, 0.4205800134584999905, 0.4520026581421999756, 0.4834253028259000162, 0.5148479475096000568, 0.5462705921932000663, 0.5776932368768999959, 0.6091158815606000365, 0.6405385262443000771, 0.6719611709280000067, 0.7033838156117000473, 0.7348064602953000568, 0.7662291049789999864, 0.7976517496627000270, 0.8290743943464000676, 0.8604970390300999972, 0.8919196837138000378, 0.9233423283974000473, 0.9547649730810999769, 0.9861876177648000175 ),
 .UNSPECIFIED. ) ;
#15921 = ORIENTED_EDGE ( 'NONE', *, *, #20131, .T. ) ;
#15922 = CARTESIAN_POINT ( 'NONE',  ( 8.361422056298998484, -5.126342729456004221, 6.365321850284000327 ) ) ;
#15923 = ORIENTED_EDGE ( 'NONE', *, *, #8369, .T. ) ;
#15924 = CARTESIAN_POINT ( 'NONE',  ( 9.743561007103998861, 5.287400066955999733, 8.939966147452000911 ) ) ;
#15925 = APPLICATION_CONTEXT ( 'automotive_design' ) ;
#15926 = CARTESIAN_POINT ( 'NONE',  ( 10.94846415877000112, 3.841064079579000090, -9.341816855317999213 ) ) ;
#15927 = B_SPLINE_CURVE_WITH_KNOTS ( 'NONE', 3,
 ( #52355, #43245, #63171, #15641, #57949 ),
 .UNSPECIFIED., .F., .F.,
 ( 4, 1, 4 ),
 ( 0.000000000000000000, 0.5000000000000000000, 1.000000000000000000 ),
 .UNSPECIFIED. ) ;
#15928 = CARTESIAN_POINT ( 'NONE',  ( 11.09999999999999964, 4.000000000000000000, 7.500000000000000000 ) ) ;
#15929 = CARTESIAN_POINT ( 'NONE',  ( 9.269210841233000764, 3.098073081301000009, -8.567513114264999174 ) ) ;
#15930 = CIRCLE ( 'NONE', #8150, 5.000000000000000000 ) ;
#15931 = CARTESIAN_POINT ( 'NONE',  ( 10.59999999999999964, 4.599999999999999645, 4.756097560976000338 ) ) ;
#15932 = CARTESIAN_POINT ( 'NONE',  ( 8.938868730821853958, -3.795034549399585178, -6.149945561018825835 ) ) ;
#15933 = CARTESIAN_POINT ( 'NONE',  ( 18.15872407313728587, 0.1621987986621301059, 13.89873133405097327 ) ) ;
#15934 = CARTESIAN_POINT ( 'NONE',  ( 8.725348536223782148, -2.649439212887072959, 7.500023728975150128 ) ) ;
#15935 = EDGE_LOOP ( 'NONE', ( #68857, #38589, #38889, #34377 ) ) ;
#15936 = CARTESIAN_POINT ( 'NONE',  ( 12.78455560662700208, -11.44263450739000021, 4.698119303721000506 ) ) ;
#15937 = CARTESIAN_POINT ( 'NONE',  ( 12.07656516821461068, -3.100463633631699967, 6.592171857671999646 ) ) ;
#15938 = CARTESIAN_POINT ( 'NONE',  ( 18.16002775367444144, -0.1622926916309997414, -13.89880504292134944 ) ) ;
#15939 = EDGE_CURVE ( 'NONE', #67742, #2068, #1825, .T. ) ;
#15940 = EDGE_CURVE ( 'NONE', #45376, #35517, #25426, .T. ) ;
#15941 = CARTESIAN_POINT ( 'NONE',  ( 8.694605646795000808, -5.290204991635000020, 8.768102264518001121 ) ) ;
#15943 = CARTESIAN_POINT ( 'NONE',  ( 24.53428991195500330, 3.614319144953999530, 12.31267516478999902 ) ) ;
#15942 = CARTESIAN_POINT ( 'NONE',  ( 10.99933470386000067, 5.081013421858999735, 8.239043921879998678 ) ) ;
#15944 = COLOUR_RGB ( '', 0.08235294, 0.09019608, 0.10196078) ;
#15945 = CARTESIAN_POINT ( 'NONE',  ( 11.60118044953561878, 5.133201153721000054, -8.090905336380599167 ) ) ;
#15946 = EDGE_CURVE ( 'NONE', #31242, #28639, #61878, .T. ) ;
#15947 = CARTESIAN_POINT ( 'NONE',  ( 10.61094409420999973, -5.100000000000000533, -6.571291218949999902 ) ) ;
#15948 = CARTESIAN_POINT ( 'NONE',  ( 10.33688779216199904, 4.801941500727100021, -7.789199634454999632 ) ) ;
#15949 = CARTESIAN_POINT ( 'NONE',  ( 17.94753454920341440, -0.4864235087029702420, 12.68745975172790530 ) ) ;
#15950 = CARTESIAN_POINT ( 'NONE',  ( 7.127282214532000282, 0.07550418544918999220, 1.270944974832999952 ) ) ;
#15951 = CYLINDRICAL_SURFACE ( 'NONE', #55574, 0.5000000000000004441 ) ;
#15952 = VERTEX_POINT ( 'NONE', #47449 ) ;
#15953 = CARTESIAN_POINT ( 'NONE',  ( 9.176355646795000709, -2.935738482289000029, 6.259841087764999479 ) ) ;
#15954 = CARTESIAN_POINT ( 'NONE',  ( 9.219964158774999419, 3.941185585667000169, -8.896279800194999865 ) ) ;
#15955 = PLANE ( 'NONE',  #309 ) ;
#15956 = CARTESIAN_POINT ( 'NONE',  ( 9.123929153134323400, -5.099761357576727328, 6.165062780802330167 ) ) ;
#15957 = ORIENTED_EDGE ( 'NONE', *, *, #66296, .F. ) ;
#15958 = CARTESIAN_POINT ( 'NONE',  ( 0.7186698601468000103, 2.838478058858999731, -1.283102133118000143 ) ) ;
#15959 = EDGE_CURVE ( 'NONE', #15130, #62127, #14940, .T. ) ;
#15960 = LINE ( 'NONE', #5809, #8612 ) ;
#15961 = CARTESIAN_POINT ( 'NONE',  ( 2.504702091563999478, 3.604403478001999783, -1.066139224190999935 ) ) ;
#15962 = ORIENTED_EDGE ( 'NONE', *, *, #15940, .T. ) ;
#15963 = DIRECTION ( 'NONE',  ( -1.000000000000000000, 0.000000000000000000, 0.000000000000000000 ) ) ;
#15964 = CARTESIAN_POINT ( 'NONE',  ( 0.1500002361980000143, 0.000000000000000000, 0.000000000000000000 ) ) ;
#15965 = CARTESIAN_POINT ( 'NONE',  ( 10.05041772631199848, 4.549624259497900169, 6.368647051112000135 ) ) ;
#15966 = CARTESIAN_POINT ( 'NONE',  ( 5.557969180997336167, 12.17302321295358603, 3.765215263421144432 ) ) ;
#15967 = CARTESIAN_POINT ( 'NONE',  ( 7.603420280409000753, 5.687206835507000235, 6.847268999608999707 ) ) ;
#15968 = ORIENTED_EDGE ( 'NONE', *, *, #29144, .F. ) ;
#15969 = CARTESIAN_POINT ( 'NONE',  ( 7.835751895984281568, -4.956109399768123147, 6.487758672992816500 ) ) ;
#15970 = B_SPLINE_CURVE_WITH_KNOTS ( 'NONE', 3,
 ( #12322, #43794, #59863, #50414 ),
 .UNSPECIFIED., .F., .F.,
 ( 4, 4 ),
 ( 0.000000000000000000, 1.000000000000000000 ),
 .UNSPECIFIED. ) ;
#15971 = CARTESIAN_POINT ( 'NONE',  ( 6.961329719590000131, 5.346927244140000646, -8.589407719218000281 ) ) ;
#15972 = CARTESIAN_POINT ( 'NONE',  ( 8.493055160192083619, -2.517084544257638612, 6.576072328180241122 ) ) ;
#15973 = CARTESIAN_POINT ( 'NONE',  ( 11.08810207955139937, -4.796537143354000499, -7.174999999999999822 ) ) ;
#15974 = VERTEX_POINT ( 'NONE', #21215 ) ;
#15976 = CARTESIAN_POINT ( 'NONE',  ( 16.39955778315600199, -3.526114926816000139, -11.96132012103000086 ) ) ;
#15975 = AXIS2_PLACEMENT_3D ( 'NONE', #16809, #26972, #31528 ) ;
#15977 = CARTESIAN_POINT ( 'NONE',  ( 11.56566386073000174, 11.72961781202000076, 1.923363593971999963 ) ) ;
#15978 = EDGE_LOOP ( 'NONE', ( #30371, #52965, #54261, #5325 ) ) ;
#15979 = CARTESIAN_POINT ( 'NONE',  ( 24.92741773699590624, 2.996169077880856957, -11.61847982281971881 ) ) ;
#15980 = DIRECTION ( 'NONE',  ( 1.000000000000000000, 0.000000000000000000, 0.000000000000000000 ) ) ;
#15981 = FACE_OUTER_BOUND ( 'NONE', #31904, .T. ) ;
#15982 = EDGE_LOOP ( 'NONE', ( #11149, #21650, #68673, #25770 ) ) ;
#15983 = DIRECTION ( 'NONE',  ( 1.000000000000000000, 0.000000000000000000, 0.000000000000000000 ) ) ;
#15984 = CARTESIAN_POINT ( 'NONE',  ( 7.924878289113897800, 5.349357204871084903, 7.500005630225526687 ) ) ;
#15985 = CARTESIAN_POINT ( 'NONE',  ( 10.56591429142999949, 4.019686495353769651, -6.466681092390999197 ) ) ;
#15986 = CARTESIAN_POINT ( 'NONE',  ( 12.49878241383750321, 3.044913063694494770, -12.30777011605604798 ) ) ;
#15987 = CARTESIAN_POINT ( 'NONE',  ( 11.01810807141099957, -3.940954591493389891, 6.223352037434000117 ) ) ;
#15988 = ORIENTED_EDGE ( 'NONE', *, *, #9398, .F. ) ;
#15989 = CARTESIAN_POINT ( 'NONE',  ( 8.411454719592999396, 3.882020551409000042, 5.870058896428999695 ) ) ;
#15990 = ORIENTED_EDGE ( 'NONE', *, *, #24138, .F. ) ;
#15991 = CARTESIAN_POINT ( 'NONE',  ( 9.383499245234512287, -5.249996043174973259, -7.336369100805424814 ) ) ;
#15992 = CARTESIAN_POINT ( 'NONE',  ( 9.214144353209000826, -5.421531391267000011, 6.381128921159999301 ) ) ;
#15993 = CARTESIAN_POINT ( 'NONE',  ( 11.02144803208000035, 6.131092151569999871, -5.118571239882999890 ) ) ;
#15994 = ORIENTED_EDGE ( 'NONE', *, *, #30658, .F. ) ;
#15995 = FACE_OUTER_BOUND ( 'NONE', #47456, .T. ) ;
#15996 = CARTESIAN_POINT ( 'NONE',  ( 6.032801325126996517, 9.323366446862999979, -4.734513139768997902 ) ) ;
#15997 = CARTESIAN_POINT ( 'NONE',  ( 7.906851002540999929, 2.832432432432000269, -6.822293592207000934 ) ) ;
#15998 = EDGE_CURVE ( 'NONE', #14358, #56969, #59117, .T. ) ;
#15999 = DIRECTION ( 'NONE',  ( 0.000000000000000000, -0.008867170401640422917, -0.9999606858717338120 ) ) ;
#16000 = CARTESIAN_POINT ( 'NONE',  ( 12.10383213726159113, -2.332238815612519112, -13.80437617213671508 ) ) ;
#16001 = EDGE_CURVE ( 'NONE', #47667, #58927, #36265, .T. ) ;
#16002 = CARTESIAN_POINT ( 'NONE',  ( 10.45672469555900008, -3.566534988568399900, -6.750062220519700062 ) ) ;
#16003 = ADVANCED_FACE ( 'NONE', ( #63160 ), #48039, .F. ) ;
#16004 = CARTESIAN_POINT ( 'NONE',  ( 10.90000154029999990, 0.000000000000000000, 0.000000000000000000 ) ) ;
#16005 = CARTESIAN_POINT ( 'NONE',  ( 18.11163387652233681, -2.018964330316879607, 12.43719698804479101 ) ) ;
#16006 = ORIENTED_EDGE ( 'NONE', *, *, #45095, .T. ) ;
#16007 =( BOUNDED_SURFACE ( )  B_SPLINE_SURFACE ( 3, 3, ( 
 ( #35073, #49152, #40640, #22578 ),
 ( #43920, #38315, #3244, #65224 ),
 ( #12445, #2895, #17339, #11740 ),
 ( #33083, #38669, #56738, #59988 ) ),
 .UNSPECIFIED., .F., .F., .F. ) 
 B_SPLINE_SURFACE_WITH_KNOTS ( ( 4, 4 ),
 ( 4, 4 ),
 ( 0.000000000000000000, 1.000000000000000000 ),
 ( 0.000000000000000000, 1.000000000000000000 ),
 .UNSPECIFIED. ) 
 GEOMETRIC_REPRESENTATION_ITEM ( )  RATIONAL_B_SPLINE_SURFACE ( (
 ( 1.512182578520000042, 1.160176301760999840, 1.160176301760999840, 1.512182578520000042),
 ( 1.111288591041000196, 0.8526025270081000196, 0.8526025270081000196, 1.111288591041000196),
 ( 1.111288591041000196, 0.8526025270081000196, 0.8526025270081000196, 1.111288591041000196),
 ( 1.512182578520000042, 1.160176301760999840, 1.160176301760999840, 1.512182578520000042) ) ) 
 REPRESENTATION_ITEM ( '' )  SURFACE ( )  );
#16008 = CARTESIAN_POINT ( 'NONE',  ( 9.515584277044482064, -4.716917290452846245, 6.568532107505763662 ) ) ;
#16009 = ORIENTED_EDGE ( 'NONE', *, *, #12313, .F. ) ;
#16010 = DIRECTION ( 'NONE',  ( 0.000000000000000000, 0.000000000000000000, 1.000000000000000000 ) ) ;
#16011 = CARTESIAN_POINT ( 'NONE',  ( -0.2999999999999999889, -0.5773502691895999739, 1.000000000000000000 ) ) ;
#16012 = LINE ( 'NONE', #58318, #21582 ) ;
#16013 = CARTESIAN_POINT ( 'NONE',  ( 11.03408597791999846, 2.992846905312999795, -9.056576857348998644 ) ) ;
#16014 = DIRECTION ( 'NONE',  ( 0.000000000000000000, 1.000000000000000000, 0.000000000000000000 ) ) ;
#16015 = CARTESIAN_POINT ( 'NONE',  ( 18.18005043890188688, 2.480435639343892440, -12.45614914497210179 ) ) ;
#16016 = CARTESIAN_POINT ( 'NONE',  ( 24.03017386583299952, -13.13663164873999989, 3.281013120054999899 ) ) ;
#16017 = CARTESIAN_POINT ( 'NONE',  ( 8.790860954911998704, 4.097566467530549872, -8.421893466755800972 ) ) ;
#16018 = EDGE_LOOP ( 'NONE', ( #10167, #12074, #12554, #13888, #60911 ) ) ;
#16019 = CARTESIAN_POINT ( 'NONE',  ( 11.57240408529958842, -4.732472998177641443, -7.017887023514779443 ) ) ;
#16020 = CARTESIAN_POINT ( 'NONE',  ( 12.34709291757831195, -2.925445075551590612, 12.34221984780393733 ) ) ;
#16021 = CARTESIAN_POINT ( 'NONE',  ( 2.155140132542666453, 0.9161175952574702741, 3.408904368339106927 ) ) ;
#16022 = CARTESIAN_POINT ( 'NONE',  ( 11.48146005378009882, -3.088328798999600000, 7.986817550794899745 ) ) ;
#16023 = CARTESIAN_POINT ( 'NONE',  ( 18.44383669537300108, 2.795303817231000298, -11.36579926027000020 ) ) ;
#16024 = AXIS2_PLACEMENT_3D ( 'NONE', #23960, #23611, #2633 ) ;
#16025 = CARTESIAN_POINT ( 'NONE',  ( 11.83518044953559922, 4.768048975940600620, -7.900497508315099893 ) ) ;
#16026 = ADVANCED_FACE ( 'NONE', ( #41087 ), #51234, .T. ) ;
#16027 = CARTESIAN_POINT ( 'NONE',  ( 12.76382339226414153, -0.6237239846186475312, 12.67937377942300614 ) ) ;
#16028 = CARTESIAN_POINT ( 'NONE',  ( 5.584969860377806405, -12.14796130797234497, -3.754865623502119831 ) ) ;
#16029 = CARTESIAN_POINT ( 'NONE',  ( 10.25461802485000007, 2.860644035673999941, 6.604613005744999654 ) ) ;
#16030 = CARTESIAN_POINT ( 'NONE',  ( 11.80600022547799988, -3.313997181012000137, 11.22408540768999963 ) ) ;
#16031 = VERTEX_POINT ( 'NONE', #44969 ) ;
#16032 = CARTESIAN_POINT ( 'NONE',  ( 25.29986325275000070, 2.258942858049999725, 11.29419282279020287 ) ) ;
#16033 = CARTESIAN_POINT ( 'NONE',  ( 7.227579511121000166, -0.3967607077929999893, 1.060625802389000061 ) ) ;
#16034 = CARTESIAN_POINT ( 'NONE',  ( 17.83329178774383550, 3.059742244759366514, 13.53861815793071877 ) ) ;
#16035 = CARTESIAN_POINT ( 'NONE',  ( 9.323523248789006956, 2.820543420478710761, -8.179640942048592933 ) ) ;
#16036 = CARTESIAN_POINT ( 'NONE',  ( 24.56500367226799852, 8.792450275430001128, -9.097562849135000462 ) ) ;
#16037 = CARTESIAN_POINT ( 'NONE',  ( 11.11302897915239818, -3.708003626182200030, -8.602736702002999891 ) ) ;
#16038 = ORIENTED_EDGE ( 'NONE', *, *, #56664, .T. ) ;
#16039 = AXIS2_PLACEMENT_3D ( 'NONE', #14684, #62565, #62902 ) ;
#16040 = CARTESIAN_POINT ( 'NONE',  ( 5.657901059018296763, -12.07783836333845073, 3.734765664958815456 ) ) ;
#16041 = CARTESIAN_POINT ( 'NONE',  ( 13.84412491599044337, 8.835575362389644027, 7.593298916478570249 ) ) ;
#16042 = EDGE_CURVE ( 'NONE', #30003, #33549, #8582, .T. ) ;
#16044 = CARTESIAN_POINT ( 'NONE',  ( 9.771640687501500722, -2.873222873813889411, 6.752018918873273989 ) ) ;
#16043 = CARTESIAN_POINT ( 'NONE',  ( 9.600045280412000892, 3.021734963141999852, -6.070209284876999511 ) ) ;
#16045 = CARTESIAN_POINT ( 'NONE',  ( 25.00272599386161332, 11.89255749221432623, -2.924338816029021348 ) ) ;
#16046 = VERTEX_POINT ( 'NONE', #14177 ) ;
#16047 = CARTESIAN_POINT ( 'NONE',  ( 10.59303303094000093, 2.436236667456999960, 7.793464546548000804 ) ) ;
#16048 = CARTESIAN_POINT ( 'NONE',  ( 18.06381123663118871, -2.863168028152635713, -13.58964369048649523 ) ) ;
#16049 = CARTESIAN_POINT ( 'NONE',  ( 10.70287750876920008, 3.530799696887600092, 6.771886227364699806 ) ) ;
#16050 = CARTESIAN_POINT ( 'NONE',  ( 10.34947173981000113, -4.457565973839000328, 6.154866550070000386 ) ) ;
#16051 = CARTESIAN_POINT ( 'NONE',  ( 8.887168146795000112, -2.193670085072000120, 7.400591740205000768 ) ) ;
#16052 = VERTEX_POINT ( 'NONE', #13836 ) ;
#16053 = CARTESIAN_POINT ( 'NONE',  ( 9.316114158771000575, 3.677414437776999723, 9.250745771096999803 ) ) ;
#16054 = B_SPLINE_CURVE_WITH_KNOTS ( 'NONE', 3,
 ( #41109, #57178, #51589, #40414 ),
 .UNSPECIFIED., .F., .F.,
 ( 4, 4 ),
 ( 0.000000000000000000, 1.000000000000000000 ),
 .UNSPECIFIED. ) ;
#16056 = CARTESIAN_POINT ( 'NONE',  ( 10.48598064679000075, -5.506038521567000465, -7.274786670944999756 ) ) ;
#16055 = CARTESIAN_POINT ( 'NONE',  ( 10.37837607040047594, 4.867967756586605965, -7.396454632467190926 ) ) ;
#16057 = CARTESIAN_POINT ( 'NONE',  ( 7.759089400014850035, -5.269491846164327420, 8.691428595288718029 ) ) ;
#16058 = CARTESIAN_POINT ( 'NONE',  ( 17.94287402937880316, -0.4902502634346644905, 13.88836422974693718 ) ) ;
#16059 = CARTESIAN_POINT ( 'NONE',  ( 1.690792463676000112, 0.6682336154344999946, -3.189788463028000454 ) ) ;
#16060 = VERTEX_POINT ( 'NONE', #35166 ) ;
#16061 = CARTESIAN_POINT ( 'NONE',  ( 9.560596873515667227, 4.629523725463624118, -8.592232985442823434 ) ) ;
#16062 = CARTESIAN_POINT ( 'NONE',  ( 11.02641638348499953, -4.974961480482700260, 7.737488872214999702 ) ) ;
#16063 = CARTESIAN_POINT ( 'NONE',  ( 11.42887348028849992, 2.875789035466000065, 6.892162778124999889 ) ) ;
#16064 = EDGE_LOOP ( 'NONE', ( #57785, #25209, #14007, #33744 ) ) ;
#16065 = B_SPLINE_SURFACE_WITH_KNOTS ( 'NONE', 3, 3, ( 
 ( #66415, #18534, #61182, #55938, #29381, #2790, #24115, #45449, #29729, #8387, #4150, #19210, #36322, #25831, #47161, #25490, #24464, #20242, #40534, #56621, #51710, #19902, #8726, #51033, #30401, #31091, #46129, #62202, #30739, #14660, #15345, #63216, #67780, #45789, #62876 ),
 ( #3805, #9062, #61859, #68461, #41228, #41567, #25143, #19560, #46474, #14996, #46818, #36673, #20584, #9394, #41910, #3133, #14323, #35648, #9743, #67101, #13980, #62539, #35976, #40882, #57638, #57292, #56960, #30069, #52399, #35305, #68123, #51372, #4491, #3470, #24806 ),
 ( #67436, #52047, #5873, #6215, #17051, #69162, #63912, #59024, #58330, #27553, #5190, #37351, #64937, #11461, #11128, #26873, #32121, #58676, #16022, #43291, #53438, #10775, #68812, #48882, #48189, #642, #5534, #21271, #291, #21951, #53776, #43640, #989, #32460, #22300 ),
 ( #57993, #10093, #31428, #32802, #21610, #64253, #42943, #52744, #4839, #26180, #47507, #16366, #42601, #20933, #64596, #37695, #42268, #27211, #47855, #48536, #16706, #63572, #38035, #10432, #59361, #54116, #15684, #37018, #31773, #53090, #26527, #6565, #66672, #12166, #17409 ) ),
 .UNSPECIFIED., .F., .F., .F.,
 ( 4, 4 ),
 ( 4, 1, 1, 1, 1, 1, 1, 1, 1, 1, 1, 1, 1, 1, 1, 1, 1, 1, 1, 1, 1, 1, 1, 1, 1, 1, 1, 1, 1, 1, 1, 1, 4 ),
 ( -0.02000000000000000042, 1.020000000000000018 ),
 ( 0.1633025096610999927, 0.1899619885200000136, 0.2166214673788000034, 0.2432809462376999965, 0.2699404250964999585, 0.2965999039553000038, 0.3232593828141999692, 0.3499188616730000145, 0.3765783405318000043, 0.4032378193906999697, 0.4298972982494999595, 0.4565567771083000048, 0.4832162559671999702, 0.5098757348260000155, 0.5365352136848999809, 0.5631946925437000262, 0.5898541714025000715, 0.6165136502614000369, 0.6431731291201999712, 0.6698326079790000165, 0.6964920868378999819, 0.7231515656967000272, 0.7498110445554999615, 0.7764705234143999268, 0.8031300022731999722, 0.8297894811320000175, 0.8564489599908999828, 0.8831084388497000282, 0.9097679177085999935, 0.9364273965674000388, 0.9630868754261999731, 0.9897463542851000495, 1.016405833144000015 ),
 .UNSPECIFIED. ) ;
#16066 = CARTESIAN_POINT ( 'NONE',  ( 9.509454719593000149, 3.116293075258000478, -6.208411413796000033 ) ) ;
#16067 = CARTESIAN_POINT ( 'NONE',  ( 12.53584957871190753, 1.812149883874475176, -12.46900695079346022 ) ) ;
#16068 = CARTESIAN_POINT ( 'NONE',  ( 10.97769598648999967, -2.990523684589000197, 6.898940957443399746 ) ) ;
#16069 = CARTESIAN_POINT ( 'NONE',  ( 24.56665995394800106, -3.304342232863999751, -12.00441819182999836 ) ) ;
#16070 = AXIS2_PLACEMENT_3D ( 'NONE', #284, #48874, #32452 ) ;
#16071 = CARTESIAN_POINT ( 'NONE',  ( 10.64393020684969926, 5.250000000000000000, -7.500000000000000000 ) ) ;
#16072 = ORIENTED_EDGE ( 'NONE', *, *, #48928, .T. ) ;
#16073 = CARTESIAN_POINT ( 'NONE',  ( 16.09996065438095769, -9.056490835163780062, -8.652417574211050066 ) ) ;
#16074 = B_SPLINE_CURVE_WITH_KNOTS ( 'NONE', 3,
 ( #17496, #38820, #65724, #17848, #23771 ),
 .UNSPECIFIED., .F., .F.,
 ( 4, 1, 4 ),
 ( 0.000000000000000000, 0.5000000000000000000, 1.000000000000000000 ),
 .UNSPECIFIED. ) ;
#16075 = CARTESIAN_POINT ( 'NONE',  ( 23.96074334152477192, 9.430604214506258742, 9.306875196542495843 ) ) ;
#16076 = ORIENTED_EDGE ( 'NONE', *, *, #7655, .F. ) ;
#16077 = DIRECTION ( 'NONE',  ( -1.000000000000000000, 0.000000000000000000, 0.000000000000000000 ) ) ;
#16078 = CARTESIAN_POINT ( 'NONE',  ( 10.79718447801629999, 5.003225587801999552, 7.522119512433738997 ) ) ;
#16079 = DIRECTION ( 'NONE',  ( 0.000000000000000000, -0.1807154286440006141, -0.9835354258236025382 ) ) ;
#16080 = CARTESIAN_POINT ( 'NONE',  ( 10.51140238467000110, 2.326714339996000191, -7.741210149842999932 ) ) ;
#16081 = CARTESIAN_POINT ( 'NONE',  ( 8.196365526475007712, 5.108366921470007149, 6.411205986879997099 ) ) ;
#16082 = ADVANCED_FACE ( 'NONE', ( #7547 ), #37435, .F. ) ;
#16083 = CARTESIAN_POINT ( 'NONE',  ( 10.61382642076999971, -3.385081736013999976, 5.849525238167000651 ) ) ;
#16084 = EDGE_CURVE ( 'NONE', #16031, #15625, #17683, .T. ) ;
#16085 = CARTESIAN_POINT ( 'NONE',  ( 17.61479688768388741, -0.7169431667913691575, -12.57958639523259237 ) ) ;
#16086 = DIRECTION ( 'NONE',  ( -1.000000000000000000, 0.000000000000000000, 0.000000000000000000 ) ) ;
#16087 = CARTESIAN_POINT ( 'NONE',  ( 10.84641504065830020, -3.195537720350400068, -6.900173947321999179 ) ) ;
#16088 = ADVANCED_FACE ( 'NONE', ( #47366 ), #58193, .T. ) ;
#16089 = EDGE_CURVE ( 'NONE', #23400, #14432, #21016, .T. ) ;
#16090 = CARTESIAN_POINT ( 'NONE',  ( 8.727045280411999784, 3.882020551409000042, 5.870058896428999695 ) ) ;
#16091 = ORIENTED_EDGE ( 'NONE', *, *, #28689, .T. ) ;
#16092 = CIRCLE ( 'NONE', #26128, 2.100000000000000977 ) ;
#16093 = SHAPE_REPRESENTATION_RELATIONSHIP ( 'NONE' , 'NONE' ,  #26842, #5248 ) ;
#16094 = CARTESIAN_POINT ( 'NONE',  ( 24.71765875488695485, -3.123588627309684895, 11.79180799685195780 ) ) ;
#16095 = DIRECTION ( 'NONE',  ( 1.000000000000000000, 0.000000000000000000, 0.000000000000000000 ) ) ;
#16096 = DIRECTION ( 'NONE',  ( 8.759270281372000635E-11, -8.759291270753999297E-11, 1.000000000000000000 ) ) ;
#16097 = AXIS2_PLACEMENT_3D ( 'NONE', #62000, #9191, #14113 ) ;
#16098 = CARTESIAN_POINT ( 'NONE',  ( 18.25561427624396771, 2.667326636134571771, 12.31445830791193963 ) ) ;
#16099 = CARTESIAN_POINT ( 'NONE',  ( 11.49999035076000276, -3.886252136122000156, 11.90689009355000039 ) ) ;
#16100 = CARTESIAN_POINT ( 'NONE',  ( 11.07109548961999934, 7.377812892753000007, 6.318590435936999761 ) ) ;
#16101 = CARTESIAN_POINT ( 'NONE',  ( 9.241224735070849405, -2.676616289842693952, 7.234190499188664525 ) ) ;
#16102 = CARTESIAN_POINT ( 'NONE',  ( 12.80505043854146940, -1.816877544077282636, 13.85235828181317252 ) ) ;
#16103 = EDGE_LOOP ( 'NONE', ( #49521, #51974, #47827, #9970, #44310 ) ) ;
#16104 = CARTESIAN_POINT ( 'NONE',  ( 12.27226887596755489, -1.991660198615909039, 12.44160671058019041 ) ) ;
#16105 = B_SPLINE_CURVE_WITH_KNOTS ( 'NONE', 3,
 ( #53996, #47735, #59587, #37570, #10318 ),
 .UNSPECIFIED., .F., .F.,
 ( 4, 1, 4 ),
 ( 0.000000000000000000, 0.5000000000000000000, 1.000000000000000000 ),
 .UNSPECIFIED. ) ;
#16106 = CARTESIAN_POINT ( 'NONE',  ( 10.21225461470299933, -4.973404788313100511, -7.747639695388999215 ) ) ;
#16107 = CARTESIAN_POINT ( 'NONE',  ( 11.00000005150999982, -4.755975669291000300E-06, 1.428076682242000113E-06 ) ) ;
#16108 = ADVANCED_FACE ( 'NONE', ( #37213 ), #25343, .T. ) ;
#16109 = CARTESIAN_POINT ( 'NONE',  ( 10.19256470245000123, -2.560274838243000062, 7.664550593243999899 ) ) ;
#16110 = CARTESIAN_POINT ( 'NONE',  ( 11.56795257254739973, -4.963546614172099858, 7.219770138693499817 ) ) ;
#16111 = CARTESIAN_POINT ( 'NONE',  ( 11.55610404293055993, 3.497163090439000310, -8.523936114709998790 ) ) ;
#16112 = CARTESIAN_POINT ( 'NONE',  ( 12.44248249217651647, 0.6233258800551656487, 12.58457734799055139 ) ) ;
#16113 = B_SPLINE_CURVE_WITH_KNOTS ( 'NONE', 3,
 ( #48605, #49286, #24450, #13963 ),
 .UNSPECIFIED., .F., .F.,
 ( 4, 4 ),
 ( 0.000000000000000000, 0.2126015446065814829 ),
 .UNSPECIFIED. ) ;
#16114 = CARTESIAN_POINT ( 'NONE',  ( 8.724507172011824352, 3.875764422069721604, 6.625492773506611144 ) ) ;
#16115 = CARTESIAN_POINT ( 'NONE',  ( 9.773145834241621088, 2.820529238741949385, -8.179623275354476419 ) ) ;
#16116 = CARTESIAN_POINT ( 'NONE',  ( 12.44904482565494419, 1.853472941501685289, 12.46293187093603194 ) ) ;
#16118 = CARTESIAN_POINT ( 'NONE',  ( 8.368323341230000878, 4.780986922229000236, 6.267222470044999660 ) ) ;
#16117 = CARTESIAN_POINT ( 'NONE',  ( 9.099784697134998268, 4.619613413415000203, -6.540930833646799947 ) ) ;
#16119 = CARTESIAN_POINT ( 'NONE',  ( 11.30995122972050027, 4.452766304612699955, -6.452959986593999275 ) ) ;
#16120 = CARTESIAN_POINT ( 'NONE',  ( 8.220124669774001802, 3.381964873247001790, -6.130490311850000928 ) ) ;
#16121 = CARTESIAN_POINT ( 'NONE',  ( 11.26847444708000090, 2.565620268983000329, -7.116623294300999270 ) ) ;
#16122 = CARTESIAN_POINT ( 'NONE',  ( 10.03590035061499997, 4.340961869598300105, -8.732935057095000175 ) ) ;
#16124 = CARTESIAN_POINT ( 'NONE',  ( 12.20227052528876044, 2.665223631340718935, 12.41153314565065457 ) ) ;
#16123 = DIRECTION ( 'NONE',  ( 1.000000000000000000, 0.000000000000000000, 0.000000000000000000 ) ) ;
#16125 = CARTESIAN_POINT ( 'NONE',  ( 11.18424042080583369, -3.455907502640803486, -6.342116603374312156 ) ) ;
#16126 = ORIENTED_EDGE ( 'NONE', *, *, #9861, .T. ) ;
#16127 = VECTOR ( 'NONE', #62041, 1000.000000000000000 ) ;
#16128 = FACE_OUTER_BOUND ( 'NONE', #19614, .T. ) ;
#16129 = CARTESIAN_POINT ( 'NONE',  ( 9.041074696475142503, 2.899999999999999911, 6.201633003104277897 ) ) ;
#16130 = EDGE_CURVE ( 'NONE', #46269, #48331, #27712, .T. ) ;
#16131 = LINE ( 'NONE', #37456, #39664 ) ;
#16132 = CARTESIAN_POINT ( 'NONE',  ( 9.323721904869998411, 4.756019688173900306, 7.075568408810499754 ) ) ;
#16133 = B_SPLINE_CURVE_WITH_KNOTS ( 'NONE', 3,
 ( #67724, #52346, #62485, #4097, #9340, #36964, #31038, #20186 ),
 .UNSPECIFIED., .F., .F.,
 ( 4, 2, 2, 4 ),
 ( 0.000000000000000000, 0.2499999999999992228, 0.4999999999999984457, 1.000000000000000000 ),
 .UNSPECIFIED. ) ;
#16134 = EDGE_CURVE ( 'NONE', #23202, #21742, #31630, .T. ) ;
#16135 = CARTESIAN_POINT ( 'NONE',  ( 12.24735473125027774, -2.217676833728435604, 13.72929951782216484 ) ) ;
#16136 = CARTESIAN_POINT ( 'NONE',  ( 12.18106278541542054, 2.459077072170055001, 13.68201856772054548 ) ) ;
#16137 = CARTESIAN_POINT ( 'NONE',  ( 8.975960865537832234, -5.125960927305071024, -7.646523491995670163 ) ) ;
#16138 = ORIENTED_EDGE ( 'NONE', *, *, #26355, .T. ) ;
#16139 = CARTESIAN_POINT ( 'NONE',  ( 5.253261820982999986, 0.3908910841886000243, 1.214078939262000167 ) ) ;
#16140 = CIRCLE ( 'NONE', #55228, 13.89999856298999958 ) ;
#16141 = CARTESIAN_POINT ( 'NONE',  ( 18.17590806570262529, 2.418078130900048972, -13.69056546383534290 ) ) ;
#16142 = LINE ( 'NONE', #63334, #66728 ) ;
#16143 = CARTESIAN_POINT ( 'NONE',  ( 5.699999772733999492, -12.03770622561999915, -3.722046322334000124 ) ) ;
#16144 = CARTESIAN_POINT ( 'NONE',  ( 18.14681149257596360, 2.701359571199342113, -12.40239981104076605 ) ) ;
#16145 = CARTESIAN_POINT ( 'NONE',  ( 9.681310023244000362, -3.426978632899654542, 8.622334741229296995 ) ) ;
#16146 = CARTESIAN_POINT ( 'NONE',  ( 17.83361872141519910, 3.059864849503202588, 12.30332992014442439 ) ) ;
#16147 = CARTESIAN_POINT ( 'NONE',  ( 11.53142637459347775, -3.735369041114874111, 11.95516355327115399 ) ) ;
#16148 = CARTESIAN_POINT ( 'NONE',  ( 10.50898185320999900, -4.485028460808000439, -9.114431591966999591 ) ) ;
#16149 = CARTESIAN_POINT ( 'NONE',  ( 12.75598089128350665, 1.787835849362446439, 13.88537514715543608 ) ) ;
#16150 = CARTESIAN_POINT ( 'NONE',  ( 24.53428985175800037, 12.47024902693999948, -3.026245299674999778 ) ) ;
#16151 = CARTESIAN_POINT ( 'NONE',  ( 23.60000334400854527, 10.25389668638031004, -9.379908238711360369 ) ) ;
#16152 = CARTESIAN_POINT ( 'NONE',  ( 9.050000000000000711, 0.000000000000000000, 4.000000000000000000 ) ) ;
#16153 = AXIS2_PLACEMENT_3D ( 'NONE', #37322, #38705, #49190 ) ;
#16154 = EDGE_LOOP ( 'NONE', ( #16350, #55419, #27539, #6966 ) ) ;
#16155 = CARTESIAN_POINT ( 'NONE',  ( 9.939260841229000221, 5.099602161831000124, -9.049221499261999924 ) ) ;
#16156 = CARTESIAN_POINT ( 'NONE',  ( 11.69518313518939934, -4.537300658085600347, 6.820583637845799352 ) ) ;
#16157 = ORIENTED_EDGE ( 'NONE', *, *, #52103, .T. ) ;
#16158 = B_SPLINE_CURVE_WITH_KNOTS ( 'NONE', 3,
 ( #7135, #34063, #29168, #50476 ),
 .UNSPECIFIED., .F., .F.,
 ( 4, 4 ),
 ( 0.000000000000000000, 1.000000000000000000 ),
 .UNSPECIFIED. ) ;
#16159 = CARTESIAN_POINT ( 'NONE',  ( 13.68260097612285264, 12.30227370000273268, 2.353106563168188003 ) ) ;
#16160 = CARTESIAN_POINT ( 'NONE',  ( 10.39918582084299992, -4.746348444722899629, -6.637298362509499228 ) ) ;
#16161 = EDGE_LOOP ( 'NONE', ( #44764, #20117, #24015, #52131 ) ) ;
#16162 = CARTESIAN_POINT ( 'NONE',  ( 10.59725056272499977, 5.316133253199000208, 7.480494252843770120 ) ) ;
#16163 = CARTESIAN_POINT ( 'NONE',  ( 24.30001680216799897, -3.271769318036999774, 12.21048166890999909 ) ) ;
#16164 = CARTESIAN_POINT ( 'NONE',  ( 18.31802873821099809, -2.927761598026000112, 11.42873208727000112 ) ) ;
#16165 = CARTESIAN_POINT ( 'NONE',  ( 10.69568717260499824, -4.466067913030199676, -8.260703168378098482 ) ) ;
#16166 = CARTESIAN_POINT ( 'NONE',  ( 9.779346873515665450, -4.163624617374463988, -6.249999999999999112 ) ) ;
#16167 = CARTESIAN_POINT ( 'NONE',  ( 7.000000000000000000, -6.495985883990673670, -3.000000000000000000 ) ) ;
#16168 = CARTESIAN_POINT ( 'NONE',  ( 13.36715644869600084, 11.69666705770999826, 2.137627928029000035 ) ) ;
#16169 = EDGE_LOOP ( 'NONE', ( #43529, #24211, #32961, #68533 ) ) ;
#16170 = EDGE_CURVE ( 'NONE', #33857, #23094, #47949, .T. ) ;
#16171 = EDGE_CURVE ( 'NONE', #19987, #63565, #56879, .T. ) ;
#16172 = CARTESIAN_POINT ( 'NONE',  ( 9.915635841230999503, 3.210851187372000037, -6.346613542714999667 ) ) ;
#16173 = EDGE_LOOP ( 'NONE', ( #5504, #52610, #28554 ) ) ;
#16174 = CARTESIAN_POINT ( 'NONE',  ( 0.1801026475008349892, 1.156975259834909453, -3.039500339280597263 ) ) ;
#16175 = ORIENTED_EDGE ( 'NONE', *, *, #55596, .F. ) ;
#16176 = CARTESIAN_POINT ( 'NONE',  ( 8.946747021775999897, 3.038503783616799847, 6.656252755052399550 ) ) ;
#16177 = CARTESIAN_POINT ( 'NONE',  ( 18.16462229618758428, -2.361607881905639417, -12.48272818380096894 ) ) ;
#16178 =( GEOMETRIC_REPRESENTATION_CONTEXT ( 3 ) GLOBAL_UNCERTAINTY_ASSIGNED_CONTEXT ( ( #60254 ) ) GLOBAL_UNIT_ASSIGNED_CONTEXT ( ( #45434, #61508, #8373 ) ) REPRESENTATION_CONTEXT ( 'NONE', 'WORKASPACE' ) );
#16179 = CARTESIAN_POINT ( 'NONE',  ( 10.58522900337914052, -2.975308710305338167, 5.037100615727592157 ) ) ;
#16180 = CARTESIAN_POINT ( 'NONE',  ( 10.14393020684899938, 5.250000000000000000, -7.500000000000000000 ) ) ;
#16181 = CARTESIAN_POINT ( 'NONE',  ( 27.64127793187000037, 11.00717859340000082, -1.432487142323000118 ) ) ;
#16182 = CARTESIAN_POINT ( 'NONE',  ( 12.72272221947699045, 0.6198980793944576240, 13.88138779565240100 ) ) ;
#16183 = ORIENTED_EDGE ( 'NONE', *, *, #13990, .F. ) ;
#16184 = CARTESIAN_POINT ( 'NONE',  ( 12.25978835901500119, 11.49417283396999956, -4.331891014347999835 ) ) ;
#16185 = FACE_OUTER_BOUND ( 'NONE', #29640, .T. ) ;
#16186 = EDGE_CURVE ( 'NONE', #65344, #19244, #20102, .T. ) ;
#16187 = B_SPLINE_CURVE_WITH_KNOTS ( 'NONE', 1,
 ( #12623, #33952 ),
 .UNSPECIFIED., .F., .F.,
 ( 2, 2 ),
 ( 0.000000000000000000, 1.000000000000000000 ),
 .UNSPECIFIED. ) ;
#16188 = CARTESIAN_POINT ( 'NONE',  ( 10.03743284169262573, 3.545113930219122800, 8.247402791297171021 ) ) ;
#16189 = CARTESIAN_POINT ( 'NONE',  ( 5.232160619701999416, -0.3008961189268999914, 1.086704895458000086 ) ) ;
#16190 = CARTESIAN_POINT ( 'NONE',  ( 9.594139158774000364, 2.212639797530000063, -6.855876382544999537 ) ) ;
#16191 = VECTOR ( 'NONE', #25990, 1000.000000000000114 ) ;
#16192 = CARTESIAN_POINT ( 'NONE',  ( 18.44496314779700086, -2.860815007322000447, 12.13831535021000008 ) ) ;
#16193 = CARTESIAN_POINT ( 'NONE',  ( 10.14584566409999944, -5.370505908760000224, -6.826219946961000318 ) ) ;
#16194 = ORIENTED_EDGE ( 'NONE', *, *, #64871, .F. ) ;
#16195 = ORIENTED_EDGE ( 'NONE', *, *, #22725, .F. ) ;
#16196 = CARTESIAN_POINT ( 'NONE',  ( 8.722235841230000730, 3.844886277615000125, -8.888911790991000927 ) ) ;
#16197 = CARTESIAN_POINT ( 'NONE',  ( 11.50004197952388552, 11.55567553918560542, 1.481524017262679127 ) ) ;
#16198 = CARTESIAN_POINT ( 'NONE',  ( 18.27946005101761884, -2.709881966525854224, 13.73658560568321185 ) ) ;
#16199 = CARTESIAN_POINT ( 'NONE',  ( 13.55563472374800149, 9.144188282469000839, 7.452974878632000255 ) ) ;
#16200 = CARTESIAN_POINT ( 'NONE',  ( 12.80505043854144276, 0.7192913403693015351, 12.57945229203838267 ) ) ;
#16201 = CARTESIAN_POINT ( 'NONE',  ( 24.84557873272407136, -3.513964920196102071, -11.93639205272353010 ) ) ;
#16202 = CARTESIAN_POINT ( 'NONE',  ( 10.26788779216199821, 4.929030047862200448, -7.835030859477799758 ) ) ;
#16204 = CARTESIAN_POINT ( 'NONE',  ( 2.040019101166500093, 3.500000000000000888, -0.4817981237446227749 ) ) ;
#16203 = CARTESIAN_POINT ( 'NONE',  ( 9.749747021775998945, -4.754947163618299832, 6.837506920432799618 ) ) ;
#16205 = CARTESIAN_POINT ( 'NONE',  ( 5.700000000000000178, 13.04986661130000059, 1.811520473896000016 ) ) ;
#16206 = ORIENTED_EDGE ( 'NONE', *, *, #26881, .T. ) ;
#16207 = CARTESIAN_POINT ( 'NONE',  ( 9.719606904206999687, -5.967761543230999166, 7.406644089178000101 ) ) ;
#16208 = CARTESIAN_POINT ( 'NONE',  ( 10.54555864497999984, 5.007105485494000696, 6.711254117843599154 ) ) ;
#16209 = CARTESIAN_POINT ( 'NONE',  ( 11.09999999999999964, 6.361341001828001218, -5.393275588238999774 ) ) ;
#16210 = CARTESIAN_POINT ( 'NONE',  ( 9.753140057121997941, -4.104977100659999323, 9.293279163877999238 ) ) ;
#16211 = EDGE_CURVE ( 'NONE', #14714, #43600, #24363, .T. ) ;
#16212 = CARTESIAN_POINT ( 'NONE',  ( 18.09742839075014587, 2.810734143470918767, -12.37374591514403122 ) ) ;
#16213 = CARTESIAN_POINT ( 'NONE',  ( 9.731876262297951996, -2.899999999999999911, -6.324732395500358706 ) ) ;
#16214 = CIRCLE ( 'NONE', #66477, 12.99999867215000116 ) ;
#16215 = CARTESIAN_POINT ( 'NONE',  ( 11.02452225494999993, 2.775477745048999800, -6.571291218949999902 ) ) ;
#16216 = CARTESIAN_POINT ( 'NONE',  ( 9.763317406968999634, -3.838745722419000028, -8.351883209406098629 ) ) ;
#16217 = CARTESIAN_POINT ( 'NONE',  ( 5.930189463737000288, 0.7526323975856999970, -1.087207638099000118 ) ) ;
#16218 = B_SPLINE_SURFACE_WITH_KNOTS ( 'NONE', 3, 3, ( 
 ( #57078, #41350, #3926, #47285 ),
 ( #62661, #30518, #36100, #9520 ),
 ( #21055, #62994, #30862, #63690 ),
 ( #15122, #36443, #9871, #15805 ),
 ( #57760, #31215, #20709, #38153 ) ),
 .UNSPECIFIED., .F., .F., .F.,
 ( 4, 1, 4 ),
 ( 4, 4 ),
 ( 0.9643675639056999982, 1.000000000000000000, 1.004735132284999999 ),
 ( -0.1730180444169999998, 1.173018043257999965 ),
 .UNSPECIFIED. ) ;
#16219 = DIRECTION ( 'NONE',  ( -1.000000000000000000, 0.000000000000000000, 0.000000000000000000 ) ) ;
#16220 = CARTESIAN_POINT ( 'NONE',  ( 0.1499942179680000542, -2.749953718116142198, -0.3599680999394080372 ) ) ;
#16221 = ORIENTED_EDGE ( 'NONE', *, *, #26372, .T. ) ;
#16222 = CARTESIAN_POINT ( 'NONE',  ( 12.25134400021322456, 0.2899325138666232204, -12.69554708236672980 ) ) ;
#16223 = CARTESIAN_POINT ( 'NONE',  ( 11.71210404293059959, 3.618181340822599790, -8.277504409418298792 ) ) ;
#16224 = CARTESIAN_POINT ( 'NONE',  ( 5.399998984437000438, -12.98068687585000092, 1.765643277146000001 ) ) ;
#16225 = CARTESIAN_POINT ( 'NONE',  ( 10.26811392801000089, -4.000000000000000000, 4.767677575776000154 ) ) ;
#16226 = CARTESIAN_POINT ( 'NONE',  ( 1.665556799207791983, 0.4581489286485003198, 3.500000000000000444 ) ) ;
#16227 = EDGE_LOOP ( 'NONE', ( #35972, #36248, #57866 ) ) ;
#16228 = CARTESIAN_POINT ( 'NONE',  ( 25.25778441053600076, -11.13231713549000013, -3.460093662997999697 ) ) ;
#16229 = APPLICATION_PROTOCOL_DEFINITION ( 'draft international standard', 'automotive_design', 1998, #23077 ) ;
#16230 = CARTESIAN_POINT ( 'NONE',  ( 10.48280513895999988, -3.096689368913399854, -6.997844089834400094 ) ) ;
#16231 = LINE ( 'NONE', #48395, #506 ) ;
#16232 = CARTESIAN_POINT ( 'NONE',  ( 8.819055905797000605, 2.899999999999999911, -6.571291218949999902 ) ) ;
#16233 = CARTESIAN_POINT ( 'NONE',  ( 4.574515983791000080E-07, 0.000000000000000000, -2.400000066502543827 ) ) ;
#16234 = CARTESIAN_POINT ( 'NONE',  ( 11.44366954483529852, 4.485203148598100320, -6.751356298874699569 ) ) ;
#16235 = ORIENTED_EDGE ( 'NONE', *, *, #5592, .T. ) ;
#16236 = CARTESIAN_POINT ( 'NONE',  ( 9.632185590920999019, -5.638162562978999759, 6.476633609657000079 ) ) ;
#16237 = CARTESIAN_POINT ( 'NONE',  ( 18.01279121882204137, 2.925678518064911859, -13.57390968381829310 ) ) ;
#16238 = ORIENTED_EDGE ( 'NONE', *, *, #53369, .F. ) ;
#16239 = CARTESIAN_POINT ( 'NONE',  ( 6.992194708760999688, -9.194551129401000722, 5.189166568983999639 ) ) ;
#16240 = CARTESIAN_POINT ( 'NONE',  ( 7.775620559622000272, -4.636725880537000855, 9.378965771357000492 ) ) ;
#16241 = AXIS2_PLACEMENT_3D ( 'NONE', #57729, #19997, #30831 ) ;
#16242 = CARTESIAN_POINT ( 'NONE',  ( 9.518314158773000244, 4.845406482350000488, -6.387189183984999907 ) ) ;
#16243 = ORIENTED_EDGE ( 'NONE', *, *, #38938, .T. ) ;
#16244 = FACE_OUTER_BOUND ( 'NONE', #152, .T. ) ;
#16245 = CARTESIAN_POINT ( 'NONE',  ( 18.12841930325693696, 0.2489729014332486556, -12.69672092236991112 ) ) ;
#16246 = LINE ( 'NONE', #58904, #23061 ) ;
#16247 = CARTESIAN_POINT ( 'NONE',  ( 8.154750263806279875, -3.054975986857539016, 6.324465894181788173 ) ) ;
#16248 = ORIENTED_EDGE ( 'NONE', *, *, #134, .T. ) ;
#16249 = CARTESIAN_POINT ( 'NONE',  ( 9.166075977534999808, -4.023333687735000552, 9.122281080215000060 ) ) ;
#16250 = EDGE_CURVE ( 'NONE', #1910, #29725, #65802, .T. ) ;
#16251 = EDGE_CURVE ( 'NONE', #13504, #14332, #50199, .T. ) ;
#16252 = CARTESIAN_POINT ( 'NONE',  ( 25.57800075372000137, 11.11254651097000057, -3.219695634887000057 ) ) ;
#16253 = CARTESIAN_POINT ( 'NONE',  ( 9.573148997458000409, 5.167567567567999731, -6.822293592207000934 ) ) ;
#16254 = VERTEX_POINT ( 'NONE', #31981 ) ;
#16255 = CARTESIAN_POINT ( 'NONE',  ( 6.190443173016666023, 0.1963495408493637351, -1.499999999999999778 ) ) ;
#16256 = CARTESIAN_POINT ( 'NONE',  ( 10.61442944038000036, -5.287639274524000399, -7.937245019889999753 ) ) ;
#16257 = ORIENTED_EDGE ( 'NONE', *, *, #25874, .T. ) ;
#16258 = CARTESIAN_POINT ( 'NONE',  ( 11.59999999999999964, 5.207010770456999893, 7.174999999999999822 ) ) ;
#16259 = CARTESIAN_POINT ( 'NONE',  ( 17.99974802964005605, -1.911958328522573414, -12.45409441785080773 ) ) ;
#16260 = CARTESIAN_POINT ( 'NONE',  ( 4.761187934510999753, 1.262677799937000023, -0.9118658990719999968 ) ) ;
#16261 = CARTESIAN_POINT ( 'NONE',  ( 8.021466877102001902, 5.126313762262000751, -6.742875694880997806 ) ) ;
#16262 = CARTESIAN_POINT ( 'NONE',  ( 16.15930817923600316, 3.787151970053999950, 11.97924296128000066 ) ) ;
#16263 = CARTESIAN_POINT ( 'NONE',  ( 11.23424042080529972, 4.544092497359197402, 8.657883396625686956 ) ) ;
#16264 = CARTESIAN_POINT ( 'NONE',  ( 9.210288521113000115, -4.352953559891299840, 6.715449042252499723 ) ) ;
#16265 = B_SPLINE_CURVE_WITH_KNOTS ( 'NONE', 3,
 ( #1604, #66261, #13143, #40058, #18041 ),
 .UNSPECIFIED., .F., .F.,
 ( 4, 1, 4 ),
 ( 0.000000000000000000, 0.5000000000000000000, 1.000000000000000000 ),
 .UNSPECIFIED. ) ;
#16266 = VERTEX_POINT ( 'NONE', #15199 ) ;
#16267 = CARTESIAN_POINT ( 'NONE',  ( 9.629471092178999214, -5.100000000000000533, 6.152188490330000370 ) ) ;
#16268 = EDGE_LOOP ( 'NONE', ( #33057, #3954 ) ) ;
#16269 = CARTESIAN_POINT ( 'NONE',  ( 10.44675156161000018, 2.885046387990999772, 8.863482298832000339 ) ) ;
#16270 = FACE_OUTER_BOUND ( 'NONE', #26819, .T. ) ;
#16271 = ADVANCED_FACE ( 'NONE', ( #36524 ), #20789, .T. ) ;
#16272 = CARTESIAN_POINT ( 'NONE',  ( 18.19067337301504494, -12.06199139229578066, 3.374301501848208762 ) ) ;
#16273 = CARTESIAN_POINT ( 'NONE',  ( 12.39809172042338759, 2.025537470422473341, -13.76271392731541354 ) ) ;
#16274 = CARTESIAN_POINT ( 'NONE',  ( 10.02462472190973486, 2.899999999999999911, -6.445686799157789082 ) ) ;
#16275 = EDGE_CURVE ( 'NONE', #29023, #42061, #21136, .T. ) ;
#16276 = LINE ( 'NONE', #21519, #27620 ) ;
#16277 = CARTESIAN_POINT ( 'NONE',  ( 17.55505043854143921, -0.6250000000000001110, 13.88107975066923316 ) ) ;
#16278 = AXIS2_PLACEMENT_3D ( 'NONE', #1086, #737, #59118 ) ;
#16279 = CARTESIAN_POINT ( 'NONE',  ( 9.291454852466372927, -5.435482730291879783, -6.499550932516991786 ) ) ;
#16280 = VERTEX_POINT ( 'NONE', #63770 ) ;
#16281 = CARTESIAN_POINT ( 'NONE',  ( 12.82764013820600013, -11.38891548326999903, 4.574441164091999745 ) ) ;
#16282 = CARTESIAN_POINT ( 'NONE',  ( 12.10118044953561878, -2.866798846279000390, 6.909094663619399945 ) ) ;
#16283 = CARTESIAN_POINT ( 'NONE',  ( 18.11245875480856071, -0.2828881521639263763, -13.89612849060967648 ) ) ;
#16284 = CARTESIAN_POINT ( 'NONE',  ( 7.539230646792000279, -4.696237245142999228, 5.830277424166999900 ) ) ;
#16286 = CARTESIAN_POINT ( 'NONE',  ( 18.22958618735997049, 11.12724485990802847, -3.450621024319545427 ) ) ;
#16285 = CARTESIAN_POINT ( 'NONE',  ( 10.37873747135000002, 4.882725050998000249, 6.350806206758999650 ) ) ;
#16287 = CARTESIAN_POINT ( 'NONE',  ( 10.32533997688000049, 4.243109097101799954, -6.385465081946999355 ) ) ;
#16288 = VECTOR ( 'NONE', #3652, 1000.000000000000000 ) ;
#16289 = CARTESIAN_POINT ( 'NONE',  ( 24.55996189763800075, -8.848787117368999589, -9.333438204885000644 ) ) ;
#16290 = AXIS2_PLACEMENT_3D ( 'NONE', #15916, #36561, #36912 ) ;
#16291 = CARTESIAN_POINT ( 'NONE',  ( 9.526355082327999213, 3.611978631017199959, -6.724663065681199647 ) ) ;
#16292 = CARTESIAN_POINT ( 'NONE',  ( 18.08578179881429548, -0.3302353423713645375, 12.69422546839060395 ) ) ;
#16293 = CARTESIAN_POINT ( 'NONE',  ( 6.649829208513000189, -1.325979800714000012, 0.4909860521821999835 ) ) ;
#16294 = CARTESIAN_POINT ( 'NONE',  ( 17.89107826690531056, -3.595094513005585135, 11.99795484439375848 ) ) ;
#16295 = ORIENTED_EDGE ( 'NONE', *, *, #41039, .T. ) ;
#16296 = CARTESIAN_POINT ( 'NONE',  ( 9.149956853208999874, -4.175914961544999748, 5.699510287082000026 ) ) ;
#16297 = CARTESIAN_POINT ( 'NONE',  ( 8.513433059625000965, -5.040796345420999636, 8.522966281393001609 ) ) ;
#16298 = CARTESIAN_POINT ( 'NONE',  ( 7.716851002542999716, -2.832432432432000269, 6.822293592207000934 ) ) ;
#16299 = CARTESIAN_POINT ( 'NONE',  ( 17.60000000798000386, 11.41069016990000051, -4.623987642516999230 ) ) ;
#16300 = ORIENTED_EDGE ( 'NONE', *, *, #47968, .F. ) ;
#16301 = CARTESIAN_POINT ( 'NONE',  ( 0.5350461241980000171, -2.512770725774000180, 2.251027108384000108 ) ) ;
#16302 = CARTESIAN_POINT ( 'NONE',  ( 10.64902344389989963, 3.116469856398800253, 8.036199780531900316 ) ) ;
#16303 = CARTESIAN_POINT ( 'NONE',  ( 11.35906500789999996, 2.719101288111000159, -7.157645240044000268 ) ) ;
#16304 = ADVANCED_FACE ( 'NONE', ( #15881 ), #26849, .F. ) ;
#16305 = ORIENTED_EDGE ( 'NONE', *, *, #64949, .T. ) ;
#16306 = EDGE_CURVE ( 'NONE', #25126, #9641, #31923, .T. ) ;
#16307 = CARTESIAN_POINT ( 'NONE',  ( 9.248087964304161801, 4.327168543240617282, -6.282577178243121452 ) ) ;
#16308 = CARTESIAN_POINT ( 'NONE',  ( 10.86301932002748138, -5.250000000000001776, -7.799851088612627770 ) ) ;
#16309 = CARTESIAN_POINT ( 'NONE',  ( 17.90971610687748594, 3.107943374821388272, -12.21068061720391995 ) ) ;
#16310 = CARTESIAN_POINT ( 'NONE',  ( 7.955097046864369581, -4.953350247991573418, 6.431944445602010063 ) ) ;
#16311 = CARTESIAN_POINT ( 'NONE',  ( 9.362885841227999606, 3.677414437776999723, 9.250745771096999803 ) ) ;
#16312 = VERTEX_POINT ( 'NONE', #10985 ) ;
#16313 = CARTESIAN_POINT ( 'NONE',  ( 6.104775144120000441, -0.04112960214766999550, -1.467935932961000001 ) ) ;
#16314 = CARTESIAN_POINT ( 'NONE',  ( 7.209954719586999516, 2.634456420141999988, -6.433888043919999689 ) ) ;
#16315 = CARTESIAN_POINT ( 'NONE',  ( 8.554703854670005825, -3.570844187153873417, 5.814174462132309706 ) ) ;
#16316 = CARTESIAN_POINT ( 'NONE',  ( 9.142797255588000382, -2.721932483203000075, 7.554109351283189611 ) ) ;
#16317 = EDGE_LOOP ( 'NONE', ( #24858, #36537, #60978, #31920, #24563 ) ) ;
#16318 = DIRECTION ( 'NONE',  ( 0.000000000000000000, 0.9916377111174247139, 0.1290528957048031888 ) ) ;
#16319 = CARTESIAN_POINT ( 'NONE',  ( 6.355026506350000659, 1.500000000000000000, 0.000000000000000000 ) ) ;
#16320 = ORIENTED_EDGE ( 'NONE', *, *, #55932, .T. ) ;
#16321 = CARTESIAN_POINT ( 'NONE',  ( 25.22253823781074900, 2.724025653123483881, -11.39869274941884392 ) ) ;
#16322 = CARTESIAN_POINT ( 'NONE',  ( 7.721047324851166849, -2.916517839021724789, 6.666908917546550128 ) ) ;
#16323 = AXIS2_PLACEMENT_3D ( 'NONE', #41890, #63196, #4819 ) ;
#16324 = CARTESIAN_POINT ( 'NONE',  ( 17.55505043854147118, -3.199698446519375850, -12.18695736643652694 ) ) ;
#16325 = VERTEX_POINT ( 'NONE', #37897 ) ;
#16326 = CARTESIAN_POINT ( 'NONE',  ( 11.59999999999999964, -4.883784007588900522, -7.825000000000000178 ) ) ;
#16327 = CARTESIAN_POINT ( 'NONE',  ( 9.715118312915786092, -4.417515367316165786, -8.786662241963096420 ) ) ;
#16328 = CARTESIAN_POINT ( 'NONE',  ( 23.73953470779122554, -13.33634092520827252, 3.648239340457724467 ) ) ;
#16329 = CARTESIAN_POINT ( 'NONE',  ( 11.29998636608000062, 3.695122995756999984, -11.25914041192000070 ) ) ;
#16330 = CARTESIAN_POINT ( 'NONE',  ( 11.60887482311539998, -2.815046254222000055, 7.021250586468399391 ) ) ;
#16331 = ORIENTED_EDGE ( 'NONE', *, *, #23754, .T. ) ;
#16332 = CARTESIAN_POINT ( 'NONE',  ( 9.015545280411000562, 4.175915362023999933, 5.699506188181000077 ) ) ;
#16333 = EDGE_CURVE ( 'NONE', #8503, #23086, #28586, .T. ) ;
#16334 = ADVANCED_FACE ( 'NONE', ( #27769 ), #496, .T. ) ;
#16335 = ORIENTED_EDGE ( 'NONE', *, *, #58247, .F. ) ;
#16336 = CARTESIAN_POINT ( 'NONE',  ( 10.09393020685000053, -2.750000000000000000, 7.500000000000000000 ) ) ;
#16337 = VECTOR ( 'NONE', #5299, 1000.000000000000227 ) ;
#16338 = ADVANCED_FACE ( 'NONE', ( #21811 ), #22499, .T. ) ;
#16339 = CARTESIAN_POINT ( 'NONE',  ( 17.92027680868936201, 0.6284010951822294189, 12.58437167746827789 ) ) ;
#16340 = CARTESIAN_POINT ( 'NONE',  ( 11.01665246377999985, 5.432467678272000278, -4.991868250041999744 ) ) ;
#16341 = ORIENTED_EDGE ( 'NONE', *, *, #12355, .F. ) ;
#16342 = CARTESIAN_POINT ( 'NONE',  ( 5.500000000000000000, 0.000000000000000000, 0.000000000000000000 ) ) ;
#16343 = CARTESIAN_POINT ( 'NONE',  ( 10.73976354018279977, 3.672815144550903632, -6.282534154164605589 ) ) ;
#16344 = CARTESIAN_POINT ( 'NONE',  ( 8.983146706529641534, 2.899999999999999911, 6.231099004629861327 ) ) ;
#16345 = CARTESIAN_POINT ( 'NONE',  ( 8.475341021510232054, 5.350570349241480450, 7.499981640446101494 ) ) ;
#16346 = CARTESIAN_POINT ( 'NONE',  ( 12.10457356466343626, -2.707610175640964734, -13.73569711802853277 ) ) ;
#16347 = CARTESIAN_POINT ( 'NONE',  ( 10.32949413291699869, -3.087070836781100169, -7.083453279150199400 ) ) ;
#16348 = CARTESIAN_POINT ( 'NONE',  ( 13.69997185827399910, -9.599065136398367670, -6.667560658748436175 ) ) ;
#16349 = CARTESIAN_POINT ( 'NONE',  ( 18.28003019995800571, -2.460172313524578325, 12.35749544995779559 ) ) ;
#16350 = ORIENTED_EDGE ( 'NONE', *, *, #64235, .F. ) ;
#16351 = CARTESIAN_POINT ( 'NONE',  ( 11.55300581613033906, -2.892415530317000272, -8.211208432468300344 ) ) ;
#16352 = ORIENTED_EDGE ( 'NONE', *, *, #36928, .F. ) ;
#16353 = CARTESIAN_POINT ( 'NONE',  ( 11.26490954471000094, -12.17992731521000138, -1.606774076355000025 ) ) ;
#16354 = FACE_OUTER_BOUND ( 'NONE', #14615, .T. ) ;
#16355 = CARTESIAN_POINT ( 'NONE',  ( 9.975298369746390392, 5.350379160513678123, 7.499985214262784083 ) ) ;
#16356 = ADVANCED_FACE ( 'NONE', ( #43145 ), #64446, .T. ) ;
#16357 = CARTESIAN_POINT ( 'NONE',  ( 10.56591477248000110, -5.293237054095000005, -7.067083954277999958 ) ) ;
#16358 = PLANE ( 'NONE',  #60699 ) ;
#16359 = CARTESIAN_POINT ( 'NONE',  ( 24.38581461189300015, -12.22838082518000036, 3.200660937889999946 ) ) ;
#16360 = CARTESIAN_POINT ( 'NONE',  ( 10.31667774810000004, 3.819530253758000260, 6.062195927068000145 ) ) ;
#16361 = ORIENTED_EDGE ( 'NONE', *, *, #11281, .T. ) ;
#16362 = CARTESIAN_POINT ( 'NONE',  ( 10.98768472639999949, -0.3876847264043000174, -4.945212061661000469 ) ) ;
#16363 = CARTESIAN_POINT ( 'NONE',  ( 11.27110638630999873, 5.469603964121000139, 8.504707115835000053 ) ) ;
#16364 = CARTESIAN_POINT ( 'NONE',  ( 2.092640132542666898, 3.058252359239899132, 1.762666431298155034 ) ) ;
#16365 = B_SPLINE_CURVE_WITH_KNOTS ( 'NONE', 3,
 ( #63345, #57762, #4972, #9873, #47633, #41690, #31217, #51833, #25266, #19331 ),
 .UNSPECIFIED., .F., .F.,
 ( 4, 2, 2, 2, 4 ),
 ( 0.1254223444949154886, 0.3127174981214190796, 0.5000126517479226429, 0.6873078053744264837, 0.8746029590009303245 ),
 .UNSPECIFIED. ) ;
#16366 = CARTESIAN_POINT ( 'NONE',  ( 11.69434208742519843, -4.478858766422799675, 6.747282993577999655 ) ) ;
#16367 = CARTESIAN_POINT ( 'NONE',  ( 10.83253786428999987, -2.899999999999999911, 6.571291218949999902 ) ) ;
#16368 = CARTESIAN_POINT ( 'NONE',  ( 11.26902897915239876, 4.221721321201099997, -8.337339982364900592 ) ) ;
#16369 = VECTOR ( 'NONE', #68006, 1000.000000000000114 ) ;
#16370 = CARTESIAN_POINT ( 'NONE',  ( 12.39271969839518661, -0.4698014501121478559, 12.68830453558791405 ) ) ;
#16371 = AXIS2_PLACEMENT_3D ( 'NONE', #40014, #8187, #61328 ) ;
#16372 = CARTESIAN_POINT ( 'NONE',  ( 23.58566160172500048, -10.19392717108999946, -9.581222027289999943 ) ) ;
#16373 = CARTESIAN_POINT ( 'NONE',  ( 10.50285691784999997, 5.158890929072000198, 8.369954994793999958 ) ) ;
#16374 = CARTESIAN_POINT ( 'NONE',  ( 11.84835150974899953, -3.192438788486000156, 11.44998398973999976 ) ) ;
#16375 = AXIS2_PLACEMENT_3D ( 'NONE', #2561, #45225, #66187 ) ;
#16376 = VERTEX_POINT ( 'NONE', #59566 ) ;
#16377 = DIRECTION ( 'NONE',  ( 0.7071067811865475727, -0.7071067811865475727, 0.000000000000000000 ) ) ;
#16378 = CARTESIAN_POINT ( 'NONE',  ( 6.862162629864999808, -1.172778741670000180, 0.4342585038969999922 ) ) ;
#16379 = CARTESIAN_POINT ( 'NONE',  ( 18.15991033943441835, 2.341318227119850715, 13.70580147614463051 ) ) ;
#16380 = CARTESIAN_POINT ( 'NONE',  ( 11.09999999999999964, 5.299316147296000423, -5.124965750789000296 ) ) ;
#16381 = CARTESIAN_POINT ( 'NONE',  ( 10.59610807141099897, -3.947296672195129918, -8.639522915742999132 ) ) ;
#16382 = ORIENTED_EDGE ( 'NONE', *, *, #25878, .T. ) ;
#16383 = DIRECTION ( 'NONE',  ( 0.000000000000000000, -1.000000000000000000, 0.000000000000000000 ) ) ;
#16384 = CARTESIAN_POINT ( 'NONE',  ( 7.448642219589999947, 4.628941086829000184, 5.991667691044999522 ) ) ;
#16386 = CARTESIAN_POINT ( 'NONE',  ( 10.93210843320491499, -5.137688304401064165, -8.098394516494938244 ) ) ;
#16385 = CARTESIAN_POINT ( 'NONE',  ( 8.233179719589999834, 5.203550244299999683, -8.391678825488000371 ) ) ;
#16387 = CARTESIAN_POINT ( 'NONE',  ( 10.59999999999999964, 3.399999999999999911, 4.756097560976000338 ) ) ;
#16388 = EDGE_CURVE ( 'NONE', #1808, #25355, #16572, .T. ) ;
#16389 = ORIENTED_EDGE ( 'NONE', *, *, #15055, .F. ) ;
#16390 = ADVANCED_FACE ( 'NONE', ( #6767 ), #20094, .F. ) ;
#16391 = B_SPLINE_CURVE_WITH_KNOTS ( 'NONE', 3,
 ( #32122, #48537, #49913, #49565, #13558, #45022, #66327, #23344, #40126, #44342, #2365, #6911, #1676, #28957, #23686, #34541, #3045, #24378, #13215, #55854, #65638, #7263, #29294, #61438, #45366 ),
 .UNSPECIFIED., .F., .F.,
 ( 4, 2, 2, 1, 1, 1, 2, 2, 2, 2, 2, 2, 2, 4 ),
 ( 0.1993834124056478585, 0.2494219491302857028, 0.2525493576755761804, 0.2556767662208666025, 0.2619315833114475578, 0.2744412174926094683, 0.2994604858549331228, 0.3995375593042285178, 0.4996146327535239129, 0.5496531694781714439, 0.5996917062028190859, 0.7998458531014098760, 0.8999229265507049380, 1.000000000000000000 ),
 .UNSPECIFIED. ) ;
#16392 = CARTESIAN_POINT ( 'NONE',  ( 9.351497027444999333, 4.821940693094999730, 8.950154065657999425 ) ) ;
#16393 = CARTESIAN_POINT ( 'NONE',  ( 17.67509761310387617, -1.797476384633009072, -13.88413128968476506 ) ) ;
#16394 = CARTESIAN_POINT ( 'NONE',  ( 11.16641369783139837, 3.949373449607799902, 6.497808498716000081 ) ) ;
#16395 = CARTESIAN_POINT ( 'NONE',  ( 10.76010362286999822, -4.535387425205000156, 6.001717576299999024 ) ) ;
#16396 = CARTESIAN_POINT ( 'NONE',  ( 7.101308059622001068, -3.554853390786000045, 8.889491623367000273 ) ) ;
#16397 = ORIENTED_EDGE ( 'NONE', *, *, #35075, .T. ) ;
#16398 = CARTESIAN_POINT ( 'NONE',  ( 8.032364158772001161, 3.524748802314000340, 5.573833469815000718 ) ) ;
#16400 = CARTESIAN_POINT ( 'NONE',  ( 10.20608185320999972, -2.622355301673999772, -6.528538675937999969 ) ) ;
#16399 = CARTESIAN_POINT ( 'NONE',  ( 10.87068169682078178, 4.873909797778569697, -7.480731692978241476 ) ) ;
#16401 = CARTESIAN_POINT ( 'NONE',  ( 7.754742686019933551, -5.333685489479075947, 8.616430321029321604 ) ) ;
#16402 = CARTESIAN_POINT ( 'NONE',  ( 9.657547180956999711, -5.333447643521000536, 6.049925825719999928 ) ) ;
#16403 = CARTESIAN_POINT ( 'NONE',  ( 1.643110514234999986, -1.247131703260000002, -3.010971457459999723 ) ) ;
#16404 = ORIENTED_EDGE ( 'NONE', *, *, #14830, .T. ) ;
#16405 = CARTESIAN_POINT ( 'NONE',  ( 9.602263540182329749, 5.092232985442822546, -8.129523725463620565 ) ) ;
#16406 = CARTESIAN_POINT ( 'NONE',  ( 11.07564694612699974, -4.931992688388300294, 7.128058497017000228 ) ) ;
#16407 = CARTESIAN_POINT ( 'NONE',  ( 11.40425819896749893, 2.744109752373000255, 7.263238376356399684 ) ) ;
#16408 = EDGE_LOOP ( 'NONE', ( #54488, #38517, #18067, #45185 ) ) ;
#16409 = CARTESIAN_POINT ( 'NONE',  ( 9.608904719592000987, 4.946705552514000459, -6.253848946732999181 ) ) ;
#16410 = CARTESIAN_POINT ( 'NONE',  ( 12.22684347114279824, 2.045928570575534788, -12.43279008976418787 ) ) ;
#16411 = CARTESIAN_POINT ( 'NONE',  ( 11.02799293566599914, -3.193321847920899792, 6.510429574318199464 ) ) ;
#16412 = EDGE_CURVE ( 'NONE', #23153, #45049, #25264, .T. ) ;
#16413 = ORIENTED_EDGE ( 'NONE', *, *, #31798, .T. ) ;
#16414 = CARTESIAN_POINT ( 'NONE',  ( 3.999971066382000284, 2.149963194831999935, 0.000000000000000000 ) ) ;
#16415 = VECTOR ( 'NONE', #28779, 1000.000000000000000 ) ;
#16417 = EDGE_CURVE ( 'NONE', #35697, #13467, #42384, .T. ) ;
#16416 = FACE_OUTER_BOUND ( 'NONE', #66201, .T. ) ;
#16418 = ORIENTED_EDGE ( 'NONE', *, *, #48179, .F. ) ;
#16419 = CARTESIAN_POINT ( 'NONE',  ( 8.304129440378000382, -3.650411072918999800, 6.083135626079000602 ) ) ;
#16420 = CARTESIAN_POINT ( 'NONE',  ( 5.700859839683917407, 0.3926218265389221362, -1.460959015002473160 ) ) ;
#16421 = ORIENTED_EDGE ( 'NONE', *, *, #46204, .F. ) ;
#16422 = CARTESIAN_POINT ( 'NONE',  ( 12.32444827497858597, -3.019497106116459939, -12.23286052727262607 ) ) ;
#16423 = CARTESIAN_POINT ( 'NONE',  ( 11.09256785386839894, 3.167490253789400523, 6.939751505745099358 ) ) ;
#16424 = CARTESIAN_POINT ( 'NONE',  ( 9.696080515601000371, 2.554416243104999928, 7.600685069647000525 ) ) ;
#16425 = CARTESIAN_POINT ( 'NONE',  ( 10.98435102962999999, 2.894555727676000334, -4.879788070431000158 ) ) ;
#16426 = CARTESIAN_POINT ( 'NONE',  ( 25.59997277611800115, 2.578802611042650509E-13, -11.19994871957399241 ) ) ;
#16427 = CARTESIAN_POINT ( 'NONE',  ( 10.72520823780999955, -5.521647200017000934, 6.612992938078999572 ) ) ;
#16428 = CARTESIAN_POINT ( 'NONE',  ( 17.87637886473325466, -0.6448943924266655747, -12.58348668657565739 ) ) ;
#16429 = CONICAL_SURFACE ( 'NONE', #13107, 12.69999976913000062, 0.7853981453603698926 ) ;
#16430 = CARTESIAN_POINT ( 'NONE',  ( 6.999999085428001422, -12.01420426511556094, 3.456409902911533383 ) ) ;
#16431 = CARTESIAN_POINT ( 'NONE',  ( 11.33872066707849768, -3.141388196630700236, -6.980638253271099103 ) ) ;
#16432 = CARTESIAN_POINT ( 'NONE',  ( 8.598670280411999656, 2.376526778640999815, 7.686980884243000745 ) ) ;
#16433 = EDGE_LOOP ( 'NONE', ( #16758, #52289, #58773, #48819 ) ) ;
#16434 = AXIS2_PLACEMENT_3D ( 'NONE', #10622, #59207, #21122 ) ;
#16435 = DIRECTION ( 'NONE',  ( 1.000000000000000000, 0.000000000000000000, 0.000000000000000000 ) ) ;
#16436 = CARTESIAN_POINT ( 'NONE',  ( 24.54174074855145804, -8.849271461538792849, -9.279828214374076012 ) ) ;
#16437 = CARTESIAN_POINT ( 'NONE',  ( 11.82330164685100193, 12.43416923969000010, 1.799281280950999928 ) ) ;
#16438 = ADVANCED_FACE ( 'NONE', ( #58115 ), #5521, .T. ) ;
#16439 = CARTESIAN_POINT ( 'NONE',  ( 18.21786174063354125, 2.187645605293237594, 12.40865382983254328 ) ) ;
#16440 = CARTESIAN_POINT ( 'NONE',  ( 11.07074946250000025, 6.638246904777000523, 5.577396945824999897 ) ) ;
#16441 = CARTESIAN_POINT ( 'NONE',  ( 11.07111654620999985, 7.823241544734999664, 6.598400448272999874 ) ) ;
#16442 = AXIS2_PLACEMENT_3D ( 'NONE', #41374, #66901, #14805 ) ;
#16443 = CARTESIAN_POINT ( 'NONE',  ( 12.33074081237575648, -0.4072355409555394323, -12.69121720794965391 ) ) ;
#16444 = DIRECTION ( 'NONE',  ( 0.000000000000000000, 0.8648648648648717963, -0.5020047465136829867 ) ) ;
#16445 = ORIENTED_EDGE ( 'NONE', *, *, #57682, .F. ) ;
#16446 = CARTESIAN_POINT ( 'NONE',  ( 12.44969725703165864, -3.107561633766898535, 12.21077779329595181 ) ) ;
#16447 = CARTESIAN_POINT ( 'NONE',  ( 9.505051052051998184, -2.879444846832000415, -7.719295683256799379 ) ) ;
#16448 = CARTESIAN_POINT ( 'NONE',  ( 9.449618669012016525, -4.457228036536642790, 8.907268959278543008 ) ) ;
#16449 = CARTESIAN_POINT ( 'NONE',  ( 8.293430908490591946, 2.934198963169226015, -6.452279353973301212 ) ) ;
#16450 = CARTESIAN_POINT ( 'NONE',  ( 11.86333594839950045, -3.340240242524600056, 8.256087240512899328 ) ) ;
#16451 = CARTESIAN_POINT ( 'NONE',  ( 11.69559063708295987, 5.086518862378000883, -7.805482129094999166 ) ) ;
#16452 = CARTESIAN_POINT ( 'NONE',  ( 12.57206729000417589, 0.6812425322175417186, 12.58157083403807164 ) ) ;
#16453 = DIRECTION ( 'NONE',  ( 0.7071068208980029191, 0.000000000000000000, -0.7071067414750898950 ) ) ;
#16454 = CARTESIAN_POINT ( 'NONE',  ( 24.96658222323440057, -10.83443034510523617, -3.855530974724861615 ) ) ;
#16455 = CARTESIAN_POINT ( 'NONE',  ( 12.41053097114615333, 2.984774150185583341, 12.32529705072536963 ) ) ;
#16456 = DIRECTION ( 'NONE',  ( 1.000000000000000000, 0.000000000000000000, 0.000000000000000000 ) ) ;
#16457 = CARTESIAN_POINT ( 'NONE',  ( 10.69456919669529960, 5.093991349577000172, -7.823222900359999343 ) ) ;
#16458 = CARTESIAN_POINT ( 'NONE',  ( 12.57461732485479899, 12.11259905827362182, -3.187575261700099638 ) ) ;
#16459 = CARTESIAN_POINT ( 'NONE',  ( 10.71315778041000044, 2.619207518211999819, -8.142085279690999045 ) ) ;
#16460 = CARTESIAN_POINT ( 'NONE',  ( 8.516151519676999015, 4.027664626136379766, -8.778912113473998247 ) ) ;
#16462 = CARTESIAN_POINT ( 'NONE',  ( 18.08719379937462435, -0.3285641700896766437, 12.69429818673183874 ) ) ;
#16461 = CARTESIAN_POINT ( 'NONE',  ( 17.60000000000000142, -10.78295181803999903, 4.410266442048000002 ) ) ;
#16463 = CARTESIAN_POINT ( 'NONE',  ( 11.35393383743268103, 12.19578912482747590, 1.764073084349790266 ) ) ;
#16464 = VERTEX_POINT ( 'NONE', #52177 ) ;
#16465 = B_SPLINE_CURVE_WITH_KNOTS ( 'NONE', 3,
 ( #48041, #21463, #63765, #31976, #4688, #68316 ),
 .UNSPECIFIED., .F., .F.,
 ( 4, 2, 4 ),
 ( 0.000000000000000000, 0.5000000000000000000, 1.000000000000000000 ),
 .UNSPECIFIED. ) ;
#16466 = CARTESIAN_POINT ( 'NONE',  ( 12.39297475233172641, 0.4699412921624549488, 12.68829632721468670 ) ) ;
#16467 = DIRECTION ( 'NONE',  ( -1.000000000000000000, 0.000000000000000000, 0.000000000000000000 ) ) ;
#16468 = PRESENTATION_LAYER_ASSIGNMENT (  '', '', ( #33255 ) ) ;
#16469 = CARTESIAN_POINT ( 'NONE',  ( 18.20120694895331681, 0.3761765225308036920, -12.59508068833545025 ) ) ;
#16470 = CARTESIAN_POINT ( 'NONE',  ( 8.817138961223998095, 4.718363881473300658, 7.014550357332099750 ) ) ;
#16471 = EDGE_CURVE ( 'NONE', #65069, #57137, #10216, .T. ) ;
#16472 = EDGE_CURVE ( 'NONE', #10742, #19003, #41004, .T. ) ;
#16474 = CARTESIAN_POINT ( 'NONE',  ( 12.14279580514170220, -2.220721880347446220, 13.82275356517832243 ) ) ;
#16473 = CONICAL_SURFACE ( 'NONE', #26576, 0.4311160744474001327, 0.7853981633972997312 ) ;
#16475 = DIRECTION ( 'NONE',  ( 0.000000000000000000, -0.5592907522138691467, 0.8289715643422543856 ) ) ;
#16476 = CARTESIAN_POINT ( 'NONE',  ( 10.81746213571000048, 5.100000000000000533, 6.571291218949999902 ) ) ;
#16477 = VERTEX_POINT ( 'NONE', #26303 ) ;
#16478 = EDGE_CURVE ( 'NONE', #39483, #20439, #19683, .T. ) ;
#16479 = ADVANCED_FACE ( 'NONE', ( #25953 ), #58452, .F. ) ;
#16480 = DIRECTION ( 'NONE',  ( 0.000000000000000000, 1.000000000000000000, 0.000000000000000000 ) ) ;
#16481 = CARTESIAN_POINT ( 'NONE',  ( 9.674960421382822418, -2.650268802167429438, 7.499999178247414910 ) ) ;
#16482 = VECTOR ( 'NONE', #16914, 1000.000000000000000 ) ;
#16483 = CARTESIAN_POINT ( 'NONE',  ( 18.20279897579440131, -3.027817980922570484, 11.45825916412429812 ) ) ;
#16484 = CARTESIAN_POINT ( 'NONE',  ( 6.899999691988000450, -11.00717859340000082, -1.432487142323000118 ) ) ;
#16485 = CARTESIAN_POINT ( 'NONE',  ( 18.12481736082884254, 2.757674955237351622, -12.38783183949681899 ) ) ;
#16486 = CARTESIAN_POINT ( 'NONE',  ( 9.114639751325487538, -2.815014287255568792, -7.959719964829115035 ) ) ;
#16487 = CARTESIAN_POINT ( 'NONE',  ( 10.85056919669530018, 4.830699382454300306, 7.254567470917099747 ) ) ;
#16488 = CIRCLE ( 'NONE', #38813, 0.4999999999999996114 ) ;
#16489 = CARTESIAN_POINT ( 'NONE',  ( 15.79991751193278482, 9.060349897821472709, 8.357793075677504291 ) ) ;
#16490 = CARTESIAN_POINT ( 'NONE',  ( 10.35753185321000025, -5.367809014988999650, -6.514738374536999999 ) ) ;
#16491 = CARTESIAN_POINT ( 'NONE',  ( 12.07956470885934586, 2.330212498102625762, 13.80606232674509215 ) ) ;
#16492 = B_SPLINE_SURFACE_WITH_KNOTS ( 'NONE', 3, 3, ( 
 ( #39769, #11455, #1667, #39074 ),
 ( #54803, #12502, #32795, #59701 ),
 ( #22635, #38376, #43979, #27547 ),
 ( #48875, #28238, #65286, #34181 ),
 ( #17400, #22294, #43634, #7599 ),
 ( #64928, #49554, #22984, #65630 ),
 ( #60397, #65971, #18099, #56527 ),
 ( #24025, #3377, #35215, #8971 ),
 ( #61431, #30647, #3038, #13548 ),
 ( #8632, #24714, #41141, #30310 ),
 ( #51957, #46730, #62451, #13207 ),
 ( #67345, #56873, #8293, #35556 ) ),
 .UNSPECIFIED., .F., .F., .F.,
 ( 4, 1, 1, 1, 1, 1, 1, 1, 1, 4 ),
 ( 4, 4 ),
 ( 0.01095835123444999920, 0.05000000000000000278, 0.1000000000000000056, 0.1499999999999999944, 0.2000000000000000111, 0.2500000000000000000, 0.2999999999999999889, 0.3499999999999999778, 0.4000000000000000222, 0.4461837860292000024 ),
 ( -0.2706701102521000268, 1.270791538669000076 ),
 .UNSPECIFIED. ) ;
#16493 = CARTESIAN_POINT ( 'NONE',  ( 25.49995441705259935, 2.042062856630685097, 11.11383374566986326 ) ) ;
#16494 = CARTESIAN_POINT ( 'NONE',  ( 24.11241132672047272, 9.193877876179779918, -9.158456253082972509 ) ) ;
#16495 = CARTESIAN_POINT ( 'NONE',  ( 27.09999999999999787, 4.013733789776000248E-13, 10.75000000000000000 ) ) ;
#16496 = ORIENTED_EDGE ( 'NONE', *, *, #65528, .F. ) ;
#16497 = CARTESIAN_POINT ( 'NONE',  ( 11.09999999999999964, 5.449702574547000467, 5.124965750789000296 ) ) ;
#16498 = CARTESIAN_POINT ( 'NONE',  ( 10.88287885159599888, -3.139900861731399928, 7.602606670248799325 ) ) ;
#16499 = ORIENTED_EDGE ( 'NONE', *, *, #47837, .F. ) ;
#16500 = CARTESIAN_POINT ( 'NONE',  ( 17.59665311020859235, -3.123961325934789812, 13.52113166927136589 ) ) ;
#16501 = CARTESIAN_POINT ( 'NONE',  ( 11.42887348028849992, -5.124210964533999935, -8.107837221875000111 ) ) ;
#16502 = VERTEX_POINT ( 'NONE', #4277 ) ;
#16503 = CARTESIAN_POINT ( 'NONE',  ( 10.77368717260499942, 3.460071470104900015, 6.618743573831199711 ) ) ;
#16504 = CARTESIAN_POINT ( 'NONE',  ( 6.649371033313499879, 0.7294112533789433028, 0.8667001409038291859 ) ) ;
#16505 = CARTESIAN_POINT ( 'NONE',  ( 10.34920446231350155, -2.899999999999999911, -6.662590550579927218 ) ) ;
#16506 = CARTESIAN_POINT ( 'NONE',  ( 18.53960231418900051, -2.682082126742999950, 11.29772413421000188 ) ) ;
#16507 = DIRECTION ( 'NONE',  ( 1.000000000000000000, 0.000000000000000000, 0.000000000000000000 ) ) ;
#16508 = CARTESIAN_POINT ( 'NONE',  ( 12.23478023516057611, 0.2564316838161031509, -13.89683092737869075 ) ) ;
#16509 = CARTESIAN_POINT ( 'NONE',  ( 6.834986978535497748, -1.140791068544842579, -0.07160982795898844511 ) ) ;
#16510 = CARTESIAN_POINT ( 'NONE',  ( 10.56591477248000110, -5.293237054095000005, -7.067083954277999958 ) ) ;
#16511 = CARTESIAN_POINT ( 'NONE',  ( 13.55481756226799916, 11.54935041389000006, 2.400813070608000199 ) ) ;
#16512 = ORIENTED_EDGE ( 'NONE', *, *, #25108, .F. ) ;
#16513 = CONICAL_SURFACE ( 'NONE', #19863, 1.949999999913999860, 0.7853981633972997312 ) ;
#16514 = DIRECTION ( 'NONE',  ( -1.000000000000000000, 0.000000000000000000, 0.000000000000000000 ) ) ;
#16515 = ORIENTED_EDGE ( 'NONE', *, *, #4010, .F. ) ;
#16516 = CARTESIAN_POINT ( 'NONE',  ( 10.24846228258000025, 4.234133568259999869, -5.660851473941000300 ) ) ;
#16517 = EDGE_LOOP ( 'NONE', ( #66378, #65360, #42130 ) ) ;
#16518 = CARTESIAN_POINT ( 'NONE',  ( 18.28072526159327893, -2.330763871328881187, -13.80597059071421562 ) ) ;
#16519 = CARTESIAN_POINT ( 'NONE',  ( 18.06437450929129085, -2.862796250983955737, -12.35961424106608497 ) ) ;
#16520 = EDGE_CURVE ( 'NONE', #1441, #61281, #35271, .T. ) ;
#16521 = VECTOR ( 'NONE', #43408, 1000.000000000000000 ) ;
#16522 = CARTESIAN_POINT ( 'NONE',  ( 10.64914416493166449, 3.188141180065802160, 7.176001761109866095 ) ) ;
#16523 = CARTESIAN_POINT ( 'NONE',  ( 13.49980696793000057, 9.514462421839999351, 7.834836582454001608 ) ) ;
#16524 = CARTESIAN_POINT ( 'NONE',  ( 9.903944471677000649, -5.205019707614999547, 6.747219600580999455 ) ) ;
#16525 = ADVANCED_FACE ( 'NONE', ( #26653 ), #16218, .F. ) ;
#16526 = AXIS2_PLACEMENT_3D ( 'NONE', #6223, #38742, #27562 ) ;
#16527 = CARTESIAN_POINT ( 'NONE',  ( 5.500000000000000000, -1.199999999999999956, -9.776630298829998011 ) ) ;
#16528 = CARTESIAN_POINT ( 'NONE',  ( 12.18028570900101215, 0.01996689158402554023, 13.89998575767904043 ) ) ;
#16529 = ORIENTED_EDGE ( 'NONE', *, *, #956, .T. ) ;
#16530 = CARTESIAN_POINT ( 'NONE',  ( 12.53679426224900162, 11.40784081139999984, -4.532785132108998916 ) ) ;
#16531 = CARTESIAN_POINT ( 'NONE',  ( 18.39660364871399878, 11.70009917314000170, -4.315816162729000816 ) ) ;
#16532 = DIRECTION ( 'NONE',  ( 0.000000000000000000, 1.000000000000000000, 0.000000000000000000 ) ) ;
#16533 = VECTOR ( 'NONE', #58196, 1000.000000000000114 ) ;
#16534 = CARTESIAN_POINT ( 'NONE',  ( 4.984592376538000025, 1.123536932646000075, 0.9667689356016999636 ) ) ;
#16535 = CARTESIAN_POINT ( 'NONE',  ( 25.60000000000000142, 2.023980670379999847, 11.01542190082000161 ) ) ;
#16536 = CARTESIAN_POINT ( 'NONE',  ( 17.98972740837745476, 12.09687365817480575, -3.246763311060390844 ) ) ;
#16537 = CARTESIAN_POINT ( 'NONE',  ( 10.16989351219999982, -2.594225604561000154, -6.291264536816999708 ) ) ;
#16538 = VERTEX_POINT ( 'NONE', #28031 ) ;
#16539 = AXIS2_PLACEMENT_3D ( 'NONE', #48226, #11498, #58034 ) ;
#16540 = CARTESIAN_POINT ( 'NONE',  ( 25.29995823066400362, -11.13046982544999963, 3.427501264366999756 ) ) ;
#16541 = CARTESIAN_POINT ( 'NONE',  ( 4.464594377645832779, -0.6414890624138858133, 1.377603488137450594 ) ) ;
#16542 = CARTESIAN_POINT ( 'NONE',  ( 18.30000000000000071, 14.70300865175000027, -5.744762642578000289 ) ) ;
#16543 = CARTESIAN_POINT ( 'NONE',  ( 8.587675602096970451, -2.935917077764118144, 6.277144180784712368 ) ) ;
#16544 = DIRECTION ( 'NONE',  ( -1.000000000000000000, 0.000000000000000000, 0.000000000000000000 ) ) ;
#16545 = CARTESIAN_POINT ( 'NONE',  ( 11.42834208742529967, 3.293478249981899975, -8.610579932818998472 ) ) ;
#16546 = CARTESIAN_POINT ( 'NONE',  ( 9.913279731609000223, 4.090130512164860122, -6.499640669006000238 ) ) ;
#16548 = CARTESIAN_POINT ( 'NONE',  ( 8.341176297635993109, 4.893934000596881440, -6.169995681351899464 ) ) ;
#16547 = CARTESIAN_POINT ( 'NONE',  ( 10.02635508232799921, -4.388021368982800041, 8.275336934318801241 ) ) ;
#16549 = CARTESIAN_POINT ( 'NONE',  ( 8.164796825344000197, -3.457406484157000026, 6.165651553258999940 ) ) ;
#16550 = ORIENTED_EDGE ( 'NONE', *, *, #53541, .T. ) ;
#16551 = B_SPLINE_CURVE_WITH_KNOTS ( 'NONE', 3,
 ( #56547, #30669, #3737, #9672, #13907, #25071 ),
 .UNSPECIFIED., .F., .F.,
 ( 4, 2, 4 ),
 ( 0.000000000000000000, 0.1967045975185045814, 0.3934091950370091628 ),
 .UNSPECIFIED. ) ;
#16552 = LINE ( 'NONE', #9666, #64576 ) ;
#16553 = CARTESIAN_POINT ( 'NONE',  ( 7.491953176340000908, -3.528027000165000704, 6.607934030033999484 ) ) ;
#16554 = CARTESIAN_POINT ( 'NONE',  ( 10.01163399569799850, 5.134843509922999871, 7.374045024026299799 ) ) ;
#16555 = CARTESIAN_POINT ( 'NONE',  ( 11.66883611674750654, -3.345348949920207815, 11.86065797283158929 ) ) ;
#16556 = ADVANCED_FACE ( 'NONE', ( #65056 ), #22422, .F. ) ;
#16557 = CARTESIAN_POINT ( 'NONE',  ( 9.691080333872001518, -5.335644368206000188, 8.701217921043999937 ) ) ;
#16558 = CARTESIAN_POINT ( 'NONE',  ( 18.10321044366099486, 2.800384071015809884, -12.37651499847982528 ) ) ;
#16559 = CARTESIAN_POINT ( 'NONE',  ( 16.07059379716000080, -3.381060347337999872, -11.29912544500000138 ) ) ;
#16560 = EDGE_CURVE ( 'NONE', #22542, #51145, #44119, .T. ) ;
#16561 = EDGE_CURVE ( 'NONE', #48552, #6251, #1109, .T. ) ;
#16562 = CARTESIAN_POINT ( 'NONE',  ( 9.280051052051998539, -3.014287398677499841, -7.692906630067099627 ) ) ;
#16563 = CARTESIAN_POINT ( 'NONE',  ( 6.131846742205000034, 0.002616650692276999927, 1.322296913527999829 ) ) ;
#16564 = CARTESIAN_POINT ( 'NONE',  ( 11.22299000889467635, -4.227343628179307977, 6.655959434011009535 ) ) ;
#16565 = CONICAL_SURFACE ( 'NONE', #40050, 12.47499939740000130, 0.7853981102588313279 ) ;
#16566 = DIRECTION ( 'NONE',  ( 1.000000000000000000, 0.000000000000000000, 0.000000000000000000 ) ) ;
#16567 = VERTEX_POINT ( 'NONE', #17536 ) ;
#16568 = CARTESIAN_POINT ( 'NONE',  ( 11.09999999999999964, -2.700000000000000178, 5.160242730440000258 ) ) ;
#16569 = CARTESIAN_POINT ( 'NONE',  ( 10.97364560330029981, 4.265439025801100570, -6.675475461903199736 ) ) ;
#16570 = CARTESIAN_POINT ( 'NONE',  ( 5.407309473666999544, -12.95251760905999916, 1.915207572622000143 ) ) ;
#16572 = LINE ( 'NONE', #33356, #41259 ) ;
#16571 = AXIS2_PLACEMENT_3D ( 'NONE', #21711, #48289, #68921 ) ;
#16573 = DIRECTION ( 'NONE',  ( 0.8843050080896810439, -0.1786786090465959931, -0.4313682966290904863 ) ) ;
#16574 = ORIENTED_EDGE ( 'NONE', *, *, #37918, .F. ) ;
#16575 = CARTESIAN_POINT ( 'NONE',  ( 11.49999144015000319, 3.886253129992999877, -11.90689313971000018 ) ) ;
#16576 = CARTESIAN_POINT ( 'NONE',  ( 10.39969598649000027, -3.111999510220800236, -8.028730309000598808 ) ) ;
#16577 = CARTESIAN_POINT ( 'NONE',  ( 18.13610002192212534, 0.2304169715249079764, 12.69719098617350639 ) ) ;
#16578 = EDGE_CURVE ( 'NONE', #12259, #69104, #32331, .T. ) ;
#16579 = CARTESIAN_POINT ( 'NONE',  ( 10.59393020684899867, -2.750000000000000000, 7.500000000000000000 ) ) ;
#16580 = CARTESIAN_POINT ( 'NONE',  ( 7.650096249917202940, 4.657077951104835023, -8.696453622792276406 ) ) ;
#16581 = VECTOR ( 'NONE', #430, 1000.000000000000114 ) ;
#16582 = CARTESIAN_POINT ( 'NONE',  ( 10.61257802013489737, 3.108115747127599970, -7.479237407015119743 ) ) ;
#16583 = EDGE_LOOP ( 'NONE', ( #41695, #10802, #60446, #31797, #53479, #6258 ) ) ;
#16584 = CARTESIAN_POINT ( 'NONE',  ( 10.05691733561000056, -2.453480799114999833, 6.657106310117000270 ) ) ;
#16585 = CARTESIAN_POINT ( 'NONE',  ( 18.16386294024314907, 2.642762625146028999, -13.64216358405141705 ) ) ;
#16586 = ORIENTED_EDGE ( 'NONE', *, *, #20293, .F. ) ;
#16587 = LINE ( 'NONE', #5745, #8319 ) ;
#16588 = CARTESIAN_POINT ( 'NONE',  ( 24.97040879175293426, 8.550777727342323331, -8.358969513697752873 ) ) ;
#16589 = CARTESIAN_POINT ( 'NONE',  ( 15.45728973496400194, 8.836548693809998412, 7.950469186927999310 ) ) ;
#16590 = AXIS2_PLACEMENT_3D ( 'NONE', #3787, #57272, #51355 ) ;
#16591 = VERTEX_POINT ( 'NONE', #6334 ) ;
#16592 = CARTESIAN_POINT ( 'NONE',  ( 23.58888338209971991, -2.922255725552524996, -13.61648187270552945 ) ) ;
#16593 = CARTESIAN_POINT ( 'NONE',  ( 18.12515139794686192, 0.2563289266177934400, -12.69652241465648679 ) ) ;
#16594 = CARTESIAN_POINT ( 'NONE',  ( 10.34393020684899867, -5.250000000000000000, -7.500000000000000000 ) ) ;
#16595 = CARTESIAN_POINT ( 'NONE',  ( 9.457108735800074939, 5.237413963666066152, 8.039587586354246085 ) ) ;
#16596 = EDGE_LOOP ( 'NONE', ( #18675, #38433, #40416, #47022 ) ) ;
#16597 = CARTESIAN_POINT ( 'NONE',  ( 10.80815535238000002, -2.937528991339000140, 8.948455587554001056 ) ) ;
#16598 = CARTESIAN_POINT ( 'NONE',  ( 25.09299849713500308, 11.65481204179000052, -3.020019037700000020 ) ) ;
#16599 = DIRECTION ( 'NONE',  ( 4.399946526753046019E-15, -1.000000000000000000, -1.785362917591035329E-14 ) ) ;
#16600 = ORIENTED_EDGE ( 'NONE', *, *, #59093, .F. ) ;
#16601 = DIRECTION ( 'NONE',  ( -1.000000000000000000, 0.000000000000000000, 0.000000000000000000 ) ) ;
#16602 = CARTESIAN_POINT ( 'NONE',  ( 8.474485200571999499, 5.100000000000000533, 6.560614371780999043 ) ) ;
#16603 = VERTEX_POINT ( 'NONE', #27332 ) ;
#16604 = CARTESIAN_POINT ( 'NONE',  ( 9.178734463322998138, 4.104624583183299258, 6.501052555474699624 ) ) ;
#16605 = DIRECTION ( 'NONE',  ( 0.000000000000000000, 0.000000000000000000, -1.000000000000000000 ) ) ;
#16606 = CARTESIAN_POINT ( 'NONE',  ( 4.853281127746000401, 0.06624698400605999460, 1.414933278434000075 ) ) ;
#16607 = CARTESIAN_POINT ( 'NONE',  ( 11.59999999999999964, 4.016704963253245886, -6.452290402036156891 ) ) ;
#16608 = CARTESIAN_POINT ( 'NONE',  ( 1.284778341492999868E-07, 0.000000000000000000, -2.574999650349000024 ) ) ;
#16609 = CARTESIAN_POINT ( 'NONE',  ( 7.225316516319210791, 3.408784923954944812, -8.751707459018776447 ) ) ;
#16610 = CARTESIAN_POINT ( 'NONE',  ( 24.05220180837281063, 12.62753229755031015, 3.430343039253267445 ) ) ;
#16611 = EDGE_CURVE ( 'NONE', #5014, #60256, #5159, .T. ) ;
#16612 = CARTESIAN_POINT ( 'NONE',  ( 8.719914745407999490, 3.934662526658240012, -8.403568966271999230 ) ) ;
#16613 = ORIENTED_EDGE ( 'NONE', *, *, #63198, .F. ) ;
#16614 = CARTESIAN_POINT ( 'NONE',  ( 10.05691520198999989, 2.453477278391000382, 6.657104391228999773 ) ) ;
#16615 = CARTESIAN_POINT ( 'NONE',  ( 10.22907665877000127, 4.838498214728000235, -5.852435699035000383 ) ) ;
#16616 = DIRECTION ( 'NONE',  ( 1.000000000000000000, 0.000000000000000000, 0.000000000000000000 ) ) ;
#16617 = CARTESIAN_POINT ( 'NONE',  ( 12.66212950609378574, 3.108785237067038132, -13.52531707329825572 ) ) ;
#16618 = CARTESIAN_POINT ( 'NONE',  ( 3.690346968721999854, -1.826556930874999818, 3.227001764767000402 ) ) ;
#16619 = CARTESIAN_POINT ( 'NONE',  ( 9.781666627457001439, -5.464740618746000145, 8.817321229216000589 ) ) ;
#16620 = CARTESIAN_POINT ( 'NONE',  ( 11.16486084871730000, 5.207010770456999893, -7.174999999999999822 ) ) ;
#16621 = CARTESIAN_POINT ( 'NONE',  ( 17.85613310415347144, 0.5477939754035893172, 13.88547043407462667 ) ) ;
#16622 = ORIENTED_EDGE ( 'NONE', *, *, #26124, .T. ) ;
#16623 = VERTEX_POINT ( 'NONE', #11935 ) ;
#16624 = AXIS2_PLACEMENT_3D ( 'NONE', #63233, #41582, #3820 ) ;
#16625 = CARTESIAN_POINT ( 'NONE',  ( 12.32624190542397002, 0.4017285589307815763, 13.89218662323935050 ) ) ;
#16626 = CARTESIAN_POINT ( 'NONE',  ( 12.50370260275542478, -0.5476489827201047600, -13.88547809940108024 ) ) ;
#16627 = CARTESIAN_POINT ( 'NONE',  ( 7.225322421146570306, -2.650264760010439868, 7.500018091723870128 ) ) ;
#16628 = CARTESIAN_POINT ( 'NONE',  ( 17.81146176621321331, -0.5702785222767412510, -13.88425216382592886 ) ) ;
#16629 = CARTESIAN_POINT ( 'NONE',  ( 7.603418146792000343, -5.687202994508999687, 6.847270485579000088 ) ) ;
#16631 = CARTESIAN_POINT ( 'NONE',  ( 18.01256889503158121, 11.20125638878172936, -3.203298770437340348 ) ) ;
#16630 = CARTESIAN_POINT ( 'NONE',  ( 10.13370934641699961, -2.844451673749999632, 8.048718920009699573 ) ) ;
#16632 = CARTESIAN_POINT ( 'NONE',  ( 10.64533863405319991, 4.703785194191100416, -8.397761948794601139 ) ) ;
#16633 = DIRECTION ( 'NONE',  ( 0.000000000000000000, -0.8648648648648717963, 0.5020047465136829867 ) ) ;
#16634 = DIRECTION ( 'NONE',  ( -1.000000000000000000, 0.000000000000000000, 0.000000000000000000 ) ) ;
#16635 = CARTESIAN_POINT ( 'NONE',  ( 18.18003632999695895, -0.02081145935391651852, 12.69999906470293283 ) ) ;
#16636 = B_SPLINE_SURFACE_WITH_KNOTS ( 'NONE', 3, 3, ( 
 ( #68182, #4551, #25200, #57018, #68872, #36733, #52107, #58052, #15054, #25890, #30795, #62932, #62594, #36033, #14035, #26241, #10155, #41970, #47221, #51429, #51768, #14381, #35701, #9117, #3866, #4900, #40938, #24861, #9805, #46189, #8782, #47569, #68524, #19962, #67499, #31154, #20991, #61920, #56683, #35361, #52456, #57694, #30126, #14717, #57348, #19617, #62260, #20646, #4211, #9453, #25549, #20299, #46874, #41626, #42997, #53148, #33205, #32515, #54171, #64305, #53492, #11178, #6270, #38089, #27964, #11865, #43355 ),
 ( #48241, #43697, #42327, #6626, #5928, #53830, #5584, #27611, #48593, #26928, #63965, #22359, #64656, #26587, #47909, #32179, #48939, #21328, #17108, #16760, #695, #27269, #37752, #11515, #59416, #32859, #49274, #54524, #6, #16423, #63629, #15746, #1047, #5249, #64991, #59765, #1384, #38442, #58385, #37073, #42656, #16078, #59078, #346, #10492, #21663, #22007, #31832, #10836, #37410, #58731, #29014, #29704, #8358, #12919, #34599, #56251, #39833, #55912, #50320, #38792, #12224, #28658, #39135, #40179, #66733, #18163 ),
 ( #51005, #61495, #23743, #13613, #34935, #7316, #49970, #24091, #22700, #44045, #55566, #60808, #33900, #8015, #2419, #55217, #44398, #2765, #45081, #6972, #28301, #12569, #29353, #1729, #18852, #66388, #18511, #7667, #39485, #61154, #13272, #50664, #45424, #65350, #33551, #34246, #17469, #60118, #54871, #2085, #49623, #23048, #65697, #17821, #60462, #23403, #44741, #66039, #19872, #46789, #52020, #3779, #61832, #25116, #3104, #56936, #19184, #35278, #46448, #4120, #14632, #14968, #35950, #24437, #67748, #57264, #19531 ),
 ( #45763, #40507, #9032, #51681, #41203, #20212, #41538, #62513, #13952, #56594, #9364, #62850, #30710, #25457, #8700, #68095, #67071, #30044, #51347, #3439, #24776, #46103, #30373, #67409, #62172, #40852, #14294, #35623, #24310, #13826, #35154, #61373, #12446, #8233, #28536, #44624, #39710, #7536, #56469, #50200, #44960, #19059, #34125, #2300, #18727, #2640, #3322, #51226, #55787, #29580, #29918, #13491, #50882, #23967, #33778, #55096, #23620, #12796, #8572, #40385, #61030, #45302, #18385, #49849, #34813, #66264, #24654 ) ),
 .UNSPECIFIED., .F., .F., .F.,
 ( 4, 4 ),
 ( 4, 1, 1, 1, 1, 1, 1, 1, 1, 1, 1, 1, 1, 1, 1, 1, 1, 1, 1, 1, 1, 1, 1, 1, 1, 1, 1, 1, 1, 1, 1, 1, 1, 1, 1, 1, 1, 1, 1, 1, 1, 1, 1, 1, 1, 1, 1, 1, 1, 1, 1, 1, 1, 1, 1, 1, 1, 1, 1, 1, 1, 1, 1, 1, 4 ),
 ( -0.02000000000000000042, 1.020000000000000018 ),
 ( 0.008747244164287000176, 0.02453926110774999961, 0.04033127805120999970, 0.05612329499467000327, 0.07191531193812999989, 0.08770732888158999652, 0.1034993458251000087, 0.1192913627684999978, 0.1350833797120000179, 0.1508753966553999792, 0.1666674135988999994, 0.1824594305423999918, 0.1982514474858000086, 0.2140434644293000011, 0.2298354813727000179, 0.2456274983162000103, 0.2614195152596999749, 0.2772115322030999640, 0.2930035491465999842, 0.3087955660900000288, 0.3245875830334999934, 0.3403795999769999581, 0.3561716169204000026, 0.3719636338639000228, 0.3877556508073999875, 0.4035476677507999765, 0.4193396846942999967, 0.4351317016376999858, 0.4509237185811999504, 0.4667157355247000261, 0.4825077524681000152, 0.4982997694115999798, 0.5140917863550000799, 0.5298838032985000446, 0.5456758202420000092, 0.5614678371854000538, 0.5772598541289000185, 0.5930518710723000630, 0.6088438880158000277, 0.6246359049592999924, 0.6404279219027000369, 0.6562199388462000016, 0.6720119557896999662, 0.6878039727331000108, 0.7035959896765999755, 0.7193880066200000201, 0.7351800235634999847, 0.7509720405069999494, 0.7667640574504001050, 0.7825560743939000696, 0.7983480913373000032, 0.8141401082808000789, 0.8299321252243000435, 0.8457241421676999771, 0.8615161591112000528, 0.8773081760545999863, 0.8931001929981000620, 0.9088922099416000266, 0.9246842268849999602, 0.9404762438285000359, 0.9562682607720000005, 0.9720602777153999341, 0.9878522946589000098, 1.003644311601999961, 1.019436328545999970 ),
 .UNSPECIFIED. ) ;
#16637 = LINE ( 'NONE', #54042, #13797 ) ;
#16638 = CYLINDRICAL_SURFACE ( 'NONE', #23225, 1.350000000000000533 ) ;
#16639 = ORIENTED_EDGE ( 'NONE', *, *, #51141, .T. ) ;
#16640 = CARTESIAN_POINT ( 'NONE',  ( 8.727043146794999373, -3.882020254083999866, 5.870054788755000530 ) ) ;
#16641 = CARTESIAN_POINT ( 'NONE',  ( 8.871889158775999817, 2.702406276695999754, -6.981052078638000147 ) ) ;
#16642 = ADVANCED_FACE ( 'NONE', ( #64365 ), #37903, .F. ) ;
#16643 = ADVANCED_FACE ( 'NONE', ( #37470 ), #16829, .T. ) ;
#16644 = CARTESIAN_POINT ( 'NONE',  ( 8.266851002545999805, 2.832432432432000269, 6.822293592207000934 ) ) ;
#16645 = CARTESIAN_POINT ( 'NONE',  ( 25.55274001713692655, -11.13099802292605389, -3.116587923746078292 ) ) ;
#16646 = CARTESIAN_POINT ( 'NONE',  ( 0.5022402514714999766, 2.306917309723999665, 2.681989686974000087 ) ) ;
#16647 = CARTESIAN_POINT ( 'NONE',  ( 10.77879632507499785, 4.423544049216699747, 6.714825466131699727 ) ) ;
#16648 = CARTESIAN_POINT ( 'NONE',  ( 2.266292344358999955, -3.720972690152000162, 0.5317331180723999795 ) ) ;
#16649 = VERTEX_POINT ( 'NONE', #67 ) ;
#16650 = CARTESIAN_POINT ( 'NONE',  ( 6.999999691988000095, 13.87069231928999891, -4.225386915259999654 ) ) ;
#16651 = CARTESIAN_POINT ( 'NONE',  ( 11.03482133862663517, -3.057020944820409536, -8.373613860257943742 ) ) ;
#16652 = CARTESIAN_POINT ( 'NONE',  ( 10.09964828895399869, 5.121614868497999851, 6.887384543790600056 ) ) ;
#16653 = CARTESIAN_POINT ( 'NONE',  ( 5.518321182381299650, 12.20777697080807300, 3.787023466221932200 ) ) ;
#16654 = CARTESIAN_POINT ( 'NONE',  ( 8.796579719592999780, 2.368264398678999516, 7.410200237937000445 ) ) ;
#16655 = EDGE_LOOP ( 'NONE', ( #30989, #16413, #64911, #68092, #8008, #29314 ) ) ;
#16656 = CARTESIAN_POINT ( 'NONE',  ( 5.679587365828999701, -0.1291622704458000037, -1.609550399409999999 ) ) ;
#16657 = CARTESIAN_POINT ( 'NONE',  ( 7.598895280409000641, 4.462983737834999687, -8.994919855354998717 ) ) ;
#16658 = EDGE_CURVE ( 'NONE', #15819, #56117, #54451, .T. ) ;
#16659 = CARTESIAN_POINT ( 'NONE',  ( 8.304386322453103375, -4.439452195556469860, 9.191388126121186275 ) ) ;
#16660 = CARTESIAN_POINT ( 'NONE',  ( 9.370759580229000463, -5.244164909883999748, 7.797385380423699885 ) ) ;
#16661 = VERTEX_POINT ( 'NONE', #32247 ) ;
#16662 = CARTESIAN_POINT ( 'NONE',  ( 16.18326532032400067, -3.458591647041000083, -11.88419159288000060 ) ) ;
#16663 = CARTESIAN_POINT ( 'NONE',  ( 11.44446504844000145, 11.61858443320999967, 1.410913393917999858 ) ) ;
#16664 = VERTEX_POINT ( 'NONE', #33622 ) ;
#16665 = EDGE_CURVE ( 'NONE', #51145, #12348, #42722, .T. ) ;
#16666 = CARTESIAN_POINT ( 'NONE',  ( 24.51106247826800910, 3.208407811236159812, -11.97394356203530030 ) ) ;
#16667 = CARTESIAN_POINT ( 'NONE',  ( 7.744301838472999577, -3.130384865731000055, 6.467396727560999814 ) ) ;
#16668 = CARTESIAN_POINT ( 'NONE',  ( 18.16600461949965961, -0.1321590433901045358, -13.89915950722680016 ) ) ;
#16669 = ORIENTED_EDGE ( 'NONE', *, *, #7850, .T. ) ;
#16670 = CARTESIAN_POINT ( 'NONE',  ( 9.599999931441001166, -2.935682118448999844, 6.844464000216799349 ) ) ;
#16671 = CARTESIAN_POINT ( 'NONE',  ( 17.55505043854147118, -1.875000000000000000, 13.78631952119024895 ) ) ;
#16672 = CARTESIAN_POINT ( 'NONE',  ( 10.22934687351666661, -4.163624617374463099, 8.750000000000000000 ) ) ;
#16673 = DIRECTION ( 'NONE',  ( -1.000000000000000000, 0.000000000000000000, 0.000000000000000000 ) ) ;
#16674 = CARTESIAN_POINT ( 'NONE',  ( 10.79657053952199952, -4.502253688815499366, 8.675184076076000395 ) ) ;
#16675 = ORIENTED_EDGE ( 'NONE', *, *, #55741, .F. ) ;
#16676 = CARTESIAN_POINT ( 'NONE',  ( 8.732392219593000604, 2.806082850903000026, 8.615880516515998622 ) ) ;
#16677 = ORIENTED_EDGE ( 'NONE', *, *, #64209, .F. ) ;
#16678 = CARTESIAN_POINT ( 'NONE',  ( 9.916846873516668381, -4.768183399968644487, 6.500416447002274722 ) ) ;
#16679 = CARTESIAN_POINT ( 'NONE',  ( 15.46531638133300035, -9.264179323101998875, -8.208366262023000459 ) ) ;
#16680 = CARTESIAN_POINT ( 'NONE',  ( 10.97046361309999973, 6.164149261029999494, -5.039793574291000056 ) ) ;
#16681 = ORIENTED_EDGE ( 'NONE', *, *, #50834, .T. ) ;
#16682 = CARTESIAN_POINT ( 'NONE',  ( 12.18180637322648430, -2.452078064253476519, -12.46259978693893267 ) ) ;
#16683 = CARTESIAN_POINT ( 'NONE',  ( 0.4200574278457634425, -2.102383120260660210, -2.734278034550727376 ) ) ;
#16684 = DIRECTION ( 'NONE',  ( 0.000000000000000000, 1.000000000000000000, 0.000000000000000000 ) ) ;
#16685 = CARTESIAN_POINT ( 'NONE',  ( 24.19055685125828603, -3.314211647974591113, -12.40155450095146428 ) ) ;
#16686 = CARTESIAN_POINT ( 'NONE',  ( 12.23477282158795809, -2.066986176408053932, -13.84657559728969645 ) ) ;
#16687 = CARTESIAN_POINT ( 'NONE',  ( 10.79718447801629999, -2.996774412198000448, -7.477880487566260115 ) ) ;
#16688 = CARTESIAN_POINT ( 'NONE',  ( 12.15578049617215939, -2.108731457858033842, 12.42302753736614562 ) ) ;
#16689 = CARTESIAN_POINT ( 'NONE',  ( 18.27123885515672441, -2.366823750208070898, 12.37571350032474626 ) ) ;
#16690 = VERTEX_POINT ( 'NONE', #64026 ) ;
#16691 = CARTESIAN_POINT ( 'NONE',  ( 11.30878751119029957, -5.041025164610000608, -8.044634158732998586 ) ) ;
#16692 = EDGE_LOOP ( 'NONE', ( #1348, #16837, #42301, #4864, #7420 ) ) ;
#16693 = FACE_OUTER_BOUND ( 'NONE', #39133, .T. ) ;
#16694 = CARTESIAN_POINT ( 'NONE',  ( 9.635004719593998956, 2.334550724494000029, -7.977056617806000283 ) ) ;
#16695 = CARTESIAN_POINT ( 'NONE',  ( 10.64127413024999846, 2.258699798012000048, -6.863478635463000188 ) ) ;
#16696 = CARTESIAN_POINT ( 'NONE',  ( 23.59999467231800097, -10.30760443253999981, -9.317695455237998914 ) ) ;
#16697 = CARTESIAN_POINT ( 'NONE',  ( 11.65221028326116048, -4.908903471848705458, 7.824988602100019008 ) ) ;
#16698 = PRODUCT_DEFINITION ( 'UNKNOWN', '', #24024, #35999 ) ;
#16699 = CARTESIAN_POINT ( 'NONE',  ( 24.08696074224200245, -12.68545904450999906, 3.367396192228000018 ) ) ;
#16700 = CARTESIAN_POINT ( 'NONE',  ( 17.55505043854147118, -1.760910691117812954, -12.47634535983622861 ) ) ;
#16701 = ORIENTED_EDGE ( 'NONE', *, *, #69132, .F. ) ;
#16702 = DIRECTION ( 'NONE',  ( -1.000000000000000000, 0.000000000000000000, 0.000000000000000000 ) ) ;
#16703 = CARTESIAN_POINT ( 'NONE',  ( 10.34021053755999908, 4.202028620710000162, 9.459600235481000041 ) ) ;
#16704 = B_SPLINE_CURVE_WITH_KNOTS ( 'NONE', 3,
 ( #43055, #12285, #11926, #33266 ),
 .UNSPECIFIED., .F., .F.,
 ( 4, 4 ),
 ( 0.000000000000000000, 1.000000000000000000 ),
 .UNSPECIFIED. ) ;
#16705 = DIRECTION ( 'NONE',  ( 1.000000000000000000, 0.000000000000000000, 0.000000000000000000 ) ) ;
#16706 = CARTESIAN_POINT ( 'NONE',  ( 11.32035090130999855, -3.241273085157000189, 7.030721746772699454 ) ) ;
#16707 = CARTESIAN_POINT ( 'NONE',  ( 5.440293001548999641, 12.88483958404999896, -2.133988467673999967 ) ) ;
#16708 = CARTESIAN_POINT ( 'NONE',  ( 11.81056516821459823, 4.609678151793300316, -8.115298063151199059 ) ) ;
#16709 = CARTESIAN_POINT ( 'NONE',  ( 10.19474327641866473, 5.745204535562014492, 7.382935988871072830 ) ) ;
#16710 = CARTESIAN_POINT ( 'NONE',  ( 23.66585382769999768, -10.00662356887000115, -9.518285594139999972 ) ) ;
#16711 = CARTESIAN_POINT ( 'NONE',  ( 23.81895245337700118, -9.670840248742999634, 9.333086655847001367 ) ) ;
#16712 = CARTESIAN_POINT ( 'NONE',  ( 7.000000000000000000, 0.5292307692307999245, 2.083846153846000249 ) ) ;
#16713 = VERTEX_POINT ( 'NONE', #10902 ) ;
#16714 = CARTESIAN_POINT ( 'NONE',  ( 9.120035841232999374, 5.288433695693000480, -8.041290150997999930 ) ) ;
#16715 = CARTESIAN_POINT ( 'NONE',  ( 7.550000000000000711, -4.000000000000000000, 8.849999999999999645 ) ) ;
#16716 = ADVANCED_FACE ( 'NONE', ( #37817 ), #63606, .T. ) ;
#16717 = EDGE_CURVE ( 'NONE', #52202, #41725, #19404, .T. ) ;
#16718 = CARTESIAN_POINT ( 'NONE',  ( 18.15125141007961318, 2.312191647150520613, 13.71145324559127054 ) ) ;
#16719 = DIRECTION ( 'NONE',  ( 1.000000000000000000, 0.000000000000000000, 0.000000000000000000 ) ) ;
#16720 = CARTESIAN_POINT ( 'NONE',  ( 10.49349279008999858, -4.332388355267299929, -8.734031750754999379 ) ) ;
#16721 = ORIENTED_EDGE ( 'NONE', *, *, #59302, .F. ) ;
#16722 = B_SPLINE_CURVE_WITH_KNOTS ( 'NONE', 3,
 ( #17828, #23055, #16430, #65706 ),
 .UNSPECIFIED., .F., .F.,
 ( 4, 4 ),
 ( 0.000000000000000000, 1.000000000000000000 ),
 .UNSPECIFIED. ) ;
#16723 = CARTESIAN_POINT ( 'NONE',  ( 16.09992084546400193, -8.991497430826001391, -8.719551690569000257 ) ) ;
#16724 = CARTESIAN_POINT ( 'NONE',  ( 9.079732780410999737, 5.421534627450999899, 6.381126373995999579 ) ) ;
#16726 = FACE_OUTER_BOUND ( 'NONE', #26122, .T. ) ;
#16725 = CARTESIAN_POINT ( 'NONE',  ( 9.360279719594000625, 3.031907308384000022, -8.729608011560001657 ) ) ;
#16727 = CARTESIAN_POINT ( 'NONE',  ( 2.939204570973131148, -1.496697095495769902, 2.893778235148168676 ) ) ;
#16728 = ORIENTED_EDGE ( 'NONE', *, *, #49081, .F. ) ;
#16729 = B_SPLINE_CURVE_WITH_KNOTS ( 'NONE', 3,
 ( #46760, #53033, #36261, #30678 ),
 .UNSPECIFIED., .F., .F.,
 ( 4, 4 ),
 ( 0.000000000000000000, 1.000000000000000000 ),
 .UNSPECIFIED. ) ;
#16730 = CARTESIAN_POINT ( 'NONE',  ( 9.834151567923001380, 5.173929249342999803, 8.813048229486998508 ) ) ;
#16731 = CARTESIAN_POINT ( 'NONE',  ( 18.23099845246962047, -2.253777188809249932, -13.81740256423587709 ) ) ;
#16732 = CARTESIAN_POINT ( 'NONE',  ( 10.35410941423799791, 4.742797679580299963, 8.174686939644999484 ) ) ;
#16733 = CARTESIAN_POINT ( 'NONE',  ( 10.01532628870999986, -4.946995631616999844, 8.559221361189001342 ) ) ;
#16734 = CARTESIAN_POINT ( 'NONE',  ( 7.722357335211003537, 2.834201928695000650, 6.826641520477001457 ) ) ;
#16735 = VERTEX_POINT ( 'NONE', #27684 ) ;
#16736 = CARTESIAN_POINT ( 'NONE',  ( 8.391562694006999834, 2.899763935154999750, -6.589890517430999850 ) ) ;
#16738 = CARTESIAN_POINT ( 'NONE',  ( 10.84974435320999930, -5.265000209383999596, -6.385811305909999902 ) ) ;
#16737 = CARTESIAN_POINT ( 'NONE',  ( 12.66849918197500102, -12.16651130357000099, 3.137066692814999946 ) ) ;
#16739 = AXIS2_PLACEMENT_3D ( 'NONE', #66549, #29524, #19347 ) ;
#16740 = CARTESIAN_POINT ( 'NONE',  ( 7.807002133442725089, -4.386469107892202679, 9.196132381460992988 ) ) ;
#16741 = CARTESIAN_POINT ( 'NONE',  ( 9.305875415870998424, -4.945293979885000191, 9.077881967919999795 ) ) ;
#16742 = CARTESIAN_POINT ( 'NONE',  ( 11.30367835872029936, -5.113555564477999305, -6.798177532456199934 ) ) ;
#16743 = VERTEX_POINT ( 'NONE', #59480 ) ;
#16744 = CARTESIAN_POINT ( 'NONE',  ( 9.404346873515669003, 2.750000000000000000, -7.663624617374465764 ) ) ;
#16745 = CARTESIAN_POINT ( 'NONE',  ( 11.22333863405319931, -3.380905141010200232, 6.710270673950399889 ) ) ;
#16746 = EDGE_CURVE ( 'NONE', #11095, #63961, #66082, .T. ) ;
#16747 = CARTESIAN_POINT ( 'NONE',  ( 7.411012926802005296, 3.233242541571998085, 6.481873309613996881 ) ) ;
#16748 = CARTESIAN_POINT ( 'NONE',  ( 11.13349010443639919, 5.274453806861999716, 7.404690636538299842 ) ) ;
#16749 = ORIENTED_EDGE ( 'NONE', *, *, #53094, .F. ) ;
#16750 = CARTESIAN_POINT ( 'NONE',  ( 9.319414158774000256, 2.656512020013999997, -7.884832994446999699 ) ) ;
#16751 = CARTESIAN_POINT ( 'NONE',  ( 12.33239129661525268, 1.934538128658851885, -12.45060726317137778 ) ) ;
#16752 = CARTESIAN_POINT ( 'NONE',  ( 11.05569598648999907, -2.869047858956000230, 6.826612223887499553 ) ) ;
#16753 = CARTESIAN_POINT ( 'NONE',  ( 9.262755466223577372, 2.920626183394224196, -8.329572976240578797 ) ) ;
#16754 = CARTESIAN_POINT ( 'NONE',  ( 18.16732611089587124, 2.625479215054820070, -13.64604457655927305 ) ) ;
#16755 = ORIENTED_EDGE ( 'NONE', *, *, #20126, .F. ) ;
#16756 = FACE_OUTER_BOUND ( 'NONE', #33145, .T. ) ;
#16757 = CARTESIAN_POINT ( 'NONE',  ( 16.86666666233133327, 3.345268057356068692, 11.86064107292373571 ) ) ;
#16758 = ORIENTED_EDGE ( 'NONE', *, *, #15270, .F. ) ;
#16759 = CARTESIAN_POINT ( 'NONE',  ( 11.30000000000000071, 11.28618258042000022, 10.08934826511999994 ) ) ;
#16760 = CARTESIAN_POINT ( 'NONE',  ( 11.33872066707849768, 4.858611803369300652, 8.019361746728900897 ) ) ;
#16761 = DIRECTION ( 'NONE',  ( 1.000000000000000000, 0.000000000000000000, 0.000000000000000000 ) ) ;
#16762 = CARTESIAN_POINT ( 'NONE',  ( 11.11264834745999863, 2.146077493652999824, -7.517188756437000130 ) ) ;
#16763 = CARTESIAN_POINT ( 'NONE',  ( 7.729292060080003246, 5.085123327752999245, 6.553315682963002153 ) ) ;
#16764 = CARTESIAN_POINT ( 'NONE',  ( 7.986083034292184912, -5.349307872168665767, 7.676713696079082716 ) ) ;
#16765 = CARTESIAN_POINT ( 'NONE',  ( 11.32299956498189886, 2.792989229543000107, -7.174999999999999822 ) ) ;
#16766 = CARTESIAN_POINT ( 'NONE',  ( 17.81083341652436403, -0.6731412448965096162, -12.58200685883812753 ) ) ;
#16767 = CARTESIAN_POINT ( 'NONE',  ( 12.18214412808134206, 2.552249690270588012, -12.43927262873618211 ) ) ;
#16768 = CARTESIAN_POINT ( 'NONE',  ( 10.84226088462129844, -3.997572771977982775, -6.359261544073000039 ) ) ;
#16769 = CARTESIAN_POINT ( 'NONE',  ( 9.112170280412000167, 2.368264398678999516, 7.410200237937000445 ) ) ;
#16770 = ORIENTED_EDGE ( 'NONE', *, *, #48313, .T. ) ;
#16771 = PRESENTATION_STYLE_ASSIGNMENT (( #4911 ) ) ;
#16772 = CARTESIAN_POINT ( 'NONE',  ( 24.35365242081700288, -11.54878985755999388, 2.979915831581000152 ) ) ;
#16773 = CARTESIAN_POINT ( 'NONE',  ( 11.59999999999999964, -4.817420948848700313, -7.174999999999999822 ) ) ;
#16774 = LINE ( 'NONE', #49638, #53771 ) ;
#16775 = AXIS2_PLACEMENT_3D ( 'NONE', #67941, #9210, #3622 ) ;
#16776 = CARTESIAN_POINT ( 'NONE',  ( 18.27918563591880385, 2.436421501371055065, 12.36221688302663146 ) ) ;
#16777 = EDGE_CURVE ( 'NONE', #52199, #33729, #47776, .T. ) ;
#16778 = CARTESIAN_POINT ( 'NONE',  ( 10.90000000000000036, 0.2500000000000000000, -4.902439024389999567 ) ) ;
#16779 = EDGE_CURVE ( 'NONE', #28326, #23313, #43506, .T. ) ;
#16780 = CYLINDRICAL_SURFACE ( 'NONE', #21071, 0.5999999999999999778 ) ;
#16781 = PLANE ( 'NONE',  #42497 ) ;
#16782 = B_SPLINE_CURVE_WITH_KNOTS ( 'NONE', 3,
 ( #35626, #68098, #62175, #41541, #14971, #24094 ),
 .UNSPECIFIED., .F., .F.,
 ( 4, 2, 4 ),
 ( 0.000000000000000000, 0.5000000000000000000, 1.000000000000000000 ),
 .UNSPECIFIED. ) ;
#16783 = CARTESIAN_POINT ( 'NONE',  ( 25.55266313104714726, -2.866471730758334058, 11.19811586864718933 ) ) ;
#16784 = ORIENTED_EDGE ( 'NONE', *, *, #54718, .T. ) ;
#16785 = CARTESIAN_POINT ( 'NONE',  ( 12.25790434794253692, -2.952613167459266830, 12.24916959777017667 ) ) ;
#16786 = CARTESIAN_POINT ( 'NONE',  ( 9.933633995697999097, -3.001718438313799808, -7.610798122400000310 ) ) ;
#16787 = CARTESIAN_POINT ( 'NONE',  ( 10.18240541510999897, 2.607737086676999994, 7.783408568367999436 ) ) ;
#16788 = CIRCLE ( 'NONE', #27991, 1.000000000000000222 ) ;
#16789 = B_SPLINE_CURVE_WITH_KNOTS ( 'NONE', 3,
 ( #67922, #10573, #63708, #20380 ),
 .UNSPECIFIED., .F., .F.,
 ( 4, 4 ),
 ( 0.000000000000000000, 1.000000000000000000 ),
 .UNSPECIFIED. ) ;
#16790 = CARTESIAN_POINT ( 'NONE',  ( 8.288209573716871503, 2.946091060167179698, -6.424054805521736355 ) ) ;
#16791 = B_SPLINE_SURFACE_WITH_KNOTS ( 'NONE', 3, 3, ( 
 ( #21346, #15763, #6288, #42345 ),
 ( #27635, #37425, #10510, #37090 ),
 ( #53850, #11535, #5948, #43374 ),
 ( #367, #32199, #59782, #43017 ),
 ( #63644, #64674, #58748, #58405 ),
 ( #26948, #1065, #21009, #715 ),
 ( #68891, #54189, #26605, #32877 ),
 ( #48956, #48259, #11197, #21681 ),
 ( #10853, #22376, #31850, #38109 ),
 ( #53165, #47587, #16441, #27290 ),
 ( #11886, #53512, #43717, #25 ),
 ( #52824, #65010, #16100, #4920 ),
 ( #32535, #17129, #38463, #59096 ),
 ( #64320, #48610, #47926, #5601 ) ),
 .UNSPECIFIED., .F., .F., .F.,
 ( 4, 1, 1, 1, 1, 1, 1, 1, 1, 1, 1, 4 ),
 ( 4, 4 ),
 ( -0.008665511476623999690, 0.000000000000000000, 0.1111111111111000027, 0.2222222222222000054, 0.3333333333333000081, 0.4444444444444000109, 0.5555555555555999891, 0.6666666666667000474, 0.7777777777777999946, 0.8888888888888999418, 1.000000000000000000, 1.011507985605999860 ),
 ( -0.2206650672664999813, 1.220665067267000081 ),
 .UNSPECIFIED. ) ;
#16792 = CARTESIAN_POINT ( 'NONE',  ( 10.40333997687999990, 4.213854445120500003, -6.519583185858300212 ) ) ;
#16793 = CARTESIAN_POINT ( 'NONE',  ( 12.30913258640366870, -0.5248261352964553872, 12.58906749861124119 ) ) ;
#16794 = CARTESIAN_POINT ( 'NONE',  ( 8.368323341230000878, 4.780986922229000236, 6.267222470044999660 ) ) ;
#16795 = CARTESIAN_POINT ( 'NONE',  ( 9.710633014819311626, 3.646661381981713301, -8.850710600599320799 ) ) ;
#16796 = CARTESIAN_POINT ( 'NONE',  ( 12.19425446308164140, 2.632875717725343012, 12.41961888770621592 ) ) ;
#16797 = CARTESIAN_POINT ( 'NONE',  ( 18.01911383344807405, -3.562435417629448597, -12.00770609665208966 ) ) ;
#16798 = CARTESIAN_POINT ( 'NONE',  ( 11.53148876160955005, 3.209326035813000022, -8.322268080792200706 ) ) ;
#16799 = CARTESIAN_POINT ( 'NONE',  ( 11.07484075165016613, 2.725159248349832364, -6.497852970900666492 ) ) ;
#16800 = EDGE_CURVE ( 'NONE', #61758, #26679, #41075, .T. ) ;
#16801 = CARTESIAN_POINT ( 'NONE',  ( 10.61443584123000150, 5.287628373050000441, -7.937241318065001217 ) ) ;
#16802 = CARTESIAN_POINT ( 'NONE',  ( 9.525000000000000355, 4.417172942406000224, 8.783926296998000538 ) ) ;
#16804 = CARTESIAN_POINT ( 'NONE',  ( 18.06844660307579531, -0.3566172609784874492, 12.69326555881911034 ) ) ;
#16803 = CARTESIAN_POINT ( 'NONE',  ( 8.493369886551995762, 5.097498803759001440, 6.607670056088003285 ) ) ;
#16805 = CARTESIAN_POINT ( 'NONE',  ( 11.00000000000000000, 4.991767524623399233, 7.825000000000000178 ) ) ;
#16806 = EDGE_LOOP ( 'NONE', ( #5243, #20594, #61152, #57204 ) ) ;
#16807 = EDGE_CURVE ( 'NONE', #26903, #62306, #22288, .T. ) ;
#16808 = B_SPLINE_CURVE_WITH_KNOTS ( 'NONE', 3,
 ( #3242, #8145, #51477, #39971 ),
 .UNSPECIFIED., .F., .F.,
 ( 4, 4 ),
 ( 0.6941835283959838510, 1.000000000000000000 ),
 .UNSPECIFIED. ) ;
#16809 = CARTESIAN_POINT ( 'NONE',  ( 11.09999999999999964, -4.000000000000000000, 7.500000000000000000 ) ) ;
#16810 = CARTESIAN_POINT ( 'NONE',  ( 23.89491306796949033, -9.543190063518746769, -9.361237058299565206 ) ) ;
#16811 = CARTESIAN_POINT ( 'NONE',  ( 12.41307909110101804, -11.56466389787636473, 4.809819853924211408 ) ) ;
#16812 = DIRECTION ( 'NONE',  ( -1.000000000000000000, 0.000000000000000000, 0.000000000000000000 ) ) ;
#16813 = CARTESIAN_POINT ( 'NONE',  ( 12.41877979183516700, -1.899635599875575176, 13.87052873021461430 ) ) ;
#16814 = CARTESIAN_POINT ( 'NONE',  ( 9.470944094206000585, -5.100000000000000533, 6.571291218949999902 ) ) ;
#16815 = DIRECTION ( 'NONE',  ( 0.000000000000000000, 0.000000000000000000, -1.000000000000000000 ) ) ;
#16816 = ORIENTED_EDGE ( 'NONE', *, *, #17941, .F. ) ;
#16817 = DIRECTION ( 'NONE',  ( -1.000000000000000000, 0.000000000000000000, 0.000000000000000000 ) ) ;
#16818 = B_SPLINE_CURVE_WITH_KNOTS ( 'NONE', 3,
 ( #59609, #55409, #54712, #7501, #2267, #22202, #18351, #28148, #39674, #16951, #60993, #13113 ),
 .UNSPECIFIED., .F., .F.,
 ( 4, 2, 2, 2, 2, 4 ),
 ( 0.000000000000000000, 0.2499999999999970579, 0.3749999999999958922, 0.4999999999999947820, 0.7499999999999973355, 1.000000000000000000 ),
 .UNSPECIFIED. ) ;
#16819 = CARTESIAN_POINT ( 'NONE',  ( 7.000000000000000000, 8.307879248642999315, 4.307879248643000203 ) ) ;
#16820 = DIRECTION ( 'NONE',  ( 0.000000000000000000, 1.000000000000000000, 0.000000000000000000 ) ) ;
#16821 = CARTESIAN_POINT ( 'NONE',  ( 0.8897459993062000194, -3.461062994654999780, -0.9617132324576000979 ) ) ;
#16822 = CARTESIAN_POINT ( 'NONE',  ( 18.36030550607078737, -3.088870463273618139, 11.23311224736321101 ) ) ;
#16823 = EDGE_CURVE ( 'NONE', #29320, #15110, #50246, .T. ) ;
#16824 = VECTOR ( 'NONE', #44336, 1000.000000000000000 ) ;
#16825 = CARTESIAN_POINT ( 'NONE',  ( 17.69913221809297710, 1.891485217175129963, -12.57274297139331587 ) ) ;
#16826 = CARTESIAN_POINT ( 'NONE',  ( 10.18240541510999897, 2.607737086676999994, 7.783408568367999436 ) ) ;
#16827 = CARTESIAN_POINT ( 'NONE',  ( 10.75210807141120029, 4.040019166404060336, 6.634727177901499573 ) ) ;
#16829 = CYLINDRICAL_SURFACE ( 'NONE', #34591, 0.4999999999999998335 ) ;
#16828 = AXIS2_PLACEMENT_3D ( 'NONE', #33419, #54036, #16633 ) ;
#16830 = CARTESIAN_POINT ( 'NONE',  ( 10.44811814679000150, -5.235603901491000300, -6.609968500665999613 ) ) ;
#16831 = CARTESIAN_POINT ( 'NONE',  ( 7.844724277266999835, 4.719412473309000156, 6.357657803787000184 ) ) ;
#16832 = CARTESIAN_POINT ( 'NONE',  ( 9.832537864288001472, 2.899999999999999911, 6.571291218949999902 ) ) ;
#16833 = FACE_OUTER_BOUND ( 'NONE', #67517, .T. ) ;
#16834 = DIRECTION ( 'NONE',  ( 0.000000000000000000, 1.000000000000000000, 0.000000000000000000 ) ) ;
#16835 = B_SPLINE_CURVE_WITH_KNOTS ( 'NONE', 3,
 ( #9767, #3493, #46502, #67122 ),
 .UNSPECIFIED., .F., .F.,
 ( 4, 4 ),
 ( 0.000000000000000000, 1.000000000000000000 ),
 .UNSPECIFIED. ) ;
#16836 = B_SPLINE_CURVE_WITH_KNOTS ( 'NONE', 3,
 ( #12408, #45606, #2263, #17658 ),
 .UNSPECIFIED., .F., .F.,
 ( 4, 4 ),
 ( 0.000000000000000000, 1.000000000000000000 ),
 .UNSPECIFIED. ) ;
#16837 = ORIENTED_EDGE ( 'NONE', *, *, #41377, .F. ) ;
#16838 = CARTESIAN_POINT ( 'NONE',  ( 7.402683226288421459, 2.556880117659619867, 8.471723903841693826 ) ) ;
#16839 = CARTESIAN_POINT ( 'NONE',  ( 11.54333729122640051, -5.003122373830000136, 7.526388557597149642 ) ) ;
#16840 = ORIENTED_EDGE ( 'NONE', *, *, #7932, .T. ) ;
#16841 = CARTESIAN_POINT ( 'NONE',  ( 17.99219435089542074, -2.053195051521780279, 13.75813171417237868 ) ) ;
#16842 = CARTESIAN_POINT ( 'NONE',  ( 10.12841772631199966, -3.509411006705700053, -8.509834072393999804 ) ) ;
#16843 = ORIENTED_EDGE ( 'NONE', *, *, #44885, .F. ) ;
#16844 = CARTESIAN_POINT ( 'NONE',  ( 11.67403632436368888, 3.023821283238099955, 7.727966254184200245 ) ) ;
#16845 = CARTESIAN_POINT ( 'NONE',  ( 6.374674949252075784, -0.9558318679937189977, -0.6073786151858517890 ) ) ;
#16846 = CARTESIAN_POINT ( 'NONE',  ( 24.13790633822682352, 3.328477659013978407, -12.49555518615514949 ) ) ;
#16847 = B_SPLINE_CURVE_WITH_KNOTS ( 'NONE', 3,
 ( #60452, #23731, #49958, #2072 ),
 .UNSPECIFIED., .F., .F.,
 ( 4, 4 ),
 ( 0.000000000000000000, 1.000000000000000000 ),
 .UNSPECIFIED. ) ;
#16848 = DIRECTION ( 'NONE',  ( -1.000000000000000000, 0.000000000000000000, 0.000000000000000000 ) ) ;
#16849 = CARTESIAN_POINT ( 'NONE',  ( 8.832537864289999874, 2.899999999999999911, 6.571291218949999902 ) ) ;
#16850 = CARTESIAN_POINT ( 'NONE',  ( 12.21982127437517285, 0.2196390009034050184, -13.89766917373429678 ) ) ;
#16851 = CARTESIAN_POINT ( 'NONE',  ( 11.60000000000000142, -4.400439255161257002, -6.596661741119738132 ) ) ;
#16852 = CARTESIAN_POINT ( 'NONE',  ( 9.870877370727999534, -2.904359058094999835, -8.563874348197000330 ) ) ;
#16853 = CARTESIAN_POINT ( 'NONE',  ( 11.68748876160954886, -4.600381688599499697, -8.124372018288600117 ) ) ;
#16854 = EDGE_LOOP ( 'NONE', ( #16382, #3280, #10998, #5088 ) ) ;
#16855 = CARTESIAN_POINT ( 'NONE',  ( 9.318935841232999451, 2.644017913812000131, -7.838184857420000817 ) ) ;
#16856 = EDGE_LOOP ( 'NONE', ( #12112, #50354, #24190 ) ) ;
#16857 = CARTESIAN_POINT ( 'NONE',  ( 10.74809687351632448, 4.327184855449106138, -6.282534154164607365 ) ) ;
#16858 = ORIENTED_EDGE ( 'NONE', *, *, #49582, .T. ) ;
#16859 = CARTESIAN_POINT ( 'NONE',  ( 5.200000000000000178, 0.2500000000000000000, -9.776630298829998011 ) ) ;
#16860 = CARTESIAN_POINT ( 'NONE',  ( 18.00599872992922457, -2.932869382066921826, -12.34010572687589757 ) ) ;
#16861 = CARTESIAN_POINT ( 'NONE',  ( 25.29995737991200144, -8.533537546129998930, 7.925519566782000425 ) ) ;
#16862 = CARTESIAN_POINT ( 'NONE',  ( 10.19601354018254291, 4.999583552997727054, -6.731816600031361730 ) ) ;
#16863 = EDGE_CURVE ( 'NONE', #14127, #8973, #34406, .T. ) ;
#16864 = CARTESIAN_POINT ( 'NONE',  ( 12.54503913623221578, 3.068442045733652979, 13.53626685534802476 ) ) ;
#16865 = EDGE_CURVE ( 'NONE', #6782, #13349, #59393, .T. ) ;
#16866 = CARTESIAN_POINT ( 'NONE',  ( 17.59669571873555682, -1.876302067258580619, 12.57524312254454202 ) ) ;
#16867 = CARTESIAN_POINT ( 'NONE',  ( 7.862706706567756498, 3.149338860038144006, -6.385288329380975014 ) ) ;
#16868 = EDGE_CURVE ( 'NONE', #47736, #12318, #47638, .T. ) ;
#16869 = CIRCLE ( 'NONE', #55963, 12.60000000000000142 ) ;
#16870 = CARTESIAN_POINT ( 'NONE',  ( 12.44045292577857786, 0.5080432161604395702, 13.88750743611952210 ) ) ;
#16871 = ORIENTED_EDGE ( 'NONE', *, *, #1484, .F. ) ;
#16872 = CARTESIAN_POINT ( 'NONE',  ( 7.405090560819000522, 5.321245676936000812, -7.068438969505000280 ) ) ;
#16873 = CARTESIAN_POINT ( 'NONE',  ( 8.906851002547000462, 2.832432432432000269, -6.822293592207000934 ) ) ;
#16874 = CARTESIAN_POINT ( 'NONE',  ( 9.986774547327625484, 4.078513067950353843, 8.371417217572535208 ) ) ;
#16875 = CARTESIAN_POINT ( 'NONE',  ( 4.285264598750999632, -0.3285995775302999466, -1.445177149630999969 ) ) ;
#16876 = CARTESIAN_POINT ( 'NONE',  ( 9.535554719593998030, 3.927090956378999742, -9.230892435423001530 ) ) ;
#16877 = CARTESIAN_POINT ( 'NONE',  ( 18.31684170297491576, 11.66237234948261836, -4.568609802378666984 ) ) ;
#16878 = CARTESIAN_POINT ( 'NONE',  ( 10.48414299032999963, -4.098653366703000067, -9.351353705206001621 ) ) ;
#16879 = VERTEX_POINT ( 'NONE', #36277 ) ;
#16880 = CARTESIAN_POINT ( 'NONE',  ( 9.643930206848999376, 5.250000000000000000, 7.500000000000000000 ) ) ;
#16881 = AXIS2_PLACEMENT_3D ( 'NONE', #18258, #34346, #29800 ) ;
#16882 = CARTESIAN_POINT ( 'NONE',  ( 13.69997185827400266, -11.40547114375999982, -2.374390024598000082 ) ) ;
#16883 = CARTESIAN_POINT ( 'NONE',  ( 12.80505043854143388, 1.787816316115912185, -13.88537766212463254 ) ) ;
#16884 = CARTESIAN_POINT ( 'NONE',  ( 11.83518044953559922, 4.768048975940600620, -7.900497508315099893 ) ) ;
#16885 = CARTESIAN_POINT ( 'NONE',  ( 5.927943173016666734, 0.9218200799623694763, 1.199500263597272465 ) ) ;
#16886 = CARTESIAN_POINT ( 'NONE',  ( 10.85679632507500081, 4.490665650747399873, -8.409605917786398877 ) ) ;
#16887 = CARTESIAN_POINT ( 'NONE',  ( 9.685317406968998455, 4.186809223719299311, -8.486886322867700727 ) ) ;
#16889 = FACE_OUTER_BOUND ( 'NONE', #10206, .T. ) ;
#16888 = CARTESIAN_POINT ( 'NONE',  ( 9.547113844317999920, -3.746347404385800051, 8.471855267550699509 ) ) ;
#16890 = CARTESIAN_POINT ( 'NONE',  ( 7.717562992925000032, 2.846244489068278316, 6.797277731627717756 ) ) ;
#16891 = ORIENTED_EDGE ( 'NONE', *, *, #16211, .F. ) ;
#16892 = CARTESIAN_POINT ( 'NONE',  ( 11.02301463001509774, 4.547357026650399980, 8.376661845795100092 ) ) ;
#16893 = CARTESIAN_POINT ( 'NONE',  ( 7.559219638201004621, -3.224407481241000628, 6.403792276147000528 ) ) ;
#16894 = CARTESIAN_POINT ( 'NONE',  ( 9.051138961223999857, 5.059894361919000438, 6.783753885003399375 ) ) ;
#16895 = CARTESIAN_POINT ( 'NONE',  ( 11.09999999999999964, 5.449702572737000317, -5.124965750789000296 ) ) ;
#16896 = CARTESIAN_POINT ( 'NONE',  ( 10.06844525594999951, -4.148609764890999863, 8.941457795715999524 ) ) ;
#16897 = CARTESIAN_POINT ( 'NONE',  ( -0.2999999999999999889, -0.5773502691895999739, -1.000000000000000000 ) ) ;
#16898 = DIRECTION ( 'NONE',  ( -0.8660254037844288266, 0.000000000000000000, -0.5000000000000169864 ) ) ;
#16899 = CARTESIAN_POINT ( 'NONE',  ( 9.913279731609000223, -3.909869487835140323, -6.499640669006000238 ) ) ;
#16900 = CARTESIAN_POINT ( 'NONE',  ( 5.202515767743999930, 0.1165019947749000029, 1.093825345293000018 ) ) ;
#16901 = EDGE_CURVE ( 'NONE', #30682, #46086, #57592, .T. ) ;
#16902 = CARTESIAN_POINT ( 'NONE',  ( 11.29683585285767755, -3.460706475588385178, 6.812066793331982950 ) ) ;
#16903 = CARTESIAN_POINT ( 'NONE',  ( 24.60170725920900026, -3.645111442846999950, 12.27956986324999988 ) ) ;
#16904 = CARTESIAN_POINT ( 'NONE',  ( 12.08902763632552002, -4.786505910413500153, 7.862914650060299770 ) ) ;
#16905 = CARTESIAN_POINT ( 'NONE',  ( 11.81056516821459823, 4.609678151793300316, -8.115298063151199059 ) ) ;
#16906 = EDGE_CURVE ( 'NONE', #42489, #26585, #6757, .T. ) ;
#16907 = CARTESIAN_POINT ( 'NONE',  ( 8.199995110659001440, -2.894508759333000114, 6.645190873281999089 ) ) ;
#16908 = CARTESIAN_POINT ( 'NONE',  ( 24.69847988401100380, -8.734423968153000928, 9.243501732991999731 ) ) ;
#16909 = CARTESIAN_POINT ( 'NONE',  ( 0.9468067992084583384, 0.9161175952574844850, -3.408904368339102930 ) ) ;
#16910 = ORIENTED_EDGE ( 'NONE', *, *, #62093, .T. ) ;
#16911 = CARTESIAN_POINT ( 'NONE',  ( 10.83253786428999987, 2.899999999999999911, 6.571291218949999902 ) ) ;
#16912 = CARTESIAN_POINT ( 'NONE',  ( 10.61257802013489737, -4.891884252872400474, -7.479237407015119743 ) ) ;
#16913 = CARTESIAN_POINT ( 'NONE',  ( 18.10291658807267368, 0.3009529451927861476, 12.69520353502463550 ) ) ;
#16914 = DIRECTION ( 'NONE',  ( 1.000000000000000000, -1.210302035963000169E-10, 1.972161209128000006E-09 ) ) ;
#16915 = CARTESIAN_POINT ( 'NONE',  ( 10.47530200610849604, 5.350262918594154371, 7.499984559551275964 ) ) ;
#16916 = CARTESIAN_POINT ( 'NONE',  ( 13.64331666222400052, 12.23490852752999913, 2.418322770048999981 ) ) ;
#16917 = VERTEX_POINT ( 'NONE', #66456 ) ;
#16918 = FACE_OUTER_BOUND ( 'NONE', #57874, .T. ) ;
#16919 = CARTESIAN_POINT ( 'NONE',  ( 17.98387256218933672, 2.954798081836346402, -13.56641578797405323 ) ) ;
#16920 = VERTEX_POINT ( 'NONE', #34663 ) ;
#16921 = CARTESIAN_POINT ( 'NONE',  ( 13.69586690835513210, 11.42311322218458969, 2.288407577489913525 ) ) ;
#16922 = CARTESIAN_POINT ( 'NONE',  ( 9.251933059621999078, -5.159251056493999954, 9.109488373271000583 ) ) ;
#16923 = CARTESIAN_POINT ( 'NONE',  ( 15.65609597790000151, 8.788746246889001412, 7.589637905006999752 ) ) ;
#16924 = VERTEX_POINT ( 'NONE', #18577 ) ;
#16925 = CARTESIAN_POINT ( 'NONE',  ( 23.74397595434759722, -13.10155070693668122, 3.794838497900099750 ) ) ;
#16926 = CARTESIAN_POINT ( 'NONE',  ( 10.88813259637009878, -5.155817667926999803, -8.129798612793599943 ) ) ;
#16927 = AXIS2_PLACEMENT_3D ( 'NONE', #5268, #47240, #42347 ) ;
#16928 = CARTESIAN_POINT ( 'NONE',  ( 7.423620280405000216, 3.447598131391000020, -9.141997724497999300 ) ) ;
#16929 = FACE_OUTER_BOUND ( 'NONE', #13198, .T. ) ;
#16930 = CARTESIAN_POINT ( 'NONE',  ( 9.468459139564425087, 5.148170612271298907, 8.212595183817528621 ) ) ;
#16931 = VERTEX_POINT ( 'NONE', #29425 ) ;
#16932 = CARTESIAN_POINT ( 'NONE',  ( 9.261668853699999815, -2.944250413017999612, 6.507387951280999339 ) ) ;
#16933 = CARTESIAN_POINT ( 'NONE',  ( 25.36466183423599929, 11.12554151139999981, -3.380142950005000202 ) ) ;
#16934 = DIRECTION ( 'NONE',  ( 0.000000000000000000, 0.000000000000000000, -1.000000000000000000 ) ) ;
#16935 = ORIENTED_EDGE ( 'NONE', *, *, #48313, .F. ) ;
#16936 = CARTESIAN_POINT ( 'NONE',  ( 11.66889198463462840, -3.216368914751022157, 11.40336763631111516 ) ) ;
#16937 = CARTESIAN_POINT ( 'NONE',  ( 10.19794194037999979, -4.262172867567000090, -8.834326937932999613 ) ) ;
#16938 = VERTEX_POINT ( 'NONE', #13678 ) ;
#16939 = CARTESIAN_POINT ( 'NONE',  ( 10.08857120343299840, 3.944651031655580287, 6.359530327585999565 ) ) ;
#16940 = CARTESIAN_POINT ( 'NONE',  ( 17.65082925870469666, -1.766819657443025937, -12.47551016841904215 ) ) ;
#16941 = CARTESIAN_POINT ( 'NONE',  ( 4.692768490066000275, 0.1331025639088000145, -1.551817757593000113 ) ) ;
#16942 = CIRCLE ( 'NONE', #43762, 1.349999999999999867 ) ;
#16943 = CARTESIAN_POINT ( 'NONE',  ( 11.60000000000000142, 4.247874375640066980, -6.451199048602686226 ) ) ;
#16944 = CARTESIAN_POINT ( 'NONE',  ( 24.87149320935953156, 11.61826505781595742, -3.203182254666349316 ) ) ;
#16945 = ADVANCED_FACE ( 'NONE', ( #50733 ), #45492, .F. ) ;
#16946 = CARTESIAN_POINT ( 'NONE',  ( 9.028772138681999238, 3.677371150249499898, 8.304747519296199698 ) ) ;
#16947 = ADVANCED_FACE ( 'NONE', ( #45828 ), #63528, .F. ) ;
#16948 = EDGE_CURVE ( 'NONE', #40442, #57158, #19278, .T. ) ;
#16949 = CARTESIAN_POINT ( 'NONE',  ( 9.334238628924479642, -3.792635205665601195, 9.233780771583109725 ) ) ;
#16950 = ORIENTED_EDGE ( 'NONE', *, *, #63620, .T. ) ;
#16951 = CARTESIAN_POINT ( 'NONE',  ( 8.307734559752500303, -5.093561253831357938, 6.540208455084596473 ) ) ;
#16952 = CARTESIAN_POINT ( 'NONE',  ( 11.19050471959000070, 2.516756593394000152, -6.840361808223000217 ) ) ;
#16953 = CARTESIAN_POINT ( 'NONE',  ( 4.500000125099000492, 1.829647544581999737E-13, 0.000000000000000000 ) ) ;
#16954 = CARTESIAN_POINT ( 'NONE',  ( 12.54721708147385506, 1.835134883933968064, -13.87920628830544878 ) ) ;
#16955 = CARTESIAN_POINT ( 'NONE',  ( 9.194602547868999665, -5.157768569202000108, 8.637845986715998237 ) ) ;
#16956 = CARTESIAN_POINT ( 'NONE',  ( 18.17902784157848117, 0.04113803725885954027, 13.89993798560270832 ) ) ;
#16957 = CARTESIAN_POINT ( 'NONE',  ( 25.48313530789599923, -2.676704236843000295, 11.27114544762000037 ) ) ;
#16958 = ORIENTED_EDGE ( 'NONE', *, *, #31575, .T. ) ;
#16959 = VERTEX_POINT ( 'NONE', #37308 ) ;
#16960 = CARTESIAN_POINT ( 'NONE',  ( 9.910633732652998518, 2.107262079134000210, 7.885285091859000062 ) ) ;
#16961 = CARTESIAN_POINT ( 'NONE',  ( 12.18105065343300275, -0.04081304477956804178, 13.89993877190689453 ) ) ;
#16962 = CARTESIAN_POINT ( 'NONE',  ( 12.54853131234585994, -0.5702303675871001065, -13.88425454623346944 ) ) ;
#16963 = CARTESIAN_POINT ( 'NONE',  ( 10.81316193496000011, -3.756072284922999938, 6.071597915422999314 ) ) ;
#16964 = CARTESIAN_POINT ( 'NONE',  ( 18.18005043854833147, -0.04052532577797417906, -13.90000015527654931 ) ) ;
#16965 = B_SPLINE_CURVE_WITH_KNOTS ( 'NONE', 3,
 ( #64383, #6702, #7054, #27348, #54953, #28043, #16504, #49351, #1813, #48670, #23133, #64729, #12650, #21744, #38167, #775, #22781, #16845, #65429, #43076, #48324, #38878, #37831, #1122, #5665, #428, #27699, #22435, #44131, #44484, #65775, #17552, #39218, #60200, #22090, #12304, #59497, #32594, #17901, #6351, #60544, #27006, #43435, #33980, #59154, #53908, #43777, #11595, #6008, #32939, #49015, #54249, #65071, #17191, #38522, #59844, #66124, #7396, #7750, #51089, #29091, #61576, #56335, #13692, #24519 ),
 .UNSPECIFIED., .F., .F.,
 ( 4, 2, 2, 2, 2, 2, 2, 2, 2, 2, 2, 2, 2, 2, 2, 2, 1, 2, 2, 2, 2, 2, 2, 2, 2, 2, 2, 2, 2, 2, 2, 2, 4 ),
 ( 0.000000000000000000, 0.03125000000000000000, 0.06250000000000000000, 0.09375000000000000000, 0.1250000000000000000, 0.1562500000000000000, 0.1875000000000000000, 0.2187500000000000000, 0.2500000000000000000, 0.2812500000000000000, 0.3125000000000000000, 0.3437500000000000000, 0.3750000000000000000, 0.4062500000000000000, 0.4375000000000000000, 0.4687500000000000000, 0.5000000000000000000, 0.5312500000000000000, 0.5625000000000000000, 0.5937500000000000000, 0.6250000000000000000, 0.6562500000000000000, 0.6875000000000000000, 0.7187500000000000000, 0.7500000000000000000, 0.7812500000000000000, 0.8125000000000000000, 0.8437500000000000000, 0.8750000000000000000, 0.9062500000000000000, 0.9375000000000000000, 0.9687500000000000000, 1.000000000000000000 ),
 .UNSPECIFIED. ) ;
#16966 = EDGE_CURVE ( 'NONE', #5467, #23807, #15927, .T. ) ;
#16967 = CARTESIAN_POINT ( 'NONE',  ( 8.154706853209001238, -4.255646685191999623, 9.114089645792999406 ) ) ;
#16968 = DIRECTION ( 'NONE',  ( 0.000000000000000000, -0.8648648648648720183, -0.5020047465136825426 ) ) ;
#16970 = CARTESIAN_POINT ( 'NONE',  ( 13.56663524094155626, 11.53596571847202767, 2.401556225329833705 ) ) ;
#16969 = CARTESIAN_POINT ( 'NONE',  ( 10.18436764078099976, -3.396982508013000501, 8.628164124510998789 ) ) ;
#16971 = CARTESIAN_POINT ( 'NONE',  ( 10.32118582084299874, 3.163839350524900063, -6.533484739457099622 ) ) ;
#16972 = VECTOR ( 'NONE', #3948, 1000.000000000000000 ) ;
#16973 = CARTESIAN_POINT ( 'NONE',  ( 7.564999999998999414, 5.349999999999999645, -7.500000000000000000 ) ) ;
#16974 = B_SPLINE_CURVE_WITH_KNOTS ( 'NONE', 3,
 ( #36293, #57613, #31063, #10407, #52371, #47137, #68438, #20558, #47481, #68787, #42242, #31749, #53067, #5166 ),
 .UNSPECIFIED., .F., .F.,
 ( 4, 2, 2, 2, 2, 2, 4 ),
 ( 0.000000000000000000, 0.1249999999999983624, 0.2499999999999967248, 0.4999999999999945599, 0.6249999999999958922, 0.7499999999999972244, 1.000000000000000000 ),
 .UNSPECIFIED. ) ;
#16975 = LINE ( 'NONE', #1253, #15103 ) ;
#16976 = CARTESIAN_POINT ( 'NONE',  ( 18.17001854112162818, -0.1120021961262577387, 12.69934078656687682 ) ) ;
#16977 = DIRECTION ( 'NONE',  ( 0.000000000000000000, -1.000000000000000000, 0.000000000000000000 ) ) ;
#16978 = CARTESIAN_POINT ( 'NONE',  ( 18.49995202021990082, -2.953582884391593222, 12.17185907300070902 ) ) ;
#16979 = ORIENTED_EDGE ( 'NONE', *, *, #23916, .F. ) ;
#16980 = PLANE ( 'NONE',  #66497 ) ;
#16981 = CARTESIAN_POINT ( 'NONE',  ( 8.523814158775000038, 4.920236664407999783, -6.448229650796999834 ) ) ;
#16982 = CARTESIAN_POINT ( 'NONE',  ( 24.96658174203486169, 8.756202942073826989, -7.455126426642118886 ) ) ;
#16983 = DIRECTION ( 'NONE',  ( 1.000000000000000000, 0.000000000000000000, 0.000000000000000000 ) ) ;
#16984 = CIRCLE ( 'NONE', #56076, 0.4999999999999997224 ) ;
#16985 = CARTESIAN_POINT ( 'NONE',  ( 0.3293854016218999980, 3.323048643578999872, -0.5818070024050000510 ) ) ;
#16986 = ADVANCED_FACE ( 'NONE', ( #21228 ), #68418, .F. ) ;
#16987 = CARTESIAN_POINT ( 'NONE',  ( 10.52435971519499880, 4.532462039660099862, 8.385788382729799650 ) ) ;
#16988 = CARTESIAN_POINT ( 'NONE',  ( 3.076885484853999930, 3.060286776641000017, 2.182434864853000089 ) ) ;
#16989 = ORIENTED_EDGE ( 'NONE', *, *, #25252, .F. ) ;
#16990 = B_SPLINE_CURVE_WITH_KNOTS ( 'NONE', 3,
 ( #3260, #57084, #36106, #24590, #56756, #45912, #46946, #8852, #67224, #19337, #30189, #61993, #62667, #24928, #14787, #57422, #9527, #30870, #68251, #12556 ),
 .UNSPECIFIED., .F., .F.,
 ( 4, 2, 2, 2, 2, 2, 2, 2, 2, 4 ),
 ( 0.5011597829075521426, 0.5050569721035867987, 0.5089541612996214548, 0.5167485396916908780, 0.5323372964758295023, 0.5635148100441073060, 0.5946923236123851098, 0.6258698371806629135, 0.7505798914537751276, 1.000000000000000000 ),
 .UNSPECIFIED. ) ;
#16991 = B_SPLINE_CURVE_WITH_KNOTS ( 'NONE', 3,
 ( #12791, #39017, #65569, #18040, #6842, #1603, #48809, #61025, #23614, #13142 ),
 .UNSPECIFIED., .F., .F.,
 ( 4, 2, 2, 2, 4 ),
 ( 0.000000000000000000, 0.2500000000000001665, 0.5000000000000003331, 0.7500000000000001110, 1.000000000000000000 ),
 .UNSPECIFIED. ) ;
#16992 = CARTESIAN_POINT ( 'NONE',  ( 12.16000645811906544, 0.3284204639250600799, -12.59572022474404740 ) ) ;
#16993 = CARTESIAN_POINT ( 'NONE',  ( 20.10000000000000142, 0.000000000000000000, 0.000000000000000000 ) ) ;
#16994 = CARTESIAN_POINT ( 'NONE',  ( 18.18412234634028479, 2.838955764657549175, -12.27602435542071824 ) ) ;
#16995 = EDGE_CURVE ( 'NONE', #41132, #35889, #15604, .T. ) ;
#16996 = DIRECTION ( 'NONE',  ( 0.000000000000000000, -0.9617682489148012825, 0.2738646296610005582 ) ) ;
#16997 = CARTESIAN_POINT ( 'NONE',  ( 8.052732780410000402, 4.968147183437999992, 5.971792472497999604 ) ) ;
#16998 = ORIENTED_EDGE ( 'NONE', *, *, #20827, .F. ) ;
#16999 = CARTESIAN_POINT ( 'NONE',  ( 6.183730561998000752, -0.04522467425096000221, -1.614091090670999984 ) ) ;
#17000 = CARTESIAN_POINT ( 'NONE',  ( 8.444220280407998658, 5.223492654083000453, -6.524203877525000195 ) ) ;
#17002 = CARTESIAN_POINT ( 'NONE',  ( 10.88314899746000108, 5.167567567567999731, 6.822293592207000934 ) ) ;
#17001 = CARTESIAN_POINT ( 'NONE',  ( 8.390259216738563453, -2.723240919514677838, 8.682674612182450957 ) ) ;
#17003 = CARTESIAN_POINT ( 'NONE',  ( 11.72001955192552280, -12.39031618367880938, -1.831854259321207490 ) ) ;
#17004 = ORIENTED_EDGE ( 'NONE', *, *, #64541, .F. ) ;
#17005 = CARTESIAN_POINT ( 'NONE',  ( 16.43986884071599874, -3.414349888938000177, -11.89720686373000191 ) ) ;
#17006 = CARTESIAN_POINT ( 'NONE',  ( 11.44750515593000095, 11.62256912479000093, 1.379235499629000161 ) ) ;
#17007 = VERTEX_POINT ( 'NONE', #10733 ) ;
#17008 = CARTESIAN_POINT ( 'NONE',  ( 12.70915608521899465, 1.765590719831859223, -12.47568749010001632 ) ) ;
#17009 = CARTESIAN_POINT ( 'NONE',  ( 16.44004776902900034, 3.254301421112999915, 11.33671678219000079 ) ) ;
#17010 = CARTESIAN_POINT ( 'NONE',  ( 18.17005425344203928, 0.1118032413084525528, -13.89939982891984904 ) ) ;
#17011 = ORIENTED_EDGE ( 'NONE', *, *, #10001, .F. ) ;
#17012 = CARTESIAN_POINT ( 'NONE',  ( 10.48121855676791903, -3.643715756357204683, -9.239801132892552005 ) ) ;
#17013 = CARTESIAN_POINT ( 'NONE',  ( 7.197921422182000484, 8.271573195358998376, 4.408111321959999884 ) ) ;
#17014 = CARTESIAN_POINT ( 'NONE',  ( 11.36056039236529891, 4.891071240644300211, -7.543366519014379712 ) ) ;
#17015 = CARTESIAN_POINT ( 'NONE',  ( 8.174990947233153449, 2.650692654198087972, 7.500004443805798005 ) ) ;
#17016 = CARTESIAN_POINT ( 'NONE',  ( 11.26426088462129904, -3.997280690308189666, 8.778009775371000245 ) ) ;
#17017 = ORIENTED_EDGE ( 'NONE', *, *, #49352, .F. ) ;
#17018 = CARTESIAN_POINT ( 'NONE',  ( 8.320864158774000430, 3.894644548817000285, 6.044465307984999924 ) ) ;
#17019 = CARTESIAN_POINT ( 'NONE',  ( 10.53521345716899837, 4.924890298941200228, -8.340879262988799780 ) ) ;
#17020 = ORIENTED_EDGE ( 'NONE', *, *, #62182, .F. ) ;
#17021 = CARTESIAN_POINT ( 'NONE',  ( 10.01059687351666661, -3.370476274536376771, 6.407767014557176566 ) ) ;
#17022 = VECTOR ( 'NONE', #17527, 1000.000000000000000 ) ;
#17023 = CARTESIAN_POINT ( 'NONE',  ( 18.90826270587400160, 0.000000000000000000, 0.000000000000000000 ) ) ;
#17024 = CARTESIAN_POINT ( 'NONE',  ( 11.07206066007000089, 5.780045616399000608, -5.100130972279999675 ) ) ;
#17025 = ORIENTED_EDGE ( 'NONE', *, *, #24455, .F. ) ;
#17026 = CARTESIAN_POINT ( 'NONE',  ( 12.49819407809065908, -1.955416873541954592, -12.56189665940130062 ) ) ;
#17027 = CARTESIAN_POINT ( 'NONE',  ( 10.70851354018270030, 4.163624617374472869, -6.250000000000001776 ) ) ;
#17028 = CARTESIAN_POINT ( 'NONE',  ( 7.689997165042062655, 3.420006650669772608, -5.735732650232894692 ) ) ;
#17029 = CARTESIAN_POINT ( 'NONE',  ( 7.000000000000000000, -0.2392304845412999981, 3.000000000000000000 ) ) ;
#17030 = CARTESIAN_POINT ( 'NONE',  ( 12.43994760172713754, -1.886699913279273444, -13.87229234465171679 ) ) ;
#17031 = CARTESIAN_POINT ( 'NONE',  ( 11.40841235500449891, -4.841138636481000290, -6.729431436870699557 ) ) ;
#17032 = CARTESIAN_POINT ( 'NONE',  ( 10.47145237372899906, 4.043732047787757189, 6.225919055146349912 ) ) ;
#17034 = EDGE_CURVE ( 'NONE', #65121, #69025, #64327, .T. ) ;
#17033 = CARTESIAN_POINT ( 'NONE',  ( 17.84655355976684632, -1.821424963963782506, 12.46765546240475508 ) ) ;
#17035 = EDGE_LOOP ( 'NONE', ( #6602, #2614, #55867, #14561, #16295, #58977 ) ) ;
#17036 = CARTESIAN_POINT ( 'NONE',  ( 11.05946005378019947, -2.963614890480000152, -6.946587256304699309 ) ) ;
#17037 = ORIENTED_EDGE ( 'NONE', *, *, #46879, .F. ) ;
#17038 = VECTOR ( 'NONE', #16573, 1000.000000000000000 ) ;
#17039 = CARTESIAN_POINT ( 'NONE',  ( 25.39938977705818957, 2.782691790074335092, -11.32464129750441373 ) ) ;
#17040 = CARTESIAN_POINT ( 'NONE',  ( 9.585279719593998493, 2.928319778732999978, -8.861178115809998701 ) ) ;
#17041 = CARTESIAN_POINT ( 'NONE',  ( 5.002606837613999602, -0.4199405305951999789, 1.440017343911000003 ) ) ;
#17042 = CARTESIAN_POINT ( 'NONE',  ( 10.73506343560000076, -5.202499304193000107, -8.441414596927000247 ) ) ;
#17043 = CARTESIAN_POINT ( 'NONE',  ( 20.00000000000000000, 11.79499999999999993, 0.000000000000000000 ) ) ;
#17044 = CARTESIAN_POINT ( 'NONE',  ( 8.883148997460001084, -5.167567567567999731, 6.822293592207000934 ) ) ;
#17045 = CARTESIAN_POINT ( 'NONE',  ( 10.26947109217999810, -5.100000000000000533, -6.152188490330000370 ) ) ;
#17046 = ORIENTED_EDGE ( 'NONE', *, *, #67881, .F. ) ;
#17047 = CARTESIAN_POINT ( 'NONE',  ( 10.07314899745999881, 5.167567567567999731, -6.822293592207000934 ) ) ;
#17048 = CARTESIAN_POINT ( 'NONE',  ( 11.02286749330999882, 2.398743616553999924, 6.352468982205000891 ) ) ;
#17049 = DIRECTION ( 'NONE',  ( 0.000000000000000000, 1.000000000000000000, 0.000000000000000000 ) ) ;
#17050 = EDGE_CURVE ( 'NONE', #30347, #7557, #55191, .T. ) ;
#17051 = CARTESIAN_POINT ( 'NONE',  ( 12.06322412107030928, -3.945399343424460525, 8.532060764998998792 ) ) ;
#17052 = CARTESIAN_POINT ( 'NONE',  ( 18.05609597790000009, 3.343430715100999873, -11.12052764821000039 ) ) ;
#17053 = CARTESIAN_POINT ( 'NONE',  ( 10.38287885159599888, 4.860099138268600072, -7.397393329751199786 ) ) ;
#17054 = CARTESIAN_POINT ( 'NONE',  ( 24.45625562770040773, -12.38367834655976907, -3.108174973275622310 ) ) ;
#17055 = CARTESIAN_POINT ( 'NONE',  ( 24.32839125186500340, -9.022429054383998448, -9.339811860416999068 ) ) ;
#17056 = CARTESIAN_POINT ( 'NONE',  ( 11.09378572506000005, 2.399999999999999911, 6.571291218949999902 ) ) ;
#17057 = B_SPLINE_CURVE_WITH_KNOTS ( 'NONE', 3,
 ( #49180, #27173, #1291, #17724, #22604, #12127, #48496, #11421, #43948, #26832, #253, #65252, #58634, #54771 ),
 .UNSPECIFIED., .F., .F.,
 ( 4, 2, 2, 2, 2, 2, 4 ),
 ( 0.000000000000000000, 0.1250000000000005274, 0.2500000000000010547, 0.5000000000000021094, 0.6250000000000014433, 0.7500000000000006661, 1.000000000000000000 ),
 .UNSPECIFIED. ) ;
#17058 = LINE ( 'NONE', #48890, #55619 ) ;
#17059 = B_SPLINE_SURFACE_WITH_KNOTS ( 'NONE', 3, 3, ( 
 ( #55688, #50785, #7785, #29125, #39955, #7432, #28783, #13725, #17937, #39601, #39256, #60581, #33673, #60237, #8476, #18282, #23514, #28429, #24203 ),
 ( #50094, #35054, #12340, #18625, #2203, #1852, #60925, #12686, #18965, #40291, #44856, #19300, #23170, #51125, #13039, #3227, #44519, #34369, #2880 ),
 ( #2534, #65812, #34021, #23862, #55336, #66163, #66504, #13389, #34711, #45545, #56023, #66851, #10188, #68212, #67877, #9489, #68557, #41659, #46568 ),
 ( #62963, #3899, #31518, #62626, #14751, #4586, #57049, #14416, #9150, #15091, #47600, #52490, #20331, #36764, #58085, #46910, #14070, #35394, #36415 ) ),
 .UNSPECIFIED., .F., .F., .F.,
 ( 4, 4 ),
 ( 4, 1, 1, 1, 1, 1, 1, 1, 1, 1, 1, 1, 1, 1, 1, 1, 4 ),
 ( -0.1039086239011999951, 1.103908623900999864 ),
 ( -0.008849010032007000384, 0.01991027257200999809, 0.04866955517603999831, 0.07742883778006000306, 0.1061881203840999988, 0.1349474029881000126, 0.1637066855920999986, 0.1924659681960999846, 0.2212252508002000018, 0.2499845334042000156, 0.2787438160081999738, 0.3075030986121999876, 0.3362623812162000014, 0.3650216638202999908, 0.3937809464243000046, 0.4225402290282999629, 0.4512995116322999767 ),
 .UNSPECIFIED. ) ;
#17060 = VERTEX_POINT ( 'NONE', #4793 ) ;
#17061 = CARTESIAN_POINT ( 'NONE',  ( 8.722235841230000730, 3.844886277615000125, -8.888911790991000927 ) ) ;
#17062 = CARTESIAN_POINT ( 'NONE',  ( 6.928451469095000093, -1.283620250890999959, 0.4753010861453000335 ) ) ;
#17063 = CARTESIAN_POINT ( 'NONE',  ( 18.11274618065387898, 2.217676902473667333, 13.72925005197110870 ) ) ;
#17064 = CARTESIAN_POINT ( 'NONE',  ( 12.99999999998900080, -12.39025855408000076, -1.832244667012999928 ) ) ;
#17065 = CARTESIAN_POINT ( 'NONE',  ( 11.45348876160960039, -4.885820101980599794, -8.421216112044099589 ) ) ;
#17066 = ORIENTED_EDGE ( 'NONE', *, *, #46591, .F. ) ;
#17067 = CIRCLE ( 'NONE', #55012, 1.800000000000000044 ) ;
#17068 = CARTESIAN_POINT ( 'NONE',  ( 10.64831157502426429, -4.679757719901565416, -8.679446014678198651 ) ) ;
#17069 = CARTESIAN_POINT ( 'NONE',  ( 7.860170280410000210, 2.263558315407000254, 8.007442119518000112 ) ) ;
#17071 = CARTESIAN_POINT ( 'NONE',  ( 4.933367189779430895, -2.033301450227492424, 8.777104316792798490E-10 ) ) ;
#17070 = CARTESIAN_POINT ( 'NONE',  ( 9.848670280409999478, 5.002683760508999988, -8.912673867568997821 ) ) ;
#17072 = CARTESIAN_POINT ( 'NONE',  ( 6.999999691988000095, 11.00717859340000082, 1.432487142323000118 ) ) ;
#17073 = ORIENTED_EDGE ( 'NONE', *, *, #37169, .T. ) ;
#17074 = CARTESIAN_POINT ( 'NONE',  ( 9.966324641169999055, 2.303991951421000106, 6.575630951545000435 ) ) ;
#17075 = CARTESIAN_POINT ( 'NONE',  ( 18.24173484165870818, -2.753291453986189463, -13.72661349255300500 ) ) ;
#17076 = CARTESIAN_POINT ( 'NONE',  ( 11.14179841651039915, 3.646693590264900031, 6.560784671286499226 ) ) ;
#17077 = ADVANCED_FACE ( 'NONE', ( #20541 ), #15300, .T. ) ;
#17078 = CARTESIAN_POINT ( 'NONE',  ( 9.442085454646999665, -4.742494605615999781, 8.809986937145000141 ) ) ;
#17079 = CARTESIAN_POINT ( 'NONE',  ( 8.500493705215999896, 2.902642539927001941, 6.605602875546000341 ) ) ;
#17080 = ORIENTED_EDGE ( 'NONE', *, *, #14019, .T. ) ;
#17081 = CARTESIAN_POINT ( 'NONE',  ( 11.09999999999999964, 5.299999999254000116, 5.148510364898998937 ) ) ;
#17083 = CARTESIAN_POINT ( 'NONE',  ( 10.78888064679000003, -2.675723359162999859, -6.748225798259000818 ) ) ;
#17082 = CARTESIAN_POINT ( 'NONE',  ( 12.82792991967100171, -11.81434786598999942, 3.324782598720999793 ) ) ;
#17084 = CARTESIAN_POINT ( 'NONE',  ( 7.898220110652619752, -2.603757854786413972, 8.536907500157953521 ) ) ;
#17085 = CIRCLE ( 'NONE', #36063, 0.7500000000000000000 ) ;
#17086 = CARTESIAN_POINT ( 'NONE',  ( 9.691080333872001518, -5.335644368206000188, 8.701217921043999937 ) ) ;
#17087 = CYLINDRICAL_SURFACE ( 'NONE', #38785, 1.350000000000000089 ) ;
#17088 = ORIENTED_EDGE ( 'NONE', *, *, #50129, .F. ) ;
#17089 = CARTESIAN_POINT ( 'NONE',  ( 24.14319173801533935, -9.149649622521751624, 9.124492735417254252 ) ) ;
#17090 = CARTESIAN_POINT ( 'NONE',  ( 10.78026357027499849, -3.014700852776899698, 7.309904858193100097 ) ) ;
#17091 = CARTESIAN_POINT ( 'NONE',  ( 7.911791375976998886, 3.505433841991000499, 6.324291089890995643 ) ) ;
#17092 = CARTESIAN_POINT ( 'NONE',  ( 10.37457053952199892, 3.551693493661699730, 8.548957288282998945 ) ) ;
#17093 = VECTOR ( 'NONE', #12583, 1000.000000000000000 ) ;
#17094 = ORIENTED_EDGE ( 'NONE', *, *, #45869, .F. ) ;
#17095 = CARTESIAN_POINT ( 'NONE',  ( 8.871889158775999817, 2.702406276695999754, -6.981052078638000147 ) ) ;
#17096 = CARTESIAN_POINT ( 'NONE',  ( 23.62003806996300170, 13.19646996404000028, -4.177448498581999736 ) ) ;
#17097 = CARTESIAN_POINT ( 'NONE',  ( 12.22799143493887897, 2.916631933635859486, -12.25779765684317191 ) ) ;
#17098 = CARTESIAN_POINT ( 'NONE',  ( 11.18035971519489813, -3.321859513918399731, 8.628134814664999652 ) ) ;
#17099 = B_SPLINE_CURVE_WITH_KNOTS ( 'NONE', 3,
 ( #11423, #37655, #42562, #601, #37996, #63870, #17013, #32764 ),
 .UNSPECIFIED., .F., .F.,
 ( 4, 1, 1, 1, 1, 4 ),
 ( 0.000000000000000000, 0.2000000000000000111, 0.4000000000000000222, 0.5999999999999999778, 0.8000000000000000444, 1.000000000000000000 ),
 .UNSPECIFIED. ) ;
#17100 = ORIENTED_EDGE ( 'NONE', *, *, #7679, .F. ) ;
#17101 = CARTESIAN_POINT ( 'NONE',  ( 10.14393020684899938, -2.750000000000000000, -7.500000000000000000 ) ) ;
#17102 = CARTESIAN_POINT ( 'NONE',  ( 24.30000000000000071, 0.000000000000000000, 0.000000000000000000 ) ) ;
#17103 = ORIENTED_EDGE ( 'NONE', *, *, #54129, .T. ) ;
#17104 = CARTESIAN_POINT ( 'NONE',  ( 9.566483607044000692, -4.108965473266000146, 8.851626696081998702 ) ) ;
#17105 = CARTESIAN_POINT ( 'NONE',  ( 23.91429184840559685, 9.509214059390449947, 9.346071062481517089 ) ) ;
#17106 = ORIENTED_EDGE ( 'NONE', *, *, #41377, .T. ) ;
#17107 = CARTESIAN_POINT ( 'NONE',  ( 9.510596873516666605, 4.629523725463622341, 6.407767014557176566 ) ) ;
#17108 = CARTESIAN_POINT ( 'NONE',  ( 11.36333594839950045, 4.659759757475400832, 8.256087240512899328 ) ) ;
#17109 = CARTESIAN_POINT ( 'NONE',  ( 10.17284693385832206, 4.293232846717514484, -8.835933254752031729 ) ) ;
#17110 = CARTESIAN_POINT ( 'NONE',  ( 11.12983972340999905, 2.716185796578999945, -4.845726974617000415 ) ) ;
#17111 = CARTESIAN_POINT ( 'NONE',  ( 18.19494255922599990, -11.55196140944999961, 4.440362831676999633 ) ) ;
#17112 = CARTESIAN_POINT ( 'NONE',  ( 11.09999999999999964, 5.350000000000000533, 7.500000000000000000 ) ) ;
#17113 = CARTESIAN_POINT ( 'NONE',  ( 13.67476513888300005, 9.526862765824999357, 8.046751417967000108 ) ) ;
#17114 = CARTESIAN_POINT ( 'NONE',  ( 18.15872281507842700, 0.1622035078961276411, -12.69861136640060195 ) ) ;
#17115 = CARTESIAN_POINT ( 'NONE',  ( 12.22440656764569056, 2.731388741921196850, -12.39466681324993225 ) ) ;
#17116 = CARTESIAN_POINT ( 'NONE',  ( 10.13662282008599824, -3.405288783432600219, -8.459250300176799797 ) ) ;
#17117 = EDGE_CURVE ( 'NONE', #13349, #25042, #78, .T. ) ;
#17119 = EDGE_CURVE ( 'NONE', #43628, #27393, #18997, .T. ) ;
#17118 = CARTESIAN_POINT ( 'NONE',  ( 8.289114158772999730, 4.310355144869000732, 9.459505265942000918 ) ) ;
#17120 = ORIENTED_EDGE ( 'NONE', *, *, #18314, .T. ) ;
#17121 = VECTOR ( 'NONE', #21495, 1000.000000000000114 ) ;
#17122 = AXIS2_PLACEMENT_3D ( 'NONE', #41917, #42608, #63226 ) ;
#17123 = CARTESIAN_POINT ( 'NONE',  ( 23.89320776801300283, -12.21745654473000542, 3.256241354580001524 ) ) ;
#17124 = CARTESIAN_POINT ( 'NONE',  ( 7.163103445601981534, 3.030767263943030976, 8.474512546327412466 ) ) ;
#17125 = CARTESIAN_POINT ( 'NONE',  ( 16.39999999270239428, 3.259293166955308685, 11.55581727975966544 ) ) ;
#17126 = CARTESIAN_POINT ( 'NONE',  ( 18.05422494319413929, 1.958382419481330627, 12.44687927882536549 ) ) ;
#17127 = DIRECTION ( 'NONE',  ( 1.000000000000000000, 0.000000000000000000, 0.000000000000000000 ) ) ;
#17129 = CARTESIAN_POINT ( 'NONE',  ( 11.01668711954999935, 7.361592993461999690, 6.178312432500000284 ) ) ;
#17128 = B_SPLINE_CURVE_WITH_KNOTS ( 'NONE', 3,
 ( #49722, #54622, #445, #10937 ),
 .UNSPECIFIED., .F., .F.,
 ( 4, 4 ),
 ( 0.000000000000000000, 1.000000000000000000 ),
 .UNSPECIFIED. ) ;
#17130 = CARTESIAN_POINT ( 'NONE',  ( 10.20815392832262702, -4.380187932396833794, 6.711971190259613529 ) ) ;
#17131 = CARTESIAN_POINT ( 'NONE',  ( 9.957462135714001406, -5.100000000000000533, -6.571291218949999902 ) ) ;
#17132 = EDGE_LOOP ( 'NONE', ( #17163, #53582, #14120, #30196 ) ) ;
#17133 = CARTESIAN_POINT ( 'NONE',  ( 12.18817755169816053, -2.859236737590006516, 12.27131451573979248 ) ) ;
#17134 = CARTESIAN_POINT ( 'NONE',  ( 9.327747021775998348, -4.858221690000700477, -8.253120162257399528 ) ) ;
#17135 = CARTESIAN_POINT ( 'NONE',  ( 24.62773497368900166, -3.462213745051000213, -12.08749688049000071 ) ) ;
#17136 = EDGE_CURVE ( 'NONE', #30347, #44476, #5565, .T. ) ;
#17137 = CARTESIAN_POINT ( 'NONE',  ( 9.447848023450999833, -5.447470167531999863, 7.431328114251999573 ) ) ;
#17138 = EDGE_CURVE ( 'NONE', #35342, #54502, #62605, .T. ) ;
#17139 = CARTESIAN_POINT ( 'NONE',  ( 10.69872335273220010, 4.349306362047499874, -8.440710326446700051 ) ) ;
#17140 = CARTESIAN_POINT ( 'NONE',  ( 12.38211335778635735, -0.5846869236304570450, 12.58643362292763612 ) ) ;
#17141 = AXIS2_PLACEMENT_3D ( 'NONE', #35049, #35389, #3892 ) ;
#17142 = CARTESIAN_POINT ( 'NONE',  ( 8.983795280412000039, 3.979464555644999901, 9.134076336209998814 ) ) ;
#17143 = CARTESIAN_POINT ( 'NONE',  ( 9.471374412057000924, 2.030666183831999927, 7.549764512038000142 ) ) ;
#17144 = CARTESIAN_POINT ( 'NONE',  ( 12.63203184702126691, 3.100663238843660352, 12.29110965694881941 ) ) ;
#17145 = ORIENTED_EDGE ( 'NONE', *, *, #31882, .F. ) ;
#17146 = DIRECTION ( 'NONE',  ( -1.000000000000000000, 0.000000000000000000, 0.000000000000000000 ) ) ;
#17147 = CARTESIAN_POINT ( 'NONE',  ( 11.11302897915239818, 4.291996373817799970, -8.602736702002999891 ) ) ;
#17148 = CARTESIAN_POINT ( 'NONE',  ( 17.82167905068868308, -0.6689867242971705430, 12.58222862546947241 ) ) ;
#17149 = CARTESIAN_POINT ( 'NONE',  ( 11.09999999999999964, -5.299999999999999822, 5.160242713806000303 ) ) ;
#17151 = CARTESIAN_POINT ( 'NONE',  ( 17.82907313211138600, -0.5620966109762222107, 12.68325743355232582 ) ) ;
#17150 = CARTESIAN_POINT ( 'NONE',  ( 8.251334741087001490, 4.957169262993001091, 6.172567036706003485 ) ) ;
#17152 = CARTESIAN_POINT ( 'NONE',  ( 10.65364694612719809, -4.804498860841600383, -7.821061011719899980 ) ) ;
#17153 = LINE ( 'NONE', #59808, #55361 ) ;
#17154 = VERTEX_POINT ( 'NONE', #34146 ) ;
#17155 = CARTESIAN_POINT ( 'NONE',  ( 1.548656882336000074, -2.727979478513999911, -1.783091295463999915 ) ) ;
#17156 = CARTESIAN_POINT ( 'NONE',  ( 7.100000000000000533, 0.000000000000000000, 0.000000000000000000 ) ) ;
#17157 = CARTESIAN_POINT ( 'NONE',  ( 18.28019316479310774, -0.1878083608821064232, -12.60000737103649016 ) ) ;
#17158 = CARTESIAN_POINT ( 'NONE',  ( 17.65323508308281930, 1.760912828005752884, -12.47634505842159847 ) ) ;
#17159 = CARTESIAN_POINT ( 'NONE',  ( 12.22680470609052961, -2.076949241994384465, 13.84509419021260079 ) ) ;
#17160 = CARTESIAN_POINT ( 'NONE',  ( 20.00000000000000000, -11.79499999999999993, 0.000000000000000000 ) ) ;
#17161 = CARTESIAN_POINT ( 'NONE',  ( 24.15344905084700144, 3.593700277778999919, -12.72454352958999912 ) ) ;
#17162 = CARTESIAN_POINT ( 'NONE',  ( 13.43043922992600159, -12.41458792447999926, -1.928118222792999825 ) ) ;
#17163 = ORIENTED_EDGE ( 'NONE', *, *, #53955, .F. ) ;
#17164 = VECTOR ( 'NONE', #2282, 1000.000000000000114 ) ;
#17165 = CARTESIAN_POINT ( 'NONE',  ( 12.10941541367886209, 11.07487266647606816, -3.615341446703132622 ) ) ;
#17166 = CYLINDRICAL_SURFACE ( 'NONE', #24090, 1.350000000000000089 ) ;
#17167 = VECTOR ( 'NONE', #26255, 1000.000000000000114 ) ;
#17168 = CARTESIAN_POINT ( 'NONE',  ( 17.80000000001300009, -3.351264566333000072, -11.15757590352999884 ) ) ;
#17169 = CARTESIAN_POINT ( 'NONE',  ( 0.7991554384871001337, -3.621562729233000599, -1.006310721376000084 ) ) ;
#17170 = DIRECTION ( 'NONE',  ( 1.000000000000000000, 0.000000000000000000, 5.031225091942999521E-14 ) ) ;
#17171 = CARTESIAN_POINT ( 'NONE',  ( 18.02490773331091134, -11.46571851143742826, 4.499230601365909799 ) ) ;
#17172 = CARTESIAN_POINT ( 'NONE',  ( 9.758504216683469679, -3.836370129433865017, 8.749972943975897977 ) ) ;
#17173 = CARTESIAN_POINT ( 'NONE',  ( 10.50595525820100029, 3.918212119278319694, 8.362327856951900173 ) ) ;
#17174 = ADVANCED_FACE ( 'NONE', ( #23305 ), #59318, .T. ) ;
#17175 = EDGE_CURVE ( 'NONE', #26690, #8994, #50114, .T. ) ;
#17176 = B_SPLINE_CURVE_WITH_KNOTS ( 'NONE', 3,
 ( #35698, #3860, #34329, #18588, #51087, #18242, #39563, #13003, #55648, #50399 ),
 .UNSPECIFIED., .F., .F.,
 ( 4, 2, 2, 2, 4 ),
 ( 0.000000000000000000, 0.1477786706793876581, 0.2216680060190820700, 0.2586126736889285960, 0.2955573413587750942 ),
 .UNSPECIFIED. ) ;
#17177 = DIRECTION ( 'NONE',  ( -0.000000000000000000, 0.7507612787780010288, 0.6605736161001442008 ) ) ;
#17178 = CARTESIAN_POINT ( 'NONE',  ( 10.43325685320999874, -5.596199512734999715, -8.042023143828998855 ) ) ;
#17179 = CARTESIAN_POINT ( 'NONE',  ( 12.35751123582549127, 3.100314578113210207, 13.65257769756134820 ) ) ;
#17180 = CARTESIAN_POINT ( 'NONE',  ( 9.617147628285000138, -2.491831134779999957, -6.388915175267000812 ) ) ;
#17181 = LINE ( 'NONE', #23472, #56711 ) ;
#17182 = CARTESIAN_POINT ( 'NONE',  ( 9.421209229099421378, 5.348866595988766015, 7.442183899411809911 ) ) ;
#17183 = EDGE_LOOP ( 'NONE', ( #26998, #64931, #53816, #59598, #15812, #3875, #693, #15099, #54259, #58499, #26313, #22851, #49679, #36637, #20756, #63954, #29203, #12802, #13112, #24910 ) ) ;
#17185 = CARTESIAN_POINT ( 'NONE',  ( 11.09999999999999964, -5.299999999999999822, 5.160242713806000303 ) ) ;
#17184 = B_SPLINE_CURVE_WITH_KNOTS ( 'NONE', 3,
 ( #47134, #57608, #56931, #67406 ),
 .UNSPECIFIED., .F., .F.,
 ( 4, 4 ),
 ( 0.000000000000000000, 1.000000000000000000 ),
 .UNSPECIFIED. ) ;
#17186 = ORIENTED_EDGE ( 'NONE', *, *, #66755, .T. ) ;
#17187 = CARTESIAN_POINT ( 'NONE',  ( 18.15894044208802427, -2.662322226546016690, 13.63771003692132844 ) ) ;
#17188 = CARTESIAN_POINT ( 'NONE',  ( 10.56733863405299800, -3.211524470605299886, -8.505794571537999005 ) ) ;
#17189 = ORIENTED_EDGE ( 'NONE', *, *, #20354, .F. ) ;
#17190 = CARTESIAN_POINT ( 'NONE',  ( 11.44366954483529852, 4.485203148598100320, 8.248643701125299543 ) ) ;
#17191 = CARTESIAN_POINT ( 'NONE',  ( 5.485952324345468867, 0.4288768802937203417, -1.048267794080263604 ) ) ;
#17193 = LINE ( 'NONE', #42738, #16581 ) ;
#17192 = CIRCLE ( 'NONE', #56284, 5.000000000000000000 ) ;
#17194 = CARTESIAN_POINT ( 'NONE',  ( 8.621524209948782769, -3.647212272540656830, 8.851469415033186294 ) ) ;
#17195 = CARTESIAN_POINT ( 'NONE',  ( 7.307500000000000107, -0.2999999999999999889, -3.149999999999999911 ) ) ;
#17196 = CARTESIAN_POINT ( 'NONE',  ( 10.75851354018278982, -3.836375382625526687, 8.749999999999996447 ) ) ;
#17197 = CARTESIAN_POINT ( 'NONE',  ( 17.81057016328025000, 0.6732419856523146340, -12.58200148172923782 ) ) ;
#17198 = B_SPLINE_CURVE_WITH_KNOTS ( 'NONE', 3,
 ( #9221, #57121, #39681, #35472, #30561, #55764, #56794, #34787, #7866, #50511, #51536, #2612, #23944, #45276 ),
 .UNSPECIFIED., .F., .F.,
 ( 4, 2, 2, 2, 2, 2, 4 ),
 ( 0.000000000000000000, 0.2492980987599822951, 0.3739471481399732067, 0.4051094104849721211, 0.4362716728299709801, 0.4674339351749699500, 0.4985961975199688090 ),
 .UNSPECIFIED. ) ;
#17199 = CARTESIAN_POINT ( 'NONE',  ( 10.39355669675000016, -4.089958462238000081, -9.188182957628999503 ) ) ;
#17200 = AXIS2_PLACEMENT_3D ( 'NONE', #29596, #20109, #19768 ) ;
#17201 = CARTESIAN_POINT ( 'NONE',  ( 11.83518044953559922, -3.231951024059400268, -7.900497508315099893 ) ) ;
#17202 = ORIENTED_EDGE ( 'NONE', *, *, #23270, .F. ) ;
#17203 = EDGE_CURVE ( 'NONE', #19729, #13791, #39346, .T. ) ;
#17205 = EDGE_CURVE ( 'NONE', #15208, #38268, #12597, .T. ) ;
#17204 = CARTESIAN_POINT ( 'NONE',  ( 9.965360841230999966, 4.034680274230000308, -6.102912434217000026 ) ) ;
#17206 = VERTEX_POINT ( 'NONE', #17721 ) ;
#17207 = CARTESIAN_POINT ( 'NONE',  ( 10.75851354018298522, 4.163624617374472869, -6.250000000000000888 ) ) ;
#17208 = B_SPLINE_CURVE_WITH_KNOTS ( 'NONE', 3,
 ( #48159, #58644, #21576, #48504 ),
 .UNSPECIFIED., .F., .F.,
 ( 4, 4 ),
 ( 0.000000000000000000, 1.000000000000000000 ),
 .UNSPECIFIED. ) ;
#17209 =( LENGTH_UNIT ( ) NAMED_UNIT ( * ) SI_UNIT ( .MILLI., .METRE. ) );
#17210 = EDGE_CURVE ( 'NONE', #7298, #37494, #67678, .T. ) ;
#17211 = ORIENTED_EDGE ( 'NONE', *, *, #8629, .T. ) ;
#17212 = DIRECTION ( 'NONE',  ( 1.000000000000000000, 0.000000000000000000, 0.000000000000000000 ) ) ;
#17213 = LINE ( 'NONE', #38537, #30527 ) ;
#17214 = CARTESIAN_POINT ( 'NONE',  ( 25.21375942257175495, -8.515658397323806028, 8.063058284021709099 ) ) ;
#17215 = CARTESIAN_POINT ( 'NONE',  ( 10.11496314287999887, 5.251703735191999733, -7.236139910592400248 ) ) ;
#17216 = DIRECTION ( 'NONE',  ( -1.000000000000000000, 0.000000000000000000, 0.000000000000000000 ) ) ;
#17217 = B_SPLINE_SURFACE_WITH_KNOTS ( 'NONE', 3, 3, ( 
 ( #47452, #41514, #4440, #25433, #56909, #68409, #26126, #35926, #14943, #62149, #63163, #4784, #51656, #14267, #14608, #57239, #51993, #57941, #36268, #24751, #9691, #47110, #68758, #46766, #30349, #35595, #46076, #62824, #20530, #15292, #9006, #31376, #10037, #52688, #42214 ),
 ( #63519, #15633, #10381, #31719, #3752, #27161, #48482, #42549, #22249, #589, #48828, #11755, #5486, #17356, #69112, #53725, #37983, #21220, #5824, #64886, #60003, #64199, #26821, #33096, #42892, #12114, #63857, #16314, #48139, #937, #37641, #43585, #15971, #26473, #58972 ),
 ( #6513, #43236, #54413, #6161, #17000, #21898, #54064, #32410, #64542, #27502, #1277, #37300, #58622, #38329, #10723, #21556, #241, #59659, #53041, #11075, #32751, #16657, #27858, #43935, #59309, #32069, #38682, #49166, #11410, #53385, #22592, #65239, #5135, #47806, #8246 ),
 ( #18744, #2312, #39035, #1622, #54758, #13507, #34491, #44972, #12459, #50897, #2993, #29243, #49509, #45317, #65587, #33793, #7552, #66276, #55804, #66622, #39373, #40075, #23634, #6859, #22937, #56138, #1975, #18400, #17712, #61386, #66965, #50553, #34826, #28906, #55455 ) ),
 .UNSPECIFIED., .F., .F., .F.,
 ( 4, 4 ),
 ( 4, 1, 1, 1, 1, 1, 1, 1, 1, 1, 1, 1, 1, 1, 1, 1, 1, 1, 1, 1, 1, 1, 1, 1, 1, 1, 1, 1, 1, 1, 1, 1, 4 ),
 ( -0.1039370721279000015, 1.103937072127999963 ),
 ( -0.01999999999998999800, 0.01250000000001000137, 0.04499999999999999833, 0.07749999999999999944, 0.1100000000000000006, 0.1424999999999999878, 0.1749999999999999889, 0.2074999999999999900, 0.2399999999999999911, 0.2725000000000000200, 0.3049999999999999933, 0.3375000000000000222, 0.3699999999999999956, 0.4025000000000000244, 0.4349999999999999978, 0.4675000000000000266, 0.5000000000000000000, 0.5324999999999999734, 0.5649999999999999467, 0.5975000000000000311, 0.6300000000000000044, 0.6624999999999999778, 0.6949999999999999512, 0.7275000000000000355, 0.7600000000000000089, 0.7924999999999999822, 0.8249999999999999556, 0.8575000000000000400, 0.8900000000000000133, 0.9224999999999999867, 0.9549999999999999600, 0.9875000000000000444, 1.020000000000000018 ),
 .UNSPECIFIED. ) ;
#17218 = CARTESIAN_POINT ( 'NONE',  ( 9.514108112060000622, -4.887639888682999256, 8.462756667353000140 ) ) ;
#17219 = FACE_OUTER_BOUND ( 'NONE', #11373, .T. ) ;
#17220 = CARTESIAN_POINT ( 'NONE',  ( 12.18004362304668575, 0.009762789003246823832, 13.90000041479089532 ) ) ;
#17221 = ORIENTED_EDGE ( 'NONE', *, *, #54974, .T. ) ;
#17222 = CARTESIAN_POINT ( 'NONE',  ( 7.042728317542000127, 5.321245676936000812, -7.068438969505000280 ) ) ;
#17223 = CARTESIAN_POINT ( 'NONE',  ( 10.74549835728371150, 4.944659509662737484, -4.827072369406659291 ) ) ;
#17224 = CARTESIAN_POINT ( 'NONE',  ( 10.16407857760462718, 3.262163830883630489, 7.029755324101339298 ) ) ;
#17225 = CARTESIAN_POINT ( 'NONE',  ( 4.364220016632000210, -0.2958825345050999922, -1.301287971988999814 ) ) ;
#17226 = AXIS2_PLACEMENT_3D ( 'NONE', #65559, #61015, #17682 ) ;
#17227 = B_SPLINE_SURFACE_WITH_KNOTS ( 'NONE', 3, 3, ( 
 ( #63257, #36359, #53809, #21309 ),
 ( #4530, #63948, #58712, #10816 ),
 ( #47200, #57673, #32158, #31810 ),
 ( #48223, #10132, #330, #15384 ),
 ( #36712, #5909, #21644, #46856 ),
 ( #20279, #62913, #9781, #31132 ),
 ( #58032, #52783, #26219, #47548 ),
 ( #20971, #17797, #65327, #7296 ),
 ( #60439, #27249, #43675, #6948 ),
 ( #48917, #33877, #17446, #11845 ),
 ( #55194, #23028, #33530, #32840 ),
 ( #44377, #28637, #39461, #54849 ) ),
 .UNSPECIFIED., .F., .F., .F.,
 ( 4, 1, 1, 1, 1, 1, 1, 1, 1, 4 ),
 ( 4, 4 ),
 ( 0.01098173103564000115, 0.05000000000000000278, 0.1000000000000000056, 0.1499999999999999944, 0.2000000000000000111, 0.2500000000000000000, 0.2999999999999999889, 0.3499999999999999778, 0.4000000000000000222, 0.4470370502493000164 ),
 ( -0.2706693728835000146, 1.270788559091000192 ),
 .UNSPECIFIED. ) ;
#17228 = ADVANCED_FACE ( 'NONE', ( #12820 ), #32434, .F. ) ;
#17229 = CARTESIAN_POINT ( 'NONE',  ( 10.19741084123000086, 4.262870449202000422, -8.811513791423999820 ) ) ;
#17230 = CYLINDRICAL_SURFACE ( 'NONE', #38042, 0.9499999999999999556 ) ;
#17231 = CARTESIAN_POINT ( 'NONE',  ( 9.843620110012999191, -5.021680390140000227, -8.761463725090999688 ) ) ;
#17232 = VERTEX_POINT ( 'NONE', #46696 ) ;
#17233 = CARTESIAN_POINT ( 'NONE',  ( 9.564964385875493136, -5.350010280223940207, -7.500002129152480101 ) ) ;
#17234 = CARTESIAN_POINT ( 'NONE',  ( 8.199995110659001440, -2.894508759333000114, 6.645190873281999089 ) ) ;
#17235 = DIRECTION ( 'NONE',  ( 1.000000000000000000, -9.560371307181999538E-10, -1.449016008921000004E-09 ) ) ;
#17236 = CARTESIAN_POINT ( 'NONE',  ( 8.629140486159279533, -3.010722422556198818, -6.580811551485690636 ) ) ;
#17237 = DIRECTION ( 'NONE',  ( 1.000000000000000000, 0.000000000000000000, 0.000000000000000000 ) ) ;
#17238 = CARTESIAN_POINT ( 'NONE',  ( 24.37808884332112314, 12.29705478244968830, -3.189923896649337731 ) ) ;
#17239 = CARTESIAN_POINT ( 'NONE',  ( 10.47769598648999967, 5.009476315410999803, -8.101059042556599366 ) ) ;
#17240 = CARTESIAN_POINT ( 'NONE',  ( 8.900113844317997902, 4.253652595614200393, -6.528144732449299603 ) ) ;
#17242 = FACE_OUTER_BOUND ( 'NONE', #59087, .T. ) ;
#17241 = CARTESIAN_POINT ( 'NONE',  ( 10.15300081823900058, -4.767147064380999666, 7.096028062709999418 ) ) ;
#17243 = CIRCLE ( 'NONE', #2723, 2.149999999999999911 ) ;
#17244 = CARTESIAN_POINT ( 'NONE',  ( 9.406851002546000373, -2.832432432432000269, -6.822293592207000934 ) ) ;
#17245 = ORIENTED_EDGE ( 'NONE', *, *, #54400, .T. ) ;
#17246 = CARTESIAN_POINT ( 'NONE',  ( 11.59966954483535773, 4.638989336656000440, 8.485927942460499196 ) ) ;
#17247 = CARTESIAN_POINT ( 'NONE',  ( 7.575821720216998401, -3.529668843644999221, 6.549222992663997545 ) ) ;
#17248 = CARTESIAN_POINT ( 'NONE',  ( 10.26492546752099955, 2.860918852493000486, 7.578921399676699089 ) ) ;
#17249 = CARTESIAN_POINT ( 'NONE',  ( 4.599999999999999645, -0.6250000000000001110, 13.88107975066923494 ) ) ;
#17250 = CARTESIAN_POINT ( 'NONE',  ( 11.11845396862999991, -5.767021056207999763, 7.178419201465000121 ) ) ;
#17251 = DIRECTION ( 'NONE',  ( -1.000000000000000000, -1.776356839247999994E-14, 0.000000000000000000 ) ) ;
#17252 = CARTESIAN_POINT ( 'NONE',  ( 5.407309682995999900, -12.95251760905999916, -1.915207572622000143 ) ) ;
#17253 = APPLICATION_CONTEXT ( 'automotive_design' ) ;
#17254 = CARTESIAN_POINT ( 'NONE',  ( 9.077417874593999514, -4.924352284713100047, -7.892956936667999912 ) ) ;
#17255 = DIRECTION ( 'NONE',  ( 0.000000000000000000, -1.000000000000000000, 0.000000000000000000 ) ) ;
#17256 = CARTESIAN_POINT ( 'NONE',  ( 5.173974669483000888, -0.6654033835843000677, 1.142600628630999982 ) ) ;
#17257 = CARTESIAN_POINT ( 'NONE',  ( 6.999999999999999112, 6.725428974790256476, 3.045254342161083816 ) ) ;
#17258 = FACE_OUTER_BOUND ( 'NONE', #25732, .T. ) ;
#17259 = ADVANCED_FACE ( 'NONE', ( #61730 ), #11209, .T. ) ;
#17260 = EDGE_CURVE ( 'NONE', #22975, #7379, #37596, .T. ) ;
#17261 = CARTESIAN_POINT ( 'NONE',  ( 12.73299791870421060, 0.6209187240130102925, -12.67955909024710337 ) ) ;
#17262 = CARTESIAN_POINT ( 'NONE',  ( 10.89979975933730039, 4.819074589197400726, -7.218192605361100078 ) ) ;
#17263 = CARTESIAN_POINT ( 'NONE',  ( 12.27225454754552558, 2.172654780177386780, -13.73747135094945371 ) ) ;
#17264 = CARTESIAN_POINT ( 'NONE',  ( 24.67333001244800172, -8.700662965794998982, 9.017020110425999491 ) ) ;
#17265 = CARTESIAN_POINT ( 'NONE',  ( 0.9363901325418041433, 0.4581489286485155299, -3.499999999999999556 ) ) ;
#17266 = ORIENTED_EDGE ( 'NONE', *, *, #12756, .T. ) ;
#17267 = CARTESIAN_POINT ( 'NONE',  ( 7.725062132959652494, -2.650631715052233162, 7.500008390440855877 ) ) ;
#17268 = CARTESIAN_POINT ( 'NONE',  ( 12.15456646199063506, -0.3226776716457278593, -13.99628514671255886 ) ) ;
#17269 = CARTESIAN_POINT ( 'NONE',  ( 11.18923293495519822, -5.032672437899000428, -7.458486839450950256 ) ) ;
#17270 = CARTESIAN_POINT ( 'NONE',  ( 12.40000000000000213, -12.27510221496999954, -1.916289661941000144 ) ) ;
#17271 = CARTESIAN_POINT ( 'NONE',  ( 4.900006121741999898, -6.122517096885939548E-17, -1.999970730383187734 ) ) ;
#17272 = CARTESIAN_POINT ( 'NONE',  ( 0.1500002361980000143, 0.000000000000000000, 0.000000000000000000 ) ) ;
#17273 = CARTESIAN_POINT ( 'NONE',  ( 5.619239821441324167, 12.11503533077830319, -3.745341923021909381 ) ) ;
#17274 = ORIENTED_EDGE ( 'NONE', *, *, #5903, .F. ) ;
#17275 = VECTOR ( 'NONE', #66605, 1000.000000000000000 ) ;
#17276 = CARTESIAN_POINT ( 'NONE',  ( 25.59994555223700274, -10.55174472786000095, 3.754934689065000164 ) ) ;
#17277 = CARTESIAN_POINT ( 'NONE',  ( 17.60330540716445213, 3.246896514464374661, -13.61828436941213205 ) ) ;
#17278 = ORIENTED_EDGE ( 'NONE', *, *, #65815, .F. ) ;
#17279 = DIRECTION ( 'NONE',  ( 1.000000000000000000, 0.000000000000000000, 0.000000000000000000 ) ) ;
#17280 = CARTESIAN_POINT ( 'NONE',  ( 25.05006280129954277, 8.531455033317872250, -8.270352402647430878 ) ) ;
#17281 = CARTESIAN_POINT ( 'NONE',  ( 8.523814158775000038, 4.920236664407999783, -6.448229650796999834 ) ) ;
#17282 = CARTESIAN_POINT ( 'NONE',  ( 7.975339216757299177, -5.350090185752664595, 7.499980949462679014 ) ) ;
#17283 = CARTESIAN_POINT ( 'NONE',  ( 17.55505043854143565, 1.787816316115924842, -13.88537766212463254 ) ) ;
#17284 = CARTESIAN_POINT ( 'NONE',  ( 7.464485841224999696, 4.562063799276000253, -9.314837681783000534 ) ) ;
#17285 = DIRECTION ( 'NONE',  ( 0.000000000000000000, 0.9624505444715651947, -0.2714570858282905341 ) ) ;
#17286 = CARTESIAN_POINT ( 'NONE',  ( 11.01666666666868188, -3.382745367834177230, 8.852578401490447391 ) ) ;
#17287 = ORIENTED_EDGE ( 'NONE', *, *, #65698, .F. ) ;
#17288 = CARTESIAN_POINT ( 'NONE',  ( 9.944325809452999820, -5.443013936195000291, 7.367349259341000156 ) ) ;
#17289 = CARTESIAN_POINT ( 'NONE',  ( 1.700000000000000178, 0.000000000000000000, 0.000000000000000000 ) ) ;
#17290 = CARTESIAN_POINT ( 'NONE',  ( 17.55505043854143565, 1.875000000000000000, -25.00000000000000000 ) ) ;
#17291 = ORIENTED_EDGE ( 'NONE', *, *, #36782, .F. ) ;
#17292 = LINE ( 'NONE', #15909, #8032 ) ;
#17293 = CARTESIAN_POINT ( 'NONE',  ( 10.14521814679000045, -3.576528389491000048, -8.962725485696999783 ) ) ;
#17294 = EDGE_CURVE ( 'NONE', #58219, #30029, #21826, .T. ) ;
#17295 = B_SPLINE_CURVE_WITH_KNOTS ( 'NONE', 3,
 ( #19316, #54397, #24909, #51144 ),
 .UNSPECIFIED., .F., .F.,
 ( 4, 4 ),
 ( 0.000000000000000000, 1.000000000000000000 ),
 .UNSPECIFIED. ) ;
#17296 = ORIENTED_EDGE ( 'NONE', *, *, #26066, .F. ) ;
#17297 = CARTESIAN_POINT ( 'NONE',  ( 9.305380199233999505, 4.996570247675600207, 7.625259896924899472 ) ) ;
#17298 = CARTESIAN_POINT ( 'NONE',  ( 17.99911394258101183, -3.049496102151224797, -12.22541657636149282 ) ) ;
#17299 = CARTESIAN_POINT ( 'NONE',  ( 4.716442238856000557, 1.389484359140999992, -0.2752418227443999554 ) ) ;
#17300 = VECTOR ( 'NONE', #2174, 1000.000000000000114 ) ;
#17301 = CARTESIAN_POINT ( 'NONE',  ( 8.090553154006000725, 4.882634821118998047, -6.178046870599000151 ) ) ;
#17302 = CARTESIAN_POINT ( 'NONE',  ( 8.411640687506832137, 2.873222873817933731, -6.752018918866305341 ) ) ;
#17303 = DIRECTION ( 'NONE',  ( -1.000000000000000000, 0.000000000000000000, 0.000000000000000000 ) ) ;
#17304 = CARTESIAN_POINT ( 'NONE',  ( 10.09058376188599837, 3.152987476450699766, 6.960174024681499816 ) ) ;
#17305 = CARTESIAN_POINT ( 'NONE',  ( 8.229954139086000708, -4.681838082657003852, 6.132216288069997745 ) ) ;
#17306 = ORIENTED_EDGE ( 'NONE', *, *, #17404, .T. ) ;
#17307 = CARTESIAN_POINT ( 'NONE',  ( 11.00588826681000043, 3.012760565655999923, 5.961496895743000124 ) ) ;
#17308 = CARTESIAN_POINT ( 'NONE',  ( 10.52384528040999889, 5.441915759804999198, -7.989632847918000103 ) ) ;
#17309 = CARTESIAN_POINT ( 'NONE',  ( 17.96054543402357595, -12.10037373249118886, 3.233681995861158676 ) ) ;
#17310 = CARTESIAN_POINT ( 'NONE',  ( 12.41877979183513148, 1.899635599875573178, -13.87052873021461785 ) ) ;
#17311 = CARTESIAN_POINT ( 'NONE',  ( 10.11496314287999887, -2.748296264808000267, -7.236139910592400248 ) ) ;
#17312 = CARTESIAN_POINT ( 'NONE',  ( 9.318721994369999706, -2.755032632138999737, 8.795122807847999269 ) ) ;
#17313 = EDGE_CURVE ( 'NONE', #68412, #31887, #7638, .T. ) ;
#17314 = CARTESIAN_POINT ( 'NONE',  ( 18.23388030753891798, -0.2566959043864896484, 13.99765098363215188 ) ) ;
#17315 = CARTESIAN_POINT ( 'NONE',  ( 25.57799932127799991, -2.767938380759999983, 11.23359650972000168 ) ) ;
#17316 = ORIENTED_EDGE ( 'NONE', *, *, #28012, .T. ) ;
#17317 = ORIENTED_EDGE ( 'NONE', *, *, #3546, .T. ) ;
#17318 = CARTESIAN_POINT ( 'NONE',  ( 9.395239158775000377, 5.045571591548999812, -9.086294919530001124 ) ) ;
#17319 = CARTESIAN_POINT ( 'NONE',  ( 12.39297058734143953, -0.4699376426033362031, 13.88930769708871971 ) ) ;
#17320 = CARTESIAN_POINT ( 'NONE',  ( 12.26182380057219135, -0.3097576186077237170, -13.89536933048183975 ) ) ;
#17321 = FACE_OUTER_BOUND ( 'NONE', #28095, .T. ) ;
#17322 = DIRECTION ( 'NONE',  ( -1.000000000000000000, 0.000000000000000000, 0.000000000000000000 ) ) ;
#17323 = CARTESIAN_POINT ( 'NONE',  ( 7.999933059623999476, -5.198566224659999513, 8.332559954171999905 ) ) ;
#17324 = CARTESIAN_POINT ( 'NONE',  ( 8.737760194560388882, 3.933854210954582431, -8.370465981241707709 ) ) ;
#17326 = CARTESIAN_POINT ( 'NONE',  ( 11.07128162083999889, -6.555044467076000636, 5.493351806897000422 ) ) ;
#17325 = CARTESIAN_POINT ( 'NONE',  ( 10.33634252387499863, -5.264483068122999931, 7.693563834190999984 ) ) ;
#17327 = CARTESIAN_POINT ( 'NONE',  ( 10.59195391537400077, 5.057233422790000432, -8.218034727798299244 ) ) ;
#17328 = FACE_OUTER_BOUND ( 'NONE', #53257, .T. ) ;
#17329 = ADVANCED_FACE ( 'NONE', ( #29537 ), #50153, .T. ) ;
#17330 = CARTESIAN_POINT ( 'NONE',  ( 23.61660710412960995, 10.09774633507085539, -9.649252052224994713 ) ) ;
#17331 = CARTESIAN_POINT ( 'NONE',  ( 18.09636316215240015, -0.3125877143166536642, 12.69482668528968183 ) ) ;
#17332 = CARTESIAN_POINT ( 'NONE',  ( 6.966776889526476779, -12.39113590211060156, -2.782306601751617592 ) ) ;
#17333 = CARTESIAN_POINT ( 'NONE',  ( 18.16637421207913761, -2.630058154436578643, -12.42030992558146707 ) ) ;
#17334 = EDGE_LOOP ( 'NONE', ( #50558, #22930, #13644, #51158 ) ) ;
#17336 = CARTESIAN_POINT ( 'NONE',  ( 3.427367260881082789, 2.126417870048149528, -2.817200031586805764 ) ) ;
#17335 = CARTESIAN_POINT ( 'NONE',  ( 8.930995559624999913, -2.019079883662000086, 7.390983468784999566 ) ) ;
#17337 = CARTESIAN_POINT ( 'NONE',  ( 9.301695280414000067, 5.619431609641999614, -8.115423117607999615 ) ) ;
#17338 = DIRECTION ( 'NONE',  ( 1.000000000000000000, 0.000000000000000000, 0.000000000000000000 ) ) ;
#17339 = CARTESIAN_POINT ( 'NONE',  ( 23.56666365135700403, 8.673757318211000822, -7.881093921744994901 ) ) ;
#17340 = CARTESIAN_POINT ( 'NONE',  ( 0.9135616966234998415, 3.275095586319999974, -0.8499908244220999443 ) ) ;
#17341 = VECTOR ( 'NONE', #41036, 1000.000000000000000 ) ;
#17342 = CARTESIAN_POINT ( 'NONE',  ( 9.419900841099883237, 2.377805712834746288, 8.156167515375480903 ) ) ;
#17343 = CARTESIAN_POINT ( 'NONE',  ( 3.119794096232999969, 3.591452193409999882, 0.07293853716477999294 ) ) ;
#17344 = VERTEX_POINT ( 'NONE', #59233 ) ;
#17345 = EDGE_CURVE ( 'NONE', #19919, #46460, #857, .T. ) ;
#17346 = EDGE_CURVE ( 'NONE', #67708, #68916, #33020, .T. ) ;
#17347 = CARTESIAN_POINT ( 'NONE',  ( 12.08466115484542414, 0.08185661189466880705, -12.59973963693671983 ) ) ;
#17348 = CARTESIAN_POINT ( 'NONE',  ( 17.55505043854144276, 0.6250000000000001110, 12.67928921589117586 ) ) ;
#17349 = CARTESIAN_POINT ( 'NONE',  ( 17.92000013766227440, 3.102113379644126923, -12.21216327800867951 ) ) ;
#17350 = CARTESIAN_POINT ( 'NONE',  ( 24.19015434441247692, -12.39791403410435322, -3.330852224754460078 ) ) ;
#17351 = CARTESIAN_POINT ( 'NONE',  ( 7.384454719589999883, 3.346262376537000094, 6.002251090845000192 ) ) ;
#17352 = ORIENTED_EDGE ( 'NONE', *, *, #54974, .F. ) ;
#17353 = CARTESIAN_POINT ( 'NONE',  ( 6.788702397400999899, 1.551976682437999910, -0.4457619964912000188 ) ) ;
#17354 = EDGE_CURVE ( 'NONE', #8802, #37404, #45175, .T. ) ;
#17355 = ADVANCED_FACE ( 'NONE', ( #35438 ), #56764, .F. ) ;
#17356 = CARTESIAN_POINT ( 'NONE',  ( 7.906104719586000584, 5.732261791031000087, -7.476053406707000804 ) ) ;
#17358 = CARTESIAN_POINT ( 'NONE',  ( 9.966324641169999055, 2.303991951421000106, 6.575630951545000435 ) ) ;
#17357 = CARTESIAN_POINT ( 'NONE',  ( 25.60000000000000142, 0.000000000000000000, 0.000000000000000000 ) ) ;
#17359 = CARTESIAN_POINT ( 'NONE',  ( 10.90000000000000036, -1.199999999999999956, -9.776630298829998011 ) ) ;
#17360 = ORIENTED_EDGE ( 'NONE', *, *, #23607, .T. ) ;
#17361 = PLANE ( 'NONE',  #45607 ) ;
#17362 = CARTESIAN_POINT ( 'NONE',  ( 9.514108112060000622, -4.887639888682999256, 8.462756667353000140 ) ) ;
#17363 = VERTEX_POINT ( 'NONE', #60969 ) ;
#17364 = CARTESIAN_POINT ( 'NONE',  ( 24.68356055557331885, 3.139996735530106609, -11.82109522866602447 ) ) ;
#17365 = CARTESIAN_POINT ( 'NONE',  ( 16.00249209530700156, 3.346223412964000055, 11.40475585647000045 ) ) ;
#17366 = CARTESIAN_POINT ( 'NONE',  ( 18.05092994784024540, -0.3809766167652369195, -13.89298487834588514 ) ) ;
#17367 = ORIENTED_EDGE ( 'NONE', *, *, #18227, .T. ) ;
#17368 = CARTESIAN_POINT ( 'NONE',  ( 13.49980696793000057, 9.514462421839999351, 7.834836582454001608 ) ) ;
#17369 = CARTESIAN_POINT ( 'NONE',  ( 5.000000000000000000, 0.8000000000000000444, 3.149999999999999911 ) ) ;
#17370 = CARTESIAN_POINT ( 'NONE',  ( 10.77879632507499785, 4.423544049216699747, -8.285174533868300273 ) ) ;
#17371 = CARTESIAN_POINT ( 'NONE',  ( 8.953527735834686752, -2.251939686354768710, 7.420637145815573987 ) ) ;
#17372 = CARTESIAN_POINT ( 'NONE',  ( 18.29998515896361866, -2.924733550950529448, 11.97422828356911317 ) ) ;
#17373 = ORIENTED_EDGE ( 'NONE', *, *, #18228, .T. ) ;
#17374 = CARTESIAN_POINT ( 'NONE',  ( 8.641801658773999861, 2.933833973450999721, 8.496479443567000800 ) ) ;
#17375 = CARTESIAN_POINT ( 'NONE',  ( 23.61708161427199926, -13.18086190930000079, -4.239849120749999756 ) ) ;
#17376 = DIRECTION ( 'NONE',  ( 1.000000000000000000, 0.000000000000000000, 0.000000000000000000 ) ) ;
#17377 = VECTOR ( 'NONE', #43005, 1000.000000000000000 ) ;
#17378 = CARTESIAN_POINT ( 'NONE',  ( 15.61722669115800066, -9.375864875015000877, -8.222239459497000524 ) ) ;
#17379 = EDGE_LOOP ( 'NONE', ( #67227, #53157, #39898, #51424 ) ) ;
#17380 = B_SPLINE_SURFACE_WITH_KNOTS ( 'NONE', 1, 3, ( 
 ( #2770, #2091, #1734, #12230, #60812, #34941, #54876, #34604, #18857, #33556, #23749, #55917, #44403, #38799, #12575, #8364, #34252, #6978, #33905, #12925, #45429, #40184, #49976, #55222, #29019, #13618, #23053, #29709, #65703, #51010, #50326, #24442, #55572, #28663, #23409, #44746, #66045, #18168, #45768, #17474, #60124, #39490, #45086, #13278, #66393, #18516, #39838, #61160, #30049, #20561, #56599, #63193, #41887, #51686, #24781, #51352, #57269, #68100, #25807, #20217, #57616, #62178, #14637, #46454, #31066, #15322, #62518, #19189, #9719, #3784, #3444, #61838, #41208, #36647, #35284, #14973, #68441, #13957, #57970, #40857, #47140, #30715, #10069, #35955, #56941, #9369, #52374, #19538, #25122, #52025 ),
 ( #67753, #19879, #67076, #4468, #14300, #31404, #41543, #30378, #35628, #4817, #52719, #4126, #26159, #40512, #8706, #25462, #62855, #46795, #36296, #9037, #46108, #67414, #59688, #21930, #53415, #32782, #43268, #11440, #47484, #63887, #27192, #68790, #54095, #11788, #5513, #58307, #54443, #16346, #48512, #38363, #20907, #33127, #42244, #48167, #26502, #6192, #6544, #26854, #22280, #16000, #27534, #15663, #42923, #5852, #620, #53070, #38014, #64575, #43622, #64916, #53755, #63550, #16686, #69142, #48860, #36994, #969, #37330, #271, #59339, #5169, #10410, #31752, #47832, #17030, #21250, #58654, #32439, #21586, #42578, #10755, #32099, #64229, #37673, #59002, #11104, #12145, #34167, #45000, #54790 ) ),
 .UNSPECIFIED., .F., .F., .F.,
 ( 2, 2 ),
 ( 4, 2, 2, 2, 2, 2, 2, 2, 2, 2, 2, 2, 2, 2, 2, 2, 2, 2, 2, 2, 2, 2, 2, 2, 2, 2, 2, 2, 2, 2, 2, 2, 2, 2, 2, 2, 2, 2, 2, 2, 2, 2, 2, 2, 4 ),
 ( 0.000000000000000000, 1.000000000000000000 ),
 ( 0.000000000000000000, 7.143002489358809843E-05, 0.0001428600497871761969, 0.0002142900746807642953, 0.0002857200995743523937, 0.0003214351120211464429, 0.0003571501244679404921, 0.0003928651369147345414, 0.0004285801493615285906, 0.0005000101742551166890, 0.0005357251867019107924, 0.0005714401991487047874, 0.0006071552115954987824, 0.0006428702240422928859, 0.0007143002489358809843, 0.0007857302738294690827, 0.0008214452862762631861, 0.0008571602987230571812, 0.0009285903236166452796, 0.001000020348510233378, 0.001071450373403821585, 0.001142880398297409575, 0.001214310423190997565, 0.001285740448084585772, 0.001321455460531379984, 0.001357170472978173979, 0.001428600497871761969, 0.001500030522765349959, 0.001535745535212143954, 0.001571460547658938165, 0.001607175560105732377, 0.001642890572552526372, 0.001714320597446114362, 0.001750035609892908357, 0.001785750622339702352, 0.001821465634786496347, 0.001857180647233290559, 0.001928610672126878766, 0.001964325684573672761, 0.002000040697020466756, 0.002035755709467261185, 0.002071470721914055180, 0.002142900746807643170, 0.002214330771701231160, 0.002285760796594819150 ),
 .UNSPECIFIED. ) ;
#17381 = CARTESIAN_POINT ( 'NONE',  ( 12.70145053304005067, -1.883559157534606898, -12.57401126189225771 ) ) ;
#17382 = CARTESIAN_POINT ( 'NONE',  ( 10.59393020684899867, 5.250000000000000000, -7.500000000000000000 ) ) ;
#17383 = CARTESIAN_POINT ( 'NONE',  ( 10.93769906941999892, 2.936877991120999898, -4.920829195977000303 ) ) ;
#17384 = CARTESIAN_POINT ( 'NONE',  ( 7.102397164862999546, -0.2464401224313000349, 3.049949836518000001 ) ) ;
#17385 = CARTESIAN_POINT ( 'NONE',  ( 7.100000000000000533, 0.000000000000000000, 0.000000000000000000 ) ) ;
#17386 = CARTESIAN_POINT ( 'NONE',  ( 10.67410807141119911, -3.953638752893899877, -8.502397868920999358 ) ) ;
#17387 = CARTESIAN_POINT ( 'NONE',  ( 12.80505043854144098, -0.6250000000000006661, -13.88107975066922428 ) ) ;
#17388 = CARTESIAN_POINT ( 'NONE',  ( 17.57591323121273064, -3.124999405572034927, 12.28374652565519831 ) ) ;
#17389 = ORIENTED_EDGE ( 'NONE', *, *, #15011, .F. ) ;
#17390 = CARTESIAN_POINT ( 'NONE',  ( 11.01279632507519857, -3.375091146194399983, -8.658468685623999406 ) ) ;
#17391 = ORIENTED_EDGE ( 'NONE', *, *, #21955, .F. ) ;
#17392 = CARTESIAN_POINT ( 'NONE',  ( 11.74257329013500240, -12.32813410531000109, -1.877195977750000022 ) ) ;
#17393 = AXIS2_PLACEMENT_3D ( 'NONE', #38931, #7449, #28800 ) ;
#17394 = CARTESIAN_POINT ( 'NONE',  ( 8.739649184022004746, -2.648220570447153310, 7.263719241076167954 ) ) ;
#17395 = CARTESIAN_POINT ( 'NONE',  ( 2.419324796670999866, 1.946756166963000023, 2.762316150676000337 ) ) ;
#17396 = CARTESIAN_POINT ( 'NONE',  ( 10.97075054419999951, -2.648517896406999750, -6.788869136079999755 ) ) ;
#17397 = CIRCLE ( 'NONE', #59812, 1.000000000000000888 ) ;
#17398 = EDGE_CURVE ( 'NONE', #67539, #41699, #9192, .T. ) ;
#17399 = CARTESIAN_POINT ( 'NONE',  ( 9.140753410162000492, -5.100000000000000533, 6.175944241622000064 ) ) ;
#17400 = CARTESIAN_POINT ( 'NONE',  ( 23.91167052346600386, 12.75422773238000040, 3.593058583353999857 ) ) ;
#17401 = CARTESIAN_POINT ( 'NONE',  ( 11.39043504475232993, 2.929202812228125286, 6.797261353019674601 ) ) ;
#17402 = B_SPLINE_CURVE_WITH_KNOTS ( 'NONE', 3,
 ( #635, #16697, #38375, #48180 ),
 .UNSPECIFIED., .F., .F.,
 ( 4, 4 ),
 ( 0.000000000000000000, 1.000000000000000000 ),
 .UNSPECIFIED. ) ;
#17403 = ORIENTED_EDGE ( 'NONE', *, *, #23689, .F. ) ;
#17404 = EDGE_CURVE ( 'NONE', #55971, #66816, #30198, .T. ) ;
#17405 = CARTESIAN_POINT ( 'NONE',  ( 1.908466522725666525, -0.7663246491380455439, -3.431732421873642025 ) ) ;
#17406 = B_SPLINE_CURVE_WITH_KNOTS ( 'NONE', 3,
 ( #56673, #24160, #8430, #25188 ),
 .UNSPECIFIED., .F., .F.,
 ( 4, 4 ),
 ( 0.000000000000000000, 1.000000000000000000 ),
 .UNSPECIFIED. ) ;
#17407 = CARTESIAN_POINT ( 'NONE',  ( 10.62197831623999988, 5.779783227492000464, 7.256572995198999898 ) ) ;
#17408 = CARTESIAN_POINT ( 'NONE',  ( 10.06819717210663612, -5.125396288445600135, -6.749639981115930887 ) ) ;
#17409 = CARTESIAN_POINT ( 'NONE',  ( 10.78014141025500017, -3.582647672488299850, 6.756653759087999589 ) ) ;
#17410 = CARTESIAN_POINT ( 'NONE',  ( 18.12922381500399993, 3.157787539580000136, -11.36563583066999961 ) ) ;
#17411 = CARTESIAN_POINT ( 'NONE',  ( 10.85056919669530018, 4.830699382454300306, -7.745432529082900253 ) ) ;
#17412 = DIRECTION ( 'NONE',  ( 0.000000000000000000, 0.8648648648648717963, -0.5020047465136829867 ) ) ;
#17413 = CARTESIAN_POINT ( 'NONE',  ( 10.44222949779799947, 4.633452903845899584, -8.449985803660998940 ) ) ;
#17414 = CARTESIAN_POINT ( 'NONE',  ( 23.82000366591099905, -9.668684621276998570, -9.332229521209001177 ) ) ;
#17415 = CARTESIAN_POINT ( 'NONE',  ( 24.56892343362300224, -8.855981324802000287, 9.405092422590000112 ) ) ;
#17416 = CARTESIAN_POINT ( 'NONE',  ( 11.80912799980900019, -3.189026639965999443, 11.45098040807999951 ) ) ;
#17417 = VERTEX_POINT ( 'NONE', #50141 ) ;
#17418 = CARTESIAN_POINT ( 'NONE',  ( 7.565629440376999248, -3.206365290996999740, 5.681739161071000410 ) ) ;
#17419 = CARTESIAN_POINT ( 'NONE',  ( 9.355720302797999821, -5.362859773739999447, -6.470306978669999154 ) ) ;
#17420 = CARTESIAN_POINT ( 'NONE',  ( 17.98404385246622539, 2.954974373217227779, 13.56632247660221147 ) ) ;
#17421 = CARTESIAN_POINT ( 'NONE',  ( 8.933148997457999840, -5.167567567567999731, 6.822293592207000934 ) ) ;
#17422 = CARTESIAN_POINT ( 'NONE',  ( 10.61656919669529842, -2.774362666861999838, -7.862118085997298778 ) ) ;
#17423 = ORIENTED_EDGE ( 'NONE', *, *, #5762, .F. ) ;
#17424 = CARTESIAN_POINT ( 'NONE',  ( 25.26979871721500359, 2.550136720506999577, -11.36439046742999892 ) ) ;
#17425 = CARTESIAN_POINT ( 'NONE',  ( 7.705392219590000202, 3.245534453799999941, 8.949623695221001540 ) ) ;
#17426 = CIRCLE ( 'NONE', #12951, 1.550000000000000044 ) ;
#17428 = DIRECTION ( 'NONE',  ( -1.000000000000000000, -1.776356839370000173E-14, 0.000000000000000000 ) ) ;
#17427 = CARTESIAN_POINT ( 'NONE',  ( 9.790085841230000696, 5.149303692842000402, -5.987168472229000393 ) ) ;
#17429 = CARTESIAN_POINT ( 'NONE',  ( 3.064955461405348469, -2.879526833223610804, -1.523935657190285564 ) ) ;
#17430 = ORIENTED_EDGE ( 'NONE', *, *, #48297, .F. ) ;
#17431 = CARTESIAN_POINT ( 'NONE',  ( 10.66951519566999806, 4.592673277375999952, 5.841403042559999648 ) ) ;
#17432 = CARTESIAN_POINT ( 'NONE',  ( 17.75741541229206177, -3.091422763980662403, -13.53001720626202520 ) ) ;
#17433 = CARTESIAN_POINT ( 'NONE',  ( 10.28441772631199846, 4.372518460886800185, 6.733203680593099705 ) ) ;
#17434 = CARTESIAN_POINT ( 'NONE',  ( 9.959635380193999410, -5.406637819064000539, 7.700301345050000634 ) ) ;
#17435 = CARTESIAN_POINT ( 'NONE',  ( 7.726096713366001900, 2.834812733921999062, 6.825604963486997079 ) ) ;
#17436 = ORIENTED_EDGE ( 'NONE', *, *, #3608, .T. ) ;
#17437 = DIRECTION ( 'NONE',  ( -1.000000000000000000, 0.000000000000000000, 0.000000000000000000 ) ) ;
#17438 = ADVANCED_FACE ( 'NONE', ( #3601 ), #24937, .F. ) ;
#17439 = EDGE_CURVE ( 'NONE', #4322, #31587, #29323, .T. ) ;
#17440 = LINE ( 'NONE', #13160, #66251 ) ;
#17442 = CARTESIAN_POINT ( 'NONE',  ( 10.92546935320999957, -5.641520548727999795, -7.883473948564999390 ) ) ;
#17441 = CARTESIAN_POINT ( 'NONE',  ( 10.98768472639999949, -0.3876847264043000174, -4.945212061661000469 ) ) ;
#17443 = CARTESIAN_POINT ( 'NONE',  ( 7.771966698881652924, -5.059393530258413207, 8.879290890679834902 ) ) ;
#17444 = CARTESIAN_POINT ( 'NONE',  ( 9.409308287954999628, -2.634700736117999931, 8.920302460802998823 ) ) ;
#17446 = CARTESIAN_POINT ( 'NONE',  ( 23.55381184191400123, 3.060945918118999742, 13.69458336343999960 ) ) ;
#17445 = CIRCLE ( 'NONE', #53174, 12.49999909015999577 ) ;
#17447 = CARTESIAN_POINT ( 'NONE',  ( 10.46192546752100050, -5.139081147506999514, 7.578921399676699089 ) ) ;
#17448 = ORIENTED_EDGE ( 'NONE', *, *, #34206, .F. ) ;
#17449 = CARTESIAN_POINT ( 'NONE',  ( 24.14104147839731240, -9.152730137167427671, 9.126869235150973481 ) ) ;
#17450 = CARTESIAN_POINT ( 'NONE',  ( 11.39149144726329865, -4.659577337894599935, 8.430724369296298093 ) ) ;
#17451 = ORIENTED_EDGE ( 'NONE', *, *, #3074, .F. ) ;
#17452 = CARTESIAN_POINT ( 'NONE',  ( 7.528515907654997896, 3.227039430994999236, 6.419564954296006931 ) ) ;
#17453 = CARTESIAN_POINT ( 'NONE',  ( 10.17764828895399809, 5.001141961424000471, 6.953185708700699408 ) ) ;
#17454 = ORIENTED_EDGE ( 'NONE', *, *, #34669, .T. ) ;
#17455 = CARTESIAN_POINT ( 'NONE',  ( 8.722714158775000115, 3.892978337449999771, -8.893414073324001023 ) ) ;
#17456 = CARTESIAN_POINT ( 'NONE',  ( 23.55075825960500069, 13.34757147688000067, -4.341189614811999498 ) ) ;
#17457 = CARTESIAN_POINT ( 'NONE',  ( 12.30724456330681349, 3.003488097433216097, -12.23679193692685097 ) ) ;
#17458 = CARTESIAN_POINT ( 'NONE',  ( 10.87199293566600034, -3.366612813978900220, 6.723009541442299231 ) ) ;
#17459 = B_SPLINE_CURVE_WITH_KNOTS ( 'NONE', 3,
 ( #7090, #45878, #54991, #61609 ),
 .UNSPECIFIED., .F., .F.,
 ( 4, 4 ),
 ( 0.000000000000000000, 1.000000000000000000 ),
 .UNSPECIFIED. ) ;
#17460 = EDGE_CURVE ( 'NONE', #10760, #59329, #2921, .T. ) ;
#17461 = ORIENTED_EDGE ( 'NONE', *, *, #63680, .T. ) ;
#17462 = CARTESIAN_POINT ( 'NONE',  ( 10.99999999839000075, 0.3999999983917999491, 7.388315149414999894 ) ) ;
#17463 = CARTESIAN_POINT ( 'NONE',  ( 11.09999999999999964, -5.449702613288000208, -5.124965750789000296 ) ) ;
#17464 = ORIENTED_EDGE ( 'NONE', *, *, #60921, .T. ) ;
#17465 = CARTESIAN_POINT ( 'NONE',  ( 9.579652738407363088, 4.352972272612339211, 8.851639610528335922 ) ) ;
#17466 = CARTESIAN_POINT ( 'NONE',  ( 23.57773536430026695, 10.35457686501782604, 9.360237667582394394 ) ) ;
#17467 = VERTEX_POINT ( 'NONE', #40332 ) ;
#17468 = CARTESIAN_POINT ( 'NONE',  ( 12.53614341883834271, -3.148504814753052106, -12.20028441070642877 ) ) ;
#17469 = CARTESIAN_POINT ( 'NONE',  ( 10.84226088462129844, 4.002427228022017225, 8.640738455926999961 ) ) ;
#17470 = CARTESIAN_POINT ( 'NONE',  ( 24.35365242081699932, 1.906711579001001189, -11.36048031431998595 ) ) ;
#17471 = CARTESIAN_POINT ( 'NONE',  ( 9.934212804449000345, 5.120437537252000126, -8.883398686237999442 ) ) ;
#17472 = CARTESIAN_POINT ( 'NONE',  ( 17.73384588713700083, -11.55359908321999995, 4.937673966378999246 ) ) ;
#17473 = CARTESIAN_POINT ( 'NONE',  ( 10.63462194421999918, -5.668721490782999695, 6.527259573254000635 ) ) ;
#17474 = CARTESIAN_POINT ( 'NONE',  ( 12.18828317886891455, -2.603111844536877495, -13.65101713889819557 ) ) ;
#17475 = CARTESIAN_POINT ( 'NONE',  ( 18.16408092502819116, -0.1418569258565843816, -12.69895512164410079 ) ) ;
#17476 = CARTESIAN_POINT ( 'NONE',  ( 12.47602583993394632, 1.943637617988461352, -12.56471729223955336 ) ) ;
#17477 = CARTESIAN_POINT ( 'NONE',  ( 10.47303166480599934, -5.137916160623999140, -7.580230465881790280 ) ) ;
#17478 = CARTESIAN_POINT ( 'NONE',  ( 8.353301658773000682, 2.800103557244999930, 9.079946116129001155 ) ) ;
#17479 = ORIENTED_EDGE ( 'NONE', *, *, #52310, .F. ) ;
#17480 =( LENGTH_UNIT ( ) NAMED_UNIT ( * ) SI_UNIT ( .MILLI., .METRE. ) );
#17481 = VECTOR ( 'NONE', #38699, 1000.000000000000114 ) ;
#17482 = CARTESIAN_POINT ( 'NONE',  ( 11.60000000000000142, -4.549997407263328242, -8.379764693824251154 ) ) ;
#17483 = DIRECTION ( 'NONE',  ( -1.000000000000000000, 0.000000000000000000, 0.000000000000000000 ) ) ;
#17484 = CARTESIAN_POINT ( 'NONE',  ( 11.71271957899600125, 12.11624328427999941, 2.031646723569000113 ) ) ;
#17485 = AXIS2_PLACEMENT_3D ( 'NONE', #9524, #25616, #61990 ) ;
#17486 = CARTESIAN_POINT ( 'NONE',  ( 18.24314268136835437, 2.253095180823019295, 12.39692251310592397 ) ) ;
#17487 = CARTESIAN_POINT ( 'NONE',  ( 11.07126769815000067, 5.548036418162999972, 5.077736284810999479 ) ) ;
#17488 = CARTESIAN_POINT ( 'NONE',  ( 11.01811411617009817, 2.973039408543999951, -7.825000000000000178 ) ) ;
#17489 = ADVANCED_FACE ( 'NONE', ( #61655 ), #14511, .T. ) ;
#17490 = CARTESIAN_POINT ( 'NONE',  ( 25.60000000000000142, 9.899494936611999307, 9.899494936611999307 ) ) ;
#17491 = FACE_OUTER_BOUND ( 'NONE', #33972, .T. ) ;
#17492 = ORIENTED_EDGE ( 'NONE', *, *, #47754, .T. ) ;
#17493 = CARTESIAN_POINT ( 'NONE',  ( 12.08596835297192307, -2.576236330983343148, 12.33383868535373118 ) ) ;
#17494 = CARTESIAN_POINT ( 'NONE',  ( 10.36422949779699820, -3.442773960835399993, -8.335668797826500054 ) ) ;
#17495 = DIRECTION ( 'NONE',  ( 1.000000000000000000, 0.000000000000000000, 0.000000000000000000 ) ) ;
#17496 = CARTESIAN_POINT ( 'NONE',  ( 8.331682137624000006, -5.101289325373999262, 6.607176193198000647 ) ) ;
#17497 = VECTOR ( 'NONE', #24318, 1000.000000000000000 ) ;
#17498 = CARTESIAN_POINT ( 'NONE',  ( 11.40841235500449891, 3.158861363519000154, -6.729431436870699557 ) ) ;
#17499 = VERTEX_POINT ( 'NONE', #35102 ) ;
#17500 = CARTESIAN_POINT ( 'NONE',  ( 12.08146954708835707, -0.04649795050485633352, 12.59991969135870171 ) ) ;
#17501 = CARTESIAN_POINT ( 'NONE',  ( 8.304135841228999837, 3.650414032626000171, 6.083147621602999600 ) ) ;
#17502 = FACE_OUTER_BOUND ( 'NONE', #59621, .T. ) ;
#17503 = CARTESIAN_POINT ( 'NONE',  ( 12.41452611191162880, 2.987998126639116236, 12.32436705583800318 ) ) ;
#17504 = VERTEX_POINT ( 'NONE', #62676 ) ;
#17505 = DIRECTION ( 'NONE',  ( -1.000000000000000000, 0.000000000000000000, 0.000000000000000000 ) ) ;
#17506 = CARTESIAN_POINT ( 'NONE',  ( 10.34995525820099971, 3.892289273474800471, -6.364355462479999836 ) ) ;
#17507 = DIRECTION ( 'NONE',  ( -1.000000000000000000, 0.000000000000000000, 0.000000000000000000 ) ) ;
#17509 = CARTESIAN_POINT ( 'NONE',  ( 18.03350839596208033, -0.4021454014604768368, 12.69143011154429246 ) ) ;
#17508 = CARTESIAN_POINT ( 'NONE',  ( 8.064674013518999374, 4.643178316509001036, 6.221316387655001279 ) ) ;
#17510 = CARTESIAN_POINT ( 'NONE',  ( 9.680747021775999883, -4.651672637235799712, 6.928134003122899287 ) ) ;
#17511 = CARTESIAN_POINT ( 'NONE',  ( 10.33364828895399867, -3.239803852721999888, -7.915211961479200475 ) ) ;
#17512 = CARTESIAN_POINT ( 'NONE',  ( 10.10000000000000142, -11.84999999999999964, 0.000000000000000000 ) ) ;
#17513 = ORIENTED_EDGE ( 'NONE', *, *, #28685, .T. ) ;
#17514 = CARTESIAN_POINT ( 'NONE',  ( 1.930112477862999887, -1.998287707672000035, 2.574515877127999897 ) ) ;
#17515 = CARTESIAN_POINT ( 'NONE',  ( 23.71152083938696009, -9.910026289319734616, -9.457066222056473848 ) ) ;
#17516 = CARTESIAN_POINT ( 'NONE',  ( 12.49459120400055667, -12.10614746208238302, 3.212001293532054103 ) ) ;
#17517 = CARTESIAN_POINT ( 'NONE',  ( 9.045101285863999863, 3.441732526340400167, 8.163359157892799089 ) ) ;
#17518 = CARTESIAN_POINT ( 'NONE',  ( 11.03443712336079940, -2.942831166283299105, -7.175021320887989162 ) ) ;
#17519 = CARTESIAN_POINT ( 'NONE',  ( 12.37945077454914156, -1.926407208811270033, 13.86683589633374503 ) ) ;
#17520 = CARTESIAN_POINT ( 'NONE',  ( 10.97197891481999932, 2.857467565480000360, 4.995747414879000203 ) ) ;
#17521 = CARTESIAN_POINT ( 'NONE',  ( 11.09999999999999964, 5.449702574547000467, 5.124965750789000296 ) ) ;
#17522 = CARTESIAN_POINT ( 'NONE',  ( 13.60156003475500164, -12.26415473033000048, -2.266572665737999870 ) ) ;
#17523 = ORIENTED_EDGE ( 'NONE', *, *, #52867, .T. ) ;
#17524 = CARTESIAN_POINT ( 'NONE',  ( 7.542083333330625194, 4.829638071966136259, -6.420449762762456380 ) ) ;
#17525 = EDGE_CURVE ( 'NONE', #19259, #48851, #16789, .T. ) ;
#17526 = EDGE_CURVE ( 'NONE', #21757, #42930, #34639, .T. ) ;
#17527 = DIRECTION ( 'NONE',  ( -1.000000000000000000, 0.000000000000000000, 0.000000000000000000 ) ) ;
#17528 = CARTESIAN_POINT ( 'NONE',  ( 9.179055905797000037, 2.899999999999999911, 6.571291218949999902 ) ) ;
#17529 = CARTESIAN_POINT ( 'NONE',  ( 18.26547113879619033, -3.186161613544661098, -11.20588962290425528 ) ) ;
#17530 = CARTESIAN_POINT ( 'NONE',  ( 0.5607456912831000340, 3.437215509016000148, 1.521310954037999874 ) ) ;
#17531 = CARTESIAN_POINT ( 'NONE',  ( 1.928056799206333327, 2.150913519912206695, -2.798833948393627313 ) ) ;
#17532 = CARTESIAN_POINT ( 'NONE',  ( 24.30001697352500045, -3.271769158411000245, -12.21048181092999840 ) ) ;
#17533 = FACE_OUTER_BOUND ( 'NONE', #26483, .T. ) ;
#17534 = COLOUR_RGB ( '', 0.72549020, 0.75294118, 0.79215686) ;
#17535 = CARTESIAN_POINT ( 'NONE',  ( 11.24441369783139777, 3.956299011112040187, 6.634905315059499209 ) ) ;
#17536 = CARTESIAN_POINT ( 'NONE',  ( 11.79999999471800010, -3.216299622513999701, 11.40340969442000052 ) ) ;
#17537 = CARTESIAN_POINT ( 'NONE',  ( 10.67529314679000052, -3.066674550532999977, -8.703235919197002346 ) ) ;
#17538 = VECTOR ( 'NONE', #22848, 1000.000000000000114 ) ;
#17539 = CARTESIAN_POINT ( 'NONE',  ( 10.98768472625999948, -6.720753154780999772, 5.471698433974999887 ) ) ;
#17540 = CARTESIAN_POINT ( 'NONE',  ( 10.59999999999999964, 4.599999999999999645, 4.756097560976000338 ) ) ;
#17541 = CARTESIAN_POINT ( 'NONE',  ( 24.67921570607400383, -3.567514742249000115, 12.13750887372000165 ) ) ;
#17542 = ADVANCED_FACE ( 'NONE', ( #68956 ), #613, .F. ) ;
#17543 = ORIENTED_EDGE ( 'NONE', *, *, #5054, .T. ) ;
#17544 = CARTESIAN_POINT ( 'NONE',  ( 9.442010841233001273, 5.045571591548999812, -9.086294919530001124 ) ) ;
#17545 = VERTEX_POINT ( 'NONE', #24859 ) ;
#17546 = VECTOR ( 'NONE', #56127, 1000.000000000000000 ) ;
#17547 = CARTESIAN_POINT ( 'NONE',  ( 18.16667230414096323, -2.370970514942110974, 13.69998174157045234 ) ) ;
#17548 = CARTESIAN_POINT ( 'NONE',  ( 10.05862282008599884, -3.333723918618700210, -8.574682153725998290 ) ) ;
#17549 = EDGE_LOOP ( 'NONE', ( #18927, #65668, #58683, #8742, #7742, #59073, #1026, #61055 ) ) ;
#17550 = ADVANCED_FACE ( 'NONE', ( #66123 ), #60543, .F. ) ;
#17551 = CARTESIAN_POINT ( 'NONE',  ( 11.14767835872009982, 3.125658946326500320, 8.051056647135798272 ) ) ;
#17552 = CARTESIAN_POINT ( 'NONE',  ( 6.035344492469169708, 0.9622224758110548004, -0.5982748535759940811 ) ) ;
#17553 = CARTESIAN_POINT ( 'NONE',  ( 24.04054642575986378, 3.344385333844766883, -12.67224307145318818 ) ) ;
#17554 = CARTESIAN_POINT ( 'NONE',  ( 11.27110638630999873, 5.469603964121000139, 8.504707115835000053 ) ) ;
#17555 = DIRECTION ( 'NONE',  ( 0.000000000000000000, 1.000000000000000000, 0.000000000000000000 ) ) ;
#17556 = CARTESIAN_POINT ( 'NONE',  ( 10.81059687351633336, -4.629523725463621453, 8.592232985442823434 ) ) ;
#17557 = CARTESIAN_POINT ( 'NONE',  ( 11.83178351958400043, 3.316209711830000018, -11.22342786695999983 ) ) ;
#17558 = AXIS2_PLACEMENT_3D ( 'NONE', #54763, #54069, #40323 ) ;
#17559 = CARTESIAN_POINT ( 'NONE',  ( 10.02800210979000184, -3.452027005875999865, -6.074520565702999697 ) ) ;
#17560 = DIRECTION ( 'NONE',  ( -0.000000000000000000, -0.000000000000000000, 1.000000000000000000 ) ) ;
#17561 = ORIENTED_EDGE ( 'NONE', *, *, #68895, .F. ) ;
#17562 = CARTESIAN_POINT ( 'NONE',  ( 10.55909255430753824, -3.020528152026101143, -5.017625565365243290 ) ) ;
#17563 = ORIENTED_EDGE ( 'NONE', *, *, #43679, .T. ) ;
#17564 = CARTESIAN_POINT ( 'NONE',  ( -15.86200481174999943, 5.599999999999999645, 6.571291218949999902 ) ) ;
#17565 = ORIENTED_EDGE ( 'NONE', *, *, #9794, .T. ) ;
#17566 = FACE_OUTER_BOUND ( 'NONE', #63069, .T. ) ;
#17567 = CARTESIAN_POINT ( 'NONE',  ( 10.33085896026999961, -4.880781593996999845, 4.717851323696000243 ) ) ;
#17568 = CARTESIAN_POINT ( 'NONE',  ( 10.47683719568447636, 4.186288604638629174, 8.354041075310609799 ) ) ;
#17569 = CARTESIAN_POINT ( 'NONE',  ( 10.14029229006299992, 5.106256438265999620, -6.857675253263499471 ) ) ;
#17570 = CARTESIAN_POINT ( 'NONE',  ( 12.20320247475634545, 2.331154411892200962, 13.70777421733259516 ) ) ;
#17571 = CARTESIAN_POINT ( 'NONE',  ( 10.37026726325999881, -5.571557883540000589, 7.748386351620999868 ) ) ;
#17572 = ORIENTED_EDGE ( 'NONE', *, *, #58583, .T. ) ;
#17573 = CARTESIAN_POINT ( 'NONE',  ( 12.10000669845703847, -11.02846243759423039, 3.754394857303111621 ) ) ;
#17574 = CARTESIAN_POINT ( 'NONE',  ( 12.32658172867158797, 0.5491314443420094449, 13.98923457196398168 ) ) ;
#17575 = ORIENTED_EDGE ( 'NONE', *, *, #44232, .T. ) ;
#17576 = CARTESIAN_POINT ( 'NONE',  ( 7.157271682457999162, 5.172411450403999744, -8.246583185469999577 ) ) ;
#17577 = CARTESIAN_POINT ( 'NONE',  ( 8.865073590557452476, 2.650142864597553327, -7.500004675916596142 ) ) ;
#17578 = CARTESIAN_POINT ( 'NONE',  ( 23.62920471791399990, -3.420566888407999606, -13.57806623620999886 ) ) ;
#17579 = CARTESIAN_POINT ( 'NONE',  ( 4.579397794411000255, 0.8193957582319000288, 1.053447925930000029 ) ) ;
#17580 = AXIS2_PLACEMENT_3D ( 'NONE', #65409, #18220, #7033 ) ;
#17581 = CARTESIAN_POINT ( 'NONE',  ( 8.631645280409999899, 3.826300099041999747, -9.055335252254000267 ) ) ;
#17582 = MECHANICAL_DESIGN_GEOMETRIC_PRESENTATION_REPRESENTATION (  '', ( #18685 ), #47728 ) ;
#17583 = FACE_OUTER_BOUND ( 'NONE', #58822, .T. ) ;
#17584 = CARTESIAN_POINT ( 'NONE',  ( 10.75911128370000114, -4.477561100530000004, -5.708582007447000173 ) ) ;
#17585 = PRODUCT_RELATED_PRODUCT_CATEGORY ( 'part', '', ( #46133 ) ) ;
#17586 = DIRECTION ( 'NONE',  ( 0.000000000000000000, 1.000000000000000000, 0.000000000000000000 ) ) ;
#17587 = FACE_OUTER_BOUND ( 'NONE', #4673, .T. ) ;
#17588 = AXIS2_PLACEMENT_3D ( 'NONE', #1675, #7262, #2364 ) ;
#17589 = CARTESIAN_POINT ( 'NONE',  ( 4.600000533658279878, -13.89999946622000060, -2.316960006352999632E-09 ) ) ;
#17590 = DIRECTION ( 'NONE',  ( 0.000000000000000000, -1.000000000000000000, 0.000000000000000000 ) ) ;
#17591 = CARTESIAN_POINT ( 'NONE',  ( 8.558656745902677443, -3.294699824964758772, 5.942504329580781786 ) ) ;
#17592 = CARTESIAN_POINT ( 'NONE',  ( 12.08019350287876925, 0.1887961028408512432, 12.59999260960569067 ) ) ;
#17593 = CARTESIAN_POINT ( 'NONE',  ( 10.44999293566599974, 4.720032669050099550, -8.383280442119700027 ) ) ;
#17594 = CARTESIAN_POINT ( 'NONE',  ( 9.837292290062999101, 4.868609929059700470, -6.995659746333000584 ) ) ;
#17596 = CARTESIAN_POINT ( 'NONE',  ( 10.27199419957999993, -3.240085154792000210, 4.537815602971000395 ) ) ;
#17595 = CARTESIAN_POINT ( 'NONE',  ( 9.722405316139999698, -4.184077495686000958, 6.652755395362000002 ) ) ;
#17597 = CARTESIAN_POINT ( 'NONE',  ( 7.575821720216998401, -3.529668843644999221, 6.549222992663997545 ) ) ;
#17598 = ORIENTED_EDGE ( 'NONE', *, *, #25440, .F. ) ;
#17599 = AXIS2_PLACEMENT_3D ( 'NONE', #49072, #23195, #22844 ) ;
#17600 = B_SPLINE_CURVE_WITH_KNOTS ( 'NONE', 3,
 ( #8144, #60251, #44871, #45214, #50109, #61286, #12699, #2548, #39969, #6751, #13402, #7446, #34383, #50800, #66175, #28796, #55701, #18639, #29138, #50446, #12353, #22835, #65480, #33341, #29493, #33686, #38572, #2892, #54656, #60593, #28090, #49404, #55003, #28442, #1866, #65826, #23529, #34037, #2215, #62311, #52157, #24906, #20009, #51814, #36084, #14428, #57399, #8488, #41334, #3241, #13737, #40303, #40988, #3912, #62641, #20346, #8828, #9504, #19313, #14767, #35070, #30846, #14083, #68227, #4260 ),
 .UNSPECIFIED., .F., .F.,
 ( 4, 1, 1, 1, 1, 1, 1, 1, 1, 1, 1, 1, 1, 1, 1, 1, 1, 1, 1, 1, 1, 1, 1, 1, 1, 1, 1, 1, 1, 1, 1, 1, 1, 1, 1, 1, 1, 1, 1, 1, 1, 1, 1, 1, 1, 1, 1, 1, 1, 1, 1, 1, 1, 1, 1, 1, 1, 1, 1, 1, 1, 1, 4 ),
 ( 0.000000000000000000, 0.01249986222369741350, 0.02874986775682985066, 0.04499987328996228608, 0.06124987882309472498, 0.07749988435622716387, 0.09374988988935960277, 0.1099998954224920417, 0.1262499009556244944, 0.1424999064887569056, 0.1587499120218893722, 0.1749999175550217834, 0.1912499230881542500, 0.2074999286212866612, 0.2237499341544191278, 0.2399999396875515389, 0.2562499452206840056, 0.2724999507538165000, 0.2887499562869488834, 0.3049999618200813223, 0.3212499673532137612, 0.3374999728863462556, 0.3537499784194786390, 0.3699999839526110779, 0.3862499894857435168, 0.4024999950188760112, 0.4187500005520083945, 0.4350000060851408334, 0.4512500116182732723, 0.4675000171514057667, 0.4837500226845381501, 0.5000000282176706445, 0.5162500337508029169, 0.5325000392839354113, 0.5487500448170677947, 0.5650000503502002891, 0.5812500558833327835, 0.5975000614164651669, 0.6137500669495976613, 0.6300000724827300447, 0.6462500780158624281, 0.6625000835489949225, 0.6787500890821273059, 0.6950000946152598003, 0.7112501001483922947, 0.7275001056815246780, 0.7437501112146571725, 0.7600001167477895558, 0.7762501222809219392, 0.7925001278140544336, 0.8087501333471868170, 0.8250001388803193114, 0.8412501444134518058, 0.8575001499465841892, 0.8737501554797166836, 0.8900001610128490670, 0.9062501665459814504, 0.9225001720791139448, 0.9387501776122463282, 0.9550001831453788226, 0.9712501886785112060, 0.9875001942116437004, 1.000000000000000000 ),
 .UNSPECIFIED. ) ;
#17601 = CARTESIAN_POINT ( 'NONE',  ( 11.30878751119029957, 2.958974835389999836, 6.955365841266999638 ) ) ;
#17602 = CARTESIAN_POINT ( 'NONE',  ( 7.428159769834000059, -3.524402284009999331, 6.653317709399996005 ) ) ;
#17603 = CARTESIAN_POINT ( 'NONE',  ( 9.177784697135001224, 4.694174896253500151, 8.574479223074998657 ) ) ;
#17604 = CARTESIAN_POINT ( 'NONE',  ( 10.35685100253999913, 2.832432432432000269, -6.822293592207000934 ) ) ;
#17605 = CARTESIAN_POINT ( 'NONE',  ( 9.323728576950999880, -3.947350124452999598, 6.051857392047999440 ) ) ;
#17606 = CARTESIAN_POINT ( 'NONE',  ( 10.01186131679890856, -2.762178309543651178, 6.265253433400348015 ) ) ;
#17608 = CARTESIAN_POINT ( 'NONE',  ( 11.71260115691700143, 3.298410940261000235, -11.83433202606999934 ) ) ;
#17607 = UNCERTAINTY_MEASURE_WITH_UNIT (LENGTH_MEASURE( 1.000000000000000082E-05 ), #17209, 'distance_accuracy_value', 'NONE');
#17609 = EDGE_LOOP ( 'NONE', ( #46493, #20640, #8188, #13685 ) ) ;
#17610 = EDGE_CURVE ( 'NONE', #42540, #10227, #53451, .T. ) ;
#17611 = EDGE_CURVE ( 'NONE', #7298, #15615, #25963, .T. ) ;
#17612 = CARTESIAN_POINT ( 'NONE',  ( 9.963938025973998691, -4.522194782554399772, -6.642005297568199573 ) ) ;
#17613 = CARTESIAN_POINT ( 'NONE',  ( 8.599999999999999645, 4.000000000000000000, 7.500000000000000000 ) ) ;
#17614 = CARTESIAN_POINT ( 'NONE',  ( 5.167306792578000518, -1.056937757944000023, -1.220746830110999825 ) ) ;
#17615 = CARTESIAN_POINT ( 'NONE',  ( 6.999999999999998224, 9.596681707279657303, -4.662612261201800834 ) ) ;
#17616 = CYLINDRICAL_SURFACE ( 'NONE', #32829, 13.10000000000000142 ) ;
#17617 = B_SPLINE_CURVE_WITH_KNOTS ( 'NONE', 3,
 ( #19832, #36599, #40807, #46750, #51302, #67364, #68055, #36250, #9671, #47436 ),
 .UNSPECIFIED., .F., .F.,
 ( 4, 2, 2, 2, 4 ),
 ( 0.5000000000000000000, 0.6250000000000000000, 0.7500000000000000000, 0.8750000000000000000, 1.000000000000000000 ),
 .UNSPECIFIED. ) ;
#17618 = CARTESIAN_POINT ( 'NONE',  ( 12.01518179236249040, -4.180996681294200101, 8.347076615013298451 ) ) ;
#17619 = CARTESIAN_POINT ( 'NONE',  ( 10.99410672858429905, 3.198097575668700010, -6.896755974168000236 ) ) ;
#17620 = FACE_OUTER_BOUND ( 'NONE', #20735, .T. ) ;
#17621 = CARTESIAN_POINT ( 'NONE',  ( 8.434520297147999557, 5.100000003584000297, 6.577489351425000130 ) ) ;
#17622 = DIRECTION ( 'NONE',  ( -1.000000000000000000, 6.086974017450490350E-15, -6.313390726317570167E-15 ) ) ;
#17623 = ORIENTED_EDGE ( 'NONE', *, *, #23580, .F. ) ;
#17624 = CARTESIAN_POINT ( 'NONE',  ( 7.579654319238870563, -4.353725718092394281, 8.815991072544541396 ) ) ;
#17625 = AXIS2_PLACEMENT_3D ( 'NONE', #6886, #43962, #32436 ) ;
#17626 = CARTESIAN_POINT ( 'NONE',  ( 12.76393046405280174, 0.6239795106976173678, -13.88114172264460322 ) ) ;
#17627 = CARTESIAN_POINT ( 'NONE',  ( 8.365056901398830291, 2.650139792115765669, -7.500003826568613086 ) ) ;
#17628 = CARTESIAN_POINT ( 'NONE',  ( 24.56885749267500074, -8.742331804604999590, -8.862243903196000971 ) ) ;
#17629 = CARTESIAN_POINT ( 'NONE',  ( 13.35262485425710999, -11.51206127779176036, -1.787622147836161579 ) ) ;
#17630 = CARTESIAN_POINT ( 'NONE',  ( 18.29999330150736014, -11.02846243710336616, 3.754394858745019103 ) ) ;
#17631 = CARTESIAN_POINT ( 'NONE',  ( 5.670648345173815663, 12.06568050912902734, -3.730933605404140430 ) ) ;
#17632 = VERTEX_POINT ( 'NONE', #18929 ) ;
#17633 = AXIS2_PLACEMENT_3D ( 'NONE', #65061, #49695, #23815 ) ;
#17634 = DIRECTION ( 'NONE',  ( 0.000000000000000000, 1.000000000000000000, 0.000000000000000000 ) ) ;
#17635 = CARTESIAN_POINT ( 'NONE',  ( 17.77706283214423877, 1.915668542326107726, -13.78016448532188676 ) ) ;
#17636 = ORIENTED_EDGE ( 'NONE', *, *, #14691, .F. ) ;
#17637 = EDGE_CURVE ( 'NONE', #38378, #31683, #10111, .T. ) ;
#17638 = DIRECTION ( 'NONE',  ( 1.000000000000000000, 0.000000000000000000, 0.000000000000000000 ) ) ;
#17639 = CARTESIAN_POINT ( 'NONE',  ( 9.123558059623999128, -5.558929022707999046, 6.272984818914999927 ) ) ;
#17640 = CARTESIAN_POINT ( 'NONE',  ( 9.319414158774000256, 2.656512020013999997, -7.884832994446999699 ) ) ;
#17641 = CARTESIAN_POINT ( 'NONE',  ( 11.10000000000000142, -2.722910913279374068, -8.517131090127774584 ) ) ;
#17642 = CARTESIAN_POINT ( 'NONE',  ( 11.76588784977539781, -5.120865761890000201, -7.435950347916509884 ) ) ;
#17643 = CARTESIAN_POINT ( 'NONE',  ( 17.63846197675113103, 0.6206501420305031713, -12.67957965403867426 ) ) ;
#17644 = PLANE ( 'NONE',  #20645 ) ;
#17645 = ORIENTED_EDGE ( 'NONE', *, *, #58725, .F. ) ;
#17646 = DIRECTION ( 'NONE',  ( 0.000000000000000000, -0.8646938284590766077, 0.5022992962614868384 ) ) ;
#17647 = FACE_OUTER_BOUND ( 'NONE', #21244, .T. ) ;
#17648 = CARTESIAN_POINT ( 'NONE',  ( 9.345514158774999913, 5.775964236216999836, -8.174909295649001706 ) ) ;
#17649 = ORIENTED_EDGE ( 'NONE', *, *, #6943, .T. ) ;
#17650 = AXIS2_PLACEMENT_3D ( 'NONE', #50634, #13244, #25087 ) ;
#17651 = CARTESIAN_POINT ( 'NONE',  ( 10.89218604104999955, 2.661903984162000469, -8.236033286991000679 ) ) ;
#17652 = CARTESIAN_POINT ( 'NONE',  ( 11.18236694037999968, -4.516641106826999597, -8.757887038823000125 ) ) ;
#17653 = VERTEX_POINT ( 'NONE', #29785 ) ;
#17654 = CARTESIAN_POINT ( 'NONE',  ( 9.457355082327998375, 3.550486524676900402, 8.398209294002699110 ) ) ;
#17655 = CARTESIAN_POINT ( 'NONE',  ( 17.91037351677410072, -3.107515944418828280, -12.21078942061118155 ) ) ;
#17656 = CARTESIAN_POINT ( 'NONE',  ( 9.560596873515667227, 4.629523725463624118, 6.407767014557177454 ) ) ;
#17657 = CARTESIAN_POINT ( 'NONE',  ( 16.34794651623100137, 3.644047358192000097, 12.02362153922000054 ) ) ;
#17658 = CARTESIAN_POINT ( 'NONE',  ( 11.08757144985999865, 2.712428550139000194, 6.571291218949999902 ) ) ;
#17659 = AXIS2_PLACEMENT_3D ( 'NONE', #19171, #45751, #40495 ) ;
#17660 = CARTESIAN_POINT ( 'NONE',  ( 9.054101285863998427, 3.441732526340400167, 8.163359157892799089 ) ) ;
#17661 = ORIENTED_EDGE ( 'NONE', *, *, #55579, .F. ) ;
#17662 = FACE_OUTER_BOUND ( 'NONE', #22210, .T. ) ;
#17663 = CARTESIAN_POINT ( 'NONE',  ( 10.10735778041000010, 4.293584699549000128, -8.994197232567001876 ) ) ;
#17664 = CARTESIAN_POINT ( 'NONE',  ( 17.87831314280386152, -11.54767577568710557, 4.850450964119741748 ) ) ;
#17665 = CARTESIAN_POINT ( 'NONE',  ( 12.41482009541958931, 2.988314721215474368, -13.55768135971568178 ) ) ;
#17666 = CARTESIAN_POINT ( 'NONE',  ( 10.90000000011000125, -2.899999999889000257, -6.571291220762999430 ) ) ;
#17667 = CARTESIAN_POINT ( 'NONE',  ( 9.967845797207999681, -2.034786297409000078, 7.636877353231999344 ) ) ;
#17668 = CARTESIAN_POINT ( 'NONE',  ( 17.67410956179875114, -0.7206971133477443336, 13.98143832535763131 ) ) ;
#17669 = CARTESIAN_POINT ( 'NONE',  ( 17.88363324756175388, 0.5317637309505709453, 13.88630818040731718 ) ) ;
#17670 = EDGE_CURVE ( 'NONE', #36315, #60701, #28449, .T. ) ;
#17671 = EDGE_CURVE ( 'NONE', #28975, #29686, #44671, .T. ) ;
#17672 = EDGE_LOOP ( 'NONE', ( #22115, #7847, #40691, #1669 ) ) ;
#17673 = ORIENTED_EDGE ( 'NONE', *, *, #27146, .T. ) ;
#17674 = CARTESIAN_POINT ( 'NONE',  ( 9.286929719595001131, 4.102804347295999854, -5.770625657082999460 ) ) ;
#17675 = CARTESIAN_POINT ( 'NONE',  ( 12.39828470338709110, -0.4745495849572874958, 13.88909655037513602 ) ) ;
#17676 = CARTESIAN_POINT ( 'NONE',  ( 12.24748039821077583, -0.2825697095353449928, -13.89613713856699029 ) ) ;
#17677 = CARTESIAN_POINT ( 'NONE',  ( 11.00000000000000000, -3.008232475376599879, -7.174999999999999822 ) ) ;
#17678 = CARTESIAN_POINT ( 'NONE',  ( 5.000000000000000000, 0.2999999999999999889, -9.776630298829998011 ) ) ;
#17679 = CARTESIAN_POINT ( 'NONE',  ( 7.037120559622001004, -4.623636604834999275, 8.651469651195000665 ) ) ;
#17680 = CARTESIAN_POINT ( 'NONE',  ( 24.67921139482200132, 8.727627377900999406, -9.158314240160001063 ) ) ;
#17683 = B_SPLINE_CURVE_WITH_KNOTS ( 'NONE', 3,
 ( #36182, #42119, #42804, #4694 ),
 .UNSPECIFIED., .F., .F.,
 ( 4, 4 ),
 ( 0.000000000000000000, 1.000000000000000000 ),
 .UNSPECIFIED. ) ;
#17682 = DIRECTION ( 'NONE',  ( 0.000000000000000000, -0.1218274111675001353, -0.9925512993736016476 ) ) ;
#17681 = CARTESIAN_POINT ( 'NONE',  ( 10.79226717315700057, -4.973628086880700572, 8.329718467866699783 ) ) ;
#17684 = CARTESIAN_POINT ( 'NONE',  ( 8.629835589027990750, -5.187744040556002467, -6.859988146772001194 ) ) ;
#17685 = CARTESIAN_POINT ( 'NONE',  ( 7.544160676995611325, 5.349767121210510901, -7.146874343389594486 ) ) ;
#17686 = DIRECTION ( 'NONE',  ( 1.000000000000000000, 0.000000000000000000, 0.000000000000000000 ) ) ;
#17687 = CARTESIAN_POINT ( 'NONE',  ( 17.71747088695468264, 0.6038699852804538803, 12.68066884516330362 ) ) ;
#17688 = CARTESIAN_POINT ( 'NONE',  ( 6.548735035738999954, -1.228754840668000003, 0.9029015244175999655 ) ) ;
#17689 = CIRCLE ( 'NONE', #35558, 8.250000000000000000 ) ;
#17690 = CARTESIAN_POINT ( 'NONE',  ( 4.149992563291999836, 1.599290730647368930, 1.229060429538529675 ) ) ;
#17691 = ORIENTED_EDGE ( 'NONE', *, *, #6336, .F. ) ;
#17693 = CARTESIAN_POINT ( 'NONE',  ( 10.96914282210478042, 4.267867395145749754, 8.332067702129235087 ) ) ;
#17692 = CARTESIAN_POINT ( 'NONE',  ( 11.08923508776348754, -3.836355263994051690, -9.039235091851082871 ) ) ;
#17694 = CARTESIAN_POINT ( 'NONE',  ( 9.152520280414000453, 4.102804347295999854, -5.770625657082999460 ) ) ;
#17695 = EDGE_CURVE ( 'NONE', #40162, #68990, #41967, .T. ) ;
#17696 = CARTESIAN_POINT ( 'NONE',  ( 12.58276127734165151, -1.915504326815320901, 13.78019217388816919 ) ) ;
#17697 = CARTESIAN_POINT ( 'NONE',  ( 10.26328274790922634, -2.909659596545102644, -8.325272347294594866 ) ) ;
#17698 = CARTESIAN_POINT ( 'NONE',  ( 8.434756776051003158, -5.098765216145000778, 6.624660916390000764 ) ) ;
#17699 = AXIS2_PLACEMENT_3D ( 'NONE', #14512, #47356, #46671 ) ;
#17700 = ADVANCED_FACE ( 'NONE', ( #58049 ), #54732, .T. ) ;
#17701 = CARTESIAN_POINT ( 'NONE',  ( 11.16486084871730000, -2.792989229543000107, -7.174999999999999822 ) ) ;
#17702 = CARTESIAN_POINT ( 'NONE',  ( 25.30000327618300204, -8.756202924575998026, -7.455126447192999883 ) ) ;
#17703 = CARTESIAN_POINT ( 'NONE',  ( 2.309200955736999905, -2.649983027386999979, 2.425167579440000054 ) ) ;
#17704 = EDGE_LOOP ( 'NONE', ( #64986, #46169, #35936, #17513, #28066, #47590, #35018, #30416, #25068, #22448, #17805, #55550, #42277 ) ) ;
#17705 = COLOUR_RGB ( '', 0.72549020, 0.75294118, 0.79215686) ;
#17706 = CARTESIAN_POINT ( 'NONE',  ( 12.16008153508535194, -0.3287229608534210090, -12.59571550161850340 ) ) ;
#17707 = CARTESIAN_POINT ( 'NONE',  ( 12.08810207955109917, -4.796537143354000499, 7.825000000000000178 ) ) ;
#17708 = CARTESIAN_POINT ( 'NONE',  ( 11.09999999999999964, 5.538898460221000519, 7.685179721164000277 ) ) ;
#17709 = CARTESIAN_POINT ( 'NONE',  ( 8.630420280412000267, 5.808262417891000062, 7.446016144116000213 ) ) ;
#17710 = ORIENTED_EDGE ( 'NONE', *, *, #12794, .T. ) ;
#17711 = CARTESIAN_POINT ( 'NONE',  ( 6.558504020673000312, -0.8406263976572999619, -1.204107458873000081 ) ) ;
#17712 = CARTESIAN_POINT ( 'NONE',  ( 7.341410841227999917, 2.603491674958000157, -7.446887986542999549 ) ) ;
#17714 = CARTESIAN_POINT ( 'NONE',  ( 10.81499708368641954, 2.650004840405624673, -7.499999822193707644 ) ) ;
#17713 = DIRECTION ( 'NONE',  ( 1.000000000000000000, 0.000000000000000000, 0.000000000000000000 ) ) ;
#17715 = CARTESIAN_POINT ( 'NONE',  ( 10.97124174884019965, 3.963805917081910213, -8.815770025351000072 ) ) ;
#17716 = EDGE_LOOP ( 'NONE', ( #48417, #48142, #29612, #14839 ) ) ;
#17717 = CARTESIAN_POINT ( 'NONE',  ( 8.200000998245998929, 12.50000000000000000, 0.000000000000000000 ) ) ;
#17718 = EDGE_LOOP ( 'NONE', ( #68696, #44287, #52643, #53679, #20389 ) ) ;
#17719 = EDGE_CURVE ( 'NONE', #63101, #60029, #14728, .T. ) ;
#17720 = CARTESIAN_POINT ( 'NONE',  ( 16.39999999439439549, -3.511866690759578802, -11.95216930658972032 ) ) ;
#17721 = CARTESIAN_POINT ( 'NONE',  ( 10.84393020684979980, 2.750000000000000000, -7.500000000000000000 ) ) ;
#17722 = CARTESIAN_POINT ( 'NONE',  ( 18.15872407313727876, -0.1621987986621310773, -13.89873133405096794 ) ) ;
#17723 = ORIENTED_EDGE ( 'NONE', *, *, #46796, .F. ) ;
#17724 = CARTESIAN_POINT ( 'NONE',  ( 16.07905395910119850, -8.470000438687037558, -7.998963526368340737 ) ) ;
#17725 = CARTESIAN_POINT ( 'NONE',  ( 8.817462135714999150, -5.100000000000000533, 6.571291218949999902 ) ) ;
#17726 = CARTESIAN_POINT ( 'NONE',  ( 7.491064158769000336, 4.422660346525999486, -6.167928437610999737 ) ) ;
#17727 = LINE ( 'NONE', #39050, #17481 ) ;
#17728 = CARTESIAN_POINT ( 'NONE',  ( 5.377827132531639798, -0.3835239794964074300, 1.315189805302956927 ) ) ;
#17729 = VERTEX_POINT ( 'NONE', #30792 ) ;
#17730 = CARTESIAN_POINT ( 'NONE',  ( 6.555026506349999948, -1.500000000000000000, 0.000000000000000000 ) ) ;
#17731 = B_SPLINE_CURVE_WITH_KNOTS ( 'NONE', 3,
 ( #15626, #32741, #41849, #58271, #20868, #42885, #36957, #16307, #63155, #68400, #10373, #42206, #54057, #48475, #37293, #27154, #234, #58964 ),
 .UNSPECIFIED., .F., .F.,
 ( 4, 2, 2, 2, 2, 2, 2, 2, 4 ),
 ( 0.1494581667962512628, 0.2557758959467198445, 0.3620936250971884540, 0.4684113542476570080, 0.5747290833981256730, 0.6810468125485942270, 0.7873645416990627810, 0.8936822708495314460, 1.000000000000000000 ),
 .UNSPECIFIED. ) ;
#17732 = CARTESIAN_POINT ( 'NONE',  ( 24.32784151249200377, -12.60041493477000074, -3.144063045006000312 ) ) ;
#17733 = CARTESIAN_POINT ( 'NONE',  ( 16.10004050617000360, 8.286228349446574271, 9.446703038322560531 ) ) ;
#17734 = CARTESIAN_POINT ( 'NONE',  ( 12.80505043854146940, -3.248109929747638347, 13.61799478206225444 ) ) ;
#17735 = B_SPLINE_CURVE_WITH_KNOTS ( 'NONE', 3,
 ( #46570, #9491, #19302, #56374, #14072, #61611, #50787, #13727 ),
 .UNSPECIFIED., .F., .F.,
 ( 4, 2, 2, 4 ),
 ( 0.000000000000000000, 0.4999999999999993339, 0.7499999999999996669, 1.000000000000000000 ),
 .UNSPECIFIED. ) ;
#17736 = ORIENTED_EDGE ( 'NONE', *, *, #22270, .F. ) ;
#17737 = CARTESIAN_POINT ( 'NONE',  ( 25.34047077108162327, 2.680020306167191446, 11.33984167324305581 ) ) ;
#17738 = CIRCLE ( 'NONE', #36692, 0.6999999999999992895 ) ;
#17739 = CARTESIAN_POINT ( 'NONE',  ( 10.93499870985557010, 2.931393928242580937, 4.937945785150366085 ) ) ;
#17740 = CARTESIAN_POINT ( 'NONE',  ( 11.57299956498156845, 5.207010770456999893, -7.825000000000000178 ) ) ;
#17741 = FACE_OUTER_BOUND ( 'NONE', #6322, .T. ) ;
#17742 = CARTESIAN_POINT ( 'NONE',  ( 8.100000113405998903, -12.39999890530000037, 0.000000000000000000 ) ) ;
#17743 = VECTOR ( 'NONE', #58096, 1000.000000000000114 ) ;
#17744 = CARTESIAN_POINT ( 'NONE',  ( 5.815443173017626144, 1.499999999999999778, 0.1963495408493654004 ) ) ;
#17745 = CARTESIAN_POINT ( 'NONE',  ( 17.83364017334651308, -3.059569048391924451, 12.30342972110860345 ) ) ;
#17746 = ORIENTED_EDGE ( 'NONE', *, *, #43025, .T. ) ;
#17747 = CARTESIAN_POINT ( 'NONE',  ( 11.26212378248529866, -4.615095948180499619, -6.336291382830999908 ) ) ;
#17748 = ORIENTED_EDGE ( 'NONE', *, *, #44074, .T. ) ;
#17749 = CARTESIAN_POINT ( 'NONE',  ( 25.46375345652300126, 2.879422156700999658, -11.30951020355999859 ) ) ;
#17750 = CARTESIAN_POINT ( 'NONE',  ( 8.549914158773001205, 2.141799395716999843, -7.895788736628000848 ) ) ;
#17751 = CARTESIAN_POINT ( 'NONE',  ( 2.705986907149000142, 2.679358243340999923, -1.776962442616000004 ) ) ;
#17752 = CARTESIAN_POINT ( 'NONE',  ( 9.988720925027999797, -2.842024021884000273, -6.504330542082999322 ) ) ;
#17753 = CARTESIAN_POINT ( 'NONE',  ( 18.18005043799233178, 2.500000011518615395, -12.45159158845316405 ) ) ;
#17754 = DIRECTION ( 'NONE',  ( -0.7071067811865952013, -0.7071067811864951702, -8.251241205416942814E-08 ) ) ;
#17755 = EDGE_CURVE ( 'NONE', #46470, #1871, #4458, .T. ) ;
#17757 = EDGE_CURVE ( 'NONE', #66745, #54548, #12997, .T. ) ;
#17756 = CARTESIAN_POINT ( 'NONE',  ( 11.32299956498189886, 2.792989229543000107, 7.825000000000000178 ) ) ;
#17758 = ORIENTED_EDGE ( 'NONE', *, *, #30641, .T. ) ;
#17759 = CARTESIAN_POINT ( 'NONE',  ( 1.854719994300333408, -2.744941749261882169, -2.197574953528185215 ) ) ;
#17760 = ADVANCED_FACE ( 'NONE', ( #68869 ), #12316, .F. ) ;
#17761 = CARTESIAN_POINT ( 'NONE',  ( 10.97718582084299932, -4.656536239972400182, 8.258888014436699621 ) ) ;
#17762 = CARTESIAN_POINT ( 'NONE',  ( 10.43579914648999996, 2.587602126999999808, 6.390037244031000263 ) ) ;
#17763 = CARTESIAN_POINT ( 'NONE',  ( 10.27706886429732158, -2.899999999999999911, -6.444141223373538452 ) ) ;
#17764 = FACE_OUTER_BOUND ( 'NONE', #66585, .T. ) ;
#17765 = DIRECTION ( 'NONE',  ( 1.000000000000000000, 0.000000000000000000, 0.000000000000000000 ) ) ;
#17766 = CARTESIAN_POINT ( 'NONE',  ( 10.89979975933730039, 4.819074589197400726, -7.218192605361100078 ) ) ;
#17768 = CARTESIAN_POINT ( 'NONE',  ( 7.100000000000397549, 3.326107221750500997, -6.287467994316567221 ) ) ;
#17767 = CONTEXT_DEPENDENT_SHAPE_REPRESENTATION ( #31556, #42783 ) ;
#17769 = CARTESIAN_POINT ( 'NONE',  ( 9.960975701332998256, 4.837683410033799980, -8.275900091855099561 ) ) ;
#17770 = CARTESIAN_POINT ( 'NONE',  ( 23.99050544320700240, -9.436313469635999596, 9.573822194107998840 ) ) ;
#17771 = DIRECTION ( 'NONE',  ( 0.000000000000000000, 0.9999992323442526976, 0.001239076634196941903 ) ) ;
#17772 = ORIENTED_EDGE ( 'NONE', *, *, #49899, .T. ) ;
#17773 = CARTESIAN_POINT ( 'NONE',  ( 8.887168146795000112, -2.193670085072000120, 7.400591740205000768 ) ) ;
#17774 = CARTESIAN_POINT ( 'NONE',  ( 9.798320215454998205, -2.757678812098000254, -6.584768124342000206 ) ) ;
#17775 = CARTESIAN_POINT ( 'NONE',  ( 18.25665235842813061, 2.332587565413955399, 13.80433135817204970 ) ) ;
#17776 = CARTESIAN_POINT ( 'NONE',  ( 23.89320776801300283, -3.288740538444000716, 12.20874841465999516 ) ) ;
#17777 = CARTESIAN_POINT ( 'NONE',  ( 11.35502763632549872, -5.160433036184000066, -6.964545474268299508 ) ) ;
#17778 = ORIENTED_EDGE ( 'NONE', *, *, #10084, .F. ) ;
#17779 = CARTESIAN_POINT ( 'NONE',  ( 24.37899125153199975, 3.167412086455000164, -12.03697597459000157 ) ) ;
#17780 = CARTESIAN_POINT ( 'NONE',  ( 7.384454719589999883, 3.346262376537000094, 6.002251090845000192 ) ) ;
#17782 = CARTESIAN_POINT ( 'NONE',  ( 9.234200250017998712, -3.906155787512310074, 6.613277660092100163 ) ) ;
#17781 = CARTESIAN_POINT ( 'NONE',  ( 8.414360841228999632, 5.461114003844000031, -8.582501063019000398 ) ) ;
#17783 = CARTESIAN_POINT ( 'NONE',  ( 10.83487665876999984, 5.800192368099000184, -7.920541111170000370 ) ) ;
#17784 = ORIENTED_EDGE ( 'NONE', *, *, #56320, .F. ) ;
#17785 = CARTESIAN_POINT ( 'NONE',  ( 10.07770645819999977, 4.622041375574999833, 5.671348593713000596 ) ) ;
#17787 = CARTESIAN_POINT ( 'NONE',  ( 18.07920178076630435, -2.013390639430573170, -13.85446980737595979 ) ) ;
#17786 = VECTOR ( 'NONE', #66689, 1000.000000000000000 ) ;
#17788 = CARTESIAN_POINT ( 'NONE',  ( 11.68333460557258796, 4.162011815820000571, 6.509695444280099608 ) ) ;
#17789 = CARTESIAN_POINT ( 'NONE',  ( 9.409421956854998825, -2.113407700033000047, 7.914197133433000353 ) ) ;
#17790 = CARTESIAN_POINT ( 'NONE',  ( 8.898558059623999483, -5.146736128384000075, 6.597417125647000447 ) ) ;
#17791 = ORIENTED_EDGE ( 'NONE', *, *, #16333, .F. ) ;
#17792 = LINE ( 'NONE', #28631, #46690 ) ;
#17794 = CARTESIAN_POINT ( 'NONE',  ( 1.323890132541374998, -2.150913519912200478, -2.798833948393631754 ) ) ;
#17793 = CARTESIAN_POINT ( 'NONE',  ( 12.25978835901500119, -11.49417283396999956, 4.331891014347999835 ) ) ;
#17795 = CARTESIAN_POINT ( 'NONE',  ( 8.039320795308336542, -3.234825695714153238, 5.919796682457031167 ) ) ;
#17796 = CARTESIAN_POINT ( 'NONE',  ( 10.87021507563000000, -2.226042145532000305, 7.782753277595999997 ) ) ;
#17797 = CARTESIAN_POINT ( 'NONE',  ( 23.66565973993500194, 3.239486956716000066, 13.42552446105999842 ) ) ;
#17798 = CARTESIAN_POINT ( 'NONE',  ( 10.08198825978599977, -4.149395984695000372, 6.368003848175999515 ) ) ;
#17799 = ORIENTED_EDGE ( 'NONE', *, *, #43986, .T. ) ;
#17800 = CARTESIAN_POINT ( 'NONE',  ( 23.85847181463605438, -9.608971930760668911, 9.387888383478362186 ) ) ;
#17801 = CARTESIAN_POINT ( 'NONE',  ( 10.97303166480599934, -5.137916160623999140, 7.419769534118209720 ) ) ;
#17802 = ORIENTED_EDGE ( 'NONE', *, *, #6462, .T. ) ;
#17803 = ADVANCED_FACE ( 'NONE', ( #15742 ), #37070, .F. ) ;
#17804 = CARTESIAN_POINT ( 'NONE',  ( 10.12309687351566900, -2.782534154164605145, 7.172815144550900968 ) ) ;
#17805 = ORIENTED_EDGE ( 'NONE', *, *, #14134, .T. ) ;
#17806 = B_SPLINE_SURFACE_WITH_KNOTS ( 'NONE', 3, 3, ( 
 ( #67381, #45050, #46075, #8671 ),
 ( #18826, #18134, #40152, #61466 ),
 ( #39456, #14266, #3073, #45736 ),
 ( #56906, #34905, #3751, #50977 ),
 ( #60775, #8331, #29674, #67045 ),
 ( #9005, #13923, #30348, #56564 ),
 ( #55539, #2391, #3414, #24750 ),
 ( #4783, #30683, #52687, #67722 ),
 ( #14605, #4096, #31375, #47805 ) ),
 .UNSPECIFIED., .F., .F., .F.,
 ( 4, 1, 1, 1, 1, 1, 4 ),
 ( 4, 4 ),
 ( 0.05182816266979999725, 0.1666666666667000196, 0.3333333333333000081, 0.5000000000000000000, 0.6666666666667000474, 0.8333333333333000637, 0.9772240888782000034 ),
 ( -0.1900389547208000129, 1.190219847277000031 ),
 .UNSPECIFIED. ) ;
#17807 = CARTESIAN_POINT ( 'NONE',  ( 9.972410841228999345, 4.357364160690000432, -9.282962013144999247 ) ) ;
#17808 = EDGE_CURVE ( 'NONE', #31101, #63766, #51388, .T. ) ;
#17809 = CARTESIAN_POINT ( 'NONE',  ( 24.32840188601700149, 12.59971520604000084, -3.143741918347000119 ) ) ;
#17810 = CARTESIAN_POINT ( 'NONE',  ( 11.12299956498149811, 5.207010770456999893, 7.174999999999999822 ) ) ;
#17811 = CARTESIAN_POINT ( 'NONE',  ( 12.09872039853181036, 2.644866564252636110, -12.31930286224045368 ) ) ;
#17812 = CARTESIAN_POINT ( 'NONE',  ( 11.56456920625009843, -3.962850971080120299, 8.532838639935999225 ) ) ;
#17813 = ORIENTED_EDGE ( 'NONE', *, *, #6609, .T. ) ;
#17814 = DIRECTION ( 'NONE',  ( 0.000000000000000000, 1.000000000000000000, 0.000000000000000000 ) ) ;
#17815 = ORIENTED_EDGE ( 'NONE', *, *, #21684, .F. ) ;
#17816 = CARTESIAN_POINT ( 'NONE',  ( 7.919004440377000797, -5.361050935357000391, 6.973449182446000094 ) ) ;
#17817 = DIRECTION ( 'NONE',  ( 0.000000000000000000, -1.099932466989999959E-09, 1.000000000000000000 ) ) ;
#17818 = ORIENTED_EDGE ( 'NONE', *, *, #40724, .T. ) ;
#17819 = B_SPLINE_SURFACE_WITH_KNOTS ( 'NONE', 1, 3, ( 
 ( #58403, #31847, #3539, #57712, #46206, #67513, #62278, #14396, #57032, #31168, #30470, #14733, #36049, #57366, #19980, #41302, #9820, #9470, #30812, #4227, #25564, #20314, #54543, #65007, #53848, #64318, #22024, #17126, #48954, #38809, #22717, #26603, #27288, #48257, #48608, #713, #26945, #365, #21679, #43372, #43014, #32875, #16439, #5945, #59092, #17486, #11533, #32195, #47924, #5599, #37768, #32533, #38461, #16776, #5263, #59433, #6286, #27981, #11195, #10851, #16098, #53163, #64671, #38107, #54187, #53510, #27633, #1063, #1400, #11884, #33221, #22374, #60134, #43713, #59780, #6640, #22, #12243, #49289, #44065, #65366, #21342, #42672, #58746, #63979, #37423, #29028, #39849, #51024, #34616, #3123, #49992, #55929, #23762, #49640, #18525, #33569, #2781, #61514, #8378, #7332, #6989, #40197, #2434 ),
 ( #40525, #56268, #45097, #34954, #8031, #45440, #66406, #29369, #12935, #7687, #50684, #24454, #1746, #23067, #66752, #44415, #2103, #55234, #18869, #54888, #23420, #13291, #28675, #13629, #45779, #61170, #65715, #19202, #29721, #44756, #39155, #24107, #67090, #61851, #28319, #17836, #60479, #12587, #33916, #66059, #18179, #39501, #60824, #34262, #55584, #50337, #51363, #20232, #52037, #31418, #20573, #52734, #30390, #15335, #25821, #14650, #25134, #4140, #47151, #9732, #68801, #4829, #56612, #57281, #9051, #9385, #30730, #56952, #46466, #51700, #31081, #67767, #4481, #30061, #8718, #19893, #3797, #20922, #36663, #25476, #57983, #36312, #68451, #46808, #14985, #62531, #68114, #57629, #26171, #3458, #24795, #41899, #46121, #41220, #35640, #63206, #13968, #35966, #62867, #41557, #10080, #47496, #52386, #67427 ) ),
 .UNSPECIFIED., .F., .F., .F.,
 ( 2, 2 ),
 ( 4, 2, 2, 2, 2, 2, 2, 2, 2, 2, 2, 2, 2, 2, 2, 2, 2, 2, 2, 2, 2, 2, 2, 2, 2, 2, 2, 2, 2, 2, 2, 2, 2, 2, 2, 2, 2, 2, 2, 2, 2, 2, 2, 2, 2, 2, 2, 2, 2, 2, 2, 4 ),
 ( 0.000000000000000000, 1.000000000000000000 ),
 ( 0.000000000000000000, 7.157017711320847928E-05, 0.0001431403542264169586, 0.0002147105313396254378, 0.0002326030756179275644, 0.0002504956198962296639, 0.0002862807084528339171, 0.0003220657970094381703, 0.0003578508855660424235, 0.0003936359741226466225, 0.0004294210626792508757, 0.0004652061512358551289, 0.0005009912397924593279, 0.0005367763283490635268, 0.0005725614169056678342, 0.0006441315940188763406, 0.0006799166825754805396, 0.0007157017711320848470, 0.0007335943154103870007, 0.0007514868596886890460, 0.0007872719482452932450, 0.0008588421253585017514, 0.0008946272139151059503, 0.0009304123024717102577, 0.0009661973910283144567, 0.001001982479584918656, 0.001073552656698127054, 0.001145122833811335668, 0.001216693010924544283, 0.001288263188037752681, 0.001359833365150961079, 0.001395618453707565387, 0.001431403542264169694, 0.001467188630820774001, 0.001502973719377378092, 0.001574543896490586490, 0.001646114073603795105, 0.001681899162160399412, 0.001717684250717003503, 0.001735576794995305656, 0.001753469339273607593, 0.001789254427830211901, 0.001860824604943420515, 0.001896609693500024823, 0.001932394782056628913, 0.001968179870613233004, 0.001986072414891535375, 0.002003964959169837311, 0.002075535136283045493, 0.002147105313396254107, 0.002218675490509462722, 0.002290245667622671337 ),
 .UNSPECIFIED. ) ;
#17820 = CARTESIAN_POINT ( 'NONE',  ( 12.09902206169136818, -2.644659774828333365, -12.31933076163361029 ) ) ;
#17821 = CARTESIAN_POINT ( 'NONE',  ( 10.66995391537419913, 4.943675741382899780, 6.859089544950699668 ) ) ;
#17822 = CARTESIAN_POINT ( 'NONE',  ( 10.41839555962000041, -4.531908721143000029, -9.270473926467998282 ) ) ;
#17823 = CARTESIAN_POINT ( 'NONE',  ( 10.95552360838999917, 4.744046441415999738, -9.198140387677000263 ) ) ;
#17824 = CARTESIAN_POINT ( 'NONE',  ( 18.45060561202799931, -11.83531674184000160, 3.931800577755000248 ) ) ;
#17825 = CARTESIAN_POINT ( 'NONE',  ( 8.079724940884622342, -4.352763894256449717, 8.815588961479031482 ) ) ;
#17826 = CARTESIAN_POINT ( 'NONE',  ( 5.500000000000000000, -11.95749337870000062, 3.642574926947999892 ) ) ;
#17827 = CARTESIAN_POINT ( 'NONE',  ( 18.06356912472852372, -0.3639343692979916667, -12.69299665021505419 ) ) ;
#17828 = CARTESIAN_POINT ( 'NONE',  ( 6.899999691988000450, -12.20988339176000004, 3.111064831549000154 ) ) ;
#17829 = CARTESIAN_POINT ( 'NONE',  ( 10.17764828895399809, -2.998858038575999974, -8.046814291299300592 ) ) ;
#17830 = CARTESIAN_POINT ( 'NONE',  ( 1.849999551004999798, 0.000000000000000000, 0.000000000000000000 ) ) ;
#17831 = VERTEX_POINT ( 'NONE', #41283 ) ;
#17832 = CARTESIAN_POINT ( 'NONE',  ( 23.56666365135700403, -11.61524011578000604, 3.333188920255001353 ) ) ;
#17833 = CARTESIAN_POINT ( 'NONE',  ( 16.09992084546400193, -8.991497430826001391, -8.719551690569000257 ) ) ;
#17834 = CARTESIAN_POINT ( 'NONE',  ( 10.12671450658999994, 3.117528978489000124, 8.613535509676999880 ) ) ;
#17835 = CARTESIAN_POINT ( 'NONE',  ( 10.72303311070000120, 3.890114357827999747, -8.859327677199999584 ) ) ;
#17836 = CARTESIAN_POINT ( 'NONE',  ( 18.07985789204853688, 2.160546346826199837, 12.52419258880425446 ) ) ;
#17837 = CARTESIAN_POINT ( 'NONE',  ( 13.50000000000303224, -9.278109357271722146, -7.623553959385361622 ) ) ;
#17839 = EDGE_CURVE ( 'NONE', #17921, #33287, #50505, .T. ) ;
#17838 = CARTESIAN_POINT ( 'NONE',  ( 9.781673028307999118, 5.464749740720999505, 8.817329433105999925 ) ) ;
#17840 = CARTESIAN_POINT ( 'NONE',  ( 10.68940772478662637, -4.553612660159668479, 6.822471183635139269 ) ) ;
#17841 = EDGE_CURVE ( 'NONE', #36843, #56572, #23881, .T. ) ;
#17842 = CARTESIAN_POINT ( 'NONE',  ( 8.768793171737998549, 3.595811914175000013, 6.625874414451000227 ) ) ;
#17843 = EDGE_CURVE ( 'NONE', #44736, #3420, #53843, .T. ) ;
#17844 = ORIENTED_EDGE ( 'NONE', *, *, #22639, .T. ) ;
#17845 = CARTESIAN_POINT ( 'NONE',  ( 12.33364759508191355, -3.027124203391260870, 12.23096800428945841 ) ) ;
#17846 = CARTESIAN_POINT ( 'NONE',  ( 10.13425461470299993, -4.840245908677600184, -7.713763321667399531 ) ) ;
#17847 = CARTESIAN_POINT ( 'NONE',  ( 24.46729256464000457, -3.339593025236999857, -12.12065414616999881 ) ) ;
#17848 = CARTESIAN_POINT ( 'NONE',  ( 8.434600867921000500, -5.100000003633000212, 6.577466067358000323 ) ) ;
#17849 = CARTESIAN_POINT ( 'NONE',  ( 11.05964426047339799, 4.687693494822500639, -8.577215873335999774 ) ) ;
#17850 = CARTESIAN_POINT ( 'NONE',  ( 12.57154173166082956, -0.6810629908226978335, 12.58158054216573518 ) ) ;
#17851 = CARTESIAN_POINT ( 'NONE',  ( 7.919010841228001141, 5.361039412362000434, 6.973453640356000349 ) ) ;
#17852 = CARTESIAN_POINT ( 'NONE',  ( 10.71256887705999894, 5.951815279772000089, 7.233043586354999555 ) ) ;
#17853 = CARTESIAN_POINT ( 'NONE',  ( 12.78086743291007821, 1.761210985583066213, 12.47630298729255571 ) ) ;
#17854 = ORIENTED_EDGE ( 'NONE', *, *, #49130, .T. ) ;
#17855 = CARTESIAN_POINT ( 'NONE',  ( 9.295789158775001226, 5.835196551504000517, -7.008466539623000813 ) ) ;
#17856 = CARTESIAN_POINT ( 'NONE',  ( 11.08425954179440076, 4.982976321082899673, -8.316745941391600283 ) ) ;
#17857 = B_SPLINE_CURVE_WITH_KNOTS ( 'NONE', 3,
 ( #61734, #13855, #56496, #8600, #46006, #29950, #56845, #51253, #35523, #8943 ),
 .UNSPECIFIED., .F., .F.,
 ( 4, 2, 2, 2, 4 ),
 ( 0.1324350869623206473, 0.3493263152217405132, 0.5662175434811602681, 0.7831087717405801341, 1.000000000000000000 ),
 .UNSPECIFIED. ) ;
#17858 = ADVANCED_FACE ( 'NONE', ( #22004 ), #11175, .T. ) ;
#17859 = FACE_OUTER_BOUND ( 'NONE', #33088, .T. ) ;
#17861 = CARTESIAN_POINT ( 'NONE',  ( 24.99828551773858010, 11.48454095403716124, 3.234327495894459670 ) ) ;
#17860 = CARTESIAN_POINT ( 'NONE',  ( 11.53159663549335967, -3.486713160360387143, 11.11613240505404754 ) ) ;
#17862 = CARTESIAN_POINT ( 'NONE',  ( 10.10932996542199902, -4.697624103824200148, 6.777391592843399870 ) ) ;
#17863 = CARTESIAN_POINT ( 'NONE',  ( 11.44133594839949986, -3.430493414882899827, -6.847343244997600387 ) ) ;
#17864 = ORIENTED_EDGE ( 'NONE', *, *, #12080, .T. ) ;
#17865 = B_SPLINE_CURVE_WITH_KNOTS ( 'NONE', 3,
 ( #37772, #6292, #15765, #38111, #10512, #21349, #48614, #5269, #21685, #59437, #59785, #58750, #48958, #32202, #717, #47928, #369, #11199 ),
 .UNSPECIFIED., .F., .F.,
 ( 4, 2, 2, 2, 2, 2, 2, 2, 4 ),
 ( 0.000000000000000000, 0.1250000000000000000, 0.2500000000000000000, 0.3750000000000000000, 0.5000000000000000000, 0.6250000000000000000, 0.7500000000000000000, 0.8750000000000000000, 1.000000000000000000 ),
 .UNSPECIFIED. ) ;
#17866 = CARTESIAN_POINT ( 'NONE',  ( 2.290900752179999778, 2.610776529918000133, -2.002676742402000443 ) ) ;
#17867 = CARTESIAN_POINT ( 'NONE',  ( 23.74396121059458409, -9.837233145174325344, -9.448860444549127990 ) ) ;
#17868 = DIRECTION ( 'NONE',  ( 0.000000000000000000, 1.000000000000000000, -1.181194934447000133E-14 ) ) ;
#17869 = CARTESIAN_POINT ( 'NONE',  ( 6.999999691988000095, -12.49999909016000110, 4.774434232535999529E-10 ) ) ;
#17870 = CARTESIAN_POINT ( 'NONE',  ( 17.55505043854144276, -0.6250000000000001110, -12.67928921589118474 ) ) ;
#17871 = CARTESIAN_POINT ( 'NONE',  ( 12.43914160838493821, -1.887194142572512945, 13.87222517180307690 ) ) ;
#17872 = DIRECTION ( 'NONE',  ( -1.000000000000000000, 0.000000000000000000, 0.000000000000000000 ) ) ;
#17873 = DIRECTION ( 'NONE',  ( 0.000000000000000000, 1.000000000000000000, 0.000000000000000000 ) ) ;
#17874 = CARTESIAN_POINT ( 'NONE',  ( 13.55309301929700005, -12.11670754034000019, -2.533073449765999907 ) ) ;
#17875 = EDGE_LOOP ( 'NONE', ( #48059, #27321, #9198, #61713 ) ) ;
#17876 = CARTESIAN_POINT ( 'NONE',  ( 10.31021345716899873, -3.363461959113699606, -8.078719053813800954 ) ) ;
#17877 = LINE ( 'NONE', #60517, #2513 ) ;
#17878 = CARTESIAN_POINT ( 'NONE',  ( 18.15919096721171400, 2.338588349694056490, -13.70638546470270214 ) ) ;
#17879 = CARTESIAN_POINT ( 'NONE',  ( 3.400000000000000355, 0.000000000000000000, 0.000000000000000000 ) ) ;
#17880 = CARTESIAN_POINT ( 'NONE',  ( 10.76537527815838580, -5.100000000000000533, 6.445686799303629755 ) ) ;
#17881 = ORIENTED_EDGE ( 'NONE', *, *, #23214, .F. ) ;
#17882 = CARTESIAN_POINT ( 'NONE',  ( 23.58333423472800305, -7.629452625224000015E-13, 2.908784324518000003E-13 ) ) ;
#17883 = CARTESIAN_POINT ( 'NONE',  ( 17.96249544862750369, 2.025954803622692868, -12.54949280001588896 ) ) ;
#17884 = CARTESIAN_POINT ( 'NONE',  ( 10.12671450658999994, 3.117528978489000124, 8.613535509676999880 ) ) ;
#17885 = CARTESIAN_POINT ( 'NONE',  ( 10.65364694612719809, 3.195501139158400061, 7.178938988280099132 ) ) ;
#17886 = B_SPLINE_CURVE_WITH_KNOTS ( 'NONE', 3,
 ( #59673, #1638, #6529, #22952, #44307, #42907, #53400, #37315, #26835, #16672, #7226, #24341, #13856, #35184, #61401, #12473, #8260, #28563 ),
 .UNSPECIFIED., .F., .F.,
 ( 4, 2, 2, 2, 2, 2, 2, 2, 4 ),
 ( 0.000000000000000000, 0.1250000000000003331, 0.2500000000000006661, 0.3750000000000009992, 0.5000000000000013323, 0.6250000000000009992, 0.7500000000000006661, 0.8750000000000003331, 1.000000000000000000 ),
 .UNSPECIFIED. ) ;
#17887 = B_SPLINE_CURVE_WITH_KNOTS ( 'NONE', 3,
 ( #1518, #48728, #6753, #60253, #44873 ),
 .UNSPECIFIED., .F., .F.,
 ( 4, 1, 4 ),
 ( 0.000000000000000000, 0.5000000000000000000, 1.000000000000000000 ),
 .UNSPECIFIED. ) ;
#17888 = DIRECTION ( 'NONE',  ( -1.000000000000000000, 0.000000000000000000, 0.000000000000000000 ) ) ;
#17889 = CARTESIAN_POINT ( 'NONE',  ( 10.19794194037999979, -4.262172867567000090, -8.834326937932999613 ) ) ;
#17890 = EDGE_CURVE ( 'NONE', #33549, #26364, #22138, .T. ) ;
#17891 = CARTESIAN_POINT ( 'NONE',  ( 17.92038287126899121, 0.6379138416578098436, -13.98550699733554303 ) ) ;
#17892 = CARTESIAN_POINT ( 'NONE',  ( 24.26733149983100191, 12.18172987844000055, 3.303689625207000269 ) ) ;
#17893 = CARTESIAN_POINT ( 'NONE',  ( 12.24260341319699918, -2.772876882430816536, 12.38382274645855041 ) ) ;
#17894 = ORIENTED_EDGE ( 'NONE', *, *, #36467, .T. ) ;
#17895 = CARTESIAN_POINT ( 'NONE',  ( 9.243110841233001196, 4.112741311853999271, -5.603466076760000192 ) ) ;
#17896 = EDGE_LOOP ( 'NONE', ( #13539, #53047, #23125, #41510 ) ) ;
#17897 = CARTESIAN_POINT ( 'NONE',  ( 17.86985707050058636, -3.040024008573237069, 13.54397559521889605 ) ) ;
#17898 = CARTESIAN_POINT ( 'NONE',  ( 5.500000000000000000, 0.8000000000000000444, -3.149999999999999911 ) ) ;
#17899 = ORIENTED_EDGE ( 'NONE', *, *, #10436, .T. ) ;
#17900 = CARTESIAN_POINT ( 'NONE',  ( 10.93479632507519916, 4.557787252275099732, 6.465962698293999722 ) ) ;
#17901 = CARTESIAN_POINT ( 'NONE',  ( 5.841441374307528633, -1.121062338676339865, -0.1678582702746748423 ) ) ;
#17902 = CARTESIAN_POINT ( 'NONE',  ( 12.80505043854143388, 3.124999999999999556, -12.28374638332999602 ) ) ;
#17903 = CARTESIAN_POINT ( 'NONE',  ( 9.380783851237000093, 2.204242311415999911, 7.545378292079000460 ) ) ;
#17904 = DIRECTION ( 'NONE',  ( 1.000000000000000000, 0.000000000000000000, 0.000000000000000000 ) ) ;
#17905 = CARTESIAN_POINT ( 'NONE',  ( 10.82101354018304207, -4.768183399968640934, 8.499583552997727054 ) ) ;
#17906 = CARTESIAN_POINT ( 'NONE',  ( 11.72781722417300188, 3.253150999210000283, -11.33706231867000014 ) ) ;
#17907 = CARTESIAN_POINT ( 'NONE',  ( 10.90421209872000041, -3.863781031729999871, -9.185081053980001187 ) ) ;
#17908 = CARTESIAN_POINT ( 'NONE',  ( 3.999999999999999112, -1.719326598156197150, -1.321078631445046669 ) ) ;
#17909 = CARTESIAN_POINT ( 'NONE',  ( 25.30000327618300204, 8.756202924575998026, 7.455126447192999883 ) ) ;
#17910 = EDGE_LOOP ( 'NONE', ( #18101, #19663, #50793, #29860 ) ) ;
#17911 = AXIS2_PLACEMENT_3D ( 'NONE', #58382, #51765, #47566 ) ;
#17912 = CARTESIAN_POINT ( 'NONE',  ( 9.893930206848997599, 2.750000000000000000, 7.500000000000000000 ) ) ;
#17913 = SURFACE_STYLE_FILL_AREA ( #65788 ) ;
#17914 = B_SPLINE_CURVE_WITH_KNOTS ( 'NONE', 3,
 ( #10046, #68076, #24759, #68417 ),
 .UNSPECIFIED., .F., .F.,
 ( 4, 4 ),
 ( 0.000000000000000000, 1.000000000000000000 ),
 .UNSPECIFIED. ) ;
#17915 = CARTESIAN_POINT ( 'NONE',  ( 10.76874784196215629, 3.036568074332222089, -4.838413581444926059 ) ) ;
#17916 = CARTESIAN_POINT ( 'NONE',  ( 10.68674208995000008, -5.041113534315000422, 5.111026935337999788 ) ) ;
#17917 = CARTESIAN_POINT ( 'NONE',  ( 8.599999952505998024, -4.749999993641800700, -7.500000000000000000 ) ) ;
#17918 = CARTESIAN_POINT ( 'NONE',  ( 17.60000000024299993, 11.86189249994999884, -3.298671769835999967 ) ) ;
#17919 = CARTESIAN_POINT ( 'NONE',  ( 12.27233953995986582, 2.172968329541575372, 13.73735571485410745 ) ) ;
#17920 = CARTESIAN_POINT ( 'NONE',  ( 10.44675369521999997, -2.885048926231000177, 8.863479194807000638 ) ) ;
#17921 = VERTEX_POINT ( 'NONE', #42653 ) ;
#17922 = CARTESIAN_POINT ( 'NONE',  ( 7.850909765600520451, 2.904933541014710130, -6.663705336267816470 ) ) ;
#17923 = EDGE_CURVE ( 'NONE', #54822, #34817, #1341, .T. ) ;
#17924 = CARTESIAN_POINT ( 'NONE',  ( 12.60420804235854675, -0.5919407257947376655, 13.88303015925714590 ) ) ;
#17925 = EDGE_CURVE ( 'NONE', #65484, #53853, #27608, .T. ) ;
#17926 = ORIENTED_EDGE ( 'NONE', *, *, #60057, .T. ) ;
#17927 = DIRECTION ( 'NONE',  ( 1.000000000000000000, 0.000000000000000000, 0.000000000000000000 ) ) ;
#17928 = CARTESIAN_POINT ( 'NONE',  ( 17.56468935039100288, 12.04942594313000015, -3.198374858544000165 ) ) ;
#17929 = CARTESIAN_POINT ( 'NONE',  ( 8.846962924124625260, 4.841836872161519700, 7.261582451272839300 ) ) ;
#17930 = CYLINDRICAL_SURFACE ( 'NONE', #54022, 0.5000000000000002220 ) ;
#17931 = CARTESIAN_POINT ( 'NONE',  ( 9.436104719595000745, 5.619431609641999614, -8.115423117607999615 ) ) ;
#17932 = CARTESIAN_POINT ( 'NONE',  ( 9.979346873516126593, 4.163624617374466652, -8.749999999999998224 ) ) ;
#17933 = CARTESIAN_POINT ( 'NONE',  ( 11.11264194660999927, -2.146089039267000231, -7.517188649391000510 ) ) ;
#17934 = CARTESIAN_POINT ( 'NONE',  ( 10.90000668870999867, -1.199999999999999956, -9.776630298829998011 ) ) ;
#17935 = CARTESIAN_POINT ( 'NONE',  ( 10.90000000000000036, -1.199999999999999956, 9.776630298829998011 ) ) ;
#17936 = DIRECTION ( 'NONE',  ( 0.000000000000000000, 1.000000000000000000, 0.000000000000000000 ) ) ;
#17937 = CARTESIAN_POINT ( 'NONE',  ( 9.392147628284998717, -2.890602650755999647, -6.682694598879999504 ) ) ;
#17938 = CARTESIAN_POINT ( 'NONE',  ( 11.04749144726329924, 3.499163784537000055, -6.793273974143599681 ) ) ;
#17939 = CARTESIAN_POINT ( 'NONE',  ( 1.146806799208750061, -0.9161175952574931447, 3.408904368339100710 ) ) ;
#17940 = CARTESIAN_POINT ( 'NONE',  ( 11.10101463001529964, 4.622233839778099984, -6.503413421344399481 ) ) ;
#17941 = EDGE_CURVE ( 'NONE', #5127, #24516, #21239, .T. ) ;
#17942 = CARTESIAN_POINT ( 'NONE',  ( 9.381367640780998940, 4.473477001189199775, -6.614188603779100006 ) ) ;
#17944 = CARTESIAN_POINT ( 'NONE',  ( 10.54700110996000006, -2.946846751162999656, 4.944912775081999889 ) ) ;
#17943 = CARTESIAN_POINT ( 'NONE',  ( 10.43162143724499913, -3.424116261072899903, 8.148124882831599081 ) ) ;
#17945 = CARTESIAN_POINT ( 'NONE',  ( 7.443695762906002322, -3.525420668437998728, 6.642224720921002579 ) ) ;
#17946 = ORIENTED_EDGE ( 'NONE', *, *, #15270, .T. ) ;
#17947 = EDGE_CURVE ( 'NONE', #34052, #65107, #61411, .T. ) ;
#17948 = VECTOR ( 'NONE', #18275, 1000.000000000000114 ) ;
#17949 = CARTESIAN_POINT ( 'NONE',  ( 10.51925056272499859, 5.174767082365999471, 7.482589369563879877 ) ) ;
#17950 = CARTESIAN_POINT ( 'NONE',  ( 9.013429960698999821, -4.933961117404000341, 8.417889755737999025 ) ) ;
#17951 = CARTESIAN_POINT ( 'NONE',  ( 9.986304848515999311, 5.038423216181000086, 7.025224608805800131 ) ) ;
#17952 = CARTESIAN_POINT ( 'NONE',  ( 10.64393020684969926, -2.750000000000000000, -7.500000000000000000 ) ) ;
#17953 = B_SPLINE_CURVE_WITH_KNOTS ( 'NONE', 3,
 ( #11557, #6313, #47142, #15324, #36650, #47835, #274, #63889, #26856, #20563, #32441, #10412, #31070, #31754 ),
 .UNSPECIFIED., .F., .F.,
 ( 4, 2, 2, 2, 2, 2, 4 ),
 ( 0.000000000000000000, 0.1250000000000049682, 0.2500000000000099365, 0.5000000000000114353, 0.6250000000000086597, 0.7500000000000056621, 1.000000000000000000 ),
 .UNSPECIFIED. ) ;
#17954 = CARTESIAN_POINT ( 'NONE',  ( 9.034116535116000435, -4.695350938297000454, 8.660677768253002284 ) ) ;
#17955 = LINE ( 'NONE', #12356, #37499 ) ;
#17956 = FACE_OUTER_BOUND ( 'NONE', #5881, .T. ) ;
#17957 = ORIENTED_EDGE ( 'NONE', *, *, #10783, .T. ) ;
#17958 = VECTOR ( 'NONE', #11294, 1000.000000000000114 ) ;
#17959 = CARTESIAN_POINT ( 'NONE',  ( 10.18144474310099845, -2.984290294633999974, -7.992914665944799602 ) ) ;
#17960 = FACE_OUTER_BOUND ( 'NONE', #61017, .T. ) ;
#17961 = CARTESIAN_POINT ( 'NONE',  ( 5.822692947599000135, 1.526675769738000010, -0.5259243426933000176 ) ) ;
#17962 = CARTESIAN_POINT ( 'NONE',  ( 9.065585557054992805, -2.892971862670999705, -6.682168649839002939 ) ) ;
#17963 = CARTESIAN_POINT ( 'NONE',  ( 8.849999778957998942, -4.000000000000000000, -8.499999833805500060 ) ) ;
#17964 = CARTESIAN_POINT ( 'NONE',  ( 12.11364291764652990, -4.859654669415900408, 7.606265891492399511 ) ) ;
#17965 = CARTESIAN_POINT ( 'NONE',  ( 11.33872066707849768, 4.858611803369300652, -6.980638253271099103 ) ) ;
#17966 = CARTESIAN_POINT ( 'NONE',  ( 12.23350478622814741, 2.246345293432832513, -13.72400836783244849 ) ) ;
#17967 = CARTESIAN_POINT ( 'NONE',  ( 9.776078604427999252, -4.565692099013000771, -8.879633571423999783 ) ) ;
#17968 = CARTESIAN_POINT ( 'NONE',  ( 6.999998782146999332, 11.95749337870000062, -3.642574926947999892 ) ) ;
#17969 = ORIENTED_EDGE ( 'NONE', *, *, #15530, .T. ) ;
#17970 = CARTESIAN_POINT ( 'NONE',  ( 0.000000000000000000, -2.319305672483364056, -1.781768641235244921 ) ) ;
#17971 = CARTESIAN_POINT ( 'NONE',  ( 12.47502503668309615, 0.5311540453515636306, -13.88634387573209494 ) ) ;
#17972 = CARTESIAN_POINT ( 'NONE',  ( 13.80679720086500062, -8.861764092194999165, -7.504495031742999700 ) ) ;
#17973 = CARTESIAN_POINT ( 'NONE',  ( 11.56914347478616634, 4.748726180097643912, -8.529874251157636422 ) ) ;
#17974 = DIRECTION ( 'NONE',  ( 1.000000000000000000, 0.000000000000000000, 0.000000000000000000 ) ) ;
#17975 = CARTESIAN_POINT ( 'NONE',  ( 7.000000000000001776, 8.872191283697411279, 4.648286939382654026 ) ) ;
#17976 = CARTESIAN_POINT ( 'NONE',  ( 13.73494720760600174, 12.32760134815999997, 2.421442066891999811 ) ) ;
#17977 = ORIENTED_EDGE ( 'NONE', *, *, #61009, .F. ) ;
#17978 = FILL_AREA_STYLE ('',( #44562 ) ) ;
#17979 = CARTESIAN_POINT ( 'NONE',  ( 17.84567419427290602, 3.186977498899956185, -13.63243182350604243 ) ) ;
#17980 = ORIENTED_EDGE ( 'NONE', *, *, #3689, .T. ) ;
#17981 = CARTESIAN_POINT ( 'NONE',  ( 10.44079553769483404, -5.100000000000000533, 6.662590550628412878 ) ) ;
#17982 = CARTESIAN_POINT ( 'NONE',  ( 18.06247470437139313, 3.164801830692924867, 11.41978211458705950 ) ) ;
#17983 = CARTESIAN_POINT ( 'NONE',  ( 8.456370280410999030, 2.836879604150999601, -8.783908972046001296 ) ) ;
#17984 = CARTESIAN_POINT ( 'NONE',  ( 24.67921139482200132, 8.727627377900999406, -9.158314240160001063 ) ) ;
#17985 = CARTESIAN_POINT ( 'NONE',  ( 18.18005043854144276, 0.000000000000000000, -25.00000000000000000 ) ) ;
#17986 = CARTESIAN_POINT ( 'NONE',  ( 18.04535692659925417, 0.3877536850257900514, -12.69203640188974447 ) ) ;
#17987 = AXIS2_PLACEMENT_3D ( 'NONE', #17249, #39615, #23875 ) ;
#17988 = CARTESIAN_POINT ( 'NONE',  ( 11.05833333333536928, -2.548905579444654901, 7.980400043918773889 ) ) ;
#17989 = EDGE_LOOP ( 'NONE', ( #14867, #63456 ) ) ;
#17990 = CARTESIAN_POINT ( 'NONE',  ( 8.856851002545001350, 2.832432432432000269, -6.822293592207000934 ) ) ;
#17991 = DIRECTION ( 'NONE',  ( 1.000000000000000000, 0.000000000000000000, 0.000000000000000000 ) ) ;
#17992 = CARTESIAN_POINT ( 'NONE',  ( 6.950000000000000178, 5.221516520829000640, -8.074802043613001246 ) ) ;
#17993 = ORIENTED_EDGE ( 'NONE', *, *, #51651, .F. ) ;
#17994 = CARTESIAN_POINT ( 'NONE',  ( 10.14584353048000054, 5.370502454907000178, -6.826221644974000746 ) ) ;
#17995 = CARTESIAN_POINT ( 'NONE',  ( 11.01267610329000135, -8.059176674844000132, 6.866686629167999101 ) ) ;
#17996 = VERTEX_POINT ( 'NONE', #27266 ) ;
#17997 = CARTESIAN_POINT ( 'NONE',  ( 8.976101285863999024, 3.353260484332500013, 8.268485718282699182 ) ) ;
#17998 = B_SPLINE_CURVE_WITH_KNOTS ( 'NONE', 1,
 ( #12833, #19099 ),
 .UNSPECIFIED., .F., .F.,
 ( 2, 2 ),
 ( 0.000000000000000000, 1.000000000000000000 ),
 .UNSPECIFIED. ) ;
#17999 = CARTESIAN_POINT ( 'NONE',  ( 18.02766945781921137, -1.934589073148406779, -12.45059934707292548 ) ) ;
#18000 = CIRCLE ( 'NONE', #34721, 12.84999890301999947 ) ;
#18001 = DIRECTION ( 'NONE',  ( 0.7660444348520201174, 3.621652213051094873E-11, 0.6427876195387159930 ) ) ;
#18002 = CARTESIAN_POINT ( 'NONE',  ( 24.62769666374738620, -3.584151135392908305, -12.19978398752706106 ) ) ;
#18003 = CARTESIAN_POINT ( 'NONE',  ( 10.27427156480999848, -4.600000212792999754, 4.944156960788000710 ) ) ;
#18004 = AXIS2_PLACEMENT_3D ( 'NONE', #8224, #3312, #56112 ) ;
#18005 = CARTESIAN_POINT ( 'NONE',  ( 9.712659112603999390, 3.623260508844300176, 6.719118894894999805 ) ) ;
#18006 = EDGE_CURVE ( 'NONE', #33549, #9331, #5548, .T. ) ;
#18007 = CARTESIAN_POINT ( 'NONE',  ( 9.351982841559774329, -3.410536830733829294, 9.136515536752833455 ) ) ;
#18008 = EDGE_CURVE ( 'NONE', #63300, #5868, #58064, .T. ) ;
#18009 = ORIENTED_EDGE ( 'NONE', *, *, #46793, .F. ) ;
#18010 = CARTESIAN_POINT ( 'NONE',  ( 17.55505043854144276, 0.6250000000000001110, -25.00000000000000000 ) ) ;
#18011 = CARTESIAN_POINT ( 'NONE',  ( 10.47111721959000086, 5.170640285885000687, -8.712953516124999354 ) ) ;
#18012 = CARTESIAN_POINT ( 'NONE',  ( 11.13214415304999960, -5.330901272402999602, -5.052956475076999077 ) ) ;
#18013 = CARTESIAN_POINT ( 'NONE',  ( 12.51770044094176981, 3.055120810438261891, -13.53992139506082104 ) ) ;
#18014 = LINE ( 'NONE', #7506, #3570 ) ;
#18015 = CARTESIAN_POINT ( 'NONE',  ( 25.29576976926500009, 2.995598598314000327, 11.41691922160000061 ) ) ;
#18016 = CARTESIAN_POINT ( 'NONE',  ( 17.57900095810616037, -0.7302151993337174796, 13.98094363222392467 ) ) ;
#18017 = CIRCLE ( 'NONE', #13575, 1.000000000000000888 ) ;
#18018 = CARTESIAN_POINT ( 'NONE',  ( 25.19216327953800061, -2.891353817808000048, 11.44527084745000067 ) ) ;
#18019 = B_SPLINE_CURVE_WITH_KNOTS ( 'NONE', 3,
 ( #60545, #12651, #55651, #23483, #51090, #18245 ),
 .UNSPECIFIED., .F., .F.,
 ( 4, 2, 4 ),
 ( 0.000000000000000000, 0.5000000000000000000, 1.000000000000000000 ),
 .UNSPECIFIED. ) ;
#18020 = VERTEX_POINT ( 'NONE', #49967 ) ;
#18021 = EDGE_LOOP ( 'NONE', ( #31642, #33369, #41905, #2277 ) ) ;
#18022 = CARTESIAN_POINT ( 'NONE',  ( 8.649364158774000444, 3.038023536984999939, -5.861661709981000001 ) ) ;
#18023 = CARTESIAN_POINT ( 'NONE',  ( 12.31002172256219929, -0.3816054325215895160, 13.89295103372929496 ) ) ;
#18024 = CARTESIAN_POINT ( 'NONE',  ( 10.72272469555899832, -3.360453478306600239, 8.606479382885998675 ) ) ;
#18025 = CARTESIAN_POINT ( 'NONE',  ( 10.50286331871000023, -5.158900740613000302, 8.369962360110999811 ) ) ;
#18026 = CARTESIAN_POINT ( 'NONE',  ( 9.135904863751600047, -5.220041948655085307, 6.249571414823495097 ) ) ;
#18027 = CARTESIAN_POINT ( 'NONE',  ( 8.513433059625000965, -5.040796345420999636, 8.522966281393001609 ) ) ;
#18028 = EDGE_CURVE ( 'NONE', #52150, #41893, #53583, .T. ) ;
#18029 = DIRECTION ( 'NONE',  ( -0.7071067811865475727, 0.7071067811865475727, 0.000000000000000000 ) ) ;
#18031 = CARTESIAN_POINT ( 'NONE',  ( 16.39999999379500295, 3.351248059343999941, 11.15756683833000018 ) ) ;
#18030 = CARTESIAN_POINT ( 'NONE',  ( 10.86825461470400001, -5.239722547583999912, 7.184607557167700165 ) ) ;
#18032 = CARTESIAN_POINT ( 'NONE',  ( 10.81349144726329925, 3.261052100888700345, -6.457276458983999490 ) ) ;
#18033 = ADVANCED_FACE ( 'NONE', ( #44738 ), #45420, .T. ) ;
#18034 = CARTESIAN_POINT ( 'NONE',  ( 12.61475641026223649, 0.7110419930738796079, 13.98197980709405108 ) ) ;
#18035 = CARTESIAN_POINT ( 'NONE',  ( 8.842468108405999061, 4.834201109053600121, -7.736255015838599647 ) ) ;
#18036 = CARTESIAN_POINT ( 'NONE',  ( 7.881386633191600488, 5.152558727359871860, 6.796436030802987638 ) ) ;
#18037 = CARTESIAN_POINT ( 'NONE',  ( 8.470944094208999076, 5.100000000000000533, 6.571291218949999902 ) ) ;
#18038 = CARTESIAN_POINT ( 'NONE',  ( 4.149992563291999836, -1.229060429538530563, 1.599290730647368486 ) ) ;
#18039 = ORIENTED_EDGE ( 'NONE', *, *, #28287, .T. ) ;
#18041 = CARTESIAN_POINT ( 'NONE',  ( 7.931011803055000975, 3.387313518888000363, -6.297038610257000180 ) ) ;
#18040 = CARTESIAN_POINT ( 'NONE',  ( 11.68424042080583547, -3.455907502640803486, 8.657883396625683403 ) ) ;
#18042 = CARTESIAN_POINT ( 'NONE',  ( 9.211104719594999324, 5.462898983065000102, -8.055936939571999744 ) ) ;
#18043 = CARTESIAN_POINT ( 'NONE',  ( 24.30000000000000071, 10.83443035398000021, 3.855530949778000149 ) ) ;
#18044 = CARTESIAN_POINT ( 'NONE',  ( 24.30000000000000071, -8.810505093353000916, 8.810505093353000916 ) ) ;
#18045 = CARTESIAN_POINT ( 'NONE',  ( 11.09999999999999964, 0.000000000000000000, 0.000000000000000000 ) ) ;
#18046 = PLANE ( 'NONE',  #63290 ) ;
#18047 = CARTESIAN_POINT ( 'NONE',  ( 2.118473157973999932, 3.592226503575000507, 0.01333834274854999932 ) ) ;
#18048 = EDGE_LOOP ( 'NONE', ( #39421, #50888, #20044, #4609 ) ) ;
#18049 = CARTESIAN_POINT ( 'NONE',  ( 12.11827192994440772, 0.2307628456012717488, -12.59789151516663175 ) ) ;
#18051 = VECTOR ( 'NONE', #67946, 1000.000000000000000 ) ;
#18050 = CARTESIAN_POINT ( 'NONE',  ( 11.04783424078000031, -2.764605797469000148, 5.041477660832000218 ) ) ;
#18052 = CARTESIAN_POINT ( 'NONE',  ( 24.08742106046339160, -12.56972931058949072, -3.401799986514439045 ) ) ;
#18053 = CARTESIAN_POINT ( 'NONE',  ( 8.732392219593000604, 2.806082850903000026, 8.615880516515998622 ) ) ;
#18054 = ORIENTED_EDGE ( 'NONE', *, *, #53369, .T. ) ;
#18055 = CARTESIAN_POINT ( 'NONE',  ( 5.449388989100000025, -1.346921469446999975, 0.5851709088685000948 ) ) ;
#18056 = CARTESIAN_POINT ( 'NONE',  ( 10.95126072563318331, 9.104112520226776084, 6.364239214224977736 ) ) ;
#18058 = CARTESIAN_POINT ( 'NONE',  ( 11.12299956498149811, 5.207010770456999893, 7.174999999999999822 ) ) ;
#18057 = CYLINDRICAL_SURFACE ( 'NONE', #9554, 11.50000000000000178 ) ;
#18059 = CARTESIAN_POINT ( 'NONE',  ( 10.76346886766499900, 3.365322927604099679, -6.346853961441000003 ) ) ;
#18060 = ORIENTED_EDGE ( 'NONE', *, *, #16800, .F. ) ;
#18061 = ORIENTED_EDGE ( 'NONE', *, *, #60222, .T. ) ;
#18062 = CARTESIAN_POINT ( 'NONE',  ( 11.15221028326116048, 3.091096528151293210, 7.824988602100019008 ) ) ;
#18063 = CIRCLE ( 'NONE', #64941, 12.20000000000000107 ) ;
#18064 = CARTESIAN_POINT ( 'NONE',  ( 17.98240304306455428, -0.4561791668615495787, -13.88992602861184089 ) ) ;
#18065 = EDGE_CURVE ( 'NONE', #16046, #38239, #6281, .T. ) ;
#18066 = EDGE_CURVE ( 'NONE', #41893, #54978, #60459, .T. ) ;
#18067 = ORIENTED_EDGE ( 'NONE', *, *, #46487, .T. ) ;
#18068 = CARTESIAN_POINT ( 'NONE',  ( 10.95996395620064412, 8.913960680409392268, -6.449865299654371498 ) ) ;
#18069 = DIRECTION ( 'NONE',  ( -0.6427876096865049460, 0.000000000000000000, 0.7660444431190069903 ) ) ;
#18070 = CARTESIAN_POINT ( 'NONE',  ( 7.341889158769000723, 2.602490396417999730, -7.495170534277000307 ) ) ;
#18071 = DIRECTION ( 'NONE',  ( 0.000000000000000000, 1.000000000000000000, 0.000000000000000000 ) ) ;
#18072 = CARTESIAN_POINT ( 'NONE',  ( 18.17608830303634093, -2.571081551981528879, 12.43475473546731891 ) ) ;
#18073 = ORIENTED_EDGE ( 'NONE', *, *, #18254, .F. ) ;
#18074 = CARTESIAN_POINT ( 'NONE',  ( 7.999926658772999133, 5.198556077301000222, 8.332552905512999430 ) ) ;
#18075 = CARTESIAN_POINT ( 'NONE',  ( 23.99166156695100227, -13.00799102709000010, -3.384109424371999797 ) ) ;
#18076 = CARTESIAN_POINT ( 'NONE',  ( 9.810596873515665450, 3.370476274536378103, 8.592232985442823434 ) ) ;
#18077 = CARTESIAN_POINT ( 'NONE',  ( 12.61587921995040595, -3.224448188361915157, 13.62362021573694015 ) ) ;
#18078 = ORIENTED_EDGE ( 'NONE', *, *, #57966, .T. ) ;
#18079 = CARTESIAN_POINT ( 'NONE',  ( 25.46373185538400463, 11.23406899464000119, 3.161078463958999496 ) ) ;
#18080 = CARTESIAN_POINT ( 'NONE',  ( 8.751496707488000126, -3.918323994020610268, -8.356402621895700378 ) ) ;
#18081 = CARTESIAN_POINT ( 'NONE',  ( 11.48052502238429895, 5.045683737783986267, -7.824990984965952912 ) ) ;
#18082 = CARTESIAN_POINT ( 'NONE',  ( 9.118435835444836712, 5.100000000000000533, 6.178531823618069296 ) ) ;
#18083 = CARTESIAN_POINT ( 'NONE',  ( 10.38314899745999931, -5.167567567567999731, 6.822293592207000934 ) ) ;
#18084 = CARTESIAN_POINT ( 'NONE',  ( 5.982109839683626973, -0.9218200799623778030, 1.199500263597266914 ) ) ;
#18085 = CARTESIAN_POINT ( 'NONE',  ( 17.94956985871015931, -2.984774188598619649, 12.32531689504261685 ) ) ;
#18086 = ORIENTED_EDGE ( 'NONE', *, *, #37253, .F. ) ;
#18087 = EDGE_CURVE ( 'NONE', #22430, #13791, #67068, .T. ) ;
#18088 = CARTESIAN_POINT ( 'NONE',  ( 11.40211496860029783, -3.206052520092899982, -7.093139000852099585 ) ) ;
#18089 = ADVANCED_FACE ( 'NONE', ( #30040 ), #50245, .T. ) ;
#18090 = ORIENTED_EDGE ( 'NONE', *, *, #45479, .T. ) ;
#18091 = CARTESIAN_POINT ( 'NONE',  ( 18.17891100653320891, 2.457162529407604712, 13.68241659864889748 ) ) ;
#18092 = CARTESIAN_POINT ( 'NONE',  ( 8.400739158770999637, 4.933589693325000525, -9.154576215408999573 ) ) ;
#18093 = B_SPLINE_CURVE_WITH_KNOTS ( 'NONE', 3,
 ( #55559, #29697, #12912, #55209, #8009, #3097 ),
 .UNSPECIFIED., .F., .F.,
 ( 4, 2, 4 ),
 ( 0.000000000000000000, 0.5000000000000000000, 1.000000000000000000 ),
 .UNSPECIFIED. ) ;
#18094 = CIRCLE ( 'NONE', #57148, 1.300160515709999354 ) ;
#18095 = EDGE_CURVE ( 'NONE', #55008, #38535, #36391, .T. ) ;
#18096 = CARTESIAN_POINT ( 'NONE',  ( 2.712743541013000304, -0.2306114756280000233, -3.371506406067999784 ) ) ;
#18097 = CARTESIAN_POINT ( 'NONE',  ( 11.01003172897000049, -3.180716007396000133, -6.283809484240999943 ) ) ;
#18098 = CARTESIAN_POINT ( 'NONE',  ( 5.700000000000000178, 0.000000000000000000, 0.000000000000000000 ) ) ;
#18099 = CARTESIAN_POINT ( 'NONE',  ( 23.73670661716200314, 13.28054472774000061, 3.698137085571999716 ) ) ;
#18100 = FACE_OUTER_BOUND ( 'NONE', #63738, .T. ) ;
#18101 = ORIENTED_EDGE ( 'NONE', *, *, #1880, .T. ) ;
#18102 = CARTESIAN_POINT ( 'NONE',  ( 10.14405657264394378, -4.746626309883068551, -8.655951532184957387 ) ) ;
#18103 = CARTESIAN_POINT ( 'NONE',  ( 12.08487348028855024, -4.882707455860599843, 7.022738645480499642 ) ) ;
#18104 = CARTESIAN_POINT ( 'NONE',  ( 10.68903608760000168, 2.568976842941999905, 7.728092503410000091 ) ) ;
#18105 = CARTESIAN_POINT ( 'NONE',  ( 10.22422653164065487, -2.899999999999999911, -6.304440313833538312 ) ) ;
#18106 = CARTESIAN_POINT ( 'NONE',  ( 24.30000000000000071, -2.204728229456999866, -11.99913219504999873 ) ) ;
#18107 = CARTESIAN_POINT ( 'NONE',  ( 11.05833333333436741, 2.548905579443693448, 7.980400043919090969 ) ) ;
#18108 = CARTESIAN_POINT ( 'NONE',  ( 11.09256785386839894, 3.167490253789400523, -8.060248494254899754 ) ) ;
#18109 = EDGE_CURVE ( 'NONE', #62685, #68419, #9629, .T. ) ;
#18110 = CARTESIAN_POINT ( 'NONE',  ( 7.100000000000459721, 5.092549871003397399, -6.644539875156245223 ) ) ;
#18111 = AXIS2_PLACEMENT_3D ( 'NONE', #5188, #26525, #69161 ) ;
#18112 = CARTESIAN_POINT ( 'NONE',  ( 10.31558376188599802, 3.037118682679400106, -8.113672563022399586 ) ) ;
#18113 = FACE_OUTER_BOUND ( 'NONE', #39109, .T. ) ;
#18114 = CARTESIAN_POINT ( 'NONE',  ( 8.126439348839909371, 4.834870829740609111, -6.246114233407420890 ) ) ;
#18115 = CARTESIAN_POINT ( 'NONE',  ( 10.87947334122999976, 2.817426144593000004, -6.828668581221999823 ) ) ;
#18116 = ORIENTED_EDGE ( 'NONE', *, *, #46844, .T. ) ;
#18117 = CARTESIAN_POINT ( 'NONE',  ( 7.282480646792000023, -3.448181789123000218, 9.222458996124998976 ) ) ;
#18118 = CARTESIAN_POINT ( 'NONE',  ( 17.67509761310384064, 1.797476384633017066, 13.88413128968476684 ) ) ;
#18119 = CARTESIAN_POINT ( 'NONE',  ( 27.09999999999999787, 1.806713620938000108E-12, -9.250000000000000000 ) ) ;
#18120 = CARTESIAN_POINT ( 'NONE',  ( 10.98579841651039857, -4.449968941611500028, -8.696179055230999211 ) ) ;
#18121 = ORIENTED_EDGE ( 'NONE', *, *, #41537, .T. ) ;
#18122 = CARTESIAN_POINT ( 'NONE',  ( 25.37646785958400031, 2.613418185928999993, -11.31776759263999921 ) ) ;
#18123 = CARTESIAN_POINT ( 'NONE',  ( 9.069718325438000051, 4.108964550738000376, 8.851615252874999840 ) ) ;
#18125 = CARTESIAN_POINT ( 'NONE',  ( 11.22056920625029974, 4.047312782235129802, 8.815417147437999645 ) ) ;
#18124 = CARTESIAN_POINT ( 'NONE',  ( 8.655270280412999284, 4.162493982103000256, -5.775210092227999858 ) ) ;
#18126 = CARTESIAN_POINT ( 'NONE',  ( 10.07762665876999897, 2.169012810937000157, -7.244984731085000185 ) ) ;
#18127 = ORIENTED_EDGE ( 'NONE', *, *, #40789, .F. ) ;
#18128 = CARTESIAN_POINT ( 'NONE',  ( 10.41185190929999926, 2.101586107686999938, 7.856266936613998553 ) ) ;
#18129 = CARTESIAN_POINT ( 'NONE',  ( 25.37959880612143948, 3.026669825678802273, -11.38055956022503246 ) ) ;
#18130 = CARTESIAN_POINT ( 'NONE',  ( 10.94072200990529886, 2.922907051630999842, 7.875713849677398848 ) ) ;
#18131 = CARTESIAN_POINT ( 'NONE',  ( 10.27968096967000022, -5.739708848514999850, 7.774962785835000112 ) ) ;
#18132 = CARTESIAN_POINT ( 'NONE',  ( 7.470056312015993960, 3.527048554922000090, 6.623442700707995456 ) ) ;
#18133 = ORIENTED_EDGE ( 'NONE', *, *, #56625, .T. ) ;
#18134 = CARTESIAN_POINT ( 'NONE',  ( 11.80561165699200110, -3.526771526455999783, 11.96112153682000034 ) ) ;
#18135 = CARTESIAN_POINT ( 'NONE',  ( 1.386390132541124309, 0.4581489286485156964, -3.499999999999998668 ) ) ;
#18136 = CARTESIAN_POINT ( 'NONE',  ( 7.933903043726158621, -2.295323260153894651, 7.847068492003852924 ) ) ;
#18137 = CARTESIAN_POINT ( 'NONE',  ( 10.99433452212999818, -3.697619272994999928, 5.729306330972000261 ) ) ;
#18138 = CARTESIAN_POINT ( 'NONE',  ( 11.09999999999999964, -4.000000000000000000, -7.500000000000000000 ) ) ;
#18139 = CARTESIAN_POINT ( 'NONE',  ( 10.20863399569799945, -2.865156490077000129, 7.374045024026299799 ) ) ;
#18140 = EDGE_LOOP ( 'NONE', ( #31356, #10603, #14490, #33077, #53648 ) ) ;
#18142 = CARTESIAN_POINT ( 'NONE',  ( 24.14647631174685216, -9.144949018368393467, 9.120856162720306415 ) ) ;
#18141 = AXIS2_PLACEMENT_3D ( 'NONE', #6832, #54381, #1592 ) ;
#18143 = CARTESIAN_POINT ( 'NONE',  ( 10.63662282008600002, -3.405288783432600219, 6.540749699823199315 ) ) ;
#18144 = ORIENTED_EDGE ( 'NONE', *, *, #10605, .T. ) ;
#18145 = CARTESIAN_POINT ( 'NONE',  ( 9.015584277044482064, 3.283082709547154643, 6.568532107505763662 ) ) ;
#18146 = VERTEX_POINT ( 'NONE', #8012 ) ;
#18147 = EDGE_CURVE ( 'NONE', #21661, #22433, #50661, .T. ) ;
#18148 = EDGE_CURVE ( 'NONE', #68176, #1231, #4810, .T. ) ;
#18149 = CARTESIAN_POINT ( 'NONE',  ( 8.216604719590000272, 5.331510020787000315, -8.114341808290998159 ) ) ;
#18150 = CARTESIAN_POINT ( 'NONE',  ( 10.92968717260509948, 3.312350236372100021, -8.622362941748999532 ) ) ;
#18151 = CARTESIAN_POINT ( 'NONE',  ( 8.229424060894674042, 4.864026623416703110, 6.209051899842799926 ) ) ;
#18152 = CARTESIAN_POINT ( 'NONE',  ( 12.10442723766653472, 2.667336250084659799, -12.31445622895738978 ) ) ;
#18153 = CARTESIAN_POINT ( 'NONE',  ( 12.00687348028854906, -5.003459210197000573, 6.957450711802899868 ) ) ;
#18154 = CARTESIAN_POINT ( 'NONE',  ( 11.06591429142999949, -3.980313504646230349, 8.533318907609000803 ) ) ;
#18155 = ORIENTED_EDGE ( 'NONE', *, *, #43595, .T. ) ;
#18156 = DIRECTION ( 'NONE',  ( 0.000000000000000000, 0.000000000000000000, -1.000000000000000000 ) ) ;
#18157 = VECTOR ( 'NONE', #20559, 1000.000000000000000 ) ;
#18158 = VERTEX_POINT ( 'NONE', #25801 ) ;
#18159 = CARTESIAN_POINT ( 'NONE',  ( 8.379706853209000883, -4.282999948634999221, 9.286791354293999490 ) ) ;
#18160 = DIRECTION ( 'NONE',  ( 1.000000000000000000, 0.000000000000000000, 0.000000000000000000 ) ) ;
#18161 = VERTEX_POINT ( 'NONE', #40848 ) ;
#18162 = CARTESIAN_POINT ( 'NONE',  ( 12.40831127361658837, -1.878029834076337723, -12.45925554172551308 ) ) ;
#18163 = CARTESIAN_POINT ( 'NONE',  ( 10.20641772631199906, 4.431553727090300043, 6.611684804099500212 ) ) ;
#18164 = CARTESIAN_POINT ( 'NONE',  ( 10.45625805961999966, -3.661873208228000109, -9.317463915629002003 ) ) ;
#18165 = CARTESIAN_POINT ( 'NONE',  ( 7.000000000000000000, 0.000000000000000000, 0.000000000000000000 ) ) ;
#18166 = CARTESIAN_POINT ( 'NONE',  ( 18.31117841518900136, -11.80507181181000043, 3.724836393661000056 ) ) ;
#18167 = CARTESIAN_POINT ( 'NONE',  ( 8.734814475091132735, 4.056037006134289413, 6.616514917701350029 ) ) ;
#18168 = CARTESIAN_POINT ( 'NONE',  ( 12.20116045406121863, -2.662322297126388015, -13.63765712018376952 ) ) ;
#18169 = CARTESIAN_POINT ( 'NONE',  ( 18.12436022580823902, 0.2580991232524043055, -12.69647497719791573 ) ) ;
#18170 = CARTESIAN_POINT ( 'NONE',  ( 11.29364426047339975, -3.533902447304699823, -8.230103870496201068 ) ) ;
#18171 = CARTESIAN_POINT ( 'NONE',  ( 11.13764426047339917, -3.386171819220400003, -8.461511872390000022 ) ) ;
#18172 = CARTESIAN_POINT ( 'NONE',  ( 7.968176658772001097, 2.280568568659000483, 6.510284508622999233 ) ) ;
#18173 = ORIENTED_EDGE ( 'NONE', *, *, #19342, .T. ) ;
#18174 = CARTESIAN_POINT ( 'NONE',  ( 23.60000000000000142, 9.289189189551001036, -7.908916752675001050 ) ) ;
#18175 = CARTESIAN_POINT ( 'NONE',  ( 8.121343566036543393, 3.646810248691461531, 8.848457998379188894 ) ) ;
#18176 = EDGE_CURVE ( 'NONE', #34355, #36450, #30706, .T. ) ;
#18177 = B_SPLINE_CURVE_WITH_KNOTS ( 'NONE', 3,
 ( #49578, #55865, #7973, #39094 ),
 .UNSPECIFIED., .F., .F.,
 ( 4, 4 ),
 ( 0.000000000000000000, 1.000000000000000000 ),
 .UNSPECIFIED. ) ;
#18178 = CARTESIAN_POINT ( 'NONE',  ( 10.25165889348999926, 3.418644779562000302, -8.733642166016998942 ) ) ;
#18179 = CARTESIAN_POINT ( 'NONE',  ( 18.10356236467037050, 2.200227019994205779, 12.51636715934673205 ) ) ;
#18180 = CARTESIAN_POINT ( 'NONE',  ( 10.84920446230533386, 2.899999999999999911, -6.662590550568697090 ) ) ;
#18181 = CARTESIAN_POINT ( 'NONE',  ( 9.194604681486000075, 5.157771204918000230, 8.637848577075999401 ) ) ;
#18182 = CARTESIAN_POINT ( 'NONE',  ( 9.549596101582627838, -4.563377510236459322, 8.169431139013614285 ) ) ;
#18183 = CARTESIAN_POINT ( 'NONE',  ( 8.755786719645998417, 3.934709392726489785, 6.597079156813799194 ) ) ;
#18184 = VERTEX_POINT ( 'NONE', #15316 ) ;
#18185 = CARTESIAN_POINT ( 'NONE',  ( 12.21314472040068644, -2.700933736278045227, 12.40250870093142410 ) ) ;
#18186 = CARTESIAN_POINT ( 'NONE',  ( 9.477709346417000802, -3.092687088662700035, -7.069157126958599768 ) ) ;
#18187 = FACE_OUTER_BOUND ( 'NONE', #56680, .T. ) ;
#18188 = CARTESIAN_POINT ( 'NONE',  ( 9.307788144226000426, -3.909067355573210278, 6.546538158064899804 ) ) ;
#18189 = AXIS2_PLACEMENT_3D ( 'NONE', #52059, #41580, #47866 ) ;
#18190 = CARTESIAN_POINT ( 'NONE',  ( 10.54687750876899877, 3.382085645339300228, -8.458891008702400072 ) ) ;
#18191 = EDGE_CURVE ( 'NONE', #31999, #13082, #46422, .T. ) ;
#18192 = CARTESIAN_POINT ( 'NONE',  ( 12.16275096843967951, -0.3336735144251360974, 12.59558214381612551 ) ) ;
#18193 = CARTESIAN_POINT ( 'NONE',  ( 7.956795280408998750, 4.524487726177000013, 9.047753146378999745 ) ) ;
#18194 = CARTESIAN_POINT ( 'NONE',  ( 11.27110638630999873, 5.469603964121000139, 8.504707115835000053 ) ) ;
#18195 = CARTESIAN_POINT ( 'NONE',  ( 8.771640687504598688, -2.873222873814833545, 6.752018918871646846 ) ) ;
#18196 = ORIENTED_EDGE ( 'NONE', *, *, #32578, .F. ) ;
#18197 = CARTESIAN_POINT ( 'NONE',  ( 9.047164158776000775, 2.156584729807999867, -7.959751745006000689 ) ) ;
#18198 = CARTESIAN_POINT ( 'NONE',  ( 10.54272335273199879, 4.444874504667400750, -8.698083075453000745 ) ) ;
#18199 = CARTESIAN_POINT ( 'NONE',  ( 10.75620859869496115, -5.323164692320646374, 8.643262214358355067 ) ) ;
#18201 = CARTESIAN_POINT ( 'NONE',  ( 17.88362877536322060, -0.5317665474973085615, 12.68501283761687226 ) ) ;
#18200 = CARTESIAN_POINT ( 'NONE',  ( 7.100000000000000533, -4.000000000000000000, 8.849999999999999645 ) ) ;
#18202 = CARTESIAN_POINT ( 'NONE',  ( 10.51459632033899894, -4.929952350555500296, 7.879514065647800436 ) ) ;
#18203 = CARTESIAN_POINT ( 'NONE',  ( 11.78594988689359901, -3.606563555963900214, -8.271690446953899212 ) ) ;
#18204 = ORIENTED_EDGE ( 'NONE', *, *, #40469, .F. ) ;
#18205 = VECTOR ( 'NONE', #18757, 1000.000000000000000 ) ;
#18206 = CARTESIAN_POINT ( 'NONE',  ( 1.257791847628999982, 1.635708097465000010, -3.009863393104000195 ) ) ;
#18207 = CARTESIAN_POINT ( 'NONE',  ( 12.24143698068993835, 11.79508855326024275, -3.559061050734573683 ) ) ;
#18208 = LINE ( 'NONE', #23450, #6204 ) ;
#18209 = CARTESIAN_POINT ( 'NONE',  ( 18.11804139221521837, -2.771758052479264656, 13.61206300402962910 ) ) ;
#18210 = CARTESIAN_POINT ( 'NONE',  ( 17.33333333127366771, 3.351260669886487964, 11.15757822838322433 ) ) ;
#18211 = CARTESIAN_POINT ( 'NONE',  ( 4.900006121741999898, -1.599333684796363508, -1.229093439949825672 ) ) ;
#18212 = DIRECTION ( 'NONE',  ( 0.9999999999995219380, -9.778750326963210600E-07, 5.518476893961119184E-11 ) ) ;
#18213 = DIRECTION ( 'NONE',  ( 0.000000000000000000, -1.000000000000000000, 0.000000000000000000 ) ) ;
#18214 = CARTESIAN_POINT ( 'NONE',  ( 23.67317737304023595, 13.19576797240445565, 3.926420038237877996 ) ) ;
#18215 = EDGE_LOOP ( 'NONE', ( #6224, #17673, #45323 ) ) ;
#18216 = CARTESIAN_POINT ( 'NONE',  ( 9.933148997456999751, 5.167567567567999731, 6.822293592207000934 ) ) ;
#18217 = CARTESIAN_POINT ( 'NONE',  ( 24.66908015013045130, -8.674046118889807033, 8.642878031199991540 ) ) ;
#18218 = CARTESIAN_POINT ( 'NONE',  ( 17.80000000001300009, -3.351264566333000072, -11.15757590352999884 ) ) ;
#18219 = CARTESIAN_POINT ( 'NONE',  ( -14.79345512259999929, 10.48174933044999868, 5.405686454350000503 ) ) ;
#18220 = DIRECTION ( 'NONE',  ( 1.000000000000000000, 0.000000000000000000, 0.000000000000000000 ) ) ;
#18222 = ORIENTED_EDGE ( 'NONE', *, *, #11203, .F. ) ;
#18221 = B_SPLINE_CURVE_WITH_KNOTS ( 'NONE', 3,
 ( #22786, #23485, #38881, #6354 ),
 .UNSPECIFIED., .F., .F.,
 ( 4, 4 ),
 ( 0.000000000000000000, 1.000000000000000000 ),
 .UNSPECIFIED. ) ;
#18223 = CARTESIAN_POINT ( 'NONE',  ( 1.886390132539666142, 0.4581489286485156964, -3.499999999999998668 ) ) ;
#18224 = DIRECTION ( 'NONE',  ( -1.000000000000000000, 0.000000000000000000, 0.000000000000000000 ) ) ;
#18225 = CARTESIAN_POINT ( 'NONE',  ( 9.893930206848999376, -5.250000000000000000, 7.500000000000000000 ) ) ;
#18226 = CARTESIAN_POINT ( 'NONE',  ( 11.38795122972049967, 4.398282450130399646, 8.421043941822800249 ) ) ;
#18227 = EDGE_CURVE ( 'NONE', #56220, #36266, #11365, .T. ) ;
#18228 = EDGE_CURVE ( 'NONE', #44093, #46698, #9361, .T. ) ;
#18229 = CARTESIAN_POINT ( 'NONE',  ( 9.574741131515299486, -3.579783539280765314, 8.799459768376697966 ) ) ;
#18230 = CARTESIAN_POINT ( 'NONE',  ( 11.22022944037999892, -3.883088694641999794, -8.854817792072001481 ) ) ;
#18231 = CARTESIAN_POINT ( 'NONE',  ( 15.89979320884932967, -7.372865056442189591, -9.926947018133246203 ) ) ;
#18232 = EDGE_CURVE ( 'NONE', #10880, #11774, #62509, .T. ) ;
#18233 = EDGE_CURVE ( 'NONE', #7194, #28894, #17184, .T. ) ;
#18234 = DIRECTION ( 'NONE',  ( 1.000000000000000000, 0.000000000000000000, 0.000000000000000000 ) ) ;
#18235 = CARTESIAN_POINT ( 'NONE',  ( 12.22440656761272137, -2.731388741841335399, 12.39466681327069786 ) ) ;
#18236 = VERTEX_POINT ( 'NONE', #47476 ) ;
#18237 = CARTESIAN_POINT ( 'NONE',  ( 8.056242640631749552, 3.593179318435525182, 5.798412987495025206 ) ) ;
#18238 = VERTEX_POINT ( 'NONE', #9029 ) ;
#18239 = CARTESIAN_POINT ( 'NONE',  ( 17.89590342297357495, -3.023973030522680627, 13.54825986461598397 ) ) ;
#18240 = CARTESIAN_POINT ( 'NONE',  ( 10.93656785386839836, -5.060279460151999587, -8.213529149347399638 ) ) ;
#18241 = ORIENTED_EDGE ( 'NONE', *, *, #63566, .T. ) ;
#18242 = CARTESIAN_POINT ( 'NONE',  ( 8.967233804172259681, -5.342662483617720781, 7.359968207274207863 ) ) ;
#18243 = CARTESIAN_POINT ( 'NONE',  ( 10.86190547754509872, 4.891676932241900033, 7.471700551735359852 ) ) ;
#18244 = CARTESIAN_POINT ( 'NONE',  ( 5.500000000000000000, 2.200000000000000178, 0.000000000000000000 ) ) ;
#18245 = CARTESIAN_POINT ( 'NONE',  ( 23.56665676678199972, 13.31363904818000066, -4.296982115204999175 ) ) ;
#18246 = CARTESIAN_POINT ( 'NONE',  ( 17.55505043854147118, -3.125000000000000000, -25.00000000000000000 ) ) ;
#18247 = CARTESIAN_POINT ( 'NONE',  ( 10.56590837162999996, 5.293226105229999590, -7.067087619452999903 ) ) ;
#18248 = CARTESIAN_POINT ( 'NONE',  ( 11.10000000008000143, 8.133170861274999552, -6.729066177741999333 ) ) ;
#18249 = CARTESIAN_POINT ( 'NONE',  ( 11.80443633831200145, 3.376482451534999818, -11.11063790749999924 ) ) ;
#18250 = CARTESIAN_POINT ( 'NONE',  ( 10.10656447933000024, -4.887648864398999926, -6.257283015674000026 ) ) ;
#18251 = CARTESIAN_POINT ( 'NONE',  ( 25.39994675527849921, -8.680020655622012526, -7.390263983914230117 ) ) ;
#18252 = CARTESIAN_POINT ( 'NONE',  ( 23.59999172348799945, -10.30759808834999980, 9.317726582648999667 ) ) ;
#18253 = ORIENTED_EDGE ( 'NONE', *, *, #24889, .F. ) ;
#18254 = EDGE_CURVE ( 'NONE', #50708, #21446, #35620, .T. ) ;
#18255 = CIRCLE ( 'NONE', #23839, 10.75000000000000533 ) ;
#18256 = CARTESIAN_POINT ( 'NONE',  ( 8.876902336861421716, 4.269588175475919734, -6.500155937682548846 ) ) ;
#18257 = SHAPE_REPRESENTATION_RELATIONSHIP ( 'NONE' , 'NONE' ,  #55423, #64411 ) ;
#18258 = CARTESIAN_POINT ( 'NONE',  ( 3.500000000000000000, 0.000000000000000000, 0.000000000000000000 ) ) ;
#18259 = CARTESIAN_POINT ( 'NONE',  ( 11.04322985880000196, -5.244997146226999973, 5.031759926182000520 ) ) ;
#18260 = CARTESIAN_POINT ( 'NONE',  ( 10.77332351902758845, -2.820285017511723336, -8.179908095962412418 ) ) ;
#18261 = CARTESIAN_POINT ( 'NONE',  ( 9.196006702408606515, 4.999605512837394627, 8.268211173249300217 ) ) ;
#18262 = CARTESIAN_POINT ( 'NONE',  ( 12.36790649065924086, 2.053195086250957591, 13.75808315936462378 ) ) ;
#18263 = CARTESIAN_POINT ( 'NONE',  ( 9.813358178091998951, -5.349400659402999914, 6.657024270273000255 ) ) ;
#18264 = VERTEX_POINT ( 'NONE', #41879 ) ;
#18265 = CARTESIAN_POINT ( 'NONE',  ( 11.33810207955129812, 4.796537143354000499, -7.825000000000000178 ) ) ;
#18266 = CARTESIAN_POINT ( 'NONE',  ( 12.09857429938281825, 0.1657344298535193272, 13.99903850390423088 ) ) ;
#18267 =( BOUNDED_SURFACE ( )  B_SPLINE_SURFACE ( 3, 3, ( 
 ( #36855, #20083, #10277, #36504, #63751, #31610, #41412, #52932, #41753, #30924, #3987 ),
 ( #26366, #42440, #47692, #48028, #69004, #132, #15863, #58513, #53275, #10617, #52582 ),
 ( #5377, #62718, #52236, #15181, #31271, #57824, #9933, #16893, #64093, #7102, #65477 ),
 ( #6749, #32307, #11305, #64431, #54301, #38222, #10968, #17247, #16553, #28440, #17602 ) ),
 .UNSPECIFIED., .F., .F., .T. ) 
 B_SPLINE_SURFACE_WITH_KNOTS ( ( 4, 4 ),
 ( 4, 1, 1, 1, 1, 1, 1, 1, 4 ),
 ( 0.000000000000000000, 1.000000000000000000 ),
 ( -0.004668278336391999857, 0.000000000000000000, 0.03269534097185999855, 0.06255479614191999937, 0.08986301827556000821, 0.1148786485006000058, 0.1378153831697999931, 0.1587710662428999941, 0.1687086804768000159 ),
 .UNSPECIFIED. ) 
 GEOMETRIC_REPRESENTATION_ITEM ( )  RATIONAL_B_SPLINE_SURFACE ( (
 ( 1.221011660805000121, 1.221011660805000121, 1.221011660805000121, 1.221011660805000121, 1.221011660805000121, 1.221011660805000121, 1.221011660805000121, 1.221011660805000121, 1.221011660805000121, 1.221011660805000121, 1.221011660805000121),
 ( 0.9263294463983999805, 0.9263294463983999805, 0.9263294463983999805, 0.9263294463983999805, 0.9263294463983999805, 0.9263294463983999805, 0.9263294463983999805, 0.9263294463983999805, 0.9263294463983999805, 0.9263294463983999805, 0.9263294463983999805),
 ( 0.9263294463983999805, 0.9263294463983999805, 0.9263294463983999805, 0.9263294463983999805, 0.9263294463983999805, 0.9263294463983999805, 0.9263294463983999805, 0.9263294463983999805, 0.9263294463983999805, 0.9263294463983999805, 0.9263294463983999805),
 ( 1.221011660805000121, 1.221011660805000121, 1.221011660805000121, 1.221011660805000121, 1.221011660805000121, 1.221011660805000121, 1.221011660805000121, 1.221011660805000121, 1.221011660805000121, 1.221011660805000121, 1.221011660805000121) ) ) 
 REPRESENTATION_ITEM ( '' )  SURFACE ( )  );
#18268 = ORIENTED_EDGE ( 'NONE', *, *, #35057, .T. ) ;
#18269 = PLANE ( 'NONE',  #67761 ) ;
#18270 = CARTESIAN_POINT ( 'NONE',  ( 9.405375278053794474, 5.100000000000000533, -6.445686799063087058 ) ) ;
#18271 = CARTESIAN_POINT ( 'NONE',  ( 23.51695530179700100, -2.932378615205000205, -13.82491157443000063 ) ) ;
#18272 = CARTESIAN_POINT ( 'NONE',  ( 8.483378221910873762, 3.070366253409245072, 6.121136983106237217 ) ) ;
#18273 = CARTESIAN_POINT ( 'NONE',  ( 9.278070280414000948, 2.546924812613000189, -6.918870225297999887 ) ) ;
#18274 = EDGE_CURVE ( 'NONE', #26681, #25668, #68091, .T. ) ;
#18275 = DIRECTION ( 'NONE',  ( -0.7071067939406878722, 0.000000000000000000, 0.7071067684324069402 ) ) ;
#18276 = CARTESIAN_POINT ( 'NONE',  ( 24.60109542855846243, 8.755194900634329258, 9.042388595921103445 ) ) ;
#18277 = CARTESIAN_POINT ( 'NONE',  ( 10.90000000000000036, -5.599999999999999645, 6.571291218949999902 ) ) ;
#18278 = B_SPLINE_CURVE_WITH_KNOTS ( 'NONE', 3,
 ( #60079, #23362, #1690, #22316, #44357, #1004, #17068, #59724, #33166, #18945, #8798, #61936, #65791, #66483, #18260, #18606, #39932, #66142 ),
 .UNSPECIFIED., .F., .F.,
 ( 4, 2, 2, 2, 2, 2, 2, 2, 4 ),
 ( 0.1254144463278223376, 0.2190603764462324965, 0.3127063065646425999, 0.4063522366830527588, 0.4999981668014629177, 0.5936440969198727435, 0.6872900270382826804, 0.7809359571566925062, 0.8745818872751025541 ),
 .UNSPECIFIED. ) ;
#18279 = CARTESIAN_POINT ( 'NONE',  ( 9.709999999999999076, 4.496968146123999865, -8.755198255949000696 ) ) ;
#18280 = EDGE_CURVE ( 'NONE', #45160, #23923, #63544, .T. ) ;
#18281 = DIRECTION ( 'NONE',  ( -0.000000000000000000, 1.000000000000000000, 0.000000000000000000 ) ) ;
#18282 = CARTESIAN_POINT ( 'NONE',  ( 9.084135711596999840, -5.371875912611999482, -7.370590366721999409 ) ) ;
#18283 = CARTESIAN_POINT ( 'NONE',  ( 10.62903166480609940, 3.135947233695900227, -7.560921321260908989 ) ) ;
#18284 = CYLINDRICAL_SURFACE ( 'NONE', #34967, 1.625000000000000000 ) ;
#18285 = CARTESIAN_POINT ( 'NONE',  ( 10.77368717260499942, 3.460071470104900015, -8.381256426168800289 ) ) ;
#18286 = CARTESIAN_POINT ( 'NONE',  ( 9.708633995697999453, 5.134843509922999871, -7.625954975973699312 ) ) ;
#18288 = CARTESIAN_POINT ( 'NONE',  ( 11.49999975383417450, -5.062986770486452848, 7.633391978603163430 ) ) ;
#18287 = CARTESIAN_POINT ( 'NONE',  ( 9.367797255588000027, -3.133765047594600173, 7.536673658251589636 ) ) ;
#18289 = DIRECTION ( 'NONE',  ( 0.000000000000000000, -0.9659258262890757507, 0.2588190451024934835 ) ) ;
#18290 = ORIENTED_EDGE ( 'NONE', *, *, #19173, .T. ) ;
#18291 = AXIS2_PLACEMENT_3D ( 'NONE', #15070, #46553, #52471 ) ;
#18292 = CARTESIAN_POINT ( 'NONE',  ( 10.47769598648999967, 5.009476315410999803, 6.898940957443399746 ) ) ;
#18293 = CARTESIAN_POINT ( 'NONE',  ( 9.414314870535999802, -3.941041813398000304, 5.878346364186999295 ) ) ;
#18294 = CARTESIAN_POINT ( 'NONE',  ( 8.880265421554998539, 3.785712956512099936, 6.391527115138999626 ) ) ;
#18295 = CARTESIAN_POINT ( 'NONE',  ( 10.81059687351629961, -4.629523725463621453, -6.407767014557176566 ) ) ;
#18296 = CARTESIAN_POINT ( 'NONE',  ( 11.08992739829000129, -5.210546653347999602, 8.327600405525998895 ) ) ;
#18297 = DIRECTION ( 'NONE',  ( 0.000000000000000000, -1.000000000000000000, 0.000000000000000000 ) ) ;
#18298 = UNCERTAINTY_MEASURE_WITH_UNIT (LENGTH_MEASURE( 1.000000000000000082E-05 ), #13706, 'distance_accuracy_value', 'NONE');
#18299 = ORIENTED_EDGE ( 'NONE', *, *, #38119, .F. ) ;
#18300 = CONICAL_SURFACE ( 'NONE', #16039, 0.9999998338055000602, 0.7853981908209605178 ) ;
#18301 = CARTESIAN_POINT ( 'NONE',  ( 8.898101285863999621, -4.735211557675400584, -6.626387721327399838 ) ) ;
#18302 = CARTESIAN_POINT ( 'NONE',  ( 9.666846873516664829, -3.231816600031351516, -6.500416447002278275 ) ) ;
#18303 = CARTESIAN_POINT ( 'NONE',  ( 5.599162447775000828, -0.8041423837011999476, 1.228772791746999937 ) ) ;
#18304 = CIRCLE ( 'NONE', #1526, 12.42499880353999941 ) ;
#18305 = CARTESIAN_POINT ( 'NONE',  ( 24.72545694048200104, -3.605123969772000336, 12.13009300416999992 ) ) ;
#18306 = CARTESIAN_POINT ( 'NONE',  ( 10.57980110216399972, 3.260758259645400337, -7.048535450274799885 ) ) ;
#18307 = DIRECTION ( 'NONE',  ( 0.000000000000000000, 1.000000000000000000, 0.000000000000000000 ) ) ;
#18308 = CARTESIAN_POINT ( 'NONE',  ( 9.485316810687001166, -2.477793449086000077, -8.275032865112999403 ) ) ;
#18309 = CARTESIAN_POINT ( 'NONE',  ( 25.25777602213000250, 11.13232791465999938, 3.460084468564999849 ) ) ;
#18310 = ORIENTED_EDGE ( 'NONE', *, *, #62037, .F. ) ;
#18311 = CARTESIAN_POINT ( 'NONE',  ( 24.45998291059600049, -11.93731034918999967, -3.254645430195999722 ) ) ;
#18312 = EDGE_CURVE ( 'NONE', #21446, #66731, #23006, .T. ) ;
#18313 = CARTESIAN_POINT ( 'NONE',  ( 12.09164601416805418, -0.1306247939804573710, -13.99939550958098344 ) ) ;
#18314 = EDGE_CURVE ( 'NONE', #59129, #426, #10062, .T. ) ;
#18315 = CARTESIAN_POINT ( 'NONE',  ( 20.00000000000000000, -11.79499999999999993, 0.000000000000000000 ) ) ;
#18316 = CARTESIAN_POINT ( 'NONE',  ( 25.52465649271900006, -8.322333800095998768, -8.137666643170000214 ) ) ;
#18317 = CARTESIAN_POINT ( 'NONE',  ( 3.500000000000000000, -2.946081722130999836, 0.9972449351501998516 ) ) ;
#18318 = CARTESIAN_POINT ( 'NONE',  ( 6.999999999999996447, 8.647867546315030296, 4.556671657224676153 ) ) ;
#18319 = CARTESIAN_POINT ( 'NONE',  ( 13.37677363193000168, 12.31133347089000019, 1.988942882797000156 ) ) ;
#18320 = VERTEX_POINT ( 'NONE', #51343 ) ;
#18321 = CARTESIAN_POINT ( 'NONE',  ( 23.89320776801300283, 8.928716006283003992, 8.952507060077003587 ) ) ;
#18322 = CARTESIAN_POINT ( 'NONE',  ( 17.98481728017920744, 2.046093834626821373, -13.75931539188737673 ) ) ;
#18323 = ORIENTED_EDGE ( 'NONE', *, *, #18399, .F. ) ;
#18324 = PLANE ( 'NONE',  #19447 ) ;
#18325 = DIRECTION ( 'NONE',  ( 1.000000000000000000, 0.000000000000000000, 0.000000000000000000 ) ) ;
#18326 = CARTESIAN_POINT ( 'NONE',  ( 9.889535841229999846, 5.798263352390999437, -8.113145944980999502 ) ) ;
#18327 = CARTESIAN_POINT ( 'NONE',  ( 11.54664311227086948, -3.555960431980462300, 6.293666904468257606 ) ) ;
#18328 = CARTESIAN_POINT ( 'NONE',  ( 10.76346886766499900, -4.634677072395899877, -6.346853961441000003 ) ) ;
#18329 = CARTESIAN_POINT ( 'NONE',  ( 9.276366930216616069, -4.996498776711455925, -6.096478446050083377 ) ) ;
#18330 = CARTESIAN_POINT ( 'NONE',  ( 4.815443173016668688, 1.499999999999999778, 0.1963495408493654004 ) ) ;
#18331 = ORIENTED_EDGE ( 'NONE', *, *, #33192, .T. ) ;
#18332 = CARTESIAN_POINT ( 'NONE',  ( 10.19256470245000123, -2.560274838243000062, 7.664550593243999899 ) ) ;
#18333 = B_SPLINE_CURVE_WITH_KNOTS ( 'NONE', 3,
 ( #66494, #3218, #35046, #24885 ),
 .UNSPECIFIED., .F., .F.,
 ( 4, 4 ),
 ( 0.000000000000000000, 1.000000000000000000 ),
 .UNSPECIFIED. ) ;
#18334 = B_SPLINE_CURVE_WITH_KNOTS ( 'NONE', 3,
 ( #55221, #7321, #49975, #699, #48943, #43701, #2090, #44745, #59421, #38446, #61837, #45085, #56598, #56255, #51351, #57268, #67752, #30048 ),
 .UNSPECIFIED., .F., .F.,
 ( 4, 2, 2, 2, 2, 2, 2, 2, 4 ),
 ( 0.000000000000000000, 0.1250000000000000000, 0.2500000000000000000, 0.3750000000000000000, 0.5000000000000000000, 0.6250000000000000000, 0.7500000000000000000, 0.8750000000000000000, 1.000000000000000000 ),
 .UNSPECIFIED. ) ;
#18335 = CARTESIAN_POINT ( 'NONE',  ( 18.15125492452900957, -2.687770500432731691, -13.63179079422069861 ) ) ;
#18336 = DIRECTION ( 'NONE',  ( 0.000000000000000000, 0.9916377111174247139, 0.1290528957048031888 ) ) ;
#18337 = ORIENTED_EDGE ( 'NONE', *, *, #18573, .T. ) ;
#18338 = EDGE_CURVE ( 'NONE', #37252, #23962, #67207, .T. ) ;
#18339 = AXIS2_PLACEMENT_3D ( 'NONE', #54383, #65209, #27134 ) ;
#18340 = CARTESIAN_POINT ( 'NONE',  ( 10.06728116094000036, 4.192860729918999496, -5.985054792427000336 ) ) ;
#18341 = DIRECTION ( 'NONE',  ( 1.000000000000000000, 0.000000000000000000, 0.000000000000000000 ) ) ;
#18342 = ORIENTED_EDGE ( 'NONE', *, *, #57313, .F. ) ;
#18343 = CARTESIAN_POINT ( 'NONE',  ( 9.959912909067998754, 3.190593056227700064, 6.509421987543800192 ) ) ;
#18344 = CARTESIAN_POINT ( 'NONE',  ( 18.16715147695115817, -2.094590662098729794, -12.42468172752983868 ) ) ;
#18345 = DIRECTION ( 'NONE',  ( 0.000000000000000000, -1.000000000000000000, 0.000000000000000000 ) ) ;
#18346 = PLANE ( 'NONE',  #3714 ) ;
#18347 = CARTESIAN_POINT ( 'NONE',  ( 11.75761329816000078, -11.49411629629000053, -1.653020190619000074 ) ) ;
#18348 = CARTESIAN_POINT ( 'NONE',  ( 9.231405316140000039, 3.815922504313999930, 6.652755395362000002 ) ) ;
#18349 = CARTESIAN_POINT ( 'NONE',  ( 9.382621648424837701, -2.846608892234664623, 8.802369146277571943 ) ) ;
#18350 = ORIENTED_EDGE ( 'NONE', *, *, #20871, .F. ) ;
#18351 = CARTESIAN_POINT ( 'NONE',  ( 8.250655866767852231, -4.995175266012890525, 6.333805738284204345 ) ) ;
#18352 = CARTESIAN_POINT ( 'NONE',  ( 10.20607971959000082, 2.622352165399999713, -6.528536464360000124 ) ) ;
#18353 = VECTOR ( 'NONE', #7146, 1000.000000000000000 ) ;
#18354 = CARTESIAN_POINT ( 'NONE',  ( 17.55505043854147118, -3.248147246781390329, -13.61798588129781074 ) ) ;
#18355 = CARTESIAN_POINT ( 'NONE',  ( 12.25686392147156667, 2.040034559784659418, -13.85057184956195542 ) ) ;
#18356 = CARTESIAN_POINT ( 'NONE',  ( 10.36825461470400001, -5.239722547583999912, -7.815392442832299835 ) ) ;
#18357 = CARTESIAN_POINT ( 'NONE',  ( 10.77962878203999963, -2.397503436487000261, 7.755423856053000442 ) ) ;
#18358 = CARTESIAN_POINT ( 'NONE',  ( 18.10142235202799199, 0.3036576181174170941, 13.89554011873103612 ) ) ;
#18359 = CIRCLE ( 'NONE', #41805, 12.50000000000000000 ) ;
#18360 = CARTESIAN_POINT ( 'NONE',  ( 10.22180282789683403, 2.874603711584076571, 6.749639981064802008 ) ) ;
#18361 = B_SPLINE_CURVE_WITH_KNOTS ( 'NONE', 3,
 ( #20524, #35920, #5129, #26466, #62818, #14937 ),
 .UNSPECIFIED., .F., .F.,
 ( 4, 2, 4 ),
 ( 0.000000000000000000, 0.5000000000000000000, 1.000000000000000000 ),
 .UNSPECIFIED. ) ;
#18362 = VERTEX_POINT ( 'NONE', #21579 ) ;
#18363 = ORIENTED_EDGE ( 'NONE', *, *, #25219, .T. ) ;
#18364 = CARTESIAN_POINT ( 'NONE',  ( 9.535554719593998030, 3.927090956378999742, -9.230892435423001530 ) ) ;
#18365 = EDGE_CURVE ( 'NONE', #2080, #29508, #33121, .T. ) ;
#18366 = CARTESIAN_POINT ( 'NONE',  ( 12.18002302684040572, 0.03981422818502264316, 13.90000146831297023 ) ) ;
#18367 = CARTESIAN_POINT ( 'NONE',  ( 12.19576242957797518, -2.360357254127059434, 13.70208745183731835 ) ) ;
#18368 = CARTESIAN_POINT ( 'NONE',  ( 10.95319771758351735, 2.911823740494093649, -4.928389130528513462 ) ) ;
#18369 = CARTESIAN_POINT ( 'NONE',  ( 9.181706853207000307, -3.734278838175999482, 8.942129638874000364 ) ) ;
#18370 = CARTESIAN_POINT ( 'NONE',  ( 8.316694573732000606, -2.898380360490000029, 6.611503418275999522 ) ) ;
#18372 = DIRECTION ( 'NONE',  ( -0.000000000000000000, -0.000000000000000000, 1.000000000000000000 ) ) ;
#18371 = CARTESIAN_POINT ( 'NONE',  ( 10.43564655415099907, -3.447209681134600245, 6.500921769151600138 ) ) ;
#18373 = CARTESIAN_POINT ( 'NONE',  ( 10.73964560330029983, 4.391636236366600166, -6.283473206644000442 ) ) ;
#18374 = ORIENTED_EDGE ( 'NONE', *, *, #33192, .F. ) ;
#18375 = CARTESIAN_POINT ( 'NONE',  ( 12.57118179866913366, -0.6928235585660844631, 13.98285841810620234 ) ) ;
#18376 = CARTESIAN_POINT ( 'NONE',  ( 10.85500481460000088, -2.931066281534000062, -5.151242807010000035 ) ) ;
#18377 = CARTESIAN_POINT ( 'NONE',  ( 4.700001368028300597, 0.000000000000000000, 0.000000000000000000 ) ) ;
#18378 = CARTESIAN_POINT ( 'NONE',  ( 12.20062903852581293, -0.1603600964026583309, 12.69865684038667908 ) ) ;
#18379 = CARTESIAN_POINT ( 'NONE',  ( 18.13957898673052327, -2.721486385301765676, -12.39720401458348675 ) ) ;
#18380 = ORIENTED_EDGE ( 'NONE', *, *, #10415, .T. ) ;
#18382 = CARTESIAN_POINT ( 'NONE',  ( 8.893723582519571735, 5.100000000000000533, -6.421373690736477791 ) ) ;
#18381 = CARTESIAN_POINT ( 'NONE',  ( 9.251933059621999078, -5.159251056493999954, 9.109488373271000583 ) ) ;
#18383 = CARTESIAN_POINT ( 'NONE',  ( 8.962479719595000560, 2.546924812613000189, -6.918870225297999887 ) ) ;
#18384 = CARTESIAN_POINT ( 'NONE',  ( 12.35317296531423104, -2.068098628661974914, 13.75563068618459184 ) ) ;
#18385 = CARTESIAN_POINT ( 'NONE',  ( 10.12426357027499790, 5.254871132332000094, 7.257895958275299542 ) ) ;
#18386 = AXIS2_PLACEMENT_3D ( 'NONE', #5737, #58198, #5053 ) ;
#18387 = DIRECTION ( 'NONE',  ( -1.000000000000000000, 0.000000000000000000, 0.000000000000000000 ) ) ;
#18388 = B_SPLINE_SURFACE_WITH_KNOTS ( 'NONE', 1, 3, ( 
 ( #64990, #33204, #54523, #6625, #22699, #44044, #65348, #27268, #49622, #1727, #345, #53829, #48591, #44397, #17468, #54870, #694, #11514, #6970, #21662, #32858, #32178, #54169, #53491, #5583, #22006, #42995, #64304, #37750, #16422, #11177, #43354, #65696, #34934, #24436, #40506, #39484, #39134, #3102, #34598, #55911, #12917, #29702, #33898, #61153, #17820, #60461, #18508, #13271, #24089, #61831, #13951, #2764, #30042, #12568, #23742, #55565, #45422, #66732, #8014, #29352, #18851, #45762, #67070, #7666, #51346, #3438, #7315, #34245, #29013, #24775, #13612, #19183, #50319, #50663, #35276, #2084, #40178, #55216, #45080, #56593, #39832, #2418, #61494, #8357, #18162, #56250, #28657, #51004, #49969, #8699, #23402, #44740, #60806, #66038, #66387, #14967, #36291, #62512, #10065, #14293, #41536, #46102, #40850, #68094, #62849, #4463, #42241 ),
 ( #67408, #56934, #58302, #52018, #14630, #68786, #46788, #31399, #19530, #35949, #25803, #47136, #4812, #57610, #4119, #62171, #25115, #20211, #5165, #36990, #35622, #10406, #9031, #30372, #51680, #67747, #41882, #19871, #3778, #30709, #68435, #57263, #9363, #25456, #41202, #9715, #31060, #52370, #52715, #26153, #63546, #20557, #47479, #57965, #63188, #15318, #36642, #20903, #15658, #31748, #53065, #46446, #37326, #48856, #33470, #38358, #16682, #69138, #59335, #964, #59684, #266, #22275, #27186, #32435, #60030, #54090, #43264, #53751, #48163, #6188, #27883, #11783, #48508, #37668, #64569, #64912, #38010, #22617, #43960, #11436, #58650, #43618, #54786, #33123, #32777, #21246, #27529, #17026, #54438, #21581, #6539, #614, #5848, #12139, #49194, #1302, #21926, #42918, #65267, #17381, #5509, #38710, #26498, #47828, #42573, #63883, #64225 ) ),
 .UNSPECIFIED., .F., .F., .F.,
 ( 2, 2 ),
 ( 4, 2, 2, 2, 2, 2, 2, 2, 2, 2, 2, 2, 2, 2, 2, 2, 2, 2, 2, 2, 2, 2, 2, 2, 2, 2, 2, 2, 2, 2, 2, 2, 2, 2, 2, 2, 2, 2, 2, 2, 2, 2, 2, 2, 2, 2, 2, 2, 2, 2, 2, 2, 2, 4 ),
 ( 0.000000000000000000, 1.000000000000000000 ),
 ( 0.000000000000000000, 7.156607294609339200E-05, 0.0001431321458921867840, 0.0001789151823652334597, 0.0002146982188382801624, 0.0002325897370748035138, 0.0002504812553113268652, 0.0002862642917843735680, 0.0003220473282574202708, 0.0003578303647304669193, 0.0003936134012035136221, 0.0004293964376765603249, 0.0004651794741496070276, 0.0004830709923861303519, 0.0005009625106226537304, 0.0005725285835687471360, 0.0006440946565148405415, 0.0007156607294609338386, 0.0007872268024070272442, 0.0008587928753531206497, 0.0008945759118261674067, 0.0009303589482992140553, 0.0009661419847722607038, 0.001001925021245307461, 0.001037708057718354218, 0.001073491094191400975, 0.001145057167137494272, 0.001180840203610541029, 0.001216623240083587569, 0.001252406276556634326, 0.001288189313029681083, 0.001359755385975774380, 0.001395538422448821137, 0.001431321458921867677, 0.001467104495394914434, 0.001502887531867961191, 0.001574453604814054488, 0.001646019677760147785, 0.001681802714233194542, 0.001717585750706241299, 0.001753368787179288056, 0.001789151823652334813, 0.001860717896598428111, 0.001896500933071474868, 0.001932283969544521408, 0.001968067006017567948, 0.002003850042490614922, 0.002039633078963661895, 0.002075416115436708436, 0.002146982188382801950, 0.002182765224855848490, 0.002218548261328895030, 0.002254331297801942004, 0.002290114334274988544 ),
 .UNSPECIFIED. ) ;
#18389 = CARTESIAN_POINT ( 'NONE',  ( 9.309825924086673865, 4.346446645907335871, 9.216763236637257606 ) ) ;
#18390 = CARTESIAN_POINT ( 'NONE',  ( 2.129593803058000390, 1.784639509494000187, -2.764404103036999683 ) ) ;
#18391 = EDGE_LOOP ( 'NONE', ( #20618, #47515, #67588, #21638, #10347, #3486, #28268, #40476, #12564, #41186 ) ) ;
#18392 = CARTESIAN_POINT ( 'NONE',  ( 12.25943167926922861, 0.4738025322793235627, -12.59109159930368449 ) ) ;
#18393 = CARTESIAN_POINT ( 'NONE',  ( 7.800894438721999613, -3.218815632501999868, 6.398977300879999497 ) ) ;
#18394 = CARTESIAN_POINT ( 'NONE',  ( 24.14324442345568400, -12.47686306304178139, -3.361569000410982611 ) ) ;
#18395 = CARTESIAN_POINT ( 'NONE',  ( 7.678989158771000412, 2.599243720295000060, 7.909344432242998657 ) ) ;
#18396 = ORIENTED_EDGE ( 'NONE', *, *, #1197, .T. ) ;
#18397 = CARTESIAN_POINT ( 'NONE',  ( 5.600631947950999390, -0.1174666901181000006, -1.463806399069999875 ) ) ;
#18398 = ADVANCED_FACE ( 'NONE', ( #38007 ), #33580, .F. ) ;
#18399 = EDGE_CURVE ( 'NONE', #32077, #43802, #65850, .T. ) ;
#18400 = CARTESIAN_POINT ( 'NONE',  ( 7.391135841228000380, 2.898440551356999961, -6.639986657414999272 ) ) ;
#18402 = CARTESIAN_POINT ( 'NONE',  ( 24.53429014662800256, -8.855930250654999725, 9.286429702500999639 ) ) ;
#18401 = DIRECTION ( 'NONE',  ( 1.000000000000000000, 0.000000000000000000, 0.000000000000000000 ) ) ;
#18403 = AXIS2_PLACEMENT_3D ( 'NONE', #38283, #32369, #21513 ) ;
#18404 = CARTESIAN_POINT ( 'NONE',  ( 11.80233327354039830, 2.898463260143000042, -6.779499720266399798 ) ) ;
#18405 = ORIENTED_EDGE ( 'NONE', *, *, #7360, .T. ) ;
#18406 = PLANE ( 'NONE',  #21625 ) ;
#18407 = ORIENTED_EDGE ( 'NONE', *, *, #13974, .F. ) ;
#18408 = CARTESIAN_POINT ( 'NONE',  ( 9.457111106897940545, -5.237397863424940958, 8.039624212520665836 ) ) ;
#18409 = CARTESIAN_POINT ( 'NONE',  ( 24.95275982371617118, -8.555910667412625514, -8.377686648711669903 ) ) ;
#18410 = AXIS2_PLACEMENT_3D ( 'NONE', #4299, #41372, #63013 ) ;
#18411 = CARTESIAN_POINT ( 'NONE',  ( 18.25531185377812449, -0.1895042076700518829, -13.99872220539657697 ) ) ;
#18412 = ORIENTED_EDGE ( 'NONE', *, *, #57294, .F. ) ;
#18413 = CARTESIAN_POINT ( 'NONE',  ( 7.603392156809999136, -9.092031481190000264, 5.808920680900000022 ) ) ;
#18414 = DIRECTION ( 'NONE',  ( 1.000000000000000000, 0.000000000000000000, 0.000000000000000000 ) ) ;
#18415 = DIRECTION ( 'NONE',  ( 1.000000000000000000, 0.000000000000000000, 0.000000000000000000 ) ) ;
#18416 = CARTESIAN_POINT ( 'NONE',  ( 9.143998948451265818, -2.899999999999999911, 6.465127702479446015 ) ) ;
#18417 = CARTESIAN_POINT ( 'NONE',  ( 18.17920460084962286, -2.538974945121682758, 12.44245230910560451 ) ) ;
#18418 = ORIENTED_EDGE ( 'NONE', *, *, #19487, .F. ) ;
#18419 = LINE ( 'NONE', #1642, #24233 ) ;
#18420 = CARTESIAN_POINT ( 'NONE',  ( 23.73802563651300090, -13.27927394169999786, -3.696043905241999994 ) ) ;
#18421 = EDGE_CURVE ( 'NONE', #18264, #16254, #62505, .T. ) ;
#18422 = CIRCLE ( 'NONE', #45218, 0.6999999999999992895 ) ;
#18423 = CARTESIAN_POINT ( 'NONE',  ( 9.685596873515667227, 5.092232985442825210, 8.129523725463618788 ) ) ;
#18424 = CARTESIAN_POINT ( 'NONE',  ( 9.725191424783300675, -2.649754699899359522, 7.500009801425228773 ) ) ;
#18425 = EDGE_LOOP ( 'NONE', ( #31781, #29701, #42367, #3956, #42667, #17221, #39495, #21806 ) ) ;
#18426 = DIRECTION ( 'NONE',  ( 0.000000000000000000, 1.000000000000000000, 0.000000000000000000 ) ) ;
#18427 = EDGE_CURVE ( 'NONE', #67391, #21093, #10502, .T. ) ;
#18428 = CARTESIAN_POINT ( 'NONE',  ( 11.03482133862663517, 4.942979055179590908, -8.373613860257943742 ) ) ;
#18429 = CARTESIAN_POINT ( 'NONE',  ( 8.137522165044002165, 2.460709986978387054, -6.460953617291827378 ) ) ;
#18430 = CARTESIAN_POINT ( 'NONE',  ( 10.00551210286899995, -4.217228369037729685, -8.756187319522087620 ) ) ;
#18431 = DIRECTION ( 'NONE',  ( -1.000000000000000000, -9.409886301854999796E-10, -4.862374338246000196E-11 ) ) ;
#18432 = CARTESIAN_POINT ( 'NONE',  ( 12.22351867101279232, -0.2292390942789200303, -13.89746050377129727 ) ) ;
#18433 = CARTESIAN_POINT ( 'NONE',  ( 17.98432920965427328, -2.954704375608637967, 12.33394473884601794 ) ) ;
#18434 = ORIENTED_EDGE ( 'NONE', *, *, #2220, .T. ) ;
#18435 = CARTESIAN_POINT ( 'NONE',  ( 11.59603632436369125, -4.842640371965599932, -7.303218851299499548 ) ) ;
#18436 = ORIENTED_EDGE ( 'NONE', *, *, #48533, .F. ) ;
#18437 = CARTESIAN_POINT ( 'NONE',  ( 0.1499942179680000265, 0.3599680999393979897, 2.749953718116143531 ) ) ;
#18438 = CARTESIAN_POINT ( 'NONE',  ( 9.377520280414000098, 4.092867382745001059, -5.937785237406000505 ) ) ;
#18439 = CARTESIAN_POINT ( 'NONE',  ( 2.664069943672000118, 1.422849972570999988, -2.883063314296999913 ) ) ;
#18440 = B_SPLINE_CURVE_WITH_KNOTS ( 'NONE', 3,
 ( #44693, #40456, #18805, #13564, #2372, #65988, #39432, #60753, #13902, #45029, #7616, #12868, #29654, #34884, #34196, #61102, #28963, #3053 ),
 .UNSPECIFIED., .F., .F.,
 ( 4, 2, 2, 2, 2, 2, 2, 2, 4 ),
 ( 0.000000000000000000, 0.1250000000000000833, 0.2500000000000001110, 0.3750000000000001665, 0.5000000000000002220, 0.6250000000000002220, 0.7500000000000001110, 0.8750000000000001110, 1.000000000000000000 ),
 .UNSPECIFIED. ) ;
#18441 = CARTESIAN_POINT ( 'NONE',  ( 9.910158555493998378, -2.531067292016000003, -7.917737669614999696 ) ) ;
#18442 = CARTESIAN_POINT ( 'NONE',  ( 6.899999438051000133, 1.266765207443000030, 0.8033093483900000109 ) ) ;
#18443 = CARTESIAN_POINT ( 'NONE',  ( 7.924470805432005882, 3.443171588504001068, -6.303962341916999890 ) ) ;
#18444 = ORIENTED_EDGE ( 'NONE', *, *, #20398, .F. ) ;
#18445 = CARTESIAN_POINT ( 'NONE',  ( 12.01102763632551884, -4.911148285670300595, 7.920427941950599404 ) ) ;
#18446 = CARTESIAN_POINT ( 'NONE',  ( 10.96580581817999978, 4.930645553951000792, 6.170542400361000546 ) ) ;
#18447 = CARTESIAN_POINT ( 'NONE',  ( 24.34833259009266726, -8.895958638017500419, -8.895958638017500419 ) ) ;
#18448 = LINE ( 'NONE', #55157, #25364 ) ;
#18449 = CARTESIAN_POINT ( 'NONE',  ( 10.95833333333431980, 4.952949899269658118, 8.562434272074012753 ) ) ;
#18450 = CARTESIAN_POINT ( 'NONE',  ( 10.72749279009019929, 3.774717370312400178, -8.336388861178200216 ) ) ;
#18452 = CARTESIAN_POINT ( 'NONE',  ( 24.95781814977000224, -12.04098704729999803, 2.875621858674000109 ) ) ;
#18451 = ITEM_DEFINED_TRANSFORMATION ( 'NONE', 'NONE', #66433,  #9676 ) ;
#18453 = VECTOR ( 'NONE', #60169, 1000.000000000000000 ) ;
#18454 = EDGE_CURVE ( 'NONE', #37636, #29023, #46901, .T. ) ;
#18455 = CARTESIAN_POINT ( 'NONE',  ( 9.477709346417000802, 4.907312911337299965, -7.069157126958599768 ) ) ;
#18456 = CARTESIAN_POINT ( 'NONE',  ( 18.24522866045826675, -0.2205548374446849313, 12.59807454672507632 ) ) ;
#18457 = CARTESIAN_POINT ( 'NONE',  ( 9.133199450400327990, -5.099761357576727328, 6.159710572180335575 ) ) ;
#18458 = CARTESIAN_POINT ( 'NONE',  ( 10.91620964606000044, 2.818413279081999789, -6.814156272943999504 ) ) ;
#18459 = CARTESIAN_POINT ( 'NONE',  ( 10.17270667456000055, 4.650145611776999921, -8.655516756809999990 ) ) ;
#18460 = ORIENTED_EDGE ( 'NONE', *, *, #65734, .T. ) ;
#18461 = CARTESIAN_POINT ( 'NONE',  ( 7.924355646793000751, -2.432121990576000314, 6.597519606637999523 ) ) ;
#18462 = CARTESIAN_POINT ( 'NONE',  ( 17.92097207270825265, 1.887179018856774748, 13.87222722961341326 ) ) ;
#18463 = CARTESIAN_POINT ( 'NONE',  ( 23.56666365135700403, -2.963314674619003330, 12.23574966049000423 ) ) ;
#18464 = CARTESIAN_POINT ( 'NONE',  ( 9.843930206850000530, -5.250000000000000000, -7.500000000000000000 ) ) ;
#18465 = ORIENTED_EDGE ( 'NONE', *, *, #33187, .F. ) ;
#18466 = CARTESIAN_POINT ( 'NONE',  ( 17.87616489729400371, 3.527537751923000009, 11.96092219328000006 ) ) ;
#18468 = CARTESIAN_POINT ( 'NONE',  ( 9.234020077949999461, -4.063547279775290733, 6.621188087644399367 ) ) ;
#18467 = CARTESIAN_POINT ( 'NONE',  ( 10.19391290906799874, -4.548591194283900130, -8.171383386399000415 ) ) ;
#18469 = CARTESIAN_POINT ( 'NONE',  ( 11.08729332543999924, 2.258658230726000138, -7.034579402814999938 ) ) ;
#18470 = ORIENTED_EDGE ( 'NONE', *, *, #53310, .F. ) ;
#18471 = CARTESIAN_POINT ( 'NONE',  ( 9.353724647487000610, 2.823567847429000022, 9.032053040610000139 ) ) ;
#18472 = CARTESIAN_POINT ( 'NONE',  ( 10.10000000000000142, -12.35000000006999876, 0.000000000000000000 ) ) ;
#18473 = CARTESIAN_POINT ( 'NONE',  ( 11.62994988689359843, 4.518136976474400157, 6.483720595741000459 ) ) ;
#18474 = CARTESIAN_POINT ( 'NONE',  ( 9.799258316471000541, -4.057329063942999525, 9.430691159271001212 ) ) ;
#18475 = CARTESIAN_POINT ( 'NONE',  ( 30.60000000000000142, 0.000000000000000000, 0.000000000000000000 ) ) ;
#18476 = ORIENTED_EDGE ( 'NONE', *, *, #37007, .T. ) ;
#18477 = CYLINDRICAL_SURFACE ( 'NONE', #25470, 0.5000000000000002220 ) ;
#18478 = ADVANCED_FACE ( 'NONE', ( #52246 ), #41418, .F. ) ;
#18479 = EDGE_CURVE ( 'NONE', #54437, #8552, #58520, .T. ) ;
#18480 = CARTESIAN_POINT ( 'NONE',  ( 13.99999997324030865, 8.827177816329516702, 7.803278505680539823 ) ) ;
#18481 = CARTESIAN_POINT ( 'NONE',  ( 8.060801445049092351, -3.692626997221928331, 5.787670773964787685 ) ) ;
#18482 = CARTESIAN_POINT ( 'NONE',  ( 9.166075977534999808, -4.023333687735000552, 9.122281080215000060 ) ) ;
#18483 = CARTESIAN_POINT ( 'NONE',  ( 10.93479632507519916, -3.442212747724900268, -8.534037301706000278 ) ) ;
#18484 = CARTESIAN_POINT ( 'NONE',  ( 9.704063610504999104, -3.588011994494999968, 6.583971515917899531 ) ) ;
#18485 = ORIENTED_EDGE ( 'NONE', *, *, #34023, .T. ) ;
#18486 = DIRECTION ( 'NONE',  ( -1.000000000000000000, 0.000000000000000000, 0.000000000000000000 ) ) ;
#18487 = EDGE_CURVE ( 'NONE', #17632, #36266, #35535, .T. ) ;
#18488 = B_SPLINE_CURVE_WITH_KNOTS ( 'NONE', 3,
 ( #41798, #15229, #41116, #9628 ),
 .UNSPECIFIED., .F., .F.,
 ( 4, 4 ),
 ( 0.000000000000000000, 1.000000000000000000 ),
 .UNSPECIFIED. ) ;
#18489 = CARTESIAN_POINT ( 'NONE',  ( 10.80072469555900128, -3.429147315060100176, 8.487632181750699445 ) ) ;
#18490 = ORIENTED_EDGE ( 'NONE', *, *, #6068, .F. ) ;
#18491 = DIRECTION ( 'NONE',  ( 1.000000000000000000, 0.000000000000000000, 0.000000000000000000 ) ) ;
#18492 = ORIENTED_EDGE ( 'NONE', *, *, #4738, .T. ) ;
#18493 = B_SPLINE_CURVE_WITH_KNOTS ( 'NONE', 3,
 ( #51384, #3481, #45798, #40546, #34285, #24817, #66078, #61192, #45461, #18199, #13313, #67111, #60846, #66425, #29047, #35316, #34635, #55947, #8052, #50703, #24126, #13648, #66775, #46143, #18891, #40216, #56634, #34976, #8737, #40894, #35658, #62890, #57650, #68475, #37029, #58341, #47172 ),
 .UNSPECIFIED., .F., .F.,
 ( 4, 2, 2, 2, 2, 2, 2, 2, 2, 1, 1, 1, 2, 2, 2, 2, 2, 2, 2, 4 ),
 ( 0.000000000000000000, 0.06250000000000018041, 0.1250000000000003608, 0.1875000000000005551, 0.2500000000000007216, 0.3125000000000008882, 0.3750000000000011102, 0.4375000000000012768, 0.4687500000000014433, 0.4843750000000012212, 0.4921875000000011657, 0.4960937500000008327, 0.4980468750000006106, 0.5000000000000003331, 0.6250000000000004441, 0.7500000000000005551, 0.8125000000000004441, 0.8750000000000003331, 0.9375000000000001110, 1.000000000000000000 ),
 .UNSPECIFIED. ) ;
#18494 = CARTESIAN_POINT ( 'NONE',  ( 18.50001572531400029, -1.956586073098988354, -12.40985500209093928 ) ) ;
#18495 = CARTESIAN_POINT ( 'NONE',  ( 9.640910841231999484, 2.212639797530000063, -6.855876382544999537 ) ) ;
#18496 = CARTESIAN_POINT ( 'NONE',  ( 11.59456039236534330, 5.314711678001000195, -7.563984187103470092 ) ) ;
#18497 = LINE ( 'NONE', #17810, #27683 ) ;
#18498 = CARTESIAN_POINT ( 'NONE',  ( 12.14412415394998668, 2.776584135961351674, -12.29026848248285830 ) ) ;
#18499 = CARTESIAN_POINT ( 'NONE',  ( 11.39564560330030041, -3.692495237344800341, 8.455191956516999952 ) ) ;
#18500 = CARTESIAN_POINT ( 'NONE',  ( 11.19057802013490033, -5.033226574983999946, 7.524052967375959966 ) ) ;
#18501 = VERTEX_POINT ( 'NONE', #31969 ) ;
#18502 = CARTESIAN_POINT ( 'NONE',  ( 9.614763540183330903, 5.217465845835394411, 7.827184855449092815 ) ) ;
#18503 = AXIS2_PLACEMENT_3D ( 'NONE', #67883, #3904, #47259 ) ;
#18504 = ORIENTED_EDGE ( 'NONE', *, *, #35927, .T. ) ;
#18505 = CARTESIAN_POINT ( 'NONE',  ( 8.636456853209999451, -3.869396851328000153, 5.695656592546999519 ) ) ;
#18506 = CARTESIAN_POINT ( 'NONE',  ( 24.01911657365105768, 9.335961567032249775, 9.253293928180594818 ) ) ;
#18507 = ORIENTED_EDGE ( 'NONE', *, *, #28058, .T. ) ;
#18508 = CARTESIAN_POINT ( 'NONE',  ( 12.09179812036145663, -2.610377073672084158, -12.32664058968471998 ) ) ;
#18509 = EDGE_CURVE ( 'NONE', #44907, #62317, #44700, .T. ) ;
#18511 = CARTESIAN_POINT ( 'NONE',  ( 11.08841369783139896, 3.942447888101379583, 6.360711682373000109 ) ) ;
#18510 = VECTOR ( 'NONE', #27740, 1000.000000000000000 ) ;
#18512 = CARTESIAN_POINT ( 'NONE',  ( 10.03977055961999909, -2.255583827894000137, -8.111980070942999888 ) ) ;
#18513 = CARTESIAN_POINT ( 'NONE',  ( 2.210247277619000084, 2.108360286353999413, -2.286637680308000409 ) ) ;
#18514 = CARTESIAN_POINT ( 'NONE',  ( 8.496399244692801389, 5.100022896384949433, -6.666166966519626591 ) ) ;
#18515 = CARTESIAN_POINT ( 'NONE',  ( 24.72544608131900290, -8.702416312033001589, 9.187185040896000743 ) ) ;
#18516 = CARTESIAN_POINT ( 'NONE',  ( 12.18472169747688660, -2.421093590824783703, -13.68984525495557314 ) ) ;
#18517 = CARTESIAN_POINT ( 'NONE',  ( 18.02541143671232504, -0.4116921281473265304, -12.69102089861181248 ) ) ;
#18518 = DIRECTION ( 'NONE',  ( 1.000000000000000000, 0.000000000000000000, -3.552713678909000227E-14 ) ) ;
#18519 = CARTESIAN_POINT ( 'NONE',  ( 10.78887616594230003, -4.386455737425299262, -6.281817606595999415 ) ) ;
#18520 = CARTESIAN_POINT ( 'NONE',  ( 8.930989158774000458, 2.019067547072999957, 7.390982789861999969 ) ) ;
#18521 = ORIENTED_EDGE ( 'NONE', *, *, #36470, .F. ) ;
#18522 = CYLINDRICAL_SURFACE ( 'NONE', #1223, 0.6999999999999992895 ) ;
#18523 = CARTESIAN_POINT ( 'NONE',  ( 7.397586123398784075, 4.761547826166538044, 6.352807996277898717 ) ) ;
#18524 = CARTESIAN_POINT ( 'NONE',  ( 23.95226462695299929, -3.419397922773000253, 12.89848026480999899 ) ) ;
#18525 = CARTESIAN_POINT ( 'NONE',  ( 17.81301359322643307, 3.153051599267165717, 12.19911286921121452 ) ) ;
#18526 = CARTESIAN_POINT ( 'NONE',  ( 17.55505043854143921, -0.7302158263239086899, 13.98094363220831049 ) ) ;
#18527 = CARTESIAN_POINT ( 'NONE',  ( 10.24961997674000003, 4.184221916050000267, 9.286882020979000174 ) ) ;
#18528 = CARTESIAN_POINT ( 'NONE',  ( 8.037016222020598732, 5.285842885613642572, -7.027160484499655801 ) ) ;
#18529 = CARTESIAN_POINT ( 'NONE',  ( 12.57114114721769838, -0.6824382160044792922, -12.58151825845880367 ) ) ;
#18530 = VERTEX_POINT ( 'NONE', #36511 ) ;
#18531 = CARTESIAN_POINT ( 'NONE',  ( 12.25653845796827035, -2.200227119461482861, 12.51640343681225787 ) ) ;
#18532 = CARTESIAN_POINT ( 'NONE',  ( 10.26090035061499961, -3.768906505327899836, -8.335645555860798694 ) ) ;
#18533 = CARTESIAN_POINT ( 'NONE',  ( 10.92717848204000042, 5.023653513500000223, 8.718036113327999104 ) ) ;
#18534 = CARTESIAN_POINT ( 'NONE',  ( 12.33003632436370012, -5.243255406354000669, 7.790336465152099876 ) ) ;
#18535 = CARTESIAN_POINT ( 'NONE',  ( 10.89149144726329865, 3.340422662105400065, -6.569275630703699242 ) ) ;
#18536 = CARTESIAN_POINT ( 'NONE',  ( 12.31563516348837695, 0.3888461597108430756, 12.69199065798140680 ) ) ;
#18537 = AXIS2_PLACEMENT_3D ( 'NONE', #45553, #66859, #18972 ) ;
#18538 = EDGE_CURVE ( 'NONE', #61665, #34641, #29103, .T. ) ;
#18539 = EDGE_CURVE ( 'NONE', #3659, #24513, #26844, .T. ) ;
#18540 = CARTESIAN_POINT ( 'NONE',  ( 8.674239158774001979, 5.983047240001000411, 7.440798119034999658 ) ) ;
#18541 = CARTESIAN_POINT ( 'NONE',  ( 11.11845610223999969, 5.767025078915000158, 7.178418469370999588 ) ) ;
#18542 = CARTESIAN_POINT ( 'NONE',  ( 12.64104727702813413, 1.896551500700491832, 12.57186431639862256 ) ) ;
#18543 = EDGE_LOOP ( 'NONE', ( #67886, #36945, #66121, #12979, #38531, #22944, #25086 ) ) ;
#18544 = CARTESIAN_POINT ( 'NONE',  ( 8.400739158770999637, 4.933589693325000525, -9.154576215408999573 ) ) ;
#18545 = CARTESIAN_POINT ( 'NONE',  ( 10.61656919669529842, 5.225637333137999718, -7.862118085997298778 ) ) ;
#18546 = DIRECTION ( 'NONE',  ( 0.000000000000000000, -1.000000000000000000, 0.000000000000000000 ) ) ;
#18548 = CARTESIAN_POINT ( 'NONE',  ( 1.550973465874000201, 3.500000000000000000, 0.000000000000000000 ) ) ;
#18547 = CARTESIAN_POINT ( 'NONE',  ( 11.50002032348423242, -3.558966193428903413, 11.09334449156782654 ) ) ;
#18549 = CARTESIAN_POINT ( 'NONE',  ( 9.881367640780998940, -3.526522998810799781, 8.385811396220899994 ) ) ;
#18550 = CARTESIAN_POINT ( 'NONE',  ( 11.09672200990539892, -4.817867935977999672, -7.214709569664399247 ) ) ;
#18551 = EDGE_LOOP ( 'NONE', ( #28487, #19341, #21672, #44464, #43433, #43043 ) ) ;
#18552 = CIRCLE ( 'NONE', #68781, 11.35000000000000675 ) ;
#18553 = CARTESIAN_POINT ( 'NONE',  ( 1.500974932896000036, -3.258362327980000028, 0.06604197684371000687 ) ) ;
#18554 = CARTESIAN_POINT ( 'NONE',  ( 18.07980528509186868, -0.3396180385173929173, -12.69389128024175939 ) ) ;
#18555 = AXIS2_PLACEMENT_3D ( 'NONE', #57886, #47402, #32020 ) ;
#18556 = LINE ( 'NONE', #61883, #22927 ) ;
#18557 = CARTESIAN_POINT ( 'NONE',  ( 17.96849574077155154, -2.968826013449940238, 13.56277633467806787 ) ) ;
#18558 = ADVANCED_BREP_SHAPE_REPRESENTATION ( '', ( #53935, #9676 ), #9731 ) ;
#18559 = DIRECTION ( 'NONE',  ( -1.000000000000000000, 0.000000000000000000, 2.886579864060000134E-14 ) ) ;
#18560 = CARTESIAN_POINT ( 'NONE',  ( 15.96457203294232841, 8.635839794706024364, 7.819790491316798153 ) ) ;
#18561 = CARTESIAN_POINT ( 'NONE',  ( 10.61094409420999973, 5.100000000000000533, -6.571291218949999902 ) ) ;
#18562 = LINE ( 'NONE', #15715, #29921 ) ;
#18563 = CARTESIAN_POINT ( 'NONE',  ( 13.58069952315600126, -12.39169461668999972, -2.069104550346000160 ) ) ;
#18564 = ORIENTED_EDGE ( 'NONE', *, *, #65878, .F. ) ;
#18565 = CARTESIAN_POINT ( 'NONE',  ( 8.753448341231001351, 2.876288091423999660, 6.568897128359000526 ) ) ;
#18566 = ADVANCED_FACE ( 'NONE', ( #25333 ), #60378, .F. ) ;
#18567 = CARTESIAN_POINT ( 'NONE',  ( 13.00000000009400303, -11.69118001589999878, -1.923222888683999932 ) ) ;
#18568 = CARTESIAN_POINT ( 'NONE',  ( 7.355148097746750935, -3.352078922218864498, 9.122887315503605876 ) ) ;
#18569 = DIRECTION ( 'NONE',  ( -2.154007395656495261E-21, 3.276905819395100166E-06, -0.9999999999946310725 ) ) ;
#18570 = CARTESIAN_POINT ( 'NONE',  ( 1.933975548942000078, -3.260690222378000325, 1.050103212221999982 ) ) ;
#18571 = ORIENTED_EDGE ( 'NONE', *, *, #12794, .F. ) ;
#18572 = DIRECTION ( 'NONE',  ( 0.7071182117976623216, 0.000000000000000000, -0.7070953503906501902 ) ) ;
#18573 = EDGE_CURVE ( 'NONE', #33733, #66584, #37873, .T. ) ;
#18574 = DIRECTION ( 'NONE',  ( -0.5000000000000169864, 0.000000000000000000, -0.8660254037844288266 ) ) ;
#18575 = CARTESIAN_POINT ( 'NONE',  ( 10.61382428715999993, 3.385080336122999967, 5.849521480782000182 ) ) ;
#18576 = CARTESIAN_POINT ( 'NONE',  ( 10.43210941423799909, 4.641185166475500168, 8.082391773166900606 ) ) ;
#18577 = CARTESIAN_POINT ( 'NONE',  ( 5.000000000000000000, 0.6153846153845999867, 2.423076923076999734 ) ) ;
#18578 = CARTESIAN_POINT ( 'NONE',  ( 18.30000000000000071, -2.818726571106858980, -11.83569999720589294 ) ) ;
#18579 = CARTESIAN_POINT ( 'NONE',  ( 18.20121223423996781, -0.3818843735617438173, -13.99543728850909297 ) ) ;
#18580 = CARTESIAN_POINT ( 'NONE',  ( 12.17041751275704620, -10.92137764442966308, 4.055351144497368665 ) ) ;
#18581 = CARTESIAN_POINT ( 'NONE',  ( 12.23606560774678087, -2.758669204864329760, 12.38755309842819763 ) ) ;
#18582 = B_SPLINE_CURVE_WITH_KNOTS ( 'NONE', 3,
 ( #46316, #67617, #30923, #26365 ),
 .UNSPECIFIED., .F., .F.,
 ( 4, 4 ),
 ( 0.000000000000000000, 1.000000000000000000 ),
 .UNSPECIFIED. ) ;
#18583 = CARTESIAN_POINT ( 'NONE',  ( 8.215396629533129769, 5.723734980850093912, 7.813254138193835630 ) ) ;
#18584 = ORIENTED_EDGE ( 'NONE', *, *, #12102, .F. ) ;
#18585 = CARTESIAN_POINT ( 'NONE',  ( 17.63746348810185793, -1.880115813469444230, 13.78555441649717928 ) ) ;
#18586 = CARTESIAN_POINT ( 'NONE',  ( 10.37041638348499895, -5.241705141469999774, -7.197535585171899619 ) ) ;
#18587 = ORIENTED_EDGE ( 'NONE', *, *, #19573, .T. ) ;
#18588 = CARTESIAN_POINT ( 'NONE',  ( 8.959695231899726053, -5.323626131866632250, 7.230905480027200127 ) ) ;
#18589 = CARTESIAN_POINT ( 'NONE',  ( 18.49996808500599954, -1.807259459756127784, 11.54438823573780759 ) ) ;
#18590 = DIRECTION ( 'NONE',  ( 1.000000000000000000, 0.000000000000000000, 0.000000000000000000 ) ) ;
#18591 = ADVANCED_FACE ( 'NONE', ( #33674 ), #37523, .F. ) ;
#18592 = CARTESIAN_POINT ( 'NONE',  ( 9.716851002543000604, -2.832432432432000269, 6.822293592207000934 ) ) ;
#18593 = AXIS2_PLACEMENT_3D ( 'NONE', #67735, #4450, #57249 ) ;
#18594 = FACE_OUTER_BOUND ( 'NONE', #40222, .T. ) ;
#18595 = CARTESIAN_POINT ( 'NONE',  ( 10.13381533919000077, 5.176445833090999926, -8.189798585019000043 ) ) ;
#18596 = CARTESIAN_POINT ( 'NONE',  ( 9.360840674114760063, -8.748618759363480990, -6.377268954453227501 ) ) ;
#18597 = CARTESIAN_POINT ( 'NONE',  ( 9.924739995124999936, -5.060461104229999840, 8.686133300732999274 ) ) ;
#18598 = CARTESIAN_POINT ( 'NONE',  ( 11.68610928851700237, 3.397019518052000198, -11.10441497445000003 ) ) ;
#18599 = CARTESIAN_POINT ( 'NONE',  ( 23.56664678325900297, -13.31363270032999857, -4.296980171176000063 ) ) ;
#18600 = CARTESIAN_POINT ( 'NONE',  ( 11.65871932425156920, -4.147141405561299621, -8.492622906483498824 ) ) ;
#18601 = B_SPLINE_CURVE_WITH_KNOTS ( 'NONE', 3,
 ( #18820, #51984, #14259, #35588 ),
 .UNSPECIFIED., .F., .F.,
 ( 4, 4 ),
 ( 0.000000000000000000, 1.000000000000000000 ),
 .UNSPECIFIED. ) ;
#18602 = ORIENTED_EDGE ( 'NONE', *, *, #17670, .T. ) ;
#18603 = AXIS2_PLACEMENT_3D ( 'NONE', #6155, #48476, #54753 ) ;
#18604 = CARTESIAN_POINT ( 'NONE',  ( 9.849204462306566654, 2.899999999999999911, -6.662590550605539619 ) ) ;
#18605 = CARTESIAN_POINT ( 'NONE',  ( 24.44496487975900223, 3.224879802562000464, -12.03535984693000138 ) ) ;
#18606 = CARTESIAN_POINT ( 'NONE',  ( 10.79415884302813389, -2.685269952713060793, -7.853379249108617621 ) ) ;
#18607 = CARTESIAN_POINT ( 'NONE',  ( 9.258504216683467902, 4.163629870566138536, 8.749972943975897977 ) ) ;
#18608 = CARTESIAN_POINT ( 'NONE',  ( 12.42225061842103173, 2.005837741177417310, 13.76588300560132261 ) ) ;
#18609 = CARTESIAN_POINT ( 'NONE',  ( 9.611390067472999732, -3.334847606888000193, 5.869121315726000709 ) ) ;
#18610 = ORIENTED_EDGE ( 'NONE', *, *, #49962, .F. ) ;
#18611 = CARTESIAN_POINT ( 'NONE',  ( 12.34510720075386558, 0.4232991632631661894, -12.69050643261670430 ) ) ;
#18612 = CARTESIAN_POINT ( 'NONE',  ( 12.58477985662609022, -0.5849891190461631307, 13.88342664904964430 ) ) ;
#18613 = ORIENTED_EDGE ( 'NONE', *, *, #59679, .T. ) ;
#18614 = FACE_OUTER_BOUND ( 'NONE', #23978, .T. ) ;
#18615 = CARTESIAN_POINT ( 'NONE',  ( 10.61094409420999973, -5.100000000000000533, -6.571291218949999902 ) ) ;
#18616 = CARTESIAN_POINT ( 'NONE',  ( 9.024266954400625096, 3.674418004489155010, 8.312113682386053526 ) ) ;
#18617 = CARTESIAN_POINT ( 'NONE',  ( 27.64127793187000037, -5.599999999999999645, 6.571291218949999902 ) ) ;
#18618 = CARTESIAN_POINT ( 'NONE',  ( 17.55505043854143565, 3.125000000000000000, -25.00000000000000000 ) ) ;
#18619 = CARTESIAN_POINT ( 'NONE',  ( 11.06992513079000062, 8.140394931567000114, -6.682140483390000441 ) ) ;
#18620 = EDGE_CURVE ( 'NONE', #14252, #5489, #63698, .T. ) ;
#18621 = ADVANCED_FACE ( 'NONE', ( #43116 ), #11989, .T. ) ;
#18622 = CARTESIAN_POINT ( 'NONE',  ( 0.5979711358043999780, 3.275095586319999974, -0.8499908244220999443 ) ) ;
#18623 = DIRECTION ( 'NONE',  ( 1.000000000000000000, 0.000000000000000000, 0.000000000000000000 ) ) ;
#18624 = CARTESIAN_POINT ( 'NONE',  ( 12.39015342239245854, 3.070413439580832016, 12.22017215029075388 ) ) ;
#18625 = CARTESIAN_POINT ( 'NONE',  ( 9.702742433789000032, -5.491975933468000726, -7.893788029530999673 ) ) ;
#18626 = ADVANCED_FACE ( 'NONE', ( #28079 ), #38916, .T. ) ;
#18627 = CARTESIAN_POINT ( 'NONE',  ( 10.28441772631199846, 4.372518460886800185, -8.266796319406900295 ) ) ;
#18628 = CARTESIAN_POINT ( 'NONE',  ( 18.39984528086700166, -1.003641614260999896E-13, 7.549516567450998842E-14 ) ) ;
#18629 = CARTESIAN_POINT ( 'NONE',  ( 10.86190547754509872, 4.891676932241900033, -7.528299448264639260 ) ) ;
#18630 = CARTESIAN_POINT ( 'NONE',  ( 8.948759580228999866, 2.889471124893000287, -7.234556850645999404 ) ) ;
#18632 = CARTESIAN_POINT ( 'NONE',  ( 11.09500527153999982, -2.761300632964000190, 5.054570525499999967 ) ) ;
#18631 = CARTESIAN_POINT ( 'NONE',  ( 9.241151519676998660, -3.981249765141819719, 6.633192605878799775 ) ) ;
#18633 = CARTESIAN_POINT ( 'NONE',  ( 23.62209727552723848, -13.40165364989338137, 3.913322289613119231 ) ) ;
#18634 = VERTEX_POINT ( 'NONE', #49393 ) ;
#18635 = VECTOR ( 'NONE', #36546, 1000.000000000000000 ) ;
#18636 = DIRECTION ( 'NONE',  ( 1.000000000000000000, 0.000000000000000000, 0.000000000000000000 ) ) ;
#18637 = CARTESIAN_POINT ( 'NONE',  ( 9.753140057121997941, -4.104977100659999323, 9.293279163877999238 ) ) ;
#18638 = CARTESIAN_POINT ( 'NONE',  ( 10.00962143724499853, 4.667147537636399335, 8.250837174995698575 ) ) ;
#18639 = CARTESIAN_POINT ( 'NONE',  ( 9.910787105781626138, 4.756649759826824919, -7.060667085372605456 ) ) ;
#18640 = CARTESIAN_POINT ( 'NONE',  ( 10.50286331871000023, -5.158900740613000302, 8.369962360110999811 ) ) ;
#18641 = CIRCLE ( 'NONE', #27563, 13.92493900950999830 ) ;
#18642 = CARTESIAN_POINT ( 'NONE',  ( 12.30950027207670239, 2.881007065246251386, 13.58518188446331187 ) ) ;
#18643 = VERTEX_POINT ( 'NONE', #42772 ) ;
#18644 = CARTESIAN_POINT ( 'NONE',  ( 8.872772138681998655, -4.424886761933599644, -6.440186012775000357 ) ) ;
#18645 = CARTESIAN_POINT ( 'NONE',  ( 11.36673756060750939, -11.69736410939764859, -1.420371773397748560 ) ) ;
#18646 = CARTESIAN_POINT ( 'NONE',  ( 18.25703273071135158, 2.298329627318192792, -12.38863175403534989 ) ) ;
#18647 = CARTESIAN_POINT ( 'NONE',  ( 10.38462472191413255, 2.899999999999999911, 6.445686799157043012 ) ) ;
#18648 = CARTESIAN_POINT ( 'NONE',  ( 11.00000000000000000, -0.4000000000000000222, 7.331472342878999626 ) ) ;
#18649 = CARTESIAN_POINT ( 'NONE',  ( 11.43718179236249988, 3.790319673775199849, -6.518682001772900136 ) ) ;
#18651 = CIRCLE ( 'NONE', #27580, 0.6999999999999992895 ) ;
#18650 = CARTESIAN_POINT ( 'NONE',  ( 6.899999691988000450, 12.43893545635000031, -2.828937028792000152 ) ) ;
#18652 = CARTESIAN_POINT ( 'NONE',  ( 9.130720302798000176, -5.231133027468000130, -6.569831606205999819 ) ) ;
#18653 = CARTESIAN_POINT ( 'NONE',  ( 24.87547603600999935, 11.55042631839000045, 3.247370472710000122 ) ) ;
#18654 = ORIENTED_EDGE ( 'NONE', *, *, #57285, .F. ) ;
#18655 = CARTESIAN_POINT ( 'NONE',  ( 8.383148997457999130, 5.167567567567999731, 6.822293592207000934 ) ) ;
#18656 = CARTESIAN_POINT ( 'NONE',  ( 12.18894359730773580, -0.3856318793704111569, -13.99470184309725873 ) ) ;
#18657 = CARTESIAN_POINT ( 'NONE',  ( 17.60000000000000142, -10.78295181803999903, 4.410266442048000002 ) ) ;
#18658 = CARTESIAN_POINT ( 'NONE',  ( 11.44571737393083133, 2.988799872700407700, -8.273761053885758443 ) ) ;
#18659 = CARTESIAN_POINT ( 'NONE',  ( 10.44601354018326944, -4.999583552997726166, -8.268183399968640046 ) ) ;
#18660 = CARTESIAN_POINT ( 'NONE',  ( 9.410004719593999312, 2.495531372253999791, -7.930944806125000746 ) ) ;
#18661 = CARTESIAN_POINT ( 'NONE',  ( 16.39999999347100257, 3.345256695718999751, 11.86066175541999890 ) ) ;
#18662 = ORIENTED_EDGE ( 'NONE', *, *, #51000, .T. ) ;
#18663 = CARTESIAN_POINT ( 'NONE',  ( 23.50387503050299998, 0.000000000000000000, 0.000000000000000000 ) ) ;
#18664 = CARTESIAN_POINT ( 'NONE',  ( 18.17181771166723792, 2.603111764601558686, -13.65106951237197030 ) ) ;
#18665 = EDGE_LOOP ( 'NONE', ( #42139, #9377, #61519, #18610 ) ) ;
#18666 = DIRECTION ( 'NONE',  ( 0.000000000000000000, 0.000000000000000000, -1.000000000000000000 ) ) ;
#18667 = CARTESIAN_POINT ( 'NONE',  ( 25.12925359016687921, 2.819714440734963024, 11.46538652554768944 ) ) ;
#18668 = ADVANCED_FACE ( 'NONE', ( #1504 ), #10959, .T. ) ;
#18669 = CARTESIAN_POINT ( 'NONE',  ( 9.202245280414000916, 5.095038542659000136, -6.157541456184000062 ) ) ;
#18670 = CARTESIAN_POINT ( 'NONE',  ( 24.12730418717761793, -12.50340476629924780, 3.372662146504148417 ) ) ;
#18671 = CARTESIAN_POINT ( 'NONE',  ( 11.56322412107030928, -3.945399343424460525, -6.467939235001000320 ) ) ;
#18672 = CARTESIAN_POINT ( 'NONE',  ( 18.06407908477376623, 0.3627935496694635886, -12.69302875402908803 ) ) ;
#18673 = EDGE_CURVE ( 'NONE', #1379, #13517, #38559, .T. ) ;
#18674 = CARTESIAN_POINT ( 'NONE',  ( 11.00833333333534370, -3.620091288824273335, 8.928205453213877263 ) ) ;
#18675 = ORIENTED_EDGE ( 'NONE', *, *, #4808, .T. ) ;
#18676 = CARTESIAN_POINT ( 'NONE',  ( 10.00551210286899995, 3.782771630962269871, -8.756187319522087620 ) ) ;
#18677 = FACE_OUTER_BOUND ( 'NONE', #15166, .T. ) ;
#18678 = CARTESIAN_POINT ( 'NONE',  ( 9.494689158774999527, 2.824732249080000202, -8.992748220058999209 ) ) ;
#18679 = ORIENTED_EDGE ( 'NONE', *, *, #66995, .T. ) ;
#18680 = CARTESIAN_POINT ( 'NONE',  ( 10.80159548023000049, 2.805082485475999476, -8.157276499959001725 ) ) ;
#18681 = CARTESIAN_POINT ( 'NONE',  ( 25.60000000000000142, 10.55164198324999880, 3.754898126455999741 ) ) ;
#18682 = ORIENTED_EDGE ( 'NONE', *, *, #46980, .T. ) ;
#18683 = CARTESIAN_POINT ( 'NONE',  ( 9.835279731608999043, 4.102460098134500299, 8.637205511891998810 ) ) ;
#18684 = CARTESIAN_POINT ( 'NONE',  ( 18.22966818124863408, -2.744306698987320381, -12.29751612260396776 ) ) ;
#18685 = STYLED_ITEM ( 'NONE', ( #59513 ), #61967 ) ;
#18686 = CARTESIAN_POINT ( 'NONE',  ( 5.200000000000000178, 0.000000000000000000, 0.000000000000000000 ) ) ;
#18687 = CARTESIAN_POINT ( 'NONE',  ( 11.30000000000000071, 3.781170807299996550, -11.56421779094657332 ) ) ;
#18688 = B_SPLINE_CURVE_WITH_KNOTS ( 'NONE', 3,
 ( #59690, #48514, #21932, #11791, #43270, #64578, #59341, #16688, #38016, #54446, #32784, #49201, #54098, #43967, #6194, #1308 ),
 .UNSPECIFIED., .F., .F.,
 ( 4, 2, 2, 2, 2, 2, 2, 4 ),
 ( 0.000000000000000000, 0.06249999999999911182, 0.1249999999999982236, 0.2499999999999983347, 0.4999999999999987788, 0.7499999999999992228, 0.8749999999999996669, 1.000000000000000000 ),
 .UNSPECIFIED. ) ;
#18689 = CIRCLE ( 'NONE', #26520, 1.625000000000000000 ) ;
#18690 = CARTESIAN_POINT ( 'NONE',  ( 24.36958145701300182, -12.05823614978999991, -3.270605474396000023 ) ) ;
#18691 = CARTESIAN_POINT ( 'NONE',  ( 9.389934021418374854, -2.724469859320958420, 8.694040795412995237 ) ) ;
#18692 = ORIENTED_EDGE ( 'NONE', *, *, #59255, .F. ) ;
#18693 = LINE ( 'NONE', #57114, #12453 ) ;
#18694 = CARTESIAN_POINT ( 'NONE',  ( 10.01676721958999927, 4.324998751150999965, -9.154078823942999321 ) ) ;
#18695 = DIRECTION ( 'NONE',  ( -0.7071067811865475727, 0.7071067811865475727, 0.000000000000000000 ) ) ;
#18696 = AXIS2_PLACEMENT_3D ( 'NONE', #58953, #22232, #32394 ) ;
#18697 = CARTESIAN_POINT ( 'NONE',  ( 12.21493840618615501, 2.942228658260936935, -13.68734401625692954 ) ) ;
#18698 = CARTESIAN_POINT ( 'NONE',  ( 9.962988259787000089, -4.167373623506299474, -8.768215461831999846 ) ) ;
#18699 = CARTESIAN_POINT ( 'NONE',  ( 9.753140057121997941, -4.104977100659999323, 9.293279163877999238 ) ) ;
#18700 = CARTESIAN_POINT ( 'NONE',  ( 17.83170738868395588, 0.5608030988280853224, 13.88477341743901938 ) ) ;
#18701 = CARTESIAN_POINT ( 'NONE',  ( 7.867118290853380991, 5.122083207617727396, 6.719810845265266508 ) ) ;
#18702 = EDGE_LOOP ( 'NONE', ( #43090, #36317, #50984, #45060 ) ) ;
#18703 = EDGE_LOOP ( 'NONE', ( #47215, #52694, #1370, #3425, #56592 ) ) ;
#18704 = CARTESIAN_POINT ( 'NONE',  ( 8.541054719591000932, 3.807713920470999991, -9.221758713517999695 ) ) ;
#18705 = DIRECTION ( 'NONE',  ( 0.000000000000000000, 1.000000000000000000, 0.000000000000000000 ) ) ;
#18706 = EDGE_CURVE ( 'NONE', #44775, #57248, #23758, .T. ) ;
#18707 = EDGE_CURVE ( 'NONE', #31683, #64075, #60238, .T. ) ;
#18708 = CARTESIAN_POINT ( 'NONE',  ( 12.20205663652224892, -2.664445670458811755, 13.63720455645838214 ) ) ;
#18709 = CARTESIAN_POINT ( 'NONE',  ( 9.129428851719998406, -5.099284414202999827, 6.151604790022999758 ) ) ;
#18710 = CARTESIAN_POINT ( 'NONE',  ( 23.64815810203500135, 10.02631040633000126, -9.635204500925999227 ) ) ;
#18711 = CARTESIAN_POINT ( 'NONE',  ( 15.90003771078200145, -3.695138809391000034, -11.25918926437999978 ) ) ;
#18713 = CARTESIAN_POINT ( 'NONE',  ( 11.02035356290999957, -5.792383855159999761, 5.015468424570999950 ) ) ;
#18712 = CARTESIAN_POINT ( 'NONE',  ( 9.802417874594000935, -5.050800927762999493, 7.053287723251499663 ) ) ;
#18714 = CARTESIAN_POINT ( 'NONE',  ( 7.766851002543999627, -2.832432432432000269, 6.822293592207000934 ) ) ;
#18715 = VERTEX_POINT ( 'NONE', #5705 ) ;
#18716 = DIRECTION ( 'NONE',  ( -1.000000000000000000, 0.000000000000000000, 0.000000000000000000 ) ) ;
#18717 = CARTESIAN_POINT ( 'NONE',  ( 11.09999999999999964, -2.649999999999999911, 7.500000000000000000 ) ) ;
#18718 = CARTESIAN_POINT ( 'NONE',  ( 17.60655599801541271, 0.6229596466635312080, 12.67942438339646571 ) ) ;
#18719 = CARTESIAN_POINT ( 'NONE',  ( 12.23148815955828184, -0.2485241243391712040, 12.69673260777796209 ) ) ;
#18720 = CARTESIAN_POINT ( 'NONE',  ( 17.76019544541307127, -3.091716410407808535, -12.29381940409253104 ) ) ;
#18721 = ORIENTED_EDGE ( 'NONE', *, *, #14747, .T. ) ;
#18723 = CARTESIAN_POINT ( 'NONE',  ( 12.07911454974952115, -2.296549521770721913, -12.39040777274321670 ) ) ;
#18722 = CARTESIAN_POINT ( 'NONE',  ( 11.09999999999999964, 2.649999999999999911, 7.500000000000000000 ) ) ;
#18724 = CARTESIAN_POINT ( 'NONE',  ( 8.406645280410000254, 3.807713920470999991, -9.221758713517999695 ) ) ;
#18725 = FACE_OUTER_BOUND ( 'NONE', #48647, .T. ) ;
#18726 = ADVANCED_FACE ( 'NONE', ( #27046 ), #464, .T. ) ;
#18727 = CARTESIAN_POINT ( 'NONE',  ( 10.56733863405299800, 4.788475529394700558, 6.494205428462000107 ) ) ;
#18728 = VECTOR ( 'NONE', #6411, 1000.000000000000000 ) ;
#18729 = B_SPLINE_CURVE_WITH_KNOTS ( 'NONE', 3,
 ( #20747, #30218, #24959, #35798 ),
 .UNSPECIFIED., .F., .F.,
 ( 4, 4 ),
 ( 0.000000000000000000, 1.000000000000000000 ),
 .UNSPECIFIED. ) ;
#18730 = SURFACE_STYLE_FILL_AREA ( #50540 ) ;
#18731 = STYLED_ITEM ( 'NONE', ( #16771 ), #24370 ) ;
#18732 = CARTESIAN_POINT ( 'NONE',  ( 18.19991756629429602, -3.160410836633248621, -11.91446384612378750 ) ) ;
#18733 = CARTESIAN_POINT ( 'NONE',  ( 3.219931333175999999, -2.814609116688000068, 2.491254988490000155 ) ) ;
#18734 = VERTEX_POINT ( 'NONE', #6047 ) ;
#18735 = B_SPLINE_CURVE_WITH_KNOTS ( 'NONE', 3,
 ( #38712, #60031, #27530, #33124, #16683, #11437, #5849, #58651, #268, #49537 ),
 .UNSPECIFIED., .F., .F.,
 ( 4, 2, 2, 2, 4 ),
 ( 0.3720125677995148594, 0.5290094258496361723, 0.6860062838997573742, 0.8430031419498786871, 1.000000000000000000 ),
 .UNSPECIFIED. ) ;
#18736 = CARTESIAN_POINT ( 'NONE',  ( 12.27985646406008335, -0.3389720875425251689, -12.69391532355469110 ) ) ;
#18737 = CARTESIAN_POINT ( 'NONE',  ( 11.09999999999999964, -7.940796613052000019, -6.945951997396999644 ) ) ;
#18738 = CARTESIAN_POINT ( 'NONE',  ( 24.00507456979297061, -12.70418999682170913, -3.471506332325644095 ) ) ;
#18740 = CARTESIAN_POINT ( 'NONE',  ( 24.70770306079000278, 3.610860736573000107, -12.15153796058999980 ) ) ;
#18739 = AXIS2_PLACEMENT_3D ( 'NONE', #40638, #40305, #3913 ) ;
#18741 = DIRECTION ( 'NONE',  ( 0.000000000000000000, 1.000000000000000000, 0.000000000000000000 ) ) ;
#18742 = ORIENTED_EDGE ( 'NONE', *, *, #22639, .F. ) ;
#18743 = CARTESIAN_POINT ( 'NONE',  ( 6.126648365476000002, 1.250196283310000211, -0.4306799594067000081 ) ) ;
#18744 = CARTESIAN_POINT ( 'NONE',  ( 8.683985841228999192, 4.472863460285000592, -8.721137209586000694 ) ) ;
#18746 = CARTESIAN_POINT ( 'NONE',  ( 9.069066892820998760, -5.132803099462346808, -6.762400598726751255 ) ) ;
#18745 = CARTESIAN_POINT ( 'NONE',  ( 9.625409048293999348, -2.899999999999999911, -6.226580113766999602 ) ) ;
#18747 = PLANE ( 'NONE',  #17200 ) ;
#18748 = CARTESIAN_POINT ( 'NONE',  ( 11.76077869730539938, 3.404661623424200201, -6.326049646822999861 ) ) ;
#18749 = VERTEX_POINT ( 'NONE', #48712 ) ;
#18750 = CARTESIAN_POINT ( 'NONE',  ( 10.03612181215999932, -3.011786236723999810, 8.746965724352000038 ) ) ;
#18751 = ORIENTED_EDGE ( 'NONE', *, *, #55200, .T. ) ;
#18752 = CARTESIAN_POINT ( 'NONE',  ( 23.66004879239100234, -13.39256420742000131, 3.813548264891000183 ) ) ;
#18753 = CARTESIAN_POINT ( 'NONE',  ( 9.202754440379999679, -2.542850487891999745, 7.419808283050000064 ) ) ;
#18754 = CARTESIAN_POINT ( 'NONE',  ( 18.10028295948237798, -0.4818816852691614194, -13.99171642476389898 ) ) ;
#18755 = ORIENTED_EDGE ( 'NONE', *, *, #55712, .F. ) ;
#18756 = CARTESIAN_POINT ( 'NONE',  ( 25.29989727901499919, -2.078227429405999693, -11.31065739696999906 ) ) ;
#18757 = DIRECTION ( 'NONE',  ( -1.000000000000000000, 0.000000000000000000, 0.000000000000000000 ) ) ;
#18758 = VECTOR ( 'NONE', #13251, 1000.000000000000114 ) ;
#18759 = CARTESIAN_POINT ( 'NONE',  ( 7.888864158768998713, 2.841678116489999795, -6.718113446527000931 ) ) ;
#18760 = ADVANCED_FACE ( 'NONE', ( #815 ), #12364, .F. ) ;
#18761 = CARTESIAN_POINT ( 'NONE',  ( 10.21685100254000034, 2.832432432432000269, 6.822293592207000934 ) ) ;
#18762 = DIRECTION ( 'NONE',  ( 2.186536431443105034E-10, -0.8764392776392420092, -0.4815124013057229813 ) ) ;
#18763 = ORIENTED_EDGE ( 'NONE', *, *, #5200, .T. ) ;
#18764 = CARTESIAN_POINT ( 'NONE',  ( 10.52638330645999964, -2.451090818816000105, 6.282756943804999494 ) ) ;
#18765 = CARTESIAN_POINT ( 'NONE',  ( 12.43967993051479759, -3.007449918965191760, -13.55258931251709242 ) ) ;
#18766 = CARTESIAN_POINT ( 'NONE',  ( 11.09999999999999964, -6.593648099371000271, -5.598803483715999896 ) ) ;
#18767 = CARTESIAN_POINT ( 'NONE',  ( 23.66004879239100234, 0.000000000000000000, 0.000000000000000000 ) ) ;
#18768 = CARTESIAN_POINT ( 'NONE',  ( 12.08083412505908427, -2.710618184188187119, 13.73644169169829965 ) ) ;
#18769 = ORIENTED_EDGE ( 'NONE', *, *, #25731, .T. ) ;
#18770 = PRODUCT ( 'Drip Tip - Airflow Cap', 'Drip Tip - Airflow Cap', '', ( #22161 ) ) ;
#18771 = DIRECTION ( 'NONE',  ( 1.000000000000000000, 0.000000000000000000, 0.000000000000000000 ) ) ;
#18772 = DIRECTION ( 'NONE',  ( -1.000000000000000000, 0.000000000000000000, 0.000000000000000000 ) ) ;
#18773 = CARTESIAN_POINT ( 'NONE',  ( 3.500000000000000444, 3.440400109149063024, 0.5815178920906223237 ) ) ;
#18774 = CARTESIAN_POINT ( 'NONE',  ( 24.30000000000000071, 2.078227429405999693, 11.31065739696999906 ) ) ;
#18775 = CARTESIAN_POINT ( 'NONE',  ( 9.051550650638001017, -2.899999999999999911, 6.227445478845999638 ) ) ;
#18776 = CARTESIAN_POINT ( 'NONE',  ( 12.18028570900101215, -0.01996689158402697659, -13.89998575767903155 ) ) ;
#18777 = CARTESIAN_POINT ( 'NONE',  ( 18.13637388831912745, -2.729759562904666037, 12.39509076542458921 ) ) ;
#18778 = ORIENTED_EDGE ( 'NONE', *, *, #29818, .F. ) ;
#18779 = CARTESIAN_POINT ( 'NONE',  ( 10.81524174883999834, -4.028418853626810403, -8.533115712456000423 ) ) ;
#18780 = ORIENTED_EDGE ( 'NONE', *, *, #67769, .F. ) ;
#18781 = CARTESIAN_POINT ( 'NONE',  ( 0.1499942179680000265, -0.7197945678028389027, 2.678379783547566895 ) ) ;
#18782 = CARTESIAN_POINT ( 'NONE',  ( 8.780820280412001466, 2.567871051582000241, -6.869011921437000012 ) ) ;
#18783 = CARTESIAN_POINT ( 'NONE',  ( 3.041322614968000160, -2.841635719351000233, -1.503882494686000104 ) ) ;
#18784 = CARTESIAN_POINT ( 'NONE',  ( 11.07336076184000007, -2.375557098086999996, -8.393541296344000813 ) ) ;
#18785 = CONICAL_SURFACE ( 'NONE', #53359, 2.074968475931999734, 0.7853828752794411727 ) ;
#18786 = CARTESIAN_POINT ( 'NONE',  ( 10.36503728015293646, 2.650011783304074164, -7.500002219258057323 ) ) ;
#18787 = CARTESIAN_POINT ( 'NONE',  ( 9.020066447149183375, -5.146940009916286307, 8.214567059322398279 ) ) ;
#18788 = ORIENTED_EDGE ( 'NONE', *, *, #62444, .F. ) ;
#18789 = VECTOR ( 'NONE', #61783, 1000.000000000000114 ) ;
#18790 = EDGE_CURVE ( 'NONE', #9042, #35521, #21273, .T. ) ;
#18791 = CARTESIAN_POINT ( 'NONE',  ( 11.80995122972050027, -3.547233695387300045, 8.547040013405998948 ) ) ;
#18792 = CARTESIAN_POINT ( 'NONE',  ( 9.199602729599000384, 2.551394566582000145, 7.536605852160000119 ) ) ;
#18793 = EDGE_CURVE ( 'NONE', #16649, #63146, #65949, .T. ) ;
#18794 = CARTESIAN_POINT ( 'NONE',  ( 9.856851002545999663, -2.832432432432000269, -6.822293592207000934 ) ) ;
#18795 = CARTESIAN_POINT ( 'NONE',  ( 7.501441940376999185, -2.138201851198999748, 6.814774777484000623 ) ) ;
#18797 = CARTESIAN_POINT ( 'NONE',  ( 10.91666666666762886, 5.385217356303825476, 7.523132604489796371 ) ) ;
#18796 = CARTESIAN_POINT ( 'NONE',  ( 9.290193290418001126, 2.377818438998999806, 7.540992072119000689 ) ) ;
#18798 = VECTOR ( 'NONE', #26472, 1000.000000000000000 ) ;
#18799 = CARTESIAN_POINT ( 'NONE',  ( 10.69872335273220010, 4.349306362047499874, -8.440710326446700051 ) ) ;
#18800 = DIRECTION ( 'NONE',  ( 1.000000000000000000, 9.560366183076000235E-10, 1.449015955545000044E-09 ) ) ;
#18801 = CARTESIAN_POINT ( 'NONE',  ( 9.173759580228997734, 3.023107159668900312, -7.266499081715599218 ) ) ;
#18802 = CARTESIAN_POINT ( 'NONE',  ( 17.67321935251239751, -0.7100593550699877410, 12.57997761080729759 ) ) ;
#18803 = CARTESIAN_POINT ( 'NONE',  ( 24.36504260745899941, 3.372670036896999513, 12.24415025393999912 ) ) ;
#18804 = AXIS2_PLACEMENT_3D ( 'NONE', #63167, #47810, #16318 ) ;
#18805 = CARTESIAN_POINT ( 'NONE',  ( 0.7690682080319749536, -3.431488182670113574, -0.7957590664505270750 ) ) ;
#18806 = CARTESIAN_POINT ( 'NONE',  ( 11.10664834123000055, 5.324188120986000250, -7.809342242343999985 ) ) ;
#18807 = ORIENTED_EDGE ( 'NONE', *, *, #53310, .T. ) ;
#18808 = CARTESIAN_POINT ( 'NONE',  ( 7.410855646792000151, -2.302293129340000188, 6.875167727519000849 ) ) ;
#18809 = CARTESIAN_POINT ( 'NONE',  ( 18.06232794982559753, 1.996188719851612170, 13.85695876210811406 ) ) ;
#18810 = EDGE_CURVE ( 'NONE', #21934, #16920, #24626, .T. ) ;
#18811 = CARTESIAN_POINT ( 'NONE',  ( 15.90018573812067615, -4.599694346030117842, -10.96245233228866667 ) ) ;
#18812 = CARTESIAN_POINT ( 'NONE',  ( 10.38314899745999931, 5.167567567567999731, 6.822293592207000934 ) ) ;
#18813 = ORIENTED_EDGE ( 'NONE', *, *, #19990, .T. ) ;
#18814 = ADVANCED_FACE ( 'NONE', ( #31439 ), #62214, .F. ) ;
#18815 = CARTESIAN_POINT ( 'NONE',  ( 8.128301658772999261, 3.117378429069999957, 8.662179062556001341 ) ) ;
#18817 = CARTESIAN_POINT ( 'NONE',  ( 5.500000000000000000, 0.000000000000000000, 0.000000000000000000 ) ) ;
#18816 = CARTESIAN_POINT ( 'NONE',  ( 9.491735841231999871, 3.920043641733999884, -9.398198753036000497 ) ) ;
#18818 = CARTESIAN_POINT ( 'NONE',  ( 16.13140881196041221, 3.487052973477671181, 11.11602635788046278 ) ) ;
#18819 = VERTEX_POINT ( 'NONE', #4502 ) ;
#18820 = CARTESIAN_POINT ( 'NONE',  ( 11.61486084871780022, -2.792989229543000107, 7.825000000000000178 ) ) ;
#18821 = CARTESIAN_POINT ( 'NONE',  ( 9.247349085094461074, -4.940696344428553211, -6.064447655904166901 ) ) ;
#18822 = CARTESIAN_POINT ( 'NONE',  ( 11.11302897915239818, 4.291996373817799970, 6.397263297997000109 ) ) ;
#18823 = CARTESIAN_POINT ( 'NONE',  ( 11.14993998249000029, -2.627133311863999676, 6.696092388640000337 ) ) ;
#18824 = CARTESIAN_POINT ( 'NONE',  ( 9.725191424783275806, 2.649754699899339538, 7.500009801425228773 ) ) ;
#18825 = ORIENTED_EDGE ( 'NONE', *, *, #49899, .F. ) ;
#18826 = CARTESIAN_POINT ( 'NONE',  ( 11.80415302574500203, -3.641975138519000232, 12.02422332381999937 ) ) ;
#18827 = CARTESIAN_POINT ( 'NONE',  ( 10.10735564678999943, -4.293585439421999439, -8.994200998147999115 ) ) ;
#18828 = CARTESIAN_POINT ( 'NONE',  ( 8.005929440722622914, -2.667435911584553843, 6.373521026562600333 ) ) ;
#18829 = CARTESIAN_POINT ( 'NONE',  ( 10.55991645936999923, -5.094263939633999705, 6.075409946530999861 ) ) ;
#18830 = CARTESIAN_POINT ( 'NONE',  ( 11.52166954483529793, -3.437903757373499847, -6.632714178206799538 ) ) ;
#18831 = CARTESIAN_POINT ( 'NONE',  ( 10.56324205624999912, -4.409476560233800413, 6.434137271007999814 ) ) ;
#18832 = ORIENTED_EDGE ( 'NONE', *, *, #63215, .T. ) ;
#18833 = CARTESIAN_POINT ( 'NONE',  ( 10.98942773129999928, -5.061072618684999469, -5.190416327777001015 ) ) ;
#18834 = CARTESIAN_POINT ( 'NONE',  ( 11.60887482311539998, -2.815046254222000055, 7.021250586468399391 ) ) ;
#18835 = ORIENTED_EDGE ( 'NONE', *, *, #15665, .F. ) ;
#18836 = CARTESIAN_POINT ( 'NONE',  ( 9.096071945540000314, -5.102479135096000817, -6.621020973615999061 ) ) ;
#18837 = VERTEX_POINT ( 'NONE', #4162 ) ;
#18838 = CARTESIAN_POINT ( 'NONE',  ( 10.10633213213999859, -4.301175052434000001, -8.935144319903001175 ) ) ;
#18839 = CARTESIAN_POINT ( 'NONE',  ( 8.994485841233000656, 3.854507394315999758, -9.394302886912999639 ) ) ;
#18840 = CIRCLE ( 'NONE', #27768, 2.700000000000000178 ) ;
#18841 = CARTESIAN_POINT ( 'NONE',  ( 8.202894943314742449, -2.713916317890127328, 7.026332083725546518 ) ) ;
#18842 = FACE_OUTER_BOUND ( 'NONE', #59639, .T. ) ;
#18843 = CARTESIAN_POINT ( 'NONE',  ( 12.21868246241196587, 2.283434118842407656, -12.49941978418538824 ) ) ;
#18844 = CARTESIAN_POINT ( 'NONE',  ( 11.17410807141120088, -3.953638752893899877, 6.497602131078999754 ) ) ;
#18845 = CARTESIAN_POINT ( 'NONE',  ( 11.02946886766499901, -4.430164648092599577, 8.281567006984099422 ) ) ;
#18846 = VERTEX_POINT ( 'NONE', #19570 ) ;
#18847 = CARTESIAN_POINT ( 'NONE',  ( 7.524264477127990070, 5.120202152877183721, 8.282468543079009038 ) ) ;
#18848 = CARTESIAN_POINT ( 'NONE',  ( 8.893206853209999707, -3.977267280662000193, 9.308921106447000327 ) ) ;
#18849 = DIRECTION ( 'NONE',  ( -1.000000000000000000, 0.000000000000000000, 0.000000000000000000 ) ) ;
#18850 = ORIENTED_EDGE ( 'NONE', *, *, #53095, .T. ) ;
#18851 = CARTESIAN_POINT ( 'NONE',  ( 12.09756245983761147, -2.320968861236850422, -12.38441143973091840 ) ) ;
#18852 = CARTESIAN_POINT ( 'NONE',  ( 11.13764426047339917, 4.613828180779599997, 6.538488127609999978 ) ) ;
#18853 = CARTESIAN_POINT ( 'NONE',  ( 10.58470685321000104, -2.966812129551000154, -8.831977776575000050 ) ) ;
#18854 = CARTESIAN_POINT ( 'NONE',  ( 6.346693173016666911, 1.310679582531385501, 0.7554284705563518720 ) ) ;
#18855 = CARTESIAN_POINT ( 'NONE',  ( 18.53494720760600245, -3.035003031749999636, -12.19105792290999979 ) ) ;
#18856 = CARTESIAN_POINT ( 'NONE',  ( 9.769471092180999960, 5.100000000000000533, -6.152188490330000370 ) ) ;
#18857 = CARTESIAN_POINT ( 'NONE',  ( 12.58300520725476623, -3.084588251740257192, -13.53188417542246214 ) ) ;
#18858 = CARTESIAN_POINT ( 'NONE',  ( 17.80401300531091024, -0.5733651658914323823, -12.68257300503909768 ) ) ;
#18859 = CARTESIAN_POINT ( 'NONE',  ( 11.39210538575740017, -3.157545584346100220, -7.298582155985900322 ) ) ;
#18860 = CARTESIAN_POINT ( 'NONE',  ( 10.96118313518939935, -4.792748567750200195, -8.502430091786999711 ) ) ;
#18861 = CARTESIAN_POINT ( 'NONE',  ( 17.75579847504525333, -3.171737058802227338, 12.19426492080491542 ) ) ;
#18862 = VERTEX_POINT ( 'NONE', #52058 ) ;
#18863 = EDGE_LOOP ( 'NONE', ( #38348, #46026, #50641, #68291 ) ) ;
#18864 = CIRCLE ( 'NONE', #52333, 0.3000000000000000444 ) ;
#18865 = CARTESIAN_POINT ( 'NONE',  ( 12.48078237978696414, -11.21561491931810473, 3.152940285099523621 ) ) ;
#18866 = CARTESIAN_POINT ( 'NONE',  ( 8.090129597172534659, 4.176673380087977172, 8.851094058677711374 ) ) ;
#18867 = CARTESIAN_POINT ( 'NONE',  ( 10.90634530628000043, 3.089682683751000081, -6.534327427410000055 ) ) ;
#18868 = DIRECTION ( 'NONE',  ( 0.000000000000000000, 0.000000000000000000, 1.000000000000000000 ) ) ;
#18869 = CARTESIAN_POINT ( 'NONE',  ( 17.87014202174171373, 1.960141137139741252, 12.56108054050352507 ) ) ;
#18870 = DIRECTION ( 'NONE',  ( -1.000000000000000000, 0.000000000000000000, 0.000000000000000000 ) ) ;
#18871 = CARTESIAN_POINT ( 'NONE',  ( 9.256664404737000140, 4.025830366070999311, 9.295863330698999505 ) ) ;
#18872 = CARTESIAN_POINT ( 'NONE',  ( 11.37077408945316925, -5.183263708087437749, -7.913130250469239790 ) ) ;
#18873 = ADVANCED_FACE ( 'NONE', ( #63230 ), #25500, .T. ) ;
#18874 = ORIENTED_EDGE ( 'NONE', *, *, #46345, .F. ) ;
#18875 = CARTESIAN_POINT ( 'NONE',  ( 12.34586232581682808, -2.075512354070471854, 12.54043254740684077 ) ) ;
#18876 = ADVANCED_FACE ( 'NONE', ( #15008 ), #1759, .F. ) ;
#18877 = CARTESIAN_POINT ( 'NONE',  ( 9.376392757686998536, -3.322036695224600322, -8.241085728986799808 ) ) ;
#18878 = CARTESIAN_POINT ( 'NONE',  ( 9.869051220224999810, 5.575171928796999410, 7.724300137354000562 ) ) ;
#18879 = CARTESIAN_POINT ( 'NONE',  ( 9.242292592096250203, 3.634505416671740097, 8.705986097797767442 ) ) ;
#18880 = CARTESIAN_POINT ( 'NONE',  ( 10.12841772631199966, 4.490588993294299947, -8.509834072393999804 ) ) ;
#18881 = CARTESIAN_POINT ( 'NONE',  ( 12.55627843433555846, 0.5734477787136632587, 12.68256797703445038 ) ) ;
#18882 = CARTESIAN_POINT ( 'NONE',  ( 9.406704719590001318, 3.705846972803000128, 9.096435887808000942 ) ) ;
#18883 = B_SPLINE_CURVE_WITH_KNOTS ( 'NONE', 3,
 ( #21871, #69084, #16970, #47775 ),
 .UNSPECIFIED., .F., .F.,
 ( 4, 4 ),
 ( 0.000000000000000000, 1.000000000000000000 ),
 .UNSPECIFIED. ) ;
#18884 = B_SPLINE_CURVE_WITH_KNOTS ( 'NONE', 3,
 ( #47672, #35803, #26694, #53249 ),
 .UNSPECIFIED., .F., .F.,
 ( 4, 4 ),
 ( 0.000000000000000000, 1.000000000000000000 ),
 .UNSPECIFIED. ) ;
#18885 = CARTESIAN_POINT ( 'NONE',  ( 9.323722176100000425, 3.947350570199999797, 6.051869652381999920 ) ) ;
#18886 = AXIS2_PLACEMENT_3D ( 'NONE', #46306, #19732, #41055 ) ;
#18887 = CARTESIAN_POINT ( 'NONE',  ( 12.58248715490565672, 1.915879699765342226, 12.56863216566090991 ) ) ;
#18888 = EDGE_LOOP ( 'NONE', ( #24674, #49614, #21068, #55755 ) ) ;
#18889 = CARTESIAN_POINT ( 'NONE',  ( 10.03280471959000231, 3.987760651117999711, -9.123263301387000368 ) ) ;
#18890 = CARTESIAN_POINT ( 'NONE',  ( 10.64118447801629941, 5.277702140407999565, -7.471828720557429193 ) ) ;
#18891 = CARTESIAN_POINT ( 'NONE',  ( 10.83610788131087688, -3.761915004978170440, 9.251916359107640986 ) ) ;
#18893 = CARTESIAN_POINT ( 'NONE',  ( 10.30226354018233437, 2.907767014557178786, 8.129523725463625894 ) ) ;
#18892 = CARTESIAN_POINT ( 'NONE',  ( 9.523691940378000709, -4.852736108563000528, 8.683927195503999386 ) ) ;
#18894 = CARTESIAN_POINT ( 'NONE',  ( 9.452784697134999803, -3.529509552262100058, 8.228249052908999772 ) ) ;
#18895 = CARTESIAN_POINT ( 'NONE',  ( 11.16641369783139837, -4.050626550392200542, -8.502191501283999031 ) ) ;
#18896 = ORIENTED_EDGE ( 'NONE', *, *, #30948, .F. ) ;
#18897 = CARTESIAN_POINT ( 'NONE',  ( 1.777519953414000042, -1.374622313384999961, -3.318774223758000019 ) ) ;
#18898 = EDGE_CURVE ( 'NONE', #41892, #48331, #64263, .T. ) ;
#18899 = CARTESIAN_POINT ( 'NONE',  ( 11.53192018828833731, 3.091029700564639437, 7.824998071251875409 ) ) ;
#18900 = CARTESIAN_POINT ( 'NONE',  ( 9.324071121570657539, -3.025928824985222754, 7.751553442067931066 ) ) ;
#18901 = DIRECTION ( 'NONE',  ( -1.000000000000000000, 0.000000000000000000, 0.000000000000000000 ) ) ;
#18902 = CARTESIAN_POINT ( 'NONE',  ( 7.726719758561022999, 3.010539354342125051, 6.557630410916043928 ) ) ;
#18903 = CARTESIAN_POINT ( 'NONE',  ( 12.54773036592023949, -3.200672309338196797, 13.62922281487128906 ) ) ;
#18904 = CARTESIAN_POINT ( 'NONE',  ( 8.474280730212667478, 2.899999999999999911, -6.567100790826333245 ) ) ;
#18905 = CARTESIAN_POINT ( 'NONE',  ( 13.00000000009400303, 11.69118001589999878, 1.923222888683999932 ) ) ;
#18906 = CARTESIAN_POINT ( 'NONE',  ( 10.90000000000000036, -5.283926297003000094, 7.082827057608000132 ) ) ;
#18907 = EDGE_LOOP ( 'NONE', ( #41848, #11715, #17448, #51647 ) ) ;
#18908 = CARTESIAN_POINT ( 'NONE',  ( 8.277732780410000046, 4.874567052833000069, 6.119507471270999588 ) ) ;
#18909 = DIRECTION ( 'NONE',  ( 0.000000000000000000, 0.000000000000000000, -1.000000000000000000 ) ) ;
#18910 = LINE ( 'NONE', #56311, #50885 ) ;
#18911 = CARTESIAN_POINT ( 'NONE',  ( 11.59999999999999964, 3.116215992411100366, -7.825000000000000178 ) ) ;
#18912 = CARTESIAN_POINT ( 'NONE',  ( 1.604975240918999901, 3.542864650996000453, -0.5932612529451999350 ) ) ;
#18913 = ORIENTED_EDGE ( 'NONE', *, *, #63540, .T. ) ;
#18914 = CARTESIAN_POINT ( 'NONE',  ( 10.85460595134761874, 2.649926015913104393, -7.676664732030197058 ) ) ;
#18915 = DIRECTION ( 'NONE',  ( -1.000000000000000000, 0.000000000000000000, 0.000000000000000000 ) ) ;
#18916 = CARTESIAN_POINT ( 'NONE',  ( 10.44675156161000018, 2.885046387990999772, 8.863482298832000339 ) ) ;
#18917 = CARTESIAN_POINT ( 'NONE',  ( 11.63410404293056999, 3.557672215630899970, 6.599279737936000423 ) ) ;
#18918 = CARTESIAN_POINT ( 'NONE',  ( 11.01053724730969918, 3.051574408741400291, -7.174999999999999822 ) ) ;
#18919 = CARTESIAN_POINT ( 'NONE',  ( 11.09999999999999964, -11.35000000000000142, 0.000000000000000000 ) ) ;
#18920 = CARTESIAN_POINT ( 'NONE',  ( 11.49999144015000319, 3.886253129992999877, -11.90689313971000018 ) ) ;
#18921 = FACE_OUTER_BOUND ( 'NONE', #1702, .T. ) ;
#18922 = CARTESIAN_POINT ( 'NONE',  ( 12.26368341514495519, -2.812488373138167130, 12.37327521545045883 ) ) ;
#18923 = CARTESIAN_POINT ( 'NONE',  ( 8.383086419343017681, 2.825288952757737171, 8.816744424860624818 ) ) ;
#18924 = ORIENTED_EDGE ( 'NONE', *, *, #11507, .F. ) ;
#18925 = CARTESIAN_POINT ( 'NONE',  ( 18.08598429698836085, -3.015255620044101192, 13.67144160714441981 ) ) ;
#18926 = CARTESIAN_POINT ( 'NONE',  ( 17.55505043854143565, 3.125000000000000000, -13.52084414783465682 ) ) ;
#18927 = ORIENTED_EDGE ( 'NONE', *, *, #8958, .F. ) ;
#18928 = ORIENTED_EDGE ( 'NONE', *, *, #57646, .T. ) ;
#18929 = CARTESIAN_POINT ( 'NONE',  ( 15.40000000005200143, -9.187454762873001002, -8.213177997099000649 ) ) ;
#18930 = CARTESIAN_POINT ( 'NONE',  ( 9.614763540183330903, 5.217465845835394411, -7.172815144550904520 ) ) ;
#18931 = CARTESIAN_POINT ( 'NONE',  ( 24.30000000000000071, 0.000000000000000000, 0.000000000000000000 ) ) ;
#18932 = ADVANCED_FACE ( 'NONE', ( #58685 ), #49766, .F. ) ;
#18933 = CARTESIAN_POINT ( 'NONE',  ( 5.500000000000000000, -0.2500000000000000000, -9.776630298829998011 ) ) ;
#18934 = ADVANCED_FACE ( 'NONE', ( #25672 ), #46665, .F. ) ;
#18935 = CARTESIAN_POINT ( 'NONE',  ( 10.21237770872999917, 4.072568038926999812, -8.861829932786999819 ) ) ;
#18936 = CARTESIAN_POINT ( 'NONE',  ( 16.13886389318898651, -3.397126321181334063, -11.84561170022415766 ) ) ;
#18937 = CARTESIAN_POINT ( 'NONE',  ( 10.34947173981000113, -4.457565973839000328, 6.154866550070000386 ) ) ;
#18938 = CARTESIAN_POINT ( 'NONE',  ( 17.99623368854100747, 0.5708113556792957510, -12.58706429964239071 ) ) ;
#18939 = DIRECTION ( 'NONE',  ( 0.000000000000000000, 0.7198977633594745296, 0.6940801180771756229 ) ) ;
#18940 = CARTESIAN_POINT ( 'NONE',  ( 10.94903032197929882, -3.496160833528699996, -6.795411691360399686 ) ) ;
#18941 = CARTESIAN_POINT ( 'NONE',  ( 5.486746727192667983, -1.006919573152101233, 1.157429495210549941 ) ) ;
#18942 = ORIENTED_EDGE ( 'NONE', *, *, #22912, .F. ) ;
#18943 = CARTESIAN_POINT ( 'NONE',  ( 11.07206039417999932, -5.781505909594000236, -5.100555594908000145 ) ) ;
#18944 = CARTESIAN_POINT ( 'NONE',  ( 24.56710774269708608, 8.731559079190242656, 8.723167087384579688 ) ) ;
#18945 = CARTESIAN_POINT ( 'NONE',  ( 10.70039988502568029, -3.823246508712720537, -8.849946088921091913 ) ) ;
#18946 = CARTESIAN_POINT ( 'NONE',  ( 9.355088727410999283, 2.725263018055000153, -7.606911245136100064 ) ) ;
#18947 = CARTESIAN_POINT ( 'NONE',  ( 12.49029065891180146, 1.959656569402035142, 13.77327738386123102 ) ) ;
#18948 = CARTESIAN_POINT ( 'NONE',  ( 10.09181272066999924, -2.440908155048000516, 7.817368209339999652 ) ) ;
#18949 = ORIENTED_EDGE ( 'NONE', *, *, #38514, .T. ) ;
#18950 = CARTESIAN_POINT ( 'NONE',  ( 12.18827089113675832, -0.1029087316210665626, -12.69945830692974553 ) ) ;
#18951 = CARTESIAN_POINT ( 'NONE',  ( 12.78440349184324454, -0.6249994334955771835, 13.88107975403459626 ) ) ;
#18952 = ORIENTED_EDGE ( 'NONE', *, *, #31188, .F. ) ;
#18953 = CARTESIAN_POINT ( 'NONE',  ( 1.700000000000000178, 0.000000000000000000, 0.000000000000000000 ) ) ;
#18954 = ADVANCED_FACE ( 'NONE', ( #53276 ), #22964, .F. ) ;
#18955 = LINE ( 'NONE', #62619, #43807 ) ;
#18956 = AXIS2_PLACEMENT_3D ( 'NONE', #66807, #35007, #24507 ) ;
#18957 = CARTESIAN_POINT ( 'NONE',  ( 23.55356154618500142, -3.058499659814000182, -13.69546366221000078 ) ) ;
#18958 = DIRECTION ( 'NONE',  ( -0.000000000000000000, -0.000000000000000000, 1.000000000000000000 ) ) ;
#18959 = EDGE_CURVE ( 'NONE', #49620, #52300, #12115, .T. ) ;
#18960 = B_SPLINE_SURFACE_WITH_KNOTS ( 'NONE', 3, 3, ( 
 ( #15435, #52487, #4583, #20676, #42007, #36761, #32890, #17851, #1415, #1765, #27300, #12601, #7005, #17501, #16794, #48624, #54200, #727, #2116, #38824, #12256, #38474, #28337, #60492, #60151, #49656, #38122, #22038, #23083, #65380, #33585, #44430, #43727, #65728, #59449 ),
 ( #39169, #11899, #22390, #49305, #33932, #22732, #7347, #28692, #55251, #18193, #50005, #23433, #44772, #66072, #27648, #54902, #39515, #11212, #32548, #33237, #59796, #5962, #11547, #53861, #27996, #17142, #6301, #43385, #64686, #48967, #1075, #65025, #54557, #6654, #44081 ),
 ( #51037, #24120, #55941, #61186, #34279, #62207, #61864, #13306, #8043, #45455, #35310, #29387, #55599, #67105, #29734, #7700, #40210, #14329, #13641, #50697, #3139, #3475, #34628, #35652, #13984, #29041, #19213, #30075, #19564, #56966, #2794, #40539, #66767, #50351, #18882 ),
 ( #2451, #56285, #60840, #23776, #34968, #8390, #56627, #9067, #30405, #8731, #25149, #51376, #61526, #67442, #46480, #51717, #24467, #3810, #24811, #46136, #45792, #45111, #40887, #18540, #67787, #19909, #12952, #66418, #39866, #32126, #48194, #21277, #31434, #52404, #62882 ) ),
 .UNSPECIFIED., .F., .F., .F.,
 ( 4, 4 ),
 ( 4, 1, 1, 1, 1, 1, 1, 1, 1, 1, 1, 1, 1, 1, 1, 1, 1, 1, 1, 1, 1, 1, 1, 1, 1, 1, 1, 1, 1, 1, 1, 1, 4 ),
 ( -0.1039370721279000015, 1.103937072127999963 ),
 ( -0.02000000000000000042, 0.01250000000000000069, 0.04499999999999999833, 0.07749999999999999944, 0.1100000000000000006, 0.1424999999999999878, 0.1749999999999999889, 0.2074999999999999900, 0.2399999999999999911, 0.2725000000000000200, 0.3049999999999999933, 0.3375000000000000222, 0.3699999999999999956, 0.4025000000000000244, 0.4349999999999999978, 0.4675000000000000266, 0.5000000000000000000, 0.5324999999999999734, 0.5649999999999999467, 0.5975000000000000311, 0.6300000000000000044, 0.6624999999999999778, 0.6949999999999999512, 0.7275000000000000355, 0.7600000000000000089, 0.7924999999999999822, 0.8249999999999999556, 0.8575000000000000400, 0.8900000000000000133, 0.9224999999999999867, 0.9549999999999999600, 0.9875000000000000444, 1.020000000000000018 ),
 .UNSPECIFIED. ) ;
#18961 = DIRECTION ( 'NONE',  ( 0.000000000000000000, -0.8648648648648717963, -0.5020047465136829867 ) ) ;
#18962 = CARTESIAN_POINT ( 'NONE',  ( -0.06846944822773000372, 1.316872153397000034, -3.459566938009000392 ) ) ;
#18963 = CARTESIAN_POINT ( 'NONE',  ( 8.008165174986313417, 4.679062738103456631, 8.679582621499550399 ) ) ;
#18964 = CARTESIAN_POINT ( 'NONE',  ( 12.58137933218754867, 3.164643396295684141, 12.19610741112356322 ) ) ;
#18965 = CARTESIAN_POINT ( 'NONE',  ( 9.482733921870000415, -2.757678812098000254, -6.584768124342000206 ) ) ;
#18966 = CARTESIAN_POINT ( 'NONE',  ( 10.94903032197929882, 4.503839166471300004, -6.795411691360399686 ) ) ;
#18967 = FACE_OUTER_BOUND ( 'NONE', #60116, .T. ) ;
#18968 = CARTESIAN_POINT ( 'NONE',  ( 10.36325056272499978, 4.892034740700499817, -7.513220396995270001 ) ) ;
#18969 = CARTESIAN_POINT ( 'NONE',  ( 8.771455549952998254, 4.888629236328500660, -6.783011486330899231 ) ) ;
#18971 = CARTESIAN_POINT ( 'NONE',  ( 27.64127793187000037, -1.199999999999999956, -9.776630298829998011 ) ) ;
#18970 = DIRECTION ( 'NONE',  ( -8.952907862884472301E-11, 0.2714597137497840040, 0.9624498032681421122 ) ) ;
#18972 = DIRECTION ( 'NONE',  ( 0.000000000000000000, 0.000000000000000000, -1.000000000000000000 ) ) ;
#18973 = ORIENTED_EDGE ( 'NONE', *, *, #7086, .T. ) ;
#18974 = ADVANCED_FACE ( 'NONE', ( #54220 ), #5634, .F. ) ;
#18975 = CARTESIAN_POINT ( 'NONE',  ( 10.29399293566599916, 4.546741702992100009, 6.829299525004299376 ) ) ;
#18976 = CARTESIAN_POINT ( 'NONE',  ( 9.724613486786999772, -2.928302463146000179, 8.718481221599999387 ) ) ;
#18977 = CARTESIAN_POINT ( 'NONE',  ( 9.933633995697999097, 4.998281561686200192, 7.389201877599999690 ) ) ;
#18978 = DIRECTION ( 'NONE',  ( 0.000000000000000000, 0.000000000000000000, -1.000000000000000000 ) ) ;
#18979 = CARTESIAN_POINT ( 'NONE',  ( 10.68904248846000016, -2.568964727443000307, 7.728094434513999467 ) ) ;
#18980 = CARTESIAN_POINT ( 'NONE',  ( 13.50018479229797030, 11.10053973472265021, 4.255642710877637569 ) ) ;
#18981 = CARTESIAN_POINT ( 'NONE',  ( 23.56665676678700194, 2.935519496638999914, -13.67844162499000049 ) ) ;
#18982 = VERTEX_POINT ( 'NONE', #54919 ) ;
#18983 = CARTESIAN_POINT ( 'NONE',  ( 9.100734463322998735, -3.881063085044400118, -8.635600483553998785 ) ) ;
#18984 = CARTESIAN_POINT ( 'NONE',  ( 10.80830512578202018, -5.096679906444030017, -5.098988276665438413 ) ) ;
#18985 = CARTESIAN_POINT ( 'NONE',  ( 18.08807463888091860, 1.992345594299818501, -12.44148860874185125 ) ) ;
#18986 = CARTESIAN_POINT ( 'NONE',  ( 11.13220159457000058, -2.670356040834999778, 5.051244813867000083 ) ) ;
#18987 = DIRECTION ( 'NONE',  ( 0.000000000000000000, -0.1218274111675001492, 0.9925512993736016476 ) ) ;
#18988 = DIRECTION ( 'NONE',  ( 1.000000000000000000, 0.000000000000000000, 0.000000000000000000 ) ) ;
#18989 = CARTESIAN_POINT ( 'NONE',  ( 9.350728814717999882, -3.197530835772000035, -8.817973615970998935 ) ) ;
#18990 = CARTESIAN_POINT ( 'NONE',  ( 10.67905590578999941, 2.899999999999999911, 6.571291218949999902 ) ) ;
#18991 = ORIENTED_EDGE ( 'NONE', *, *, #34201, .F. ) ;
#18992 = CARTESIAN_POINT ( 'NONE',  ( 24.37846970953800252, -12.00848455234000056, -3.275549967069999902 ) ) ;
#18993 = CARTESIAN_POINT ( 'NONE',  ( 10.99791623168052723, -5.186580209184203483, -5.071961089083791840 ) ) ;
#18994 = LINE ( 'NONE', #3589, #58892 ) ;
#18995 = DIRECTION ( 'NONE',  ( 0.000000000000000000, 1.000000000000000000, 0.000000000000000000 ) ) ;
#18996 = CARTESIAN_POINT ( 'NONE',  ( 2.373822673703999353, -0.09607108383954167385, -3.514941141763996413 ) ) ;
#18997 = CIRCLE ( 'NONE', #61425, 1.300130688722000327 ) ;
#18998 = CARTESIAN_POINT ( 'NONE',  ( 9.360279719594000625, 3.031907308384000022, -8.729608011560001657 ) ) ;
#18999 = CARTESIAN_POINT ( 'NONE',  ( 15.89979320885400327, 3.824231472901999496, 11.71686814605000038 ) ) ;
#19000 = ORIENTED_EDGE ( 'NONE', *, *, #32542, .T. ) ;
#19001 = CARTESIAN_POINT ( 'NONE',  ( 9.323371907591601726, -2.820206136178896372, -8.179990968853758204 ) ) ;
#19002 = CARTESIAN_POINT ( 'NONE',  ( 18.10179698720198971, 2.997559868305863962, -13.67533242386441472 ) ) ;
#19003 = VERTEX_POINT ( 'NONE', #396 ) ;
#19004 = CARTESIAN_POINT ( 'NONE',  ( 10.74457120343299898, -4.042028078047379402, 6.634008278083699750 ) ) ;
#19005 = CARTESIAN_POINT ( 'NONE',  ( 24.97034827298988091, 2.963737632979523529, 11.58472174624901285 ) ) ;
#19006 = CARTESIAN_POINT ( 'NONE',  ( 8.655270280412999284, 4.162493982103000256, -5.775210092227999858 ) ) ;
#19007 = EDGE_CURVE ( 'NONE', #34497, #38102, #32055, .T. ) ;
#19008 = CARTESIAN_POINT ( 'NONE',  ( 13.49980696793000057, -9.514462421839999351, -7.834836582454001608 ) ) ;
#19009 = ADVANCED_FACE ( 'NONE', ( #43402 ), #27317, .T. ) ;
#19010 = CARTESIAN_POINT ( 'NONE',  ( 11.14767835872009982, -4.874341053673500568, -6.948943352864199952 ) ) ;
#19011 = CARTESIAN_POINT ( 'NONE',  ( 9.393246442089999704, -5.100000000000000533, -6.421387671005999387 ) ) ;
#19012 = EDGE_CURVE ( 'NONE', #56428, #66584, #65901, .T. ) ;
#19013 = CARTESIAN_POINT ( 'NONE',  ( 11.29996927726999978, -12.23272628844000032, -1.505586261403999870 ) ) ;
#19014 = ORIENTED_EDGE ( 'NONE', *, *, #28409, .T. ) ;
#19015 = CARTESIAN_POINT ( 'NONE',  ( 7.894723525210213033, 2.729257430866120604, -7.000779463158162130 ) ) ;
#19016 = CARTESIAN_POINT ( 'NONE',  ( 8.734814475091132735, 4.056037006134289413, -8.383485082298649971 ) ) ;
#19017 = CARTESIAN_POINT ( 'NONE',  ( 8.748814158775001459, 5.251032986819000214, -6.070151079272999795 ) ) ;
#19018 = VERTEX_POINT ( 'NONE', #59814 ) ;
#19019 = CARTESIAN_POINT ( 'NONE',  ( 10.26368708477999903, 4.794139572939999816, -8.804452601708000259 ) ) ;
#19020 = DIRECTION ( 'NONE',  ( 0.000000000000000000, 0.000000000000000000, 1.000000000000000000 ) ) ;
#19021 = VERTEX_POINT ( 'NONE', #7717 ) ;
#19022 = CARTESIAN_POINT ( 'NONE',  ( 8.644809814040998575, 4.698458605182900705, 6.596733927440100231 ) ) ;
#19023 = CARTESIAN_POINT ( 'NONE',  ( 17.87877696946770811, -3.124133162484060033, -12.20654824865395049 ) ) ;
#19024 = CARTESIAN_POINT ( 'NONE',  ( 11.44446504844000145, -11.61858443320999967, -1.410913393917999858 ) ) ;
#19025 = DIRECTION ( 'NONE',  ( -0.8660254038577466229, -7.065136648043377324E-14, -0.4999999998730267903 ) ) ;
#19026 = CARTESIAN_POINT ( 'NONE',  ( 9.382630518809056852, -2.846461560144221803, 8.802238404894030310 ) ) ;
#19027 = ORIENTED_EDGE ( 'NONE', *, *, #6941, .F. ) ;
#19028 = CARTESIAN_POINT ( 'NONE',  ( 11.59999999999999964, 3.168976350368595263, 7.002620348270788497 ) ) ;
#19029 = CARTESIAN_POINT ( 'NONE',  ( 9.934999999999998721, -4.640430492595999823, -9.117542781427999898 ) ) ;
#19030 = DIRECTION ( 'NONE',  ( 0.000000000000000000, 1.000000000000000000, 0.000000000000000000 ) ) ;
#19031 = CARTESIAN_POINT ( 'NONE',  ( 12.42020189403035779, 3.137187437229806086, -13.64398187047951971 ) ) ;
#19032 = CARTESIAN_POINT ( 'NONE',  ( 9.583051052052001140, -2.744602294987000146, -7.745684736446600382 ) ) ;
#19033 = CARTESIAN_POINT ( 'NONE',  ( 10.37373728961999930, -2.215269876326000364, 7.703982265807999497 ) ) ;
#19034 = CARTESIAN_POINT ( 'NONE',  ( 17.78802761781599528, 0.6915911779535691695, 13.98290807251246548 ) ) ;
#19035 = CARTESIAN_POINT ( 'NONE',  ( 11.01356641589999974, -2.786433584103999994, 6.253463831328000211 ) ) ;
#19036 = ORIENTED_EDGE ( 'NONE', *, *, #24051, .F. ) ;
#19037 = ORIENTED_EDGE ( 'NONE', *, *, #57252, .F. ) ;
#19038 = CARTESIAN_POINT ( 'NONE',  ( 9.775320280412000074, 2.527713920559999661, -6.969421869128999525 ) ) ;
#19039 = CARTESIAN_POINT ( 'NONE',  ( 11.09999999999999964, 4.000000000000000000, 7.500000000000000000 ) ) ;
#19040 = CARTESIAN_POINT ( 'NONE',  ( 12.27225454755311596, -2.172654780165926613, 13.73747135095148408 ) ) ;
#19041 = CARTESIAN_POINT ( 'NONE',  ( 9.972537864286000087, -2.899999999999999911, -6.571291218949999902 ) ) ;
#19042 = DIRECTION ( 'NONE',  ( 0.000000000000000000, 0.000000000000000000, 1.000000000000000000 ) ) ;
#19044 = B_SPLINE_CURVE_WITH_KNOTS ( 'NONE', 3,
 ( #7603, #41049, #67262, #19378, #14144, #62371, #14487, #51874, #5012, #16877, #32627, #112, #11287, #32292, #21774, #48012, #10948, #58497, #53253, #26347, #31254, #16536, #64759, #37862, #47676, #10600 ),
 .UNSPECIFIED., .F., .F.,
 ( 4, 2, 2, 2, 2, 2, 2, 2, 2, 2, 2, 2, 4 ),
 ( 0.000000000000000000, 0.06249999999999719669, 0.09374999999999751588, 0.1249999999999978351, 0.2499999999999957812, 0.3749999999999937272, 0.4999999999999916733, 0.6249999999999895639, 0.7499999999999875655, 0.8124999999999880096, 0.8437499999999883427, 0.8749999999999886757, 1.000000000000000000 ),
 .UNSPECIFIED. ) ;
#19043 = CARTESIAN_POINT ( 'NONE',  ( 6.953073139469000630, -9.233001678504999532, 5.200628701625999994 ) ) ;
#19046 = CARTESIAN_POINT ( 'NONE',  ( 8.962151703908455502, 2.270851035168802490, 7.235830473402728558 ) ) ;
#19045 = CARTESIAN_POINT ( 'NONE',  ( 9.475151519677000422, -3.972335373863620234, 6.221087886525999089 ) ) ;
#19047 = CARTESIAN_POINT ( 'NONE',  ( 12.08810207955109917, -4.796537143354000499, 7.825000000000000178 ) ) ;
#19048 = ORIENTED_EDGE ( 'NONE', *, *, #66539, .T. ) ;
#19049 = CYLINDRICAL_SURFACE ( 'NONE', #54820, 0.5500000000000000444 ) ;
#19050 = EDGE_CURVE ( 'NONE', #49079, #46011, #13322, .T. ) ;
#19051 = CARTESIAN_POINT ( 'NONE',  ( 23.56666365135700403, -11.16210620494999439, -3.571147222960000533 ) ) ;
#19052 = CARTESIAN_POINT ( 'NONE',  ( 9.402304893999998470, -4.531444417037000072, -6.133284059228000018 ) ) ;
#19053 = CARTESIAN_POINT ( 'NONE',  ( 18.12461185120978868, 0.2575478136180248678, 12.69649014468028980 ) ) ;
#19054 = CARTESIAN_POINT ( 'NONE',  ( 12.70148909159118844, -0.6166679310204360442, 12.67983904306179888 ) ) ;
#19055 = ADVANCED_FACE ( 'NONE', ( #14001 ), #3155, .T. ) ;
#19056 = CARTESIAN_POINT ( 'NONE',  ( 4.500000000000000000, 0.000000000000000000, 0.000000000000000000 ) ) ;
#19057 = CARTESIAN_POINT ( 'NONE',  ( 10.96431548498000197, -5.151797042792000347, 5.074130565745999633 ) ) ;
#19058 = CARTESIAN_POINT ( 'NONE',  ( 10.22514748322308797, 2.649941783575544108, 7.500008211948054893 ) ) ;
#19059 = CARTESIAN_POINT ( 'NONE',  ( 10.64118447801629941, 5.277702140407999565, 7.528171279442569919 ) ) ;
#19060 = CARTESIAN_POINT ( 'NONE',  ( 24.34833250312466646, -3.256146816482774486, -12.15210535601315733 ) ) ;
#19061 = CARTESIAN_POINT ( 'NONE',  ( 0.3276025866252778029, -2.044343127223234191, 2.661567956154585524 ) ) ;
#19062 = CARTESIAN_POINT ( 'NONE',  ( 9.898726835366622012, 2.762657331216825884, -6.942781169495302329 ) ) ;
#19063 = VERTEX_POINT ( 'NONE', #66786 ) ;
#19064 = CARTESIAN_POINT ( 'NONE',  ( 12.49249186488742680, -0.5416145769730054127, -12.68445494689095732 ) ) ;
#19065 = CARTESIAN_POINT ( 'NONE',  ( 11.03776249210999971, -8.050323671732000363, -6.914613055281999543 ) ) ;
#19066 = DIRECTION ( 'NONE',  ( -1.000000000000000000, 0.000000000000000000, 0.000000000000000000 ) ) ;
#19067 = CARTESIAN_POINT ( 'NONE',  ( 7.550614158771000284, 4.468366666325000125, 8.882140983065999862 ) ) ;
#19068 = DIRECTION ( 'NONE',  ( 1.000000000000000000, 0.000000000000000000, 0.000000000000000000 ) ) ;
#19069 = ORIENTED_EDGE ( 'NONE', *, *, #68328, .T. ) ;
#19070 = CARTESIAN_POINT ( 'NONE',  ( 6.198935906450000033, 0.002327316029692999642, 1.176084684120999979 ) ) ;
#19071 = CARTESIAN_POINT ( 'NONE',  ( 10.91574126908911069, 9.681045672762477849, 5.885333278431389203 ) ) ;
#19072 = CARTESIAN_POINT ( 'NONE',  ( 10.57538794102195290, 5.349775832304656475, -7.676723066621553571 ) ) ;
#19073 = CARTESIAN_POINT ( 'NONE',  ( 1.573890132540375131, 2.150913519912194705, 2.798833948393636639 ) ) ;
#19074 = CARTESIAN_POINT ( 'NONE',  ( 10.64391429142989765, 4.022379549362480766, -6.325326139450999641 ) ) ;
#19075 = ORIENTED_EDGE ( 'NONE', *, *, #21853, .F. ) ;
#19076 = B_SPLINE_CURVE_WITH_KNOTS ( 'NONE', 3,
 ( #7600, #65972, #64929, #39420 ),
 .UNSPECIFIED., .F., .F.,
 ( 4, 4 ),
 ( 0.000000000000000000, 1.000000000000000000 ),
 .UNSPECIFIED. ) ;
#19077 = CARTESIAN_POINT ( 'NONE',  ( 11.01776264201000011, -4.914128622650000722, 8.587713430305999651 ) ) ;
#19078 = ORIENTED_EDGE ( 'NONE', *, *, #6068, .T. ) ;
#19079 = VECTOR ( 'NONE', #26862, 999.9999999999998863 ) ;
#19080 = DIRECTION ( 'NONE',  ( 0.000000000000000000, 0.000000000000000000, -1.000000000000000000 ) ) ;
#19081 = CARTESIAN_POINT ( 'NONE',  ( 16.04750315638899849, 3.679714098878999806, 11.11063745184000062 ) ) ;
#19082 = CARTESIAN_POINT ( 'NONE',  ( 18.25578913467704112, 0.1888260363403093667, -13.99874504378992413 ) ) ;
#19083 = EDGE_CURVE ( 'NONE', #59297, #23381, #55617, .T. ) ;
#19084 = EDGE_LOOP ( 'NONE', ( #1991, #18434, #50907, #55561 ) ) ;
#19085 = CARTESIAN_POINT ( 'NONE',  ( 10.98934649328336732, 7.566743496310233574, -6.301340071414541555 ) ) ;
#19086 = EDGE_CURVE ( 'NONE', #61050, #46630, #67084, .T. ) ;
#19087 = CARTESIAN_POINT ( 'NONE',  ( 9.225741355579115677, 4.497363567101849036, 9.030598125317942149 ) ) ;
#19088 = VECTOR ( 'NONE', #18800, 1000.000000000000000 ) ;
#19089 = DIRECTION ( 'NONE',  ( -0.7071067268961630514, -0.09465676129217508172, 0.7007425877737639697 ) ) ;
#19090 = DIRECTION ( 'NONE',  ( -1.000000000000000000, 0.000000000000000000, 0.000000000000000000 ) ) ;
#19091 = EDGE_CURVE ( 'NONE', #5123, #14810, #52528, .T. ) ;
#19092 = CARTESIAN_POINT ( 'NONE',  ( 17.96886609968857584, -2.968499926956239765, 12.32999726799531004 ) ) ;
#19093 = ORIENTED_EDGE ( 'NONE', *, *, #4416, .T. ) ;
#19094 = CARTESIAN_POINT ( 'NONE',  ( 10.77462219945999955, -5.575466189878000911, 8.682669263022999573 ) ) ;
#19095 = ADVANCED_FACE ( 'NONE', ( #56302 ), #7875, .F. ) ;
#19096 = CARTESIAN_POINT ( 'NONE',  ( 11.59999999999999964, 5.179498027601999510, 7.825000000000000178 ) ) ;
#19097 = CARTESIAN_POINT ( 'NONE',  ( 10.40434687351665310, 2.750000000000000000, -7.663624617374465764 ) ) ;
#19098 =( NAMED_UNIT ( * ) SI_UNIT ( $, .STERADIAN. ) SOLID_ANGLE_UNIT ( ) );
#19099 = CARTESIAN_POINT ( 'NONE',  ( 17.55505043854147118, -1.760845406083394682, 12.47635457398814829 ) ) ;
#19100 = ORIENTED_EDGE ( 'NONE', *, *, #64483, .T. ) ;
#19101 = CARTESIAN_POINT ( 'NONE',  ( 10.41164068750943450, -2.873222873819646583, -6.752018918863353925 ) ) ;
#19102 = CARTESIAN_POINT ( 'NONE',  ( 10.91872448493765724, -2.825398922886805497, -6.797111659689116792 ) ) ;
#19103 = CARTESIAN_POINT ( 'NONE',  ( 10.67500447327519097, 2.650284540010591439, 7.500001951671590561 ) ) ;
#19104 = CARTESIAN_POINT ( 'NONE',  ( 24.00507894008998022, -3.345686396274558216, -12.73791187279332249 ) ) ;
#19105 = CARTESIAN_POINT ( 'NONE',  ( 11.64444011873732698, 3.380850026661442964, -11.14878564717023401 ) ) ;
#19106 = CARTESIAN_POINT ( 'NONE',  ( 12.47427908008581987, -0.5306878043354068542, -13.88636785578042421 ) ) ;
#19107 = CARTESIAN_POINT ( 'NONE',  ( 18.16006747845244007, -2.341920795209953443, 12.48703680160762097 ) ) ;
#19108 = ORIENTED_EDGE ( 'NONE', *, *, #4512, .F. ) ;
#19109 = CARTESIAN_POINT ( 'NONE',  ( 11.18923293495519822, -5.032672437899000428, -7.458486839450950256 ) ) ;
#19110 = ORIENTED_EDGE ( 'NONE', *, *, #45232, .T. ) ;
#19111 = CARTESIAN_POINT ( 'NONE',  ( 10.48165121391000021, 4.022873529486999722, 9.090897232145000117 ) ) ;
#19112 = ADVANCED_FACE ( 'NONE', ( #34646 ), #8063, .F. ) ;
#19113 = CARTESIAN_POINT ( 'NONE',  ( 11.09999999999999964, 5.350000000000000533, -7.500000000000000000 ) ) ;
#19114 = CARTESIAN_POINT ( 'NONE',  ( 8.938854719593997800, 5.597201461420000967, -8.171008079894999554 ) ) ;
#19115 = CARTESIAN_POINT ( 'NONE',  ( 3.096752846175000240, -1.627991971746999944, 3.147629369397000332 ) ) ;
#19116 = CARTESIAN_POINT ( 'NONE',  ( 10.01276877312999858, -3.440626575163999945, -9.267592337498999910 ) ) ;
#19117 = LINE ( 'NONE', #45699, #22761 ) ;
#19118 = CARTESIAN_POINT ( 'NONE',  ( 25.30000327618300204, -10.83443035398000021, 3.855530949778000149 ) ) ;
#19119 = ORIENTED_EDGE ( 'NONE', *, *, #18066, .T. ) ;
#19120 = CARTESIAN_POINT ( 'NONE',  ( 11.85918179236250047, -4.238363971154499588, 8.615559381441000752 ) ) ;
#19121 = CARTESIAN_POINT ( 'NONE',  ( 10.90374609491999891, 3.726846467344000047, 5.900456154266000119 ) ) ;
#19122 = CARTESIAN_POINT ( 'NONE',  ( 10.62549262323914334, -5.350086361207873509, -7.676738019119357048 ) ) ;
#19123 = CARTESIAN_POINT ( 'NONE',  ( 7.629816940376999312, -4.763531818439999732, 5.668890958491999754 ) ) ;
#19125 = CARTESIAN_POINT ( 'NONE',  ( 11.00000000000000000, -2.920245322398999921, -7.825000000000000178 ) ) ;
#19124 = CARTESIAN_POINT ( 'NONE',  ( 11.08492721656000057, 3.668390701878999849, 5.558148445539999649 ) ) ;
#19126 = CARTESIAN_POINT ( 'NONE',  ( 11.69559063708295987, 5.086518862378000883, -7.805482129094999166 ) ) ;
#19127 = CARTESIAN_POINT ( 'NONE',  ( 10.93529823098193710, 2.837224294051361451, -6.734948068539347688 ) ) ;
#19128 = EDGE_CURVE ( 'NONE', #5014, #12823, #42075, .T. ) ;
#19129 = CARTESIAN_POINT ( 'NONE',  ( 9.984292290062997566, 4.868609929059700470, -6.995659746333000584 ) ) ;
#19130 = FACE_OUTER_BOUND ( 'NONE', #8340, .T. ) ;
#19131 = B_SPLINE_CURVE_WITH_KNOTS ( 'NONE', 3,
 ( #53527, #47252, #5619, #16115, #63309, #68555, #16795, #37785, #20677, #47939, #26960, #15436, #37440, #58762, #11213, #26272 ),
 .UNSPECIFIED., .F., .F.,
 ( 4, 2, 2, 2, 2, 2, 2, 4 ),
 ( 0.1254233535197428473, 0.2190668680422942494, 0.3127103825648456237, 0.4999974116099478172, 0.5936409261324988584, 0.6872844406550501217, 0.7809279551776012740, 0.8745714697001524263 ),
 .UNSPECIFIED. ) ;
#19132 = CARTESIAN_POINT ( 'NONE',  ( 24.54688887196200042, 3.662825465818000392, 12.34578425079000041 ) ) ;
#19133 = CARTESIAN_POINT ( 'NONE',  ( 8.119711571783735593, 5.029157459567885624, -6.453063860975558619 ) ) ;
#19134 = EDGE_CURVE ( 'NONE', #64166, #7303, #51241, .T. ) ;
#19135 = CARTESIAN_POINT ( 'NONE',  ( 9.236413463905998711, -3.915843685459630574, 6.617590440947399344 ) ) ;
#19136 = ORIENTED_EDGE ( 'NONE', *, *, #3791, .T. ) ;
#19137 = CARTESIAN_POINT ( 'NONE',  ( 7.705394353206999725, -3.245532552444000185, 8.949627348471000943 ) ) ;
#19138 = B_SPLINE_CURVE_WITH_KNOTS ( 'NONE', 3,
 ( #33183, #1025, #49601, #2061, #6250 ),
 .UNSPECIFIED., .F., .F.,
 ( 4, 1, 4 ),
 ( 0.000000000000000000, 0.5000000000000000000, 1.000000000000000000 ),
 .UNSPECIFIED. ) ;
#19139 = CARTESIAN_POINT ( 'NONE',  ( 17.99965052394114906, 1.940731178328044093, 13.86484045969604395 ) ) ;
#19140 = CARTESIAN_POINT ( 'NONE',  ( 13.00000000001300116, -11.52577654661000039, -1.696746661728000038 ) ) ;
#19141 = DIRECTION ( 'NONE',  ( 1.000000000000000000, 0.000000000000000000, 0.000000000000000000 ) ) ;
#19142 = ORIENTED_EDGE ( 'NONE', *, *, #12414, .F. ) ;
#19143 = FACE_OUTER_BOUND ( 'NONE', #46429, .T. ) ;
#19145 = CARTESIAN_POINT ( 'NONE',  ( 11.63611496860034933, 5.171412538012999605, 8.100294210499798808 ) ) ;
#19144 = CARTESIAN_POINT ( 'NONE',  ( 9.383380199233998908, -3.139757597894699881, -7.391875284387199763 ) ) ;
#19146 = CLOSED_SHELL ( 'NONE', ( #5869, #34070, #17550, #44949, #7055, #55904, #6373, #2873, #24871, #49985, #55116, #57093, #67961, #64711, #54632, #34419, #13849, #12959, #44013, #14847, #14132, #50541, #55316, #15476, #35796, #46655, #16088, #53616, #59120, #23837, #50527, #65419, #23915, #24001, #25393, #9335, #59657, #49003, #39479, #44140, #49794, #2627, #49474, #22436, #43536, #20704, #36520, #64004, #21686, #29814, #45369, #60362, #32280, #20207, #9208, #63064, #52725, #37009, #3022, #5346, #68025, #7797, #63421, #57916, #31283, #37355, #34152, #46013, #10175, #68806, #40443, #12228, #36409, #49051, #28845, #26861, #63430, #26401, #49577, #64453, #28407, #58478, #9074, #31535, #38030, #35638, #40272, #67382, #559, #645, #47066, #30398, #63822, #34851, #30722, #14990, #16556, #62809, #42079, #24419, #26524, #50519, #8490, #42002, #8214, #64685, #32316, #22040, #60635, #64762, #3988, #1756, #4471, #1569, #36519, #52662, #59597, #23238, #35753, #65022, #39756, #4164, #41433 ) ) ;
#19147 = CARTESIAN_POINT ( 'NONE',  ( 10.90000000000000036, -8.091320520030999219, -7.077643127633000297 ) ) ;
#19148 = ORIENTED_EDGE ( 'NONE', *, *, #67102, .T. ) ;
#19149 = CARTESIAN_POINT ( 'NONE',  ( 1.384306799207333460, -1.762666431298145930, -3.058252359239904905 ) ) ;
#19150 = CARTESIAN_POINT ( 'NONE',  ( 18.03520353647602903, -3.065561386738608007, -13.66025540057654375 ) ) ;
#19151 = CARTESIAN_POINT ( 'NONE',  ( 10.37457053952199892, 3.551693493661699730, 8.548957288282998945 ) ) ;
#19152 = CARTESIAN_POINT ( 'NONE',  ( 10.41185831014999863, -2.101597930377999912, 7.856264717901999539 ) ) ;
#19153 = PLANE ( 'NONE',  #8665 ) ;
#19154 = EDGE_LOOP ( 'NONE', ( #3634, #63893, #5923, #34323 ) ) ;
#19155 = FACE_OUTER_BOUND ( 'NONE', #4524, .T. ) ;
#19156 = CARTESIAN_POINT ( 'NONE',  ( 13.99999999379500082, 8.815218614167999789, 7.616697584347000394 ) ) ;
#19157 = CARTESIAN_POINT ( 'NONE',  ( 7.962503634123480722, -2.285285773337808912, 7.208897372649888169 ) ) ;
#19158 = CARTESIAN_POINT ( 'NONE',  ( 9.414314870535999802, -3.941041813398000304, 5.878346364186999295 ) ) ;
#19159 = CARTESIAN_POINT ( 'NONE',  ( 10.68546886766499959, -4.566506264294200257, -6.470713638631999665 ) ) ;
#19160 = CARTESIAN_POINT ( 'NONE',  ( 9.119480666858999385, -3.619299191678599925, 6.423523106103999680 ) ) ;
#19161 = ORIENTED_EDGE ( 'NONE', *, *, #40041, .T. ) ;
#19162 = CARTESIAN_POINT ( 'NONE',  ( 10.48315960899000032, -5.083827399151000570, -4.649899757833000358 ) ) ;
#19163 = B_SPLINE_CURVE_WITH_KNOTS ( 'NONE', 3,
 ( #59555, #7109, #60255, #14000, #1519, #11655, #832, #12357, #12703, #22838, #12007, #33689, #34040, #65830, #43488, #64785, #55007, #43832 ),
 .UNSPECIFIED., .F., .F.,
 ( 4, 2, 2, 2, 2, 2, 2, 2, 4 ),
 ( 0.000000000000000000, 0.1250000000000000000, 0.2500000000000000000, 0.3750000000000000000, 0.5000000000000000000, 0.6250000000000000000, 0.7500000000000000000, 0.8750000000000000000, 1.000000000000000000 ),
 .UNSPECIFIED. ) ;
#19164 = CARTESIAN_POINT ( 'NONE',  ( 7.307500000000000107, -0.2500000000000000000, -3.149999999999999911 ) ) ;
#19165 = ORIENTED_EDGE ( 'NONE', *, *, #52834, .F. ) ;
#19166 = DIRECTION ( 'NONE',  ( 0.000000000000000000, 0.000000000000000000, -1.000000000000000000 ) ) ;
#19167 = ORIENTED_EDGE ( 'NONE', *, *, #47274, .T. ) ;
#19168 = CARTESIAN_POINT ( 'NONE',  ( 10.09166489801000033, -4.565692099013000771, -8.879633571423999783 ) ) ;
#19169 = CARTESIAN_POINT ( 'NONE',  ( 8.356920280409999791, 4.851303550474000303, -9.008742670124000540 ) ) ;
#19170 = CARTESIAN_POINT ( 'NONE',  ( 11.83003632436370012, 2.756744593645999775, -7.209663534847899236 ) ) ;
#19171 = CARTESIAN_POINT ( 'NONE',  ( 11.59999999999999964, -4.000000000000000000, -7.500000000000000000 ) ) ;
#19172 = CARTESIAN_POINT ( 'NONE',  ( 12.39767999896653450, 2.025889534879409037, -12.54950459294603071 ) ) ;
#19173 = EDGE_CURVE ( 'NONE', #718, #2928, #36252, .T. ) ;
#19174 = CARTESIAN_POINT ( 'NONE',  ( 10.87872469555899890, -3.497841151814999883, 8.368784980615899372 ) ) ;
#19175 = CARTESIAN_POINT ( 'NONE',  ( 9.234510841229999656, 5.964723767581000757, 7.776480083716999836 ) ) ;
#19176 = EDGE_CURVE ( 'NONE', #5868, #59008, #16788, .T. ) ;
#19177 = ORIENTED_EDGE ( 'NONE', *, *, #39025, .T. ) ;
#19178 = B_SPLINE_CURVE_WITH_KNOTS ( 'NONE', 3,
 ( #55969, #66102, #40236, #13332, #8075, #12983, #55628, #29417, #50726, #45483, #61553, #13670, #34998, #56313, #57672, #47890, #16058, #3840, #36357, #10467, #9780, #58031, #46513, #63256, #58366, #42637, #30435, #20970, #31463, #51746, #62912, #31131, #56994, #63608, #9431, #47546, #52782, #20278, #52085, #63947, #31809, #25178, #52433, #4529, #15383, #53126 ),
 .UNSPECIFIED., .F., .F.,
 ( 4, 2, 2, 2, 2, 2, 2, 2, 2, 2, 2, 2, 2, 2, 1, 2, 2, 2, 2, 2, 1, 2, 2, 4 ),
 ( 0.000000000000000000, 0.06247329711231583427, 0.09370994566847631879, 0.1249465942246368033, 0.1405649185027146864, 0.1561832427807925694, 0.1874198913369436725, 0.2030382156150212780, 0.2186565398930988835, 0.2264657020321358682, 0.2342748641711728530, 0.2498931884492468225, 0.2811298370053947893, 0.2889389991444329397, 0.2967481612834710902, 0.3123664855615474467, 0.3279848098396238032, 0.3436031341177001597, 0.3748397826738527616, 0.3904581069519290071, 0.4060764312300053636, 0.4373130797861564112, 0.4685497283423075143, 0.4997863768984585620 ),
 .UNSPECIFIED. ) ;
#19179 = CARTESIAN_POINT ( 'NONE',  ( 9.843930206850000530, 2.750000000000000000, 7.500000000000000000 ) ) ;
#19180 = CARTESIAN_POINT ( 'NONE',  ( 9.021581853209999835, -2.193670085072000120, 7.400591740205000768 ) ) ;
#19181 = CARTESIAN_POINT ( 'NONE',  ( 10.97499895057999986, -3.730349362740999292E-14, -9.259260025373999922E-14 ) ) ;
#19182 = ORIENTED_EDGE ( 'NONE', *, *, #65753, .F. ) ;
#19183 = CARTESIAN_POINT ( 'NONE',  ( 12.18627227647246691, -2.104539383777993766, -12.42301525548629471 ) ) ;
#19184 = CARTESIAN_POINT ( 'NONE',  ( 10.34995525820099971, 3.892289273474800471, 8.635644537520001052 ) ) ;
#19185 = CARTESIAN_POINT ( 'NONE',  ( 10.09249435321000021, -2.841617206345000035, -8.724656239052000828 ) ) ;
#19186 = LINE ( 'NONE', #51349, #26560 ) ;
#19187 = CARTESIAN_POINT ( 'NONE',  ( 17.61786948987200319, -12.16775412387000088, 3.132314945639000037 ) ) ;
#19188 = CARTESIAN_POINT ( 'NONE',  ( 8.995772571291157149, 2.998508658148201889, -8.076234199639099387 ) ) ;
#19189 = CARTESIAN_POINT ( 'NONE',  ( 12.39041931600613466, -2.032227219086497616, -13.76156428297224998 ) ) ;
#19190 = CARTESIAN_POINT ( 'NONE',  ( 17.62710295837868557, -0.6209187240130101815, -12.67955909024710337 ) ) ;
#19191 = CARTESIAN_POINT ( 'NONE',  ( 11.28118179236249929, -4.267047616085000605, -6.250199235344999771 ) ) ;
#19193 = FACE_OUTER_BOUND ( 'NONE', #61397, .T. ) ;
#19192 = B_SPLINE_CURVE_WITH_KNOTS ( 'NONE', 3,
 ( #17577, #50083, #12677, #16873 ),
 .UNSPECIFIED., .F., .F.,
 ( 4, 4 ),
 ( 0.8745808026672123869, 1.000000000000000000 ),
 .UNSPECIFIED. ) ;
#19194 = ORIENTED_EDGE ( 'NONE', *, *, #52475, .T. ) ;
#19195 = ORIENTED_EDGE ( 'NONE', *, *, #2778, .T. ) ;
#19196 = ADVANCED_FACE ( 'NONE', ( #19926 ), #12360, .T. ) ;
#19197 = VECTOR ( 'NONE', #373, 1000.000000000000000 ) ;
#19198 = CARTESIAN_POINT ( 'NONE',  ( 23.60000000000000142, 0.9826074463019562888, -13.89481017416844288 ) ) ;
#19199 = CARTESIAN_POINT ( 'NONE',  ( 7.986083034292075666, 5.349307872168524547, 7.676713696079059623 ) ) ;
#19200 = CARTESIAN_POINT ( 'NONE',  ( 10.56590837162999996, 5.293226105229999590, -7.067087619452999903 ) ) ;
#19201 = FACE_BOUND ( 'NONE', #63394, .T. ) ;
#19202 = CARTESIAN_POINT ( 'NONE',  ( 17.98531014845338660, 2.046560857067137640, 12.54571659797612071 ) ) ;
#19203 = CARTESIAN_POINT ( 'NONE',  ( 17.88705809229600163, 3.642474092890999771, -12.02409483768999898 ) ) ;
#19204 = CARTESIAN_POINT ( 'NONE',  ( 9.538432183420001209, 5.620896541217999420, 7.423100299691999915 ) ) ;
#19205 = CARTESIAN_POINT ( 'NONE',  ( 10.28172590882367743, -3.320041345951468159, -8.679799923475449930 ) ) ;
#19206 = ORIENTED_EDGE ( 'NONE', *, *, #27270, .F. ) ;
#19207 = CARTESIAN_POINT ( 'NONE',  ( 12.76350981947229890, -1.876041592482997400, 12.57528602315340294 ) ) ;
#19208 = CARTESIAN_POINT ( 'NONE',  ( 8.844480666858999030, -3.665111009453500213, -8.446938520915798776 ) ) ;
#19209 = CARTESIAN_POINT ( 'NONE',  ( 11.14994211610999919, 2.627136771666999771, 6.696094414592000277 ) ) ;
#19210 = CARTESIAN_POINT ( 'NONE',  ( 11.92834208742529967, -4.706521750018099581, 6.389420067180999752 ) ) ;
#19211 = CARTESIAN_POINT ( 'NONE',  ( 10.91610672858429965, 3.088399709291500095, -6.814233985789400094 ) ) ;
#19212 = CARTESIAN_POINT ( 'NONE',  ( 12.30935811146625980, 0.3808128809978839624, 12.69231869260112155 ) ) ;
#19213 = CARTESIAN_POINT ( 'NONE',  ( 8.957392219593000249, 2.678331728353000152, 8.735281589464001684 ) ) ;
#19214 = CARTESIAN_POINT ( 'NONE',  ( 10.53138775541999905, 5.607751175212000838, 7.280102404048999887 ) ) ;
#19215 = CARTESIAN_POINT ( 'NONE',  ( 12.24703709751428349, 2.218305284339069594, 12.51274264014588589 ) ) ;
#19216 = ADVANCED_FACE ( 'NONE', ( #53113 ), #62900, .F. ) ;
#19217 = ORIENTED_EDGE ( 'NONE', *, *, #24474, .F. ) ;
#19218 = CARTESIAN_POINT ( 'NONE',  ( 9.874770280412001000, 4.038835765825999680, -5.935509327774999733 ) ) ;
#19219 = CARTESIAN_POINT ( 'NONE',  ( 10.93656785386839836, 2.939720539848000413, -8.213529149347399638 ) ) ;
#19220 = CARTESIAN_POINT ( 'NONE',  ( 13.50018479229300006, 11.60142623882999935, 2.415183939829000259 ) ) ;
#19222 = CARTESIAN_POINT ( 'NONE',  ( 10.27101354018233437, 3.231816600031359066, 8.499583552997725278 ) ) ;
#19221 = CARTESIAN_POINT ( 'NONE',  ( 7.919004440377000797, -5.361050935357000391, 6.973449182446000094 ) ) ;
#19223 = CARTESIAN_POINT ( 'NONE',  ( 12.09999999999999787, -3.165084187357962264, 8.298683811023391144 ) ) ;
#19224 = CARTESIAN_POINT ( 'NONE',  ( 10.57564694612699974, -4.931992688388300294, -7.871941502982999772 ) ) ;
#19225 = ORIENTED_EDGE ( 'NONE', *, *, #20355, .F. ) ;
#19226 = VECTOR ( 'NONE', #12826, 1000.000000000000000 ) ;
#19227 = CARTESIAN_POINT ( 'NONE',  ( 2.249566109761000465, -3.577811800725999802, 1.152232014823999950 ) ) ;
#19228 = CARTESIAN_POINT ( 'NONE',  ( 17.98740632602357792, -0.4515327042052340034, -12.68919950485279990 ) ) ;
#19230 = CARTESIAN_POINT ( 'NONE',  ( 5.500000000000000000, -12.78667792605000031, -2.345384795463000049 ) ) ;
#19229 = CARTESIAN_POINT ( 'NONE',  ( 12.79999999914999975, 12.11987927271999865, -3.159802730921999814 ) ) ;
#19231 = DIRECTION ( 'NONE',  ( -1.000000000000000000, 0.000000000000000000, 0.000000000000000000 ) ) ;
#19232 = CARTESIAN_POINT ( 'NONE',  ( 10.12671450658999994, 3.117528978489000124, 8.613535509676999880 ) ) ;
#19233 = CARTESIAN_POINT ( 'NONE',  ( 10.99999999997000089, 4.000000000000000000, -7.500000000000000000 ) ) ;
#19234 = FACE_OUTER_BOUND ( 'NONE', #13420, .T. ) ;
#19235 = CYLINDRICAL_SURFACE ( 'NONE', #23220, 0.6250000000000005551 ) ;
#19236 = CARTESIAN_POINT ( 'NONE',  ( 7.218293146793000048, -4.773080213113000347, 8.927399220053999329 ) ) ;
#19237 = ORIENTED_EDGE ( 'NONE', *, *, #60776, .F. ) ;
#19238 = CARTESIAN_POINT ( 'NONE',  ( 7.737829719589999655, 5.687206835507000235, 6.847268999608999707 ) ) ;
#19239 = CARTESIAN_POINT ( 'NONE',  ( 25.60000000000000142, -8.527654132749999505, 7.260537518967999482 ) ) ;
#19240 = CARTESIAN_POINT ( 'NONE',  ( 7.418346648492968320, -2.395435861435949221, 8.173148036598570698 ) ) ;
#19241 = AXIS2_PLACEMENT_3D ( 'NONE', #48942, #31486, #47912 ) ;
#19242 = DIRECTION ( 'NONE',  ( 1.000000000000000000, 0.000000000000000000, 0.000000000000000000 ) ) ;
#19243 = CARTESIAN_POINT ( 'NONE',  ( 1.600201902857000036, 0.7023893950988999713, -3.352829814747000370 ) ) ;
#19244 = VERTEX_POINT ( 'NONE', #35667 ) ;
#19245 = CARTESIAN_POINT ( 'NONE',  ( 1.477094749129042706, -2.689122896592814449, 1.917576298700700566 ) ) ;
#19246 = CARTESIAN_POINT ( 'NONE',  ( 12.27359063708300013, -3.044227915785300276, 7.231278212164300001 ) ) ;
#19247 = CARTESIAN_POINT ( 'NONE',  ( 10.76947109217999810, -5.100000000000000533, -6.152188490330000370 ) ) ;
#19248 = CARTESIAN_POINT ( 'NONE',  ( 10.87148757351999961, 5.567567343464999929, 7.772413227960999649 ) ) ;
#19249 = CARTESIAN_POINT ( 'NONE',  ( 10.40749413291699987, 4.788043169210699723, 7.859564368461399830 ) ) ;
#19250 = AXIS2_PLACEMENT_3D ( 'NONE', #23766, #6644, #6993 ) ;
#19251 = DIRECTION ( 'NONE',  ( 1.000000000000000000, 0.000000000000000000, 0.000000000000000000 ) ) ;
#19252 = CARTESIAN_POINT ( 'NONE',  ( 10.57656694038000111, -5.344897889496000865, -7.298883676216999739 ) ) ;
#19253 = CARTESIAN_POINT ( 'NONE',  ( 17.98272759268933285, 0.4562271229319662669, -13.88993195058941410 ) ) ;
#19254 = CARTESIAN_POINT ( 'NONE',  ( 10.36180282788866691, 2.874603711589695187, -6.749639981055123528 ) ) ;
#19255 = EDGE_CURVE ( 'NONE', #37562, #50185, #67804, .T. ) ;
#19256 = CARTESIAN_POINT ( 'NONE',  ( 12.80505043854146940, -1.875000000000000444, 12.57545641911172396 ) ) ;
#19257 = EDGE_CURVE ( 'NONE', #56117, #68518, #14591, .T. ) ;
#19258 = CARTESIAN_POINT ( 'NONE',  ( 8.579017984034141620, 4.083608998234213416, 5.755606773672980125 ) ) ;
#19259 = VERTEX_POINT ( 'NONE', #19584 ) ;
#19260 = CARTESIAN_POINT ( 'NONE',  ( 17.84276413147956220, -1.945066902726407365, 13.77561296414734215 ) ) ;
#19261 = CARTESIAN_POINT ( 'NONE',  ( 17.92097848889117273, 3.007049802571681862, -13.55275178749822018 ) ) ;
#19262 = ORIENTED_EDGE ( 'NONE', *, *, #58830, .F. ) ;
#19263 = VERTEX_POINT ( 'NONE', #40905 ) ;
#19264 = CARTESIAN_POINT ( 'NONE',  ( 10.69568717260499824, 3.533932086969799879, 6.739296831621899742 ) ) ;
#19265 = CARTESIAN_POINT ( 'NONE',  ( 4.149992563292000725, 0.5234817089163691373, -1.947893036340042405 ) ) ;
#19266 = CARTESIAN_POINT ( 'NONE',  ( 6.899999691988000450, 11.00717859340000082, 1.432487142323000118 ) ) ;
#19267 = CARTESIAN_POINT ( 'NONE',  ( 9.538432183420001209, 5.620896541217999420, 7.423100299691999915 ) ) ;
#19268 = DIRECTION ( 'NONE',  ( 0.7071067811865475727, -0.7071067811865475727, 0.000000000000000000 ) ) ;
#19269 = CARTESIAN_POINT ( 'NONE',  ( 9.150912690312626552, -4.805207160112336950, -7.842306439064141266 ) ) ;
#19270 = CARTESIAN_POINT ( 'NONE',  ( 10.03612181215999932, -3.011786236723999810, 8.746965724352000038 ) ) ;
#19271 = CARTESIAN_POINT ( 'NONE',  ( 18.10839966799242617, -0.4648927885597820553, -12.59142395508372836 ) ) ;
#19272 = CARTESIAN_POINT ( 'NONE',  ( 9.947300131853999972, -4.892806669161000599, -9.067746434455999704 ) ) ;
#19273 = B_SPLINE_CURVE_WITH_KNOTS ( 'NONE', 3,
 ( #20941, #53096, #10784, #295, #37023, #68469, #42273, #26189, #37358, #53442 ),
 .UNSPECIFIED., .F., .F.,
 ( 4, 2, 2, 2, 4 ),
 ( 0.000000000000000000, 0.2038808316443378454, 0.4077616632886756909, 0.6116424949330134808, 0.8155233265773513818 ),
 .UNSPECIFIED. ) ;
#19274 = CARTESIAN_POINT ( 'NONE',  ( 10.65364694612719809, -4.804498860841600383, -7.821061011719899980 ) ) ;
#19275 = CARTESIAN_POINT ( 'NONE',  ( 7.289711015751999312, -0.9708250560305000665, 0.5387387265405000347 ) ) ;
#19276 = ORIENTED_EDGE ( 'NONE', *, *, #59925, .F. ) ;
#19277 = ADVANCED_FACE ( 'NONE', ( #9765 ), #47533, .T. ) ;
#19278 = B_SPLINE_CURVE_WITH_KNOTS ( 'NONE', 3,
 ( #53049, #4448, #21906, #9700 ),
 .UNSPECIFIED., .F., .F.,
 ( 4, 4 ),
 ( 0.000000000000000000, 1.000000000000000000 ),
 .UNSPECIFIED. ) ;
#19279 = CARTESIAN_POINT ( 'NONE',  ( 10.96239535880000027, -6.767634501268999792, -5.462414138040999845 ) ) ;
#19280 = AXIS2_PLACEMENT_3D ( 'NONE', #26967, #65736, #65386 ) ;
#19281 = CARTESIAN_POINT ( 'NONE',  ( 24.76776889611345922, 8.625621812597076499, 8.557830585166838588 ) ) ;
#19282 = EDGE_CURVE ( 'NONE', #41592, #66341, #62562, .T. ) ;
#19283 = CARTESIAN_POINT ( 'NONE',  ( 24.30001683570900184, 3.271769286791000209, 12.21048169671000139 ) ) ;
#19284 = CARTESIAN_POINT ( 'NONE',  ( 9.709696787963999043, 4.219671260427300119, -6.239790126677999815 ) ) ;
#19285 = CARTESIAN_POINT ( 'NONE',  ( 12.17501771842803571, 2.156544773268126658, 13.83291087807201869 ) ) ;
#19286 = CARTESIAN_POINT ( 'NONE',  ( 9.409421956854998825, -2.113407700033000047, 7.914197133433000353 ) ) ;
#19287 = ORIENTED_EDGE ( 'NONE', *, *, #35371, .T. ) ;
#19288 = CARTESIAN_POINT ( 'NONE',  ( 12.27345231320720842, -0.3288522286823944429, -12.69427358703204156 ) ) ;
#19289 = CARTESIAN_POINT ( 'NONE',  ( 12.61757770595761663, -0.7057854747025462672, 13.98219993205038669 ) ) ;
#19290 = ORIENTED_EDGE ( 'NONE', *, *, #46095, .T. ) ;
#19291 = CARTESIAN_POINT ( 'NONE',  ( 25.30000327618300204, 2.078227429405999693, -11.31065739696999906 ) ) ;
#19292 = DIRECTION ( 'NONE',  ( 1.000000000000000000, 0.000000000000000000, 0.000000000000000000 ) ) ;
#19293 = CARTESIAN_POINT ( 'NONE',  ( 16.09992084546400193, 8.991497430826001391, 8.719551690569000257 ) ) ;
#19294 = CARTESIAN_POINT ( 'NONE',  ( 8.489029163847876092, 3.089100507813340446, 6.099830711550906059 ) ) ;
#19295 = AXIS2_PLACEMENT_3D ( 'NONE', #28223, #32780, #27531 ) ;
#19296 = CARTESIAN_POINT ( 'NONE',  ( 8.865073590557452476, 2.650142864597553327, -7.500004675916596142 ) ) ;
#19297 = CARTESIAN_POINT ( 'NONE',  ( 25.59997384872700010, 11.07537887597999848, -3.096069522331000190 ) ) ;
#19298 = CARTESIAN_POINT ( 'NONE',  ( 11.23627509987185746, 3.727547057523675988, 8.749999999999998224 ) ) ;
#19299 = CARTESIAN_POINT ( 'NONE',  ( 12.56425374667830397, 3.158898859712412577, 12.19759658245784628 ) ) ;
#19300 = CARTESIAN_POINT ( 'NONE',  ( 9.350728814717999882, -3.197530835772000035, -8.817973615970998935 ) ) ;
#19301 = CARTESIAN_POINT ( 'NONE',  ( 10.45672469555900008, 4.433465011431599656, -6.750062220519700062 ) ) ;
#19302 = CARTESIAN_POINT ( 'NONE',  ( 18.05828223140162692, 3.296090368282508454, 11.87625427050432236 ) ) ;
#19303 = CARTESIAN_POINT ( 'NONE',  ( 10.61257802013489737, 3.108115747127599970, -7.479237407015119743 ) ) ;
#19304 = CARTESIAN_POINT ( 'NONE',  ( 8.974088727410999056, 2.862182806015999947, -7.595427884080399927 ) ) ;
#19306 = CARTESIAN_POINT ( 'NONE',  ( 12.21857308197417957, 2.283092344276015595, 12.49946922046772357 ) ) ;
#19305 = CARTESIAN_POINT ( 'NONE',  ( 7.766851002543999627, 2.832432432432000269, 6.822293592207000934 ) ) ;
#19307 = DIRECTION ( 'NONE',  ( -1.000000000000000000, 0.000000000000000000, 0.000000000000000000 ) ) ;
#19308 = ORIENTED_EDGE ( 'NONE', *, *, #55091, .T. ) ;
#19309 = CARTESIAN_POINT ( 'NONE',  ( 10.69568717260499824, 3.533932086969799879, 6.739296831621899742 ) ) ;
#19310 = CARTESIAN_POINT ( 'NONE',  ( 10.49785673611999925, -3.776281940467000275, 5.717636230565000588 ) ) ;
#19311 = EDGE_CURVE ( 'NONE', #29486, #53731, #36002, .T. ) ;
#19312 = CARTESIAN_POINT ( 'NONE',  ( 9.353076168957999315, 3.420574098817999786, 6.516130052788599691 ) ) ;
#19313 = CARTESIAN_POINT ( 'NONE',  ( 8.872292071306626227, 4.874163933583397501, -7.462990653670714458 ) ) ;
#19314 = DIRECTION ( 'NONE',  ( -0.7071067811865975328, -0.7071067811864976127, 3.640777668006986975E-09 ) ) ;
#19315 = CARTESIAN_POINT ( 'NONE',  ( 23.66004879239100234, 9.998911746292000302, 9.691526727427998367 ) ) ;
#19316 = CARTESIAN_POINT ( 'NONE',  ( 9.520528907821001141, -2.899999999999999911, 6.152188490330000370 ) ) ;
#19317 = VERTEX_POINT ( 'NONE', #41935 ) ;
#19318 = B_SPLINE_CURVE_WITH_KNOTS ( 'NONE', 3,
 ( #8881, #30216, #63023, #62018 ),
 .UNSPECIFIED., .F., .F.,
 ( 4, 4 ),
 ( 0.000000000000000000, 0.1254192006116268687 ),
 .UNSPECIFIED. ) ;
#19319 = CARTESIAN_POINT ( 'NONE',  ( 9.860608878791998322, -4.258572737033900601, -6.387851364408000165 ) ) ;
#19320 = AXIS2_PLACEMENT_3D ( 'NONE', #68136, #14335, #69173 ) ;
#19321 = CARTESIAN_POINT ( 'NONE',  ( 10.45541918308390628, -4.873971636396174034, -4.983734050914551794 ) ) ;
#19322 = CARTESIAN_POINT ( 'NONE',  ( 12.02677869730533011, -4.403502086956500250, 8.295667533166499297 ) ) ;
#19323 = PRODUCT_DEFINITION_SHAPE ( 'NONE', 'NONE',  #44514 ) ;
#19324 = CARTESIAN_POINT ( 'NONE',  ( 17.55505043854143565, 3.125000000000000000, -12.28374638332999602 ) ) ;
#19325 = CARTESIAN_POINT ( 'NONE',  ( 8.973021312994999832, -2.881074422252000389, -6.370633220842000455 ) ) ;
#19326 = CARTESIAN_POINT ( 'NONE',  ( 21.72233714749290101, 6.000000000000000000, -1.351488365663999764E-13 ) ) ;
#19327 = CARTESIAN_POINT ( 'NONE',  ( 12.19673284866991914, 2.643529255688002788, -13.64196713149527618 ) ) ;
#19328 = CARTESIAN_POINT ( 'NONE',  ( 9.304144223516997769, -2.772050158355999994, -8.125211791007998841 ) ) ;
#19329 = CARTESIAN_POINT ( 'NONE',  ( 25.20343682218700110, 11.20004844819000134, 3.404174865946999695 ) ) ;
#19330 = VERTEX_POINT ( 'NONE', #4516 ) ;
#19331 = CARTESIAN_POINT ( 'NONE',  ( 8.924662153698962541, -5.350575487761723537, 7.500021879703682615 ) ) ;
#19332 = CARTESIAN_POINT ( 'NONE',  ( 12.09634358953518962, 0.1544074001204018831, -13.99915345895492003 ) ) ;
#19333 = CARTESIAN_POINT ( 'NONE',  ( 23.66004879239100234, 13.39256428908000096, 3.813547978107000080 ) ) ;
#19334 = EDGE_CURVE ( 'NONE', #37994, #62306, #46295, .T. ) ;
#19335 = CARTESIAN_POINT ( 'NONE',  ( 18.18005043875544047, -2.480307847467646543, -13.67758270278766020 ) ) ;
#19336 = EDGE_CURVE ( 'NONE', #1910, #40655, #58787, .T. ) ;
#19337 = CARTESIAN_POINT ( 'NONE',  ( 18.17512443068752148, 2.418970859032363308, 12.47009038073128551 ) ) ;
#19338 = CARTESIAN_POINT ( 'NONE',  ( 8.175739158770999992, 4.686731264770999772, -8.717075579553000608 ) ) ;
#19340 = VECTOR ( 'NONE', #25102, 1000.000000000000000 ) ;
#19339 = CARTESIAN_POINT ( 'NONE',  ( 9.050000000000000711, -7.679126935408000065, -5.093340497782000043 ) ) ;
#19341 = ORIENTED_EDGE ( 'NONE', *, *, #5695, .F. ) ;
#19342 = EDGE_CURVE ( 'NONE', #28175, #38133, #47902, .T. ) ;
#19343 = CARTESIAN_POINT ( 'NONE',  ( 8.591232269961309953, -3.293719616469516165, 8.705632950218230803 ) ) ;
#19344 = CARTESIAN_POINT ( 'NONE',  ( 18.10946311474933523, 2.988545908040622034, -13.67730534870324455 ) ) ;
#19345 = ORIENTED_EDGE ( 'NONE', *, *, #62774, .F. ) ;
#19346 = CARTESIAN_POINT ( 'NONE',  ( 10.41529229006299850, -3.250213325543700016, 7.935348007132199122 ) ) ;
#19347 = DIRECTION ( 'NONE',  ( 0.000000000000000000, -0.7614089499631907509, -0.6482718649732928107 ) ) ;
#19349 = CARTESIAN_POINT ( 'NONE',  ( 9.111654719595000174, 4.989193221215000307, -6.287302145481000082 ) ) ;
#19348 = VECTOR ( 'NONE', #50777, 1000.000000000000114 ) ;
#19350 = CARTESIAN_POINT ( 'NONE',  ( 18.23980063401623752, 2.972525811573667465, -11.47315805793748567 ) ) ;
#19351 = CARTESIAN_POINT ( 'NONE',  ( 10.73213259636989925, -4.907524392912299582, -7.994504989494399361 ) ) ;
#19352 = B_SPLINE_CURVE_WITH_KNOTS ( 'NONE', 3,
 ( #30308, #30996, #15932, #5780, #58584, #200 ),
 .UNSPECIFIED., .F., .F.,
 ( 4, 2, 4 ),
 ( 0.000000000000000000, 0.5000000000000000000, 1.000000000000000000 ),
 .UNSPECIFIED. ) ;
#19353 = CARTESIAN_POINT ( 'NONE',  ( 11.09999999999999964, -2.700688486617000006, 5.124965750789000296 ) ) ;
#19354 = FACE_OUTER_BOUND ( 'NONE', #29944, .T. ) ;
#19355 = EDGE_LOOP ( 'NONE', ( #3907, #26001, #5812, #62593 ) ) ;
#19356 = CARTESIAN_POINT ( 'NONE',  ( 7.809591065053155923, 2.953469884859488470, -8.377395465226323168 ) ) ;
#19357 = CARTESIAN_POINT ( 'NONE',  ( 17.55505043854147118, -3.125000000000000000, -13.52078605991414761 ) ) ;
#19358 = CARTESIAN_POINT ( 'NONE',  ( 9.784179719593000257, 4.042991257420999851, -5.768106221333000327 ) ) ;
#19359 = ORIENTED_EDGE ( 'NONE', *, *, #20910, .F. ) ;
#19360 = CARTESIAN_POINT ( 'NONE',  ( 10.23643409129999959, 5.517148499152000340, -6.754126239302999934 ) ) ;
#19361 = PRESENTATION_STYLE_ASSIGNMENT (( #23234 ) ) ;
#19362 = EDGE_LOOP ( 'NONE', ( #11122, #39121, #32429, #63780, #68616, #63906, #46292 ) ) ;
#19363 = CARTESIAN_POINT ( 'NONE',  ( 9.100734463322998735, 4.118936914955599882, 6.364399516445999438 ) ) ;
#19364 = CARTESIAN_POINT ( 'NONE',  ( 17.93835418254527880, -2.006228213506225710, -12.55298903047910208 ) ) ;
#19365 = EDGE_CURVE ( 'NONE', #63876, #8401, #30240, .T. ) ;
#19366 = CARTESIAN_POINT ( 'NONE',  ( 12.99999999998900080, 12.39025855408000076, 1.832244667012999928 ) ) ;
#19367 = CARTESIAN_POINT ( 'NONE',  ( 24.62773497368900166, -12.19918623920000122, -3.045383383698999857 ) ) ;
#19368 = CARTESIAN_POINT ( 'NONE',  ( 9.483644241562705801, -2.404105139695982718, 6.777660126136261454 ) ) ;
#19369 = ORIENTED_EDGE ( 'NONE', *, *, #58059, .F. ) ;
#19370 = CARTESIAN_POINT ( 'NONE',  ( -17.56123417799999942, -13.94845324556000143, -4.312847325879000770 ) ) ;
#19371 = AXIS2_PLACEMENT_3D ( 'NONE', #17102, #11509, #12216 ) ;
#19372 = CARTESIAN_POINT ( 'NONE',  ( 10.57657334123000048, 5.344886503256999433, -7.298885378918000377 ) ) ;
#19373 = CARTESIAN_POINT ( 'NONE',  ( 11.13520290286999881, -5.334297965861999558, -5.182437713717999550 ) ) ;
#19374 = CARTESIAN_POINT ( 'NONE',  ( 12.17076609166787193, 2.871707895891075335, -13.70231394784453727 ) ) ;
#19375 = CIRCLE ( 'NONE', #17122, 1.449999999999999956 ) ;
#19376 = CARTESIAN_POINT ( 'NONE',  ( 9.025809814041000578, -3.217492037304399588, -8.511961036725999463 ) ) ;
#19377 = CARTESIAN_POINT ( 'NONE',  ( 17.77667453761835503, 0.6953657024348723903, 13.98272072176121661 ) ) ;
#19378 = CARTESIAN_POINT ( 'NONE',  ( 17.79607173997655423, 11.53879313267151119, -4.871540518365785388 ) ) ;
#19379 = DIRECTION ( 'NONE',  ( 0.000000000000000000, 1.000000000000000000, 0.000000000000000000 ) ) ;
#19380 = ORIENTED_EDGE ( 'NONE', *, *, #2401, .F. ) ;
#19381 = ORIENTED_EDGE ( 'NONE', *, *, #59446, .T. ) ;
#19382 = CARTESIAN_POINT ( 'NONE',  ( 10.02394528041000044, 5.481267232667000222, -8.005061172455999241 ) ) ;
#19383 = CARTESIAN_POINT ( 'NONE',  ( 7.100083736560635295, 0.3076767997638333307, 3.048821334907659608 ) ) ;
#19384 = CARTESIAN_POINT ( 'NONE',  ( 12.23350478621572357, -2.246345293463438697, 13.72400836782633959 ) ) ;
#19385 = CARTESIAN_POINT ( 'NONE',  ( 24.16198533718584684, 3.322437203991291277, 12.45250991497782778 ) ) ;
#19386 = CARTESIAN_POINT ( 'NONE',  ( 23.74057427653900021, 9.838736938141998678, -9.517768723660999797 ) ) ;
#19387 = CARTESIAN_POINT ( 'NONE',  ( 16.26904166988085620, -3.216266637185321020, -11.40336119490550004 ) ) ;
#19389 = CARTESIAN_POINT ( 'NONE',  ( 9.004177925655991288, 2.621319625803172126, 6.376254879885641103 ) ) ;
#19388 = CARTESIAN_POINT ( 'NONE',  ( 9.929063610504998749, -3.531653260805799999, 6.458661544034999480 ) ) ;
#19390 = VECTOR ( 'NONE', #20225, 1000.000000000000114 ) ;
#19391 = CARTESIAN_POINT ( 'NONE',  ( 8.599275817281997192, -4.816070832762001430, -6.340446949048005543 ) ) ;
#19392 = EDGE_LOOP ( 'NONE', ( #33100, #48931, #49813, #13741 ) ) ;
#19393 = DIRECTION ( 'NONE',  ( -0.8660254037844288266, 0.000000000000000000, 0.5000000000000169864 ) ) ;
#19394 = VECTOR ( 'NONE', #49291, 1000.000000000000000 ) ;
#19395 = LINE ( 'NONE', #18717, #26240 ) ;
#19396 = EDGE_CURVE ( 'NONE', #22430, #32483, #38405, .T. ) ;
#19397 = EDGE_CURVE ( 'NONE', #9159, #23524, #7905, .T. ) ;
#19398 = CARTESIAN_POINT ( 'NONE',  ( 9.311718600414000235, -4.588307032459999490, -5.987050435448999508 ) ) ;
#19399 = CARTESIAN_POINT ( 'NONE',  ( 7.954101906406737754, 4.935753437653367826, 6.415772546196833126 ) ) ;
#19400 = CARTESIAN_POINT ( 'NONE',  ( 5.000030787343000327, 2.099962892530999881, 0.000000000000000000 ) ) ;
#19401 = LINE ( 'NONE', #35492, #39711 ) ;
#19402 = CARTESIAN_POINT ( 'NONE',  ( 8.414360841228999632, 5.461114003844000031, -8.582501063019000398 ) ) ;
#19403 = B_SPLINE_CURVE_WITH_KNOTS ( 'NONE', 3,
 ( #31736, #57599, #25795, #47125, #68426, #20549, #41873, #31391, #42229, #63536, #26489, #15647, #53055, #47819, #69127, #27873, #64558, #48846, #44308, #17371, #6530, #32766, #603, #49183 ),
 .UNSPECIFIED., .F., .F.,
 ( 4, 2, 1, 2, 2, 2, 2, 2, 2, 1, 2, 2, 4 ),
 ( 0.000000000000000000, 0.06250000000000012490, 0.1250000000000002498, 0.1875000000000003886, 0.2500000000000004996, 0.3750000000000006661, 0.5000000000000008882, 0.6250000000000008882, 0.6875000000000006661, 0.7500000000000005551, 0.8125000000000005551, 0.8750000000000004441, 1.000000000000000000 ),
 .UNSPECIFIED. ) ;
#19404 = B_SPLINE_CURVE_WITH_KNOTS ( 'NONE', 3,
 ( #48306, #413, #11242, #22073 ),
 .UNSPECIFIED., .F., .F.,
 ( 4, 4 ),
 ( 0.000000000000000000, 1.000000000000000000 ),
 .UNSPECIFIED. ) ;
#19405 = FACE_OUTER_BOUND ( 'NONE', #62405, .T. ) ;
#19406 = DIRECTION ( 'NONE',  ( -0.7071074674731144816, -0.7071060948993143080, 1.718725578913035619E-08 ) ) ;
#19407 = CARTESIAN_POINT ( 'NONE',  ( 0.2879790830606807628, 0.4312571902316706951, 3.287958384590494276 ) ) ;
#19408 = CARTESIAN_POINT ( 'NONE',  ( 2.251972330171000181, 2.697882917481999598, -1.828095362927000034 ) ) ;
#19409 = ORIENTED_EDGE ( 'NONE', *, *, #19007, .T. ) ;
#19410 = CARTESIAN_POINT ( 'NONE',  ( 12.70318068537856249, -0.6169782284476057477, -12.67981870385671428 ) ) ;
#19412 = CARTESIAN_POINT ( 'NONE',  ( 12.21071179156234976, -2.693740719230159009, -12.40432020969549853 ) ) ;
#19411 = B_SPLINE_CURVE_WITH_KNOTS ( 'NONE', 3,
 ( #25974, #41021, #45923, #67577, #3271, #25285, #31231, #35440, #46619, #51506 ),
 .UNSPECIFIED., .F., .F.,
 ( 4, 1, 1, 1, 1, 1, 1, 4 ),
 ( 0.000000000000000000, 0.06214647846548406601, 0.2363167115191955048, 0.4104869445722291177, 0.5846571776259398279, 0.7588274106789726359, 0.9329976437320062210, 1.000000000000000000 ),
 .UNSPECIFIED. ) ;
#19413 = CARTESIAN_POINT ( 'NONE',  ( 13.69992376746900042, 12.26631831379999937, 2.532779022035999805 ) ) ;
#19414 = CARTESIAN_POINT ( 'NONE',  ( 7.999926658772999133, 5.198556077301000222, 8.332552905512999430 ) ) ;
#19415 = CARTESIAN_POINT ( 'NONE',  ( 9.674373738639999942, -2.899999999999999911, -6.185493860157000867 ) ) ;
#19416 = ORIENTED_EDGE ( 'NONE', *, *, #38432, .T. ) ;
#19417 = CARTESIAN_POINT ( 'NONE',  ( 5.269604931988000729, 0.1309856596131999951, 1.229810997071999923 ) ) ;
#19418 = APPLICATION_PROTOCOL_DEFINITION ( 'draft international standard', 'automotive_design', 1998, #305 ) ;
#19419 = CARTESIAN_POINT ( 'NONE',  ( 10.99020523659462079, 7.555164107387456696, 6.307848186994561956 ) ) ;
#19420 = LINE ( 'NONE', #47374, #41046 ) ;
#19421 = CARTESIAN_POINT ( 'NONE',  ( 1.740556799206375294, -3.500000000000003109, 0.4581489286484972667 ) ) ;
#19422 = CARTESIAN_POINT ( 'NONE',  ( 10.73213259636989925, 3.092475607087700418, -7.994504989494399361 ) ) ;
#19423 = ORIENTED_EDGE ( 'NONE', *, *, #18233, .T. ) ;
#19424 = AXIS2_PLACEMENT_3D ( 'NONE', #52306, #36230, #67008 ) ;
#19425 = EDGE_CURVE ( 'NONE', #26212, #36211, #29594, .T. ) ;
#19426 = CARTESIAN_POINT ( 'NONE',  ( 10.48164908029000131, -4.022873587130999518, 9.090901241422999490 ) ) ;
#19427 = ORIENTED_EDGE ( 'NONE', *, *, #53660, .T. ) ;
#19428 = DIRECTION ( 'NONE',  ( 0.000000000000000000, 0.7071067811864980568, -0.7071067811865969777 ) ) ;
#19429 = CARTESIAN_POINT ( 'NONE',  ( 7.764230646791999924, -4.628942671846000501, 5.991663889842000046 ) ) ;
#19430 = CARTESIAN_POINT ( 'NONE',  ( 18.03351914841130466, 0.5491314443420087787, -13.98923457196397635 ) ) ;
#19431 = ORIENTED_EDGE ( 'NONE', *, *, #31349, .T. ) ;
#19432 = CARTESIAN_POINT ( 'NONE',  ( 10.08521345716899908, 4.924890298941200228, -8.340879262988799780 ) ) ;
#19433 = CARTESIAN_POINT ( 'NONE',  ( 3.400000000000000355, 1.000000000000000000, 0.000000000000000000 ) ) ;
#19434 = CARTESIAN_POINT ( 'NONE',  ( 8.351820280410001018, 4.901484321470999994, -8.891682961388999829 ) ) ;
#19435 = CARTESIAN_POINT ( 'NONE',  ( 9.674960421382234443, 2.650268802166420024, 7.499999178247376719 ) ) ;
#19436 = CARTESIAN_POINT ( 'NONE',  ( 10.18823468625795492, -2.651251756636299195, 7.275528047993060632 ) ) ;
#19437 = ORIENTED_EDGE ( 'NONE', *, *, #35446, .F. ) ;
#19438 = CARTESIAN_POINT ( 'NONE',  ( 11.14698053895999941, -5.129799765052999838, 5.886044098803999702 ) ) ;
#19439 = CARTESIAN_POINT ( 'NONE',  ( 12.18403211232070582, -2.428839562839110400, -13.68824371557135677 ) ) ;
#19440 = DIRECTION ( 'NONE',  ( 0.000000000000000000, 1.000000000000000000, 0.000000000000000000 ) ) ;
#19441 = CARTESIAN_POINT ( 'NONE',  ( 10.13382174003999836, -5.176455793257000337, -8.189804425074999727 ) ) ;
#19442 = B_SPLINE_CURVE_WITH_KNOTS ( 'NONE', 3,
 ( #53014, #4417, #9662, #213 ),
 .UNSPECIFIED., .F., .F.,
 ( 4, 4 ),
 ( 0.000000000000000000, 1.000000000000000000 ),
 .UNSPECIFIED. ) ;
#19443 = DIRECTION ( 'NONE',  ( 0.000000000000000000, -0.9565994702956990281, -0.2914059941558995726 ) ) ;
#19444 = ORIENTED_EDGE ( 'NONE', *, *, #23459, .T. ) ;
#19445 = CARTESIAN_POINT ( 'NONE',  ( 17.82923902985817222, 0.5617296175207505682, -13.88472048964184147 ) ) ;
#19446 = EDGE_CURVE ( 'NONE', #9641, #36464, #64598, .T. ) ;
#19447 = AXIS2_PLACEMENT_3D ( 'NONE', #2920, #17638, #65510 ) ;
#19448 = DIRECTION ( 'NONE',  ( -1.000000000000000000, 0.000000000000000000, 0.000000000000000000 ) ) ;
#19449 = CARTESIAN_POINT ( 'NONE',  ( 24.96657550120661995, 2.078227398812693139, 11.31065740259266406 ) ) ;
#19450 = CARTESIAN_POINT ( 'NONE',  ( 3.167640132544333742, -1.762666431298160141, 3.058252359239895579 ) ) ;
#19451 = VECTOR ( 'NONE', #35760, 1000.000000000000114 ) ;
#19452 = CARTESIAN_POINT ( 'NONE',  ( 12.18407604397246580, 0.07155107330948899669, -13.89975717292030311 ) ) ;
#19453 = CARTESIAN_POINT ( 'NONE',  ( 18.14163091156143892, -2.284010751868935429, 12.49929939428934311 ) ) ;
#19454 = ORIENTED_EDGE ( 'NONE', *, *, #35909, .T. ) ;
#19455 = CARTESIAN_POINT ( 'NONE',  ( 11.60477869730532774, -4.467447516829900600, -6.578238193496799724 ) ) ;
#19456 = B_SPLINE_CURVE_WITH_KNOTS ( 'NONE', 3,
 ( #17725, #55817, #29608, #39386 ),
 .UNSPECIFIED., .F., .F.,
 ( 4, 4 ),
 ( 0.000000000000000000, 1.000000000000000000 ),
 .UNSPECIFIED. ) ;
#19457 = ORIENTED_EDGE ( 'NONE', *, *, #12169, .T. ) ;
#19458 = CARTESIAN_POINT ( 'NONE',  ( 10.76010575649000067, 4.535386075958999896, 6.001721352166000223 ) ) ;
#19459 = DIRECTION ( 'NONE',  ( 0.000000000000000000, -0.9916377111174247139, 0.1290528957048031888 ) ) ;
#19460 = CARTESIAN_POINT ( 'NONE',  ( 9.137754719594999742, 2.319062457810000311, -7.919229449146000022 ) ) ;
#19461 = CARTESIAN_POINT ( 'NONE',  ( 2.551832320967999834, 0.3084989455321000551, 3.530262701594000241 ) ) ;
#19462 = B_SPLINE_CURVE_WITH_KNOTS ( 'NONE', 3,
 ( #39678, #12766, #2271, #6816, #28505, #60310, #12417, #44931, #6470, #49122, #23589, #65543, #65192, #27817, #54717, #23939, #34093, #28861 ),
 .UNSPECIFIED., .F., .F.,
 ( 4, 2, 2, 2, 2, 2, 2, 2, 4 ),
 ( 0.000000000000000000, 0.1250000000000003331, 0.2500000000000006661, 0.3750000000000009992, 0.5000000000000013323, 0.6250000000000009992, 0.7500000000000006661, 0.8750000000000003331, 1.000000000000000000 ),
 .UNSPECIFIED. ) ;
#19463 = CARTESIAN_POINT ( 'NONE',  ( 9.934206403597999113, -5.120430559539999926, -8.883390070891001855 ) ) ;
#19464 = FACE_OUTER_BOUND ( 'NONE', #41866, .T. ) ;
#19465 = CARTESIAN_POINT ( 'NONE',  ( 8.983363606030074777, -5.350321127414493283, 7.640157910728230028 ) ) ;
#19466 = ORIENTED_EDGE ( 'NONE', *, *, #67374, .T. ) ;
#19467 = CARTESIAN_POINT ( 'NONE',  ( 11.07149279008999976, -4.296686446741600385, 6.398515879103999993 ) ) ;
#19468 = CARTESIAN_POINT ( 'NONE',  ( 11.45284386393252696, -3.097320422761385750, -7.175013233162909287 ) ) ;
#19469 = CARTESIAN_POINT ( 'NONE',  ( 15.61722669115800066, 9.375864875015000877, 8.222239459497000524 ) ) ;
#19470 = DIRECTION ( 'NONE',  ( 1.000000000000000000, 0.000000000000000000, -0.000000000000000000 ) ) ;
#19472 = DIRECTION ( 'NONE',  ( -0.000000000000000000, -0.000000000000000000, 1.000000000000000000 ) ) ;
#19471 = CARTESIAN_POINT ( 'NONE',  ( 9.352253013669001191, 2.817757427878999632, 6.388459691516000127 ) ) ;
#19473 = CIRCLE ( 'NONE', #17226, 11.30000000000000604 ) ;
#19474 = CARTESIAN_POINT ( 'NONE',  ( 10.55103166480599874, 2.999015536536000504, -7.570575893572789816 ) ) ;
#19475 = CARTESIAN_POINT ( 'NONE',  ( 24.46225942633000017, -11.93531508627000015, 3.254110267536999945 ) ) ;
#19476 = CARTESIAN_POINT ( 'NONE',  ( 9.427051052051998781, 4.985712601322500603, -7.692906630067099627 ) ) ;
#19477 = EDGE_CURVE ( 'NONE', #20897, #52805, #2097, .T. ) ;
#19479 = EDGE_CURVE ( 'NONE', #63599, #63126, #40270, .T. ) ;
#19478 = B_SPLINE_CURVE_WITH_KNOTS ( 'NONE', 3,
 ( #15555, #27419, #64116, #21474 ),
 .UNSPECIFIED., .F., .F.,
 ( 4, 4 ),
 ( 0.000000000000000000, 1.000000000000000000 ),
 .UNSPECIFIED. ) ;
#19480 = CARTESIAN_POINT ( 'NONE',  ( 18.21574167892469731, 0.2964030593063826657, 12.59651778044212200 ) ) ;
#19481 = DIRECTION ( 'NONE',  ( 1.000000000000000000, 0.000000000000000000, 0.000000000000000000 ) ) ;
#19482 = CARTESIAN_POINT ( 'NONE',  ( 10.72191429142990060, 4.025072603369280522, 8.816028813488999916 ) ) ;
#19483 = CARTESIAN_POINT ( 'NONE',  ( 0.2309807866890836170, 0.4165353540672909194, -3.230960454924427072 ) ) ;
#19484 = VERTEX_POINT ( 'NONE', #23013 ) ;
#19485 = CARTESIAN_POINT ( 'NONE',  ( 8.026331853209001110, -5.601799093797000140, 7.176147756900999930 ) ) ;
#19486 = EDGE_CURVE ( 'NONE', #36624, #45349, #9008, .T. ) ;
#19487 = EDGE_CURVE ( 'NONE', #54794, #26237, #27102, .T. ) ;
#19488 = CARTESIAN_POINT ( 'NONE',  ( 17.88835954937806605, 3.166508787604171982, 13.63720117115729558 ) ) ;
#19489 = CARTESIAN_POINT ( 'NONE',  ( 6.921938604046592225, -0.09431034973223660633, 1.509148051328639051 ) ) ;
#19490 = CARTESIAN_POINT ( 'NONE',  ( 10.17349413291699811, -2.837298848764000514, -6.969488574374499201 ) ) ;
#19491 = ORIENTED_EDGE ( 'NONE', *, *, #5823, .F. ) ;
#19492 = VECTOR ( 'NONE', #20721, 999.9999999999998863 ) ;
#19493 = CARTESIAN_POINT ( 'NONE',  ( 17.86531638133300248, 3.412592442238999713, 11.89775222658999887 ) ) ;
#19494 = VECTOR ( 'NONE', #34409, 1000.000000000000000 ) ;
#19496 = CARTESIAN_POINT ( 'NONE',  ( 11.02301463001509774, 4.547357026650399980, 8.376661845795100092 ) ) ;
#19495 = CARTESIAN_POINT ( 'NONE',  ( 9.636671671056999955, -4.855035690642299784, -7.643603315539799326 ) ) ;
#19497 = CARTESIAN_POINT ( 'NONE',  ( 10.01676721958999927, 4.324998751150999965, -9.154078823942999321 ) ) ;
#19498 = ORIENTED_EDGE ( 'NONE', *, *, #13415, .T. ) ;
#19499 = CARTESIAN_POINT ( 'NONE',  ( 1.353056799207333460, -2.798833948393629534, -2.150913519912204031 ) ) ;
#19500 = CARTESIAN_POINT ( 'NONE',  ( 17.85637496866994312, -3.182194879603819970, -13.63354919460145886 ) ) ;
#19501 = CARTESIAN_POINT ( 'NONE',  ( 11.01041369783139956, 3.935522326596939902, 6.223614866029000048 ) ) ;
#19502 = CARTESIAN_POINT ( 'NONE',  ( 11.02445830383999947, -3.404091099119999519, 5.822494319281999786 ) ) ;
#19503 = DIRECTION ( 'NONE',  ( 0.000000000000000000, 1.000000000000000000, 0.000000000000000000 ) ) ;
#19504 = ORIENTED_EDGE ( 'NONE', *, *, #31067, .T. ) ;
#19505 = FACE_OUTER_BOUND ( 'NONE', #24646, .T. ) ;
#19506 = CARTESIAN_POINT ( 'NONE',  ( 18.18005043824477696, 1.062919176435095297E-10, -13.90000000153291637 ) ) ;
#19507 = CARTESIAN_POINT ( 'NONE',  ( 8.237169251180624485, -5.550135988664304243, 8.289372690488722384 ) ) ;
#19508 = CARTESIAN_POINT ( 'NONE',  ( 11.13746005378019888, -2.838900981960999825, -6.879992063401499713 ) ) ;
#19509 = CARTESIAN_POINT ( 'NONE',  ( 9.372772138682000431, -4.424886761933599644, 8.559813987224998755 ) ) ;
#19510 = ORIENTED_EDGE ( 'NONE', *, *, #39965, .F. ) ;
#19511 = CARTESIAN_POINT ( 'NONE',  ( 10.75904878004999965, -5.211536764922000131, -4.904134446986000206 ) ) ;
#19512 = CARTESIAN_POINT ( 'NONE',  ( 10.87041638348499895, -5.241705141469999774, 7.802464414828100381 ) ) ;
#19513 = ORIENTED_EDGE ( 'NONE', *, *, #48866, .T. ) ;
#19514 = CARTESIAN_POINT ( 'NONE',  ( 16.09997386696500143, -5.375854662731797795, -10.37779375783402358 ) ) ;
#19515 = EDGE_LOOP ( 'NONE', ( #37981, #29948, #47193, #37334, #27242, #49896, #58719, #38044, #5910, #49344 ) ) ;
#19516 = CARTESIAN_POINT ( 'NONE',  ( 9.705151033051999221, -4.316974633926000671, -5.653758079558000027 ) ) ;
#19517 = CARTESIAN_POINT ( 'NONE',  ( 10.32322131181000024, -3.346607553924000111, -4.621083566737000048 ) ) ;
#19518 = CARTESIAN_POINT ( 'NONE',  ( 11.22056920625029974, 4.047312782235129802, -6.184582852561999466 ) ) ;
#19519 = CARTESIAN_POINT ( 'NONE',  ( 11.30502344389999969, -5.125258734743999511, 8.182900850620900002 ) ) ;
#19520 = CARTESIAN_POINT ( 'NONE',  ( 12.26933621011913722, 2.178034692540639750, -12.52080028461861616 ) ) ;
#19521 = CARTESIAN_POINT ( 'NONE',  ( 11.48995257254740032, -5.095356924909000718, 7.181435527216799564 ) ) ;
#19522 = CARTESIAN_POINT ( 'NONE',  ( 7.667607780408999929, 5.638704226117999596, 8.266404648244000342 ) ) ;
#19523 = ORIENTED_EDGE ( 'NONE', *, *, #64292, .T. ) ;
#19524 = CARTESIAN_POINT ( 'NONE',  ( 7.487876381280277549, 5.349293767872230099, 7.706633529874828525 ) ) ;
#19525 = CIRCLE ( 'NONE', #63018, 13.17499999999999716 ) ;
#19526 = CARTESIAN_POINT ( 'NONE',  ( 7.892605646791999163, -5.480312458445999901, 8.192326492433998908 ) ) ;
#19527 = DIRECTION ( 'NONE',  ( -1.000000000000000000, 0.000000000000000000, 1.665334536957000056E-14 ) ) ;
#19528 = ORIENTED_EDGE ( 'NONE', *, *, #24080, .T. ) ;
#19529 = B_SPLINE_SURFACE_WITH_KNOTS ( 'NONE', 3, 3, ( 
 ( #7411, #44149, #34347, #60215 ),
 ( #50072, #49720, #18259, #33303 ),
 ( #1138, #56947, #24789, #65446 ),
 ( #17916, #12320, #65790, #55665 ),
 ( #33996, #6718, #65088, #39233 ),
 ( #7067, #1830, #13019, #28057 ),
 ( #28760, #51358, #17567, #60559 ),
 ( #38894, #59861, #12664, #11967 ),
 ( #44835, #44497, #22450, #55313 ),
 ( #3451, #2179, #67421, #7763 ),
 ( #23494, #30056, #46114, #19545 ) ),
 .UNSPECIFIED., .F., .F., .F.,
 ( 4, 1, 1, 1, 1, 1, 1, 1, 4 ),
 ( 4, 4 ),
 ( 0.5752755569481000641, 0.6250000000000000000, 0.6875000000000000000, 0.7500000000000000000, 0.8125000000000000000, 0.8750000000000000000, 0.9375000000000000000, 1.000000000000000000, 1.016621166648999930 ),
 ( -0.1690624953889000026, 1.168925165984000092 ),
 .UNSPECIFIED. ) ;
#19530 = CARTESIAN_POINT ( 'NONE',  ( 12.63203184702130244, -3.100663238843660352, -12.29110965694881408 ) ) ;
#19531 = CARTESIAN_POINT ( 'NONE',  ( 10.12841772631199966, 4.490588993294299947, 6.490165927606000196 ) ) ;
#19532 = EDGE_CURVE ( 'NONE', #40405, #48911, #1694, .T. ) ;
#19533 = AXIS2_PLACEMENT_3D ( 'NONE', #47841, #10417, #52728 ) ;
#19534 = CARTESIAN_POINT ( 'NONE',  ( 10.48598064679000075, -5.506038521567000465, -7.274786670944999756 ) ) ;
#19535 = FACE_OUTER_BOUND ( 'NONE', #41981, .T. ) ;
#19536 = CARTESIAN_POINT ( 'NONE',  ( 17.90096402402700093, -11.91930970589999994, 3.312615672289999758 ) ) ;
#19537 = DIRECTION ( 'NONE',  ( -0.000000000000000000, -0.000000000000000000, 1.000000000000000000 ) ) ;
#19538 = CARTESIAN_POINT ( 'NONE',  ( 12.76358260308701986, -1.876037923228467186, -13.78611687077049197 ) ) ;
#19539 = ADVANCED_FACE ( 'NONE', ( #13915 ), #39166, .T. ) ;
#19540 = CARTESIAN_POINT ( 'NONE',  ( 11.24441369783139777, -4.043700988887960257, -8.365094684940499903 ) ) ;
#19541 = CARTESIAN_POINT ( 'NONE',  ( 10.46887750876899936, -4.692271380433699512, -8.574279626736998949 ) ) ;
#19542 = CARTESIAN_POINT ( 'NONE',  ( 8.600625070212519319, -4.994744277835623691, 6.120354035033368056 ) ) ;
#19543 = ORIENTED_EDGE ( 'NONE', *, *, #38747, .F. ) ;
#19544 = ORIENTED_EDGE ( 'NONE', *, *, #2442, .T. ) ;
#19545 = CARTESIAN_POINT ( 'NONE',  ( 10.26109516073000094, -4.557161966536000364, 4.532202352624000063 ) ) ;
#19546 =( NAMED_UNIT ( * ) PLANE_ANGLE_UNIT ( ) SI_UNIT ( $, .RADIAN. ) );
#19547 = CARTESIAN_POINT ( 'NONE',  ( 24.30000000000000071, 2.524919604596999712, -12.12772056298999956 ) ) ;
#19548 = CARTESIAN_POINT ( 'NONE',  ( 9.143927823787141307, 5.249988444743199700, -7.499999844943244121 ) ) ;
#19549 = CARTESIAN_POINT ( 'NONE',  ( 9.949437606643998677, 2.508497579857000392, -7.171862210735000076 ) ) ;
#19550 = CARTESIAN_POINT ( 'NONE',  ( 24.44496412535000118, -8.810486166165000910, -8.810507954003998776 ) ) ;
#19551 = AXIS2_PLACEMENT_3D ( 'NONE', #51812, #3910, #25244 ) ;
#19552 = DIRECTION ( 'NONE',  ( 0.000000000000000000, -0.7146936510866647163, -0.6994376205898656940 ) ) ;
#19553 = CARTESIAN_POINT ( 'NONE',  ( 23.54908302934800091, -13.36512341691999950, 4.295216725789000378 ) ) ;
#19554 = CARTESIAN_POINT ( 'NONE',  ( 10.90374609491999891, 3.726846467344000047, 5.900456154266000119 ) ) ;
#19555 = CARTESIAN_POINT ( 'NONE',  ( 9.251496707488000126, -3.918323994020610268, 6.643597378104299622 ) ) ;
#19556 = EDGE_LOOP ( 'NONE', ( #53445, #17636, #52623, #26476, #35881 ) ) ;
#19557 = CARTESIAN_POINT ( 'NONE',  ( 12.38992078601024005, -2.032669449810693862, 12.54828005421690840 ) ) ;
#19558 = CARTESIAN_POINT ( 'NONE',  ( 23.56695925801778557, -10.30432770669533404, -9.462935969010649373 ) ) ;
#19559 = CARTESIAN_POINT ( 'NONE',  ( 11.18484176840999922, 2.599663474744000169, 7.740674686800000259 ) ) ;
#19560 = CARTESIAN_POINT ( 'NONE',  ( 12.01656039236534923, -2.826501801118000312, 7.442888368925779652 ) ) ;
#19561 = CARTESIAN_POINT ( 'NONE',  ( 21.10000000000000142, -12.35000000006999876, 0.000000000000000000 ) ) ;
#19562 = CARTESIAN_POINT ( 'NONE',  ( 10.29657053952199952, 3.497746311184500190, -6.324815923923999605 ) ) ;
#19563 = CARTESIAN_POINT ( 'NONE',  ( 12.25868397512095243, 0.3036663359794751216, 12.69511825016612860 ) ) ;
#19564 = CARTESIAN_POINT ( 'NONE',  ( 9.085767219592000288, 2.821863697211000055, 6.127145479358000024 ) ) ;
#19565 = ADVANCED_FACE ( 'NONE', ( #59296 ), #44191, .F. ) ;
#19566 = CARTESIAN_POINT ( 'NONE',  ( 10.68403803949000164, 5.436614310638000269, 8.578436083822998270 ) ) ;
#19567 = CARTESIAN_POINT ( 'NONE',  ( 12.72194006826442347, 1.880463790526824441, 12.57452048663021849 ) ) ;
#19568 = EDGE_LOOP ( 'NONE', ( #21947, #17661, #19027, #18490, #39610, #28117 ) ) ;
#19569 = CARTESIAN_POINT ( 'NONE',  ( 9.725595280412999699, 2.495531372253999791, -7.930944806125000746 ) ) ;
#19570 = CARTESIAN_POINT ( 'NONE',  ( 12.80505043854143388, 1.875000000000000000, 13.78627172894481667 ) ) ;
#19571 = EDGE_CURVE ( 'NONE', #26471, #4832, #48765, .T. ) ;
#19572 = CIRCLE ( 'NONE', #68710, 0.6999999999999992895 ) ;
#19573 = EDGE_CURVE ( 'NONE', #7219, #27235, #32475, .T. ) ;
#19574 = CARTESIAN_POINT ( 'NONE',  ( 13.50000000000000178, 11.91410841793398312, 2.466613755757246285 ) ) ;
#19576 = CARTESIAN_POINT ( 'NONE',  ( 24.72675083956480435, 11.76478169716107480, 3.190859653314884081 ) ) ;
#19575 = CARTESIAN_POINT ( 'NONE',  ( 9.433105646793000787, -4.954907757874000396, 8.825780921426000347 ) ) ;
#19577 = CARTESIAN_POINT ( 'NONE',  ( 12.10000000000000142, -3.752125624359934353, 8.548800951397312886 ) ) ;
#19578 = CARTESIAN_POINT ( 'NONE',  ( 11.41256651104150066, -3.901000349726440053, -6.501426055769400136 ) ) ;
#19579 = ORIENTED_EDGE ( 'NONE', *, *, #47552, .F. ) ;
#19580 = CARTESIAN_POINT ( 'NONE',  ( 0.9780474580060999346, 3.010927365844000114, -1.992372462812000089 ) ) ;
#19581 = CARTESIAN_POINT ( 'NONE',  ( 18.02962380189445923, -0.4069377585276638398, -12.69123026938757981 ) ) ;
#19583 = CARTESIAN_POINT ( 'NONE',  ( 9.099999931440999390, 4.000000000000000000, -7.500000000000000000 ) ) ;
#19582 = DIRECTION ( 'NONE',  ( 0.7071067811865474617, 0.7071067811865474617, -2.638502694198172937E-09 ) ) ;
#19584 = CARTESIAN_POINT ( 'NONE',  ( 12.79999999202000005, -11.41069016990000051, 4.623987642516999230 ) ) ;
#19585 = CARTESIAN_POINT ( 'NONE',  ( 16.00000000900400110, -11.53038407186596892, 4.891407584292653432 ) ) ;
#19586 = CARTESIAN_POINT ( 'NONE',  ( 15.82968830470293398, 8.721231603648991637, 7.724200095969830038 ) ) ;
#19587 = DIRECTION ( 'NONE',  ( -1.000000000000000000, 0.000000000000000000, 0.000000000000000000 ) ) ;
#19588 = CARTESIAN_POINT ( 'NONE',  ( 24.71805762077055135, -11.77340594384550343, 3.190795258418060776 ) ) ;
#19589 = CARTESIAN_POINT ( 'NONE',  ( 8.079129440378000737, -3.524751762020000179, 5.573845465339999805 ) ) ;
#19590 = VERTEX_POINT ( 'NONE', #13831 ) ;
#19591 = CARTESIAN_POINT ( 'NONE',  ( 7.443295280410000103, 4.698356649019999942, 8.789431186081998248 ) ) ;
#19592 = EDGE_CURVE ( 'NONE', #67932, #17996, #53684, .T. ) ;
#19594 = CARTESIAN_POINT ( 'NONE',  ( 13.26247400726062509, -11.68416116973912011, -1.976808445614455900 ) ) ;
#19593 = CARTESIAN_POINT ( 'NONE',  ( 4.965649514109999885, 0.1599529892900000139, 1.501782300629000089 ) ) ;
#19595 = CARTESIAN_POINT ( 'NONE',  ( 7.464673621134763515, -2.291441534361882137, 7.172437561238989012 ) ) ;
#19596 = CARTESIAN_POINT ( 'NONE',  ( 9.289886373836322875, -3.999992178805580334, 6.560153657526066162 ) ) ;
#19597 = CARTESIAN_POINT ( 'NONE',  ( 1.647883852297000074, 2.470933839010999833, -2.372615558983000472 ) ) ;
#19598 = ORIENTED_EDGE ( 'NONE', *, *, #60611, .F. ) ;
#19599 = CARTESIAN_POINT ( 'NONE',  ( 1.572458648010261806, -2.764615070225285631, -1.807037445058709224 ) ) ;
#19600 = B_SPLINE_CURVE_WITH_KNOTS ( 'NONE', 3,
 ( #61942, #41991, #14056, #56705, #67519, #15426 ),
 .UNSPECIFIED., .F., .F.,
 ( 4, 2, 4 ),
 ( 0.000000000000000000, 0.5000000000000000000, 1.000000000000000000 ),
 .UNSPECIFIED. ) ;
#19601 = CARTESIAN_POINT ( 'NONE',  ( 11.37518447801629939, -3.134012688501500055, 7.519093628927509876 ) ) ;
#19602 = CARTESIAN_POINT ( 'NONE',  ( 23.59999172237900211, -2.915589696762999949, -13.58550518520000061 ) ) ;
#19603 = CARTESIAN_POINT ( 'NONE',  ( 11.09425120759000016, 2.431871068503000277, 7.769513029648000391 ) ) ;
#19604 = CIRCLE ( 'NONE', #37455, 1.625000000000000000 ) ;
#19605 = CARTESIAN_POINT ( 'NONE',  ( 11.46179707368349909, 3.501542828836900156, 8.370914060838998694 ) ) ;
#19606 = CARTESIAN_POINT ( 'NONE',  ( 10.94076550314999885, 5.140765503144999471, -6.571291218949999902 ) ) ;
#19607 = CARTESIAN_POINT ( 'NONE',  ( 12.80505043854144276, 0.7302158263239216796, -13.98094363220830871 ) ) ;
#19608 = DIRECTION ( 'NONE',  ( 0.8480635683783770418, 0.000000000000000000, -0.5298945026977860406 ) ) ;
#19609 = CARTESIAN_POINT ( 'NONE',  ( 7.572196646342158388, 3.914246498630762350, 5.749145437917528412 ) ) ;
#19610 = ORIENTED_EDGE ( 'NONE', *, *, #14410, .F. ) ;
#19611 = CARTESIAN_POINT ( 'NONE',  ( 18.10179698720202879, -2.997559868305876840, 13.67533242386440939 ) ) ;
#19612 = CARTESIAN_POINT ( 'NONE',  ( -14.79345512259999929, -10.48174933044999868, -5.405686454350000503 ) ) ;
#19613 = ORIENTED_EDGE ( 'NONE', *, *, #14825, .F. ) ;
#19614 = EDGE_LOOP ( 'NONE', ( #68488, #22051, #24088, #49697 ) ) ;
#19615 = CARTESIAN_POINT ( 'NONE',  ( 25.02478460520268300, -2.919208160324095580, -11.54269743113043489 ) ) ;
#19616 = LINE ( 'NONE', #2167, #65084 ) ;
#19617 = CARTESIAN_POINT ( 'NONE',  ( 10.77672335273219950, 4.301522290735800169, 6.687976048055599421 ) ) ;
#19618 = CARTESIAN_POINT ( 'NONE',  ( 9.075483283097998566, 4.020836891789999257, 8.948690653012000951 ) ) ;
#19619 = CARTESIAN_POINT ( 'NONE',  ( 10.89218604104999955, 2.661903984162000469, -8.236033286991000679 ) ) ;
#19620 = CARTESIAN_POINT ( 'NONE',  ( 9.936116252963625328, -3.418844976054905782, -6.845942581217610012 ) ) ;
#19621 = CARTESIAN_POINT ( 'NONE',  ( 10.96207173348999930, -5.399846879528999999, 7.743266618618998898 ) ) ;
#19622 = B_SPLINE_CURVE_WITH_KNOTS ( 'NONE', 3,
 ( #26562, #15380, #30771, #20275 ),
 .UNSPECIFIED., .F., .F.,
 ( 4, 4 ),
 ( 0.000000000000000000, 1.000000000000000000 ),
 .UNSPECIFIED. ) ;
#19623 = CARTESIAN_POINT ( 'NONE',  ( 18.22962529608893689, -0.2638285456865464007, -12.59724228039519822 ) ) ;
#19624 = EDGE_CURVE ( 'NONE', #25967, #57124, #4541, .T. ) ;
#19625 = CARTESIAN_POINT ( 'NONE',  ( 5.500000000000000000, 11.06886219213000011, 1.536526853569999851 ) ) ;
#19626 = CARTESIAN_POINT ( 'NONE',  ( 11.04749144726329924, -4.500836215462999945, -6.793273974143599681 ) ) ;
#19627 = CARTESIAN_POINT ( 'NONE',  ( 8.111573341229000533, 3.326263523254000098, 8.794511546544999447 ) ) ;
#19628 = ORIENTED_EDGE ( 'NONE', *, *, #15854, .F. ) ;
#19629 = VECTOR ( 'NONE', #12301, 999.9999999999998863 ) ;
#19630 = CARTESIAN_POINT ( 'NONE',  ( 9.535395982797806980, -4.311073552809155274, 6.345787448237017792 ) ) ;
#19631 = DIRECTION ( 'NONE',  ( 0.000000000000000000, -0.7071067811865475727, -0.7071067811865475727 ) ) ;
#19632 = FACE_OUTER_BOUND ( 'NONE', #5744, .T. ) ;
#19633 = AXIS2_PLACEMENT_3D ( 'NONE', #13397, #18289, #40297 ) ;
#19634 = CARTESIAN_POINT ( 'NONE',  ( 9.813871383455010644, 10.26951666917000061, 4.796847285345002376 ) ) ;
#19635 = CARTESIAN_POINT ( 'NONE',  ( 9.507063610504999929, 4.524705472883399970, -8.666648427848999248 ) ) ;
#19636 = CARTESIAN_POINT ( 'NONE',  ( 12.08109376178929217, 2.472831159707305826, 13.77990118939880482 ) ) ;
#19637 = CARTESIAN_POINT ( 'NONE',  ( 9.743567407955000093, -5.287392049455999832, 8.939957179821000466 ) ) ;
#19638 = VERTEX_POINT ( 'NONE', #54228 ) ;
#19639 = CARTESIAN_POINT ( 'NONE',  ( 12.31508698968652560, -0.3880315156974609159, -12.69202109203974338 ) ) ;
#19640 = CARTESIAN_POINT ( 'NONE',  ( 5.500000000000000000, 6.217248937900999058E-14, -12.99999854704996238 ) ) ;
#19641 = VERTEX_POINT ( 'NONE', #27677 ) ;
#19642 = CARTESIAN_POINT ( 'NONE',  ( 23.50387503050299998, 0.000000000000000000, 0.000000000000000000 ) ) ;
#19643 = DIRECTION ( 'NONE',  ( 0.000000000000000000, 1.000000000000000000, 0.000000000000000000 ) ) ;
#19644 = DIRECTION ( 'NONE',  ( 0.000000000000000000, 1.000000000000000000, 0.000000000000000000 ) ) ;
#19645 = CARTESIAN_POINT ( 'NONE',  ( 12.33518044953559922, -3.231951024059400268, 7.099502491684900107 ) ) ;
#19646 = CONICAL_SURFACE ( 'NONE', #28588, 2.649999808707999893, 0.7853980705567794596 ) ;
#19647 = B_SPLINE_CURVE_WITH_KNOTS ( 'NONE', 3,
 ( #61716, #66960, #19760, #30594 ),
 .UNSPECIFIED., .F., .F.,
 ( 4, 4 ),
 ( 0.000000000000000000, 1.000000000000000000 ),
 .UNSPECIFIED. ) ;
#19648 = VECTOR ( 'NONE', #7672, 1000.000000000000000 ) ;
#19649 = CARTESIAN_POINT ( 'NONE',  ( 16.09997386696500143, -8.350085070477001992, -8.123950967096998710 ) ) ;
#19650 = CARTESIAN_POINT ( 'NONE',  ( -0.01901103192377000262, -0.5398464557615000325, -3.496157131901000081 ) ) ;
#19651 = DIRECTION ( 'NONE',  ( 0.000000000000000000, 0.000000000000000000, -1.000000000000000000 ) ) ;
#19652 = CARTESIAN_POINT ( 'NONE',  ( 12.38044747764041098, 3.063579277862370720, 12.22188755179955777 ) ) ;
#19653 = LINE ( 'NONE', #51801, #29703 ) ;
#19654 = CARTESIAN_POINT ( 'NONE',  ( 10.52641638348499953, 3.025038519517300184, -7.262511127784999410 ) ) ;
#19655 = CARTESIAN_POINT ( 'NONE',  ( 7.289711015751999312, -0.9708250560305000665, 0.5387387265405000347 ) ) ;
#19656 = EDGE_CURVE ( 'NONE', #11774, #46140, #39246, .T. ) ;
#19657 = ADVANCED_FACE ( 'NONE', ( #38499 ), #2335, .T. ) ;
#19658 = CARTESIAN_POINT ( 'NONE',  ( 10.45625165877000029, 3.661871102473000406, -9.317475234260999883 ) ) ;
#19659 = CARTESIAN_POINT ( 'NONE',  ( 9.050076168957998490, 3.420574098817999786, -8.483869947211399420 ) ) ;
#19661 = CARTESIAN_POINT ( 'NONE',  ( 9.249283493600000128, -3.910012670022149806, 6.649720865199900466 ) ) ;
#19660 = CARTESIAN_POINT ( 'NONE',  ( 16.09055856039299925, -8.515834468357001086, -7.893949987785000566 ) ) ;
#19662 = PLANE ( 'NONE',  #47582 ) ;
#19663 = ORIENTED_EDGE ( 'NONE', *, *, #21653, .F. ) ;
#19664 = CARTESIAN_POINT ( 'NONE',  ( 10.86190547754509872, 4.891676932241900033, 7.471700551735359852 ) ) ;
#19665 = CARTESIAN_POINT ( 'NONE',  ( 9.350955436992014924, 5.758048718045908565, -7.748523603980665087 ) ) ;
#19666 = CARTESIAN_POINT ( 'NONE',  ( 9.731000818238999983, 3.111278474435999808, 7.032008172796599510 ) ) ;
#19667 = CARTESIAN_POINT ( 'NONE',  ( 10.99999999997000089, -4.000000000000000000, -7.500000000000000000 ) ) ;
#19668 = CARTESIAN_POINT ( 'NONE',  ( 0.7000000000000000666, 0.5773502691895999739, -1.000000000000000000 ) ) ;
#19669 = CARTESIAN_POINT ( 'NONE',  ( 12.80505043854143388, 3.124999999999999556, 13.52078605991414939 ) ) ;
#19670 = CARTESIAN_POINT ( 'NONE',  ( 9.457462135716001583, -5.100000000000000533, -6.571291218949999902 ) ) ;
#19671 = ORIENTED_EDGE ( 'NONE', *, *, #43970, .F. ) ;
#19672 = ADVANCED_FACE ( 'NONE', ( #42456 ), #47361, .F. ) ;
#19673 = CARTESIAN_POINT ( 'NONE',  ( 9.936596320338999533, -5.057167065956000407, -7.068569539041399175 ) ) ;
#19674 = CARTESIAN_POINT ( 'NONE',  ( 17.80000000000000071, -14.76315775485999993, -50.50083396221000243 ) ) ;
#19675 = CARTESIAN_POINT ( 'NONE',  ( 12.17403632436368888, -4.976178716761900489, 7.727966254184200245 ) ) ;
#19676 = EDGE_CURVE ( 'NONE', #6824, #54765, #23535, .T. ) ;
#19677 = CARTESIAN_POINT ( 'NONE',  ( 18.10394395700116021, 2.009981277211910111, -12.43865165640889892 ) ) ;
#19678 = CARTESIAN_POINT ( 'NONE',  ( 8.226256224620007274, -3.202920229111001049, -6.615926928587001044 ) ) ;
#19679 = CIRCLE ( 'NONE', #54300, 13.98989063585999837 ) ;
#19680 = CARTESIAN_POINT ( 'NONE',  ( 19.01453011999999987, 0.8000000000000000444, -3.149999999999999911 ) ) ;
#19681 = CARTESIAN_POINT ( 'NONE',  ( 12.19334556178055706, 2.628630841125718209, -13.64533835608825107 ) ) ;
#19683 = LINE ( 'NONE', #20024, #54677 ) ;
#19682 = B_SPLINE_CURVE_WITH_KNOTS ( 'NONE', 3,
 ( #62634, #52499, #4253, #53191 ),
 .UNSPECIFIED., .F., .F.,
 ( 4, 4 ),
 ( 0.000000000000000000, 1.000000000000000000 ),
 .UNSPECIFIED. ) ;
#19684 = DIRECTION ( 'NONE',  ( 1.000000000000000000, 0.000000000000000000, 0.000000000000000000 ) ) ;
#19685 = CARTESIAN_POINT ( 'NONE',  ( 7.000000000000000000, -7.526486366024999874, 3.526486366024999874 ) ) ;
#19686 = CARTESIAN_POINT ( 'NONE',  ( 12.09999999999999964, -4.000000000000000000, 7.500000000000000000 ) ) ;
#19688 = DIRECTION ( 'NONE',  ( 0.000000000000000000, -1.000000000000000000, 0.000000000000000000 ) ) ;
#19687 = SHAPE_REPRESENTATION ( '510 Pin Insulator', ( #9676 ), #3105 ) ;
#19689 = CARTESIAN_POINT ( 'NONE',  ( 11.10000006013000018, 9.802256759419000431, 6.071885733684999842 ) ) ;
#19690 = CARTESIAN_POINT ( 'NONE',  ( 2.350788447235875545, -1.095349359437870262, -3.341294758621923489 ) ) ;
#19691 = CARTESIAN_POINT ( 'NONE',  ( 8.672989158774999652, 4.728328492779000136, -8.692725459657999920 ) ) ;
#19692 = DIRECTION ( 'NONE',  ( -0.8231338744408063235, -0.5678473604306591982, 0.000000000000000000 ) ) ;
#19693 = ORIENTED_EDGE ( 'NONE', *, *, #37469, .F. ) ;
#19694 = AXIS2_PLACEMENT_3D ( 'NONE', #8066, #67124, #13661 ) ;
#19695 = CARTESIAN_POINT ( 'NONE',  ( 8.570375340018552279, -3.646757250303549913, 8.848425586001473775 ) ) ;
#19696 = CARTESIAN_POINT ( 'NONE',  ( 18.27991844657867659, 2.543687620403384031, -13.76699789025506071 ) ) ;
#19697 = ORIENTED_EDGE ( 'NONE', *, *, #3876, .F. ) ;
#19698 = CARTESIAN_POINT ( 'NONE',  ( 9.858051052051999719, -3.149129950522900234, 7.333482423122699601 ) ) ;
#19699 = CARTESIAN_POINT ( 'NONE',  ( 2.780140132544583587, -3.408904368339108260, 0.9161175952574674985 ) ) ;
#19700 = CARTESIAN_POINT ( 'NONE',  ( 8.795585841232000490, 5.251032986819000214, -6.070151079272999795 ) ) ;
#19701 = CARTESIAN_POINT ( 'NONE',  ( 11.00000000000000000, 3.031410575668799900, 7.825000000000000178 ) ) ;
#19702 = CARTESIAN_POINT ( 'NONE',  ( 11.10101463001529964, -3.377766160221900016, -6.503413421344399481 ) ) ;
#19703 = LINE ( 'NONE', #36462, #33713 ) ;
#19704 = DIRECTION ( 'NONE',  ( 0.000000000000000000, -1.000000000000000000, 0.000000000000000000 ) ) ;
#19705 = EDGE_LOOP ( 'NONE', ( #40134, #38690, #41737, #66628, #30703, #19423, #12008, #33358, #27017, #59578 ) ) ;
#19706 = CARTESIAN_POINT ( 'NONE',  ( 25.39991507555011196, 8.680020025996363131, -7.390263434115322383 ) ) ;
#19707 = CARTESIAN_POINT ( 'NONE',  ( 24.44496488041000148, -12.03536727282999941, 3.224852091355999928 ) ) ;
#19708 = CARTESIAN_POINT ( 'NONE',  ( 8.367589158771000513, 5.461114003844000031, -8.582501063019000398 ) ) ;
#19709 = EDGE_LOOP ( 'NONE', ( #45582, #39316, #12648, #10822 ) ) ;
#19710 = CARTESIAN_POINT ( 'NONE',  ( 10.75911768454999873, 4.477564074640000058, -5.708570851020999370 ) ) ;
#19711 = FILL_AREA_STYLE_COLOUR ( '', #11933 ) ;
#19712 = ORIENTED_EDGE ( 'NONE', *, *, #54552, .F. ) ;
#19713 = CARTESIAN_POINT ( 'NONE',  ( 8.720797255587999786, 5.140789995332999851, 7.548297453605989027 ) ) ;
#19714 = CARTESIAN_POINT ( 'NONE',  ( 18.08264632488623391, -2.164896798301380709, -12.52334278189865735 ) ) ;
#19715 = PRODUCT_RELATED_PRODUCT_CATEGORY ( 'part', '', ( #13747 ) ) ;
#19716 = CARTESIAN_POINT ( 'NONE',  ( 0.2000000000000000389, 2.149999999999999911, 1.476203897337000000E-12 ) ) ;
#19717 = CARTESIAN_POINT ( 'NONE',  ( 10.99183569977872565, -8.063891305078106697, -6.969091237525657512 ) ) ;
#19718 = CARTESIAN_POINT ( 'NONE',  ( 9.883148997457000817, 5.167567567567999731, 6.822293592207000934 ) ) ;
#19719 = VERTEX_POINT ( 'NONE', #22412 ) ;
#19720 = CARTESIAN_POINT ( 'NONE',  ( 8.032988339672121114, 4.532664226843759359, -6.238162434079100649 ) ) ;
#19721 = CYLINDRICAL_SURFACE ( 'NONE', #15045, 12.50000000000000000 ) ;
#19722 = CARTESIAN_POINT ( 'NONE',  ( 8.133277933996801323, -2.820894615410645123, 8.178702166372193716 ) ) ;
#19723 = CARTESIAN_POINT ( 'NONE',  ( 12.35242198444189299, 3.088429417998427962, -13.65509667848947473 ) ) ;
#19724 = CONICAL_SURFACE ( 'NONE', #13049, 1.150081764678999585, 0.7854598963975319981 ) ;
#19725 = CARTESIAN_POINT ( 'NONE',  ( 17.64985702823327074, 0.7243378955761863303, 13.98124959093732400 ) ) ;
#19726 = PLANE ( 'NONE',  #65936 ) ;
#19727 = CARTESIAN_POINT ( 'NONE',  ( 10.76232069631999977, -3.259150589222000072, -8.644998763029001054 ) ) ;
#19728 = ORIENTED_EDGE ( 'NONE', *, *, #6293, .F. ) ;
#19729 = VERTEX_POINT ( 'NONE', #39197 ) ;
#19730 = CARTESIAN_POINT ( 'NONE',  ( 10.06481084123000080, 5.336630274082000192, -7.092011739486999922 ) ) ;
#19731 = CIRCLE ( 'NONE', #58799, 12.20000000000000639 ) ;
#19732 = DIRECTION ( 'NONE',  ( -1.000000000000000000, 0.000000000000000000, 0.000000000000000000 ) ) ;
#19733 = CARTESIAN_POINT ( 'NONE',  ( 12.21215155065115532, -2.301234877124808786, 13.71362569328431391 ) ) ;
#19734 = CARTESIAN_POINT ( 'NONE',  ( 23.71889066594441786, 3.252317644464183033, 13.29341160290726798 ) ) ;
#19735 = EDGE_CURVE ( 'NONE', #58690, #60460, #55280, .T. ) ;
#19736 = ADVANCED_FACE ( 'NONE', ( #38859 ), #5042, .T. ) ;
#19737 = CARTESIAN_POINT ( 'NONE',  ( 7.890669420221000152, 4.660296061153999858, 6.322498784873999078 ) ) ;
#19738 = CARTESIAN_POINT ( 'NONE',  ( 17.89162860438300129, -3.376692001085000339, -11.11057855219999979 ) ) ;
#19740 = CARTESIAN_POINT ( 'NONE',  ( 10.90000000000000036, 0.000000000000000000, 0.000000000000000000 ) ) ;
#19739 = CARTESIAN_POINT ( 'NONE',  ( 10.89157120343299923, -4.055348968344419269, 6.359530327585999565 ) ) ;
#19741 = CARTESIAN_POINT ( 'NONE',  ( 8.894523589655003448, -4.897163489593995500, -6.153759344469004411 ) ) ;
#19742 = VERTEX_POINT ( 'NONE', #11928 ) ;
#19743 = CARTESIAN_POINT ( 'NONE',  ( 17.60000001072100062, -11.41073498373000028, 4.623967591968000335 ) ) ;
#19744 = CARTESIAN_POINT ( 'NONE',  ( 10.98991108309999909, -2.844095821392999657, -5.102617441991000646 ) ) ;
#19745 = CARTESIAN_POINT ( 'NONE',  ( 9.534310001152000780, -5.383415012847999392, -8.183490493635000362 ) ) ;
#19746 = DIRECTION ( 'NONE',  ( 1.000000000000000000, 0.000000000000000000, 0.000000000000000000 ) ) ;
#19747 = B_SPLINE_CURVE_WITH_KNOTS ( 'NONE', 3,
 ( #53425, #21594, #12847, #55145 ),
 .UNSPECIFIED., .F., .F.,
 ( 4, 4 ),
 ( 0.000000000000000000, 1.000000000000000000 ),
 .UNSPECIFIED. ) ;
#19748 = CARTESIAN_POINT ( 'NONE',  ( 18.17043869202645112, -2.609785213645622992, -12.42531509792942934 ) ) ;
#19749 = CARTESIAN_POINT ( 'NONE',  ( 24.53428985367600390, -3.614319203926000146, 12.31267510079000083 ) ) ;
#19750 = CARTESIAN_POINT ( 'NONE',  ( 24.30000000000000071, 12.03537377768999939, 3.224868684338999980 ) ) ;
#19751 = CARTESIAN_POINT ( 'NONE',  ( 13.82809631267600103, 8.844623397843001555, 7.663863542600000578 ) ) ;
#19752 = CARTESIAN_POINT ( 'NONE',  ( 16.39999999485600313, -3.595156957901000094, -11.99794989424000136 ) ) ;
#19753 = CARTESIAN_POINT ( 'NONE',  ( 10.90434687351665310, -5.250000000000000888, 7.336375382625536901 ) ) ;
#19754 = EDGE_CURVE ( 'NONE', #31394, #34575, #12286, .T. ) ;
#19755 = CARTESIAN_POINT ( 'NONE',  ( 9.188234083221754389, 2.648243641808995630, 7.263637137173954983 ) ) ;
#19756 = CARTESIAN_POINT ( 'NONE',  ( 5.700000000000000178, -11.06886219213000011, 1.536526853569999851 ) ) ;
#19757 = ORIENTED_EDGE ( 'NONE', *, *, #55663, .T. ) ;
#19758 = CARTESIAN_POINT ( 'NONE',  ( 12.55627843433555491, -0.5734477787136643689, -12.68256797703446281 ) ) ;
#19759 = CARTESIAN_POINT ( 'NONE',  ( 12.18199593247725865, -2.449686698172776289, -12.46314100319584384 ) ) ;
#19760 = CARTESIAN_POINT ( 'NONE',  ( 24.60115016796638088, -8.755275691353283207, 9.042371375187583382 ) ) ;
#19761 = CARTESIAN_POINT ( 'NONE',  ( 24.54687940532799928, 3.662828524876999836, -12.34579568540000061 ) ) ;
#19762 = DIRECTION ( 'NONE',  ( -1.000000000000000000, 0.000000000000000000, 0.000000000000000000 ) ) ;
#19763 = ORIENTED_EDGE ( 'NONE', *, *, #40642, .F. ) ;
#19764 = CARTESIAN_POINT ( 'NONE',  ( 7.099999886593999499, -12.39999890530000037, 0.000000000000000000 ) ) ;
#19765 = PRODUCT_CONTEXT ( 'NONE', #65948, 'mechanical' ) ;
#19766 = CARTESIAN_POINT ( 'NONE',  ( 0.6780453033732724011, -2.141412704026376623, 2.806277474037436992 ) ) ;
#19767 = CARTESIAN_POINT ( 'NONE',  ( 12.99325612864500279, -11.57041205278999918, -1.757148387262999822 ) ) ;
#19768 = DIRECTION ( 'NONE',  ( 0.000000000000000000, -0.000000000000000000, 1.000000000000000000 ) ) ;
#19769 = CARTESIAN_POINT ( 'NONE',  ( 11.39189666366029918, 3.947847673382490541, -8.673729056199000809 ) ) ;
#19770 = ORIENTED_EDGE ( 'NONE', *, *, #46838, .F. ) ;
#19771 = AXIS2_PLACEMENT_3D ( 'NONE', #23511, #12337, #2200 ) ;
#19772 = CARTESIAN_POINT ( 'NONE',  ( 10.96207173348999930, -5.399846879528999999, 7.743266618618998898 ) ) ;
#19773 = VERTEX_POINT ( 'NONE', #22762 ) ;
#19774 = CARTESIAN_POINT ( 'NONE',  ( 7.674792391072008613, -2.650477653308784376, 7.499986425013215552 ) ) ;
#19775 = CARTESIAN_POINT ( 'NONE',  ( 7.555275273711000494, -4.314043295739000250, 8.819145559946001356 ) ) ;
#19776 = CARTESIAN_POINT ( 'NONE',  ( 18.13027066859325487, -0.4451122480341416776, -13.99293440828418689 ) ) ;
#19777 = VERTEX_POINT ( 'NONE', #28368 ) ;
#19778 = CARTESIAN_POINT ( 'NONE',  ( 8.267367474942998840, 3.071849710027000135, -6.244583336620999958 ) ) ;
#19779 = DIRECTION ( 'NONE',  ( -1.231068759215981725E-07, 1.236409737982979503E-07, -0.9999999999999849010 ) ) ;
#19780 = CARTESIAN_POINT ( 'NONE',  ( 7.242439158769000684, 3.554387346680000004, -8.824570035521999145 ) ) ;
#19781 = STYLED_ITEM ( 'NONE', ( #26086 ), #50398 ) ;
#19782 = CARTESIAN_POINT ( 'NONE',  ( 10.18823075089156660, 2.651244971521983906, 7.275526744220880637 ) ) ;
#19783 = CARTESIAN_POINT ( 'NONE',  ( 10.20218235306506926, -2.710356544815101909, 7.038640550472702095 ) ) ;
#19784 = VERTEX_POINT ( 'NONE', #20783 ) ;
#19785 = CARTESIAN_POINT ( 'NONE',  ( 10.09196524370999981, -3.841385669346000231, 5.536421174581999338 ) ) ;
#19786 = CARTESIAN_POINT ( 'NONE',  ( 12.18947262544554100, -2.391368178663336952, -13.69585133610886452 ) ) ;
#19787 = CARTESIAN_POINT ( 'NONE',  ( 5.438359839683999830, 0.7554284705563453217, 1.310679582531389276 ) ) ;
#19788 = ORIENTED_EDGE ( 'NONE', *, *, #12840, .T. ) ;
#19789 = CARTESIAN_POINT ( 'NONE',  ( 10.44807121817999906, -3.684978196963999864, -6.173109031625999776 ) ) ;
#19790 = CIRCLE ( 'NONE', #16434, 14.00000000000000533 ) ;
#19791 = CARTESIAN_POINT ( 'NONE',  ( 7.959096408387808630, 3.398144457071999636, -6.280823960497042613 ) ) ;
#19792 = ORIENTED_EDGE ( 'NONE', *, *, #31447, .T. ) ;
#19793 = CARTESIAN_POINT ( 'NONE',  ( 24.30001680106099826, 12.21047197645999915, -3.271805488357999891 ) ) ;
#19794 = CARTESIAN_POINT ( 'NONE',  ( 5.313359839684166808, 1.310679582531387943, -0.7554284705563468760 ) ) ;
#19795 = EDGE_CURVE ( 'NONE', #44553, #43316, #40844, .T. ) ;
#19796 = CARTESIAN_POINT ( 'NONE',  ( 8.687922088694000067, 3.419384128876999718, -5.860036257779999147 ) ) ;
#19797 = CARTESIAN_POINT ( 'NONE',  ( 11.50002032348423064, 3.558966193428915403, -11.09334449156781943 ) ) ;
#19798 = EDGE_CURVE ( 'NONE', #49517, #19773, #35894, .T. ) ;
#19799 = AXIS2_PLACEMENT_3D ( 'NONE', #67564, #8851, #57421 ) ;
#19800 = CARTESIAN_POINT ( 'NONE',  ( 12.26373570557222337, 0.3125842563278190545, -13.89527356689842996 ) ) ;
#19801 = CARTESIAN_POINT ( 'NONE',  ( 18.15144633312242917, -2.312812061507715011, 12.49323956768624200 ) ) ;
#19802 = ORIENTED_EDGE ( 'NONE', *, *, #1845, .F. ) ;
#19803 = CARTESIAN_POINT ( 'NONE',  ( 3.427149063888667246, 0.04771112035505382237, -3.543401238238605533 ) ) ;
#19804 = ORIENTED_EDGE ( 'NONE', *, *, #15874, .T. ) ;
#19805 = CARTESIAN_POINT ( 'NONE',  ( 10.92717848204000042, 5.023653513500000223, 8.718036113327999104 ) ) ;
#19806 = DIRECTION ( 'NONE',  ( 0.000000000000000000, 1.000000000000000000, 0.000000000000000000 ) ) ;
#19807 = CARTESIAN_POINT ( 'NONE',  ( 8.830545280412000153, 3.207599814920999659, -6.150466394809999571 ) ) ;
#19808 = CARTESIAN_POINT ( 'NONE',  ( 3.557839444424999886, 0.04138239269183999897, 3.543466380272000116 ) ) ;
#19809 = CARTESIAN_POINT ( 'NONE',  ( 10.35427551197999918, -4.879111827962000270, -8.944027914303999793 ) ) ;
#19810 = DIRECTION ( 'NONE',  ( -1.000000000000000000, 0.000000000000000000, 0.000000000000000000 ) ) ;
#19811 = CARTESIAN_POINT ( 'NONE',  ( 9.010249263028118349, -5.224549296214872740, 8.068167775449891721 ) ) ;
#19812 = ORIENTED_EDGE ( 'NONE', *, *, #23755, .F. ) ;
#19813 = CARTESIAN_POINT ( 'NONE',  ( 11.29303032197930001, -3.336467919271199900, 8.427909097977700270 ) ) ;
#19814 = CARTESIAN_POINT ( 'NONE',  ( 3.103056799211125316, 2.798833948393625981, 2.150913519912208471 ) ) ;
#19815 = CARTESIAN_POINT ( 'NONE',  ( 8.751496707488000126, -3.918323994020610268, -8.356402621895700378 ) ) ;
#19816 = ADVANCED_FACE ( 'NONE', ( #42114 ), #4650, .T. ) ;
#19817 = PLANE ( 'NONE',  #35504 ) ;
#19819 = CARTESIAN_POINT ( 'NONE',  ( 13.49980696793000057, 9.514462421839999351, 7.834836582454001608 ) ) ;
#19818 = CARTESIAN_POINT ( 'NONE',  ( 9.629022744239000176, 5.794335169544999609, 7.414871903737999759 ) ) ;
#19820 = CARTESIAN_POINT ( 'NONE',  ( 11.70379573085659786, 5.106255642043000087, -7.691418046581699919 ) ) ;
#19821 = AXIS2_PLACEMENT_3D ( 'NONE', #64359, #53551, #42716 ) ;
#19822 = B_SPLINE_CURVE_WITH_KNOTS ( 'NONE', 3,
 ( #12298, #54946, #53900, #17185 ),
 .UNSPECIFIED., .F., .F.,
 ( 4, 4 ),
 ( 0.000000000000000000, 1.000000000000000000 ),
 .UNSPECIFIED. ) ;
#19823 = EDGE_CURVE ( 'NONE', #69025, #13775, #12494, .T. ) ;
#19824 = CARTESIAN_POINT ( 'NONE',  ( 25.46372779695100164, -11.23407511953000082, -3.161075425950000017 ) ) ;
#19825 = CARTESIAN_POINT ( 'NONE',  ( 9.680342523874998051, 3.007153757386999526, -7.348017636355000270 ) ) ;
#19826 = CARTESIAN_POINT ( 'NONE',  ( 17.60287381234529747, 0.7178228174669238904, 12.57953618971562548 ) ) ;
#19827 = CARTESIAN_POINT ( 'NONE',  ( 24.40777907822999993, 3.358845133677000216, 12.19253384565000076 ) ) ;
#19828 = CARTESIAN_POINT ( 'NONE',  ( 11.05435090131019926, 5.119447121461000449, 6.807613609764599616 ) ) ;
#19829 = CARTESIAN_POINT ( 'NONE',  ( 23.68246226653500131, 9.989803668321998842, 9.401306877296001119 ) ) ;
#19830 = ORIENTED_EDGE ( 'NONE', *, *, #65652, .T. ) ;
#19831 = CARTESIAN_POINT ( 'NONE',  ( 9.272293146792000229, -3.705847642455000202, 9.096432253453999195 ) ) ;
#19832 = CARTESIAN_POINT ( 'NONE',  ( 3.999985533191000364, -6.914809019160056625E-16, -2.149963194831858715 ) ) ;
#19833 = CARTESIAN_POINT ( 'NONE',  ( 5.000030787343000327, -1.834918991542628053, -1.057581170753189692 ) ) ;
#19834 = EDGE_LOOP ( 'NONE', ( #1614, #9773, #31573, #17451, #8047 ) ) ;
#19835 = AXIS2_PLACEMENT_3D ( 'NONE', #49689, #60873, #39203 ) ;
#19836 = CARTESIAN_POINT ( 'NONE',  ( 10.90000000000000036, -0.2999999999999999889, -9.662944685757000940 ) ) ;
#19837 = EDGE_CURVE ( 'NONE', #41592, #25195, #45074, .T. ) ;
#19838 = CARTESIAN_POINT ( 'NONE',  ( 11.55811496860034815, 5.045590851977999947, 8.035816473382100256 ) ) ;
#19839 = CARTESIAN_POINT ( 'NONE',  ( 10.97819528041000048, 5.476824759564999923, -7.128718425160999850 ) ) ;
#19840 = ORIENTED_EDGE ( 'NONE', *, *, #64818, .T. ) ;
#19841 = CARTESIAN_POINT ( 'NONE',  ( 5.169609839683333874, -0.1963495408493606265, -1.500000000000000222 ) ) ;
#19842 = CIRCLE ( 'NONE', #6406, 1.000000000000000222 ) ;
#19843 = CARTESIAN_POINT ( 'NONE',  ( 9.209046587350854907, -5.018376794265571483, -6.218521724468556222 ) ) ;
#19844 = CARTESIAN_POINT ( 'NONE',  ( 10.73964560330029983, 4.391636236366600166, 8.716526793355999558 ) ) ;
#19845 = LINE ( 'NONE', #61803, #38844 ) ;
#19846 = CARTESIAN_POINT ( 'NONE',  ( 9.753242276648803610, 2.714773723612766254, 7.027402982326849568 ) ) ;
#19847 = ORIENTED_EDGE ( 'NONE', *, *, #64394, .T. ) ;
#19848 = CARTESIAN_POINT ( 'NONE',  ( 7.840802619469265267, -4.754872393406737174, 6.367696273718201461 ) ) ;
#19849 = FACE_OUTER_BOUND ( 'NONE', #55437, .T. ) ;
#19850 = CARTESIAN_POINT ( 'NONE',  ( 8.094940203606975970, -4.449604110491481634, 5.819802056068767548 ) ) ;
#19851 = CARTESIAN_POINT ( 'NONE',  ( 10.33326717315600085, -4.973628086880700572, 8.329718467866699783 ) ) ;
#19852 = ORIENTED_EDGE ( 'NONE', *, *, #54172, .F. ) ;
#19853 = CARTESIAN_POINT ( 'NONE',  ( 10.49268136245999905, -4.966242441184999912, -4.914681127036000241 ) ) ;
#19854 = CARTESIAN_POINT ( 'NONE',  ( 11.23964560330029983, -3.608363763633400279, 8.716526793355999558 ) ) ;
#19855 = ORIENTED_EDGE ( 'NONE', *, *, #59134, .T. ) ;
#19856 = CARTESIAN_POINT ( 'NONE',  ( 10.07101354018233508, -3.231816600031356845, 6.500416447002274722 ) ) ;
#19857 = EDGE_LOOP ( 'NONE', ( #24167, #52908, #49907, #4884 ) ) ;
#19858 = LINE ( 'NONE', #25791, #27512 ) ;
#19859 = CARTESIAN_POINT ( 'NONE',  ( 2.550973465877000024, 3.500000000000000000, 0.000000000000000000 ) ) ;
#19860 = CARTESIAN_POINT ( 'NONE',  ( 10.85679632507500081, 4.490665650747399873, -8.409605917786398877 ) ) ;
#19861 = CARTESIAN_POINT ( 'NONE',  ( 12.18277869730536977, -4.531392946702499813, 8.547856079839998955 ) ) ;
#19862 = CARTESIAN_POINT ( 'NONE',  ( 12.18465059688361940, 2.421662038956231555, -12.46951891513069910 ) ) ;
#19863 = AXIS2_PLACEMENT_3D ( 'NONE', #8442, #61922, #7753 ) ;
#19864 = CARTESIAN_POINT ( 'NONE',  ( 10.62841772631199966, -3.509411006705700053, 6.490165927606000196 ) ) ;
#19865 = CARTESIAN_POINT ( 'NONE',  ( 7.330281674562000305, 4.426928431836000044, 9.293321981113999541 ) ) ;
#19866 = ORIENTED_EDGE ( 'NONE', *, *, #18538, .T. ) ;
#19867 = CARTESIAN_POINT ( 'NONE',  ( 9.489763540183334456, 4.327184855449099921, -8.717465845835395299 ) ) ;
#19868 = CARTESIAN_POINT ( 'NONE',  ( 7.262120559621999760, -4.847802017252000439, 9.065364004483999594 ) ) ;
#19869 = CARTESIAN_POINT ( 'NONE',  ( 11.41486084871699802, 2.792989229543000107, 7.174999999999999822 ) ) ;
#19870 = VERTEX_POINT ( 'NONE', #2143 ) ;
#19871 = CARTESIAN_POINT ( 'NONE',  ( 12.41452611191166255, -2.987998126639117125, -12.32436705583800673 ) ) ;
#19872 = CARTESIAN_POINT ( 'NONE',  ( 10.54687750876899877, 3.382085645339300228, 6.541108991297599928 ) ) ;
#19873 = AXIS2_PLACEMENT_3D ( 'NONE', #10124, #20961, #14687 ) ;
#19874 = CARTESIAN_POINT ( 'NONE',  ( 10.78888064679000003, -2.675723359162999859, -6.748225798259000818 ) ) ;
#19875 = CARTESIAN_POINT ( 'NONE',  ( 6.684036528646004172, 10.47948907923000306, -4.649236476274002605 ) ) ;
#19876 = CARTESIAN_POINT ( 'NONE',  ( 17.98628609634500108, -3.388648274289000284, -11.90503202562999974 ) ) ;
#19877 = EDGE_CURVE ( 'NONE', #35474, #32730, #2819, .T. ) ;
#19878 = CARTESIAN_POINT ( 'NONE',  ( 5.500000000000000000, 0.000000000000000000, 0.000000000000000000 ) ) ;
#19879 = CARTESIAN_POINT ( 'NONE',  ( 12.78089176142236383, -3.248146600645751114, -13.61798599873023718 ) ) ;
#19880 = EDGE_CURVE ( 'NONE', #3964, #8090, #24261, .T. ) ;
#19881 = CARTESIAN_POINT ( 'NONE',  ( 11.02287616594229824, -4.261927842557799551, -6.674353346984900348 ) ) ;
#19882 = CARTESIAN_POINT ( 'NONE',  ( 10.29657053952199952, -4.502253688815499366, -6.324815923923999605 ) ) ;
#19883 = EDGE_CURVE ( 'NONE', #20133, #509, #7535, .T. ) ;
#19884 = CARTESIAN_POINT ( 'NONE',  ( 8.572537312455677849, -5.041095006993285388, 6.231862335800022912 ) ) ;
#19885 = VERTEX_POINT ( 'NONE', #50380 ) ;
#19886 = VERTEX_POINT ( 'NONE', #46167 ) ;
#19887 = CARTESIAN_POINT ( 'NONE',  ( 12.15760927726063834, -0.3803681711079593963, -13.99548972734546126 ) ) ;
#19888 = AXIS2_PLACEMENT_3D ( 'NONE', #9604, #67641, #63077 ) ;
#19889 = DIRECTION ( 'NONE',  ( 1.000000000000000000, 0.000000000000000000, 0.000000000000000000 ) ) ;
#19890 = CARTESIAN_POINT ( 'NONE',  ( 4.700001368028300597, 14.00000000000000000, 0.000000000000000000 ) ) ;
#19891 = CARTESIAN_POINT ( 'NONE',  ( 9.819565861057999001, 2.688248842995000221, -7.873038103423000145 ) ) ;
#19892 = CARTESIAN_POINT ( 'NONE',  ( 8.623804163831874092, 4.944546604654881605, 6.045403407478842084 ) ) ;
#19893 = CARTESIAN_POINT ( 'NONE',  ( 18.01300802853348415, 2.925445001331293149, 12.34219835790438680 ) ) ;
#19894 = FACE_OUTER_BOUND ( 'NONE', #46813, .T. ) ;
#19895 = CARTESIAN_POINT ( 'NONE',  ( 9.137543006348998631, 2.995704926864999784, 8.544754656710999541 ) ) ;
#19896 = CONICAL_SURFACE ( 'NONE', #16539, 1.699999998954999869, 0.7853981633972997312 ) ;
#19897 = CARTESIAN_POINT ( 'NONE',  ( 11.43114108301961451, -3.379311755690166841, -6.880598518631704685 ) ) ;
#19898 = ORIENTED_EDGE ( 'NONE', *, *, #43714, .F. ) ;
#19899 = CARTESIAN_POINT ( 'NONE',  ( 9.471374412057000924, 2.030666183831999927, 7.549764512038000142 ) ) ;
#19900 = CARTESIAN_POINT ( 'NONE',  ( 9.779646554150998483, -3.580250267348600079, -8.258629096756299859 ) ) ;
#19901 = CARTESIAN_POINT ( 'NONE',  ( 9.778460659405999067, 5.743717947473999885, 7.748300625457000379 ) ) ;
#19902 = CARTESIAN_POINT ( 'NONE',  ( 11.51279632507520034, -3.375091146194399983, 6.341531314375999706 ) ) ;
#19903 = FACE_OUTER_BOUND ( 'NONE', #12456, .T. ) ;
#19904 = CIRCLE ( 'NONE', #64546, 11.50000000000000178 ) ;
#19905 = CARTESIAN_POINT ( 'NONE',  ( 9.383148997457999130, 5.167567567567999731, 6.822293592207000934 ) ) ;
#19906 = B_SPLINE_CURVE_WITH_KNOTS ( 'NONE', 3,
 ( #10899, #11239, #22068, #9868, #32576, #32245, #16145, #53888, #10212, #42382, #15119, #37815, #64024, #31895, #37131, #31212, #65, #53206 ),
 .UNSPECIFIED., .F., .F.,
 ( 4, 2, 2, 2, 2, 2, 2, 2, 4 ),
 ( 0.000000000000000000, 0.1250000000000000000, 0.2500000000000000000, 0.3750000000000000000, 0.5000000000000000000, 0.6250000000000000000, 0.7500000000000000000, 0.8750000000000000000, 1.000000000000000000 ),
 .UNSPECIFIED. ) ;
#19907 = CARTESIAN_POINT ( 'NONE',  ( 24.78226664044499827, 8.655277561894001437, 9.168097195530998889 ) ) ;
#19908 = CARTESIAN_POINT ( 'NONE',  ( 12.27985646406008335, 0.3389720875425228930, 12.69391532355468044 ) ) ;
#19909 = CARTESIAN_POINT ( 'NONE',  ( 8.802614158774000330, 3.975069902178000270, 9.483774112875002160 ) ) ;
#19910 = CARTESIAN_POINT ( 'NONE',  ( 10.24961997674000003, 4.184221916050000267, 9.286882020979000174 ) ) ;
#19911 = CARTESIAN_POINT ( 'NONE',  ( 11.53971429488000133, -3.572666839320000065, 11.04878221693000029 ) ) ;
#19912 = ORIENTED_EDGE ( 'NONE', *, *, #19397, .F. ) ;
#19913 = CARTESIAN_POINT ( 'NONE',  ( 9.088029719595001055, 2.881930053949999682, -8.823338183322999129 ) ) ;
#19914 = CARTESIAN_POINT ( 'NONE',  ( 6.972601553427999477, -1.175206010251000022, 0.8635533004969999649 ) ) ;
#19915 = CARTESIAN_POINT ( 'NONE',  ( 8.945154276125844461, 5.350566776863566965, 7.852883605855088156 ) ) ;
#19916 = CARTESIAN_POINT ( 'NONE',  ( 10.14601354018233259, 4.999583552997728830, 8.268183399968640046 ) ) ;
#19917 = CARTESIAN_POINT ( 'NONE',  ( 10.93769906950999982, 5.063122007744000008, 4.920829195600999739 ) ) ;
#19918 = CARTESIAN_POINT ( 'NONE',  ( 11.31410538575739899, -3.024036709177600368, -7.266662245194900116 ) ) ;
#19919 = VERTEX_POINT ( 'NONE', #19596 ) ;
#19920 = CARTESIAN_POINT ( 'NONE',  ( 1.438972969266999913, 1.794790469053999971, -3.302590565797000277 ) ) ;
#19921 = CARTESIAN_POINT ( 'NONE',  ( 18.17906593022175343, -0.04061720356229615858, -12.69993396819151243 ) ) ;
#19922 = EDGE_CURVE ( 'NONE', #11428, #32730, #66448, .T. ) ;
#19925 = CARTESIAN_POINT ( 'NONE',  ( 13.92966272177200260, -9.396431546200000540, -8.198412206645000921 ) ) ;
#19924 = CARTESIAN_POINT ( 'NONE',  ( 8.822164158776001130, 2.644017913812000131, -7.838184857420000817 ) ) ;
#19923 = UNCERTAINTY_MEASURE_WITH_UNIT (LENGTH_MEASURE( 1.000000000000000082E-05 ), #46116, 'distance_accuracy_value', 'NONE');
#19926 = FACE_OUTER_BOUND ( 'NONE', #66357, .T. ) ;
#19927 = DIRECTION ( 'NONE',  ( 0.000000000000000000, -0.5000000000000169864, -0.8660254037844288266 ) ) ;
#19928 = ADVANCED_FACE ( 'NONE', ( #61897 ), #28718, .T. ) ;
#19930 = CARTESIAN_POINT ( 'NONE',  ( 18.14704975929777575, -2.701423609612692900, -13.62863833005038217 ) ) ;
#19929 = AXIS2_PLACEMENT_3D ( 'NONE', #3908, #67888, #8141 ) ;
#19931 = CARTESIAN_POINT ( 'NONE',  ( 11.14595257254739913, 3.168263696564200149, 7.258104750172799768 ) ) ;
#19932 = CARTESIAN_POINT ( 'NONE',  ( 4.074968078372999791, 0.000000000000000000, 0.000000000000000000 ) ) ;
#19933 = CARTESIAN_POINT ( 'NONE',  ( 8.849379440379999906, -3.975070057433999438, 9.483761758588999058 ) ) ;
#19934 = ORIENTED_EDGE ( 'NONE', *, *, #52979, .F. ) ;
#19935 = CARTESIAN_POINT ( 'NONE',  ( 9.475899447075999404, 4.122021000979000149, 9.013569734175000292 ) ) ;
#19937 = CARTESIAN_POINT ( 'NONE',  ( 10.03977055961999909, -2.255583827894000137, -8.111980070942999888 ) ) ;
#19936 = CARTESIAN_POINT ( 'NONE',  ( 5.649576767392000320, -1.375515609181000132, 0.5142804259679000234 ) ) ;
#19938 = CARTESIAN_POINT ( 'NONE',  ( 7.581694733679056775, -4.164585657937257324, 5.768241722127926074 ) ) ;
#19939 = CIRCLE ( 'NONE', #8761, 13.98989063587000281 ) ;
#19940 = CARTESIAN_POINT ( 'NONE',  ( 7.936333720142999759, -5.123034382927999175, 6.721303993095999907 ) ) ;
#19941 = CARTESIAN_POINT ( 'NONE',  ( 2.172385296145999956, 2.895272466935999933, -1.424404891072999835 ) ) ;
#19942 = ORIENTED_EDGE ( 'NONE', *, *, #23488, .F. ) ;
#19943 = CARTESIAN_POINT ( 'NONE',  ( 0.8572294063981078516, 1.740182405912205521, 2.807159848119936463 ) ) ;
#19944 = CARTESIAN_POINT ( 'NONE',  ( 12.06025819896753859, -4.986099335708799707, 7.314099615601099558 ) ) ;
#19945 = CARTESIAN_POINT ( 'NONE',  ( 10.55162425919054137, -5.013906213569661929, 5.027077672038467782 ) ) ;
#19946 = CARTESIAN_POINT ( 'NONE',  ( 9.889842476439000052, 4.052276433608000161, 9.260531940735001299 ) ) ;
#19947 = CARTESIAN_POINT ( 'NONE',  ( 11.21149010443640037, 5.137564434800999891, 7.414927836855409460 ) ) ;
#19948 = CIRCLE ( 'NONE', #12106, 13.10000000000000320 ) ;
#19949 = CARTESIAN_POINT ( 'NONE',  ( 5.699999545467999695, -6.661338147750999827E-14, 12.60000000000318998 ) ) ;
#19950 = CARTESIAN_POINT ( 'NONE',  ( 12.80505043854144276, 0.6951438842159466391, -13.94765567169527998 ) ) ;
#19951 = CARTESIAN_POINT ( 'NONE',  ( 10.98944156655594817, -5.203365389803279228, 6.677358443460799542 ) ) ;
#19952 = CARTESIAN_POINT ( 'NONE',  ( 24.59181002256200088, -3.481107758750999537, -12.13646513482999900 ) ) ;
#19953 = VECTOR ( 'NONE', #29975, 1000.000000000000000 ) ;
#19954 = B_SPLINE_CURVE_WITH_KNOTS ( 'NONE', 3,
 ( #63296, #58070, #35380, #25217, #41989, #36749 ),
 .UNSPECIFIED., .F., .F.,
 ( 4, 2, 4 ),
 ( 0.000000000000000000, 0.5000000000000000000, 1.000000000000000000 ),
 .UNSPECIFIED. ) ;
#19955 = CARTESIAN_POINT ( 'NONE',  ( 18.17294214856818968, -2.135913245783944259, 13.83611159055835316 ) ) ;
#19956 = CARTESIAN_POINT ( 'NONE',  ( 17.86939907855665410, 3.040585884632406977, -13.54383026114252075 ) ) ;
#19957 = ORIENTED_EDGE ( 'NONE', *, *, #5264, .F. ) ;
#19958 = CARTESIAN_POINT ( 'NONE',  ( 5.449999267937000624, 2.451372438371999805E-13, 6.461498003317998333E-14 ) ) ;
#19959 = CARTESIAN_POINT ( 'NONE',  ( 9.150818738817875442, -3.048937241343601112, -6.673278530809400699 ) ) ;
#19960 = ORIENTED_EDGE ( 'NONE', *, *, #41131, .F. ) ;
#19961 = CARTESIAN_POINT ( 'NONE',  ( 9.354346873516664829, 2.749999999999999112, 7.336375382625534236 ) ) ;
#19962 = CARTESIAN_POINT ( 'NONE',  ( 11.07210672858429845, 3.307795442047700263, 8.020722037455799480 ) ) ;
#19963 = CARTESIAN_POINT ( 'NONE',  ( 10.49785886974000171, 3.776281431161999880, 5.717632172928999168 ) ) ;
#19964 = B_SPLINE_CURVE_WITH_KNOTS ( 'NONE', 3,
 ( #7978, #66346, #55526, #49586, #29312, #50625, #50966, #12881, #23012, #3064, #2726, #24049, #34210, #23365, #45384, #66694, #40141, #67035 ),
 .UNSPECIFIED., .F., .F.,
 ( 4, 2, 2, 2, 2, 2, 2, 2, 4 ),
 ( 0.000000000000000000, 0.1250000000000000000, 0.2500000000000000000, 0.3750000000000000000, 0.5000000000000000000, 0.6250000000000000000, 0.7500000000000000000, 0.8750000000000000000, 1.000000000000000000 ),
 .UNSPECIFIED. ) ;
#19965 = CARTESIAN_POINT ( 'NONE',  ( 10.86493304757000011, 4.678466548873998931, -9.048467117372998914 ) ) ;
#19966 = CARTESIAN_POINT ( 'NONE',  ( 9.885457958598628636, -3.143868186573851364, -7.319526769407151079 ) ) ;
#19967 = CARTESIAN_POINT ( 'NONE',  ( 10.42595817177000050, -5.042180160032999403, 8.702227297563000619 ) ) ;
#19968 = ADVANCED_FACE ( 'NONE', ( #14356 ), #14011, .T. ) ;
#19969 = CARTESIAN_POINT ( 'NONE',  ( 18.01033200807251689, 0.5598083480993615302, -12.58755849294668394 ) ) ;
#19970 = CARTESIAN_POINT ( 'NONE',  ( 24.30000000000000071, -12.03537377768999939, -3.224868684338999980 ) ) ;
#19971 = CARTESIAN_POINT ( 'NONE',  ( 10.57980110216399972, -4.739241740354600552, -7.048535450274799885 ) ) ;
#19972 = EDGE_CURVE ( 'NONE', #44831, #28207, #60867, .T. ) ;
#19973 = EDGE_CURVE ( 'NONE', #45574, #16052, #11341, .T. ) ;
#19974 = DIRECTION ( 'NONE',  ( 0.000000000000000000, -0.6194815870790952861, -0.7850111867164476509 ) ) ;
#19975 = VERTEX_POINT ( 'NONE', #44798 ) ;
#19976 = CARTESIAN_POINT ( 'NONE',  ( 11.12341523360999851, -6.060598086452000821, -5.274801696963999476 ) ) ;
#19977 = CARTESIAN_POINT ( 'NONE',  ( 5.700000000000000178, 0.8000000000000000444, 3.149999999999999911 ) ) ;
#19978 = DIRECTION ( 'NONE',  ( 0.8843050097021329936, -0.1786785991674020024, 0.4313682974156600181 ) ) ;
#19979 = CARTESIAN_POINT ( 'NONE',  ( 15.20000000000000107, -11.47055000429999971, 4.757693469806000053 ) ) ;
#19980 = CARTESIAN_POINT ( 'NONE',  ( 17.85722199349616446, 1.826245811740494274, 12.46695042358089012 ) ) ;
#19981 = CARTESIAN_POINT ( 'NONE',  ( 12.28223951138205550, 3.023960592195345853, 13.66951858831273370 ) ) ;
#19982 = DIRECTION ( 'NONE',  ( 0.000000000000000000, 1.000000000000000000, 0.000000000000000000 ) ) ;
#19983 = ORIENTED_EDGE ( 'NONE', *, *, #12878, .F. ) ;
#19984 = AXIS2_PLACEMENT_3D ( 'NONE', #47437, #36949, #58263 ) ;
#19985 = CARTESIAN_POINT ( 'NONE',  ( 12.18002295456110673, 0.03981407387464135084, -12.70000161046296938 ) ) ;
#19986 = CARTESIAN_POINT ( 'NONE',  ( 12.21569938124766885, -0.4259565731506597674, 13.99353270933016979 ) ) ;
#19987 = VERTEX_POINT ( 'NONE', #39896 ) ;
#19988 = CARTESIAN_POINT ( 'NONE',  ( 24.40628504395400000, 8.880942544344001988, 9.006432928708999697 ) ) ;
#19989 = CARTESIAN_POINT ( 'NONE',  ( 10.53521345716899837, 4.924890298941200228, 6.659120737011199331 ) ) ;
#19990 = EDGE_CURVE ( 'NONE', #24800, #12380, #19178, .T. ) ;
#19991 = CARTESIAN_POINT ( 'NONE',  ( 15.39999999998900293, 9.471998555523999386, 8.194929586088999685 ) ) ;
#19992 = CARTESIAN_POINT ( 'NONE',  ( 11.54749144726329924, -4.500836215462999945, 8.206726025856399431 ) ) ;
#19993 = CARTESIAN_POINT ( 'NONE',  ( 10.08351354018237345, 5.250000000000000888, -7.663624617374468428 ) ) ;
#19994 = CARTESIAN_POINT ( 'NONE',  ( 25.44993329535400051, 2.258942858049999725, 11.14410225571399948 ) ) ;
#19995 = CARTESIAN_POINT ( 'NONE',  ( 8.039443364739069509, 4.176885327615297960, 8.849067469250631035 ) ) ;
#19996 = CARTESIAN_POINT ( 'NONE',  ( 12.25620353052267042, 2.010025970016497521, 12.43864443381842833 ) ) ;
#19997 = DIRECTION ( 'NONE',  ( 1.000000000000000000, 0.000000000000000000, 0.000000000000000000 ) ) ;
#19998 = CARTESIAN_POINT ( 'NONE',  ( 10.64949279009019989, 3.739015461786900030, -8.468936491037499792 ) ) ;
#19999 = CARTESIAN_POINT ( 'NONE',  ( 9.785239991807605620, 4.544749735012262093, -8.875846220998239389 ) ) ;
#20000 = CARTESIAN_POINT ( 'NONE',  ( 10.50897971959000010, 4.485029564998000318, -9.114435267298000909 ) ) ;
#20001 = CARTESIAN_POINT ( 'NONE',  ( 9.833267173155999075, 3.026371913119300316, -6.670281532133299329 ) ) ;
#20003 = CARTESIAN_POINT ( 'NONE',  ( 12.18412391183566967, 2.571774448851283257, 12.43455553901978128 ) ) ;
#20002 = CARTESIAN_POINT ( 'NONE',  ( 10.10331523854997293, 3.090216591177149752, 8.647999319121542072 ) ) ;
#20004 = CARTESIAN_POINT ( 'NONE',  ( 8.780141893066772951, 2.899999999999999911, -6.457321861693552378 ) ) ;
#20005 = ORIENTED_EDGE ( 'NONE', *, *, #36051, .T. ) ;
#20006 = CARTESIAN_POINT ( 'NONE',  ( 10.40480513895999870, 4.779740423663599636, 7.933462475324499330 ) ) ;
#20007 = CARTESIAN_POINT ( 'NONE',  ( 9.509907746701999898, -5.077451867123000007, 8.469011304701000498 ) ) ;
#20008 = CARTESIAN_POINT ( 'NONE',  ( 10.10892546752099896, 3.135062625344399834, 7.559927309296559983 ) ) ;
#20009 = CARTESIAN_POINT ( 'NONE',  ( 9.277558426223626142, 4.358884483112399622, -8.297956262399157623 ) ) ;
#20010 = CARTESIAN_POINT ( 'NONE',  ( 10.75110221171000013, -2.822135527917999820, 6.655890318096999714 ) ) ;
#20011 = EDGE_CURVE ( 'NONE', #16325, #39811, #20049, .T. ) ;
#20012 = CARTESIAN_POINT ( 'NONE',  ( 9.332537864288001472, 2.899999999999999911, 6.571291218949999902 ) ) ;
#20013 = CARTESIAN_POINT ( 'NONE',  ( 12.20879664878247972, 2.687389840184388756, 13.63187458905523286 ) ) ;
#20014 = CARTESIAN_POINT ( 'NONE',  ( 23.66477443553700155, 3.238206668739000094, -13.42731210495999861 ) ) ;
#20015 = VERTEX_POINT ( 'NONE', #15724 ) ;
#20016 = CARTESIAN_POINT ( 'NONE',  ( 5.105886958660000197, 1.045076633341000205, 0.4412723599748000214 ) ) ;
#20017 = CARTESIAN_POINT ( 'NONE',  ( 9.098721904869998767, -2.884547197234000215, -8.126218358304999612 ) ) ;
#20018 = CARTESIAN_POINT ( 'NONE',  ( 10.37601093510613559, -4.718927363017628274, -4.957694817182617619 ) ) ;
#20019 = CARTESIAN_POINT ( 'NONE',  ( 12.10477869730532774, -4.467447516829900600, 8.421761806503198500 ) ) ;
#20020 = CARTESIAN_POINT ( 'NONE',  ( 17.89002091993512522, 1.842089822799531929, -12.46461944294985535 ) ) ;
#20021 = CARTESIAN_POINT ( 'NONE',  ( 11.13481874607999877, -2.665701152538000329, 5.178754270907999668 ) ) ;
#20022 = CARTESIAN_POINT ( 'NONE',  ( 18.08677744227652795, 2.828625537428428149, 12.36890451985948758 ) ) ;
#20023 = CARTESIAN_POINT ( 'NONE',  ( 12.30953092759153833, 2.881442378548828565, -13.58513712698574061 ) ) ;
#20024 = CARTESIAN_POINT ( 'NONE',  ( 19.89999966725400071, -12.52499966719000035, -3.709580198520000162E-10 ) ) ;
#20025 = CARTESIAN_POINT ( 'NONE',  ( 9.964045559621999004, -3.485908552077000344, -9.275738075927998594 ) ) ;
#20026 = LINE ( 'NONE', #41352, #22119 ) ;
#20027 = CARTESIAN_POINT ( 'NONE',  ( 12.19581923677612778, 0.3960277493246568414, -13.99440111282555499 ) ) ;
#20028 = DIRECTION ( 'NONE',  ( 1.000000000000000000, 0.000000000000000000, 0.000000000000000000 ) ) ;
#20029 = CYLINDRICAL_SURFACE ( 'NONE', #19799, 1.000000000000001332 ) ;
#20030 = CARTESIAN_POINT ( 'NONE',  ( 9.073148997461000675, -5.167567567567999731, -6.822293592207000934 ) ) ;
#20031 = CARTESIAN_POINT ( 'NONE',  ( 9.568039158772000619, 5.336630274082000192, -7.092011739486999922 ) ) ;
#20032 = CARTESIAN_POINT ( 'NONE',  ( 12.03979707368350027, -4.430269712815499972, 8.251775607861899786 ) ) ;
#20033 = ORIENTED_EDGE ( 'NONE', *, *, #68027, .F. ) ;
#20034 = CARTESIAN_POINT ( 'NONE',  ( 3.999999999999999112, 2.081773110051107878, 0.5564988119414340240 ) ) ;
#20035 = CARTESIAN_POINT ( 'NONE',  ( 18.02697970389225546, 1.963589444787172233, -13.86161523094991210 ) ) ;
#20036 = ORIENTED_EDGE ( 'NONE', *, *, #66212, .T. ) ;
#20037 = CARTESIAN_POINT ( 'NONE',  ( 8.570375340018618004, 3.646757250303513054, 8.848425586001186005 ) ) ;
#20038 = CARTESIAN_POINT ( 'NONE',  ( 11.67766954483535891, 4.715882430684499305, 8.604570063127999546 ) ) ;
#20039 = CARTESIAN_POINT ( 'NONE',  ( 4.149992563292000725, -1.007210908820211026, -1.747525841223985132 ) ) ;
#20040 = CARTESIAN_POINT ( 'NONE',  ( 8.475341021510246264, -5.350570349241358770, 7.499981640446112152 ) ) ;
#20041 = CARTESIAN_POINT ( 'NONE',  ( 10.60746886766490071, -4.498335456194499926, -6.594573315824700188 ) ) ;
#20042 = CARTESIAN_POINT ( 'NONE',  ( 11.60000000000000142, -3.812684744683584981, -6.446733142248666226 ) ) ;
#20043 = CARTESIAN_POINT ( 'NONE',  ( 8.455992358796999397, 2.899999999999999911, -6.571291218954000257 ) ) ;
#20044 = ORIENTED_EDGE ( 'NONE', *, *, #28320, .T. ) ;
#20045 = CARTESIAN_POINT ( 'NONE',  ( 5.599999999407000217, -1.300000000000000044, -10.56294468516420082 ) ) ;
#20046 = ADVANCED_FACE ( 'NONE', ( #4189 ), #15033, .F. ) ;
#20047 = CARTESIAN_POINT ( 'NONE',  ( 9.684729719592999331, 2.370176859044999862, -6.912649125838000508 ) ) ;
#20048 = ORIENTED_EDGE ( 'NONE', *, *, #36136, .F. ) ;
#20050 = VECTOR ( 'NONE', #4781, 1000.000000000000000 ) ;
#20049 = B_SPLINE_CURVE_WITH_KNOTS ( 'NONE', 3,
 ( #5227, #41605, #14695, #19940 ),
 .UNSPECIFIED., .F., .F.,
 ( 4, 4 ),
 ( 0.000000000000000000, 1.000000000000000000 ),
 .UNSPECIFIED. ) ;
#20051 = CARTESIAN_POINT ( 'NONE',  ( 10.78637067803999905, 5.666041748529999644, -7.787005432561999285 ) ) ;
#20052 = ORIENTED_EDGE ( 'NONE', *, *, #36578, .T. ) ;
#20053 = CARTESIAN_POINT ( 'NONE',  ( 9.782608878791998919, 3.710311786319799854, 8.745979585038000437 ) ) ;
#20054 = CARTESIAN_POINT ( 'NONE',  ( 17.78706641053896575, -1.919568985577241094, -12.56801103569108236 ) ) ;
#20055 = DIRECTION ( 'NONE',  ( 2.186536431443105034E-10, 0.8764392776392420092, -0.4815124013057229813 ) ) ;
#20056 = CARTESIAN_POINT ( 'NONE',  ( 24.46729256464000457, -12.16659091368999945, -3.168154674931000336 ) ) ;
#20057 = CARTESIAN_POINT ( 'NONE',  ( 7.562137788010000250, -9.102769276979000068, -5.790556498848999922 ) ) ;
#20058 = B_SPLINE_CURVE_WITH_KNOTS ( 'NONE', 3,
 ( #34513, #60713, #55823, #66645, #1643, #65262, #28568, #49884, #12831, #18765, #7576, #22612, #44992, #40095, #61408, #56157, #28215, #33465, #1298, #29614, #12135, #54780, #6879, #30972, #68010, #35532, #46706, #20127, #41455, #14547, #24346, #24691, #62763, #63099, #25029, #40418, #14884, #67661, #36205, #9625, #3356, #46014, #46360, #57182, #68348, #51934, #20467, #67321, #4030, #41113, #66983, #35866, #50917, #57522, #52284, #25713, #19439, #45678, #4378, #19786, #62428, #14205, #40763, #57876, #47047, #9279, #41795, #25369, #15226 ),
 .UNSPECIFIED., .F., .F.,
 ( 4, 2, 2, 2, 2, 2, 2, 2, 2, 2, 2, 2, 2, 1, 2, 2, 2, 1, 2, 2, 2, 2, 1, 2, 2, 2, 2, 2, 2, 2, 2, 2, 2, 2, 2, 4 ),
 ( 0.000000000000000000, 0.06250000000004618528, 0.1250000000000923706, 0.1562500000001154632, 0.1875000000001385558, 0.2187500000001616485, 0.2343750000001731948, 0.2500000000001847411, 0.2812500000002073341, 0.2968750000002188805, 0.3125000000002304268, 0.3281250000002419731, 0.3437500000002535194, 0.3593750000002650657, 0.3671875000002713940, 0.3750000000002777223, 0.3906250000002883804, 0.3984375000002929879, 0.4023437500002955414, 0.4062500000002980949, 0.4218750000003073097, 0.4296875000003119172, 0.4335937500003141376, 0.4355468750003134160, 0.4375000000003126943, 0.4531250000003034795, 0.4687500000002942646, 0.4843750000002850498, 0.5000000000002757794, 0.5312500000002580158, 0.5468750000002491340, 0.5625000000002402523, 0.5937500000002230438, 0.6250000000002058353, 0.7500000000001374456, 1.000000000000000000 ),
 .UNSPECIFIED. ) ;
#20059 = B_SPLINE_CURVE_WITH_KNOTS ( 'NONE', 1,
 ( #6403, #22833 ),
 .UNSPECIFIED., .F., .F.,
 ( 2, 2 ),
 ( 0.000000000000000000, 1.000000000000000000 ),
 .UNSPECIFIED. ) ;
#20060 = ORIENTED_EDGE ( 'NONE', *, *, #64638, .F. ) ;
#20061 = FACE_OUTER_BOUND ( 'NONE', #14869, .T. ) ;
#20062 = CARTESIAN_POINT ( 'NONE',  ( 11.03092334123000029, 5.020455242919999783, -6.601201971309999195 ) ) ;
#20063 = ADVANCED_FACE ( 'NONE', ( #25526 ), #41261, .F. ) ;
#20064 = CARTESIAN_POINT ( 'NONE',  ( 8.599999952505998024, 3.250000006358199744, -7.500000000000000000 ) ) ;
#20065 = CYLINDRICAL_SURFACE ( 'NONE', #22687, 1.350000000000000533 ) ;
#20066 = EDGE_CURVE ( 'NONE', #59819, #1148, #4495, .T. ) ;
#20067 = CARTESIAN_POINT ( 'NONE',  ( 18.20560607722001834, 0.3231860383015686677, 13.99628497142876249 ) ) ;
#20068 = CARTESIAN_POINT ( 'NONE',  ( 17.76937411412500367, 3.251867979506000150, 11.33740618442000070 ) ) ;
#20069 = CARTESIAN_POINT ( 'NONE',  ( 11.10061802256000085, -3.093055606601000207, -6.153681532251999542 ) ) ;
#20070 = ORIENTED_EDGE ( 'NONE', *, *, #47854, .T. ) ;
#20071 = ORIENTED_EDGE ( 'NONE', *, *, #26270, .F. ) ;
#20072 = CARTESIAN_POINT ( 'NONE',  ( 9.675870280412999236, 3.031907308384000022, -8.729608011560001657 ) ) ;
#20073 = CARTESIAN_POINT ( 'NONE',  ( 7.204907196771999978, -0.2999999999999999889, 3.099954730132999714 ) ) ;
#20074 = CARTESIAN_POINT ( 'NONE',  ( 11.49977531252999974, 12.43119799159999950, 1.530013559959999991 ) ) ;
#20075 = CARTESIAN_POINT ( 'NONE',  ( 23.61456370124183124, 3.070877465454437516, 13.52759921014553157 ) ) ;
#20076 = CARTESIAN_POINT ( 'NONE',  ( 24.42335439002600239, 8.981275493775999763, -9.518163459556999939 ) ) ;
#20077 = CARTESIAN_POINT ( 'NONE',  ( 10.09259632033899834, 3.197262364844699611, -7.172402329663099430 ) ) ;
#20079 = CARTESIAN_POINT ( 'NONE',  ( 8.625941929927966711, 5.035312777410744900, 6.089150065163800640 ) ) ;
#20078 = CARTESIAN_POINT ( 'NONE',  ( 9.876392757686998536, -3.322036695224600322, 6.758914271013199304 ) ) ;
#20080 = CARTESIAN_POINT ( 'NONE',  ( 8.263772364603003240, -4.793682714277998080, -6.586182036516001759 ) ) ;
#20081 = EDGE_LOOP ( 'NONE', ( #29233, #3202, #29176, #42654 ) ) ;
#20082 = LINE ( 'NONE', #68651, #43647 ) ;
#20083 = CARTESIAN_POINT ( 'NONE',  ( 8.493436541922999794, -2.902501512378997894, 6.607638123744003167 ) ) ;
#20084 = CARTESIAN_POINT ( 'NONE',  ( 10.21627973160999936, 4.114789684104299461, 8.774051692788999546 ) ) ;
#20085 = CARTESIAN_POINT ( 'NONE',  ( 23.60000000000000142, 9.289189189551001036, 7.908916752675001050 ) ) ;
#20086 = CARTESIAN_POINT ( 'NONE',  ( 25.30000327618300204, -2.078227429405999693, 11.31065739696999906 ) ) ;
#20087 = ADVANCED_FACE ( 'NONE', ( #62575 ), #42306, .F. ) ;
#20088 = DIRECTION ( 'NONE',  ( 0.000000000000000000, -0.2098318009950989882, 0.9777374981512947372 ) ) ;
#20089 = CARTESIAN_POINT ( 'NONE',  ( 10.14206215041823000, 3.293869621293751937, 8.705460445251068435 ) ) ;
#20090 = CARTESIAN_POINT ( 'NONE',  ( 13.59015267864900345, 8.992820872206999994, 7.631366745126000772 ) ) ;
#20091 = VECTOR ( 'NONE', #14291, 1000.000000000000000 ) ;
#20092 = CARTESIAN_POINT ( 'NONE',  ( 6.899999691988000450, -12.43893545635000031, 2.828937028792000152 ) ) ;
#20093 = CARTESIAN_POINT ( 'NONE',  ( 17.60000003688378811, 11.49036663463118835, -4.802323205938251682 ) ) ;
#20094 = B_SPLINE_SURFACE_WITH_KNOTS ( 'NONE', 3, 3, ( 
 ( #28459, #39286, #8501, #2562, #2229, #12718, #61299, #35423, #55365, #35086, #19328, #34050, #40653, #60954, #45905, #50811, #61986, #23891, #3253 ),
 ( #51156, #17967, #34398, #66878, #60607, #24582, #51490, #45226, #28813, #24922, #56048, #18989, #8845, #7460, #30183, #50123, #18652, #39632, #46253 ),
 ( #67217, #14097, #40317, #13069, #56398, #23544, #29848, #44883, #56747, #66188, #18308, #55716, #7812, #3585, #29153, #66532, #50461, #39985, #8159 ),
 ( #13418, #34737, #29505, #2904, #24234, #45572, #61636, #13752, #15469, #36795, #14781, #52520, #37133, #63343, #67558, #68243, #46603, #4619, #53209 ) ),
 .UNSPECIFIED., .F., .F., .F.,
 ( 4, 4 ),
 ( 4, 1, 1, 1, 1, 1, 1, 1, 1, 1, 1, 1, 1, 1, 1, 1, 4 ),
 ( -0.1039086239011999951, 1.103908623900999864 ),
 ( -0.008849010032007000384, 0.01991027257200999809, 0.04866955517603999831, 0.07742883778006000306, 0.1061881203840999988, 0.1349474029881000126, 0.1637066855920999986, 0.1924659681960999846, 0.2212252508002000018, 0.2499845334042000156, 0.2787438160081999738, 0.3075030986121999876, 0.3362623812162000014, 0.3650216638202999908, 0.3937809464243000046, 0.4225402290282999629, 0.4512995116322999767 ),
 .UNSPECIFIED. ) ;
#20095 = CARTESIAN_POINT ( 'NONE',  ( 0.3672260901898748431, -3.367204892844285258, 0.4416305338764572319 ) ) ;
#20096 = CARTESIAN_POINT ( 'NONE',  ( 17.79128410730675114, 1.798519029207210629, 12.47099317247404748 ) ) ;
#20097 = CARTESIAN_POINT ( 'NONE',  ( 2.442700127934999799, -0.7445022475760999514, 3.172853915553000004 ) ) ;
#20098 = ORIENTED_EDGE ( 'NONE', *, *, #64541, .T. ) ;
#20099 = CARTESIAN_POINT ( 'NONE',  ( 12.67437701660358584, 0.7076089047904963181, -12.58011506138061009 ) ) ;
#20100 = CARTESIAN_POINT ( 'NONE',  ( 12.19562994360793873, -2.360937373121109850, -12.48287347411901571 ) ) ;
#20101 = LINE ( 'NONE', #56824, #26469 ) ;
#20102 = LINE ( 'NONE', #14859, #46853 ) ;
#20103 = CARTESIAN_POINT ( 'NONE',  ( 10.11501430098066656, 5.350017391163124358, -7.499999134156894343 ) ) ;
#20104 = VERTEX_POINT ( 'NONE', #26565 ) ;
#20105 = CARTESIAN_POINT ( 'NONE',  ( 5.190649514109999529, 0.1165019947749000029, 1.093825345293000018 ) ) ;
#20106 =( NAMED_UNIT ( * ) SI_UNIT ( $, .STERADIAN. ) SOLID_ANGLE_UNIT ( ) );
#20107 = CARTESIAN_POINT ( 'NONE',  ( 17.80428133522791256, 0.5732558492893025104, 12.68257967785543627 ) ) ;
#20108 = CARTESIAN_POINT ( 'NONE',  ( 1.849999551004999798, -1.625000000000000000, 0.000000000000000000 ) ) ;
#20109 = DIRECTION ( 'NONE',  ( 0.000000000000000000, 1.000000000000000000, 0.000000000000000000 ) ) ;
#20110 = CARTESIAN_POINT ( 'NONE',  ( 11.06456920625009843, 4.037149028919880145, -6.467161360063999886 ) ) ;
#20111 = ORIENTED_EDGE ( 'NONE', *, *, #6255, .T. ) ;
#20112 = CARTESIAN_POINT ( 'NONE',  ( 10.73930809942999964, -2.762991917822000154, 6.801028165221000066 ) ) ;
#20113 = ORIENTED_EDGE ( 'NONE', *, *, #21000, .T. ) ;
#20114 = CARTESIAN_POINT ( 'NONE',  ( 9.451730340337091363, -5.271997571102815527, 7.951892843798163746 ) ) ;
#20115 = CARTESIAN_POINT ( 'NONE',  ( 8.662855646795000197, -2.741638482234999952, 6.457327039244000311 ) ) ;
#20116 = CARTESIAN_POINT ( 'NONE',  ( 0.000000000000000000, 5.100000000000000533, -7.500000000000000000 ) ) ;
#20117 = ORIENTED_EDGE ( 'NONE', *, *, #32463, .F. ) ;
#20118 = CARTESIAN_POINT ( 'NONE',  ( -1.222471984994595150E-05, -9.327013418423733093E-16, -2.899969545326207765 ) ) ;
#20119 = CARTESIAN_POINT ( 'NONE',  ( 9.150683505092615633, 4.457228368748805458, 8.907085139201905477 ) ) ;
#20120 = CARTESIAN_POINT ( 'NONE',  ( 6.695464158771000207, 4.367071440064000498, -8.848478693904000991 ) ) ;
#20121 = CARTESIAN_POINT ( 'NONE',  ( 11.07273594314529142, 5.128905988536224037, 7.824979517142727659 ) ) ;
#20122 = CARTESIAN_POINT ( 'NONE',  ( 8.186595852941859874, -2.905265993888614950, 6.578644981517261847 ) ) ;
#20123 = ORIENTED_EDGE ( 'NONE', *, *, #19571, .F. ) ;
#20124 = CARTESIAN_POINT ( 'NONE',  ( 2.042640132539832898, 3.058252359239899132, 1.762666431298154146 ) ) ;
#20125 = EDGE_CURVE ( 'NONE', #32586, #12771, #7864, .T. ) ;
#20126 = EDGE_CURVE ( 'NONE', #13996, #43864, #49176, .T. ) ;
#20127 = CARTESIAN_POINT ( 'NONE',  ( 12.23606299695368982, -2.758663578172445785, -13.61513466669021533 ) ) ;
#20128 = DIRECTION ( 'NONE',  ( 0.000000000000000000, -1.000000000000000000, 0.000000000000000000 ) ) ;
#20129 = ORIENTED_EDGE ( 'NONE', *, *, #43929, .F. ) ;
#20130 = CARTESIAN_POINT ( 'NONE',  ( 9.701728707608999969, -4.253751259212999791, -8.839942087209999855 ) ) ;
#20131 = EDGE_CURVE ( 'NONE', #27228, #2158, #63371, .T. ) ;
#20132 = CARTESIAN_POINT ( 'NONE',  ( 8.296555885771999428, 2.897911263815999838, 6.617317042653000136 ) ) ;
#20133 = VERTEX_POINT ( 'NONE', #10131 ) ;
#20134 = CARTESIAN_POINT ( 'NONE',  ( 10.95791822924240577, 2.260523080717695699, 7.333870556128064599 ) ) ;
#20135 = CARTESIAN_POINT ( 'NONE',  ( 13.50003721581400029, -9.159934378815998812, -7.517910889891000537 ) ) ;
#20136 = CARTESIAN_POINT ( 'NONE',  ( 4.600001223043999943, -13.10000000000000142, 0.000000000000000000 ) ) ;
#20137 = CARTESIAN_POINT ( 'NONE',  ( 10.93499869900965038, 5.068606067930488734, -4.937945806540904314 ) ) ;
#20138 = CARTESIAN_POINT ( 'NONE',  ( 12.76344776297775674, 3.123961325724113891, 13.52107359494105765 ) ) ;
#20139 = CARTESIAN_POINT ( 'NONE',  ( 18.06602350563010972, -2.139519659637397986, 12.52832261142687287 ) ) ;
#20140 = VERTEX_POINT ( 'NONE', #27590 ) ;
#20141 = CARTESIAN_POINT ( 'NONE',  ( 3.351443705081666558, -2.857319464356316896, -2.096114062919034904 ) ) ;
#20142 = VERTEX_POINT ( 'NONE', #48916 ) ;
#20143 = CARTESIAN_POINT ( 'NONE',  ( 10.14750576281000072, 2.602962605360999770, 6.738577830910999822 ) ) ;
#20144 = EDGE_CURVE ( 'NONE', #18982, #57692, #64634, .T. ) ;
#20145 = AXIS2_PLACEMENT_3D ( 'NONE', #48358, #64080, #54992 ) ;
#20146 = PLANE ( 'NONE',  #2098 ) ;
#20147 = DIRECTION ( 'NONE',  ( 0.000000000000000000, 0.8648648648648717963, 0.5020047465136829867 ) ) ;
#20148 = CARTESIAN_POINT ( 'NONE',  ( 3.474005517471000282, 3.100289412622999841, 1.716429986814999920 ) ) ;
#20149 = ADVANCED_FACE ( 'NONE', ( #59058 ), #56366, .T. ) ;
#20150 = CARTESIAN_POINT ( 'NONE',  ( 10.40558062080000035, -5.599331384652000310, -8.437753779290000367 ) ) ;
#20151 = CARTESIAN_POINT ( 'NONE',  ( 10.02314899745999988, -5.167567567567999731, -6.822293592207000934 ) ) ;
#20152 = CARTESIAN_POINT ( 'NONE',  ( 9.040511248533881883, -4.920473672754849481, 8.487405920180457031 ) ) ;
#20153 = ORIENTED_EDGE ( 'NONE', *, *, #16388, .F. ) ;
#20154 = CARTESIAN_POINT ( 'NONE',  ( 10.80487885159599948, -3.003595720052600448, 7.618867373350600047 ) ) ;
#20155 = CARTESIAN_POINT ( 'NONE',  ( 10.31746213571000048, 5.100000000000000533, 6.571291218949999902 ) ) ;
#20156 = CARTESIAN_POINT ( 'NONE',  ( 15.83019412026500206, 8.948785863751000491, 8.423203147821000769 ) ) ;
#20157 = DIRECTION ( 'NONE',  ( -1.000000000000000000, 0.000000000000000000, 0.000000000000000000 ) ) ;
#20159 = CYLINDRICAL_SURFACE ( 'NONE', #22812, 0.6250000000000005551 ) ;
#20158 = CARTESIAN_POINT ( 'NONE',  ( 10.77462860031000069, 5.575476001419000127, 8.682676628339999425 ) ) ;
#20160 = CARTESIAN_POINT ( 'NONE',  ( 11.50687348028854906, 2.996540789803000315, -8.042549288197099244 ) ) ;
#20161 = CARTESIAN_POINT ( 'NONE',  ( 25.37646853861900453, -11.10818234785000058, 3.395598138602999860 ) ) ;
#20162 = CARTESIAN_POINT ( 'NONE',  ( 9.247734463322998977, 4.090312251411040378, -8.362294405496898619 ) ) ;
#20163 = CARTESIAN_POINT ( 'NONE',  ( 18.27543972223745783, 0.08185661189466754417, 12.59973963693671806 ) ) ;
#20164 = CARTESIAN_POINT ( 'NONE',  ( 6.836538849395999762, 1.535441917290000013, -0.2442687810326999998 ) ) ;
#20165 = CARTESIAN_POINT ( 'NONE',  ( 11.63611496860034933, 5.171412538012999605, 8.100294210499798808 ) ) ;
#20166 = CARTESIAN_POINT ( 'NONE',  ( 23.51511354854200064, 10.47166404558000075, 9.493607764193999543 ) ) ;
#20167 = ORIENTED_EDGE ( 'NONE', *, *, #5456, .F. ) ;
#20168 = CARTESIAN_POINT ( 'NONE',  ( 9.053331853208000268, -5.618388245857000030, 7.727743016644000207 ) ) ;
#20169 = CARTESIAN_POINT ( 'NONE',  ( 17.93991242251030371, 3.137220474326295250, 13.64397427468587587 ) ) ;
#20170 = PLANE ( 'NONE',  #49021 ) ;
#20171 = ORIENTED_EDGE ( 'NONE', *, *, #2855, .F. ) ;
#20172 = CARTESIAN_POINT ( 'NONE',  ( 18.53494720760600245, 3.035003031749999636, 12.19105792290999979 ) ) ;
#20173 = VECTOR ( 'NONE', #65718, 1000.000000000000114 ) ;
#20174 = CARTESIAN_POINT ( 'NONE',  ( 11.64122412107036908, 4.062069863985690255, 8.673243607771999208 ) ) ;
#20175 = CARTESIAN_POINT ( 'NONE',  ( 11.16750778041000025, 3.188704589882000118, -8.788663768996000769 ) ) ;
#20176 = ORIENTED_EDGE ( 'NONE', *, *, #55265, .F. ) ;
#20177 = EDGE_CURVE ( 'NONE', #43301, #42419, #61773, .T. ) ;
#20178 = CARTESIAN_POINT ( 'NONE',  ( 11.79999999471800010, 3.216299622513999701, -11.40340969442000052 ) ) ;
#20179 = CARTESIAN_POINT ( 'NONE',  ( 17.55505043854147118, -3.199751711897561801, 12.18694338143115452 ) ) ;
#20180 = CARTESIAN_POINT ( 'NONE',  ( 11.50271932425157040, 3.812601581225100400, 6.235801371442999397 ) ) ;
#20181 = CARTESIAN_POINT ( 'NONE',  ( 10.80169466977000070, -3.998196228428999355, 9.431543037543999475 ) ) ;
#20182 = CARTESIAN_POINT ( 'NONE',  ( 8.335885841230000537, 4.310355144869000732, 9.459505265942000918 ) ) ;
#20183 = ORIENTED_EDGE ( 'NONE', *, *, #50775, .F. ) ;
#20184 = CARTESIAN_POINT ( 'NONE',  ( 7.867079331757252270, -5.122016962447125898, 6.719626049376892674 ) ) ;
#20185 = B_SPLINE_CURVE_WITH_KNOTS ( 'NONE', 3,
 ( #63808, #54011, #38277, #10674 ),
 .UNSPECIFIED., .F., .F.,
 ( 4, 4 ),
 ( 0.8745766503823925175, 1.000000000000000000 ),
 .UNSPECIFIED. ) ;
#20186 = CARTESIAN_POINT ( 'NONE',  ( 15.40000000009400161, 8.833277835210999740, 7.896561221812000930 ) ) ;
#20187 = CARTESIAN_POINT ( 'NONE',  ( 8.238125043277811699, -5.540983280400556765, 8.307145266245010262 ) ) ;
#20188 = CARTESIAN_POINT ( 'NONE',  ( 10.18129229006300029, -2.893743561734000380, 8.142324746736500529 ) ) ;
#20189 = VERTEX_POINT ( 'NONE', #54029 ) ;
#20190 = CARTESIAN_POINT ( 'NONE',  ( 2.823890132542957954, -2.150913519912200478, -2.798833948393631754 ) ) ;
#20191 = B_SPLINE_CURVE_WITH_KNOTS ( 'NONE', 3,
 ( #34116, #66600, #50190, #2291, #44952, #66256 ),
 .UNSPECIFIED., .F., .F.,
 ( 4, 2, 4 ),
 ( 0.000000000000000000, 0.5000000000000000000, 1.000000000000000000 ),
 .UNSPECIFIED. ) ;
#20192 = DIRECTION ( 'NONE',  ( 0.000000000000000000, 1.000000000000000000, 0.000000000000000000 ) ) ;
#20193 = ORIENTED_EDGE ( 'NONE', *, *, #29423, .T. ) ;
#20194 = DIRECTION ( 'NONE',  ( -1.000000000000000000, 0.000000000000000000, 0.000000000000000000 ) ) ;
#20195 = ORIENTED_EDGE ( 'NONE', *, *, #27574, .T. ) ;
#20196 = CARTESIAN_POINT ( 'NONE',  ( 7.717918984469999799, -2.852331559125000027, 6.784354950350999225 ) ) ;
#20197 = FACE_OUTER_BOUND ( 'NONE', #18391, .T. ) ;
#20198 = CARTESIAN_POINT ( 'NONE',  ( 11.05946005378019947, 5.036385109519999403, -6.946587256304699309 ) ) ;
#20199 = CARTESIAN_POINT ( 'NONE',  ( 11.93345123989529988, -3.459769760840400110, 6.456682674800999777 ) ) ;
#20200 = CARTESIAN_POINT ( 'NONE',  ( 12.51684016020880996, 3.054675744551020422, -12.30488183412682801 ) ) ;
#20201 = CARTESIAN_POINT ( 'NONE',  ( 12.11759063708296047, -2.782734359457999851, 7.157757529645699890 ) ) ;
#20202 = CARTESIAN_POINT ( 'NONE',  ( 7.924357780410000274, 2.432118421226999949, 6.597517552098000060 ) ) ;
#20203 = EDGE_CURVE ( 'NONE', #10513, #53921, #35047, .T. ) ;
#20204 = EDGE_CURVE ( 'NONE', #48158, #26199, #65895, .T. ) ;
#20205 = VERTEX_POINT ( 'NONE', #39340 ) ;
#20206 = CARTESIAN_POINT ( 'NONE',  ( 21.10000109091659937, -12.52500000000000036, 0.000000000000000000 ) ) ;
#20207 = ADVANCED_FACE ( 'NONE', ( #17321 ), #32379, .F. ) ;
#20208 = CARTESIAN_POINT ( 'NONE',  ( 8.289120559623999185, -4.310353212080000773, 9.459493062793997709 ) ) ;
#20209 = CARTESIAN_POINT ( 'NONE',  ( 11.09999999999999964, -5.449702618175999547, 5.124965750789000296 ) ) ;
#20210 = EDGE_LOOP ( 'NONE', ( #38264, #36028, #61147, #30541 ) ) ;
#20211 = CARTESIAN_POINT ( 'NONE',  ( 12.52646068131089230, -3.059569037265597924, -12.30341205401442828 ) ) ;
#20212 = CARTESIAN_POINT ( 'NONE',  ( 11.52733460557258915, 4.206337284815599986, 6.238754009183999472 ) ) ;
#20213 = CARTESIAN_POINT ( 'NONE',  ( 11.05391814679000184, -5.159486550382999859, -8.487149456222999433 ) ) ;
#20214 = CARTESIAN_POINT ( 'NONE',  ( -0.2999999999999999889, -0.5773502691895999739, -1.000000000000000000 ) ) ;
#20215 = CARTESIAN_POINT ( 'NONE',  ( 18.17677363193000062, -3.419785592864999835, -11.99291007725999947 ) ) ;
#20216 = CARTESIAN_POINT ( 'NONE',  ( 8.461732853997650849, 5.351516129093011109, 7.263730654262094966 ) ) ;
#20217 = CARTESIAN_POINT ( 'NONE',  ( 12.28917444793836466, -2.147008681356604498, -13.74197010666756746 ) ) ;
#20218 = CARTESIAN_POINT ( 'NONE',  ( 10.72749279009019929, -4.225282629687599822, -8.336388861178200216 ) ) ;
#20219 = LINE ( 'NONE', #4129, #10553 ) ;
#20220 = AXIS2_PLACEMENT_3D ( 'NONE', #27059, #64095, #11652 ) ;
#20221 = CARTESIAN_POINT ( 'NONE',  ( 13.70005190196300227, -9.005348107749998832, -7.391036106496999381 ) ) ;
#20222 = CARTESIAN_POINT ( 'NONE',  ( 10.59999999999999964, 3.399999999999999911, 4.756097560976000338 ) ) ;
#20223 = ORIENTED_EDGE ( 'NONE', *, *, #15265, .F. ) ;
#20224 = ORIENTED_EDGE ( 'NONE', *, *, #19086, .T. ) ;
#20225 = DIRECTION ( 'NONE',  ( -0.7071060218675898623, -0.7071075405046897133, 8.464244187133876641E-10 ) ) ;
#20226 = CARTESIAN_POINT ( 'NONE',  ( 0.000000000000000000, 0.000000000000000000, 0.000000000000000000 ) ) ;
#20227 = CARTESIAN_POINT ( 'NONE',  ( 11.66486084871730000, -2.792989229543000107, 7.825000000000000178 ) ) ;
#20228 = CARTESIAN_POINT ( 'NONE',  ( 18.14119057072321084, 2.717377330609857200, 13.62490400531196499 ) ) ;
#20229 = CARTESIAN_POINT ( 'NONE',  ( 10.81362367151999848, 3.876947539724999725, -9.022206283674000460 ) ) ;
#20230 = ADVANCED_FACE ( 'NONE', ( #48450, #6479 ), #556, .F. ) ;
#20231 = CYLINDRICAL_SURFACE ( 'NONE', #33069, 12.59999999999999964 ) ;
#20232 = CARTESIAN_POINT ( 'NONE',  ( 18.15708441975577259, 2.331821618626342296, 12.48915497634519411 ) ) ;
#20233 = CARTESIAN_POINT ( 'NONE',  ( 17.79173234077999766, 3.528207283916999781, -11.96069632439000152 ) ) ;
#20234 = CARTESIAN_POINT ( 'NONE',  ( 9.972850246170999355, 5.044468801812000081, 6.258104779495000436 ) ) ;
#20235 = TOROIDAL_SURFACE ( 'NONE', #28075, 12.35000000006999876, 0.5000000000000000000 ) ;
#20236 = VERTEX_POINT ( 'NONE', #1245 ) ;
#20237 = DIRECTION ( 'NONE',  ( 1.000000000000000000, 0.000000000000000000, 0.000000000000000000 ) ) ;
#20238 = ORIENTED_EDGE ( 'NONE', *, *, #34333, .F. ) ;
#20239 = CARTESIAN_POINT ( 'NONE',  ( 12.36861073370957875, -2.947405515254782227, 12.33600917780096395 ) ) ;
#20240 = CARTESIAN_POINT ( 'NONE',  ( 8.586491082670404396, 5.311483864045265513, -7.867512027660226615 ) ) ;
#20241 = CARTESIAN_POINT ( 'NONE',  ( 10.63461554336999981, 5.668731883089999535, 6.527253515312000154 ) ) ;
#20242 = CARTESIAN_POINT ( 'NONE',  ( 11.67901463001530082, -3.302889347096799710, 8.616511311517999872 ) ) ;
#20243 = PLANE ( 'NONE',  #2658 ) ;
#20244 = CARTESIAN_POINT ( 'NONE',  ( 11.12425657198999929, 7.502475533924000572, -6.531087594010999808 ) ) ;
#20245 = B_SPLINE_CURVE_WITH_KNOTS ( 'NONE', 3,
 ( #10725, #37985, #48141, #32073, #17003, #244 ),
 .UNSPECIFIED., .F., .F.,
 ( 4, 2, 4 ),
 ( 0.000000000000000000, 0.5000000000000000000, 1.000000000000000000 ),
 .UNSPECIFIED. ) ;
#20246 = DIRECTION ( 'NONE',  ( 1.000000000000000000, 0.000000000000000000, 0.000000000000000000 ) ) ;
#20247 = CARTESIAN_POINT ( 'NONE',  ( 10.90724142537947650, 5.175055531252366947, -8.817797332566639668 ) ) ;
#20248 = CARTESIAN_POINT ( 'NONE',  ( 7.100000000000000533, 0.000000000000000000, -11.84999999999999964 ) ) ;
#20249 = CARTESIAN_POINT ( 'NONE',  ( 10.97807333593999957, 5.235090452703000885, -6.783100406990000053 ) ) ;
#20250 = CARTESIAN_POINT ( 'NONE',  ( 11.61719580513100247, -3.441045665385999985, 11.09087012887000157 ) ) ;
#20251 = EDGE_LOOP ( 'NONE', ( #45003, #25109, #50839, #63289 ) ) ;
#20252 = CARTESIAN_POINT ( 'NONE',  ( 8.739954719592999410, 3.122811675949999977, -6.006064052396999919 ) ) ;
#20253 = CARTESIAN_POINT ( 'NONE',  ( 0.000000000000000000, 1.460905701137619417, 2.533699434756940594 ) ) ;
#20254 = CARTESIAN_POINT ( 'NONE',  ( 9.070134780760145787, 3.647129767632899977, 8.851447081754479029 ) ) ;
#20255 = CARTESIAN_POINT ( 'NONE',  ( 18.29058466016600448, 10.98038933999040445, -3.892884224338386989 ) ) ;
#20256 = CARTESIAN_POINT ( 'NONE',  ( 10.09393020684899867, 5.250000000000000000, -7.500000000000000000 ) ) ;
#20257 = CARTESIAN_POINT ( 'NONE',  ( 11.28949010443639978, -2.999324937259999935, -7.574834962826040297 ) ) ;
#20258 = ORIENTED_EDGE ( 'NONE', *, *, #60529, .F. ) ;
#20259 = CARTESIAN_POINT ( 'NONE',  ( 2.111293599500000173, -2.202566789350000054, 2.837701071685999832 ) ) ;
#20260 = CARTESIAN_POINT ( 'NONE',  ( 7.565635841228000480, 3.206360348473000332, 5.681727837477000165 ) ) ;
#20262 = CARTESIAN_POINT ( 'NONE',  ( 11.26489721861000248, 3.710193004830000252, -11.71182445734000055 ) ) ;
#20261 = CARTESIAN_POINT ( 'NONE',  ( 5.000000000000000000, -1.199999999999999956, 9.776630298829998011 ) ) ;
#20263 = CARTESIAN_POINT ( 'NONE',  ( 18.17219575274255305, -2.599291946992130953, 13.65190342897825815 ) ) ;
#20264 = EDGE_CURVE ( 'NONE', #31044, #21661, #47544, .T. ) ;
#20265 = ORIENTED_EDGE ( 'NONE', *, *, #37553, .F. ) ;
#20266 = EDGE_CURVE ( 'NONE', #24059, #55227, #55095, .T. ) ;
#20267 = DIRECTION ( 'NONE',  ( -1.000000000000000000, 0.000000000000000000, 0.000000000000000000 ) ) ;
#20268 = CARTESIAN_POINT ( 'NONE',  ( 18.12600850643438477, -2.245563876552335802, -13.72409254399188150 ) ) ;
#20269 = CARTESIAN_POINT ( 'NONE',  ( 11.76133460557259980, 4.139849081322200419, 6.645166161828299778 ) ) ;
#20270 = LINE ( 'NONE', #30428, #31062 ) ;
#20271 = CARTESIAN_POINT ( 'NONE',  ( 7.860168146793000687, -2.263562268490999951, 8.007440964304000985 ) ) ;
#20272 = VERTEX_POINT ( 'NONE', #67268 ) ;
#20273 = CARTESIAN_POINT ( 'NONE',  ( 9.615066448851507630, -5.349942704376990044, -7.499996115248991124 ) ) ;
#20275 = CARTESIAN_POINT ( 'NONE',  ( 10.59393020684899867, -2.750000000000000000, -7.500000000000000000 ) ) ;
#20274 = CARTESIAN_POINT ( 'NONE',  ( 13.70003001321900271, 9.668726926528000476, 7.961868161445000425 ) ) ;
#20276 = B_SPLINE_CURVE_WITH_KNOTS ( 'NONE', 3,
 ( #18775, #60383, #24012, #66655 ),
 .UNSPECIFIED., .F., .F.,
 ( 4, 4 ),
 ( 0.000000000000000000, 1.000000000000000000 ),
 .UNSPECIFIED. ) ;
#20277 = CARTESIAN_POINT ( 'NONE',  ( 7.644425692886670731, -5.344399174148395382, 6.396633767784401847 ) ) ;
#20278 = CARTESIAN_POINT ( 'NONE',  ( 18.14038165173055717, -0.2193642558659226471, 13.89767506191629387 ) ) ;
#20279 = CARTESIAN_POINT ( 'NONE',  ( 23.81982966688499914, 3.247549704558999828, 13.03982134601000098 ) ) ;
#20280 = ORIENTED_EDGE ( 'NONE', *, *, #53282, .F. ) ;
#20281 = CARTESIAN_POINT ( 'NONE',  ( 2.210247277619000084, 2.108360286353999413, -2.286637680308000409 ) ) ;
#20282 = CARTESIAN_POINT ( 'NONE',  ( 12.23256516821459883, -3.293702443348299980, 6.787191910456499500 ) ) ;
#20283 = CARTESIAN_POINT ( 'NONE',  ( 11.41544519387737289, 4.732426395176744016, 7.982107551664254785 ) ) ;
#20284 = CARTESIAN_POINT ( 'NONE',  ( 10.81746213571000048, 5.100000000000000533, 6.571291218949999902 ) ) ;
#20285 = CARTESIAN_POINT ( 'NONE',  ( 10.23103300763299828, 4.692441239783899931, 6.773725604892799623 ) ) ;
#20286 = VECTOR ( 'NONE', #22455, 1000.000000000000000 ) ;
#20287 = LINE ( 'NONE', #58041, #37116 ) ;
#20288 = DIRECTION ( 'NONE',  ( 0.000000000000000000, 0.000000000000000000, -1.000000000000000000 ) ) ;
#20289 = CARTESIAN_POINT ( 'NONE',  ( 11.28627509987130040, 3.727547057523676433, -6.250000000000000000 ) ) ;
#20290 = DIRECTION ( 'NONE',  ( -1.000000000000000000, 0.000000000000000000, 0.000000000000000000 ) ) ;
#20291 = CARTESIAN_POINT ( 'NONE',  ( 24.45284546249100188, -12.43926702221000014, -3.093275132500000080 ) ) ;
#20293 = EDGE_CURVE ( 'NONE', #16266, #20309, #29227, .T. ) ;
#20292 = DIRECTION ( 'NONE',  ( 0.8843050097021416533, 0.1786785991673574547, 0.4313682974156609062 ) ) ;
#20294 = ORIENTED_EDGE ( 'NONE', *, *, #44885, .T. ) ;
#20295 = CARTESIAN_POINT ( 'NONE',  ( 5.700000000000000178, -13.04986661130000059, -1.811520473896000016 ) ) ;
#20296 = DIRECTION ( 'NONE',  ( -1.000000000000000000, 0.000000000000000000, 0.000000000000000000 ) ) ;
#20297 = VERTEX_POINT ( 'NONE', #58503 ) ;
#20298 =( NAMED_UNIT ( * ) SI_UNIT ( $, .STERADIAN. ) SOLID_ANGLE_UNIT ( ) );
#20299 = CARTESIAN_POINT ( 'NONE',  ( 10.62903166480609940, 3.135947233695900227, 7.439078678739090122 ) ) ;
#20300 = CIRCLE ( 'NONE', #66060, 13.27499874714999883 ) ;
#20301 = CARTESIAN_POINT ( 'NONE',  ( 10.40726830891999910, 3.797905842462999892, 5.889914049998000500 ) ) ;
#20302 = CARTESIAN_POINT ( 'NONE',  ( 11.08752642792000032, 2.871528932589999972, -6.302908019754999813 ) ) ;
#20303 = CARTESIAN_POINT ( 'NONE',  ( 9.682824781140627834, -4.607703288839251954, -8.129467220476902511 ) ) ;
#20304 = CARTESIAN_POINT ( 'NONE',  ( 9.687876499438001332, -5.912252057206999645, 7.772299417761000306 ) ) ;
#20305 = CARTESIAN_POINT ( 'NONE',  ( 18.26375634269467341, 0.1521017209118896429, -12.59908727444664045 ) ) ;
#20306 = CARTESIAN_POINT ( 'NONE',  ( 7.474999999999999645, 5.349999999999999645, 7.500000000000000000 ) ) ;
#20307 = CARTESIAN_POINT ( 'NONE',  ( 11.62994988689359843, -3.481863023525599843, -8.516279404258998653 ) ) ;
#20308 = CARTESIAN_POINT ( 'NONE',  ( 10.10000000000000142, 12.35000000006999876, 0.000000000000000000 ) ) ;
#20309 = VERTEX_POINT ( 'NONE', #5367 ) ;
#20310 = CARTESIAN_POINT ( 'NONE',  ( 11.02755399909320566, 4.133346405062087392, 6.221473734489903151 ) ) ;
#20311 = FACE_OUTER_BOUND ( 'NONE', #20579, .T. ) ;
#20312 = CARTESIAN_POINT ( 'NONE',  ( 10.14393020684899938, 5.250000000000000000, -7.500000000000000000 ) ) ;
#20313 = EDGE_CURVE ( 'NONE', #43884, #55241, #63043, .T. ) ;
#20314 = CARTESIAN_POINT ( 'NONE',  ( 17.97079960141759258, 1.890785106268465743, 12.45732622342820406 ) ) ;
#20315 = CARTESIAN_POINT ( 'NONE',  ( 12.21441178144105422, 2.942030139115487941, 13.68739795509152657 ) ) ;
#20316 = CARTESIAN_POINT ( 'NONE',  ( 9.576494682405000347, -4.593972507100000158, 5.662052676321000177 ) ) ;
#20317 = DIRECTION ( 'NONE',  ( 0.000000000000000000, 1.000000000000000000, 0.000000000000000000 ) ) ;
#20318 = CARTESIAN_POINT ( 'NONE',  ( 12.17125901970653068, -0.3547769576528356783, 13.99550803169339730 ) ) ;
#20319 = ORIENTED_EDGE ( 'NONE', *, *, #19880, .T. ) ;
#20320 = CARTESIAN_POINT ( 'NONE',  ( 12.58695046962341380, -1.794129438118917452, 12.47161187386927672 ) ) ;
#20321 = CARTESIAN_POINT ( 'NONE',  ( 12.80505043854143388, 1.816877544077282636, -13.85235828181317252 ) ) ;
#20322 = CARTESIAN_POINT ( 'NONE',  ( 10.74609562913000005, -4.263104965433000437, 9.276976808608999647 ) ) ;
#20323 = CARTESIAN_POINT ( 'NONE',  ( 15.49019623964617054, 9.469115506160944662, 8.198265202209981339 ) ) ;
#20324 = CARTESIAN_POINT ( 'NONE',  ( 11.07980110216399972, -4.739241740354600552, 7.951464549725199227 ) ) ;
#20325 = AXIS2_PLACEMENT_3D ( 'NONE', #50567, #55123, #18415 ) ;
#20326 = CARTESIAN_POINT ( 'NONE',  ( 12.42221671361158286, 0.6112845611542794266, 12.58516990776527145 ) ) ;
#20327 = B_SPLINE_CURVE_WITH_KNOTS ( 'NONE', 3,
 ( #22967, #58999, #59336, #54439, #44317, #48509 ),
 .UNSPECIFIED., .F., .F.,
 ( 4, 2, 4 ),
 ( 0.000000000000000000, 0.5000000000000000000, 1.000000000000000000 ),
 .UNSPECIFIED. ) ;
#20328 = CARTESIAN_POINT ( 'NONE',  ( 8.731616107288068918, 4.000002263255225898, 6.618420992905501343 ) ) ;
#20329 = DIRECTION ( 'NONE',  ( -1.000000000000000000, 0.000000000000000000, 0.000000000000000000 ) ) ;
#20330 = CARTESIAN_POINT ( 'NONE',  ( 12.35979995375149265, 1.912019040637406020, 12.45409236230133843 ) ) ;
#20331 = CARTESIAN_POINT ( 'NONE',  ( 9.487899699504998452, -4.011292643094999555, -9.373220388412001114 ) ) ;
#20332 = CARTESIAN_POINT ( 'NONE',  ( 11.09256785386839894, 3.167490253789400523, -8.060248494254899754 ) ) ;
#20333 = DIRECTION ( 'NONE',  ( 0.7071067811866525998, 0.000000000000000000, -0.7071067811864425456 ) ) ;
#20334 = CARTESIAN_POINT ( 'NONE',  ( 11.05392028041000074, 5.159483628325999938, -8.487146968478000986 ) ) ;
#20335 = CARTESIAN_POINT ( 'NONE',  ( 9.022734463322999332, 4.133249246727800141, -8.772253522581999974 ) ) ;
#20337 = CARTESIAN_POINT ( 'NONE',  ( 12.20055951530072669, 2.340869620879587831, 12.48721223319318874 ) ) ;
#20336 = CARTESIAN_POINT ( 'NONE',  ( 8.205992358809998777, -3.399999999999999911, 6.138278517058000538 ) ) ;
#20338 = CARTESIAN_POINT ( 'NONE',  ( 11.20158531382784162, -3.727547057523674212, -6.250000000000000000 ) ) ;
#20339 = EDGE_LOOP ( 'NONE', ( #29809, #14339, #40192, #24265 ) ) ;
#20340 = AXIS2_PLACEMENT_3D ( 'NONE', #39951, #12684, #65109 ) ;
#20341 = FACE_OUTER_BOUND ( 'NONE', #5858, .T. ) ;
#20342 = DIRECTION ( 'NONE',  ( 0.000000000000000000, 0.000000000000000000, 1.000000000000000000 ) ) ;
#20343 = AXIS2_PLACEMENT_3D ( 'NONE', #42510, #27123, #37943 ) ;
#20344 = CARTESIAN_POINT ( 'NONE',  ( 9.628002158527587895, 2.419316678802835963, -6.689506437318967436 ) ) ;
#20345 = CARTESIAN_POINT ( 'NONE',  ( 9.678329965421998082, 3.397808798486600335, 6.876242273533999416 ) ) ;
#20346 = CARTESIAN_POINT ( 'NONE',  ( 8.948279512853625661, 4.474797027487648293, -6.765085003841553757 ) ) ;
#20347 = EDGE_CURVE ( 'NONE', #31922, #44210, #60042, .T. ) ;
#20348 = EDGE_CURVE ( 'NONE', #34817, #44723, #63398, .T. ) ;
#20349 = CARTESIAN_POINT ( 'NONE',  ( 11.43330212365182952, 3.865573515333838639, -11.84353424803224719 ) ) ;
#20350 = CARTESIAN_POINT ( 'NONE',  ( 12.76358235960665333, -3.123961849445189731, 13.52113151862113938 ) ) ;
#20351 = CARTESIAN_POINT ( 'NONE',  ( 12.30281274455054152, 2.118998859546890490, 13.74704000636842594 ) ) ;
#20352 = CARTESIAN_POINT ( 'NONE',  ( 23.73412239512900257, 3.552994768190999686, -13.41889993560000072 ) ) ;
#20353 = VERTEX_POINT ( 'NONE', #35812 ) ;
#20354 = EDGE_CURVE ( 'NONE', #52223, #48042, #58428, .T. ) ;
#20355 = EDGE_CURVE ( 'NONE', #31036, #41936, #3320, .T. ) ;
#20356 = CARTESIAN_POINT ( 'NONE',  ( 4.900628625324999987, -0.6489656778686000438, -0.9304565553949000201 ) ) ;
#20357 = CARTESIAN_POINT ( 'NONE',  ( 8.642797255587998606, -2.721932483203000075, -7.445890648716809501 ) ) ;
#20358 = CARTESIAN_POINT ( 'NONE',  ( 7.100000000000000533, -12.03770622561999915, -3.722046322334000124 ) ) ;
#20359 = CARTESIAN_POINT ( 'NONE',  ( 11.23213259636990102, -4.907524392912299582, 7.005495010505599751 ) ) ;
#20360 = CARTESIAN_POINT ( 'NONE',  ( 18.14000279917953762, 2.720357798290597540, -12.39752072230842828 ) ) ;
#20361 = CARTESIAN_POINT ( 'NONE',  ( 8.693622321799001185, -3.165380393025999162, -6.276830322369005621 ) ) ;
#20362 = CARTESIAN_POINT ( 'NONE',  ( 18.17998003037112653, 2.509683781191140994, 12.44929946636232998 ) ) ;
#20363 = CARTESIAN_POINT ( 'NONE',  ( 12.20100803655143018, 2.660536037873024728, -13.63809770147455680 ) ) ;
#20364 = DIRECTION ( 'NONE',  ( 0.000000000000000000, 1.000000000000000000, 0.000000000000000000 ) ) ;
#20365 = CARTESIAN_POINT ( 'NONE',  ( 9.888320559623000605, -5.105186397454999359, -8.895598708036001057 ) ) ;
#20366 = CARTESIAN_POINT ( 'NONE',  ( 9.517197013793815330, -5.205368702674399550, 8.206177812345709199 ) ) ;
#20367 = CARTESIAN_POINT ( 'NONE',  ( 12.58342633946451983, 0.6953657024348841587, -13.98272072176121483 ) ) ;
#20368 = CARTESIAN_POINT ( 'NONE',  ( 23.64390295928378904, 13.40130543866907153, 3.849660382617301480 ) ) ;
#20369 = CARTESIAN_POINT ( 'NONE',  ( 11.09999999883999955, 8.820692016227001275, 6.691733774959000236 ) ) ;
#20370 = CARTESIAN_POINT ( 'NONE',  ( 2.419891126640250523, 1.842658540278711010, -2.994770506591985626 ) ) ;
#20371 = EDGE_CURVE ( 'NONE', #51740, #45182, #42586, .T. ) ;
#20372 = ORIENTED_EDGE ( 'NONE', *, *, #14716, .F. ) ;
#20373 = CARTESIAN_POINT ( 'NONE',  ( 9.111654719595000174, 4.989193221215000307, -6.287302145481000082 ) ) ;
#20374 = CARTESIAN_POINT ( 'NONE',  ( 11.15364694612719809, -4.804498860841600383, 7.178938988280099132 ) ) ;
#20375 = ORIENTED_EDGE ( 'NONE', *, *, #13974, .T. ) ;
#20376 = AXIS2_PLACEMENT_3D ( 'NONE', #6323, #43753, #23106 ) ;
#20377 = CARTESIAN_POINT ( 'NONE',  ( 7.949443559528000414, 4.160078903546944318, -6.143289804786609132 ) ) ;
#20378 = CARTESIAN_POINT ( 'NONE',  ( 18.14566850323240033, 2.942004589604676923, -13.68740344564952593 ) ) ;
#20379 = EDGE_LOOP ( 'NONE', ( #12552, #25301, #61068, #27549 ) ) ;
#20380 = CARTESIAN_POINT ( 'NONE',  ( 12.80000000000000071, -10.78295181803999903, 4.410266442048000002 ) ) ;
#20381 = CARTESIAN_POINT ( 'NONE',  ( 9.392285841233000809, 5.775964236216999836, -8.174909295649001706 ) ) ;
#20382 = CARTESIAN_POINT ( 'NONE',  ( 8.649445371194000032, 5.100000000000000533, -6.459601070175000181 ) ) ;
#20383 = CARTESIAN_POINT ( 'NONE',  ( 11.15278751119019773, -4.790480620979200133, -7.913556523549700294 ) ) ;
#20384 = CARTESIAN_POINT ( 'NONE',  ( 13.49994651945300284, -12.07042783918999795, -2.492331243371999960 ) ) ;
#20385 = FACE_OUTER_BOUND ( 'NONE', #20251, .T. ) ;
#20386 = VERTEX_POINT ( 'NONE', #9572 ) ;
#20387 = FACE_OUTER_BOUND ( 'NONE', #46186, .T. ) ;
#20388 = CARTESIAN_POINT ( 'NONE',  ( 9.983079719591000156, 5.002683760508999988, -8.912673867568997821 ) ) ;
#20389 = ORIENTED_EDGE ( 'NONE', *, *, #56434, .T. ) ;
#20390 = AXIS2_PLACEMENT_3D ( 'NONE', #24583, #45906, #24235 ) ;
#20391 = CARTESIAN_POINT ( 'NONE',  ( 11.02205778663999958, 2.309481324353999554, -7.515673747780000191 ) ) ;
#20392 = PRESENTATION_STYLE_ASSIGNMENT (( #46629 ) ) ;
#20393 = ORIENTED_EDGE ( 'NONE', *, *, #63286, .T. ) ;
#20394 = CARTESIAN_POINT ( 'NONE',  ( 9.250696787962999323, 4.219671260427300119, 8.760209873321999297 ) ) ;
#20395 = CARTESIAN_POINT ( 'NONE',  ( 17.81301359322647215, -3.153051599267181260, -12.19911286921121274 ) ) ;
#20396 = EDGE_CURVE ( 'NONE', #20484, #46842, #30914, .T. ) ;
#20397 = CARTESIAN_POINT ( 'NONE',  ( 5.699999545467999695, 0.000000000000000000, 0.000000000000000000 ) ) ;
#20398 = EDGE_CURVE ( 'NONE', #55782, #25788, #68278, .T. ) ;
#20399 = FACE_OUTER_BOUND ( 'NONE', #39655, .T. ) ;
#20400 = CARTESIAN_POINT ( 'NONE',  ( 11.68114303127866194, -4.620698129841968260, 6.880574739649333083 ) ) ;
#20401 = ORIENTED_EDGE ( 'NONE', *, *, #7179, .T. ) ;
#20402 = CARTESIAN_POINT ( 'NONE',  ( 12.04183425709900135, 11.69157926155999938, -4.070931047779999368 ) ) ;
#20403 = CARTESIAN_POINT ( 'NONE',  ( 11.06878584122999953, 5.318802051720999735, -7.168446171767000052 ) ) ;
#20404 = CARTESIAN_POINT ( 'NONE',  ( 11.09034140454999928, -5.289188190482000174, -5.109507762678999754 ) ) ;
#20405 = CARTESIAN_POINT ( 'NONE',  ( 8.896714042595458949, 3.863849893574821781, 8.546714100015048388 ) ) ;
#20406 = CARTESIAN_POINT ( 'NONE',  ( 18.05935379312178668, 0.5247499651446875246, 13.99016470477802443 ) ) ;
#20407 = CARTESIAN_POINT ( 'NONE',  ( 17.86873602477000134, 3.252323392204000019, 11.33729809900999896 ) ) ;
#20408 = CARTESIAN_POINT ( 'NONE',  ( 9.675541251098000117, -4.656741678598999457, -8.653222148251000334 ) ) ;
#20409 = ORIENTED_EDGE ( 'NONE', *, *, #58785, .T. ) ;
#20410 = ORIENTED_EDGE ( 'NONE', *, *, #47968, .T. ) ;
#20411 = B_SPLINE_CURVE_WITH_KNOTS ( 'NONE', 3,
 ( #63531, #47121, #15643, #15303, #20196 ),
 .UNSPECIFIED., .F., .F.,
 ( 4, 1, 4 ),
 ( 0.000000000000000000, 0.5000000000000000000, 1.000000000000000000 ),
 .UNSPECIFIED. ) ;
#20412 = CARTESIAN_POINT ( 'NONE',  ( 10.21398584123000042, 3.990126737362999609, -8.809457313313998839 ) ) ;
#20413 = FACE_OUTER_BOUND ( 'NONE', #58284, .T. ) ;
#20414 = CARTESIAN_POINT ( 'NONE',  ( 12.33541982640536538, -2.912513636887091639, 13.57727066180282982 ) ) ;
#20415 = CARTESIAN_POINT ( 'NONE',  ( 25.37702747131099912, 8.494993186710001254, -7.921081225816001492 ) ) ;
#20416 = CARTESIAN_POINT ( 'NONE',  ( 10.68035971519489813, 4.678140486081599825, -6.371865185335000348 ) ) ;
#20417 = CARTESIAN_POINT ( 'NONE',  ( 9.282063610504998508, 4.355629271815800507, -8.290718512198798962 ) ) ;
#20419 = CARTESIAN_POINT ( 'NONE',  ( 8.616995677562000466, 4.876077402042000131, 5.996974966532000018 ) ) ;
#20418 = CARTESIAN_POINT ( 'NONE',  ( 9.523797255587998833, -2.859210004667000149, 7.548297453605989027 ) ) ;
#20420 = CARTESIAN_POINT ( 'NONE',  ( 7.736994134724001881, -2.836597362165000913, 6.822571831264003350 ) ) ;
#20421 = ORIENTED_EDGE ( 'NONE', *, *, #28495, .F. ) ;
#20422 = AXIS2_PLACEMENT_3D ( 'NONE', #3736, #10022, #41163 ) ;
#20423 = CARTESIAN_POINT ( 'NONE',  ( 11.09999999999999964, -2.700688486617000006, 5.124965750789000296 ) ) ;
#20424 = CARTESIAN_POINT ( 'NONE',  ( 10.37122746244000027, -3.416394293729999809, -5.010285895928999977 ) ) ;
#20425 = CARTESIAN_POINT ( 'NONE',  ( 9.844904806657000407, -2.626678530444999993, -7.387134320497999340 ) ) ;
#20426 = CARTESIAN_POINT ( 'NONE',  ( 7.956227822045499387, 4.972404917557740944, 6.449457438518853891 ) ) ;
#20427 = CARTESIAN_POINT ( 'NONE',  ( 18.17813913392090797, -2.550022942166513040, -12.43977370302252439 ) ) ;
#20428 = CARTESIAN_POINT ( 'NONE',  ( 4.600000127571202135, 13.89999852641999922, 0.000000000000000000 ) ) ;
#20429 = CARTESIAN_POINT ( 'NONE',  ( 16.07488484168399978, -3.504106430365000246, -11.16639795596000084 ) ) ;
#20430 = EDGE_CURVE ( 'NONE', #45133, #28965, #848, .T. ) ;
#20431 = EDGE_CURVE ( 'NONE', #55564, #47308, #4187, .T. ) ;
#20432 = CARTESIAN_POINT ( 'NONE',  ( 25.39994675531830737, 10.74016667918497525, -3.821986399293599845 ) ) ;
#20433 = CARTESIAN_POINT ( 'NONE',  ( 7.968428156063966483, 2.973737269781533410, -6.513357571637738097 ) ) ;
#20434 = AXIS2_PLACEMENT_3D ( 'NONE', #14541, #35858, #25362 ) ;
#20435 = CARTESIAN_POINT ( 'NONE',  ( 11.02934687351650389, -3.836375382625533348, 6.250000000000000000 ) ) ;
#20436 = LINE ( 'NONE', #51228, #51034 ) ;
#20437 = CARTESIAN_POINT ( 'NONE',  ( 17.74710428554446295, 3.180431966548184608, 12.19205794678931376 ) ) ;
#20438 = CARTESIAN_POINT ( 'NONE',  ( 3.162702707610999919, 2.867491953926999848, -1.874115396504999920 ) ) ;
#20439 = VERTEX_POINT ( 'NONE', #14131 ) ;
#20440 = CARTESIAN_POINT ( 'NONE',  ( 12.55608787177197172, 0.5733651658914313831, -12.68257300503909946 ) ) ;
#20441 = CARTESIAN_POINT ( 'NONE',  ( 12.27404183469016274, -2.829784921991532087, -12.36859113742059080 ) ) ;
#20442 = CARTESIAN_POINT ( 'NONE',  ( 10.90000000000000036, 0.2999999999999999889, -4.902439024389999567 ) ) ;
#20443 = DIRECTION ( 'NONE',  ( 1.000000000000000000, 0.000000000000000000, 0.000000000000000000 ) ) ;
#20444 = CARTESIAN_POINT ( 'NONE',  ( 10.12544718489628437, 5.350147103445117125, -7.676667778836200995 ) ) ;
#20445 = EDGE_LOOP ( 'NONE', ( #29591, #56874 ) ) ;
#20446 = DIRECTION ( 'NONE',  ( 0.000000000000000000, -1.000000000000000000, 0.000000000000000000 ) ) ;
#20447 = CARTESIAN_POINT ( 'NONE',  ( 0.6989630074183774688, -2.794206512036536250, 2.158557316518020741 ) ) ;
#20448 = ADVANCED_FACE ( 'NONE', ( #45941 ), #9557, .T. ) ;
#20449 = CARTESIAN_POINT ( 'NONE',  ( 13.73959992722299894, -11.36892293904000084, -2.362143082378000081 ) ) ;
#20450 = DIRECTION ( 'NONE',  ( 0.000000000000000000, -1.000000000000000000, 0.000000000000000000 ) ) ;
#20451 = CARTESIAN_POINT ( 'NONE',  ( 11.35034208742529849, 3.369365911179700301, -8.491292290686200062 ) ) ;
#20452 = ORIENTED_EDGE ( 'NONE', *, *, #37553, .T. ) ;
#20453 = CARTESIAN_POINT ( 'NONE',  ( 11.09648096125000016, -3.099777420064000033, 6.097103007060000301 ) ) ;
#20454 = ORIENTED_EDGE ( 'NONE', *, *, #19257, .T. ) ;
#20455 = CARTESIAN_POINT ( 'NONE',  ( 8.498348583768846609, -3.349589723688465526, 5.969486571880056935 ) ) ;
#20456 = CARTESIAN_POINT ( 'NONE',  ( 7.374102686541000651, -4.389298280625000714, 9.135255728583000945 ) ) ;
#20457 = CARTESIAN_POINT ( 'NONE',  ( 15.72922381500400313, 8.763625284509998892, 7.896085856502000233 ) ) ;
#20458 = ORIENTED_EDGE ( 'NONE', *, *, #50273, .T. ) ;
#20459 = CARTESIAN_POINT ( 'NONE',  ( 8.460086291669814074, 4.111641193682548767, -9.252673147083232408 ) ) ;
#20460 = DIRECTION ( 'NONE',  ( 0.000000000000000000, -1.000000000000000000, 0.000000000000000000 ) ) ;
#20461 = CARTESIAN_POINT ( 'NONE',  ( 8.261229719591000276, 4.814347755891000169, -8.757164289523000633 ) ) ;
#20462 = CYLINDRICAL_SURFACE ( 'NONE', #64358, 0.6999999999999992895 ) ;
#20463 = CYLINDRICAL_SURFACE ( 'NONE', #46300, 0.6999999999999992895 ) ;
#20464 = ORIENTED_EDGE ( 'NONE', *, *, #49273, .T. ) ;
#20465 = CARTESIAN_POINT ( 'NONE',  ( 10.68403590588000007, -5.436611040123999317, 8.578433628717998971 ) ) ;
#20466 = VECTOR ( 'NONE', #56678, 1000.000000000000000 ) ;
#20467 = CARTESIAN_POINT ( 'NONE',  ( 12.18999301580812222, -2.611634498318802677, -13.64910281353073707 ) ) ;
#20468 = DIRECTION ( 'NONE',  ( 0.000000000000000000, 1.000000000000000000, 0.000000000000000000 ) ) ;
#20469 = ORIENTED_EDGE ( 'NONE', *, *, #41537, .F. ) ;
#20470 = CARTESIAN_POINT ( 'NONE',  ( 10.93146935944000120, -2.472881306517999978, -7.514158774805000718 ) ) ;
#20471 = AXIS2_PLACEMENT_3D ( 'NONE', #36762, #21022, #47598 ) ;
#20472 = CARTESIAN_POINT ( 'NONE',  ( 10.99239898671664228, -6.454658201019197961, -5.240588185469198024 ) ) ;
#20473 = ORIENTED_EDGE ( 'NONE', *, *, #42342, .F. ) ;
#20474 = DIRECTION ( 'NONE',  ( 1.000000000000000000, 0.000000000000000000, 0.000000000000000000 ) ) ;
#20475 = CARTESIAN_POINT ( 'NONE',  ( 17.80428097310739588, 0.5732560958663720507, -13.88408533439707071 ) ) ;
#20476 = CARTESIAN_POINT ( 'NONE',  ( 5.479592101182999997, -0.7872145294400999527, 1.288886465870000109 ) ) ;
#20477 = CARTESIAN_POINT ( 'NONE',  ( 5.105026506350000659, -1.500000000000000000, 0.000000000000000000 ) ) ;
#20478 = DIRECTION ( 'NONE',  ( 0.000000000000000000, 0.7914851585299630399, -0.6111883865280813843 ) ) ;
#20479 = CARTESIAN_POINT ( 'NONE',  ( 3.084306799210666750, 1.762666431298138825, 3.058252359239908014 ) ) ;
#20480 = B_SPLINE_CURVE_WITH_KNOTS ( 'NONE', 3,
 ( #10625, #141, #37202, #55277, #28364, #32313, #42792, #49680, #58870, #66098, #49327 ),
 .UNSPECIFIED., .F., .F.,
 ( 4, 1, 1, 1, 1, 1, 1, 1, 4 ),
 ( 0.000000000000000000, 0.1099981905781512725, 0.2399987910428944826, 0.3699993915076381090, 0.4999999919727210473, 0.6300005924374643129, 0.7600011929022079116, 0.8900017933672909054, 1.000000000000000000 ),
 .UNSPECIFIED. ) ;
#20481 = EDGE_CURVE ( 'NONE', #63766, #9350, #24619, .T. ) ;
#20482 = CARTESIAN_POINT ( 'NONE',  ( 12.42259655075931590, 2.994741173188553152, 13.55594337657171700 ) ) ;
#20483 = CARTESIAN_POINT ( 'NONE',  ( 10.12670810574000058, -3.117521507207000386, 8.613544937223998943 ) ) ;
#20484 = VERTEX_POINT ( 'NONE', #30897 ) ;
#20485 = CARTESIAN_POINT ( 'NONE',  ( 3.389296384485166236, -1.580232515686062822, -3.171881757336630248 ) ) ;
#20486 = EDGE_LOOP ( 'NONE', ( #28982, #56142, #66650, #9070 ) ) ;
#20487 = CARTESIAN_POINT ( 'NONE',  ( 10.50244247011999832, 2.268911387573000038, 7.824865741583000300 ) ) ;
#20488 = CIRCLE ( 'NONE', #10449, 11.30000000000000604 ) ;
#20489 = CARTESIAN_POINT ( 'NONE',  ( 11.32240614981507676, -3.267563509902000174, -7.982093918858203629 ) ) ;
#20490 = CARTESIAN_POINT ( 'NONE',  ( 9.219485841232998524, 3.892978337449999771, -8.893414073324001023 ) ) ;
#20491 = CARTESIAN_POINT ( 'NONE',  ( 2.642422881787000133, 0.3228049546832999495, 3.693971431390000060 ) ) ;
#20492 = DIRECTION ( 'NONE',  ( 0.000000000000000000, 0.2461538461537955413, -0.9692307692307821076 ) ) ;
#20493 = DIRECTION ( 'NONE',  ( 0.000000000000000000, -0.001485959642859940649, 0.9999988959613604900 ) ) ;
#20494 = CIRCLE ( 'NONE', #34985, 1.000000000000000000 ) ;
#20495 = CARTESIAN_POINT ( 'NONE',  ( 9.526243286405723154, -2.763914616263006607, -8.778142438547300586 ) ) ;
#20496 = ORIENTED_EDGE ( 'NONE', *, *, #216, .F. ) ;
#20497 = CARTESIAN_POINT ( 'NONE',  ( 12.54853131227892327, 0.5702303675593314303, 13.88425454623471111 ) ) ;
#20498 = CARTESIAN_POINT ( 'NONE',  ( 10.99349279008999858, -4.332388355267299929, 6.265968249244999733 ) ) ;
#20499 = CARTESIAN_POINT ( 'NONE',  ( 10.28579080656071199, 5.375703358358307149, -6.377628306183688700 ) ) ;
#20500 = CARTESIAN_POINT ( 'NONE',  ( 16.13936233968600220, 9.023335130797001113, 8.741328814538000813 ) ) ;
#20501 = CARTESIAN_POINT ( 'NONE',  ( 8.656816940379998826, -5.329429281359999493, 6.027400270608000099 ) ) ;
#20503 = DIRECTION ( 'NONE',  ( -1.000000000000000000, 0.000000000000000000, 0.000000000000000000 ) ) ;
#20502 = CARTESIAN_POINT ( 'NONE',  ( 10.62697636434999993, 3.142921793056999924, 8.668445734229999644 ) ) ;
#20504 = CARTESIAN_POINT ( 'NONE',  ( 11.06379841651039797, 3.598362324325699912, -8.567697191971999970 ) ) ;
#20505 = CARTESIAN_POINT ( 'NONE',  ( 11.16486084871730000, -2.792989229543000107, -7.174999999999999822 ) ) ;
#20506 = CARTESIAN_POINT ( 'NONE',  ( 10.05826717315599872, 3.340104753140699767, -6.937642277832399174 ) ) ;
#20507 = CARTESIAN_POINT ( 'NONE',  ( 18.14493211602550460, 0.4188397444781293832, 12.59305179380755391 ) ) ;
#20508 = CARTESIAN_POINT ( 'NONE',  ( 6.849078002582999147, 0.7730190231004000490, -1.183954730321999937 ) ) ;
#20509 = DIRECTION ( 'NONE',  ( 0.000000000000000000, -1.000000000000000000, 0.000000000000000000 ) ) ;
#20510 = CARTESIAN_POINT ( 'NONE',  ( 0.2066231058121046349, -2.618168328974044765E-06, -3.206444164765644977 ) ) ;
#20511 = ORIENTED_EDGE ( 'NONE', *, *, #48444, .T. ) ;
#20512 = CARTESIAN_POINT ( 'NONE',  ( 9.160311019873999427, -4.122021308488999836, 9.013573548576999883 ) ) ;
#20513 = ADVANCED_FACE ( 'NONE', ( #3962 ), #34777, .T. ) ;
#20514 = EDGE_CURVE ( 'NONE', #56588, #59750, #61674, .T. ) ;
#20515 = CARTESIAN_POINT ( 'NONE',  ( 4.500000000000000000, 0.000000000000000000, 0.000000000000000000 ) ) ;
#20516 = CARTESIAN_POINT ( 'NONE',  ( 7.307500000000000107, -0.2500000000000000000, -3.149999999999999911 ) ) ;
#20517 = ORIENTED_EDGE ( 'NONE', *, *, #54696, .F. ) ;
#20518 = AXIS2_PLACEMENT_3D ( 'NONE', #51105, #24533, #2180 ) ;
#20519 = CARTESIAN_POINT ( 'NONE',  ( 18.44718133169100227, 2.901187496916000086, 12.12896678136999995 ) ) ;
#20520 = CARTESIAN_POINT ( 'NONE',  ( 10.56080513895999928, 5.026880838510000338, 8.070849345005600028 ) ) ;
#20521 = CARTESIAN_POINT ( 'NONE',  ( 11.09178278040999999, 4.578541652803000517, -8.908598806528001290 ) ) ;
#20522 = EDGE_LOOP ( 'NONE', ( #13186, #10632, #51903, #58698 ) ) ;
#20523 = CARTESIAN_POINT ( 'NONE',  ( 23.60000000000000142, -1.954837874162284272, -13.79162083333110367 ) ) ;
#20524 = CARTESIAN_POINT ( 'NONE',  ( 25.46372797112000086, -8.354608193938998895, 8.148457429720000533 ) ) ;
#20525 = CARTESIAN_POINT ( 'NONE',  ( 11.25656651104150008, 4.126085365637900182, 8.771777834828998976 ) ) ;
#20526 = CARTESIAN_POINT ( 'NONE',  ( 10.57893103570000015, -4.649956431060000561, 5.681096060554999383 ) ) ;
#20527 = CARTESIAN_POINT ( 'NONE',  ( 8.207510841230000409, 5.944584532500000407, 7.106843289410999631 ) ) ;
#20528 = ORIENTED_EDGE ( 'NONE', *, *, #68436, .F. ) ;
#20529 = CARTESIAN_POINT ( 'NONE',  ( 7.834146155765201236, -4.877287769396863482, 6.428085084284855810 ) ) ;
#20530 = CARTESIAN_POINT ( 'NONE',  ( 7.069639158769000176, 2.101490574575000103, -7.427795877530000368 ) ) ;
#20531 = ADVANCED_FACE ( 'NONE', ( #51864 ), #56933, .F. ) ;
#20532 = CARTESIAN_POINT ( 'NONE',  ( 8.111474497621481206, -4.780564565339348704, 5.942454047483178847 ) ) ;
#20533 = AXIS2_PLACEMENT_3D ( 'NONE', #41505, #56900, #36260 ) ;
#20534 = CARTESIAN_POINT ( 'NONE',  ( 9.727380199234000102, -2.867101906753999785, 7.642395078236999595 ) ) ;
#20535 = EDGE_LOOP ( 'NONE', ( #16243, #36501, #65014, #63874 ) ) ;
#20536 = CARTESIAN_POINT ( 'NONE',  ( 16.34794651623100137, -3.644047358192000097, -12.02362153922000054 ) ) ;
#20537 = CARTESIAN_POINT ( 'NONE',  ( 7.000000000000000000, -9.735955015381000166, 5.735955015381000166 ) ) ;
#20538 = ORIENTED_EDGE ( 'NONE', *, *, #67214, .T. ) ;
#20539 = EDGE_CURVE ( 'NONE', #16046, #62494, #64237, .T. ) ;
#20540 = DIRECTION ( 'NONE',  ( -0.000000000000000000, -0.000000000000000000, 1.000000000000000000 ) ) ;
#20541 = FACE_OUTER_BOUND ( 'NONE', #65677, .T. ) ;
#20542 = ORIENTED_EDGE ( 'NONE', *, *, #24966, .F. ) ;
#20543 = CARTESIAN_POINT ( 'NONE',  ( 18.12461517476719308, 0.2575405707509131892, -13.89679341043304106 ) ) ;
#20544 = DIRECTION ( 'NONE',  ( 1.000000000000000000, 0.000000000000000000, 0.000000000000000000 ) ) ;
#20545 = CARTESIAN_POINT ( 'NONE',  ( 2.446806799209917394, 0.9161175952574844850, -3.408904368339102930 ) ) ;
#20546 = CARTESIAN_POINT ( 'NONE',  ( 11.59966954483535773, 4.638989336656000440, -6.514072057539499916 ) ) ;
#20547 = VECTOR ( 'NONE', #27764, 1000.000000000000000 ) ;
#20548 = CARTESIAN_POINT ( 'NONE',  ( 11.02799293566599914, -3.193321847920899792, 6.510429574318199464 ) ) ;
#20549 = CARTESIAN_POINT ( 'NONE',  ( 8.683840764065545059, -5.715804157004961361, 7.158468558862815634 ) ) ;
#20550 = CARTESIAN_POINT ( 'NONE',  ( 11.63764426047339917, -3.386171819220400003, 6.538488127609999978 ) ) ;
#20551 = CARTESIAN_POINT ( 'NONE',  ( 10.78014141025500017, -3.582647672488299850, 6.756653759087999589 ) ) ;
#20552 = ORIENTED_EDGE ( 'NONE', *, *, #14019, .F. ) ;
#20553 = CARTESIAN_POINT ( 'NONE',  ( 9.164757945270768147, -2.782574339883950199, -7.172825509854745540 ) ) ;
#20554 = CARTESIAN_POINT ( 'NONE',  ( 17.78895972987641017, -0.6824382159985085128, 12.58151825845911453 ) ) ;
#20555 = DIRECTION ( 'NONE',  ( -1.000000000000000000, 0.000000000000000000, 0.000000000000000000 ) ) ;
#20556 = ORIENTED_EDGE ( 'NONE', *, *, #48532, .T. ) ;
#20557 = CARTESIAN_POINT ( 'NONE',  ( 12.21328932544282253, -2.701359397734038659, -12.40237271074984982 ) ) ;
#20558 = CARTESIAN_POINT ( 'NONE',  ( 18.26547113879826867, 3.186161613543892379, 11.20588962290447554 ) ) ;
#20559 = DIRECTION ( 'NONE',  ( 1.000000000000000000, 1.776356839339000149E-14, 1.776356839339000149E-14 ) ) ;
#20560 = CARTESIAN_POINT ( 'NONE',  ( 10.71684687351633869, 4.768183399968648040, 8.499583552997721725 ) ) ;
#20561 = CARTESIAN_POINT ( 'NONE',  ( 12.20052126010794780, -2.341019711503391942, -13.70584597024486939 ) ) ;
#20562 = CARTESIAN_POINT ( 'NONE',  ( 10.82595391537419971, -3.283439621430300104, -7.986661909549199301 ) ) ;
#20563 = CARTESIAN_POINT ( 'NONE',  ( 18.40806533023902603, 3.252985697212876559, 12.09525697359294760 ) ) ;
#20564 = CARTESIAN_POINT ( 'NONE',  ( 18.21613312502040571, -2.776914653343700135, 12.29020858420810924 ) ) ;
#20565 = ORIENTED_EDGE ( 'NONE', *, *, #11669, .T. ) ;
#20566 = ORIENTED_EDGE ( 'NONE', *, *, #46799, .F. ) ;
#20567 = AXIS2_PLACEMENT_3D ( 'NONE', #14837, #4332, #56805 ) ;
#20568 =( LENGTH_UNIT ( ) NAMED_UNIT ( * ) SI_UNIT ( .MILLI., .METRE. ) );
#20569 = CARTESIAN_POINT ( 'NONE',  ( 10.90000000000000036, -0.2500000000000000000, 4.902439024389999567 ) ) ;
#20570 = DIRECTION ( 'NONE',  ( -1.000000000000000000, 0.000000000000000000, 0.000000000000000000 ) ) ;
#20571 = CARTESIAN_POINT ( 'NONE',  ( 9.741003491525001223, 3.588532719919999892, -8.800216240366001585 ) ) ;
#20572 = DIRECTION ( 'NONE',  ( 0.8480635683783770418, 0.000000000000000000, 0.5298945026977860406 ) ) ;
#20573 = CARTESIAN_POINT ( 'NONE',  ( 18.16680584898029593, 2.371606440122839832, 12.48054868302275722 ) ) ;
#20574 = CARTESIAN_POINT ( 'NONE',  ( 24.33723891670900130, -12.30467408780000049, 3.219315065404000364 ) ) ;
#20575 = EDGE_CURVE ( 'NONE', #52805, #58951, #28349, .T. ) ;
#20576 = CARTESIAN_POINT ( 'NONE',  ( 10.49785886974000171, 3.776281431161999880, 5.717632172928999168 ) ) ;
#20577 = ORIENTED_EDGE ( 'NONE', *, *, #30982, .T. ) ;
#20578 = CARTESIAN_POINT ( 'NONE',  ( 8.677205275792569950, -4.798748112014699529, -6.411199558850072755 ) ) ;
#20579 = EDGE_LOOP ( 'NONE', ( #24181, #24070, #32797, #46210 ) ) ;
#20580 = CARTESIAN_POINT ( 'NONE',  ( 12.24413029362360561, -2.775858423521468943, 12.38303112237259640 ) ) ;
#20581 = CARTESIAN_POINT ( 'NONE',  ( 8.842468108405999061, -3.165798890946399879, -7.736255015838599647 ) ) ;
#20582 = B_SPLINE_CURVE_WITH_KNOTS ( 'NONE', 3,
 ( #38595, #59918, #7467, #23899, #50132, #18317 ),
 .UNSPECIFIED., .F., .F.,
 ( 4, 2, 4 ),
 ( 0.000000000000000000, 0.5000000000000000000, 1.000000000000000000 ),
 .UNSPECIFIED. ) ;
#20583 = CARTESIAN_POINT ( 'NONE',  ( 10.22398792753999963, 5.507894434963000130, 6.589802269404000157 ) ) ;
#20584 = CARTESIAN_POINT ( 'NONE',  ( 11.80878751119029957, -5.041025164610000608, 6.955365841266999638 ) ) ;
#20585 = CARTESIAN_POINT ( 'NONE',  ( 11.53935620825161124, -11.69940330537451878, -1.870140110077453732 ) ) ;
#20586 = VECTOR ( 'NONE', #11349, 1000.000000000000000 ) ;
#20587 = CARTESIAN_POINT ( 'NONE',  ( 9.934206403597999113, -5.120430559539999926, -8.883390070891001855 ) ) ;
#20588 = CARTESIAN_POINT ( 'NONE',  ( 10.09964828895399869, 5.121614868497999851, -8.112615456209400833 ) ) ;
#20589 = CARTESIAN_POINT ( 'NONE',  ( 12.80505043854144276, -0.6250000000000006661, 12.67928921589117586 ) ) ;
#20590 = AXIS2_PLACEMENT_3D ( 'NONE', #510, #48751, #54332 ) ;
#20591 = CARTESIAN_POINT ( 'NONE',  ( 5.699999772733999492, -12.03770622561999915, -3.722046322334000124 ) ) ;
#20592 = CARTESIAN_POINT ( 'NONE',  ( 8.169376727357384738, 5.058218492709852576, -8.358305702195062636 ) ) ;
#20593 = CARTESIAN_POINT ( 'NONE',  ( 11.44446797630000034, -3.649424658612000272, 11.12042579671999931 ) ) ;
#20594 = ORIENTED_EDGE ( 'NONE', *, *, #51447, .T. ) ;
#20595 = CARTESIAN_POINT ( 'NONE',  ( 9.576420280414000175, 4.861259245430999520, -8.806664389576001284 ) ) ;
#20596 = CARTESIAN_POINT ( 'NONE',  ( -0.000000000000000000, -2.319407620233877587, 1.781870588985297932 ) ) ;
#20597 = EDGE_CURVE ( 'NONE', #53568, #37636, #45841, .T. ) ;
#20598 = EDGE_CURVE ( 'NONE', #28877, #9679, #34173, .T. ) ;
#20599 = DIRECTION ( 'NONE',  ( 0.000000000000000000, 1.000000000000000000, 0.000000000000000000 ) ) ;
#20600 = CARTESIAN_POINT ( 'NONE',  ( 12.75601868327514410, -3.199663661910128187, -12.18696649917218977 ) ) ;
#20601 = CARTESIAN_POINT ( 'NONE',  ( 12.09999999999999787, -3.195619894033321806, 8.322973907256258741 ) ) ;
#20602 = CARTESIAN_POINT ( 'NONE',  ( 10.57149279008999798, -4.296686446741600385, -8.601484120896000007 ) ) ;
#20603 = ORIENTED_EDGE ( 'NONE', *, *, #54123, .F. ) ;
#20604 = EDGE_CURVE ( 'NONE', #63146, #49185, #40256, .T. ) ;
#20605 = CARTESIAN_POINT ( 'NONE',  ( 5.602978689601446405, -12.13075210502338841, 3.749558893020384254 ) ) ;
#20606 = CARTESIAN_POINT ( 'NONE',  ( 8.271698341229999585, 5.629399530851999955, 8.631829656822000985 ) ) ;
#20609 = CARTESIAN_POINT ( 'NONE',  ( 13.75930817923600102, -9.623971528738000103, -8.076134841847999013 ) ) ;
#20608 = CARTESIAN_POINT ( 'NONE',  ( 8.971339158776000744, 4.082930418187999955, -6.104944817728999773 ) ) ;
#20607 = PRODUCT_DEFINITION_CONTEXT ( 'detailed design', #23077, 'design' ) ;
#20610 = CARTESIAN_POINT ( 'NONE',  ( 15.89979320885400327, 3.824231472901999496, 11.71686814605000038 ) ) ;
#20611 = ORIENTED_EDGE ( 'NONE', *, *, #39881, .T. ) ;
#20612 = B_SPLINE_CURVE_WITH_KNOTS ( 'NONE', 3,
 ( #15253, #36575, #41140, #46729 ),
 .UNSPECIFIED., .F., .F.,
 ( 4, 4 ),
 ( 0.000000000000000000, 1.000000000000000000 ),
 .UNSPECIFIED. ) ;
#20613 = CARTESIAN_POINT ( 'NONE',  ( 9.792569055495000896, 3.463432304708999876, 6.184396499233999478 ) ) ;
#20614 = CARTESIAN_POINT ( 'NONE',  ( 18.17921951168942130, -2.461818733276639914, -13.68145094671735329 ) ) ;
#20615 = CARTESIAN_POINT ( 'NONE',  ( 10.38287885159599888, 4.860099138268600072, 7.602606670248799325 ) ) ;
#20616 = DIRECTION ( 'NONE',  ( -1.000000000000000000, -0.000000000000000000, -0.000000000000000000 ) ) ;
#20617 = CARTESIAN_POINT ( 'NONE',  ( 8.154706853209001238, -4.255646685191999623, 9.114089645792999406 ) ) ;
#20618 = ORIENTED_EDGE ( 'NONE', *, *, #54379, .F. ) ;
#20619 = CARTESIAN_POINT ( 'NONE',  ( 8.738426658774001154, 5.414918126383000185, 8.890678916765999418 ) ) ;
#20621 = CARTESIAN_POINT ( 'NONE',  ( 10.87274555961999845, -5.407608219159000029, -8.698392243238998844 ) ) ;
#20620 = CARTESIAN_POINT ( 'NONE',  ( 9.996404771875521789, -5.349457780297906417, 7.853068642099824359 ) ) ;
#20622 = CARTESIAN_POINT ( 'NONE',  ( 7.547935135705676757, -3.440357416814149971, 5.843313060613724019 ) ) ;
#20623 = DIRECTION ( 'NONE',  ( 1.000000000000000000, 0.000000000000000000, 0.000000000000000000 ) ) ;
#20624 = CARTESIAN_POINT ( 'NONE',  ( 1.976884160321000339, -1.998287707672000035, 2.574515877127999897 ) ) ;
#20625 = ORIENTED_EDGE ( 'NONE', *, *, #65564, .F. ) ;
#20626 = CARTESIAN_POINT ( 'NONE',  ( 1.381730850247262055, 0.8076383959196232754, 3.202530411377747743 ) ) ;
#20627 = CARTESIAN_POINT ( 'NONE',  ( 11.88795122972049967, -3.601717549869600354, 8.421043941822800249 ) ) ;
#20628 = EDGE_CURVE ( 'NONE', #11912, #1557, #38228, .T. ) ;
#20629 = CARTESIAN_POINT ( 'NONE',  ( 10.15403136780999915, 5.267988602993999514, 5.992335067371000079 ) ) ;
#20630 = CARTESIAN_POINT ( 'NONE',  ( 10.18908827523999960, 5.907871695079999874, 7.801541097952000570 ) ) ;
#20631 = CARTESIAN_POINT ( 'NONE',  ( 11.69559063708295987, 5.086518862378000883, 7.194517870904999945 ) ) ;
#20632 = ORIENTED_EDGE ( 'NONE', *, *, #59679, .F. ) ;
#20633 = CARTESIAN_POINT ( 'NONE',  ( 16.86666666253433533, -3.351256455363679887, -11.15757949424527595 ) ) ;
#20634 = CARTESIAN_POINT ( 'NONE',  ( 12.09778329087091286, 2.320992115139772327, -12.38439064982923021 ) ) ;
#20635 = CARTESIAN_POINT ( 'NONE',  ( 5.000000000000000000, 0.2999999999999999889, 3.149999999999999911 ) ) ;
#20636 = CARTESIAN_POINT ( 'NONE',  ( 25.20343575914399992, -2.651923631867000086, -11.40161457019999958 ) ) ;
#20637 = CARTESIAN_POINT ( 'NONE',  ( 18.19085350568000337, -2.166991405623368561, 13.83127841112310819 ) ) ;
#20638 = DIRECTION ( 'NONE',  ( 0.000000000000000000, -0.9553735099700839672, -0.2954005017724949389 ) ) ;
#20640 = ORIENTED_EDGE ( 'NONE', *, *, #7360, .F. ) ;
#20639 = B_SPLINE_CURVE_WITH_KNOTS ( 'NONE', 3,
 ( #9858, #31886, #62316, #19670 ),
 .UNSPECIFIED., .F., .F.,
 ( 4, 4 ),
 ( 0.000000000000000000, 1.000000000000000000 ),
 .UNSPECIFIED. ) ;
#20641 = DIRECTION ( 'NONE',  ( 1.000000000000000000, 0.000000000000000000, 0.000000000000000000 ) ) ;
#20642 = CARTESIAN_POINT ( 'NONE',  ( 9.262620115046999558, -4.656877754660387225, -6.424592926396654136 ) ) ;
#20643 = ORIENTED_EDGE ( 'NONE', *, *, #27402, .F. ) ;
#20644 = CARTESIAN_POINT ( 'NONE',  ( 8.444541443210569653, 4.172527014369068254, 6.000552138965343119 ) ) ;
#20646 = CARTESIAN_POINT ( 'NONE',  ( 10.72749279009019929, 3.774717370312400178, 6.663611138821799784 ) ) ;
#20645 = AXIS2_PLACEMENT_3D ( 'NONE', #28128, #55736, #66555 ) ;
#20647 = CARTESIAN_POINT ( 'NONE',  ( 10.44079719460000000, 5.435719122931000236, 7.303631812894000319 ) ) ;
#20648 = CARTESIAN_POINT ( 'NONE',  ( 10.94349541711000029, 3.081616890687000065, -8.919380927961000793 ) ) ;
#20649 = CARTESIAN_POINT ( 'NONE',  ( 9.480191603681626944, -3.849750744317739670, -6.638050216028796413 ) ) ;
#20650 = CARTESIAN_POINT ( 'NONE',  ( 11.09424907396999949, -2.431867116603999790, 7.769513708858000633 ) ) ;
#20651 = CARTESIAN_POINT ( 'NONE',  ( 17.74611058647003858, 0.5951698179256272869, -12.68122092285041624 ) ) ;
#20652 = CARTESIAN_POINT ( 'NONE',  ( 12.39197104278336958, 2.969147788914954234, -12.32981191671632359 ) ) ;
#20653 = CARTESIAN_POINT ( 'NONE',  ( 11.21564426047340035, -3.460037133261700149, -8.345807871442598724 ) ) ;
#20654 = CARTESIAN_POINT ( 'NONE',  ( 7.464691113743000095, 4.351669901925999895, 8.977196921526999773 ) ) ;
#20655 = ORIENTED_EDGE ( 'NONE', *, *, #39310, .F. ) ;
#20656 =( LENGTH_UNIT ( ) NAMED_UNIT ( * ) SI_UNIT ( .MILLI., .METRE. ) );
#20657 = CARTESIAN_POINT ( 'NONE',  ( 24.76774681979610548, -3.098499905868568938, 11.74894159540815508 ) ) ;
#20658 = CARTESIAN_POINT ( 'NONE',  ( 21.72233714749290101, 0.000000000000000000, -5.000000000000000000 ) ) ;
#20659 = FACE_OUTER_BOUND ( 'NONE', #43787, .T. ) ;
#20660 = CARTESIAN_POINT ( 'NONE',  ( 6.365856561449002804, 10.53291268342000464, 4.483160362205999228 ) ) ;
#20661 = ADVANCED_FACE ( 'NONE', ( #20399 ), #15836, .F. ) ;
#20662 = CARTESIAN_POINT ( 'NONE',  ( 12.38995319333355916, 1.919216742092433314, 13.86782799095450258 ) ) ;
#20663 = ADVANCED_FACE ( 'NONE', ( #58147 ), #27029, .T. ) ;
#20664 = CARTESIAN_POINT ( 'NONE',  ( 11.00589466765999802, -3.012766713855000056, 5.961506477028999385 ) ) ;
#20665 = CARTESIAN_POINT ( 'NONE',  ( 10.59999999999999964, 3.399999999999999911, -4.756097560976000338 ) ) ;
#20666 = CARTESIAN_POINT ( 'NONE',  ( 12.08004253349365342, 0.01140630886273297576, 14.00000041621361291 ) ) ;
#20667 = ORIENTED_EDGE ( 'NONE', *, *, #6687, .F. ) ;
#20668 = CARTESIAN_POINT ( 'NONE',  ( 12.54704051454020686, -1.807816716204558416, 12.46963574575698530 ) ) ;
#20669 = CARTESIAN_POINT ( 'NONE',  ( 9.834329965421998665, -4.793057006135000186, -8.321459087847200564 ) ) ;
#20670 = CARTESIAN_POINT ( 'NONE',  ( 12.80505043854143388, 1.875000000000000000, -13.78631952119025428 ) ) ;
#20671 = CARTESIAN_POINT ( 'NONE',  ( 10.40727044253999978, -3.797905333157999941, 5.889909992361999969 ) ) ;
#20672 = CARTESIAN_POINT ( 'NONE',  ( 11.74441369783139955, -4.043700988887960257, 6.634905315059499209 ) ) ;
#20673 = B_SPLINE_SURFACE_WITH_KNOTS ( 'NONE', 3, 3, ( 
 ( #38811, #55238, #7334, #1749, #60136, #55931, #22719, #29371, #8034, #17838, #12245, #54891, #23423, #34264, #61172, #55586, #23764, #28323, #49994, #12589, #61516, #44758, #27983, #6991, #45099, #39158, #23069, #49292, #28677, #50686, #1404, #50339, #34618, #44417, #45442 ),
 ( #18181, #66756, #18871, #33223, #60481, #54545, #65717, #33918, #29030, #13294, #2105, #2437, #66408, #66062, #39503, #60827, #39853, #12939, #18527, #57283, #46123, #8720, #20576, #36314, #67429, #41901, #41560, #62869, #51702, #14653, #62196, #56954, #30063, #34957, #24458 ),
 ( #67092, #41222, #13971, #68453, #46810, #51026, #13631, #51366, #19204, #40527, #56271, #25823, #35299, #8380, #35970, #20234, #14316, #4483, #29723, #45781, #35642, #9387, #47154, #24798, #3125, #61853, #67770, #52389, #56614, #3460, #19554, #40873, #9055, #30393, #30732 ),
 ( #3799, #25136, #46468, #19895, #52039, #14987, #62533, #4142, #57631, #25479, #68116, #9734, #31083, #21600, #42938, #68803, #53770, #64246, #59354, #11456, #286, #27548, #16360, #15678, #637, #37689, #47499, #59019, #20924, #32454, #42261, #31420, #15337, #11121, #52737 ) ),
 .UNSPECIFIED., .F., .F., .F.,
 ( 4, 4 ),
 ( 4, 1, 1, 1, 1, 1, 1, 1, 1, 1, 1, 1, 1, 1, 1, 1, 1, 1, 1, 1, 1, 1, 1, 1, 1, 1, 1, 1, 1, 1, 1, 1, 4 ),
 ( -0.1039370721279000015, 1.103937072127999963 ),
 ( -0.01933701211302999920, 0.01208563257065999909, 0.04350827725433999843, 0.07493092193802000645, 0.1063535666217000075, 0.1377762113054000204, 0.1691988559891000055, 0.2006215006727000150, 0.2320441453564000001, 0.2634667900400999851, 0.2948894347238000258, 0.3263120794074999553, 0.3577347240911999959, 0.3891573687748000054, 0.4205800134584999905, 0.4520026581421999756, 0.4834253028259000162, 0.5148479475096000568, 0.5462705921932000663, 0.5776932368768999959, 0.6091158815606000365, 0.6405385262443000771, 0.6719611709280000067, 0.7033838156117000473, 0.7348064602953000568, 0.7662291049789999864, 0.7976517496627000270, 0.8290743943464000676, 0.8604970390300999972, 0.8919196837138000378, 0.9233423283974000473, 0.9547649730810999769, 0.9861876177648000175 ),
 .UNSPECIFIED. ) ;
#20674 = CARTESIAN_POINT ( 'NONE',  ( 12.36386718854188693, 0.5708113556792882015, 12.58706429964239071 ) ) ;
#20675 = AXIS2_PLACEMENT_3D ( 'NONE', #63201, #4823, #47490 ) ;
#20676 = CARTESIAN_POINT ( 'NONE',  ( 7.662260841227999997, 2.688365364125000045, 8.140015608605001063 ) ) ;
#20677 = CARTESIAN_POINT ( 'NONE',  ( 9.668957801871640001, 4.353212854359610695, -8.814514396735029678 ) ) ;
#20678 = CARTESIAN_POINT ( 'NONE',  ( 12.47010838183367731, 1.842148406394422899, 12.46461078478868245 ) ) ;
#20679 = CARTESIAN_POINT ( 'NONE',  ( 10.70920446233376744, -2.899999999999999911, 6.662590550603483486 ) ) ;
#20680 = CARTESIAN_POINT ( 'NONE',  ( 11.21564426047340035, 4.539962866738299851, -8.345807871442598724 ) ) ;
#20681 = CARTESIAN_POINT ( 'NONE',  ( 11.92303154622255335, 11.77792023318604286, -4.262523390537997336 ) ) ;
#20682 = EDGE_CURVE ( 'NONE', #44911, #14252, #4651, .T. ) ;
#20683 = CARTESIAN_POINT ( 'NONE',  ( 10.82674528040999995, 3.167160000746000126, -6.225151413000000744 ) ) ;
#20684 = CARTESIAN_POINT ( 'NONE',  ( 10.01057120343299900, 3.937990586507050139, -8.777708647662999297 ) ) ;
#20685 = CARTESIAN_POINT ( 'NONE',  ( 10.90291609082000157, -2.900148980393999931, 5.141822371583000262 ) ) ;
#20686 = DIRECTION ( 'NONE',  ( 1.000000000000000000, -1.157371756819000075E-14, 2.893429392047000287E-14 ) ) ;
#20687 = ORIENTED_EDGE ( 'NONE', *, *, #18454, .F. ) ;
#20688 = B_SPLINE_CURVE_WITH_KNOTS ( 'NONE', 3,
 ( #23541, #8156, #2902, #45570, #66875, #46251 ),
 .UNSPECIFIED., .F., .F.,
 ( 4, 1, 1, 4 ),
 ( 0.000000000000000000, 0.3333333333333000081, 0.6666666666667000474, 1.000000000000000000 ),
 .UNSPECIFIED. ) ;
#20689 = EDGE_CURVE ( 'NONE', #28596, #27423, #50279, .T. ) ;
#20690 = CARTESIAN_POINT ( 'NONE',  ( 12.44873997947986055, 0.5136077743244018556, 12.68601957541667247 ) ) ;
#20691 = CARTESIAN_POINT ( 'NONE',  ( 10.21684687351595677, 4.768183399968648040, 8.499583552997721725 ) ) ;
#20692 = VECTOR ( 'NONE', #42069, 1000.000000000000000 ) ;
#20693 = DIRECTION ( 'NONE',  ( 0.000000000000000000, -0.8765967884314782577, 0.4812255921203881792 ) ) ;
#20694 = CARTESIAN_POINT ( 'NONE',  ( 9.956950584426998319, 4.344127791340399725, 8.295791434820300125 ) ) ;
#20695 = CARTESIAN_POINT ( 'NONE',  ( 4.649999478197480052, 2.033928581112999763E-13, 13.22499948080971777 ) ) ;
#20696 = CARTESIAN_POINT ( 'NONE',  ( 12.19422188688375641, -2.632730885462789328, 13.64441700900758114 ) ) ;
#20697 = CARTESIAN_POINT ( 'NONE',  ( 12.19254401040021740, 2.624350118463367298, 13.64624664189957493 ) ) ;
#20698 = CARTESIAN_POINT ( 'NONE',  ( 8.154398449966548057, 3.068578756614712688, 6.310691935350006609 ) ) ;
#20699 = VERTEX_POINT ( 'NONE', #63026 ) ;
#20700 = CARTESIAN_POINT ( 'NONE',  ( 4.398018765420999898, -1.272903806234000124, 0.08056657245258999622 ) ) ;
#20701 = CARTESIAN_POINT ( 'NONE',  ( 8.744113844317999096, -3.676949563211899807, -6.262250912840999106 ) ) ;
#20702 = FACE_OUTER_BOUND ( 'NONE', #33532, .T. ) ;
#20703 = CARTESIAN_POINT ( 'NONE',  ( 11.86056039236529891, -3.108928759355700233, 7.456633480985620288 ) ) ;
#20704 = ADVANCED_FACE ( 'NONE', ( #53591 ), #31933, .T. ) ;
#20705 = CARTESIAN_POINT ( 'NONE',  ( 18.16486442019678904, 2.361571392960268856, -12.48278654574965785 ) ) ;
#20706 = CARTESIAN_POINT ( 'NONE',  ( 6.899999691988000450, 12.20988339176000004, -3.111064831549000154 ) ) ;
#20707 = CARTESIAN_POINT ( 'NONE',  ( 18.16744427668637840, 2.624922642575843845, 12.42158156204347463 ) ) ;
#20708 = CARTESIAN_POINT ( 'NONE',  ( 7.432076984665996200, 3.524670056070998037, 6.650527748631001046 ) ) ;
#20709 = CARTESIAN_POINT ( 'NONE',  ( 10.95319508605000181, -2.845003304712999892, -5.173782098108999250 ) ) ;
#20710 = CARTESIAN_POINT ( 'NONE',  ( 24.30001694968100168, 3.271769180623000040, -12.21048179117000032 ) ) ;
#20711 = CARTESIAN_POINT ( 'NONE',  ( 9.579652738407462564, -4.352972272612487536, 8.851639610528229341 ) ) ;
#20712 = VECTOR ( 'NONE', #5008, 1000.000000000000000 ) ;
#20713 = CARTESIAN_POINT ( 'NONE',  ( 18.30000000000000071, 2.775715947008034146, -11.68320807311170917 ) ) ;
#20714 = CARTESIAN_POINT ( 'NONE',  ( 24.43231275843400141, 11.98247113617999915, 3.250307990934000024 ) ) ;
#20715 = CARTESIAN_POINT ( 'NONE',  ( 0.2000000000000000389, -2.149999999999999911, 0.000000000000000000 ) ) ;
#20716 = CARTESIAN_POINT ( 'NONE',  ( 23.64145609567900053, 13.18672912911000061, -4.069240593728999933 ) ) ;
#20717 = ORIENTED_EDGE ( 'NONE', *, *, #59344, .F. ) ;
#20718 = CARTESIAN_POINT ( 'NONE',  ( 9.898395280408998076, 3.987760651117999711, -9.123263301387000368 ) ) ;
#20719 = CARTESIAN_POINT ( 'NONE',  ( 12.06025819896753859, -4.986099335708799707, 7.314099615601099558 ) ) ;
#20720 = EDGE_LOOP ( 'NONE', ( #63051, #15968, #40458, #8283 ) ) ;
#20721 = DIRECTION ( 'NONE',  ( -0.7071067783004970631, -0.7071067840725973053, 3.040673411905991405E-08 ) ) ;
#20722 = CARTESIAN_POINT ( 'NONE',  ( 10.30072469555899950, -3.429147315060100176, -6.512367818249299667 ) ) ;
#20723 = ORIENTED_EDGE ( 'NONE', *, *, #16868, .T. ) ;
#20724 = CARTESIAN_POINT ( 'NONE',  ( 11.80233327354039830, 2.898463260143000042, 8.220500279733599314 ) ) ;
#20725 = CARTESIAN_POINT ( 'NONE',  ( 9.690635841230999858, 2.927176851028000293, -5.932007155957999878 ) ) ;
#20726 = CARTESIAN_POINT ( 'NONE',  ( 12.14122412107036908, -3.937930136014310190, 8.673243607771999208 ) ) ;
#20727 = CARTESIAN_POINT ( 'NONE',  ( 11.07907162307749793, 3.185388239149200107, 7.825000000000000178 ) ) ;
#20728 = CARTESIAN_POINT ( 'NONE',  ( 10.29399293566599916, -3.453258297007899991, -8.170700474995699736 ) ) ;
#20729 = CARTESIAN_POINT ( 'NONE',  ( 12.39297058755369463, 0.4699376427894553787, -13.88930769708015589 ) ) ;
#20730 = CARTESIAN_POINT ( 'NONE',  ( 23.73952158721290218, 9.827654401539094309, -9.725498138330634035 ) ) ;
#20731 = CARTESIAN_POINT ( 'NONE',  ( 11.09999999999999964, 5.449702574547000467, 5.124965750789000296 ) ) ;
#20732 = ORIENTED_EDGE ( 'NONE', *, *, #46236, .T. ) ;
#20733 = CARTESIAN_POINT ( 'NONE',  ( 13.46053068095500116, 9.490401724732999256, 7.804222448269000800 ) ) ;
#20734 = CARTESIAN_POINT ( 'NONE',  ( 9.775320280412000074, 2.527713920559999661, -6.969421869128999525 ) ) ;
#20735 = EDGE_LOOP ( 'NONE', ( #40591, #18742, #55112 ) ) ;
#20736 = VECTOR ( 'NONE', #62722, 1000.000000000000000 ) ;
#20737 = CARTESIAN_POINT ( 'NONE',  ( 10.62924593896999959, 3.609487840896999700, -5.855139066690000504 ) ) ;
#20738 = ORIENTED_EDGE ( 'NONE', *, *, #20744, .F. ) ;
#20739 = CARTESIAN_POINT ( 'NONE',  ( 9.833267173155999075, 3.026371913119300316, 8.329718467866699783 ) ) ;
#20740 = SURFACE_STYLE_USAGE ( .BOTH. , #6367 ) ;
#20741 = AXIS2_PLACEMENT_3D ( 'NONE', #40235, #7376, #61552 ) ;
#20742 = CARTESIAN_POINT ( 'NONE',  ( 10.14393020684899938, 5.250000000000000000, -7.500000000000000000 ) ) ;
#20743 = EDGE_CURVE ( 'NONE', #5981, #50591, #30821, .T. ) ;
#20744 = EDGE_CURVE ( 'NONE', #55952, #58625, #31585, .T. ) ;
#20745 = CARTESIAN_POINT ( 'NONE',  ( 4.600000365992000795, 13.09999963393000044, 1.605909783351000005E-09 ) ) ;
#20746 = ADVANCED_FACE ( 'NONE', ( #48342 ), #6616, .F. ) ;
#20747 = CARTESIAN_POINT ( 'NONE',  ( 25.46371819568200223, 2.879482785682999868, 11.30954024936000124 ) ) ;
#20748 = ORIENTED_EDGE ( 'NONE', *, *, #26635, .F. ) ;
#20749 = CARTESIAN_POINT ( 'NONE',  ( 12.79342929296800158, 12.04986812289999953, -3.196648259943000170 ) ) ;
#20750 = CARTESIAN_POINT ( 'NONE',  ( 17.57198442900400082, 11.38892236470999997, -4.574426315356000750 ) ) ;
#20751 = CARTESIAN_POINT ( 'NONE',  ( 8.470944094208999076, -5.100000000000000533, 6.571291218949999902 ) ) ;
#20752 = CARTESIAN_POINT ( 'NONE',  ( 8.903317944506808246, 3.725094887964653267, 8.526233764311367480 ) ) ;
#20753 = CARTESIAN_POINT ( 'NONE',  ( 8.351014158771000950, 5.616457598545999907, -8.245813000738998255 ) ) ;
#20754 = CARTESIAN_POINT ( 'NONE',  ( 18.12310803393399894, -3.320912951897000198, 11.92519506916999994 ) ) ;
#20755 = CARTESIAN_POINT ( 'NONE',  ( 9.819572261909000233, -2.688237737290000151, -7.873041261681999359 ) ) ;
#20756 = ORIENTED_EDGE ( 'NONE', *, *, #16611, .T. ) ;
#20757 = ORIENTED_EDGE ( 'NONE', *, *, #14665, .F. ) ;
#20758 = CARTESIAN_POINT ( 'NONE',  ( 10.96083988518000041, 5.155325283248000545, -5.100114892965000202 ) ) ;
#20759 = DIRECTION ( 'NONE',  ( 0.000000000000000000, 0.2714570858282905341, -0.9624505444715651947 ) ) ;
#20760 = CARTESIAN_POINT ( 'NONE',  ( 1.290556799207375205, -3.500000000000002220, 0.4581489286484968781 ) ) ;
#20761 = CARTESIAN_POINT ( 'NONE',  ( 25.60000000000000142, 0.000000000000000000, 0.000000000000000000 ) ) ;
#20762 = CARTESIAN_POINT ( 'NONE',  ( 10.52799293566599914, 4.806678152079100208, -8.489570425681801424 ) ) ;
#20763 = CARTESIAN_POINT ( 'NONE',  ( 9.307392757686999474, 4.585219941293200208, -8.139707405630899117 ) ) ;
#20765 = CARTESIAN_POINT ( 'NONE',  ( 8.436397631282501308, 5.097046128306766732, -6.518116409473913464 ) ) ;
#20764 = CARTESIAN_POINT ( 'NONE',  ( 9.927051052051998781, -3.014287398677499841, 7.307093369932900373 ) ) ;
#20766 = CARTESIAN_POINT ( 'NONE',  ( 7.475100008705002352, -3.230432416208002699, 6.447622763416998914 ) ) ;
#20767 = ORIENTED_EDGE ( 'NONE', *, *, #56671, .F. ) ;
#20768 = B_SPLINE_CURVE_WITH_KNOTS ( 'NONE', 3,
 ( #12798, #24312, #34126, #55443 ),
 .UNSPECIFIED., .F., .F.,
 ( 4, 4 ),
 ( 0.000000000000000000, 1.000000000000000000 ),
 .UNSPECIFIED. ) ;
#20769 = LINE ( 'NONE', #3646, #44806 ) ;
#20770 = CARTESIAN_POINT ( 'NONE',  ( 11.09999999999999964, -6.518019921535999295, 5.523175303137000114 ) ) ;
#20771 = CARTESIAN_POINT ( 'NONE',  ( 10.14029229006299992, 5.106256438265999620, 8.142324746736500529 ) ) ;
#20772 = CARTESIAN_POINT ( 'NONE',  ( 6.916496230701000059, -12.19459988848999998, -3.104235478652000335 ) ) ;
#20773 = CARTESIAN_POINT ( 'NONE',  ( 10.24961784311999935, -4.184221496660999406, 9.286877953065999947 ) ) ;
#20774 = CARTESIAN_POINT ( 'NONE',  ( 18.16257472042013532, 2.647071733601741084, -12.41611113201541450 ) ) ;
#20775 = CARTESIAN_POINT ( 'NONE',  ( 4.550000802215999229, 1.829647544581999737E-13, 0.000000000000000000 ) ) ;
#20776 = CARTESIAN_POINT ( 'NONE',  ( 15.89994436294300151, -8.847904542234999781, -8.580301953175000662 ) ) ;
#20777 = CARTESIAN_POINT ( 'NONE',  ( 8.222954734881996686, -4.680061443183004322, 6.135926641887999189 ) ) ;
#20778 = CARTESIAN_POINT ( 'NONE',  ( 8.733265421555000074, -4.162714371335800578, -8.341695632489900092 ) ) ;
#20779 = CARTESIAN_POINT ( 'NONE',  ( 6.261216479699999837, -0.6943539861719999484, 0.9492381903959000722 ) ) ;
#20780 = EDGE_CURVE ( 'NONE', #12815, #866, #58297, .T. ) ;
#20781 = CARTESIAN_POINT ( 'NONE',  ( 1.050973465875000068, 3.500000000000000000, 0.000000000000000000 ) ) ;
#20782 = CARTESIAN_POINT ( 'NONE',  ( 17.55505043854143565, 1.760910691117812954, 12.47634535983622861 ) ) ;
#20783 = CARTESIAN_POINT ( 'NONE',  ( 12.80505043854143388, 3.124999999999999556, -13.52084414783465505 ) ) ;
#20784 = ORIENTED_EDGE ( 'NONE', *, *, #21909, .T. ) ;
#20785 = CARTESIAN_POINT ( 'NONE',  ( 12.32802524195760263, 0.4039503557775021014, -12.69135589213616377 ) ) ;
#20786 = CARTESIAN_POINT ( 'NONE',  ( 12.22547077884265754, -2.733971791243574145, -12.39396907916229651 ) ) ;
#20787 = EDGE_CURVE ( 'NONE', #22779, #5123, #34678, .T. ) ;
#20788 = CARTESIAN_POINT ( 'NONE',  ( 6.928163941478000076, -9.243153458936999911, -5.233361216079999600 ) ) ;
#20789 = CYLINDRICAL_SURFACE ( 'NONE', #13379, 1.250000000000000222 ) ;
#20790 = CARTESIAN_POINT ( 'NONE',  ( 10.25047016403597766, 3.823336794438951802, -8.849920973561742343 ) ) ;
#20791 = ORIENTED_EDGE ( 'NONE', *, *, #28627, .F. ) ;
#20792 = DIRECTION ( 'NONE',  ( 0.000000000000000000, 1.000000000000000000, 0.000000000000000000 ) ) ;
#20793 = SHAPE_DEFINITION_REPRESENTATION ( #19323, #8579 ) ;
#20794 = CARTESIAN_POINT ( 'NONE',  ( 10.72702344389999851, -5.004394439171999664, -6.890449684422599752 ) ) ;
#20795 = CARTESIAN_POINT ( 'NONE',  ( 10.87668353155578238, 2.650012393098275520, -7.302148410131429124 ) ) ;
#20796 = FACE_OUTER_BOUND ( 'NONE', #8342, .T. ) ;
#20797 = CARTESIAN_POINT ( 'NONE',  ( 11.49999672495000169, -5.885481364898649481, 10.12743717035876223 ) ) ;
#20798 = CARTESIAN_POINT ( 'NONE',  ( 11.36056039236529891, 4.891071240644300211, -7.543366519014379712 ) ) ;
#20799 = ORIENTED_EDGE ( 'NONE', *, *, #14631, .F. ) ;
#20800 = CARTESIAN_POINT ( 'NONE',  ( 11.00589466765999802, -3.012766713855000056, 5.961506477028999385 ) ) ;
#20801 = ORIENTED_EDGE ( 'NONE', *, *, #2833, .T. ) ;
#20802 = CARTESIAN_POINT ( 'NONE',  ( 9.450686119113880679, -5.278034476077728243, 7.934633963864382800 ) ) ;
#20803 = CARTESIAN_POINT ( 'NONE',  ( 9.433105646793000787, -4.954907757874000396, 8.825780921426000347 ) ) ;
#20804 = CARTESIAN_POINT ( 'NONE',  ( 16.09055856039299925, 8.515834468357001086, 7.893949987785000566 ) ) ;
#20805 = VERTEX_POINT ( 'NONE', #17573 ) ;
#20806 = CARTESIAN_POINT ( 'NONE',  ( 0.000000000000000000, 1.781768641235091266, -2.319305672483670921 ) ) ;
#20807 = CARTESIAN_POINT ( 'NONE',  ( 8.119770280407001550, 3.402419637676000086, -5.873899751133000002 ) ) ;
#20808 = CARTESIAN_POINT ( 'NONE',  ( 9.573096873516668381, -2.782534154164605589, -7.827184855449103473 ) ) ;
#20809 = CARTESIAN_POINT ( 'NONE',  ( 9.517711781556004169, 4.527670937829623377, 8.747760000556041859 ) ) ;
#20810 = ORIENTED_EDGE ( 'NONE', *, *, #44475, .T. ) ;
#20811 = CARTESIAN_POINT ( 'NONE',  ( 10.99433452212999818, -3.697619272994999928, 5.729306330972000261 ) ) ;
#20812 = CARTESIAN_POINT ( 'NONE',  ( 17.55505043854147118, -3.125000000000000000, -12.28373071562070074 ) ) ;
#20813 = PLANE ( 'NONE',  #67363 ) ;
#20814 = ORIENTED_EDGE ( 'NONE', *, *, #1973, .T. ) ;
#20815 = VECTOR ( 'NONE', #14543, 1000.000000000000000 ) ;
#20816 = CARTESIAN_POINT ( 'NONE',  ( 9.716851002543000604, -2.832432432432000269, 6.822293592207000934 ) ) ;
#20817 = ORIENTED_EDGE ( 'NONE', *, *, #13284, .F. ) ;
#20818 = CARTESIAN_POINT ( 'NONE',  ( 23.66004879239100234, -9.998911572074998588, 9.691526907171001071 ) ) ;
#20819 = CARTESIAN_POINT ( 'NONE',  ( 24.09351921955576614, 12.55954825742757208, -3.397332434207054330 ) ) ;
#20820 = CARTESIAN_POINT ( 'NONE',  ( 17.69772537084632447, -0.6088395004560434032, -12.68034807294329980 ) ) ;
#20821 = AXIS2_PLACEMENT_3D ( 'NONE', #16004, #15667, #36996 ) ;
#20822 = FACE_OUTER_BOUND ( 'NONE', #9880, .T. ) ;
#20823 = PLANE ( 'NONE',  #31929 ) ;
#20824 = CARTESIAN_POINT ( 'NONE',  ( 24.23080198909943306, 12.32902557501668994, 3.306557022674655677 ) ) ;
#20825 = EDGE_CURVE ( 'NONE', #7065, #23338, #66592, .T. ) ;
#20826 = CARTESIAN_POINT ( 'NONE',  ( 9.446013540182333301, -4.999583552997726166, -8.268183399968640046 ) ) ;
#20827 = EDGE_CURVE ( 'NONE', #22839, #62111, #32565, .T. ) ;
#20828 = EDGE_CURVE ( 'NONE', #15877, #66683, #11619, .T. ) ;
#20829 = EDGE_LOOP ( 'NONE', ( #64920, #54770, #39761, #69148, #7589 ) ) ;
#20830 = CARTESIAN_POINT ( 'NONE',  ( 8.189586429382003985, -5.107684026525003418, 6.413118510302999731 ) ) ;
#20831 = ORIENTED_EDGE ( 'NONE', *, *, #5387, .F. ) ;
#20832 = CARTESIAN_POINT ( 'NONE',  ( 10.16829701902000060, 4.567214950372999738, 5.832525041908999341 ) ) ;
#20833 = APPLICATION_CONTEXT ( 'automotive_design' ) ;
#20834 = CARTESIAN_POINT ( 'NONE',  ( 4.570855421957501719, -1.392841697040837046, 0.6432039759612279139 ) ) ;
#20835 = CARTESIAN_POINT ( 'NONE',  ( 5.100000004521000108, 0.8000000000000000444, -3.149999999999999911 ) ) ;
#20836 = CONICAL_SURFACE ( 'NONE', #64378, 10.64999982788999944, 0.7853981633972997312 ) ;
#20837 = CARTESIAN_POINT ( 'NONE',  ( 12.36772010770944696, 2.053374490018977205, -13.75810180220399026 ) ) ;
#20838 = CARTESIAN_POINT ( 'NONE',  ( 9.814967517147769271, -2.649990781018497721, -7.499998108648967765 ) ) ;
#20839 = CARTESIAN_POINT ( 'NONE',  ( 8.327313733649477356, 2.900678655379088866, 6.583019346906352709 ) ) ;
#20840 = CARTESIAN_POINT ( 'NONE',  ( 17.69771933245237250, -0.6088408278571642018, 13.88204686096232621 ) ) ;
#20841 = DIRECTION ( 'NONE',  ( 0.000000000000000000, 0.000000000000000000, -1.000000000000000000 ) ) ;
#20842 = ORIENTED_EDGE ( 'NONE', *, *, #51796, .F. ) ;
#20843 = CARTESIAN_POINT ( 'NONE',  ( 12.39787770678336543, 0.4743614821706066409, 13.88910774393186998 ) ) ;
#20844 = CARTESIAN_POINT ( 'NONE',  ( 12.05194988689359903, -3.419512757306400363, 6.361426117087999543 ) ) ;
#20845 = CARTESIAN_POINT ( 'NONE',  ( 10.44872595140593674, 4.356130030004455200, -9.239985720784517298 ) ) ;
#20846 = CARTESIAN_POINT ( 'NONE',  ( 15.36385332268500115, 9.394483288005998745, 8.200629419667000874 ) ) ;
#20847 = EDGE_CURVE ( 'NONE', #8436, #56231, #51612, .T. ) ;
#20848 = CARTESIAN_POINT ( 'NONE',  ( 9.106129440379998385, -4.192917962110999319, 5.525484568403999930 ) ) ;
#20850 = CARTESIAN_POINT ( 'NONE',  ( 23.56666365135700403, -2.488348886737001386, -11.45224114470000565 ) ) ;
#20849 = CARTESIAN_POINT ( 'NONE',  ( 9.944319408602000365, 5.443001719280999851, 7.367350382395000175 ) ) ;
#20851 = CARTESIAN_POINT ( 'NONE',  ( 10.27610941423800028, 4.844410192686099847, -6.733017893878099791 ) ) ;
#20852 = DIRECTION ( 'NONE',  ( 1.000000000000000000, -3.631529569662070274E-15, 1.174496025128702085E-14 ) ) ;
#20853 = CARTESIAN_POINT ( 'NONE',  ( 9.019772138681998896, 3.677371150249499898, -6.695252480703800302 ) ) ;
#20854 = CARTESIAN_POINT ( 'NONE',  ( 17.88703114068441025, 0.6395598188657292127, 12.58375915074078577 ) ) ;
#20855 = CARTESIAN_POINT ( 'NONE',  ( 7.040196970683999744, 0.9502619346694000102, -0.6159082020391000167 ) ) ;
#20856 = CARTESIAN_POINT ( 'NONE',  ( 24.44496488041000148, -12.03536727282999941, 3.224852091355999928 ) ) ;
#20857 = ORIENTED_EDGE ( 'NONE', *, *, #34995, .F. ) ;
#20858 = CARTESIAN_POINT ( 'NONE',  ( 8.957394353210000659, -2.678334737187000325, 8.735278777293000729 ) ) ;
#20859 = CARTESIAN_POINT ( 'NONE',  ( 8.770183059623999355, -3.049610585291000042, 6.392533570808999421 ) ) ;
#20860 = CARTESIAN_POINT ( 'NONE',  ( 18.05265757431621410, 3.049509720595960260, 13.66384965554843589 ) ) ;
#20861 = CARTESIAN_POINT ( 'NONE',  ( 25.59997255263800042, -11.07537722176000017, -3.096069202785999952 ) ) ;
#20862 = VERTEX_POINT ( 'NONE', #34353 ) ;
#20863 = VECTOR ( 'NONE', #23884, 999.9999999999998863 ) ;
#20864 = CARTESIAN_POINT ( 'NONE',  ( 18.23043922992600230, 3.518658233831999826, 12.06062508533999988 ) ) ;
#20865 = CARTESIAN_POINT ( 'NONE',  ( 11.52166954483529793, 4.562096242626500597, 8.367285821793199574 ) ) ;
#20866 = CARTESIAN_POINT ( 'NONE',  ( 10.16821721959000158, 2.330395133894000548, -7.267461653224000173 ) ) ;
#20867 = ORIENTED_EDGE ( 'NONE', *, *, #65103, .F. ) ;
#20868 = CARTESIAN_POINT ( 'NONE',  ( 9.196006702408606515, 4.999605512837395516, -6.731788826750698007 ) ) ;
#20869 = CARTESIAN_POINT ( 'NONE',  ( 10.12435795695566476, 5.250000000000000000, -7.807440182398264206 ) ) ;
#20870 = CARTESIAN_POINT ( 'NONE',  ( 11.62579573085663043, 5.239377455231000624, 7.285547569258399747 ) ) ;
#20871 = EDGE_CURVE ( 'NONE', #37649, #59938, #5790, .T. ) ;
#20872 = CARTESIAN_POINT ( 'NONE',  ( 5.656849040862428346, 12.07883750122941002, 3.735095616318558687 ) ) ;
#20874 = CARTESIAN_POINT ( 'NONE',  ( 7.373073341229000377, 3.394842219570000097, 9.388954446285000088 ) ) ;
#20873 = AXIS2_PLACEMENT_3D ( 'NONE', #1883, #11662, #38946 ) ;
#20875 = ORIENTED_EDGE ( 'NONE', *, *, #59962, .F. ) ;
#20876 = CARTESIAN_POINT ( 'NONE',  ( 11.50001496185000072, 5.131800295740712059, -11.50030236647292270 ) ) ;
#20877 = CARTESIAN_POINT ( 'NONE',  ( 9.883148997457000817, 5.167567567567999731, 6.822293592207000934 ) ) ;
#20878 = CARTESIAN_POINT ( 'NONE',  ( 8.139549708658289973, -5.282892974517072737, 6.298817220362490588 ) ) ;
#20879 = VECTOR ( 'NONE', #32990, 1000.000000000000114 ) ;
#20880 = CARTESIAN_POINT ( 'NONE',  ( 10.84606641549978256, -3.161700962939955506, -7.747677868960886727 ) ) ;
#20881 = ORIENTED_EDGE ( 'NONE', *, *, #51190, .T. ) ;
#20882 = CARTESIAN_POINT ( 'NONE',  ( 16.13854177342199847, -3.630911166246999944, -11.92992564462999994 ) ) ;
#20883 = CARTESIAN_POINT ( 'NONE',  ( 0.5060514795710333580, 2.965189113800866139, -1.878291422148264500 ) ) ;
#20884 = ORIENTED_EDGE ( 'NONE', *, *, #56434, .F. ) ;
#20885 = CARTESIAN_POINT ( 'NONE',  ( 9.935596873515667227, -5.092232985442824322, 6.870476274536375882 ) ) ;
#20886 = CARTESIAN_POINT ( 'NONE',  ( 25.60000000000000142, 2.258942858049999725, -12.29419282279000036 ) ) ;
#20887 = CARTESIAN_POINT ( 'NONE',  ( 17.96752346481819629, 0.4700078255514612557, -13.88931146942755390 ) ) ;
#20888 = CARTESIAN_POINT ( 'NONE',  ( 5.499989001269300459, 12.65264518617999911, -3.063510750763999813 ) ) ;
#20889 = DIRECTION ( 'NONE',  ( 0.000000000000000000, 1.000000000000000000, 0.000000000000000000 ) ) ;
#20890 = AXIS2_PLACEMENT_3D ( 'NONE', #27793, #55389, #17646 ) ;
#20891 = CARTESIAN_POINT ( 'NONE',  ( 11.14767835872009982, 3.125658946326500320, -6.948943352864199952 ) ) ;
#20892 = CARTESIAN_POINT ( 'NONE',  ( 11.68412378248529926, -4.549028353065900809, 8.538714411016998795 ) ) ;
#20893 = CARTESIAN_POINT ( 'NONE',  ( 12.52601681438817138, 3.059349880828009738, -12.30349483713085235 ) ) ;
#20894 = CARTESIAN_POINT ( 'NONE',  ( 11.85918179236250047, -4.238363971154499588, 8.615559381441000752 ) ) ;
#20895 = ORIENTED_EDGE ( 'NONE', *, *, #2019, .F. ) ;
#20896 = CARTESIAN_POINT ( 'NONE',  ( 8.887170280412000523, 2.193665972875999959, 7.400591513898000073 ) ) ;
#20897 = VERTEX_POINT ( 'NONE', #39586 ) ;
#20898 = CARTESIAN_POINT ( 'NONE',  ( 9.593930206849998754, 5.250000000000000000, -7.500000000000000000 ) ) ;
#20899 = CARTESIAN_POINT ( 'NONE',  ( 9.187745559622999991, -5.964711531933999389, 7.776478361891000723 ) ) ;
#20900 = B_SPLINE_CURVE_WITH_KNOTS ( 'NONE', 3,
 ( #21779, #31259, #63397, #30912, #16197, #37182 ),
 .UNSPECIFIED., .F., .F.,
 ( 4, 2, 4 ),
 ( 0.000000000000000000, 0.5000000000000000000, 1.000000000000000000 ),
 .UNSPECIFIED. ) ;
#20901 = CARTESIAN_POINT ( 'NONE',  ( 10.04184687351587613, 4.999583552997725278, 6.731816600031356401 ) ) ;
#20902 = VERTEX_POINT ( 'NONE', #1146 ) ;
#20903 = CARTESIAN_POINT ( 'NONE',  ( 12.19026796737406748, -2.613005292445991223, -12.42452312575879425 ) ) ;
#20904 = CARTESIAN_POINT ( 'NONE',  ( 11.05639837197999853, 7.348631596275997602, -6.145103702012999491 ) ) ;
#20905 = CARTESIAN_POINT ( 'NONE',  ( 24.35365242081700288, -8.355077740100997019, 8.511587483919999642 ) ) ;
#20906 = CARTESIAN_POINT ( 'NONE',  ( 10.84184687351628540, 3.000416447002276943, 8.268183399968647151 ) ) ;
#20907 = CARTESIAN_POINT ( 'NONE',  ( 12.08611717550378550, -2.614944066661595290, -13.75364144501312147 ) ) ;
#20908 = CARTESIAN_POINT ( 'NONE',  ( 10.28441772631199846, -3.627481539113199815, -8.266796319406900295 ) ) ;
#20909 = DIRECTION ( 'NONE',  ( 1.000000000000000000, 0.000000000000000000, 0.000000000000000000 ) ) ;
#20910 = EDGE_CURVE ( 'NONE', #17653, #55241, #32959, .T. ) ;
#20912 = ADVANCED_FACE ( 'NONE', ( #17219 ), #38901, .T. ) ;
#20911 = CARTESIAN_POINT ( 'NONE',  ( 18.27818099403250329, -2.425134644239736126, 12.36441930324462213 ) ) ;
#20913 = ORIENTED_EDGE ( 'NONE', *, *, #43797, .F. ) ;
#20914 =( BOUNDED_SURFACE ( )  B_SPLINE_SURFACE ( 3, 3, ( 
 ( #65575, #60340, #13146, #34476, #66610, #61708, #17698, #40061, #7201 ),
 ( #7892, #2979, #56123, #65916, #39360, #66950, #60681, #55442, #29228 ),
 ( #50538, #45976, #10284, #9589, #14849, #57147, #57835, #52247, #9244 ),
 ( #26024, #68312, #30254, #51556, #35831, #52589, #24993, #20777, #47011 ) ),
 .UNSPECIFIED., .F., .F., .T. ) 
 B_SPLINE_SURFACE_WITH_KNOTS ( ( 4, 4 ),
 ( 4, 1, 1, 1, 1, 1, 4 ),
 ( 0.000000000000000000, 1.000000000000000000 ),
 ( 0.8657679006235999841, 0.8794646334505999974, 0.9056938526918999477, 0.9344431701380999655, 0.9658387281735000274, 1.000000000000000000, 1.004641266558000012 ),
 .UNSPECIFIED. ) 
 GEOMETRIC_REPRESENTATION_ITEM ( )  RATIONAL_B_SPLINE_SURFACE ( (
 ( 1.157353709788000007, 1.157353709788000007, 1.157353709788000007, 1.157353709788000007, 1.157353709788000007, 1.157353709788000007, 1.157353709788000007, 1.157353709788000007, 1.157353709788000007),
 ( 0.9475487634039000406, 0.9475487634039000406, 0.9475487634039000406, 0.9475487634039000406, 0.9475487634039000406, 0.9475487634039000406, 0.9475487634039000406, 0.9475487634039000406, 0.9475487634039000406),
 ( 0.9475487634039000406, 0.9475487634039000406, 0.9475487634039000406, 0.9475487634039000406, 0.9475487634039000406, 0.9475487634039000406, 0.9475487634039000406, 0.9475487634039000406, 0.9475487634039000406),
 ( 1.157353709788000007, 1.157353709788000007, 1.157353709788000007, 1.157353709788000007, 1.157353709788000007, 1.157353709788000007, 1.157353709788000007, 1.157353709788000007, 1.157353709788000007) ) ) 
 REPRESENTATION_ITEM ( '' )  SURFACE ( )  );
#20915 = VERTEX_POINT ( 'NONE', #49373 ) ;
#20916 = CARTESIAN_POINT ( 'NONE',  ( 0.000000000000000000, 0.000000000000000000, 0.000000000000000000 ) ) ;
#20917 = AXIS2_PLACEMENT_3D ( 'NONE', #56043, #50806, #61979 ) ;
#20918 = CARTESIAN_POINT ( 'NONE',  ( 10.99999648468999958, -1.199999999999999956, -11.37663418768599932 ) ) ;
#20919 = CARTESIAN_POINT ( 'NONE',  ( 0.07497316781761000082, 0.000000000000000000, 0.000000000000000000 ) ) ;
#20920 = CARTESIAN_POINT ( 'NONE',  ( 9.843622243630001378, 5.021682716044000294, -8.761466596873999535 ) ) ;
#20921 = CARTESIAN_POINT ( 'NONE',  ( 18.29998515896363287, 2.924733550950530336, -11.97422828356910607 ) ) ;
#20922 = CARTESIAN_POINT ( 'NONE',  ( 17.99515569450505481, 2.943800350515566766, 12.33701119546411284 ) ) ;
#20923 = CARTESIAN_POINT ( 'NONE',  ( 8.347004975328005116, 2.870635057193001050, -6.340345019934002124 ) ) ;
#20924 = CARTESIAN_POINT ( 'NONE',  ( 10.68903608760000168, 2.568976842941999905, 7.728092503410000091 ) ) ;
#20925 = ORIENTED_EDGE ( 'NONE', *, *, #7479, .F. ) ;
#20926 = CIRCLE ( 'NONE', #55515, 0.8000000000000002665 ) ;
#20927 = CARTESIAN_POINT ( 'NONE',  ( 8.847812662421663532, 5.766884700386136764, -7.677413152681796582 ) ) ;
#20928 = ORIENTED_EDGE ( 'NONE', *, *, #9941, .F. ) ;
#20929 = CARTESIAN_POINT ( 'NONE',  ( 9.595493858556999101, 3.928424745541000185, 5.531312048131000303 ) ) ;
#20930 = CARTESIAN_POINT ( 'NONE',  ( 9.577013376692997682, -4.772923352651200268, -7.107192877568799361 ) ) ;
#20931 = CARTESIAN_POINT ( 'NONE',  ( 10.33536974457000035, 5.153692264686000613, 8.830864265869999841 ) ) ;
#20932 = EDGE_CURVE ( 'NONE', #1963, #11428, #37498, .T. ) ;
#20933 = CARTESIAN_POINT ( 'NONE',  ( 11.61123293495519881, -4.891405920092699589, 7.535834283667469435 ) ) ;
#20934 = CARTESIAN_POINT ( 'NONE',  ( 8.970860841232001448, 4.131080973160000447, -6.108642999115999395 ) ) ;
#20935 = AXIS2_PLACEMENT_3D ( 'NONE', #62056, #30589, #24314 ) ;
#20936 = CARTESIAN_POINT ( 'NONE',  ( 11.04766418734000055, 10.00030158377000156, -5.674024927225000070 ) ) ;
#20937 = EDGE_CURVE ( 'NONE', #12035, #28207, #47088, .T. ) ;
#20938 = CARTESIAN_POINT ( 'NONE',  ( 10.19810941423799910, 4.946022705791000007, -6.640722727400100389 ) ) ;
#20939 = CARTESIAN_POINT ( 'NONE',  ( 10.79704720403517548, 5.515590898206272463, -6.594712059625336131 ) ) ;
#20940 = B_SPLINE_CURVE_WITH_KNOTS ( 'NONE', 3,
 ( #1927, #7860, #29194, #13459 ),
 .UNSPECIFIED., .F., .F.,
 ( 4, 4 ),
 ( 0.000000000000000000, 1.000000000000000000 ),
 .UNSPECIFIED. ) ;
#20941 = CARTESIAN_POINT ( 'NONE',  ( 8.179999999999999716, 4.924138593003999809, -8.484107647018999998 ) ) ;
#20942 = CARTESIAN_POINT ( 'NONE',  ( 8.158534024102223725, 5.166158726348323071, -8.205174899589399828 ) ) ;
#20943 = CARTESIAN_POINT ( 'NONE',  ( 14.46666666323366890, 9.471992681081614407, 8.194936219980966996 ) ) ;
#20944 = EDGE_LOOP ( 'NONE', ( #7948, #53872, #42678, #15815, #25160 ) ) ;
#20945 = CARTESIAN_POINT ( 'NONE',  ( 9.816185841232000442, 2.656512020013999997, -7.884832994446999699 ) ) ;
#20946 = CARTESIAN_POINT ( 'NONE',  ( 7.426446028809999156, -0.5209984338309999741, 1.392739681806999918 ) ) ;
#20947 = CARTESIAN_POINT ( 'NONE',  ( 8.789886373836322875, -3.999992178805580334, -8.439846342473931173 ) ) ;
#20948 = CARTESIAN_POINT ( 'NONE',  ( 16.00000000266000555, 11.41071763148134544, -4.623975354790890613 ) ) ;
#20949 = CARTESIAN_POINT ( 'NONE',  ( 10.62716797202100949, 4.757662754245695957, 4.769350230254125300 ) ) ;
#20950 = CARTESIAN_POINT ( 'NONE',  ( 10.39918582084299992, -4.746348444722899629, -6.637298362509499228 ) ) ;
#20951 = ORIENTED_EDGE ( 'NONE', *, *, #46261, .F. ) ;
#20952 = CARTESIAN_POINT ( 'NONE',  ( 5.610802430940820429, -12.12319474034768341, 3.747515530461446254 ) ) ;
#20953 = CARTESIAN_POINT ( 'NONE',  ( 8.656823341231000057, 5.329437560656000272, 6.027391099688998999 ) ) ;
#20955 = CARTESIAN_POINT ( 'NONE',  ( 11.53681523859000002, 3.897571790034000117, -11.94316735528000173 ) ) ;
#20954 = CARTESIAN_POINT ( 'NONE',  ( 8.474089158773999486, 4.131080973160000447, -6.108642999115999395 ) ) ;
#20956 = CARTESIAN_POINT ( 'NONE',  ( 18.17041169247335475, -2.609942250310885115, 13.64953311053600871 ) ) ;
#20957 = ORIENTED_EDGE ( 'NONE', *, *, #29605, .F. ) ;
#20958 = CARTESIAN_POINT ( 'NONE',  ( 10.42596030538999941, 5.042177533603999784, 8.702224267793999601 ) ) ;
#20959 = CARTESIAN_POINT ( 'NONE',  ( 18.17186084707622484, -2.602861751209124552, -13.65107289232777177 ) ) ;
#20960 = CARTESIAN_POINT ( 'NONE',  ( 10.53057053952199951, 3.659587858614300249, 8.296503712697200328 ) ) ;
#20961 = DIRECTION ( 'NONE',  ( 1.000000000000000000, 0.000000000000000000, 0.000000000000000000 ) ) ;
#20962 = CARTESIAN_POINT ( 'NONE',  ( 9.181706853207000307, -3.734278838175999482, 8.942129638874000364 ) ) ;
#20963 = ORIENTED_EDGE ( 'NONE', *, *, #45507, .T. ) ;
#20964 = CARTESIAN_POINT ( 'NONE',  ( 8.610051658774001027, 5.329437560656000272, 6.027391099688998999 ) ) ;
#20965 = VECTOR ( 'NONE', #67156, 1000.000000000000000 ) ;
#20967 = CARTESIAN_POINT ( 'NONE',  ( 10.30480805961999913, -5.828319785709999756, -7.226592660401000678 ) ) ;
#20966 = DIRECTION ( 'NONE',  ( -1.000000000000000000, 0.000000000000000000, 0.000000000000000000 ) ) ;
#20968 = CARTESIAN_POINT ( 'NONE',  ( 7.612466077185790603, -4.791086490674309140, 5.950606121273764870 ) ) ;
#20969 = AXIS2_PLACEMENT_3D ( 'NONE', #57006, #25538, #46864 ) ;
#20970 = CARTESIAN_POINT ( 'NONE',  ( 18.05194036312017758, -0.3791492161817762163, 13.89304085482745421 ) ) ;
#20971 = CARTESIAN_POINT ( 'NONE',  ( 23.68315585345000329, 3.147788653374999690, 13.35041697813000106 ) ) ;
#20972 = EDGE_LOOP ( 'NONE', ( #12900, #48079 ) ) ;
#20973 = CARTESIAN_POINT ( 'NONE',  ( 9.633513540182331525, 5.250000000000001776, -7.663624617374467540 ) ) ;
#20974 = CARTESIAN_POINT ( 'NONE',  ( 11.12487750876920067, -4.543557328885200697, 6.656497609330299881 ) ) ;
#20975 = CARTESIAN_POINT ( 'NONE',  ( 10.63461554336999981, 5.668731883089999535, 6.527253515312000154 ) ) ;
#20976 = VECTOR ( 'NONE', #38066, 1000.000000000000114 ) ;
#20977 = CARTESIAN_POINT ( 'NONE',  ( 10.30487885159599770, 4.996404279947399552, 7.618867373350600047 ) ) ;
#20978 = ORIENTED_EDGE ( 'NONE', *, *, #34974, .F. ) ;
#20979 = CARTESIAN_POINT ( 'NONE',  ( 23.97708694432106924, -3.345394741305891984, 12.79002816627185091 ) ) ;
#20980 = AXIS2_PLACEMENT_3D ( 'NONE', #62979, #36428, #10202 ) ;
#20981 = CARTESIAN_POINT ( 'NONE',  ( 12.19289742234818696, 2.094552964378149973, -12.42468808284045245 ) ) ;
#20982 = CARTESIAN_POINT ( 'NONE',  ( 11.72056920625029974, -3.952687217764870198, 8.815417147437999645 ) ) ;
#20983 = CARTESIAN_POINT ( 'NONE',  ( 25.48370393093700059, -2.675493841248999694, -11.27075153412999953 ) ) ;
#20984 = CIRCLE ( 'NONE', #31075, 1.300172478116999208 ) ;
#20985 = CARTESIAN_POINT ( 'NONE',  ( 18.27457017588621468, -2.425781798817269852, 13.78826143416240591 ) ) ;
#20986 = CARTESIAN_POINT ( 'NONE',  ( 24.53428991268900106, -12.47024905405999995, -3.026245386525999947 ) ) ;
#20987 = VERTEX_POINT ( 'NONE', #63983 ) ;
#20988 = CARTESIAN_POINT ( 'NONE',  ( 11.05391045180431675, 5.129049487418005704, 6.885461205208883051 ) ) ;
#20989 = DIRECTION ( 'NONE',  ( 0.000000000000000000, -0.7158784314710769925, 0.6982249432342777506 ) ) ;
#20990 = ORIENTED_EDGE ( 'NONE', *, *, #17119, .F. ) ;
#20991 = CARTESIAN_POINT ( 'NONE',  ( 10.99826088462129903, 4.001843064679911244, 8.366195817038299509 ) ) ;
#20992 = CARTESIAN_POINT ( 'NONE',  ( 5.700000000000000178, -12.50865771883999855, 2.924687089724999911 ) ) ;
#20993 = CARTESIAN_POINT ( 'NONE',  ( 10.10656234570999956, 4.887646627408000377, -6.257286147482000516 ) ) ;
#20994 = CARTESIAN_POINT ( 'NONE',  ( 8.064674013518999374, 4.643178316509001036, 6.221316387655001279 ) ) ;
#20995 = CARTESIAN_POINT ( 'NONE',  ( 10.11260824411999870, -3.359889198679999911, 5.859131457670000209 ) ) ;
#20996 = CARTESIAN_POINT ( 'NONE',  ( 17.78490268980527489, 0.5812897767837147400, -12.68208758371478595 ) ) ;
#20997 = CONICAL_SURFACE ( 'NONE', #9811, 12.71246950475999959, 0.8960553845711767273 ) ;
#20998 = DIRECTION ( 'NONE',  ( 0.9999999999993943733, 9.646910165650955666E-07, -5.296687748115971159E-07 ) ) ;
#20999 = CARTESIAN_POINT ( 'NONE',  ( 10.62487750876920067, -4.543557328885200697, -8.343502390669698343 ) ) ;
#21000 = EDGE_CURVE ( 'NONE', #14597, #66034, #36752, .T. ) ;
#21002 = EDGE_CURVE ( 'NONE', #22321, #53841, #10174, .T. ) ;
#21001 = CARTESIAN_POINT ( 'NONE',  ( 9.368920280410000245, 5.618384167307999277, 7.727742442702000503 ) ) ;
#21003 = VERTEX_POINT ( 'NONE', #15425 ) ;
#21004 = CARTESIAN_POINT ( 'NONE',  ( 11.10000000000000320, 2.593029302020504190, -6.574394117172995600 ) ) ;
#21005 = CARTESIAN_POINT ( 'NONE',  ( 3.400000000000000355, 0.000000000000000000, 0.000000000000000000 ) ) ;
#21006 = CARTESIAN_POINT ( 'NONE',  ( 10.37309687351658383, -5.217465845835394411, -7.172815144550898303 ) ) ;
#21007 = CARTESIAN_POINT ( 'NONE',  ( 6.032675742706998356, 9.323387372329005274, 4.734447514572996951 ) ) ;
#21008 = CARTESIAN_POINT ( 'NONE',  ( 11.01654511052000096, 6.705990105703999227, 5.523018908835999774 ) ) ;
#21009 = CARTESIAN_POINT ( 'NONE',  ( 11.06173598926000068, 9.149873930312999448, 6.515098905781000482 ) ) ;
#21010 = DIRECTION ( 'NONE',  ( 8.848526463087000198E-11, -8.848494979014000266E-11, -1.000000000000000000 ) ) ;
#21011 = CARTESIAN_POINT ( 'NONE',  ( 9.224507172011824352, -4.124235577930278396, 6.625492773506611144 ) ) ;
#21012 = ORIENTED_EDGE ( 'NONE', *, *, #31402, .T. ) ;
#21013 = CARTESIAN_POINT ( 'NONE',  ( 12.61568544974634953, -1.785400273382258263, 12.47286636618916589 ) ) ;
#21014 = CARTESIAN_POINT ( 'NONE',  ( 10.29025461470400060, -5.106563667948999630, -7.781516069110699263 ) ) ;
#21015 = FACE_OUTER_BOUND ( 'NONE', #39696, .T. ) ;
#21016 = B_SPLINE_CURVE_WITH_KNOTS ( 'NONE', 3,
 ( #52260, #68671, #41428, #30595 ),
 .UNSPECIFIED., .F., .F.,
 ( 4, 4 ),
 ( 0.000000000000000000, 1.000000000000000000 ),
 .UNSPECIFIED. ) ;
#21017 = CARTESIAN_POINT ( 'NONE',  ( 10.00638553269999953, -5.119272496996000399, 8.420388242270998802 ) ) ;
#21018 = CARTESIAN_POINT ( 'NONE',  ( 11.30133863405320049, -3.465595476214000215, 6.818303296693398963 ) ) ;
#21019 = EDGE_CURVE ( 'NONE', #56837, #30029, #9474, .T. ) ;
#21020 = CARTESIAN_POINT ( 'NONE',  ( 12.39267273778989420, 0.5917181940048591438, 12.58609996267493081 ) ) ;
#21021 = CARTESIAN_POINT ( 'NONE',  ( 0.2361081069562999957, 3.176450105220999909, 1.136354878726999917 ) ) ;
#21022 = DIRECTION ( 'NONE',  ( -1.000000000000000000, 0.000000000000000000, 0.000000000000000000 ) ) ;
#21023 =( GEOMETRIC_REPRESENTATION_CONTEXT ( 3 ) GLOBAL_UNCERTAINTY_ASSIGNED_CONTEXT ( ( #52767 ) ) GLOBAL_UNIT_ASSIGNED_CONTEXT ( ( #60580, #12339, #65811 ) ) REPRESENTATION_CONTEXT ( 'NONE', 'WORKASPACE' ) );
#21024 = CARTESIAN_POINT ( 'NONE',  ( 12.11481770488409282, 2.701029500518133286, 12.30709430042447394 ) ) ;
#21025 = CARTESIAN_POINT ( 'NONE',  ( 9.000480666858997836, 4.426512626096299918, -8.706015266875999359 ) ) ;
#21026 = CARTESIAN_POINT ( 'NONE',  ( 11.04333729122639873, 2.996877626170000308, -7.473611442402849470 ) ) ;
#21027 = CARTESIAN_POINT ( 'NONE',  ( 8.099999999999999645, 0.000000000000000000, 0.000000000000000000 ) ) ;
#21028 = CARTESIAN_POINT ( 'NONE',  ( 9.900934992105000276, 4.883852641422000040, -9.070888919673000927 ) ) ;
#21029 = CARTESIAN_POINT ( 'NONE',  ( 9.478659112603999404, 3.444147913214900214, -8.652134039551000910 ) ) ;
#21031 = CARTESIAN_POINT ( 'NONE',  ( 10.90437356726000040, -2.900476673752999890, 5.132566153004000320 ) ) ;
#21030 = CARTESIAN_POINT ( 'NONE',  ( 11.07299956498199833, 5.207010770456999893, -7.825000000000000178 ) ) ;
#21032 = CARTESIAN_POINT ( 'NONE',  ( 17.79999999998900151, -3.595165934733000057, -11.99793354950999991 ) ) ;
#21033 = EDGE_LOOP ( 'NONE', ( #50233, #4644, #36832 ) ) ;
#21034 = AXIS2_PLACEMENT_3D ( 'NONE', #9268, #15566, #10653 ) ;
#21035 = CARTESIAN_POINT ( 'NONE',  ( 12.29062685719103243, 0.3550721705843559173, 12.69332222955381972 ) ) ;
#21036 = CARTESIAN_POINT ( 'NONE',  ( 9.133199450400381281, 5.099761357576720222, 6.159710572180461696 ) ) ;
#21037 = CARTESIAN_POINT ( 'NONE',  ( 10.44080359545000114, -5.435731278187999393, 7.303630150377999009 ) ) ;
#21038 = CARTESIAN_POINT ( 'NONE',  ( 9.982279731608999285, 4.077800926195140008, 8.363513150096299142 ) ) ;
#21039 = MECHANICAL_DESIGN_GEOMETRIC_PRESENTATION_REPRESENTATION (  '', ( #14365 ), #44515 ) ;
#21040 = CARTESIAN_POINT ( 'NONE',  ( 23.60205915885299888, 11.88166580723999921, -3.967996863072999147 ) ) ;
#21041 = CARTESIAN_POINT ( 'NONE',  ( 12.29628962427838346, -2.863168005537272354, 13.58969864530831728 ) ) ;
#21042 = CARTESIAN_POINT ( 'NONE',  ( 12.19259091224295233, 2.624575865621845860, 13.64619539111124347 ) ) ;
#21043 = CARTESIAN_POINT ( 'NONE',  ( 10.26947109217999810, -5.100000000000000533, -6.152188490330000370 ) ) ;
#21044 = ORIENTED_EDGE ( 'NONE', *, *, #48613, .F. ) ;
#21045 = CARTESIAN_POINT ( 'NONE',  ( 4.740115987645999951, 0.5852149391565999448, 1.133269042695999929 ) ) ;
#21046 = CARTESIAN_POINT ( 'NONE',  ( 9.124051052051999733, -2.744602294987000146, -7.745684736446600382 ) ) ;
#21047 = CARTESIAN_POINT ( 'NONE',  ( 9.585762625467372899, -5.314684444510202610, -7.853443062599636981 ) ) ;
#21048 = DIRECTION ( 'NONE',  ( 0.000000000000000000, 1.000000000000000000, 0.000000000000000000 ) ) ;
#21049 = CARTESIAN_POINT ( 'NONE',  ( 18.13637388831909192, 2.729759562904666037, -12.39509076542458743 ) ) ;
#21050 = CARTESIAN_POINT ( 'NONE',  ( 8.597024389729941873, 4.990110225107529551, 6.127963972499145484 ) ) ;
#21051 = CARTESIAN_POINT ( 'NONE',  ( 18.09718405122000107, 2.811158313974275735, 12.37360767970025677 ) ) ;
#21052 = EDGE_CURVE ( 'NONE', #58368, #18643, #29974, .T. ) ;
#21053 = EDGE_CURVE ( 'NONE', #13607, #5259, #23525, .T. ) ;
#21054 = CARTESIAN_POINT ( 'NONE',  ( 8.500493705215999896, 2.902642539927001941, 6.605602875546000341 ) ) ;
#21055 = CARTESIAN_POINT ( 'NONE',  ( 11.13359748671999938, -2.664949685833000181, -5.114435929787000568 ) ) ;
#21056 = CARTESIAN_POINT ( 'NONE',  ( 10.94847055962000049, -3.841065069379000274, -9.341805385095000247 ) ) ;
#21057 = DIRECTION ( 'NONE',  ( -1.000000000000000000, 0.000000000000000000, 0.000000000000000000 ) ) ;
#21058 = LINE ( 'NONE', #6339, #56509 ) ;
#21059 = CARTESIAN_POINT ( 'NONE',  ( 11.53482133862663694, -3.057020944820409536, 6.626386139742056258 ) ) ;
#21060 = CARTESIAN_POINT ( 'NONE',  ( 11.15221028326116048, -4.908903471848705458, -7.175011397899978327 ) ) ;
#21061 = CARTESIAN_POINT ( 'NONE',  ( 24.02106212480699909, 12.55316173831000093, -3.484249586872999682 ) ) ;
#21062 = ORIENTED_EDGE ( 'NONE', *, *, #27217, .F. ) ;
#21063 = CARTESIAN_POINT ( 'NONE',  ( 9.500595280412998278, 2.334550724494000029, -7.977056617806000283 ) ) ;
#21064 = CARTESIAN_POINT ( 'NONE',  ( 10.85826357027499967, -3.149486845331399998, 7.335909308151700614 ) ) ;
#21065 = ORIENTED_EDGE ( 'NONE', *, *, #3629, .F. ) ;
#21066 = CARTESIAN_POINT ( 'NONE',  ( 13.69992376746900042, 12.26631831379999937, 2.532779022035999805 ) ) ;
#21067 = CARTESIAN_POINT ( 'NONE',  ( 10.20226357027499908, -2.879914860223000250, -7.716099591766099053 ) ) ;
#21068 = ORIENTED_EDGE ( 'NONE', *, *, #5680, .F. ) ;
#21069 = CARTESIAN_POINT ( 'NONE',  ( 11.26212378248529866, 3.384904051819500381, 8.663708617168998316 ) ) ;
#21070 = CARTESIAN_POINT ( 'NONE',  ( 9.143660841233000269, 2.235961884443999459, -6.794506518623999902 ) ) ;
#21071 = AXIS2_PLACEMENT_3D ( 'NONE', #22026, #42674, #63981 ) ;
#21072 = CARTESIAN_POINT ( 'NONE',  ( 17.79416955086200147, -3.253172910778000304, 11.33701170283999993 ) ) ;
#21073 = CARTESIAN_POINT ( 'NONE',  ( 11.11123293495519881, -4.891405920092699589, -7.464165716332529676 ) ) ;
#21074 = CARTESIAN_POINT ( 'NONE',  ( 12.18827041298537495, 0.1029057169099007185, -13.89950510286185725 ) ) ;
#21075 = DIRECTION ( 'NONE',  ( 0.5298945043518727971, -2.050974249430894312E-08, 0.8480635673448556622 ) ) ;
#21076 = AXIS2_PLACEMENT_3D ( 'NONE', #41167, #47096, #10026 ) ;
#21077 = CARTESIAN_POINT ( 'NONE',  ( 13.44051303026600053, 11.61511980691000012, 2.065108503055999911 ) ) ;
#21078 = ORIENTED_EDGE ( 'NONE', *, *, #36467, .F. ) ;
#21080 = EDGE_CURVE ( 'NONE', #6237, #50848, #368, .T. ) ;
#21079 = CARTESIAN_POINT ( 'NONE',  ( 9.766460841231999979, 3.135494838036999798, -8.598037907310999373 ) ) ;
#21081 = EDGE_LOOP ( 'NONE', ( #45421, #37145, #50647, #67247, #23822 ) ) ;
#21082 = CARTESIAN_POINT ( 'NONE',  ( 16.03328789001813703, 8.397841793663578969, 8.170414199808826439 ) ) ;
#21083 = CARTESIAN_POINT ( 'NONE',  ( 0.000000000000000000, 0.000000000000000000, 0.000000000000000000 ) ) ;
#21084 = ADVANCED_FACE ( 'NONE', ( #21683 ), #11237, .F. ) ;
#21085 = EDGE_LOOP ( 'NONE', ( #64491, #41170, #61189, #20556, #3739, #60291, #3298, #3031, #23702, #10333, #12843 ) ) ;
#21086 = CARTESIAN_POINT ( 'NONE',  ( 9.098721904869998767, 5.115452802765999785, 6.873781641694999500 ) ) ;
#21087 = CARTESIAN_POINT ( 'NONE',  ( 17.99515569450509034, -2.943800350515567210, -12.33701119546411284 ) ) ;
#21088 = CARTESIAN_POINT ( 'NONE',  ( 13.49980696792483137, 11.54838492169066022, 4.420196298692874670 ) ) ;
#21089 = B_SPLINE_CURVE_WITH_KNOTS ( 'NONE', 3,
 ( #15825, #52890, #31918, #42743, #16167, #43440 ),
 .UNSPECIFIED., .F., .F.,
 ( 4, 2, 4 ),
 ( 0.000000000000000000, 0.5000000000000000000, 1.000000000000000000 ),
 .UNSPECIFIED. ) ;
#21090 = B_SPLINE_SURFACE_WITH_KNOTS ( 'NONE', 3, 3, ( 
 ( #45202, #66507, #29823, #61961, #51128, #61275, #13393, #34715, #50788, #3231, #14073, #56723, #24897, #8819, #30162, #51465, #46227, #67534, #19658, #40977, #62301, #41663, #47945, #45, #31189, #53533, #47604, #68911, #37447, #57387, #48281, #62967, #68216, #21028, #15442 ),
 ( #15094, #5625, #31521, #52145, #52843, #63314, #21365, #26278, #4249, #4940, #57732, #36418, #58768, #42362, #63663, #42697, #37109, #26966, #58424, #20000, #15780, #31869, #10875, #10529, #5285, #46913, #41324, #10191, #26627, #53187, #58089, #64003, #68561, #36767, #62630 ),
 ( #32220, #16121, #14755, #36073, #9492, #30835, #25586, #20334, #9843, #52494, #4591, #25927, #47257, #20683, #42013, #66335, #16459, #13224, #32555, #48630, #44694, #12869, #733, #21702, #23352, #24040, #38128, #54209, #23696, #7618, #8309, #56201, #60754, #37791, #55861 ),
 ( #65989, #2034, #11218, #61447, #34197, #34551, #28964, #50269, #18806, #59113, #29655, #43392, #22046, #2373, #18115, #2716, #5968, #39433, #64692, #64342, #53867, #16801, #59455, #39782, #11553, #32896, #6308, #27307, #55516, #28609, #29303, #45030, #49923, #18459, #61104 ) ),
 .UNSPECIFIED., .F., .F., .F.,
 ( 4, 4 ),
 ( 4, 1, 1, 1, 1, 1, 1, 1, 1, 1, 1, 1, 1, 1, 1, 1, 1, 1, 1, 1, 1, 1, 1, 1, 1, 1, 1, 1, 1, 1, 1, 1, 4 ),
 ( -0.1039370721279000015, 1.103937072127999963 ),
 ( 0.2233333333344000027, 0.2480800653604999795, 0.2728267973865999840, 0.2975735294126999886, 0.3223202614387999931, 0.3470669934649999733, 0.3718137254910999778, 0.3965604575171999824, 0.4213071895433000424, 0.4460539215694000470, 0.4708006535954999960, 0.4955473856216000006, 0.5202941176476999496, 0.5450408496738000652, 0.5697875816999000698, 0.5945343137260000743, 0.6192810457521999989, 0.6440277777783000035, 0.6687745098044000081, 0.6935212418305000126, 0.7182679738566000172, 0.7430147058827000217, 0.7677614379088000263, 0.7925081699349000308, 0.8172549019609999243, 0.8420016339870999289, 0.8667483660132000445, 0.8914950980394000801, 0.9162418300655000847, 0.9409885620915999782, 0.9657352941176999828, 0.9904820261437999873, 1.015228758169999912 ),
 .UNSPECIFIED. ) ;
#21091 = DIRECTION ( 'NONE',  ( 1.000000000000000000, 0.000000000000000000, 0.000000000000000000 ) ) ;
#21092 = CARTESIAN_POINT ( 'NONE',  ( 12.19636843800076953, -0.1422577892986798820, 13.89902525486551887 ) ) ;
#21093 = VERTEX_POINT ( 'NONE', #46894 ) ;
#21094 = CARTESIAN_POINT ( 'NONE',  ( 12.64393528606200334, 11.55448221446000012, -4.935476321030999536 ) ) ;
#21095 = CARTESIAN_POINT ( 'NONE',  ( 18.14021164098500094, 11.49417283396999956, -4.331891014347999835 ) ) ;
#21096 = CARTESIAN_POINT ( 'NONE',  ( 9.784141369869628235, 4.423591863150092784, 6.734426879786121312 ) ) ;
#21097 = CARTESIAN_POINT ( 'NONE',  ( 8.424688440789097399, -5.350083765069893360, 7.500019236172019710 ) ) ;
#21098 = ADVANCED_FACE ( 'NONE', ( #53851 ), #16781, .F. ) ;
#21099 = CARTESIAN_POINT ( 'NONE',  ( 8.947714158774999760, 3.854507394315999758, -9.394302886912999639 ) ) ;
#21100 = CARTESIAN_POINT ( 'NONE',  ( 18.26281727343199890, -2.856883730594999893, 11.95041273044000008 ) ) ;
#21101 = CARTESIAN_POINT ( 'NONE',  ( 10.69578225082999978, -5.505007625740000243, -7.759264430206000540 ) ) ;
#21102 = ORIENTED_EDGE ( 'NONE', *, *, #58230, .T. ) ;
#21103 = ORIENTED_EDGE ( 'NONE', *, *, #1228, .F. ) ;
#21104 = CARTESIAN_POINT ( 'NONE',  ( 10.90728307559000143, 5.030511622218999612, -4.935980611296999498 ) ) ;
#21105 = DIRECTION ( 'NONE',  ( 1.000000000000000000, 0.000000000000000000, 0.000000000000000000 ) ) ;
#21106 = CARTESIAN_POINT ( 'NONE',  ( 12.29688428857270388, -2.864514977104569038, 13.58937626179410962 ) ) ;
#21107 = CARTESIAN_POINT ( 'NONE',  ( 5.896693173016667622, 1.310679582531385279, 0.7554284705563519831 ) ) ;
#21108 = DIRECTION ( 'NONE',  ( 0.000000000000000000, 1.000000000000000000, 0.000000000000000000 ) ) ;
#21109 = CARTESIAN_POINT ( 'NONE',  ( 9.484696787962999309, 4.148886440911999429, -6.645868410478299459 ) ) ;
#21111 = CARTESIAN_POINT ( 'NONE',  ( 8.422931970811326607, 5.091594506052739000, -6.480649903393177702 ) ) ;
#21110 = CARTESIAN_POINT ( 'NONE',  ( 9.825734463322998380, -3.895375416816699854, 6.501052555474699624 ) ) ;
#21112 = CARTESIAN_POINT ( 'NONE',  ( 7.964385314170995933, -2.867871570892000399, 6.759005350280994584 ) ) ;
#21113 = ORIENTED_EDGE ( 'NONE', *, *, #15328, .T. ) ;
#21114 = B_SPLINE_CURVE_WITH_KNOTS ( 'NONE', 3,
 ( #944, #58630, #22257, #53732, #43596, #10732, #596, #64894, #59666, #11763 ),
 .UNSPECIFIED., .F., .F.,
 ( 4, 2, 2, 2, 4 ),
 ( 0.000000000000000000, 0.2500000000000000000, 0.5000000000000000000, 0.7500000000000000000, 1.000000000000000000 ),
 .UNSPECIFIED. ) ;
#21115 = CARTESIAN_POINT ( 'NONE',  ( 9.789763540182331525, 3.672815144550904076, -6.282534154164603812 ) ) ;
#21116 = CARTESIAN_POINT ( 'NONE',  ( 11.09999999999999964, -5.449702618175999547, 5.124965750789000296 ) ) ;
#21117 = CARTESIAN_POINT ( 'NONE',  ( 9.481734463323000739, 4.133249246727800141, 6.227746477418000026 ) ) ;
#21118 = CARTESIAN_POINT ( 'NONE',  ( 8.807788144226000426, 4.090932644426789722, -8.453461841935100196 ) ) ;
#21119 = AXIS2_PLACEMENT_3D ( 'NONE', #25175, #60259, #12363 ) ;
#21120 = CARTESIAN_POINT ( 'NONE',  ( 9.305875415870998424, -4.945293979885000191, 9.077881967919999795 ) ) ;
#21121 = CARTESIAN_POINT ( 'NONE',  ( 18.17055204341999897, 2.609142802180001830, -12.42550174407591079 ) ) ;
#21122 = DIRECTION ( 'NONE',  ( 0.000000000000000000, 2.692747184616903860E-07, -0.9999999999999636957 ) ) ;
#21123 = CARTESIAN_POINT ( 'NONE',  ( 13.73937158902900180, 8.990218567665001714, 7.348698335466000486 ) ) ;
#21124 = DIRECTION ( 'NONE',  ( 1.000000000000000000, 0.000000000000000000, 0.000000000000000000 ) ) ;
#21125 = CARTESIAN_POINT ( 'NONE',  ( 9.358051052051999719, -3.149129950522900234, -7.666517576877299511 ) ) ;
#21126 = CARTESIAN_POINT ( 'NONE',  ( 6.304962922411999848, 0.03531958898060999497, -1.468087261088999895 ) ) ;
#21127 = CARTESIAN_POINT ( 'NONE',  ( 11.17375944625267792, -4.674697381537265883, 6.944236520041479288 ) ) ;
#21128 = DIRECTION ( 'NONE',  ( -1.000000000000000000, 0.000000000000000000, 0.000000000000000000 ) ) ;
#21129 = CARTESIAN_POINT ( 'NONE',  ( 18.11007341752287658, -3.284452655023379908, -11.17744038474783252 ) ) ;
#21130 = VERTEX_POINT ( 'NONE', #6643 ) ;
#21131 = EDGE_CURVE ( 'NONE', #18501, #31887, #44420, .T. ) ;
#21132 = EDGE_CURVE ( 'NONE', #32339, #44819, #50017, .T. ) ;
#21133 = CARTESIAN_POINT ( 'NONE',  ( 12.27392562293325362, 0.3300695133819715466, -12.69424233780836531 ) ) ;
#21134 = CARTESIAN_POINT ( 'NONE',  ( 11.83518044953559922, 4.768048975940600620, -7.900497508315099893 ) ) ;
#21135 = CARTESIAN_POINT ( 'NONE',  ( 16.39999999231800132, -3.216285993016000155, -11.40340220863999932 ) ) ;
#21136 = LINE ( 'NONE', #26732, #58029 ) ;
#21137 = CARTESIAN_POINT ( 'NONE',  ( 1.748890132541458753, -2.798833948393641080, 2.150913519912190708 ) ) ;
#21138 = VERTEX_POINT ( 'NONE', #44760 ) ;
#21139 = DIRECTION ( 'NONE',  ( 1.000000000000000000, 0.000000000000000000, 0.000000000000000000 ) ) ;
#21140 = EDGE_CURVE ( 'NONE', #41725, #55934, #29102, .T. ) ;
#21141 = CARTESIAN_POINT ( 'NONE',  ( 10.56591429142999949, -3.980313504646230349, -6.466681092390999197 ) ) ;
#21142 = CARTESIAN_POINT ( 'NONE',  ( 24.59231629583900158, -8.769512118076001173, -9.082544788674999481 ) ) ;
#21143 = CARTESIAN_POINT ( 'NONE',  ( 10.45851354018287616, -4.163624617374470205, 6.250000000000000000 ) ) ;
#21144 = DIRECTION ( 'NONE',  ( 0.000000000000000000, 1.000000000000000000, 0.000000000000000000 ) ) ;
#21145 = CARTESIAN_POINT ( 'NONE',  ( 10.69568717260499824, 3.533932086969799879, -8.260703168378098482 ) ) ;
#21146 = ORIENTED_EDGE ( 'NONE', *, *, #62724, .T. ) ;
#21147 = CARTESIAN_POINT ( 'NONE',  ( 10.30047649312000146, -4.027768368024999823, 9.431342508940000258 ) ) ;
#21148 = CARTESIAN_POINT ( 'NONE',  ( 17.80560960443411389, 3.072671113640228491, -13.53517819557379021 ) ) ;
#21149 = VERTEX_POINT ( 'NONE', #55588 ) ;
#21150 = CARTESIAN_POINT ( 'NONE',  ( 13.67905361531532016, 11.43958844919915308, 2.204572756910269771 ) ) ;
#21151 = CARTESIAN_POINT ( 'NONE',  ( 7.390495559621999888, -2.216884807317999861, 8.370075800106999253 ) ) ;
#21152 = PLANE ( 'NONE',  #12100 ) ;
#21153 = ORIENTED_EDGE ( 'NONE', *, *, #8914, .T. ) ;
#21154 = CARTESIAN_POINT ( 'NONE',  ( 24.30000000000000071, 0.000000000000000000, 0.000000000000000000 ) ) ;
#21155 = CARTESIAN_POINT ( 'NONE',  ( 7.274445280404999714, 5.732054911314000023, -7.535918460973999977 ) ) ;
#21156 = CARTESIAN_POINT ( 'NONE',  ( 12.80505043854146940, -3.149899482173124987, -12.25147293255931125 ) ) ;
#21157 = CARTESIAN_POINT ( 'NONE',  ( 7.260912495782270604, 3.646496072872962735, -8.815167414925308975 ) ) ;
#21158 = ORIENTED_EDGE ( 'NONE', *, *, #30641, .F. ) ;
#21159 = CARTESIAN_POINT ( 'NONE',  ( 11.05639424537999993, -5.030223832177999732, 6.028291574375000295 ) ) ;
#21160 = CARTESIAN_POINT ( 'NONE',  ( 24.37898895918399944, 12.00803319959000071, -3.275429579010999959 ) ) ;
#21161 = CARTESIAN_POINT ( 'NONE',  ( 11.79999999550100220, -3.351258778187000242, 11.15757272551999968 ) ) ;
#21162 = ORIENTED_EDGE ( 'NONE', *, *, #45342, .F. ) ;
#21163 = CARTESIAN_POINT ( 'NONE',  ( 6.127943173016666911, -0.9218200799623714747, -1.199500263597270466 ) ) ;
#21164 = ORIENTED_EDGE ( 'NONE', *, *, #36724, .F. ) ;
#21165 = CARTESIAN_POINT ( 'NONE',  ( 24.34832117038932964, 3.224867649022901794, 12.03536991383494303 ) ) ;
#21166 = CARTESIAN_POINT ( 'NONE',  ( 17.92061031166187846, -1.858910711595921583, -12.46212218156369111 ) ) ;
#21167 = CARTESIAN_POINT ( 'NONE',  ( 11.39043504475232815, 2.929202812228125730, -8.202738646980327175 ) ) ;
#21168 = CARTESIAN_POINT ( 'NONE',  ( 8.093993643936004290, 4.563399802036997244, -6.204632025667001116 ) ) ;
#21169 = DIRECTION ( 'NONE',  ( -1.000000000000000000, 0.000000000000000000, 0.000000000000000000 ) ) ;
#21170 = CARTESIAN_POINT ( 'NONE',  ( 23.84134131727602224, 12.96058960459414955, 3.649550007566405352 ) ) ;
#21171 = ORIENTED_EDGE ( 'NONE', *, *, #23066, .F. ) ;
#21172 = CARTESIAN_POINT ( 'NONE',  ( 8.295839940244002619, -5.118638632597003912, 6.383292232312004266 ) ) ;
#21173 = ORIENTED_EDGE ( 'NONE', *, *, #1177, .F. ) ;
#21174 = CARTESIAN_POINT ( 'NONE',  ( 9.409415556003999370, 2.113395950889999764, 7.914199712930999553 ) ) ;
#21175 = CARTESIAN_POINT ( 'NONE',  ( 10.56983915876999980, 2.152856944368999770, -7.425100664021000441 ) ) ;
#21176 = FACE_OUTER_BOUND ( 'NONE', #24695, .T. ) ;
#21177 = CARTESIAN_POINT ( 'NONE',  ( 12.21870270123686275, 2.283379404039359351, -13.71702370352176281 ) ) ;
#21178 = LINE ( 'NONE', #37261, #64992 ) ;
#21179 = CARTESIAN_POINT ( 'NONE',  ( 25.59994555223600088, -10.09686240769181609, -5.033199831111830669 ) ) ;
#21180 = EDGE_CURVE ( 'NONE', #44978, #25385, #4928, .T. ) ;
#21181 = CARTESIAN_POINT ( 'NONE',  ( 18.15028930682391106, -0.1908382484571597981, 13.89824168789395920 ) ) ;
#21182 = DIRECTION ( 'NONE',  ( -4.063589742475669988E-14, 0.8660931406617480288, 0.4998826579295080341 ) ) ;
#21183 = ORIENTED_EDGE ( 'NONE', *, *, #20597, .T. ) ;
#21184 = CARTESIAN_POINT ( 'NONE',  ( 12.50062609531600089, -11.46460001353999836, 4.648225426428999718 ) ) ;
#21185 = CARTESIAN_POINT ( 'NONE',  ( 11.31349144726329925, -4.738947899111299655, 8.542723541016000510 ) ) ;
#21186 = CARTESIAN_POINT ( 'NONE',  ( 18.12842152809865937, -0.2489677813733684741, -13.89700419708378298 ) ) ;
#21187 = CARTESIAN_POINT ( 'NONE',  ( 8.502043146794999728, -3.869396851328000153, 5.695656592546999519 ) ) ;
#21188 = AXIS2_PLACEMENT_3D ( 'NONE', #31046, #64207, #64552 ) ;
#21190 = CARTESIAN_POINT ( 'NONE',  ( 9.674960421382234443, 2.650268802166420024, 7.499999178247376719 ) ) ;
#21189 = CARTESIAN_POINT ( 'NONE',  ( 10.03490996941999924, 5.615906393494999982, 7.351455918368999143 ) ) ;
#21191 = CARTESIAN_POINT ( 'NONE',  ( 11.15810538575740019, 5.242981041160000188, -7.202822423614300362 ) ) ;
#21192 = B_SPLINE_CURVE_WITH_KNOTS ( 'NONE', 3,
 ( #5779, #47762, #11368, #43195 ),
 .UNSPECIFIED., .F., .F.,
 ( 4, 4 ),
 ( 0.000000000000000000, 1.000000000000000000 ),
 .UNSPECIFIED. ) ;
#21193 = CARTESIAN_POINT ( 'NONE',  ( 25.29881449893400003, -11.38089007393000074, 3.116294150075999969 ) ) ;
#21194 = CARTESIAN_POINT ( 'NONE',  ( 9.880963142879998884, 4.848366390061300102, -7.321163726496699553 ) ) ;
#21195 = CARTESIAN_POINT ( 'NONE',  ( 17.93128725136842760, -0.4990964484179727378, 12.68679736436866712 ) ) ;
#21196 = CARTESIAN_POINT ( 'NONE',  ( 6.973780705993999796, 0.1816583604578000111, -1.117739201043999930 ) ) ;
#21197 = CARTESIAN_POINT ( 'NONE',  ( 24.13682259839000110, 9.106542476583999957, 8.984439671043000786 ) ) ;
#21198 = VERTEX_POINT ( 'NONE', #13633 ) ;
#21199 = CARTESIAN_POINT ( 'NONE',  ( 7.711433059622000208, -5.797088532631000213, 8.340479314546998424 ) ) ;
#21200 = CARTESIAN_POINT ( 'NONE',  ( 9.069724726289001282, -4.108965473266000146, 8.851626696081998702 ) ) ;
#21201 = CARTESIAN_POINT ( 'NONE',  ( 5.500000000000000000, 0.000000000000000000, 0.000000000000000000 ) ) ;
#21202 = DIRECTION ( 'NONE',  ( 0.000000000000000000, 0.000000000000000000, 1.000000000000000000 ) ) ;
#21203 = ORIENTED_EDGE ( 'NONE', *, *, #48616, .T. ) ;
#21204 = CARTESIAN_POINT ( 'NONE',  ( 18.26122879894100137, 2.828234032943000020, 11.95647652451000020 ) ) ;
#21205 = CARTESIAN_POINT ( 'NONE',  ( 11.15278751119019773, 3.209519379020799867, 7.086443476450299706 ) ) ;
#21206 = CARTESIAN_POINT ( 'NONE',  ( 2.790793788209000148, -3.707132657157000022, -0.6209224904536000400 ) ) ;
#21207 = ORIENTED_EDGE ( 'NONE', *, *, #66523, .F. ) ;
#21208 = EDGE_CURVE ( 'NONE', #47368, #54348, #43328, .T. ) ;
#21209 = ADVANCED_FACE ( 'NONE', ( #60828 ), #56616, .T. ) ;
#21210 = B_SPLINE_CURVE_WITH_KNOTS ( 'NONE', 3,
 ( #21452, #68309, #48032, #42788 ),
 .UNSPECIFIED., .F., .F.,
 ( 4, 4 ),
 ( 0.000000000000000000, 1.000000000000000000 ),
 .UNSPECIFIED. ) ;
#21211 = CARTESIAN_POINT ( 'NONE',  ( 12.78109913421143418, -0.7192906882580946126, -12.57945229568000656 ) ) ;
#21212 = CARTESIAN_POINT ( 'NONE',  ( 10.08521345716899908, 4.924890298941200228, -8.340879262988799780 ) ) ;
#21213 = CARTESIAN_POINT ( 'NONE',  ( 18.10200918459796426, 2.953257374879727948, -12.24902512628088402 ) ) ;
#21214 = CARTESIAN_POINT ( 'NONE',  ( 7.225322421146570306, -2.650264760010439868, 7.500018091723870128 ) ) ;
#21215 = CARTESIAN_POINT ( 'NONE',  ( 12.80505043854143388, 3.124999999999999556, 13.52078605991414939 ) ) ;
#21216 = ORIENTED_EDGE ( 'NONE', *, *, #558, .F. ) ;
#21217 = CARTESIAN_POINT ( 'NONE',  ( 29.60000000000000142, 0.000000000000000000, -8.250000000000000000 ) ) ;
#21218 = EDGE_CURVE ( 'NONE', #23850, #64065, #35804, .T. ) ;
#21219 = EDGE_CURVE ( 'NONE', #19719, #12749, #35770, .T. ) ;
#21220 = CARTESIAN_POINT ( 'NONE',  ( 7.707204719585000419, 2.598436872309000112, -6.481704782070000448 ) ) ;
#21221 = CARTESIAN_POINT ( 'NONE',  ( 8.541897605312588126, -3.315623613928524005, 5.901107281712603125 ) ) ;
#21222 = CARTESIAN_POINT ( 'NONE',  ( 10.91991225946278199, -3.299232917623651229, -6.977491532540834207 ) ) ;
#21223 = VERTEX_POINT ( 'NONE', #39855 ) ;
#21224 = CARTESIAN_POINT ( 'NONE',  ( 2.917640132543333209, 1.762666431298152370, -3.058252359239900464 ) ) ;
#21225 = CARTESIAN_POINT ( 'NONE',  ( 11.80585503023100102, 11.57020517019000039, 1.758699328329000222 ) ) ;
#21226 = EDGE_LOOP ( 'NONE', ( #5630, #17543, #24386, #25521, #59838, #3547, #64642 ) ) ;
#21227 = CARTESIAN_POINT ( 'NONE',  ( 12.61539589080907042, 1.784264304835224690, -12.47303049908422778 ) ) ;
#21228 = FACE_OUTER_BOUND ( 'NONE', #45114, .T. ) ;
#21229 = CARTESIAN_POINT ( 'NONE',  ( 9.161916987464291395, 2.900038627299713401, -6.155438822667427701 ) ) ;
#21230 = VERTEX_POINT ( 'NONE', #67431 ) ;
#21231 = DIRECTION ( 'NONE',  ( 0.000000000000000000, 0.000000000000000000, -1.000000000000000000 ) ) ;
#21232 = CARTESIAN_POINT ( 'NONE',  ( 11.02301463001509774, 4.547357026650399980, -6.623338154204899908 ) ) ;
#21233 = CARTESIAN_POINT ( 'NONE',  ( 12.80505043854143388, 3.124999999999999556, -12.28374638332999602 ) ) ;
#21234 = CARTESIAN_POINT ( 'NONE',  ( 11.48579841651039857, -4.449968941611500028, 6.303820944768999901 ) ) ;
#21235 = VERTEX_POINT ( 'NONE', #3127 ) ;
#21236 = CARTESIAN_POINT ( 'NONE',  ( 7.191892219589999691, 3.501518846194999757, 9.055971388486000251 ) ) ;
#21237 = EDGE_CURVE ( 'NONE', #51258, #14644, #8287, .T. ) ;
#21238 = ORIENTED_EDGE ( 'NONE', *, *, #18028, .T. ) ;
#21239 = CIRCLE ( 'NONE', #8965, 11.55000444562000439 ) ;
#21240 = CARTESIAN_POINT ( 'NONE',  ( 9.458513540183334456, 3.836375382625530239, -8.749999999999998224 ) ) ;
#21241 = B_SPLINE_CURVE_WITH_KNOTS ( 'NONE', 3,
 ( #50645, #45061, #7302, #18836 ),
 .UNSPECIFIED., .F., .F.,
 ( 4, 4 ),
 ( 0.000000000000000000, 1.000000000000000000 ),
 .UNSPECIFIED. ) ;
#21242 = CARTESIAN_POINT ( 'NONE',  ( 11.52285868696541726, -3.940189611494480992, -8.771870505746530711 ) ) ;
#21243 = CARTESIAN_POINT ( 'NONE',  ( 4.699998537092440642, 0.000000000000000000, 0.000000000000000000 ) ) ;
#21244 = EDGE_LOOP ( 'NONE', ( #33200, #54723, #66023, #6871 ) ) ;
#21245 = B_SPLINE_SURFACE_WITH_KNOTS ( 'NONE', 3, 3, ( 
 ( #17218, #54272, #1487, #6371, #53927, #11618, #25727, #64402, #16524, #9989, #68364, #65094, #20483, #38543, #59865, #448, #41809, #36565, #32616, #27721, #43798, #33307, #6722, #57889, #59176, #21763, #36221, #6029, #31327, #52638, #5686, #43100, #37852, #11275, #48693 ),
 ( #795, #24189, #38898, #45526, #65795, #50767, #55670, #66837, #18263, #50416, #39583, #44839, #50077, #18948, #7072, #8115, #1834, #60219, #17571, #7768, #66486, #2861, #51108, #2184, #40277, #39238, #56008, #12324, #60907, #2519, #23846, #28411, #13372, #45181, #61594 ),
 ( #66145, #60563, #44153, #33655, #35040, #54972, #18609, #29110, #39937, #29459, #22803, #12670, #61254, #34697, #65451, #13025, #49725, #13711, #44501, #56354, #23152, #17920, #34351, #8460, #34001, #23498, #55319, #7415, #29805, #28764, #36398, #4229, #67516, #52473, #15072 ),
 ( #57714, #25908, #35717, #15424, #19286, #52125, #57368, #20316, #9822, #3210, #19637, #25566, #41643, #45863, #41304, #24538, #46893, #24879, #9472, #51448, #67172, #46555, #62949, #40611, #3884, #46209, #31502, #47238, #31170, #4571, #68197, #40958, #68541, #20664, #67858 ) ),
 .UNSPECIFIED., .F., .F., .F.,
 ( 4, 4 ),
 ( 4, 1, 1, 1, 1, 1, 1, 1, 1, 1, 1, 1, 1, 1, 1, 1, 1, 1, 1, 1, 1, 1, 1, 1, 1, 1, 1, 1, 1, 1, 1, 1, 4 ),
 ( -0.1039086239011999951, 1.103908623900999864 ),
 ( -0.01735257130020999988, 0.01084535706264999969, 0.03904328542550000031, 0.06724121378835999641, 0.09543914215121999944, 0.1236370705141000004, 0.1518349988768999959, 0.1800329272397999947, 0.2082308556026999935, 0.2364287839655000167, 0.2646267123283999601, 0.2928246406912000110, 0.3210225690540999821, 0.3492204974169000331, 0.3774184257798000042, 0.4056163541427000307, 0.4338142825054999707, 0.4620122108683999973, 0.4902101392311999928, 0.5184080675940999638, 0.5466059959569999904, 0.5748039243197999859, 0.6030018526827000125, 0.6311997810455000080, 0.6593977094084000345, 0.6875956377712000300, 0.7157935661340999456, 0.7439914944969999722, 0.7721894228597999676, 0.8003873512226999942, 0.8285852795854999897, 0.8567832079484000163, 0.8849811363112999318 ),
 .UNSPECIFIED. ) ;
#21246 = CARTESIAN_POINT ( 'NONE',  ( 12.47171258541606420, -1.971212359000197090, -12.55915788719762638 ) ) ;
#21247 = CARTESIAN_POINT ( 'NONE',  ( 9.020081723712005228, 10.01659799728000522, -5.797890173437007633 ) ) ;
#21248 = DIRECTION ( 'NONE',  ( -1.000000000000000000, 0.000000000000000000, 0.000000000000000000 ) ) ;
#21249 = LINE ( 'NONE', #68440, #22982 ) ;
#21250 = CARTESIAN_POINT ( 'NONE',  ( 12.47131944427646388, -1.869655113073437347, -13.87459630548517886 ) ) ;
#21251 = CARTESIAN_POINT ( 'NONE',  ( 11.65871932425156920, -4.147141405561299621, -8.492622906483498824 ) ) ;
#21252 = FACE_OUTER_BOUND ( 'NONE', #69094, .T. ) ;
#21253 = CARTESIAN_POINT ( 'NONE',  ( 18.14791645918234764, -2.065340611094598433, 12.42959220787597374 ) ) ;
#21254 = VERTEX_POINT ( 'NONE', #58673 ) ;
#21255 = CARTESIAN_POINT ( 'NONE',  ( 10.96239488738000034, -5.423100855659000352, -4.905500182035000378 ) ) ;
#21256 = ORIENTED_EDGE ( 'NONE', *, *, #50671, .F. ) ;
#21257 = DIRECTION ( 'NONE',  ( 1.000000000000000000, 0.000000000000000000, 0.000000000000000000 ) ) ;
#21258 = DIRECTION ( 'NONE',  ( -1.000000000000000000, 5.085933197601780420E-15, -5.275114267344730344E-15 ) ) ;
#21259 = CARTESIAN_POINT ( 'NONE',  ( 4.900006121741999898, -0.5234957687185584074, 1.947945353336631991 ) ) ;
#21260 = CARTESIAN_POINT ( 'NONE',  ( 10.23643409129999959, 5.517148499152000340, -6.754126239302999934 ) ) ;
#21261 = PLANE ( 'NONE',  #44405 ) ;
#21262 = ADVANCED_FACE ( 'NONE', ( #10772 ), #38038, .F. ) ;
#21263 = CARTESIAN_POINT ( 'NONE',  ( 23.66004879239100234, -13.39256464007999980, -3.813546745462999876 ) ) ;
#21264 = CARTESIAN_POINT ( 'NONE',  ( 15.95377458853735853, 3.445704530244193098, 11.33538647441605640 ) ) ;
#21265 = CARTESIAN_POINT ( 'NONE',  ( 17.65333285645861139, -3.199628934752127840, -12.18697561682396646 ) ) ;
#21266 = ORIENTED_EDGE ( 'NONE', *, *, #45869, .T. ) ;
#21267 = EDGE_CURVE ( 'NONE', #62089, #53586, #7407, .T. ) ;
#21268 = CARTESIAN_POINT ( 'NONE',  ( 10.32322128467999889, -3.399999874579999748, -4.621083553505000552 ) ) ;
#21269 = CARTESIAN_POINT ( 'NONE',  ( 9.533434135307000901, 2.564753581125000181, 6.150586364588000343 ) ) ;
#21270 = CARTESIAN_POINT ( 'NONE',  ( 5.000000000000000000, 0.000000000000000000, 0.000000000000000000 ) ) ;
#21271 = CARTESIAN_POINT ( 'NONE',  ( 11.10746886766490071, -4.498335456194499926, 8.405426684175299812 ) ) ;
#21273 = B_SPLINE_CURVE_WITH_KNOTS ( 'NONE', 3,
 ( #30081, #57304, #61871, #56633, #35987, #9407, #20253, #58005, #10104, #68135, #26194, #41579, #14334, #20596, #68824, #41921, #9072, #41239 ),
 .UNSPECIFIED., .F., .F.,
 ( 4, 2, 2, 2, 2, 2, 2, 2, 4 ),
 ( 0.000000000000000000, 0.1250000000000000000, 0.2500000000000000000, 0.3750000000000000000, 0.5000000000000000000, 0.6250000000000000000, 0.7500000000000000000, 0.8750000000000000000, 1.000000000000000000 ),
 .UNSPECIFIED. ) ;
#21272 = CARTESIAN_POINT ( 'NONE',  ( 18.44503807197100187, 2.664600154114999953, -11.39639460691000039 ) ) ;
#21274 = CARTESIAN_POINT ( 'NONE',  ( 11.34287482311539996, 4.803125295093300551, -7.824481664695199790 ) ) ;
#21275 = VECTOR ( 'NONE', #1322, 1000.000000000000114 ) ;
#21276 = CARTESIAN_POINT ( 'NONE',  ( 12.23133867660517282, -0.2481623978058218327, 12.69674179789668500 ) ) ;
#21277 = CARTESIAN_POINT ( 'NONE',  ( 9.187739158772000536, 5.964723767581000757, 7.776480083716999836 ) ) ;
#21278 = CARTESIAN_POINT ( 'NONE',  ( 9.970944094204998720, -5.100000000000000533, 6.571291218949999902 ) ) ;
#21279 = CARTESIAN_POINT ( 'NONE',  ( 9.198982189547734833, -2.717686045645804960, 7.939987363064203052 ) ) ;
#21280 = EDGE_LOOP ( 'NONE', ( #608, #31152, #29569, #14306 ) ) ;
#21281 = CARTESIAN_POINT ( 'NONE',  ( 9.468110841233000841, 4.082930418187999955, -6.104944817728999773 ) ) ;
#21282 = CARTESIAN_POINT ( 'NONE',  ( 6.895243336750000118, -0.9527829703796000249, 0.9274460053021000849 ) ) ;
#21283 = CARTESIAN_POINT ( 'NONE',  ( 17.88684482918178986, 3.030051203688146622, 13.54658895838268684 ) ) ;
#21284 = CARTESIAN_POINT ( 'NONE',  ( 3.489623894411582938, 3.494155582390569670, -0.4991450110755751290 ) ) ;
#21285 = PLANE ( 'NONE',  #38996 ) ;
#21286 = AXIS2_PLACEMENT_3D ( 'NONE', #42292, #52071, #14683 ) ;
#21287 = CARTESIAN_POINT ( 'NONE',  ( 11.53148876160955005, -4.790673964186999534, -8.322268080792200706 ) ) ;
#21288 = ORIENTED_EDGE ( 'NONE', *, *, #67549, .F. ) ;
#21289 = CARTESIAN_POINT ( 'NONE',  ( 2.487975856965999988, 3.176854988377000311, -1.562936765141999862 ) ) ;
#21290 = CARTESIAN_POINT ( 'NONE',  ( 18.18005043853712976, -0.02024571653066400273, -12.69999991888706958 ) ) ;
#21293 = CARTESIAN_POINT ( 'NONE',  ( 10.14393020684900115, -2.750000000000000000, 7.500000000000000000 ) ) ;
#21292 = UNCERTAINTY_MEASURE_WITH_UNIT (LENGTH_MEASURE( 1.000000000000000082E-05 ), #8573, 'distance_accuracy_value', 'NONE');
#21291 = CARTESIAN_POINT ( 'NONE',  ( 8.216604719590000272, 5.331510020787000315, -8.114341808290998159 ) ) ;
#21294 = CARTESIAN_POINT ( 'NONE',  ( 2.436201009244109983, -1.386434525806842011, 2.948195033656590081 ) ) ;
#21295 = EDGE_LOOP ( 'NONE', ( #26699, #31829, #14173, #3610 ) ) ;
#21296 = CARTESIAN_POINT ( 'NONE',  ( 11.27765994926999937, 3.273804980682999854, 6.368305648407000419 ) ) ;
#21297 = CARTESIAN_POINT ( 'NONE',  ( 18.17486206286454120, -2.582858869840499061, -13.65550477088448034 ) ) ;
#21298 = CARTESIAN_POINT ( 'NONE',  ( 10.85056919669530018, 4.830699382454300306, 7.254567470917099747 ) ) ;
#21299 = CARTESIAN_POINT ( 'NONE',  ( 10.59303089732000025, -2.436232726560000117, 7.793465286118999913 ) ) ;
#21300 = CARTESIAN_POINT ( 'NONE',  ( 7.935745559623000212, -5.430412429559000387, 7.210798766422999329 ) ) ;
#21301 = ORIENTED_EDGE ( 'NONE', *, *, #20689, .F. ) ;
#21302 = CARTESIAN_POINT ( 'NONE',  ( 7.839801658770999992, 3.084076314893000159, 9.259847992573000397 ) ) ;
#21303 = EDGE_CURVE ( 'NONE', #34155, #4646, #25735, .T. ) ;
#21304 = EDGE_CURVE ( 'NONE', #10663, #57286, #59165, .T. ) ;
#21306 = CARTESIAN_POINT ( 'NONE',  ( 9.888320559623000605, -5.105186397454999359, -8.895598708036001057 ) ) ;
#21305 = CARTESIAN_POINT ( 'NONE',  ( 10.82145113417867677, 4.723115832319042084, -7.991114136793449951 ) ) ;
#21307 = CARTESIAN_POINT ( 'NONE',  ( 7.746088648720403036, -5.452065268544131982, 8.457849491477853476 ) ) ;
#21308 = CARTESIAN_POINT ( 'NONE',  ( 25.60000000000000142, 2.976419018679000050, 11.10814700232000085 ) ) ;
#21309 = CARTESIAN_POINT ( 'NONE',  ( 24.63626838744500347, 3.694701704419999899, 12.29747005844000007 ) ) ;
#21310 = ORIENTED_EDGE ( 'NONE', *, *, #32996, .T. ) ;
#21311 = CYLINDRICAL_SURFACE ( 'NONE', #24340, 11.50000000000000178 ) ;
#21312 = CARTESIAN_POINT ( 'NONE',  ( 11.14949279009019989, -4.260984538213099526, 6.531063508962500208 ) ) ;
#21313 = CARTESIAN_POINT ( 'NONE',  ( 10.51810807141099779, 4.059045408506610109, 6.223352037434000117 ) ) ;
#21314 = ORIENTED_EDGE ( 'NONE', *, *, #12938, .F. ) ;
#21315 = CARTESIAN_POINT ( 'NONE',  ( 9.791229719590001324, 4.294368353031000396, -8.968663198664000191 ) ) ;
#21316 = VECTOR ( 'NONE', #14505, 1000.000000000000114 ) ;
#21317 = CARTESIAN_POINT ( 'NONE',  ( 12.78084734971786673, 1.760846085845573006, -12.47635444213890032 ) ) ;
#21318 = CARTESIAN_POINT ( 'NONE',  ( 11.68412378248529926, -4.549028353065900809, 8.538714411016998795 ) ) ;
#21319 = EDGE_CURVE ( 'NONE', #17831, #40269, #2321, .T. ) ;
#21320 = CARTESIAN_POINT ( 'NONE',  ( 25.27036424497699940, -2.549213983724999633, -11.36408287613999946 ) ) ;
#21321 = DIRECTION ( 'NONE',  ( 9.801401651172999747E-11, -9.801400427915999291E-11, 1.000000000000000000 ) ) ;
#21322 = VERTEX_POINT ( 'NONE', #21268 ) ;
#21323 = CARTESIAN_POINT ( 'NONE',  ( 3.899999681170999821, 0.000000000000000000, 0.000000000000000000 ) ) ;
#21324 = CARTESIAN_POINT ( 'NONE',  ( 23.76529091359962464, 9.791724092508008681, 9.440860067983548376 ) ) ;
#21326 = ORIENTED_EDGE ( 'NONE', *, *, #46796, .T. ) ;
#21325 = VECTOR ( 'NONE', #58065, 1000.000000000000000 ) ;
#21327 = DIRECTION ( 'NONE',  ( 0.000000000000000000, -1.000000000000000000, 0.000000000000000000 ) ) ;
#21328 = CARTESIAN_POINT ( 'NONE',  ( 11.38795122972049967, 4.398282450130399646, 8.421043941822800249 ) ) ;
#21329 = CARTESIAN_POINT ( 'NONE',  ( 24.63329087101643111, -8.756202933458791193, 7.455126436760659558 ) ) ;
#21330 = CARTESIAN_POINT ( 'NONE',  ( 10.58996475420000039, 2.876740601533999797, -6.236530348556999392 ) ) ;
#21331 = DIRECTION ( 'NONE',  ( -1.000000000000000000, -0.000000000000000000, -0.000000000000000000 ) ) ;
#21332 = CARTESIAN_POINT ( 'NONE',  ( 9.945535518573000999, -2.906050966242999856, 8.880386511481999534 ) ) ;
#21333 = CARTESIAN_POINT ( 'NONE',  ( 17.60287381234529036, -0.7178228174669354367, -12.57953618971562193 ) ) ;
#21334 = CONICAL_SURFACE ( 'NONE', #60413, 1.449999999965999375, 0.7853981633972997312 ) ;
#21335 = CARTESIAN_POINT ( 'NONE',  ( 9.028524608540857699, 5.063478752693338691, 8.333910756878536219 ) ) ;
#21336 = CARTESIAN_POINT ( 'NONE',  ( 10.89564560330029863, -3.692495237344800341, -6.544808043482999160 ) ) ;
#21337 = CARTESIAN_POINT ( 'NONE',  ( 7.635857780409000206, 2.466388272391000225, 6.935562100014999842 ) ) ;
#21338 = VERTEX_POINT ( 'NONE', #31423 ) ;
#21339 = CARTESIAN_POINT ( 'NONE',  ( 11.09999999999999787, 2.396165420595747442, -6.907370999140288959 ) ) ;
#21340 = CARTESIAN_POINT ( 'NONE',  ( 24.53428988874600236, -8.855929874993998752, -9.286429786912000495 ) ) ;
#21341 = CARTESIAN_POINT ( 'NONE',  ( 4.599999999999999645, 3.199751711897561357, -12.18694338143115452 ) ) ;
#21342 = CARTESIAN_POINT ( 'NONE',  ( 18.03534466112214929, 3.019381283786335413, 12.23288205540259632 ) ) ;
#21343 = AXIS2_PLACEMENT_3D ( 'NONE', #37405, #63625, #53488 ) ;
#21344 = CARTESIAN_POINT ( 'NONE',  ( 11.07206066007000089, 6.377621165504000267, 5.347654869262000510 ) ) ;
#21346 = CARTESIAN_POINT ( 'NONE',  ( 10.85407964676000070, 9.831998789269000838, 5.581261321082999771 ) ) ;
#21345 = B_SPLINE_CURVE_WITH_KNOTS ( 'NONE', 3,
 ( #21190, #63829, #6136, #38301 ),
 .UNSPECIFIED., .F., .F.,
 ( 4, 4 ),
 ( 0.7819104999562735969, 1.000000000000000000 ),
 .UNSPECIFIED. ) ;
#21347 = EDGE_CURVE ( 'NONE', #11095, #54418, #48267, .T. ) ;
#21348 = CARTESIAN_POINT ( 'NONE',  ( 12.34378620361241374, -0.4226185364342202599, -12.69055435920471098 ) ) ;
#21349 = CARTESIAN_POINT ( 'NONE',  ( 9.916846873516377059, -4.768183399968644487, -8.499583552997725278 ) ) ;
#21350 = ORIENTED_EDGE ( 'NONE', *, *, #8880, .T. ) ;
#21351 = CARTESIAN_POINT ( 'NONE',  ( 12.63888201721073834, -1.779588368642105012, 12.47369581775632952 ) ) ;
#21352 = CARTESIAN_POINT ( 'NONE',  ( 10.03696314287999947, -2.882742046518000034, -7.264481182560499128 ) ) ;
#21353 = CARTESIAN_POINT ( 'NONE',  ( 11.43336398472434645, 11.63122337162911002, 1.412340616368904067 ) ) ;
#21354 = LINE ( 'NONE', #42682, #22015 ) ;
#21355 = CARTESIAN_POINT ( 'NONE',  ( 11.76487482311540056, -3.069598554678400149, 7.124095752359899336 ) ) ;
#21356 = CARTESIAN_POINT ( 'NONE',  ( 10.30487885159599770, 4.996404279947399552, -7.381132626649399064 ) ) ;
#21357 = CARTESIAN_POINT ( 'NONE',  ( 8.719734573340000239, 3.777330902948500047, 6.647493632115700102 ) ) ;
#21358 = CARTESIAN_POINT ( 'NONE',  ( 0.03044738438019000196, -2.003871238023999801, -2.529037764236000019 ) ) ;
#21359 = CARTESIAN_POINT ( 'NONE',  ( 4.412215258034844823, -0.5741934336287252139, -0.9653862342499147653 ) ) ;
#21360 = CARTESIAN_POINT ( 'NONE',  ( 12.18627227647243139, 2.104539383777987549, 12.42301525548629826 ) ) ;
#21362 = CARTESIAN_POINT ( 'NONE',  ( 8.111573341229000533, 3.326263523254000098, 8.794511546544999447 ) ) ;
#21361 = CARTESIAN_POINT ( 'NONE',  ( 10.21426717315699939, 3.130949526459800403, -6.759401780699699103 ) ) ;
#21363 = CARTESIAN_POINT ( 'NONE',  ( 11.62994988689359843, 4.518136976474400157, -8.516279404258998653 ) ) ;
#21364 = CARTESIAN_POINT ( 'NONE',  ( 8.347004975328005116, 2.870635057193001050, -6.340345019934002124 ) ) ;
#21365 = CARTESIAN_POINT ( 'NONE',  ( 11.00119221959000093, 4.640446572790000168, -9.059321223816999336 ) ) ;
#21366 = CARTESIAN_POINT ( 'NONE',  ( 9.757279731608999640, 4.114789684104199985, -6.225948307210999566 ) ) ;
#21368 = DIRECTION ( 'NONE',  ( 0.000000000000000000, 1.000000000000000000, 0.000000000000000000 ) ) ;
#21367 = CARTESIAN_POINT ( 'NONE',  ( 17.60000001947600268, -11.86186880240999919, 3.298627760718999991 ) ) ;
#21369 = CARTESIAN_POINT ( 'NONE',  ( 8.968535790263077345, 5.344945407621378486, 7.382749812548996537 ) ) ;
#21370 = ORIENTED_EDGE ( 'NONE', *, *, #51776, .T. ) ;
#21371 = CYLINDRICAL_SURFACE ( 'NONE', #15975, 1.350000000000000089 ) ;
#21372 = CARTESIAN_POINT ( 'NONE',  ( 24.32158572772383920, -9.044138607853493994, 9.474428397134387225 ) ) ;
#21373 = CARTESIAN_POINT ( 'NONE',  ( 17.74278939939642186, 0.6963438834399311439, -12.58074676375273881 ) ) ;
#21374 = CARTESIAN_POINT ( 'NONE',  ( 9.880963142879998884, 4.848366390061300102, 7.678836273503299559 ) ) ;
#21375 = VECTOR ( 'NONE', #43885, 1000.000000000000000 ) ;
#21376 = CARTESIAN_POINT ( 'NONE',  ( 12.44779487374913529, -3.012931620461074989, 13.55119122998581283 ) ) ;
#21377 = CARTESIAN_POINT ( 'NONE',  ( 12.18521525456554500, 2.580824917997073253, 13.65593716524227830 ) ) ;
#21378 = CARTESIAN_POINT ( 'NONE',  ( 9.002376473208929752, -4.922128563344212893, -8.207577963560542145 ) ) ;
#21379 = EDGE_LOOP ( 'NONE', ( #47091, #33451, #30768, #2374 ) ) ;
#21380 = EDGE_CURVE ( 'NONE', #20862, #16031, #42449, .T. ) ;
#21381 = EDGE_CURVE ( 'NONE', #25126, #37419, #4050, .T. ) ;
#21382 = CARTESIAN_POINT ( 'NONE',  ( 5.231322606809000852, -0.4388467025999000515, 1.020924588955999912 ) ) ;
#21383 = CARTESIAN_POINT ( 'NONE',  ( 9.529317406968999649, -3.762080884004200154, -8.756892549790999070 ) ) ;
#21384 = CARTESIAN_POINT ( 'NONE',  ( 9.637847264149046467, -4.829496491575645756, -8.579553154517226332 ) ) ;
#21385 = CARTESIAN_POINT ( 'NONE',  ( 10.94532229106000010, 5.075441716071999565, -4.924547694085999794 ) ) ;
#21386 = CARTESIAN_POINT ( 'NONE',  ( 18.17899100331058548, 2.462234907104897008, -12.46031481527572637 ) ) ;
#21387 = CARTESIAN_POINT ( 'NONE',  ( 9.643927823787143083, -2.750011555256801188, 7.500000155056757656 ) ) ;
#21388 = DIRECTION ( 'NONE',  ( -1.000000000000000000, 0.000000000000000000, 0.000000000000000000 ) ) ;
#21389 = CARTESIAN_POINT ( 'NONE',  ( 15.40000000005200143, 9.187454762873001002, 8.213177997099000649 ) ) ;
#21390 = CARTESIAN_POINT ( 'NONE',  ( 10.41839555962000041, -4.531908721143000029, -9.270473926467998282 ) ) ;
#21391 = CARTESIAN_POINT ( 'NONE',  ( 4.782109839683042374, 0.9218200799623742503, -1.199500263597268912 ) ) ;
#21392 = CARTESIAN_POINT ( 'NONE',  ( 11.50001544675000176, -10.90724927943889710, 6.294778943836956131 ) ) ;
#21393 = CARTESIAN_POINT ( 'NONE',  ( 23.81723165750307913, 9.687177923879790598, -9.414241483045064030 ) ) ;
#21394 = DIRECTION ( 'NONE',  ( 1.000000000000000000, 0.000000000000000000, 0.000000000000000000 ) ) ;
#21395 = ADVANCED_FACE ( 'NONE', ( #60056 ), #11806, .F. ) ;
#21396 = VERTEX_POINT ( 'NONE', #59705 ) ;
#21397 = CARTESIAN_POINT ( 'NONE',  ( 9.881820280408998514, 4.325866256860000369, -9.125812605905000652 ) ) ;
#21398 = CARTESIAN_POINT ( 'NONE',  ( 11.81825954179440075, -3.333768806796900019, 6.946434658287599540 ) ) ;
#21399 = EDGE_LOOP ( 'NONE', ( #49888, #21203, #5755, #41860 ) ) ;
#21400 = CYLINDRICAL_SURFACE ( 'NONE', #58561, 0.6250000000000005551 ) ;
#21401 = CARTESIAN_POINT ( 'NONE',  ( 10.81764560330029923, -3.650429500487800460, -6.414140625063999401 ) ) ;
#21402 = ORIENTED_EDGE ( 'NONE', *, *, #14492, .T. ) ;
#21403 = ADVANCED_FACE ( 'NONE', ( #21948 ), #43288, .F. ) ;
#21404 = CARTESIAN_POINT ( 'NONE',  ( 25.29986325275000070, 2.258942858049999725, 12.29419282279000036 ) ) ;
#21405 = CARTESIAN_POINT ( 'NONE',  ( 24.07541911252200251, 3.340244713972364998, -12.60849197320232129 ) ) ;
#21406 = DIRECTION ( 'NONE',  ( 0.000000000000000000, 0.000000000000000000, -1.000000000000000000 ) ) ;
#21407 = CARTESIAN_POINT ( 'NONE',  ( 11.59999999999999964, -5.499854772664000357, -7.825000000000000178 ) ) ;
#21408 = CARTESIAN_POINT ( 'NONE',  ( 12.49507620391304030, 0.5430989695823158492, -13.88572189919474731 ) ) ;
#21409 = CARTESIAN_POINT ( 'NONE',  ( 7.289711015751999312, -0.9708250560305000665, 0.5387387265405000347 ) ) ;
#21410 = CARTESIAN_POINT ( 'NONE',  ( 13.08018231457700153, 11.57028798436999928, 1.758177683552999859 ) ) ;
#21411 = ORIENTED_EDGE ( 'NONE', *, *, #62179, .F. ) ;
#21412 = CARTESIAN_POINT ( 'NONE',  ( 10.21398584123000042, 3.990126737362999609, -8.809457313313998839 ) ) ;
#21413 = VERTEX_POINT ( 'NONE', #49214 ) ;
#21414 = CARTESIAN_POINT ( 'NONE',  ( 10.90000000000000036, -5.100000000000000533, -6.436740704805999691 ) ) ;
#21415 = B_SPLINE_CURVE_WITH_KNOTS ( 'NONE', 3,
 ( #68089, #30367, #42236, #10402, #57605, #9711 ),
 .UNSPECIFIED., .F., .F.,
 ( 4, 2, 4 ),
 ( 0.000000000000000000, 0.5000000000000000000, 1.000000000000000000 ),
 .UNSPECIFIED. ) ;
#21416 = VERTEX_POINT ( 'NONE', #59021 ) ;
#21417 = CARTESIAN_POINT ( 'NONE',  ( 9.681292290062998518, 5.106256438265999620, 8.142324746736500529 ) ) ;
#21418 = CARTESIAN_POINT ( 'NONE',  ( 18.15856293744596783, 11.79508858035351970, -3.559060952131059885 ) ) ;
#21419 = CARTESIAN_POINT ( 'NONE',  ( 4.500000125099000492, 1.829647544581999737E-13, 0.000000000000000000 ) ) ;
#21420 = CARTESIAN_POINT ( 'NONE',  ( 12.25867852505488820, -0.3036576181174179268, 13.89554011873103612 ) ) ;
#21421 = ORIENTED_EDGE ( 'NONE', *, *, #4267, .F. ) ;
#21422 = CARTESIAN_POINT ( 'NONE',  ( 12.13190478341600098, 11.96733320521999921, -3.503025077341000326 ) ) ;
#21423 = CARTESIAN_POINT ( 'NONE',  ( 18.12406690321100200, 11.75515418280000013, -3.561236062516000000 ) ) ;
#21424 = CARTESIAN_POINT ( 'NONE',  ( 9.201570984676626708, 3.555997837402618877, 6.746080675052237297 ) ) ;
#21425 = CARTESIAN_POINT ( 'NONE',  ( 8.876902336861419940, 4.269588175475917957, 8.499844062317453819 ) ) ;
#21426 = CONICAL_SURFACE ( 'NONE', #28134, 0.9999998338055000602, 0.7853981908209605178 ) ;
#21427 = CARTESIAN_POINT ( 'NONE',  ( 9.784179719593000257, 4.042991257420999851, -5.768106221333000327 ) ) ;
#21428 = CARTESIAN_POINT ( 'NONE',  ( 10.56498513754044311, 5.349957030113837497, -7.500000808964303545 ) ) ;
#21429 = AXIS2_PLACEMENT_3D ( 'NONE', #26783, #38287, #4742 ) ;
#21430 = CARTESIAN_POINT ( 'NONE',  ( 11.01003172897000049, -3.180716007396000133, -6.283809484240999943 ) ) ;
#21431 = EDGE_CURVE ( 'NONE', #11630, #51331, #288, .T. ) ;
#21432 = EDGE_CURVE ( 'NONE', #21901, #38721, #27550, .T. ) ;
#21433 = VERTEX_POINT ( 'NONE', #65633 ) ;
#21434 = VERTEX_POINT ( 'NONE', #54113 ) ;
#21435 = CARTESIAN_POINT ( 'NONE',  ( 8.622785841227999626, 5.189036231907000030, -8.048606212067999977 ) ) ;
#21436 = FACE_OUTER_BOUND ( 'NONE', #22353, .T. ) ;
#21437 = CARTESIAN_POINT ( 'NONE',  ( 8.712385177405817416, -3.301664264255438574, -6.339997339881533911 ) ) ;
#21438 = CARTESIAN_POINT ( 'NONE',  ( 13.64750315638899991, 9.067203425066999500, 7.400836607049000371 ) ) ;
#21439 = DIRECTION ( 'NONE',  ( 1.258720292987999992E-10, 1.258720804380000048E-10, 1.000000000000000000 ) ) ;
#21440 = B_SPLINE_CURVE_WITH_KNOTS ( 'NONE', 3,
 ( #44018, #27243, #33871, #38766 ),
 .UNSPECIFIED., .F., .F.,
 ( 4, 4 ),
 ( 0.000000000000000000, 1.000000000000000000 ),
 .UNSPECIFIED. ) ;
#21441 = CARTESIAN_POINT ( 'NONE',  ( 11.26212378248529866, 3.384904051819500381, -6.336291382830999908 ) ) ;
#21442 = CARTESIAN_POINT ( 'NONE',  ( 8.733265421555000074, 3.837285628664199866, -8.341695632489900092 ) ) ;
#21444 = CARTESIAN_POINT ( 'NONE',  ( 1.996201642328499837, 2.726743374470193437, -2.246552915429937070 ) ) ;
#21443 = CARTESIAN_POINT ( 'NONE',  ( 10.43363399569799910, -3.001718438313799808, 7.389201877599999690 ) ) ;
#21445 = CARTESIAN_POINT ( 'NONE',  ( 7.100000000000000533, -4.000000000000000000, 8.849999999999999645 ) ) ;
#21446 = VERTEX_POINT ( 'NONE', #32456 ) ;
#21447 = CARTESIAN_POINT ( 'NONE',  ( 10.50595525820100029, -4.081787880721680750, -6.637672143048099827 ) ) ;
#21448 = CARTESIAN_POINT ( 'NONE',  ( 10.33483735105000179, -3.422629205013000053, -4.713488022966999758 ) ) ;
#21449 = CARTESIAN_POINT ( 'NONE',  ( 10.06430484851600049, 5.163382381259999931, 6.968092280137199168 ) ) ;
#21450 = CARTESIAN_POINT ( 'NONE',  ( 7.000000000000000000, -9.186881182980000560, -5.186879035586000164 ) ) ;
#21451 = CARTESIAN_POINT ( 'NONE',  ( 9.318721994369999706, -2.755032632138999737, 8.795122807847999269 ) ) ;
#21452 = CARTESIAN_POINT ( 'NONE',  ( 9.817462135711998883, -5.100000000000000533, 6.571291218949999902 ) ) ;
#21453 = CARTESIAN_POINT ( 'NONE',  ( 16.44832727683000329, -3.192413998985999868, -11.44999110620999794 ) ) ;
#21454 = ADVANCED_FACE ( 'NONE', ( #54462 ), #39078, .T. ) ;
#21455 = EDGE_CURVE ( 'NONE', #48720, #50331, #32464, .T. ) ;
#21456 = CARTESIAN_POINT ( 'NONE',  ( 7.932045741440900244, 5.134137158643878429, 6.756605230894701997 ) ) ;
#21457 = LINE ( 'NONE', #31970, #10993 ) ;
#21458 = CARTESIAN_POINT ( 'NONE',  ( 9.484696787962999309, -3.851113559088000127, -6.645868410478299459 ) ) ;
#21459 = AXIS2_PLACEMENT_3D ( 'NONE', #68358, #67077, #42495 ) ;
#21460 = ADVANCED_FACE ( 'NONE', ( #11458 ), #44626, .F. ) ;
#21461 = CARTESIAN_POINT ( 'NONE',  ( 6.434332659906999652, 0.8081923938199999657, -1.046566182397999922 ) ) ;
#21462 = CARTESIAN_POINT ( 'NONE',  ( 11.41991225946277666, -3.299232917623651229, 8.022508467459166681 ) ) ;
#21463 = CARTESIAN_POINT ( 'NONE',  ( 8.798455008774128672, 4.948455060776569603, -7.736326407956449103 ) ) ;
#21464 = ORIENTED_EDGE ( 'NONE', *, *, #12478, .T. ) ;
#21465 = CARTESIAN_POINT ( 'NONE',  ( 12.40045920100465260, 0.4764818960106717571, -12.68796903437993606 ) ) ;
#21466 = CARTESIAN_POINT ( 'NONE',  ( 11.21979841651039855, 3.695024856201900132, -8.310733465454200442 ) ) ;
#21467 = DIRECTION ( 'NONE',  ( 1.000000000000000000, 0.000000000000000000, 0.000000000000000000 ) ) ;
#21468 = CARTESIAN_POINT ( 'NONE',  ( 7.100000000000000533, 0.000000000000000000, 0.000000000000000000 ) ) ;
#21469 = CARTESIAN_POINT ( 'NONE',  ( 10.18795867446423387, 4.829522773136188718, -8.579479308274169824 ) ) ;
#21470 = ORIENTED_EDGE ( 'NONE', *, *, #15618, .T. ) ;
#21471 = CARTESIAN_POINT ( 'NONE',  ( 25.27036124584200039, -11.11619549273000018, -3.474353012118999828 ) ) ;
#21472 = ITEM_DEFINED_TRANSFORMATION ( 'NONE', 'NONE', #29583,  #9676 ) ;
#21473 = CARTESIAN_POINT ( 'NONE',  ( 11.44366954483529852, -3.514796851401900124, -6.751356298874699569 ) ) ;
#21474 = CARTESIAN_POINT ( 'NONE',  ( 24.53428985367600390, -3.614319203926000146, 12.31267510079000083 ) ) ;
#21475 = CARTESIAN_POINT ( 'NONE',  ( 9.214598350284001427, -2.899999999999999911, -6.571291218949999902 ) ) ;
#21476 = FACE_OUTER_BOUND ( 'NONE', #40164, .T. ) ;
#21477 = CARTESIAN_POINT ( 'NONE',  ( 10.86190547754509872, 4.891676932241900033, -7.528299448264639260 ) ) ;
#21478 = ORIENTED_EDGE ( 'NONE', *, *, #36053, .F. ) ;
#21479 = CARTESIAN_POINT ( 'NONE',  ( 10.16829915263999951, -4.567213659083999566, 5.832528837986999726 ) ) ;
#21480 = CARTESIAN_POINT ( 'NONE',  ( 17.86985707050055794, 3.040024008573237069, -13.54397559521889249 ) ) ;
#21481 = ORIENTED_EDGE ( 'NONE', *, *, #9945, .T. ) ;
#21482 = EDGE_CURVE ( 'NONE', #66219, #8436, #9879, .T. ) ;
#21483 = DIRECTION ( 'NONE',  ( 0.7071067537449087226, -0.5063799918121058008, -0.4935375798262057745 ) ) ;
#21484 = CARTESIAN_POINT ( 'NONE',  ( 9.385311019873999072, -4.135077143711000325, 9.175520401071999288 ) ) ;
#21485 = AXIS2_PLACEMENT_3D ( 'NONE', #14576, #47420, #63132 ) ;
#21486 = CARTESIAN_POINT ( 'NONE',  ( 9.568039158772000619, 5.336630274082000192, -7.092011739486999922 ) ) ;
#21487 = ORIENTED_EDGE ( 'NONE', *, *, #36440, .T. ) ;
#21488 = CARTESIAN_POINT ( 'NONE',  ( 14.93333333119166717, -9.187454790032713703, -8.213178404203524963 ) ) ;
#21489 = CARTESIAN_POINT ( 'NONE',  ( 8.260085841226999293, 4.511685119297999869, -5.670317910541000650 ) ) ;
#21490 = DIRECTION ( 'NONE',  ( 0.000000000000000000, 1.000000000000000000, 0.000000000000000000 ) ) ;
#21491 = CARTESIAN_POINT ( 'NONE',  ( 7.281729984065945516, 3.320395505273955994, -8.679445286782913271 ) ) ;
#21492 = VERTEX_POINT ( 'NONE', #36146 ) ;
#21493 = CARTESIAN_POINT ( 'NONE',  ( 10.15903154954000165, -4.166415630773999901, 9.114167874391000623 ) ) ;
#21494 = CARTESIAN_POINT ( 'NONE',  ( 11.59999999999999787, 3.205140046301731438, 7.924485708373446791 ) ) ;
#21495 = DIRECTION ( 'NONE',  ( 0.9999999999993943733, -9.646910167131952540E-07, 5.296687751076970703E-07 ) ) ;
#21496 = EDGE_LOOP ( 'NONE', ( #38311, #36613, #15861, #34498 ) ) ;
#21497 = CARTESIAN_POINT ( 'NONE',  ( 8.978248830702483474, 4.955089878105851220, -8.117373328463406423 ) ) ;
#21498 = CARTESIAN_POINT ( 'NONE',  ( 10.46297944037999983, -3.993164663709000362, -6.140164943008000087 ) ) ;
#21499 = B_SPLINE_CURVE_WITH_KNOTS ( 'NONE', 3,
 ( #19917, #52061, #48549, #42957, #26886, #53104, #64612, #64950, #6580, #58688, #53450, #653, #47868, #37367, #20949, #22313, #15702, #1001 ),
 .UNSPECIFIED., .F., .F.,
 ( 4, 1, 2, 2, 1, 2, 2, 2, 2, 4 ),
 ( 0.000000000000000000, 0.1250000000000013323, 0.1874999999999983902, 0.2499999999999954481, 0.3749999999999931721, 0.4374999999999959477, 0.4999999999999987232, 0.6249999999999994449, 0.7500000000000002220, 1.000000000000000000 ),
 .UNSPECIFIED. ) ;
#21500 = ORIENTED_EDGE ( 'NONE', *, *, #13886, .T. ) ;
#21501 = CARTESIAN_POINT ( 'NONE',  ( 1.985247277619000217, 2.372532593102000043, -2.573147701680999599 ) ) ;
#21502 = CARTESIAN_POINT ( 'NONE',  ( 17.88934697238260796, -1.841816770035711981, -12.46465977041039963 ) ) ;
#21503 = CARTESIAN_POINT ( 'NONE',  ( 5.092749183302999860, -0.2523854654960999699, -1.393817212909000069 ) ) ;
#21504 = CARTESIAN_POINT ( 'NONE',  ( 11.59999999999999964, 3.850275034462830259, -6.485689145701417857 ) ) ;
#21505 = CARTESIAN_POINT ( 'NONE',  ( 15.95458079702100029, 3.771493919207000278, 11.78965436225000118 ) ) ;
#21506 = CARTESIAN_POINT ( 'NONE',  ( 10.45187178376759185, 5.320780938513880898, 7.955756249381567002 ) ) ;
#21507 = CARTESIAN_POINT ( 'NONE',  ( 24.30000000000000071, 0.000000000000000000, 0.000000000000000000 ) ) ;
#21508 = B_SPLINE_SURFACE_WITH_KNOTS ( 'NONE', 3, 3, ( 
 ( #43482, #53953, #32985, #42784, #5714, #48370, #6058, #38927, #16207, #22484, #27751, #58858, #1170, #825, #65126, #1864, #12351, #43826, #37882, #49063, #27395, #59202, #44179, #33684, #48724, #38568, #43127, #53617, #55001, #28088, #64780, #59894, #33339, #60249, #12001 ),
 ( #22142, #37531, #27055, #478, #59550, #1514, #21794, #54654, #49402, #32643, #18637, #24566, #28794, #39967, #23527, #39613, #40635, #67200, #61284, #56034, #13400, #8486, #19310, #34723, #40301, #8142, #29491, #2890, #60938, #13054, #45889, #50105, #2546, #2213, #44869 ),
 ( #34381, #66173, #3239, #14081, #7795, #50797, #18293, #12697, #35406, #56384, #23873, #18976, #13735, #61970, #24214, #61620, #35068, #29832, #45557, #66863, #50444, #51137, #56732, #34035, #8826, #45212, #55699, #30169, #51474, #29136, #23181, #44530, #55347, #65824, #66514 ),
 ( #17950, #39268, #60591, #7444, #30843, #41671, #31532, #4601, #9502, #20007, #25937, #36082, #42370, #25596, #46922, #36775, #41332, #46582, #62639, #47265, #10538, #15451, #31198, #68923, #21037, #9852, #46235, #67542, #52503, #63671, #68570, #58097, #42022, #31879, #37119 ) ),
 .UNSPECIFIED., .F., .F., .F.,
 ( 4, 4 ),
 ( 4, 1, 1, 1, 1, 1, 1, 1, 1, 1, 1, 1, 1, 1, 1, 1, 1, 1, 1, 1, 1, 1, 1, 1, 1, 1, 1, 1, 1, 1, 1, 1, 4 ),
 ( -0.1039086239011999951, 1.103908623900999864 ),
 ( -0.01933701211302999920, 0.01208563257065999909, 0.04350827725433999843, 0.07493092193802000645, 0.1063535666217000075, 0.1377762113054000204, 0.1691988559891000055, 0.2006215006727000150, 0.2320441453564000001, 0.2634667900400999851, 0.2948894347238000258, 0.3263120794074999553, 0.3577347240911999959, 0.3891573687748000054, 0.4205800134584999905, 0.4520026581421999756, 0.4834253028259000162, 0.5148479475096000568, 0.5462705921932000663, 0.5776932368768999959, 0.6091158815606000365, 0.6405385262443000771, 0.6719611709280000067, 0.7033838156117000473, 0.7348064602953000568, 0.7662291049789999864, 0.7976517496627000270, 0.8290743943464000676, 0.8604970390300999972, 0.8919196837138000378, 0.9233423283974000473, 0.9547649730810999769, 0.9861876177648000175 ),
 .UNSPECIFIED. ) ;
#21509 = ORIENTED_EDGE ( 'NONE', *, *, #26268, .F. ) ;
#21510 = CARTESIAN_POINT ( 'NONE',  ( 13.69996357384221497, -12.28513767539741863, -2.441259368852444211 ) ) ;
#21511 = VERTEX_POINT ( 'NONE', #35806 ) ;
#21512 = CARTESIAN_POINT ( 'NONE',  ( 9.854942824136999846, 2.800308224477999985, 9.013816726157999781 ) ) ;
#21513 = DIRECTION ( 'NONE',  ( 0.000000000000000000, 0.000000000000000000, -1.000000000000000000 ) ) ;
#21514 = B_SPLINE_CURVE_WITH_KNOTS ( 'NONE', 3,
 ( #35050, #29815, #25229, #8125 ),
 .UNSPECIFIED., .F., .F.,
 ( 4, 4 ),
 ( 0.000000000000000000, 1.000000000000000000 ),
 .UNSPECIFIED. ) ;
#21515 = DIRECTION ( 'NONE',  ( -1.000000000000000000, 0.000000000000000000, 0.000000000000000000 ) ) ;
#21516 = CARTESIAN_POINT ( 'NONE',  ( 8.622785841227999626, 5.189036231907000030, -8.048606212067999977 ) ) ;
#21517 = AXIS2_PLACEMENT_3D ( 'NONE', #21201, #21541, #11061 ) ;
#21518 = DIRECTION ( 'NONE',  ( -1.000000000000000000, 0.000000000000000000, 0.000000000000000000 ) ) ;
#21519 = CARTESIAN_POINT ( 'NONE',  ( 23.59999443371599881, 2.915558930973999985, 13.58549620949000136 ) ) ;
#21520 = CARTESIAN_POINT ( 'NONE',  ( 18.17005425344203928, -0.1118032413084528998, 13.89939982891986148 ) ) ;
#21521 = CARTESIAN_POINT ( 'NONE',  ( 9.475931479132977842, -3.758245030697716427, -9.262048976456073390 ) ) ;
#21522 = EDGE_CURVE ( 'NONE', #15201, #53670, #57458, .T. ) ;
#21523 = EDGE_CURVE ( 'NONE', #40516, #6243, #25767, .T. ) ;
#21524 = EDGE_LOOP ( 'NONE', ( #36129, #690, #45499, #40551 ) ) ;
#21525 = CARTESIAN_POINT ( 'NONE',  ( 12.44983642703673965, 0.5143249053291590878, 13.88719129590927892 ) ) ;
#21526 = CARTESIAN_POINT ( 'NONE',  ( 11.11656919669529842, -2.774362666861999838, 7.137881914002699446 ) ) ;
#21527 = CARTESIAN_POINT ( 'NONE',  ( 17.92176811225533228, -0.5062908248731810001, -13.88759084003172717 ) ) ;
#21528 = CARTESIAN_POINT ( 'NONE',  ( 7.860168146793000687, -2.263562268490999951, 8.007440964304000985 ) ) ;
#21530 = DIRECTION ( 'NONE',  ( -0.000000000000000000, -0.9999988959613604900, -0.001485959642859940649 ) ) ;
#21529 = CARTESIAN_POINT ( 'NONE',  ( 9.323722176100000425, 3.947350570199999797, 6.051869652381999920 ) ) ;
#21531 = CIRCLE ( 'NONE', #4807, 1.799999999999999600 ) ;
#21532 = CARTESIAN_POINT ( 'NONE',  ( 10.44841638348500013, 2.891666689023999925, -7.230023356477299323 ) ) ;
#21533 = CARTESIAN_POINT ( 'NONE',  ( 24.26682857475500299, -8.952388712744999921, -8.898287395196000205 ) ) ;
#21534 = CARTESIAN_POINT ( 'NONE',  ( 8.895138961223999274, 4.832207374954999857, -8.062381800110799190 ) ) ;
#21535 = CARTESIAN_POINT ( 'NONE',  ( 18.05074276561661861, -0.3808128809978877372, 12.69231869260112155 ) ) ;
#21536 = CARTESIAN_POINT ( 'NONE',  ( 6.616621076168000215, -0.9842248689287999008, 0.9580517823941999689 ) ) ;
#21537 = LINE ( 'NONE', #42528, #14301 ) ;
#21538 = ORIENTED_EDGE ( 'NONE', *, *, #56121, .T. ) ;
#21539 = CARTESIAN_POINT ( 'NONE',  ( 9.085769353209000698, -2.821866379289000193, 6.127148604720000336 ) ) ;
#21540 = CARTESIAN_POINT ( 'NONE',  ( 9.091120559621998609, -3.762710033898000184, 8.787827024292999667 ) ) ;
#21541 = DIRECTION ( 'NONE',  ( 1.000000000000000000, 0.000000000000000000, 0.000000000000000000 ) ) ;
#21542 = LINE ( 'NONE', #42199, #31171 ) ;
#21543 = ORIENTED_EDGE ( 'NONE', *, *, #42633, .T. ) ;
#21544 = ADVANCED_FACE ( 'NONE', ( #45951 ), #39422, .T. ) ;
#21545 = LINE ( 'NONE', #22580, #53463 ) ;
#21546 = CARTESIAN_POINT ( 'NONE',  ( 10.69057802013490033, 2.966773425016000054, 7.524052967375959966 ) ) ;
#21547 = CARTESIAN_POINT ( 'NONE',  ( 2.361656243241000208, -1.849229342384999919, -3.272419312099999811 ) ) ;
#21548 = ORIENTED_EDGE ( 'NONE', *, *, #14665, .T. ) ;
#21549 = CARTESIAN_POINT ( 'NONE',  ( 7.000002934099999408, 1.243449787579999883E-13, -1.714942011622999690E-13 ) ) ;
#21550 = CARTESIAN_POINT ( 'NONE',  ( 9.512931135678952543, -5.100000000000000533, 6.444141223441286925 ) ) ;
#21551 = CARTESIAN_POINT ( 'NONE',  ( 10.07503300763299947, 4.881889043637199777, 6.575021251017499679 ) ) ;
#21552 = CARTESIAN_POINT ( 'NONE',  ( 23.56664311700400205, 13.31365802054999925, 4.296923094388999331 ) ) ;
#21553 = CARTESIAN_POINT ( 'NONE',  ( 8.014948341228999240, 2.280568568659000483, 6.510284508622999233 ) ) ;
#21554 = VERTEX_POINT ( 'NONE', #49908 ) ;
#21555 = CARTESIAN_POINT ( 'NONE',  ( 6.860989938375000818, -0.07351275584480999881, 1.466703212027999914 ) ) ;
#21556 = CARTESIAN_POINT ( 'NONE',  ( 7.897245280407999779, 4.473304741848999733, -6.008315738301999609 ) ) ;
#21557 = CARTESIAN_POINT ( 'NONE',  ( 8.545743765261121894, -3.391202971854105019, 5.870433013438566050 ) ) ;
#21558 = CARTESIAN_POINT ( 'NONE',  ( 10.90000000000000036, -8.091325576830000088, 7.077637346582999811 ) ) ;
#21559 = ORIENTED_EDGE ( 'NONE', *, *, #43586, .T. ) ;
#21560 = CARTESIAN_POINT ( 'NONE',  ( 11.66889198508049930, 11.69116221025808322, 1.923144176179721887 ) ) ;
#21561 = CARTESIAN_POINT ( 'NONE',  ( 11.53713099069000059, 11.52702260260000067, 1.399766873409999945 ) ) ;
#21562 = ORIENTED_EDGE ( 'NONE', *, *, #53436, .T. ) ;
#21563 = EDGE_CURVE ( 'NONE', #34400, #14642, #34908, .T. ) ;
#21564 = CYLINDRICAL_SURFACE ( 'NONE', #36215, 0.6250000000000005551 ) ;
#21565 = CARTESIAN_POINT ( 'NONE',  ( 24.71801055494115928, -8.650035796533028787, -8.600711262961937109 ) ) ;
#21566 = CARTESIAN_POINT ( 'NONE',  ( 7.875861560654877636, -4.439160970441643705, 6.199066551597841368 ) ) ;
#21567 = EDGE_LOOP ( 'NONE', ( #52365, #18290, #22890, #35381 ) ) ;
#21568 = CARTESIAN_POINT ( 'NONE',  ( 10.66052890781999984, -2.899999999999999911, -6.152188490330000370 ) ) ;
#21569 = CARTESIAN_POINT ( 'NONE',  ( 8.975133088423635996, -5.349981448246158955, 7.499992563499107590 ) ) ;
#21570 = CARTESIAN_POINT ( 'NONE',  ( 10.32169598648999909, 4.766524664146899681, -7.956401575444799867 ) ) ;
#21571 = CARTESIAN_POINT ( 'NONE',  ( 12.70142344966302694, 3.116692473072851577, -12.28627407840914820 ) ) ;
#21572 = CARTESIAN_POINT ( 'NONE',  ( 10.59964828895399869, -2.878385131502000149, 6.887384543790600056 ) ) ;
#21573 = ORIENTED_EDGE ( 'NONE', *, *, #64240, .F. ) ;
#21574 = CARTESIAN_POINT ( 'NONE',  ( 9.208107780409999776, 5.057081813675999626, 8.967637988488998957 ) ) ;
#21575 = EDGE_LOOP ( 'NONE', ( #8026, #25812, #6716, #11039, #2524 ) ) ;
#21576 = CARTESIAN_POINT ( 'NONE',  ( 11.25740844561608611, 5.045781347359230118, 7.824999626888802240 ) ) ;
#21577 = CONICAL_SURFACE ( 'NONE', #39459, 1.700000581162000035, 0.7853984839373144844 ) ;
#21578 = CARTESIAN_POINT ( 'NONE',  ( 15.91587707751000025, -9.040653309694000939, -8.458480061295000851 ) ) ;
#21579 = CARTESIAN_POINT ( 'NONE',  ( 8.674830025576039105, -2.649890579813208191, 7.499988935010342139 ) ) ;
#21580 = EDGE_LOOP ( 'NONE', ( #65934, #19037, #13932, #54481 ) ) ;
#21581 = CARTESIAN_POINT ( 'NONE',  ( 12.52557666887736509, -1.940868768839141500, -12.56439497327413335 ) ) ;
#21582 = VECTOR ( 'NONE', #9727, 1000.000000000000000 ) ;
#21583 = CARTESIAN_POINT ( 'NONE',  ( 11.09999999999999964, 2.899999999999999911, -4.467422426380999845 ) ) ;
#21584 = CARTESIAN_POINT ( 'NONE',  ( 24.67921569845699992, 12.29514839105000057, -2.979196030862000022 ) ) ;
#21585 = CARTESIAN_POINT ( 'NONE',  ( 21.72233714749290101, 5.999764115230404649, -0.05320302240984255138 ) ) ;
#21586 = CARTESIAN_POINT ( 'NONE',  ( 12.51429325950075722, -1.848987300417688440, -13.87736530974562754 ) ) ;
#21587 = CARTESIAN_POINT ( 'NONE',  ( 10.84641504065830020, -3.195537720350400068, -6.900173947321999179 ) ) ;
#21588 = DIRECTION ( 'NONE',  ( -0.000000000000000000, 0.3222656952305000266, 0.9466492601157001641 ) ) ;
#21589 = CARTESIAN_POINT ( 'NONE',  ( 17.96998260175204010, -3.070456082915653528, 12.22016143605431004 ) ) ;
#21590 = ORIENTED_EDGE ( 'NONE', *, *, #45620, .F. ) ;
#21591 = DIRECTION ( 'NONE',  ( 1.000000000000000000, 0.000000000000000000, 0.000000000000000000 ) ) ;
#21592 = ORIENTED_EDGE ( 'NONE', *, *, #67909, .F. ) ;
#21593 = CARTESIAN_POINT ( 'NONE',  ( 11.35642168284000242, -12.27417251877000126, -1.600391102631000040 ) ) ;
#21594 = CARTESIAN_POINT ( 'NONE',  ( 7.066756274120943537, 0.2616187012132834555, -3.032564036156816023 ) ) ;
#21595 = CARTESIAN_POINT ( 'NONE',  ( 10.09133754351999990, 2.216715295763999727, -8.007133643737999407 ) ) ;
#21596 = FACE_OUTER_BOUND ( 'NONE', #3498, .T. ) ;
#21597 = CARTESIAN_POINT ( 'NONE',  ( 5.500000000000000000, 0.5415384615384001288, -2.132307692307999769 ) ) ;
#21598 = CARTESIAN_POINT ( 'NONE',  ( 8.500392882431995645, 2.902640497153002652, -6.605631719337000440 ) ) ;
#21599 = ADVANCED_FACE ( 'NONE', ( #9220 ), #19726, .T. ) ;
#21601 = EDGE_CURVE ( 'NONE', #43538, #25292, #19044, .T. ) ;
#21600 = CARTESIAN_POINT ( 'NONE',  ( 9.758140238852000437, 2.901378080241999946, 6.555076849497999625 ) ) ;
#21602 = B_SPLINE_CURVE_WITH_KNOTS ( 'NONE', 3,
 ( #22570, #27839, #32728, #18037 ),
 .UNSPECIFIED., .F., .F.,
 ( 4, 4 ),
 ( 0.000000000000000000, 1.000000000000000000 ),
 .UNSPECIFIED. ) ;
#21603 = EDGE_LOOP ( 'NONE', ( #51204, #42028, #53772 ) ) ;
#21604 = CARTESIAN_POINT ( 'NONE',  ( 18.35296092448800209, 2.690559717027000364, 11.48481263514000084 ) ) ;
#21605 = B_SPLINE_CURVE_WITH_KNOTS ( 'NONE', 3,
 ( #46595, #67901, #20018, #41342, #62655, #19321, #51149, #62986, #52170, #46246, #4270, #9171, #14775, #67552, #57071, #56741, #30177, #3247, #8151, #18984, #41682 ),
 .UNSPECIFIED., .F., .F.,
 ( 4, 2, 2, 2, 2, 2, 2, 1, 2, 2, 4 ),
 ( 0.000000000000000000, 0.2500000000000056066, 0.3750000000000068279, 0.4375000000000077716, 0.5000000000000086597, 0.6250000000000166533, 0.6875000000000203171, 0.7187500000000186517, 0.7343750000000178746, 0.7500000000000172085, 1.000000000000000000 ),
 .UNSPECIFIED. ) ;
#21606 = EDGE_CURVE ( 'NONE', #26681, #43316, #39861, .T. ) ;
#21607 = EDGE_CURVE ( 'NONE', #54071, #16464, #29840, .T. ) ;
#21608 = CARTESIAN_POINT ( 'NONE',  ( 10.18756025349000005, 5.387489739490000318, 8.640945789268998922 ) ) ;
#21609 = CARTESIAN_POINT ( 'NONE',  ( 0.5000220334827000235, 0.000000000000000000, 0.000000000000000000 ) ) ;
#21610 = CARTESIAN_POINT ( 'NONE',  ( 11.98522412107029922, -3.952868550833580130, 8.390877922225699947 ) ) ;
#21611 = CARTESIAN_POINT ( 'NONE',  ( 17.76418844530500252, 3.313976920866999798, -11.22406790378000174 ) ) ;
#21612 = AXIS2_PLACEMENT_3D ( 'NONE', #42258, #35297, #19552 ) ;
#21613 = CARTESIAN_POINT ( 'NONE',  ( 11.09672200990539892, 3.182132064022000328, -7.214709569664399247 ) ) ;
#21614 = CARTESIAN_POINT ( 'NONE',  ( 12.64262999012820998, -0.6038699852804539914, 12.68066884516330717 ) ) ;
#21615 = CARTESIAN_POINT ( 'NONE',  ( 24.42399542544800184, -8.980643143459998257, -9.517742859132999556 ) ) ;
#21616 = CARTESIAN_POINT ( 'NONE',  ( 9.696080515601000371, 2.554416243104999928, 7.600685069647000525 ) ) ;
#21617 = CARTESIAN_POINT ( 'NONE',  ( 11.60581233665799950, -3.287326773434000149, 11.32699406611000015 ) ) ;
#21618 = ORIENTED_EDGE ( 'NONE', *, *, #49164, .F. ) ;
#21619 = DIRECTION ( 'NONE',  ( -1.000000000000000000, 0.000000000000000000, 0.000000000000000000 ) ) ;
#21620 = CARTESIAN_POINT ( 'NONE',  ( 7.028075866130000016, -0.8537514372841999988, -1.069914814413999826 ) ) ;
#21621 = CARTESIAN_POINT ( 'NONE',  ( 17.69797138021023386, 3.108785234939712261, 13.52525919603468729 ) ) ;
#21622 = CARTESIAN_POINT ( 'NONE',  ( 24.70869262301700076, 8.717234922402001374, -9.201991544579998461 ) ) ;
#21623 = CARTESIAN_POINT ( 'NONE',  ( 10.89149144726329865, -4.659577337894599935, -6.569275630703699242 ) ) ;
#21624 = ORIENTED_EDGE ( 'NONE', *, *, #32052, .T. ) ;
#21625 = AXIS2_PLACEMENT_3D ( 'NONE', #60010, #2659, #38689 ) ;
#21626 = CARTESIAN_POINT ( 'NONE',  ( 5.500000000000000000, -12.22293997673000021, 3.800173559041999827 ) ) ;
#21627 = CARTESIAN_POINT ( 'NONE',  ( 8.951357780412001475, 2.821863697211000055, 6.127145479358000024 ) ) ;
#21628 = CIRCLE ( 'NONE', #57365, 1.000000000000000000 ) ;
#21630 = CARTESIAN_POINT ( 'NONE',  ( 10.58079553770030046, 5.100000000000000533, -6.662590550610039131 ) ) ;
#21629 = CARTESIAN_POINT ( 'NONE',  ( 8.953620280414000376, 2.881930053949999682, -8.823338183322999129 ) ) ;
#21631 = CARTESIAN_POINT ( 'NONE',  ( 24.30000000000000071, -10.83443035398000021, 3.855530949778000149 ) ) ;
#21632 = ORIENTED_EDGE ( 'NONE', *, *, #23488, .T. ) ;
#21633 = CARTESIAN_POINT ( 'NONE',  ( 10.92717848204000042, 5.023653513500000223, 8.718036113327999104 ) ) ;
#21634 = CARTESIAN_POINT ( 'NONE',  ( 17.63745110450242493, -3.119885622577724504, -13.52219988749414092 ) ) ;
#21635 = CARTESIAN_POINT ( 'NONE',  ( 11.41256651104150066, 4.098999650273559503, 8.498573944230598087 ) ) ;
#21636 = CARTESIAN_POINT ( 'NONE',  ( 10.70441271436000008, -3.444516450945999786, 6.009051312948000323 ) ) ;
#21637 = CARTESIAN_POINT ( 'NONE',  ( 8.475644353210000759, -5.095088356574999366, 6.286978111459999852 ) ) ;
#21638 = ORIENTED_EDGE ( 'NONE', *, *, #9398, .T. ) ;
#21639 = CARTESIAN_POINT ( 'NONE',  ( 9.278329719590999503, 5.791553967443999973, 7.752111263209999770 ) ) ;
#21641 = CARTESIAN_POINT ( 'NONE',  ( 10.37239314679000124, -3.992345679293999972, -5.977234595428000397 ) ) ;
#21640 = CARTESIAN_POINT ( 'NONE',  ( 10.33103907547007694, 4.774162136902415199, -7.899515915943056577 ) ) ;
#21642 = CARTESIAN_POINT ( 'NONE',  ( 7.888460647515415758, -2.737986541543418806, 8.699910899329831082 ) ) ;
#21643 = CARTESIAN_POINT ( 'NONE',  ( 10.65050275296000137, -5.200029647236999786, 5.937716681140000397 ) ) ;
#21644 = CARTESIAN_POINT ( 'NONE',  ( 23.99166244369300216, 3.573271009703999912, 12.95730409900999902 ) ) ;
#21645 = ORIENTED_EDGE ( 'NONE', *, *, #40023, .T. ) ;
#21646 = CARTESIAN_POINT ( 'NONE',  ( 25.09888444479172520, -11.37375950780082512, -3.274676351230203064 ) ) ;
#21647 = CARTESIAN_POINT ( 'NONE',  ( 11.90841235500450068, -4.841138636481000290, 8.270568563129298667 ) ) ;
#21648 = ADVANCED_FACE ( 'NONE', ( #42765 ), #33432, .F. ) ;
#21649 = CARTESIAN_POINT ( 'NONE',  ( 11.25656651104150008, 4.126085365637900182, 8.771777834828998976 ) ) ;
#21650 = ORIENTED_EDGE ( 'NONE', *, *, #48870, .T. ) ;
#21651 = B_SPLINE_SURFACE_WITH_KNOTS ( 'NONE', 3, 3, ( 
 ( #40464, #2043, #14254, #3402 ),
 ( #56552, #55524, #66343, #28971 ),
 ( #7625, #18466, #19493, #7280 ),
 ( #4771, #67710, #46410, #14932 ),
 ( #20864, #62472, #26113, #5124 ),
 ( #68058, #62813, #57929, #57228 ),
 ( #30337, #31707, #25075, #10369 ),
 ( #20172, #25766, #42202, #52676 ),
 ( #26460, #20519, #30672, #36952 ),
 ( #36255, #58266, #56896, #21204 ) ),
 .UNSPECIFIED., .F., .F., .F.,
 ( 4, 1, 1, 1, 1, 1, 1, 4 ),
 ( 4, 4 ),
 ( 0.07203983506773999068, 0.1428571428570999946, 0.2857142857143000203, 0.4285714285713999594, 0.5714285714286000406, 0.7142857142856999797, 0.8571428571429000609, 0.9589780836993999635 ),
 ( -0.1900620218102000158, 1.190128522698000069 ),
 .UNSPECIFIED. ) ;
#21652 = CARTESIAN_POINT ( 'NONE',  ( 8.523814158775000038, 4.920236664407999783, -6.448229650796999834 ) ) ;
#21653 = EDGE_CURVE ( 'NONE', #26199, #16266, #6732, .T. ) ;
#21654 = CARTESIAN_POINT ( 'NONE',  ( 12.44978597066678461, 1.852986171447649211, -12.46300423074626984 ) ) ;
#21655 = CARTESIAN_POINT ( 'NONE',  ( 11.72567835872029995, -4.993948309075300074, 8.126439557340900066 ) ) ;
#21656 = DIRECTION ( 'NONE',  ( 0.7071067811865475727, -0.7071067811865475727, 0.000000000000000000 ) ) ;
#21657 = CARTESIAN_POINT ( 'NONE',  ( 18.08654171823789980, 2.829006819463714795, -13.59815647008714556 ) ) ;
#21658 = ORIENTED_EDGE ( 'NONE', *, *, #35139, .F. ) ;
#21659 = CARTESIAN_POINT ( 'NONE',  ( 23.56666365135700403, 11.07911597678999271, 4.076188921308005142 ) ) ;
#21660 = CARTESIAN_POINT ( 'NONE',  ( 5.784193173017583511, 1.460959015002474493, -0.3926218265389176953 ) ) ;
#21661 = VERTEX_POINT ( 'NONE', #23857 ) ;
#21662 = CARTESIAN_POINT ( 'NONE',  ( 12.45041481799821348, -3.107897655637140044, -12.21069225363714317 ) ) ;
#21663 = CARTESIAN_POINT ( 'NONE',  ( 10.69872335273220010, 4.349306362047499874, 6.559289673553299060 ) ) ;
#21664 = CARTESIAN_POINT ( 'NONE',  ( 10.22452454188789517, 3.422561976923200078, -8.739574331469023960 ) ) ;
#21665 = CARTESIAN_POINT ( 'NONE',  ( 10.98168093019000047, 2.885380650160000116, -4.904815280032999603 ) ) ;
#21666 = CARTESIAN_POINT ( 'NONE',  ( 8.796304629759626792, -3.464785522094639969, -8.192154231972200051 ) ) ;
#21667 = CARTESIAN_POINT ( 'NONE',  ( 11.11504459742000073, -3.456612073675000119, 5.970342812640000218 ) ) ;
#21668 = CARTESIAN_POINT ( 'NONE',  ( 17.93128725136842760, 0.4990964484179722382, -12.68679736436867778 ) ) ;
#21669 = CARTESIAN_POINT ( 'NONE',  ( 12.36790781773587788, 2.946786910900277334, -12.33618673617031014 ) ) ;
#21670 = CARTESIAN_POINT ( 'NONE',  ( 10.37872469555899890, -3.497841151814999883, -6.631215019384099740 ) ) ;
#21671 = CARTESIAN_POINT ( 'NONE',  ( 8.753448341231001351, 2.876288091423999660, 6.568897128359000526 ) ) ;
#21672 = ORIENTED_EDGE ( 'NONE', *, *, #61788, .F. ) ;
#21673 = AXIS2_PLACEMENT_3D ( 'NONE', #28358, #50025, #60857 ) ;
#21674 = PRESENTATION_STYLE_ASSIGNMENT (( #11878 ) ) ;
#21675 = CARTESIAN_POINT ( 'NONE',  ( 11.09999999999999964, 2.274006712557999688, -7.281956340829000673 ) ) ;
#21676 = DIRECTION ( 'NONE',  ( 0.000000000000000000, 0.6556630511404241135, -0.7550536162215433222 ) ) ;
#21677 = CARTESIAN_POINT ( 'NONE',  ( 11.83148568236900111, 12.32826180562000040, 1.876276850727000012 ) ) ;
#21678 = AXIS2_PLACEMENT_3D ( 'NONE', #17359, #23299, #2656 ) ;
#21679 = CARTESIAN_POINT ( 'NONE',  ( 18.17657007421211190, 2.109712673715142817, 12.42212297180517133 ) ) ;
#21680 = CARTESIAN_POINT ( 'NONE',  ( 10.09999999999999964, 0.000000000000000000, 0.000000000000000000 ) ) ;
#21682 = ADVANCED_FACE ( 'NONE', ( #17583 ), #38909, .T. ) ;
#21681 = CARTESIAN_POINT ( 'NONE',  ( 11.12718332839000013, 8.468770115145998645, 6.787300010133001216 ) ) ;
#21683 = FACE_OUTER_BOUND ( 'NONE', #35176, .T. ) ;
#21684 = EDGE_CURVE ( 'NONE', #11316, #52043, #24004, .T. ) ;
#21685 = CARTESIAN_POINT ( 'NONE',  ( 9.958513540182876156, -4.163624617374470205, -8.749999999999998224 ) ) ;
#21686 = ADVANCED_FACE ( 'NONE', ( #6383 ), #57017, .F. ) ;
#21687 = ORIENTED_EDGE ( 'NONE', *, *, #50048, .T. ) ;
#21688 = CARTESIAN_POINT ( 'NONE',  ( 12.36094932703100469, -3.049537035394455309, 12.22540636754321497 ) ) ;
#21689 = CARTESIAN_POINT ( 'NONE',  ( 10.08560887879199797, -4.227457260387500249, -6.521682313853199631 ) ) ;
#21690 = CARTESIAN_POINT ( 'NONE',  ( 8.745593092018999926, -5.100000000000000533, 6.404090157675000228 ) ) ;
#21691 = CARTESIAN_POINT ( 'NONE',  ( 9.820206362952999868, -3.883324525498000224, 6.055606607331999847 ) ) ;
#21692 = CARTESIAN_POINT ( 'NONE',  ( 12.27359063708300013, -3.044227915785300276, 7.231278212164300001 ) ) ;
#21693 = CARTESIAN_POINT ( 'NONE',  ( 11.16225954179439839, 4.877394611789299894, -8.229019074832200076 ) ) ;
#21694 = CARTESIAN_POINT ( 'NONE',  ( 8.741252916288999586, 4.092558584984410608, 6.625425395127999550 ) ) ;
#21695 = CARTESIAN_POINT ( 'NONE',  ( 0.2855665232602999648, 3.161455490150999914, -0.5535149012972000460 ) ) ;
#21696 = CARTESIAN_POINT ( 'NONE',  ( 8.769549439917666334, 5.100000000000000533, 6.459823844766666490 ) ) ;
#21697 = CARTESIAN_POINT ( 'NONE',  ( 12.22372692396748484, 2.729759399082355653, 12.39506432367437583 ) ) ;
#21699 = CARTESIAN_POINT ( 'NONE',  ( 10.16000000000000014, 4.496968146123999865, -8.755198255949000696 ) ) ;
#21698 = CARTESIAN_POINT ( 'NONE',  ( 9.834329965421998665, 3.206942993865000258, -8.321459087847200564 ) ) ;
#21700 = CARTESIAN_POINT ( 'NONE',  ( 11.55610404293055993, 3.497163090439000310, -8.523936114709998790 ) ) ;
#21701 = CARTESIAN_POINT ( 'NONE',  ( 8.181902110542997875, 2.891006945229997793, -6.386045997152003828 ) ) ;
#21702 = CARTESIAN_POINT ( 'NONE',  ( 10.44812028041000040, 5.235600787608000850, -6.609970743661000903 ) ) ;
#21703 = EDGE_CURVE ( 'NONE', #29163, #40500, #49738, .T. ) ;
#21704 = CYLINDRICAL_SURFACE ( 'NONE', #49464, 0.6999999999999992895 ) ;
#21706 = CARTESIAN_POINT ( 'NONE',  ( 12.64124574432521619, 3.108970204239923874, 12.28865804429016073 ) ) ;
#21705 = CARTESIAN_POINT ( 'NONE',  ( 7.729292060080003246, 5.085123327752999245, 6.553315682963002153 ) ) ;
#21707 = DIRECTION ( 'NONE',  ( -1.000000000000000000, 0.000000000000000000, 0.000000000000000000 ) ) ;
#21708 = ORIENTED_EDGE ( 'NONE', *, *, #35370, .F. ) ;
#21709 = CIRCLE ( 'NONE', #18386, 1.049999999999999378 ) ;
#21710 = CARTESIAN_POINT ( 'NONE',  ( 12.24298814200621521, 0.2740984087646521350, 12.69603503205126316 ) ) ;
#21711 = CARTESIAN_POINT ( 'NONE',  ( 10.84999882987999875, 0.000000000000000000, 0.000000000000000000 ) ) ;
#21712 = DIRECTION ( 'NONE',  ( 0.000000000000000000, -1.000000000000000000, 0.000000000000000000 ) ) ;
#21713 = CARTESIAN_POINT ( 'NONE',  ( 17.74460677677806686, 3.176355914710234707, -12.19306589750529035 ) ) ;
#21714 = CARTESIAN_POINT ( 'NONE',  ( 12.18013031904085963, -2.522561724994069721, 13.66866813226131505 ) ) ;
#21715 = CYLINDRICAL_SURFACE ( 'NONE', #40900, 1.350000000000000533 ) ;
#21716 = CARTESIAN_POINT ( 'NONE',  ( 12.80505043854143388, 1.875000000000000000, 13.78627172894481667 ) ) ;
#21717 = ORIENTED_EDGE ( 'NONE', *, *, #43344, .F. ) ;
#21718 = CARTESIAN_POINT ( 'NONE',  ( 4.148014736430999605, 0.6585737698315999866, 0.8810829645851999681 ) ) ;
#21719 = VECTOR ( 'NONE', #59871, 1000.000000000000114 ) ;
#21720 = DIRECTION ( 'NONE',  ( 1.000000000000000000, 0.000000000000000000, 0.000000000000000000 ) ) ;
#21721 = CARTESIAN_POINT ( 'NONE',  ( 9.564964385875493136, -5.350010280223940207, -7.500002129152480101 ) ) ;
#21722 = FACE_OUTER_BOUND ( 'NONE', #37591, .T. ) ;
#21723 = CARTESIAN_POINT ( 'NONE',  ( 17.86958940788776218, 3.040180081688693470, -12.30916660591379497 ) ) ;
#21724 = CARTESIAN_POINT ( 'NONE',  ( 10.26947109217999810, 5.100000000000000533, -6.152188490330000370 ) ) ;
#21725 = CARTESIAN_POINT ( 'NONE',  ( 11.02287616594229824, 3.738072157442200005, 8.325646653015098764 ) ) ;
#21726 = CARTESIAN_POINT ( 'NONE',  ( 7.000000000000000000, -6.255435840762999966, -3.000000000000000000 ) ) ;
#21727 = CARTESIAN_POINT ( 'NONE',  ( 9.978906853208000527, -5.007779786185999171, -8.772596342864998675 ) ) ;
#21728 = ADVANCED_FACE ( 'NONE', ( #13034 ), #65807, .F. ) ;
#21729 = CARTESIAN_POINT ( 'NONE',  ( 12.80505043854143388, 1.787797342887042840, 13.88538010501570774 ) ) ;
#21730 = B_SPLINE_CURVE_WITH_KNOTS ( 'NONE', 3,
 ( #47860, #52750, #35981, #57643, #58680, #16028, #36679, #5539, #26878, #5194, #4845, #52053, #15691, #15003, #31778, #41234, #26532, #47512, #69166, #62545, #9402, #30744, #41916, #20591 ),
 .UNSPECIFIED., .F., .F.,
 ( 4, 2, 1, 1, 1, 2, 2, 1, 2, 2, 2, 2, 2, 4 ),
 ( 0.000000000000000000, 0.2499999999999459876, 0.3749999999999235056, 0.4374999999999063527, 0.4687499999999000244, 0.4843749999998934741, 0.4999999999998869238, 0.5624999999998998579, 0.5937499999999029665, 0.6249999999999059641, 0.6874999999999128475, 0.7499999999999197309, 0.8749999999999599209, 1.000000000000000000 ),
 .UNSPECIFIED. ) ;
#21731 = FACE_OUTER_BOUND ( 'NONE', #14727, .T. ) ;
#21732 = CARTESIAN_POINT ( 'NONE',  ( 24.14647270089509590, 9.145016144872478492, -9.120921824230352470 ) ) ;
#21733 = CARTESIAN_POINT ( 'NONE',  ( 9.600000000000001421, 12.34999999999999964, 4.046978687741000012E-05 ) ) ;
#21734 = APPLICATION_CONTEXT ( 'automotive_design' ) ;
#21735 = AXIS2_PLACEMENT_3D ( 'NONE', #38596, #44892, #32669 ) ;
#21736 = EDGE_LOOP ( 'NONE', ( #3189, #24736, #53364, #45254 ) ) ;
#21737 = CARTESIAN_POINT ( 'NONE',  ( 8.365779719592000063, 2.949305648881000330, -8.659807625323999503 ) ) ;
#21738 = CARTESIAN_POINT ( 'NONE',  ( 12.27359063708300013, -3.044227915785300276, 7.231278212164300001 ) ) ;
#21739 = ORIENTED_EDGE ( 'NONE', *, *, #20871, .T. ) ;
#21740 = CARTESIAN_POINT ( 'NONE',  ( 17.55505043854143921, 0.7302158263239199032, -13.98094363220830871 ) ) ;
#21741 = CARTESIAN_POINT ( 'NONE',  ( 11.47810404293059960, -4.563346034752700398, -8.647151967355000579 ) ) ;
#21742 = VERTEX_POINT ( 'NONE', #27734 ) ;
#21743 = CARTESIAN_POINT ( 'NONE',  ( 11.64633327354034797, 3.135095881599500256, 8.065722083251399610 ) ) ;
#21744 = CARTESIAN_POINT ( 'NONE',  ( 6.471626508332579242, 0.2400263920404566986, -1.106823019747933401 ) ) ;
#21745 = DIRECTION ( 'NONE',  ( 1.000000000000000000, 0.000000000000000000, 0.000000000000000000 ) ) ;
#21746 = CARTESIAN_POINT ( 'NONE',  ( 9.856851002545999663, -2.832432432432000269, -6.822293592207000934 ) ) ;
#21747 = CARTESIAN_POINT ( 'NONE',  ( 11.44366954483529852, -3.514796851401900124, -6.751356298874699569 ) ) ;
#21748 = CARTESIAN_POINT ( 'NONE',  ( 12.21931057679652177, -0.2190559830447486311, -13.89769592719591884 ) ) ;
#21749 = CARTESIAN_POINT ( 'NONE',  ( 9.582867883171827472, -3.217326796159980518, 6.525013452213887177 ) ) ;
#21750 = CARTESIAN_POINT ( 'NONE',  ( 10.33022766388000058, -2.650179121646999647, -7.694581537458001108 ) ) ;
#21751 = CARTESIAN_POINT ( 'NONE',  ( 13.32922381500400100, 11.63215034022999994, 1.960198572322999988 ) ) ;
#21752 = ORIENTED_EDGE ( 'NONE', *, *, #38135, .T. ) ;
#21753 = PLANE ( 'NONE',  #33322 ) ;
#21754 = ORIENTED_EDGE ( 'NONE', *, *, #59035, .T. ) ;
#21755 = CARTESIAN_POINT ( 'NONE',  ( 0.5091598036225351009, -3.178301708211344945, 0.6894924743205468332 ) ) ;
#21756 = SURFACE_STYLE_FILL_AREA ( #5679 ) ;
#21757 = VERTEX_POINT ( 'NONE', #54638 ) ;
#21758 = CARTESIAN_POINT ( 'NONE',  ( 17.65076761715808473, -3.243341803256440947, -13.61913462216701376 ) ) ;
#21759 = CARTESIAN_POINT ( 'NONE',  ( 17.99149020822394363, -2.947405452019512317, -12.33598828993208230 ) ) ;
#21760 =( GEOMETRIC_REPRESENTATION_CONTEXT ( 3 ) GLOBAL_UNCERTAINTY_ASSIGNED_CONTEXT ( ( #30421 ) ) GLOBAL_UNIT_ASSIGNED_CONTEXT ( ( #9045, #52381, #67085 ) ) REPRESENTATION_CONTEXT ( 'NONE', 'WORKASPACE' ) );
#21761 = CARTESIAN_POINT ( 'NONE',  ( 10.50145247700547557, 3.917463882723016599, 8.370216864706282678 ) ) ;
#21762 = PLANE ( 'NONE',  #24035 ) ;
#21763 = CARTESIAN_POINT ( 'NONE',  ( 10.85068991645999859, -4.478102922274999287, 6.162028334171000488 ) ) ;
#21764 = CARTESIAN_POINT ( 'NONE',  ( 18.17956732772856654, -2.474903466465859569, -12.45737214979850727 ) ) ;
#21765 = EDGE_CURVE ( 'NONE', #8532, #8998, #31557, .T. ) ;
#21766 = CARTESIAN_POINT ( 'NONE',  ( 12.22351867101279588, 0.2292390942789186981, 13.89746050377130793 ) ) ;
#21767 = ADVANCED_FACE ( 'NONE', ( #65105 ), #17230, .F. ) ;
#21768 = ORIENTED_EDGE ( 'NONE', *, *, #22869, .T. ) ;
#21769 = CARTESIAN_POINT ( 'NONE',  ( 12.66849918197500102, 12.16651130357000099, -3.137066692814999946 ) ) ;
#21770 = CARTESIAN_POINT ( 'NONE',  ( 18.38283964371600376, 11.91307312420999942, -3.686993282830000052 ) ) ;
#21771 = CARTESIAN_POINT ( 'NONE',  ( 9.480191603681626944, 4.150249255682260774, 8.361949783971203587 ) ) ;
#21772 = CARTESIAN_POINT ( 'NONE',  ( 4.392853487642000232, 1.339550729022999986, -0.6343589122600999941 ) ) ;
#21773 = CARTESIAN_POINT ( 'NONE',  ( 25.59994555223599733, -2.024003533649000097, 11.01554633311000053 ) ) ;
#21774 = CARTESIAN_POINT ( 'NONE',  ( 18.47691931228784057, 11.93204885577847030, -3.809797076885868439 ) ) ;
#21775 = CARTESIAN_POINT ( 'NONE',  ( 10.32701825126999928, -5.663784181836000187, -6.682035927671000408 ) ) ;
#21776 = VERTEX_POINT ( 'NONE', #66499 ) ;
#21777 = EDGE_LOOP ( 'NONE', ( #66521, #15923, #34282, #34062 ) ) ;
#21778 = CARTESIAN_POINT ( 'NONE',  ( 17.55505043854143921, 0.7302158263239199032, -13.98094363220830871 ) ) ;
#21779 = CARTESIAN_POINT ( 'NONE',  ( 11.79999999550100220, 11.52577121388000059, 1.696750555870000010 ) ) ;
#21780 = CARTESIAN_POINT ( 'NONE',  ( 17.65075606735202740, -1.792616958753535439, 13.88476197432802373 ) ) ;
#21781 = CARTESIAN_POINT ( 'NONE',  ( 0.000000000000000000, 0.000000000000000000, 0.000000000000000000 ) ) ;
#21782 = FACE_OUTER_BOUND ( 'NONE', #31874, .T. ) ;
#21783 = B_SPLINE_CURVE_WITH_KNOTS ( 'NONE', 3,
 ( #13321, #44787, #3153, #45126, #45808 ),
 .UNSPECIFIED., .F., .F.,
 ( 4, 1, 4 ),
 ( 0.000000000000000000, 0.5000000000000000000, 1.000000000000000000 ),
 .UNSPECIFIED. ) ;
#21784 = CARTESIAN_POINT ( 'NONE',  ( 11.22056920625029974, 4.047312782235129802, -6.184582852561999466 ) ) ;
#21785 = EDGE_CURVE ( 'NONE', #47809, #65244, #44512, .T. ) ;
#21786 = CARTESIAN_POINT ( 'NONE',  ( 9.786633995697998856, 4.998281561686200192, -7.610798122400000310 ) ) ;
#21788 = CARTESIAN_POINT ( 'NONE',  ( 1.985247277619000217, 2.372532593102000043, -2.573147701680999599 ) ) ;
#21787 = CARTESIAN_POINT ( 'NONE',  ( 10.81155864497999808, -3.317414799430800088, 6.965412239408199646 ) ) ;
#21789 = CARTESIAN_POINT ( 'NONE',  ( 7.602716214150000873, -2.929796814311000919, 6.536389039862005035 ) ) ;
#21790 = ORIENTED_EDGE ( 'NONE', *, *, #54038, .F. ) ;
#21791 = B_SPLINE_CURVE_WITH_KNOTS ( 'NONE', 3,
 ( #36857, #32987, #6405, #27753, #32645, #5379, #49065, #1172, #53619 ),
 .UNSPECIFIED., .F., .F.,
 ( 4, 1, 2, 2, 4 ),
 ( 0.000000000000000000, 0.2499999999999998890, 0.3750000000000004996, 0.5000000000000011102, 1.000000000000000000 ),
 .UNSPECIFIED. ) ;
#21792 = ADVANCED_FACE ( 'NONE', ( #60575 ), #34014, .F. ) ;
#21793 = CARTESIAN_POINT ( 'NONE',  ( 11.01279632507519857, 4.624908853805600906, 6.341531314375999706 ) ) ;
#21794 = CARTESIAN_POINT ( 'NONE',  ( 9.504901164121001500, -3.934733502342999678, 5.704835336325999151 ) ) ;
#21795 = CARTESIAN_POINT ( 'NONE',  ( 9.555709346417000205, 5.031430618794000331, 7.989780896525600085 ) ) ;
#21796 = FACE_OUTER_BOUND ( 'NONE', #53791, .T. ) ;
#21797 = CARTESIAN_POINT ( 'NONE',  ( 11.20904026220999938, -5.937811873294999820, 7.147336919140999001 ) ) ;
#21798 = CARTESIAN_POINT ( 'NONE',  ( 18.17230637740977883, 2.598591657315551640, -12.42808133542726701 ) ) ;
#21799 = CARTESIAN_POINT ( 'NONE',  ( 16.39974593105000267, -3.376006003137999922, -11.11079012987999981 ) ) ;
#21800 = AXIS2_PLACEMENT_3D ( 'NONE', #53933, #64756, #49042 ) ;
#21801 = CARTESIAN_POINT ( 'NONE',  ( 9.659988259785999176, -4.131418345883800747, -8.495776841814999258 ) ) ;
#21802 = CARTESIAN_POINT ( 'NONE',  ( 5.325217628334000253, -0.8655273653155000080, -0.9996707749736001292 ) ) ;
#21803 = B_SPLINE_SURFACE_WITH_KNOTS ( 'NONE', 3, 3, ( 
 ( #21938, #280, #22977, #54797 ),
 ( #1313, #11450, #28233, #49548 ),
 ( #38371, #39069, #21593, #16353 ),
 ( #42932, #33830, #5860, #6199 ),
 ( #32789, #59695, #628, #37682 ),
 ( #11796, #44326, #43974, #7247 ),
 ( #976, #17392, #38722, #48868 ),
 ( #65280, #33136, #54452, #1661 ),
 ( #6553, #55144, #27896, #49206 ) ),
 .UNSPECIFIED., .F., .F., .F.,
 ( 4, 1, 1, 1, 1, 1, 4 ),
 ( 4, 4 ),
 ( 0.02288375853139000202, 0.1666666666667000196, 0.3333333333333000081, 0.5000000000000000000, 0.6666666666667000474, 0.8333333333333000637, 0.9485331614075999118 ),
 ( -0.1900389547208000129, 1.190219847277000031 ),
 .UNSPECIFIED. ) ;
#21804 = CARTESIAN_POINT ( 'NONE',  ( 12.80505043854144098, 0.7302158263239095781, 13.98094363220830871 ) ) ;
#21805 = DIRECTION ( 'NONE',  ( 1.000000000000000000, 0.000000000000000000, 0.000000000000000000 ) ) ;
#21806 = ORIENTED_EDGE ( 'NONE', *, *, #16084, .F. ) ;
#21807 = B_SPLINE_CURVE_WITH_KNOTS ( 'NONE', 3,
 ( #2299, #28534, #61028, #18043 ),
 .UNSPECIFIED., .F., .F.,
 ( 4, 4 ),
 ( 0.000000000000000000, 1.000000000000000000 ),
 .UNSPECIFIED. ) ;
#21808 = CARTESIAN_POINT ( 'NONE',  ( 12.54669586862715036, 0.5691963043021760482, -12.68282590392938225 ) ) ;
#21809 = CARTESIAN_POINT ( 'NONE',  ( 10.99826088462129903, 4.001843064679911244, -6.633804182961699603 ) ) ;
#21810 = LINE ( 'NONE', #29152, #17538 ) ;
#21811 = FACE_OUTER_BOUND ( 'NONE', #41812, .T. ) ;
#21812 = CARTESIAN_POINT ( 'NONE',  ( 8.239310352252543268, -2.650829846289642688, 7.263894687833495567 ) ) ;
#21813 = EDGE_LOOP ( 'NONE', ( #40934, #59670, #738, #37773 ) ) ;
#21814 = CARTESIAN_POINT ( 'NONE',  ( 7.673170892156151446, -2.921517931055129580, 8.328373548166320361 ) ) ;
#21815 = ITEM_DEFINED_TRANSFORMATION ( 'NONE', 'NONE', #19533,  #9676 ) ;
#21816 = CARTESIAN_POINT ( 'NONE',  ( 11.52677869730533011, -4.403502086956500250, -6.704332466833498927 ) ) ;
#21817 = CARTESIAN_POINT ( 'NONE',  ( 18.18005043854147118, -2.500000000000000000, -25.00000000000000000 ) ) ;
#21818 = CARTESIAN_POINT ( 'NONE',  ( 13.69997185827400266, -11.40547114375999982, -2.374390024598000082 ) ) ;
#21819 = CARTESIAN_POINT ( 'NONE',  ( 10.93210843320491676, 2.862311695598936723, -8.098394516494938244 ) ) ;
#21820 = CARTESIAN_POINT ( 'NONE',  ( 11.56833327354034857, 3.253412192327699959, -7.011667014989399149 ) ) ;
#21821 = ORIENTED_EDGE ( 'NONE', *, *, #37013, .T. ) ;
#21822 = CARTESIAN_POINT ( 'NONE',  ( 9.799258316471000541, -4.057329063942999525, 9.430691159271001212 ) ) ;
#21823 = CARTESIAN_POINT ( 'NONE',  ( 18.03303331148765665, 2.902815211882732616, -13.57973159350535397 ) ) ;
#21824 = ORIENTED_EDGE ( 'NONE', *, *, #53131, .F. ) ;
#21825 = CARTESIAN_POINT ( 'NONE',  ( 7.100083736560635295, 0.3076767997638333307, -3.048821334907659608 ) ) ;
#21826 = LINE ( 'NONE', #38253, #63652 ) ;
#21827 = VECTOR ( 'NONE', #463, 999.9999999999998863 ) ;
#21828 = CARTESIAN_POINT ( 'NONE',  ( 8.722714158775000115, 3.892978337449999771, -8.893414073324001023 ) ) ;
#21829 = PRODUCT_RELATED_PRODUCT_CATEGORY ( 'part', '', ( #61747 ) ) ;
#21830 = VERTEX_POINT ( 'NONE', #54281 ) ;
#21831 = CARTESIAN_POINT ( 'NONE',  ( 6.371592353486001059, 1.499999999999999556, 0.3122588619777424968 ) ) ;
#21832 = CARTESIAN_POINT ( 'NONE',  ( 7.713110841224000147, 3.406663518590999917, -5.695144508491999602 ) ) ;
#21833 = CARTESIAN_POINT ( 'NONE',  ( 15.90006914250090198, -3.698856701507905687, -11.75540275481944619 ) ) ;
#21834 = DIRECTION ( 'NONE',  ( 0.000000000000000000, 0.000000000000000000, -1.000000000000000000 ) ) ;
#21835 = ORIENTED_EDGE ( 'NONE', *, *, #31210, .F. ) ;
#21836 = CARTESIAN_POINT ( 'NONE',  ( 9.848732933287999813, -2.769734897491000325, 6.441850735262000249 ) ) ;
#21837 = CARTESIAN_POINT ( 'NONE',  ( 24.56891981372000089, 12.04603233683999974, -3.139955828721999964 ) ) ;
#21838 = CARTESIAN_POINT ( 'NONE',  ( 11.11486084871780022, 5.207010770456999893, -7.174999999999999822 ) ) ;
#21839 = ORIENTED_EDGE ( 'NONE', *, *, #11738, .T. ) ;
#21840 = CARTESIAN_POINT ( 'NONE',  ( 6.096693173016666023, -1.310679582531386389, -0.7554284705563492075 ) ) ;
#21841 = CARTESIAN_POINT ( 'NONE',  ( 10.10735564678999943, -4.293585439421999439, -8.994200998147999115 ) ) ;
#21842 = ORIENTED_EDGE ( 'NONE', *, *, #56665, .F. ) ;
#21843 = CARTESIAN_POINT ( 'NONE',  ( 23.58115046238600954, -10.23378857499904804, 9.530750715746675539 ) ) ;
#21844 = CARTESIAN_POINT ( 'NONE',  ( 18.17906596528623098, 0.04061643748080398519, -13.89993966956671834 ) ) ;
#21845 = CARTESIAN_POINT ( 'NONE',  ( 4.408554738853999844, -0.8547558900528000603, 1.129519256798999782 ) ) ;
#21846 = CARTESIAN_POINT ( 'NONE',  ( 7.917797682304002826, 5.086214043998999124, -6.452211737291995597 ) ) ;
#21847 = CARTESIAN_POINT ( 'NONE',  ( 16.39932787941000214, 3.295363098100999810, 11.83520513879000013 ) ) ;
#21848 = CARTESIAN_POINT ( 'NONE',  ( 11.11486084871780022, -2.792989229543000107, -7.174999999999999822 ) ) ;
#21849 = CARTESIAN_POINT ( 'NONE',  ( 9.237760194560388882, -4.066145789045416237, 6.629534018758292291 ) ) ;
#21850 = ORIENTED_EDGE ( 'NONE', *, *, #57925, .T. ) ;
#21851 = EDGE_CURVE ( 'NONE', #41213, #46101, #2334, .T. ) ;
#21852 = CARTESIAN_POINT ( 'NONE',  ( 8.698396402458998367, 3.630894432589700127, -8.298253663472900499 ) ) ;
#21853 = EDGE_CURVE ( 'NONE', #23533, #35290, #55705, .T. ) ;
#21854 = ORIENTED_EDGE ( 'NONE', *, *, #38511, .T. ) ;
#21855 = CARTESIAN_POINT ( 'NONE',  ( 10.98286939055999945, 3.998514186275999638, 9.091062412789998604 ) ) ;
#21856 = CARTESIAN_POINT ( 'NONE',  ( 4.536684337565999314, -1.006062275253510663, 1.158256468153602725 ) ) ;
#21857 =( GEOMETRIC_REPRESENTATION_CONTEXT ( 3 ) GLOBAL_UNCERTAINTY_ASSIGNED_CONTEXT ( ( #10800 ) ) GLOBAL_UNIT_ASSIGNED_CONTEXT ( ( #56258, #56600, #23752 ) ) REPRESENTATION_CONTEXT ( 'NONE', 'WORKASPACE' ) );
#21858 = CARTESIAN_POINT ( 'NONE',  ( 17.60000003185799855, -12.11983897296999935, 3.159727888982000188 ) ) ;
#21859 = CARTESIAN_POINT ( 'NONE',  ( 12.20019055993959078, 2.341318142288554061, -13.70585175580907666 ) ) ;
#21860 = FACE_OUTER_BOUND ( 'NONE', #43286, .T. ) ;
#21861 = CARTESIAN_POINT ( 'NONE',  ( 18.11581248800844435, -0.2761834754990949992, 13.89631168292872587 ) ) ;
#21862 = AXIS2_PLACEMENT_3D ( 'NONE', #33404, #27821, #44935 ) ;
#21863 = CARTESIAN_POINT ( 'NONE',  ( 17.63844293491913362, 0.6206536995415011804, 13.88134483103365824 ) ) ;
#21864 = ORIENTED_EDGE ( 'NONE', *, *, #17138, .F. ) ;
#21865 = CARTESIAN_POINT ( 'NONE',  ( 12.30787805059924978, 0.3788776036388727952, 13.89305317344797253 ) ) ;
#21866 = CARTESIAN_POINT ( 'NONE',  ( 11.75656651104150008, -3.873914634362100262, 8.771777834828998976 ) ) ;
#21867 = DIRECTION ( 'NONE',  ( -1.000000000000000000, 0.000000000000000000, 0.000000000000000000 ) ) ;
#21868 = CARTESIAN_POINT ( 'NONE',  ( 10.57314899745999881, 5.167567567567999731, -6.822293592207000934 ) ) ;
#21869 = CARTESIAN_POINT ( 'NONE',  ( 8.785191940379998954, -5.414909314743000301, 8.890670256079998168 ) ) ;
#21871 = CARTESIAN_POINT ( 'NONE',  ( 13.69997185827400266, 11.40547114375999982, 2.374390024598000082 ) ) ;
#21870 = CARTESIAN_POINT ( 'NONE',  ( 10.13049857835000012, 3.092060693447000297, 8.629378633793999498 ) ) ;
#21872 = CARTESIAN_POINT ( 'NONE',  ( 11.42887348028849992, 2.875789035466000065, -8.107837221875000111 ) ) ;
#21873 = AXIS2_PLACEMENT_3D ( 'NONE', #62050, #56118, #20088 ) ;
#21874 = EDGE_CURVE ( 'NONE', #50564, #59819, #45892, .T. ) ;
#21875 = CARTESIAN_POINT ( 'NONE',  ( 24.36809152945900081, -8.862862741694000235, -8.808753452432000586 ) ) ;
#21876 = AXIS2_PLACEMENT_3D ( 'NONE', #21585, #15999, #5512 ) ;
#21877 = CARTESIAN_POINT ( 'NONE',  ( 10.34271159708237242, 5.100000000000000533, -6.305985890001590377 ) ) ;
#21878 = CARTESIAN_POINT ( 'NONE',  ( 18.08024441302280394, -0.3389720875425239477, 12.69391532355468044 ) ) ;
#21879 = DIRECTION ( 'NONE',  ( 0.9999999999938153916, -3.516990153967770421E-06, -1.152484550329258267E-11 ) ) ;
#21880 = B_SPLINE_CURVE_WITH_KNOTS ( 'NONE', 3,
 ( #56416, #8519, #23222, #44569 ),
 .UNSPECIFIED., .F., .F.,
 ( 4, 4 ),
 ( 0.8163836489557121379, 1.000000000000000000 ),
 .UNSPECIFIED. ) ;
#21881 = CARTESIAN_POINT ( 'NONE',  ( 12.79999999468004646, 11.20144845259485678, -4.552734317499857575 ) ) ;
#21882 = ORIENTED_EDGE ( 'NONE', *, *, #53954, .T. ) ;
#21883 = CARTESIAN_POINT ( 'NONE',  ( 9.112168146794999757, -2.368260286481999710, 7.410200011629000549 ) ) ;
#21884 = CARTESIAN_POINT ( 'NONE',  ( 8.962745559623000347, -5.445226602819000838, 7.703375344019999460 ) ) ;
#21885 = LINE ( 'NONE', #32396, #31608 ) ;
#21886 = CARTESIAN_POINT ( 'NONE',  ( 11.09999999999999964, -5.350000000000000533, -7.500000000000000000 ) ) ;
#21887 = CARTESIAN_POINT ( 'NONE',  ( 0.4199759624411000258, 3.484641797009000008, -0.6100991035018999975 ) ) ;
#21888 = DIRECTION ( 'NONE',  ( 1.000000000000000000, 0.000000000000000000, 0.000000000000000000 ) ) ;
#21889 = CARTESIAN_POINT ( 'NONE',  ( 2.075564546595999982, 3.096074255452000212, 2.131331154000000172 ) ) ;
#21890 = VERTEX_POINT ( 'NONE', #51797 ) ;
#21891 = CARTESIAN_POINT ( 'NONE',  ( 12.58342066637852597, -0.6849607937330853824, -12.58136878870645070 ) ) ;
#21892 = DIRECTION ( 'NONE',  ( 0.000000000000000000, 1.000000000000000000, 0.000000000000000000 ) ) ;
#21893 = CARTESIAN_POINT ( 'NONE',  ( 17.97968936757969161, 3.063621360739230415, -12.22187700344946748 ) ) ;
#21894 = CARTESIAN_POINT ( 'NONE',  ( 5.602673821508641794, 12.13104802960955197, 3.749633869517943197 ) ) ;
#21895 = CARTESIAN_POINT ( 'NONE',  ( 8.437857780412000963, 2.606995215518000286, 6.345762205468999717 ) ) ;
#21896 = ORIENTED_EDGE ( 'NONE', *, *, #7524, .F. ) ;
#21897 = CARTESIAN_POINT ( 'NONE',  ( 5.578758726594999828, -1.574491786429000006, -0.3581626104627999574 ) ) ;
#21898 = CARTESIAN_POINT ( 'NONE',  ( 8.394495280407999971, 4.421485762723999180, -5.992852494763999616 ) ) ;
#21899 = CARTESIAN_POINT ( 'NONE',  ( 8.415400305754983989, -2.414631728478774164, 8.215148636469683296 ) ) ;
#21900 = CARTESIAN_POINT ( 'NONE',  ( 9.193455549952998851, -3.004437130344999929, 8.303267676773000261 ) ) ;
#21901 = VERTEX_POINT ( 'NONE', #56367 ) ;
#21902 = DIRECTION ( 'NONE',  ( 0.000000000000000000, -1.000000000000000000, 0.000000000000000000 ) ) ;
#21903 = CARTESIAN_POINT ( 'NONE',  ( 11.56631965465000178, 11.51200727500000021, 1.523108403756999962 ) ) ;
#21904 = ORIENTED_EDGE ( 'NONE', *, *, #16042, .T. ) ;
#21905 = CARTESIAN_POINT ( 'NONE',  ( 16.10004050617000004, -3.886235259787000018, -11.90683839252000098 ) ) ;
#21906 = CARTESIAN_POINT ( 'NONE',  ( 16.39999999270239428, -3.259293166955308685, -11.55581727975966544 ) ) ;
#21907 = VECTOR ( 'NONE', #52873, 999.9999999999998863 ) ;
#21908 = CARTESIAN_POINT ( 'NONE',  ( 18.02507847443574818, -0.4124479947379862121, -13.89177559470775236 ) ) ;
#21909 = EDGE_CURVE ( 'NONE', #66745, #47384, #56567, .T. ) ;
#21910 = EDGE_CURVE ( 'NONE', #54965, #67391, #21514, .T. ) ;
#21911 = EDGE_LOOP ( 'NONE', ( #65592, #49448, #67897, #26751 ) ) ;
#21912 = CARTESIAN_POINT ( 'NONE',  ( 10.07314899745999881, -5.167567567567999731, -6.822293592207000934 ) ) ;
#21913 = SURFACE_STYLE_FILL_AREA ( #1292 ) ;
#21914 = CARTESIAN_POINT ( 'NONE',  ( 11.27745123989519982, 4.410212499603100689, -8.292221125039500151 ) ) ;
#21915 = CARTESIAN_POINT ( 'NONE',  ( 9.911640687502833558, 2.873222873817937284, -6.752018918866299124 ) ) ;
#21916 = CARTESIAN_POINT ( 'NONE',  ( 11.51041369783139956, -4.064477673403060543, 6.223614866029000048 ) ) ;
#21917 = ORIENTED_EDGE ( 'NONE', *, *, #43679, .F. ) ;
#21918 = CARTESIAN_POINT ( 'NONE',  ( 7.384454719589999883, 3.346262376537000094, 6.002251090845000192 ) ) ;
#21919 = B_SPLINE_CURVE_WITH_KNOTS ( 'NONE', 3,
 ( #43165, #33028, #64471, #54340, #32346, #37920, #64820, #16595, #32683, #52973, #16930, #15571, #5070, #68695, #58905, #27096, #5419, #174, #47388, #26059, #48759, #48411, #59239, #27437, #20809, #38263 ),
 .UNSPECIFIED., .F., .F.,
 ( 4, 2, 2, 2, 2, 2, 2, 2, 2, 2, 2, 2, 4 ),
 ( 0.2965955339900564480, 0.4724466504925387000, 0.4944280400553493493, 0.5164094296181600541, 0.5603722087437794652, 0.6482977669950162891, 0.7362233252462531130, 0.7472140200276574662, 0.7582047148090619304, 0.7801861043718725242, 0.8241488834974980415, 0.9120744417487489653, 1.000000000000000000 ),
 .UNSPECIFIED. ) ;
#21920 = ORIENTED_EDGE ( 'NONE', *, *, #60053, .T. ) ;
#21921 = CARTESIAN_POINT ( 'NONE',  ( 4.600000365992000795, -13.09999963393000044, -1.605909432238000048E-09 ) ) ;
#21922 = AXIS2_PLACEMENT_3D ( 'NONE', #56318, #12988, #45825 ) ;
#21923 = CARTESIAN_POINT ( 'NONE',  ( 15.64816728597000228, -9.503848651356001653, -8.217120907884000403 ) ) ;
#21924 = CARTESIAN_POINT ( 'NONE',  ( 11.01817350255000072, 5.556623262518999518, -4.991714128839999987 ) ) ;
#21925 = VERTEX_POINT ( 'NONE', #3555 ) ;
#21926 = CARTESIAN_POINT ( 'NONE',  ( 12.64104727702816433, -1.896551500700493165, -12.57186431639862256 ) ) ;
#21927 = DIRECTION ( 'NONE',  ( -1.000000000000000000, 0.000000000000000000, 0.000000000000000000 ) ) ;
#21928 = CARTESIAN_POINT ( 'NONE',  ( 7.908904767662867208, 2.849922932654429975, -6.792160572118948636 ) ) ;
#21929 = CARTESIAN_POINT ( 'NONE',  ( 5.000030787343000327, -2.099962892530999881, 0.000000000000000000 ) ) ;
#21930 = CARTESIAN_POINT ( 'NONE',  ( 12.28223951138208925, -3.023960592195344521, -13.66951858831273903 ) ) ;
#21931 = CARTESIAN_POINT ( 'NONE',  ( 11.50687348028854906, -5.003459210197000573, -8.042549288197099244 ) ) ;
#21932 = CARTESIAN_POINT ( 'NONE',  ( 12.70915608519175954, -1.765590719838300959, 12.47568749009910505 ) ) ;
#21933 = CARTESIAN_POINT ( 'NONE',  ( 18.26373780016888304, -2.633255345072546216, 12.32177353326231284 ) ) ;
#21934 = VERTEX_POINT ( 'NONE', #51119 ) ;
#21935 = CARTESIAN_POINT ( 'NONE',  ( 11.09590547754519996, -2.684394667508000154, -7.541753805330609239 ) ) ;
#21936 = ADVANCED_FACE ( 'NONE', ( #61950 ), #13384, .T. ) ;
#21937 = ORIENTED_EDGE ( 'NONE', *, *, #40479, .F. ) ;
#21938 = CARTESIAN_POINT ( 'NONE',  ( 11.53898320224999985, -12.47165320829000024, -1.511147746418000093 ) ) ;
#21939 = CARTESIAN_POINT ( 'NONE',  ( 9.942214158770999788, 3.986577607995999806, -9.280166295424001177 ) ) ;
#21940 = EDGE_CURVE ( 'NONE', #42555, #958, #11475, .T. ) ;
#21941 = CARTESIAN_POINT ( 'NONE',  ( 11.07336716268999943, 2.375546981533999791, -8.393546861057000541 ) ) ;
#21942 = CARTESIAN_POINT ( 'NONE',  ( 10.21238410957999854, -4.072568653311000375, -8.861841462475000597 ) ) ;
#21943 = CARTESIAN_POINT ( 'NONE',  ( 24.30000565603569029, 12.09374148929426163, 3.240508265528289744 ) ) ;
#21944 = CARTESIAN_POINT ( 'NONE',  ( 24.15348338235900272, -12.81658634417999920, 3.250012531303999808 ) ) ;
#21946 = DIRECTION ( 'NONE',  ( 0.000000000000000000, 0.000000000000000000, -1.000000000000000000 ) ) ;
#21945 = B_SPLINE_CURVE_WITH_KNOTS ( 'NONE', 1,
 ( #5082, #29710 ),
 .UNSPECIFIED., .F., .F.,
 ( 2, 2 ),
 ( 0.000000000000000000, 1.000000000000000000 ),
 .UNSPECIFIED. ) ;
#21947 = ORIENTED_EDGE ( 'NONE', *, *, #27306, .T. ) ;
#21948 = FACE_OUTER_BOUND ( 'NONE', #24007, .T. ) ;
#21949 = CARTESIAN_POINT ( 'NONE',  ( 9.442843574488000158, 2.691255504502000129, 6.269523028052000235 ) ) ;
#21950 = CARTESIAN_POINT ( 'NONE',  ( 10.11094409420000062, -5.100000000000000533, -6.571291218949999902 ) ) ;
#21951 = CARTESIAN_POINT ( 'NONE',  ( 11.02435971519499880, -3.467537960339900138, 8.385788382729799650 ) ) ;
#21952 = CARTESIAN_POINT ( 'NONE',  ( 11.30000285318000230, -11.76356368987999979, -1.428410073821000159 ) ) ;
#21953 = CARTESIAN_POINT ( 'NONE',  ( 11.14004124368000070, 9.840151972678000902, -6.095223425601000500 ) ) ;
#21954 = VECTOR ( 'NONE', #1639, 1000.000000000000000 ) ;
#21955 = EDGE_CURVE ( 'NONE', #50878, #24248, #28216, .T. ) ;
#21956 = CARTESIAN_POINT ( 'NONE',  ( 10.76947109217999810, 5.100000000000000533, -6.152188490330000370 ) ) ;
#21957 = VECTOR ( 'NONE', #63966, 1000.000000000000000 ) ;
#21958 = CARTESIAN_POINT ( 'NONE',  ( 23.85319031184999972, -9.641546400920999460, -9.631730852994000003 ) ) ;
#21959 = CARTESIAN_POINT ( 'NONE',  ( 23.83528395833900149, -9.657441433821000842, 9.482667428683999589 ) ) ;
#21960 = CARTESIAN_POINT ( 'NONE',  ( 23.59999193302000364, -13.22318594659000013, 4.267778254689999606 ) ) ;
#21961 = CIRCLE ( 'NONE', #39854, 0.6999999999999992895 ) ;
#21962 = ORIENTED_EDGE ( 'NONE', *, *, #5726, .F. ) ;
#21963 = PLANE ( 'NONE',  #26430 ) ;
#21964 = CARTESIAN_POINT ( 'NONE',  ( 6.762665658289999548, -0.7882360144965000481, 0.7672747788395000157 ) ) ;
#21965 = CARTESIAN_POINT ( 'NONE',  ( 17.99238080566774300, 2.053374525523682603, 13.75805324639251026 ) ) ;
#21966 = CARTESIAN_POINT ( 'NONE',  ( 21.70000133425200062, -14.00000000000000000, 0.000000000000000000 ) ) ;
#21967 = CARTESIAN_POINT ( 'NONE',  ( 10.32533997688000049, -3.756890902898200046, -6.385465081946999355 ) ) ;
#21968 = VERTEX_POINT ( 'NONE', #67184 ) ;
#21969 = VECTOR ( 'NONE', #650, 1000.000000000000000 ) ;
#21970 = DIRECTION ( 'NONE',  ( -1.000000000000000000, 0.000000000000000000, 0.000000000000000000 ) ) ;
#21971 = CARTESIAN_POINT ( 'NONE',  ( 8.090517219592001652, 5.342170561818999630, 8.432311822615000452 ) ) ;
#21973 = LINE ( 'NONE', #314, #57752 ) ;
#21972 = CARTESIAN_POINT ( 'NONE',  ( 9.758079719591000512, 4.905765359186999852, -8.776126235875999271 ) ) ;
#21974 = DIRECTION ( 'NONE',  ( 0.000000000000000000, 0.7158784314710769925, 0.6982249432342778617 ) ) ;
#21975 = ORIENTED_EDGE ( 'NONE', *, *, #54835, .F. ) ;
#21976 = CARTESIAN_POINT ( 'NONE',  ( 9.667078842372998082, 4.541623431405000133, 5.824038024834000460 ) ) ;
#21977 = AXIS2_PLACEMENT_3D ( 'NONE', #16152, #1114, #49343 ) ;
#21978 = CARTESIAN_POINT ( 'NONE',  ( 17.94133460182555950, -1.899620958390729086, -13.87053073593715524 ) ) ;
#21979 = CARTESIAN_POINT ( 'NONE',  ( 10.42795525820099911, 3.905250696375530239, 8.498986197235801399 ) ) ;
#21980 = CARTESIAN_POINT ( 'NONE',  ( 10.79499900793999956, -3.503951165873000040, 6.168577387731000172 ) ) ;
#21981 = CARTESIAN_POINT ( 'NONE',  ( 7.962144353208000069, -4.874569256861000177, 6.119503992241999590 ) ) ;
#21982 = ORIENTED_EDGE ( 'NONE', *, *, #30558, .F. ) ;
#21983 = CARTESIAN_POINT ( 'NONE',  ( 24.26682857475500299, 12.18233729078999872, -3.303852352193000108 ) ) ;
#21985 = CARTESIAN_POINT ( 'NONE',  ( 10.25880564679000173, -2.491773655925000330, -7.289938045981000592 ) ) ;
#21984 = CARTESIAN_POINT ( 'NONE',  ( 12.79272103475300071, -12.16747052068999935, 3.133256626080000107 ) ) ;
#21986 = CARTESIAN_POINT ( 'NONE',  ( 7.805655517671931776, -4.414680877279917759, 9.189650186020678291 ) ) ;
#21987 = CARTESIAN_POINT ( 'NONE',  ( 10.12549839661999940, -5.788806995403000144, 7.335561828691000485 ) ) ;
#21988 = CARTESIAN_POINT ( 'NONE',  ( 11.34523293495530005, -5.315205473512000012, -7.447129085684729866 ) ) ;
#21989 = VERTEX_POINT ( 'NONE', #62622 ) ;
#21990 = CARTESIAN_POINT ( 'NONE',  ( 25.12925491921549082, -11.33917288839387894, -3.290749069845217978 ) ) ;
#21991 = CARTESIAN_POINT ( 'NONE',  ( 10.73103300763300005, -3.307558760216100069, 6.773725604892799623 ) ) ;
#21992 = CARTESIAN_POINT ( 'NONE',  ( 10.76426088462129904, 4.002719309691810778, 8.778009775371000245 ) ) ;
#21993 = ORIENTED_EDGE ( 'NONE', *, *, #224, .F. ) ;
#21994 = EDGE_CURVE ( 'NONE', #59240, #56220, #49006, .T. ) ;
#21995 = EDGE_CURVE ( 'NONE', #63587, #17060, #29139, .T. ) ;
#21996 = CARTESIAN_POINT ( 'NONE',  ( 9.708354719591000048, 5.481267232667000222, -8.005061172455999241 ) ) ;
#21997 = EDGE_CURVE ( 'NONE', #49573, #25777, #27338, .T. ) ;
#21998 = CARTESIAN_POINT ( 'NONE',  ( 12.14218285455818602, 2.187615620731402810, -12.40865911928243470 ) ) ;
#21999 = CARTESIAN_POINT ( 'NONE',  ( 11.80367835872029936, -5.113555564477999305, 8.201822467543799178 ) ) ;
#22000 = CARTESIAN_POINT ( 'NONE',  ( 7.959567355576805170, 4.656486088299985227, -6.280552176398384923 ) ) ;
#22001 = CARTESIAN_POINT ( 'NONE',  ( 25.29987654162099986, -8.533547851352999203, -7.925583806936000286 ) ) ;
#22002 = EDGE_LOOP ( 'NONE', ( #36290, #8594, #7624 ) ) ;
#22003 = CARTESIAN_POINT ( 'NONE',  ( 7.790629440376999781, -3.416208448044999901, 6.162501393933999871 ) ) ;
#22004 = FACE_OUTER_BOUND ( 'NONE', #47052, .T. ) ;
#22005 = ORIENTED_EDGE ( 'NONE', *, *, #51992, .T. ) ;
#22006 = CARTESIAN_POINT ( 'NONE',  ( 12.36610530618396808, -3.052942130732431814, -12.22454734379039287 ) ) ;
#22007 = CARTESIAN_POINT ( 'NONE',  ( 10.67410807141119911, 4.046361247106100123, 6.497602131078999754 ) ) ;
#22008 = COLOUR_RGB ( '', 0.31764706, 0.68627451, 0.89019608) ;
#22009 = CARTESIAN_POINT ( 'NONE',  ( 25.29986325275000070, 2.258942858049999725, 12.29419282279000036 ) ) ;
#22010 = CARTESIAN_POINT ( 'NONE',  ( 10.86068541027999856, 2.936800615939000103, -5.173500112890999425 ) ) ;
#22011 = CARTESIAN_POINT ( 'NONE',  ( 7.875072778631000858, 5.143389081112999861, 6.784077933858997156 ) ) ;
#22012 = CARTESIAN_POINT ( 'NONE',  ( 10.96876739532000045, -2.333349849211999949, 6.524062020538999640 ) ) ;
#22013 = CARTESIAN_POINT ( 'NONE',  ( 14.03164332880499998, 9.396061154353999356, 8.198822423776999102 ) ) ;
#22014 = CARTESIAN_POINT ( 'NONE',  ( 17.98979505986429572, 0.4491390935506892612, -12.68931154995402188 ) ) ;
#22015 = VECTOR ( 'NONE', #63991, 1000.000000000000000 ) ;
#22016 = FILL_AREA_STYLE ('',( #32522 ) ) ;
#22017 = CARTESIAN_POINT ( 'NONE',  ( 11.30995122972050027, -3.547233695387300045, -6.452959986593999275 ) ) ;
#22018 = CARTESIAN_POINT ( 'NONE',  ( 9.497295280408998508, 3.734279507827999556, 8.942126004519000304 ) ) ;
#22019 = ORIENTED_EDGE ( 'NONE', *, *, #48137, .T. ) ;
#22020 = AXIS2_PLACEMENT_3D ( 'NONE', #58519, #63412, #5032 ) ;
#22021 = CARTESIAN_POINT ( 'NONE',  ( 11.59999999999999787, -4.831023649631404737, -7.997379651729213279 ) ) ;
#22022 = CARTESIAN_POINT ( 'NONE',  ( 13.69992376746900042, -12.26631831379999937, -2.532779022035999805 ) ) ;
#22023 = LINE ( 'NONE', #27632, #47039 ) ;
#22024 = CARTESIAN_POINT ( 'NONE',  ( 18.03667146358274920, 1.942392957153849409, 12.44938452643338955 ) ) ;
#22025 = FACE_OUTER_BOUND ( 'NONE', #64459, .T. ) ;
#22026 = CARTESIAN_POINT ( 'NONE',  ( -0.2999999999999999889, 0.000000000000000000, 0.000000000000000000 ) ) ;
#22027 = AXIS2_PLACEMENT_3D ( 'NONE', #66738, #50670, #7322 ) ;
#22028 = CARTESIAN_POINT ( 'NONE',  ( 10.15749563395762678, -4.774169056067385952, 7.092330352431370777 ) ) ;
#22029 = CARTESIAN_POINT ( 'NONE',  ( 5.500000000000000000, 0.000000000000000000, 0.000000000000000000 ) ) ;
#22030 = ORIENTED_EDGE ( 'NONE', *, *, #5200, .F. ) ;
#22031 = CARTESIAN_POINT ( 'NONE',  ( 12.68481529409928754, -3.190188709592561622, 12.18945115681611924 ) ) ;
#22032 = CARTESIAN_POINT ( 'NONE',  ( 9.555709346417000205, -2.968569381205999669, -7.010219103474399915 ) ) ;
#22033 = CARTESIAN_POINT ( 'NONE',  ( 11.09999999999999964, 2.700000001389000204, 5.148506132424000015 ) ) ;
#22034 = CARTESIAN_POINT ( 'NONE',  ( 23.60000000000000142, 11.85420044612000012, -3.901016762742000488 ) ) ;
#22035 = CARTESIAN_POINT ( 'NONE',  ( 10.32949413291699869, 4.912929163218899831, -7.083453279150199400 ) ) ;
#22036 = ADVANCED_FACE ( 'NONE', ( #35390 ), #1610, .F. ) ;
#22037 = CARTESIAN_POINT ( 'NONE',  ( 12.58275800453940363, -0.6847469513499573335, 12.58138041838080667 ) ) ;
#22038 = CARTESIAN_POINT ( 'NONE',  ( 9.202760841230999134, 2.542862824481000317, 7.419808961972999661 ) ) ;
#22039 = CARTESIAN_POINT ( 'NONE',  ( 17.55505043854143565, 3.199751711897561801, -12.18694338143115452 ) ) ;
#22040 = ADVANCED_FACE ( 'NONE', ( #57725 ), #12799, .T. ) ;
#22041 = CARTESIAN_POINT ( 'NONE',  ( 12.20147980349668870, 2.662577969174664272, 12.41220455913371090 ) ) ;
#22042 = LINE ( 'NONE', #58421, #51083 ) ;
#22043 = CARTESIAN_POINT ( 'NONE',  ( 10.79303032197930001, 4.663532080728800544, -6.572090902022299730 ) ) ;
#22044 = CARTESIAN_POINT ( 'NONE',  ( 12.25178171628595081, 12.07365382811639165, -3.333154641345941638 ) ) ;
#22045 = B_SPLINE_CURVE_WITH_KNOTS ( 'NONE', 3,
 ( #10479, #30782, #30443, #35689 ),
 .UNSPECIFIED., .F., .F.,
 ( 4, 4 ),
 ( 0.000000000000000000, 1.000000000000000000 ),
 .UNSPECIFIED. ) ;
#22046 = CARTESIAN_POINT ( 'NONE',  ( 10.95519834123000003, 3.860336562672999960, -6.147350406894000585 ) ) ;
#22047 = CARTESIAN_POINT ( 'NONE',  ( 12.80505043854143388, 1.760910691117811844, 12.47634535983622861 ) ) ;
#22049 = DIRECTION ( 'NONE',  ( -0.7071063294819032174, -0.7071072328909032700, 8.604668387600043697E-10 ) ) ;
#22048 = CARTESIAN_POINT ( 'NONE',  ( 8.244330716364007827, 4.955554988691996954, 6.175165069893004954 ) ) ;
#22050 = CARTESIAN_POINT ( 'NONE',  ( 25.60000000000000142, -2.258942858049999725, -12.29419282279000036 ) ) ;
#22051 = ORIENTED_EDGE ( 'NONE', *, *, #59479, .F. ) ;
#22052 = CARTESIAN_POINT ( 'NONE',  ( 12.21279950745852183, 0.1999332404310504574, 12.69788654131193795 ) ) ;
#22053 = CARTESIAN_POINT ( 'NONE',  ( 23.75089958727604156, -9.822232532321159226, -9.446477853357983179 ) ) ;
#22054 = CARTESIAN_POINT ( 'NONE',  ( 9.383148997457999130, -5.167567567567999731, 6.822293592207000934 ) ) ;
#22056 = B_SPLINE_CURVE_WITH_KNOTS ( 'NONE', 3,
 ( #52634, #9636, #57189, #36911 ),
 .UNSPECIFIED., .F., .F.,
 ( 4, 4 ),
 ( 0.000000000000000000, 1.000000000000000000 ),
 .UNSPECIFIED. ) ;
#22055 = CARTESIAN_POINT ( 'NONE',  ( 17.60408629073138087, 3.199716927301896163, -12.18695251432576931 ) ) ;
#22058 = CARTESIAN_POINT ( 'NONE',  ( 12.10810820711264846, -2.719264802799585823, 13.73338027651840321 ) ) ;
#22057 = VECTOR ( 'NONE', #30930, 1000.000000000000000 ) ;
#22059 = CARTESIAN_POINT ( 'NONE',  ( 11.30000000000000071, 11.91995148090331291, 1.454135501518458273 ) ) ;
#22060 = CARTESIAN_POINT ( 'NONE',  ( 11.00000000000000000, 2.799999999999999822, 5.865766984179000332 ) ) ;
#22061 = ORIENTED_EDGE ( 'NONE', *, *, #40787, .T. ) ;
#22062 = FACE_OUTER_BOUND ( 'NONE', #54905, .T. ) ;
#22063 = CARTESIAN_POINT ( 'NONE',  ( 18.22958240947727049, -10.92137759501516747, 4.055351289594743669 ) ) ;
#22064 = CONICAL_SURFACE ( 'NONE', #11999, 1.599998535647999987, 0.7853971506429492377 ) ;
#22065 = CARTESIAN_POINT ( 'NONE',  ( 9.762850396985012225, -2.920672817053836745, -8.329416270159347491 ) ) ;
#22066 = CARTESIAN_POINT ( 'NONE',  ( 11.23724174883999893, -4.024531238983009906, 6.608211443991299561 ) ) ;
#22067 = CARTESIAN_POINT ( 'NONE',  ( 18.22510524369412366, -11.54189923439562016, 4.316434404174353645 ) ) ;
#22068 = CARTESIAN_POINT ( 'NONE',  ( 9.620327454391748745, -2.808826379911543825, 7.911210609455967102 ) ) ;
#22069 = CARTESIAN_POINT ( 'NONE',  ( 11.09672200990539892, 3.182132064022000328, 7.785290430335599865 ) ) ;
#22070 = EDGE_CURVE ( 'NONE', #15028, #19773, #63234, .T. ) ;
#22071 = B_SPLINE_CURVE_WITH_KNOTS ( 'NONE', 3,
 ( #18592, #34679, #7056, #28391 ),
 .UNSPECIFIED., .F., .F.,
 ( 4, 4 ),
 ( 0.000000000000000000, 1.000000000000000000 ),
 .UNSPECIFIED. ) ;
#22072 = VECTOR ( 'NONE', #26075, 1000.000000000000227 ) ;
#22073 = CARTESIAN_POINT ( 'NONE',  ( 10.81021345716900051, -3.363461959113699606, 6.921280946186199934 ) ) ;
#22074 = CARTESIAN_POINT ( 'NONE',  ( 10.52384314678999999, -5.441919393629000012, -7.989634081859001036 ) ) ;
#22075 = CARTESIAN_POINT ( 'NONE',  ( 10.31021345716899873, -3.363461959113699606, -8.078719053813800954 ) ) ;
#22076 = B_SPLINE_SURFACE_WITH_KNOTS ( 'NONE', 3, 3, ( 
 ( #37654, #58986, #32422, #53737 ),
 ( #60365, #56495, #28561, #45328 ),
 ( #7918, #13175, #66638, #55121 ),
 ( #24683, #65940, #66288, #18413 ),
 ( #8258, #3006, #61056, #39047 ) ),
 .UNSPECIFIED., .F., .F., .F.,
 ( 4, 1, 4 ),
 ( 4, 4 ),
 ( 0.4073867043412000011, 0.4166666666666999919, 0.4317812135810999985 ),
 ( -0.1884351840153000168, 1.188534893118999847 ),
 .UNSPECIFIED. ) ;
#22077 = EDGE_CURVE ( 'NONE', #4993, #56617, #53217, .T. ) ;
#22078 = CARTESIAN_POINT ( 'NONE',  ( 11.09999999999999964, -5.350000000000000533, -7.500000000000000000 ) ) ;
#22079 = ADVANCED_FACE ( 'NONE', ( #11131 ), #38736, .T. ) ;
#22080 = CARTESIAN_POINT ( 'NONE',  ( 23.91316333055113574, 9.510235985825241656, -9.347881497660901928 ) ) ;
#22081 = CARTESIAN_POINT ( 'NONE',  ( 11.00000000000000000, 3.031410575668799900, -7.174999999999999822 ) ) ;
#22082 = ORIENTED_EDGE ( 'NONE', *, *, #18147, .F. ) ;
#22083 = CARTESIAN_POINT ( 'NONE',  ( 9.640910841231999484, 2.212639797530000063, -6.855876382544999537 ) ) ;
#22084 = CARTESIAN_POINT ( 'NONE',  ( 11.44487616594229884, -4.303437140848100029, 8.456491899811199531 ) ) ;
#22085 = VERTEX_POINT ( 'NONE', #54816 ) ;
#22086 = CARTESIAN_POINT ( 'NONE',  ( 18.04669395734980597, -2.113974215446797089, 13.74779306078356278 ) ) ;
#22087 = CARTESIAN_POINT ( 'NONE',  ( 10.98995257254739855, -5.095356924909000718, -7.818564472783199548 ) ) ;
#22088 = ORIENTED_EDGE ( 'NONE', *, *, #67079, .T. ) ;
#22089 = CARTESIAN_POINT ( 'NONE',  ( 10.44125056272499918, 5.033400911533000510, 7.484684486284700178 ) ) ;
#22090 = CARTESIAN_POINT ( 'NONE',  ( 5.938392933388340289, -0.2293779303045812012, -1.109941115710884274 ) ) ;
#22091 = CARTESIAN_POINT ( 'NONE',  ( 24.22569643261628869, 3.306137007861563060, -12.33866433766620929 ) ) ;
#22092 = CARTESIAN_POINT ( 'NONE',  ( 18.12922381500399993, -3.157787539580000136, 11.36563583066999961 ) ) ;
#22093 = CARTESIAN_POINT ( 'NONE',  ( 5.000000000000000000, 0.000000000000000000, 0.000000000000000000 ) ) ;
#22094 = CARTESIAN_POINT ( 'NONE',  ( 12.19608251853991909, -0.1421750971574143596, -13.89904149565844627 ) ) ;
#22095 = CARTESIAN_POINT ( 'NONE',  ( 7.200276434330572961, 0.06778569668683269434, 1.141021389174379230 ) ) ;
#22096 = CARTESIAN_POINT ( 'NONE',  ( 10.70780617489000086, -5.157482071823000780, -6.267811103859000532 ) ) ;
#22097 = CARTESIAN_POINT ( 'NONE',  ( 13.46087891924500113, 11.63300053112000043, 2.447944685581000090 ) ) ;
#22098 = ORIENTED_EDGE ( 'NONE', *, *, #23580, .T. ) ;
#22099 = VECTOR ( 'NONE', #41540, 1000.000000000000000 ) ;
#22100 = CARTESIAN_POINT ( 'NONE',  ( 9.517835841233001304, 4.883347899767999323, -6.417062834774999835 ) ) ;
#22101 = ORIENTED_EDGE ( 'NONE', *, *, #65898, .F. ) ;
#22102 = EDGE_CURVE ( 'NONE', #30666, #7406, #34042, .T. ) ;
#22103 = CARTESIAN_POINT ( 'NONE',  ( 10.87309687351627652, 2.782534154164606921, -7.172815144550898303 ) ) ;
#22104 = ORIENTED_EDGE ( 'NONE', *, *, #58166, .T. ) ;
#22105 = CARTESIAN_POINT ( 'NONE',  ( 11.53144129764059400, -11.54570453160568810, -1.556370871282598101 ) ) ;
#22106 = LINE ( 'NONE', #23147, #55080 ) ;
#22107 = VECTOR ( 'NONE', #14348, 1000.000000000000000 ) ;
#22108 = CARTESIAN_POINT ( 'NONE',  ( 24.74122194148825216, -8.638774282505121249, 8.580579725866343210 ) ) ;
#22109 = CARTESIAN_POINT ( 'NONE',  ( 18.21034928235495087, 11.77436611584341009, -3.633175583793197827 ) ) ;
#22110 = DIRECTION ( 'NONE',  ( 0.000000000000000000, 0.000000000000000000, 1.000000000000000000 ) ) ;
#22111 = LINE ( 'NONE', #57536, #63475 ) ;
#22112 = AXIS2_PLACEMENT_3D ( 'NONE', #32297, #20759, #26005 ) ;
#22113 = CARTESIAN_POINT ( 'NONE',  ( 7.849701421142106561, 2.923599143255341204, -6.630674260272470200 ) ) ;
#22114 = CARTESIAN_POINT ( 'NONE',  ( 12.76382393867145737, 0.6239806250735583371, 13.88114166035889241 ) ) ;
#22115 = ORIENTED_EDGE ( 'NONE', *, *, #26753, .F. ) ;
#22116 = CARTESIAN_POINT ( 'NONE',  ( 6.594228317542000006, 5.278582711742999756, -7.933273873238999130 ) ) ;
#22117 = CARTESIAN_POINT ( 'NONE',  ( 18.05092722032200214, 11.89802509695999966, -3.395950604129000183 ) ) ;
#22118 = CARTESIAN_POINT ( 'NONE',  ( 10.18940772478662637, 3.446387339840331965, 6.822471183635139269 ) ) ;
#22119 = VECTOR ( 'NONE', #62663, 1000.000000000000000 ) ;
#22120 = CARTESIAN_POINT ( 'NONE',  ( 4.608031265421999478, -0.9445219429904000430, 1.142243179664999886 ) ) ;
#22121 = CARTESIAN_POINT ( 'NONE',  ( 12.62607976188021119, -11.85836615252176074, 3.313854784738198500 ) ) ;
#22122 = EDGE_CURVE ( 'NONE', #8436, #67604, #5655, .T. ) ;
#22123 = CARTESIAN_POINT ( 'NONE',  ( 18.06944243593800081, -3.222040310929999762, 11.85748006108999952 ) ) ;
#22124 = CARTESIAN_POINT ( 'NONE',  ( 10.15786958814999963, -4.213496663054999480, -5.822956951053000374 ) ) ;
#22125 = EDGE_LOOP ( 'NONE', ( #21207, #42051, #10952, #22101, #16515, #38165, #38887, #33702, #61648, #43611, #15392, #17145, #56795, #29806, #194, #59180, #2577, #8867, #47030, #58383, #877, #41778, #50921, #53295, #67403 ) ) ;
#22126 = CARTESIAN_POINT ( 'NONE',  ( 13.49980696793000057, 9.514462421839999351, 7.834836582454001608 ) ) ;
#22127 = AXIS2_PLACEMENT_3D ( 'NONE', #61822, #40168, #13602 ) ;
#22128 = FACE_OUTER_BOUND ( 'NONE', #14874, .T. ) ;
#22129 = EDGE_CURVE ( 'NONE', #35108, #44937, #65987, .T. ) ;
#22130 = CARTESIAN_POINT ( 'NONE',  ( 10.90000000000000036, -2.899999999999999911, 6.414037451299000381 ) ) ;
#22131 = CARTESIAN_POINT ( 'NONE',  ( 21.60000000000000142, 0.000000000000000000, 0.000000000000000000 ) ) ;
#22132 = CARTESIAN_POINT ( 'NONE',  ( 11.85979573085659844, 4.840012015667699785, -7.645349278262099979 ) ) ;
#22133 = DIRECTION ( 'NONE',  ( 0.000000000000000000, 1.000000000000000000, 0.000000000000000000 ) ) ;
#22134 = CARTESIAN_POINT ( 'NONE',  ( 11.06456920625009843, 4.037149028919880145, -6.467161360063999886 ) ) ;
#22135 = CARTESIAN_POINT ( 'NONE',  ( 10.01459632033899894, 3.070047649444500149, -7.120485934352199564 ) ) ;
#22137 = CARTESIAN_POINT ( 'NONE',  ( 8.413394984202977156, 5.085467435940341119, -6.452616802181529110 ) ) ;
#22136 = CARTESIAN_POINT ( 'NONE',  ( 10.73557120343299864, -4.042028078047379402, 6.634008278083699750 ) ) ;
#22138 = B_SPLINE_CURVE_WITH_KNOTS ( 'NONE', 3,
 ( #44041, #10832, #17466, #65346 ),
 .UNSPECIFIED., .F., .F.,
 ( 4, 4 ),
 ( 0.000000000000000000, 1.000000000000000000 ),
 .UNSPECIFIED. ) ;
#22139 = CARTESIAN_POINT ( 'NONE',  ( 11.09999999999999964, 3.640000000000000124, -5.000000000000000000 ) ) ;
#22140 = ORIENTED_EDGE ( 'NONE', *, *, #49385, .T. ) ;
#22141 = CARTESIAN_POINT ( 'NONE',  ( 11.18923293495519822, 2.967327562101000016, 7.541513160549049744 ) ) ;
#22142 = CARTESIAN_POINT ( 'NONE',  ( 9.194602547868999665, -5.157768569202000108, 8.637845986715998237 ) ) ;
#22143 = CARTESIAN_POINT ( 'NONE',  ( 9.809000818239997699, 2.989704013253000614, 6.967988282883199602 ) ) ;
#22144 = CARTESIAN_POINT ( 'NONE',  ( 5.619513196215851991, -12.94695275183270589, -2.446394349796571444 ) ) ;
#22145 = B_SPLINE_CURVE_WITH_KNOTS ( 'NONE', 3,
 ( #27195, #68103, #53418, #32101, #68792, #69144, #41547, #52376, #4472, #62857 ),
 .UNSPECIFIED., .F., .F.,
 ( 4, 2, 2, 2, 4 ),
 ( 0.000000000000000000, 0.2500000000000000000, 0.5000000000000000000, 0.7500000000000000000, 1.000000000000000000 ),
 .UNSPECIFIED. ) ;
#22146 = CARTESIAN_POINT ( 'NONE',  ( 10.00638553269999953, -5.119272496996000399, 8.420388242270998802 ) ) ;
#22147 = FACE_BOUND ( 'NONE', #49823, .T. ) ;
#22148 = CARTESIAN_POINT ( 'NONE',  ( 7.000000000000000000, 2.200000000000000178, 0.000000000000000000 ) ) ;
#22149 = CARTESIAN_POINT ( 'NONE',  ( 8.849455549952999434, -3.218304396998100003, -6.869290649434700136 ) ) ;
#22150 = CARTESIAN_POINT ( 'NONE',  ( 6.635989938375000285, -0.06619345247263999643, 1.320670790275000117 ) ) ;
#22151 = CARTESIAN_POINT ( 'NONE',  ( 10.92760663304248325, -3.352948950021445995, 8.087719785218890678 ) ) ;
#22152 = CARTESIAN_POINT ( 'NONE',  ( 24.50399615158200106, -3.502219942208999903, 12.23695409027999936 ) ) ;
#22153 = CARTESIAN_POINT ( 'NONE',  ( 12.76382339226414864, 0.6237239846186464209, -12.67937377942301502 ) ) ;
#22154 = FACE_OUTER_BOUND ( 'NONE', #23030, .T. ) ;
#22155 = CARTESIAN_POINT ( 'NONE',  ( 7.307500000000000107, 0.2500000000000000000, -3.149999999999999911 ) ) ;
#22156 = CARTESIAN_POINT ( 'NONE',  ( 25.47111508646500155, -8.417200813839000872, 7.979926646001998414 ) ) ;
#22157 = FACE_OUTER_BOUND ( 'NONE', #34578, .T. ) ;
#22158 = VERTEX_POINT ( 'NONE', #32465 ) ;
#22159 = CARTESIAN_POINT ( 'NONE',  ( 13.50000000000000178, -11.75776087185402474, -2.440894935388740361 ) ) ;
#22160 = EDGE_CURVE ( 'NONE', #65620, #47736, #46547, .T. ) ;
#22161 = PRODUCT_CONTEXT ( 'NONE', #40042, 'mechanical' ) ;
#22162 = EDGE_CURVE ( 'NONE', #51068, #55845, #54120, .T. ) ;
#22163 = CARTESIAN_POINT ( 'NONE',  ( 11.14767835872009982, -4.874341053673500568, -6.948943352864199952 ) ) ;
#22164 = DIRECTION ( 'NONE',  ( 1.000000000000000000, 0.000000000000000000, 0.000000000000000000 ) ) ;
#22165 = CARTESIAN_POINT ( 'NONE',  ( 10.55226354018249957, -2.907767014557177898, 6.870476274536374994 ) ) ;
#22166 = CARTESIAN_POINT ( 'NONE',  ( 7.000000000000000000, 10.69544759345840745, 3.757555162259658132 ) ) ;
#22167 = CIRCLE ( 'NONE', #21034, 5.000000000000000000 ) ;
#22168 = CARTESIAN_POINT ( 'NONE',  ( 13.08701341325400236, 12.43401476831999908, 1.800486563913999971 ) ) ;
#22169 = ORIENTED_EDGE ( 'NONE', *, *, #32749, .T. ) ;
#22170 = FACE_OUTER_BOUND ( 'NONE', #53723, .T. ) ;
#22171 = FACE_OUTER_BOUND ( 'NONE', #54599, .T. ) ;
#22172 = ORIENTED_EDGE ( 'NONE', *, *, #42774, .T. ) ;
#22173 = CARTESIAN_POINT ( 'NONE',  ( 8.200000998245998929, 0.000000000000000000, 0.000000000000000000 ) ) ;
#22174 = CARTESIAN_POINT ( 'NONE',  ( 24.72251023531952541, 8.647827846133015584, -8.596833533768670321 ) ) ;
#22175 = CARTESIAN_POINT ( 'NONE',  ( 9.559179719593000613, 4.038835765825999680, -5.935509327774999733 ) ) ;
#22176 = EDGE_LOOP ( 'NONE', ( #39673, #41561, #36810, #10140 ) ) ;
#22177 = CARTESIAN_POINT ( 'NONE',  ( 23.65871306847106936, -13.20934029255680642, 3.970304306148825013 ) ) ;
#22178 = CARTESIAN_POINT ( 'NONE',  ( 11.51145123989532948, -3.394760891061399999, -8.668865425277999748 ) ) ;
#22179 = CARTESIAN_POINT ( 'NONE',  ( 7.672245280404999868, 4.523949137149999800, -5.848703038986000635 ) ) ;
#22180 = CARTESIAN_POINT ( 'NONE',  ( 10.52314899745999988, -5.167567567567999731, -6.822293592207000934 ) ) ;
#22181 = CARTESIAN_POINT ( 'NONE',  ( 7.188051286789615801, 4.829459561370207155, -8.579151395879588193 ) ) ;
#22182 = ORIENTED_EDGE ( 'NONE', *, *, #9966, .F. ) ;
#22183 = CARTESIAN_POINT ( 'NONE',  ( 10.87522165821000009, -4.831071966430999787, 6.312786525516999703 ) ) ;
#22184 = CARTESIAN_POINT ( 'NONE',  ( 25.52469358993199933, 11.20852883979999959, -3.138567732544999878 ) ) ;
#22186 =( NAMED_UNIT ( * ) PLANE_ANGLE_UNIT ( ) SI_UNIT ( $, .RADIAN. ) );
#22185 = B_SPLINE_CURVE_WITH_KNOTS ( 'NONE', 3,
 ( #56051, #23547, #45908, #23894, #17970, #67220, #12373, #49776, #13755, #50464 ),
 .UNSPECIFIED., .F., .F.,
 ( 4, 2, 2, 2, 4 ),
 ( 0.000000000000000000, 0.1250000000000000000, 0.2500000000000000000, 0.3750000000000000000, 0.5000000000000000000 ),
 .UNSPECIFIED. ) ;
#22187 = ORIENTED_EDGE ( 'NONE', *, *, #8797, .F. ) ;
#22188 = EDGE_CURVE ( 'NONE', #23757, #52126, #25062, .T. ) ;
#22189 = AXIS2_PLACEMENT_3D ( 'NONE', #13542, #24709, #45352 ) ;
#22190 = CARTESIAN_POINT ( 'NONE',  ( 8.905196823546312146, 4.608202637908532573, -8.372486832488423403 ) ) ;
#22191 = CARTESIAN_POINT ( 'NONE',  ( 10.27366694038000006, -3.065543393453000309, -8.487918777453998587 ) ) ;
#22192 = ORIENTED_EDGE ( 'NONE', *, *, #26043, .T. ) ;
#22193 = CARTESIAN_POINT ( 'NONE',  ( 10.16455864497999961, 4.898932057185599653, 6.795973491698399371 ) ) ;
#22194 = CARTESIAN_POINT ( 'NONE',  ( 18.18005043824477696, 1.062919176435095297E-10, -13.90000000153291637 ) ) ;
#22195 = EDGE_CURVE ( 'NONE', #7548, #41308, #34726, .T. ) ;
#22196 = CARTESIAN_POINT ( 'NONE',  ( 5.263797794415999931, 1.304926942633999998, 0.5509913562316999247 ) ) ;
#22197 = CARTESIAN_POINT ( 'NONE',  ( 8.024543455198998032, 4.549053763738999834, -6.246376295157002545 ) ) ;
#22198 = CARTESIAN_POINT ( 'NONE',  ( 16.18326532032400067, 3.458591647041000083, 11.88419159288000060 ) ) ;
#22199 = CARTESIAN_POINT ( 'NONE',  ( 10.54885180107587495, 4.021057955977791920, 8.964620661115885625 ) ) ;
#22200 = CARTESIAN_POINT ( 'NONE',  ( 9.327427652207148867, -3.945165805631096312, 9.238792170091185696 ) ) ;
#22201 = ORIENTED_EDGE ( 'NONE', *, *, #40106, .F. ) ;
#22202 = CARTESIAN_POINT ( 'NONE',  ( 8.245455708338628398, -4.975154674665282606, 6.309433999826808304 ) ) ;
#22203 = CARTESIAN_POINT ( 'NONE',  ( 10.45625165877000029, 3.661871102473000406, -9.317475234260999883 ) ) ;
#22204 = CARTESIAN_POINT ( 'NONE',  ( 18.50055606950828135, -11.89493552632996476, 3.924423580214191798 ) ) ;
#22205 = CARTESIAN_POINT ( 'NONE',  ( 12.24392764853879889, 2.776000094621842607, -13.61105252602849092 ) ) ;
#22206 = DIRECTION ( 'NONE',  ( 0.000000000000000000, -0.1807154286440006141, 0.9835354258236025382 ) ) ;
#22207 = CARTESIAN_POINT ( 'NONE',  ( 11.27109998545999936, -5.469594811916000054, 8.504700858852999090 ) ) ;
#22208 = CARTESIAN_POINT ( 'NONE',  ( 17.59627693841142460, -0.6239806250735587811, 13.88114166035889241 ) ) ;
#22209 = CARTESIAN_POINT ( 'NONE',  ( 24.95780670450700001, -3.530138962360999777, 11.86562507170999936 ) ) ;
#22210 = EDGE_LOOP ( 'NONE', ( #9803, #50397, #59429, #48239 ) ) ;
#22211 = ORIENTED_EDGE ( 'NONE', *, *, #37057, .T. ) ;
#22212 = CONICAL_SURFACE ( 'NONE', #54456, 1.899997304679999610, 0.7853981633972997312 ) ;
#22213 = CARTESIAN_POINT ( 'NONE',  ( 10.85737917744000036, 2.754548910086000113, 8.976376585747001258 ) ) ;
#22214 = EDGE_CURVE ( 'NONE', #7968, #25005, #32468, .T. ) ;
#22215 = CARTESIAN_POINT ( 'NONE',  ( 12.18394749351799966, 0.08111026478887338464, 13.89976203980570979 ) ) ;
#22216 = CARTESIAN_POINT ( 'NONE',  ( 12.29580333558936900, -0.3624858755954508682, -13.89364165472173873 ) ) ;
#22217 = CARTESIAN_POINT ( 'NONE',  ( 9.447848023450999833, -5.447470167531999863, 7.431328114251999573 ) ) ;
#22218 = CARTESIAN_POINT ( 'NONE',  ( 17.90980351674997451, -0.5146449798727437130, -13.88717540043696808 ) ) ;
#22219 = CARTESIAN_POINT ( 'NONE',  ( 7.833769353207999941, -2.583664704444999849, 6.684748541034000624 ) ) ;
#22220 = LINE ( 'NONE', #2284, #41585 ) ;
#22222 = DIRECTION ( 'NONE',  ( 0.000000000000000000, 1.000000000000000000, 0.000000000000000000 ) ) ;
#22221 = CARTESIAN_POINT ( 'NONE',  ( 9.855088727410999283, -5.274736981944999847, 7.393088754863899936 ) ) ;
#22223 = CARTESIAN_POINT ( 'NONE',  ( 10.49349279008999858, 3.667611644732699627, -8.734031750754999379 ) ) ;
#22224 = CARTESIAN_POINT ( 'NONE',  ( 24.36453968238300050, -8.917854847619999248, -9.043337665091998545 ) ) ;
#22225 = CARTESIAN_POINT ( 'NONE',  ( 7.900104261408000816, 3.351183067932000270, -6.316134894229000096 ) ) ;
#22226 = CARTESIAN_POINT ( 'NONE',  ( 18.12848705786300130, -0.2487950381773059993, 12.69672507751632118 ) ) ;
#22227 = B_SPLINE_SURFACE_WITH_KNOTS ( 'NONE', 3, 3, ( 
 ( #64339, #5965, #32893, #27652, #1421, #22736, #48973, #33241, #5622, #44085, #21362, #42692, #54562, #64000, #16118, #37444, #58765, #48277, #61212, #50722, #18565, #35676, #8758, #13665, #24147, #30099, #40233, #46508, #29758, #45477, #40912, #45134, #3164, #7724, #2475 ),
 ( #19591, #45817, #51403, #56309, #51063, #29065, #41256, #30431, #56989, #62234, #66445, #66794, #29414, #2816, #18908, #61549, #51741, #55964, #39892, #24835, #13329, #23801, #62571, #14351, #34994, #34653, #46162, #25173, #36009, #8070, #67811, #67466, #3499, #19935, #8415 ),
 ( #14008, #14690, #50376, #67128, #9092, #24494, #3835, #19238, #35337, #40565, #61892, #56651, #4525, #5562, #32153, #52777, #15718, #10127, #41599, #53121, #41943, #26904, #42302, #36353, #323, #9426, #64281, #53469, #26213, #63600, #63251, #21639, #15376, #57668, #10463 ),
 ( #31805, #62908, #15029, #47194, #63942, #9774, #48216, #58025, #68495, #47541, #21302, #5223, #42974, #16398, #58361, #57325, #30769, #36705, #31459, #58706, #52079, #4183, #20964, #68846, #20619, #69190, #4872, #31125, #52428, #10809, #26559, #25861, #37046, #47886, #16053 ) ),
 .UNSPECIFIED., .F., .F., .F.,
 ( 4, 4 ),
 ( 4, 1, 1, 1, 1, 1, 1, 1, 1, 1, 1, 1, 1, 1, 1, 1, 1, 1, 1, 1, 1, 1, 1, 1, 1, 1, 1, 1, 1, 1, 1, 1, 4 ),
 ( -0.1039370721279000015, 1.103937072127999963 ),
 ( -0.02000000000000000042, 0.01250000000000000069, 0.04499999999999999833, 0.07749999999999999944, 0.1100000000000000006, 0.1424999999999999878, 0.1749999999999999889, 0.2074999999999999900, 0.2399999999999999911, 0.2725000000000000200, 0.3049999999999999933, 0.3375000000000000222, 0.3699999999999999956, 0.4025000000000000244, 0.4349999999999999978, 0.4675000000000000266, 0.5000000000000000000, 0.5324999999999999734, 0.5649999999999999467, 0.5975000000000000311, 0.6300000000000000044, 0.6624999999999999778, 0.6949999999999999512, 0.7275000000000000355, 0.7600000000000000089, 0.7924999999999999822, 0.8249999999999999556, 0.8575000000000000400, 0.8900000000000000133, 0.9224999999999999867, 0.9549999999999999600, 0.9875000000000000444, 1.020000000000000018 ),
 .UNSPECIFIED. ) ;
#22228 = CARTESIAN_POINT ( 'NONE',  ( 10.34286678428582640, -2.713835889960352965, -7.027064066396518704 ) ) ;
#22229 = CARTESIAN_POINT ( 'NONE',  ( 11.80000000000000071, 50.50083396221999976, 8.814205526695999993 ) ) ;
#22230 = ORIENTED_EDGE ( 'NONE', *, *, #8235, .T. ) ;
#22231 = CARTESIAN_POINT ( 'NONE',  ( 23.73952313311524875, -3.508704810469513546, 13.37374458792384679 ) ) ;
#22232 = DIRECTION ( 'NONE',  ( 1.000000000000000000, 0.000000000000000000, 0.000000000000000000 ) ) ;
#22233 = FACE_OUTER_BOUND ( 'NONE', #31646, .T. ) ;
#22234 = CARTESIAN_POINT ( 'NONE',  ( 13.50018479229300006, -11.60142623882999935, -2.415183939829000259 ) ) ;
#22235 = B_SPLINE_CURVE_WITH_KNOTS ( 'NONE', 3,
 ( #21716, #43052, #11921, #65402 ),
 .UNSPECIFIED., .F., .F.,
 ( 4, 4 ),
 ( 0.000000000000000000, 1.000000000000000000 ),
 .UNSPECIFIED. ) ;
#22236 = CARTESIAN_POINT ( 'NONE',  ( 19.39373726536100051, -11.26964301940000013, 0.000000000000000000 ) ) ;
#22237 = CARTESIAN_POINT ( 'NONE',  ( 10.48280513895999988, 4.903310631086600146, 8.002155910165599906 ) ) ;
#22238 = CARTESIAN_POINT ( 'NONE',  ( 2.886157687091000401, -0.7705521370824999217, -3.678943691011999917 ) ) ;
#22239 = ORIENTED_EDGE ( 'NONE', *, *, #42496, .F. ) ;
#22240 = CARTESIAN_POINT ( 'NONE',  ( 12.19582542658656266, -0.3901114995139884911, -12.59396323349877989 ) ) ;
#22241 = DIRECTION ( 'NONE',  ( -1.000000000000000000, 0.000000000000000000, 0.000000000000000000 ) ) ;
#22242 = FACE_OUTER_BOUND ( 'NONE', #31471, .T. ) ;
#22243 = CARTESIAN_POINT ( 'NONE',  ( 7.110997236279914091, -3.823158075381482668, 8.850159282918328429 ) ) ;
#22244 = CARTESIAN_POINT ( 'NONE',  ( 7.058509992104999853, 4.314040636970999820, 8.819134391732999845 ) ) ;
#22245 = VERTEX_POINT ( 'NONE', #46049 ) ;
#22246 = CARTESIAN_POINT ( 'NONE',  ( 6.032487603146999611, -1.512468930016000135, 0.5654847974100999375 ) ) ;
#22247 = ADVANCED_FACE ( 'NONE', ( #51630 ), #56538, .T. ) ;
#22248 = EDGE_CURVE ( 'NONE', #47790, #38520, #44075, .T. ) ;
#22249 = CARTESIAN_POINT ( 'NONE',  ( 8.154729719586999437, 2.268410489563000176, -7.553872882963998947 ) ) ;
#22251 = CARTESIAN_POINT ( 'NONE',  ( 11.50000196593843071, 12.42140789277164714, 1.609557074791108988 ) ) ;
#22250 = CARTESIAN_POINT ( 'NONE',  ( 8.449546238384577634, -2.260405780409438403, 7.505456740821800032 ) ) ;
#22252 = CARTESIAN_POINT ( 'NONE',  ( 9.700038493598999167, -3.074215132699300135, 8.382783533462799141 ) ) ;
#22253 = ORIENTED_EDGE ( 'NONE', *, *, #20203, .T. ) ;
#22254 = CARTESIAN_POINT ( 'NONE',  ( 17.55505043854147118, -1.875000000000000000, -13.78627172894481667 ) ) ;
#22255 = CARTESIAN_POINT ( 'NONE',  ( 6.105026506350000659, -1.500000000000000000, 0.000000000000000000 ) ) ;
#22256 = ORIENTED_EDGE ( 'NONE', *, *, #65832, .T. ) ;
#22257 = CARTESIAN_POINT ( 'NONE',  ( 11.09999999999999787, 3.168181714683488970, -8.858103688129558506 ) ) ;
#22258 = CARTESIAN_POINT ( 'NONE',  ( 24.89078534325364345, -8.576153783899114202, -8.441099479427823127 ) ) ;
#22259 = CARTESIAN_POINT ( 'NONE',  ( 18.17981516808187337, 0.01996689158402835743, -13.89998575767903155 ) ) ;
#22260 = VERTEX_POINT ( 'NONE', #14240 ) ;
#22261 = CARTESIAN_POINT ( 'NONE',  ( 10.53010726722364510, -2.706054758365612489, -8.716665077408118023 ) ) ;
#22262 = DIRECTION ( 'NONE',  ( 0.000000000000000000, 0.000000000000000000, -1.000000000000000000 ) ) ;
#22263 = CARTESIAN_POINT ( 'NONE',  ( 10.36325056272499978, 4.892034740700499817, -7.513220396995270001 ) ) ;
#22264 = CARTESIAN_POINT ( 'NONE',  ( 9.972537864286000087, 2.899999999999999911, -6.571291218949999902 ) ) ;
#22265 = CARTESIAN_POINT ( 'NONE',  ( 9.433148997456999751, -5.167567567567999731, 6.822293592207000934 ) ) ;
#22266 = ORIENTED_EDGE ( 'NONE', *, *, #10476, .T. ) ;
#22267 = CARTESIAN_POINT ( 'NONE',  ( 7.962142219590999659, 4.874567052833000069, 6.119507471270999588 ) ) ;
#22268 = CARTESIAN_POINT ( 'NONE',  ( 17.67418791246062071, -1.797344534875189526, 13.88414834504120421 ) ) ;
#22269 = VERTEX_POINT ( 'NONE', #24034 ) ;
#22270 = EDGE_CURVE ( 'NONE', #1201, #63146, #7611, .T. ) ;
#22271 = CARTESIAN_POINT ( 'NONE',  ( 9.854346873516666605, -5.250000000000000000, 7.336375382625534236 ) ) ;
#22272 = DIRECTION ( 'NONE',  ( -1.000000000000000000, 0.000000000000000000, 0.000000000000000000 ) ) ;
#22273 = CARTESIAN_POINT ( 'NONE',  ( 11.07071174448999962, 6.643989958501999915, -5.583274979969999663 ) ) ;
#22274 = ORIENTED_EDGE ( 'NONE', *, *, #68827, .T. ) ;
#22275 = CARTESIAN_POINT ( 'NONE',  ( 12.20003344249116317, -2.341920628070003563, -12.48700265052703884 ) ) ;
#22276 = ADVANCED_FACE ( 'NONE', ( #50951 ), #61777, .F. ) ;
#22277 = FACE_OUTER_BOUND ( 'NONE', #31385, .T. ) ;
#22278 = CARTESIAN_POINT ( 'NONE',  ( 7.839172165042807450, 5.856979424599929374, -7.474329324089589832 ) ) ;
#22279 = CYLINDRICAL_SURFACE ( 'NONE', #11849, 1.350000000000000089 ) ;
#22280 = CARTESIAN_POINT ( 'NONE',  ( 12.09815554886061761, -2.355526959511359486, -13.80042145504354778 ) ) ;
#22281 = B_SPLINE_CURVE_WITH_KNOTS ( 'NONE', 3,
 ( #19118, #51282, #51618, #25052 ),
 .UNSPECIFIED., .F., .F.,
 ( 4, 4 ),
 ( 0.000000000000000000, 1.000000000000000000 ),
 .UNSPECIFIED. ) ;
#22282 = CARTESIAN_POINT ( 'NONE',  ( 10.60026222744819790, -4.774534945026900346, -8.138001937130599828 ) ) ;
#22283 = CARTESIAN_POINT ( 'NONE',  ( 5.950859839683750430, -0.3926218265389256890, 1.460959015002472050 ) ) ;
#22284 = CARTESIAN_POINT ( 'NONE',  ( 18.06303038656661286, -1.966720487694626041, 12.44556484937419150 ) ) ;
#22285 = ORIENTED_EDGE ( 'NONE', *, *, #33055, .T. ) ;
#22286 = CARTESIAN_POINT ( 'NONE',  ( 10.55569598648999907, -2.869047858956000230, -8.173387776112500447 ) ) ;
#22287 = ORIENTED_EDGE ( 'NONE', *, *, #11789, .T. ) ;
#22288 = CIRCLE ( 'NONE', #61372, 0.6999999999999992895 ) ;
#22289 = LINE ( 'NONE', #27542, #27799 ) ;
#22290 = CARTESIAN_POINT ( 'NONE',  ( 8.798539158775000146, 5.851083642416999631, -7.072167224702999633 ) ) ;
#22291 = CARTESIAN_POINT ( 'NONE',  ( 10.24846228258000025, 4.234133568259999869, -5.660851473941000300 ) ) ;
#22292 = CARTESIAN_POINT ( 'NONE',  ( 9.675541251098000117, -4.656741678598999457, -8.653222148251000334 ) ) ;
#22293 = FACE_OUTER_BOUND ( 'NONE', #59345, .T. ) ;
#22294 = CARTESIAN_POINT ( 'NONE',  ( 23.95109860005200275, 12.88176655920999991, 3.489107522193000133 ) ) ;
#22295 = CARTESIAN_POINT ( 'NONE',  ( 18.28081516007891949, -2.296096720418743242, -12.39048987308211203 ) ) ;
#22296 = EDGE_LOOP ( 'NONE', ( #63001, #41296, #9127, #63383, #47567 ) ) ;
#22297 = CARTESIAN_POINT ( 'NONE',  ( 10.88314899746000108, -5.167567567567999731, 6.822293592207000934 ) ) ;
#22298 = CARTESIAN_POINT ( 'NONE',  ( 10.55991859298999991, 5.094266430778000121, 6.075406703384000018 ) ) ;
#22299 = DIRECTION ( 'NONE',  ( -1.000000000000000000, 0.000000000000000000, 0.000000000000000000 ) ) ;
#22300 = CARTESIAN_POINT ( 'NONE',  ( 10.85814141025499957, -3.516507310755200066, 6.638851159159999682 ) ) ;
#22301 = CARTESIAN_POINT ( 'NONE',  ( 5.407309682996999989, 12.95251760905999916, -1.915207572621000054 ) ) ;
#22302 = CARTESIAN_POINT ( 'NONE',  ( 11.14287956900000154, 10.00655548732999911, -5.859452652895000391 ) ) ;
#22303 = CARTESIAN_POINT ( 'NONE',  ( 10.14579102373339481, 5.375586255833037619, 6.376694730363436925 ) ) ;
#22304 = EDGE_CURVE ( 'NONE', #31293, #47655, #242, .T. ) ;
#22305 = CARTESIAN_POINT ( 'NONE',  ( 23.61354982155200233, -10.15571182854999854, -9.483312721863999428 ) ) ;
#22306 = CARTESIAN_POINT ( 'NONE',  ( 24.45265751162000356, -8.898665285767000555, 9.226266223847000347 ) ) ;
#22307 = CARTESIAN_POINT ( 'NONE',  ( 25.59997277611800115, 2.578802611042650509E-13, -11.19994871957399241 ) ) ;
#22308 = ORIENTED_EDGE ( 'NONE', *, *, #40265, .T. ) ;
#22309 = CARTESIAN_POINT ( 'NONE',  ( 9.716735841232001292, 3.941185585667000169, -8.896279800194999865 ) ) ;
#22310 = CARTESIAN_POINT ( 'NONE',  ( 7.127700263164999939, 0.7483242745035000310, -1.146132291880999743 ) ) ;
#22311 = B_SPLINE_CURVE_WITH_KNOTS ( 'NONE', 3,
 ( #43731, #47942, #26963, #53530 ),
 .UNSPECIFIED., .F., .F.,
 ( 4, 4 ),
 ( 0.000000000000000000, 0.1254285313929423273 ),
 .UNSPECIFIED. ) ;
#22312 = CARTESIAN_POINT ( 'NONE',  ( 18.14704975929774022, 2.701423609612693344, 13.62863833005038572 ) ) ;
#22313 = CARTESIAN_POINT ( 'NONE',  ( 10.60679199300537867, 4.691919759246326649, 4.759410728295280002 ) ) ;
#22314 = CARTESIAN_POINT ( 'NONE',  ( 11.03502897915239878, -3.672866099873000056, -8.735435061820998826 ) ) ;
#22315 = ORIENTED_EDGE ( 'NONE', *, *, #26881, .F. ) ;
#22316 = CARTESIAN_POINT ( 'NONE',  ( 10.60664092702312189, -5.179495029648551352, -8.179803431736287322 ) ) ;
#22317 = CARTESIAN_POINT ( 'NONE',  ( 9.298698341228998743, 5.159258275969999197, 9.109498396691998678 ) ) ;
#22319 = PLANE ( 'NONE',  #62204 ) ;
#22318 = CARTESIAN_POINT ( 'NONE',  ( 8.465229719592999302, 2.567871051582000241, -6.869011921437000012 ) ) ;
#22320 = CARTESIAN_POINT ( 'NONE',  ( 2.729619753586109976, 2.715085506907106705, -1.800656924566107486 ) ) ;
#22321 = VERTEX_POINT ( 'NONE', #45711 ) ;
#22322 = CARTESIAN_POINT ( 'NONE',  ( 9.889842476439000052, 4.052276433608000161, 9.260531940735001299 ) ) ;
#22323 = CARTESIAN_POINT ( 'NONE',  ( 18.26096953105667353, -2.684662952176597006, -13.74018646639511765 ) ) ;
#22324 = CARTESIAN_POINT ( 'NONE',  ( 11.38795122972049967, 4.398282450130399646, 8.421043941822800249 ) ) ;
#22325 = CARTESIAN_POINT ( 'NONE',  ( 10.07101719722999889, -4.042170815906999337, 8.920201479886998186 ) ) ;
#22326 = CYLINDRICAL_SURFACE ( 'NONE', #46649, 1.500000000000000000 ) ;
#22327 = ORIENTED_EDGE ( 'NONE', *, *, #32070, .F. ) ;
#22328 = CARTESIAN_POINT ( 'NONE',  ( 8.434258806866999691, 2.899999996372999433, -6.577564833295999946 ) ) ;
#22329 = EDGE_CURVE ( 'NONE', #3814, #66584, #11241, .T. ) ;
#22330 = EDGE_CURVE ( 'NONE', #37494, #15848, #8542, .T. ) ;
#22332 = CARTESIAN_POINT ( 'NONE',  ( 10.97819314679000158, -5.476828481365000556, -7.128717489481000591 ) ) ;
#22331 = CARTESIAN_POINT ( 'NONE',  ( 12.56257882282300109, -11.80639483233000142, 3.358960109135999961 ) ) ;
#22333 = VECTOR ( 'NONE', #62001, 1000.000000000000000 ) ;
#22334 = CARTESIAN_POINT ( 'NONE',  ( 7.778522546713435126, -4.944928104213000886, 8.960707585029377142 ) ) ;
#22335 = CARTESIAN_POINT ( 'NONE',  ( 11.08492081570999943, -3.668392767032000013, 5.558160538745999801 ) ) ;
#22336 = CARTESIAN_POINT ( 'NONE',  ( 18.50003594167399967, -2.686563651857999613, -11.33603604486000016 ) ) ;
#22337 = ORIENTED_EDGE ( 'NONE', *, *, #22873, .F. ) ;
#22338 = CARTESIAN_POINT ( 'NONE',  ( 24.76114890596840823, -11.73048710026287722, -3.191743628542212274 ) ) ;
#22339 = ADVANCED_FACE ( 'NONE', ( #66330 ), #14515, .F. ) ;
#22340 = CARTESIAN_POINT ( 'NONE',  ( 11.17410807141120088, -3.953638752893899877, 6.497602131078999754 ) ) ;
#22341 = CARTESIAN_POINT ( 'NONE',  ( 17.65158693958703751, 1.792693047823491925, 13.88475221912152158 ) ) ;
#22342 = CARTESIAN_POINT ( 'NONE',  ( 10.13662282008599824, 4.594711216567399781, 6.540749699823199315 ) ) ;
#22343 = ORIENTED_EDGE ( 'NONE', *, *, #37441, .T. ) ;
#22344 = B_SPLINE_CURVE_WITH_KNOTS ( 'NONE', 3,
 ( #55843, #8292, #61085, #7946 ),
 .UNSPECIFIED., .F., .F.,
 ( 4, 4 ),
 ( 0.000000000000000000, 1.000000000000000000 ),
 .UNSPECIFIED. ) ;
#22345 = B_SPLINE_CURVE_WITH_KNOTS ( 'NONE', 3,
 ( #710, #64316, #37765, #59090, #11192, #32531, #10505, #31844, #53845, #10169, #53161, #31498, #4913, #25903 ),
 .UNSPECIFIED., .F., .F.,
 ( 4, 2, 2, 2, 1, 1, 2, 4 ),
 ( 0.000000000000000000, 0.09969170620282293005, 0.1246146327535289089, 0.1277299985723673315, 0.1308453643912057540, 0.1370760960288826269, 0.1495375593042358453, 0.1993834124056478585 ),
 .UNSPECIFIED. ) ;
#22346 = CARTESIAN_POINT ( 'NONE',  ( 9.369139158774000720, 2.685250982074999904, -7.026194612421999608 ) ) ;
#22347 = CARTESIAN_POINT ( 'NONE',  ( 24.45387735997000078, 12.43793564427999954, -3.092859717916999873 ) ) ;
#22348 = CARTESIAN_POINT ( 'NONE',  ( 12.29441019255333600, 2.991168332544433373, -12.23980925793768648 ) ) ;
#22349 = CARTESIAN_POINT ( 'NONE',  ( 11.88678751119029897, -5.166297436425000278, 6.889827023674499173 ) ) ;
#22350 = EDGE_LOOP ( 'NONE', ( #17645, #37529, #541, #48088 ) ) ;
#22351 = CARTESIAN_POINT ( 'NONE',  ( 9.075186946668578614, 5.349648441228561424, -7.676810942292243034 ) ) ;
#22352 = DIRECTION ( 'NONE',  ( 0.000000000000000000, 1.000000000000000000, 0.000000000000000000 ) ) ;
#22353 = EDGE_LOOP ( 'NONE', ( #11593, #19757, #30804 ) ) ;
#22354 = CARTESIAN_POINT ( 'NONE',  ( 9.459504440379001622, -5.445226602819000838, 7.703375344019999460 ) ) ;
#22355 = CARTESIAN_POINT ( 'NONE',  ( 9.333766445374624965, -5.249999999999997335, -7.340348008080749054 ) ) ;
#22356 = EDGE_LOOP ( 'NONE', ( #63330, #37485, #63615, #4855 ) ) ;
#22357 = FACE_OUTER_BOUND ( 'NONE', #13480, .T. ) ;
#22358 = EDGE_CURVE ( 'NONE', #44124, #31242, #19442, .T. ) ;
#22359 = CARTESIAN_POINT ( 'NONE',  ( 11.53564291764652872, 3.004110626587600308, 7.623106493640399606 ) ) ;
#22360 = CARTESIAN_POINT ( 'NONE',  ( 23.89320776801300283, 3.226867021032998828, -11.46303308821000044 ) ) ;
#22361 = CARTESIAN_POINT ( 'NONE',  ( 10.91194337838000017, 2.977644878599000400, -4.912228107105999442 ) ) ;
#22362 = CARTESIAN_POINT ( 'NONE',  ( 17.99398900912800059, -11.43764524146999939, 4.465475029564999865 ) ) ;
#22363 = CARTESIAN_POINT ( 'NONE',  ( 7.975339216757299177, -5.350090185752664595, 7.499980949462679014 ) ) ;
#22364 = CARTESIAN_POINT ( 'NONE',  ( 7.966901574931999797, 4.609574279519000228, -6.276317554486000816 ) ) ;
#22365 = CARTESIAN_POINT ( 'NONE',  ( 17.89428234746476676, -0.5250240499537035532, -12.68539034781189301 ) ) ;
#22366 = CARTESIAN_POINT ( 'NONE',  ( 12.18102902119794351, 2.459609776898156852, -12.46092926276592827 ) ) ;
#22367 = CARTESIAN_POINT ( 'NONE',  ( 10.37457053952199892, -4.448306506338299826, -6.451042711717000167 ) ) ;
#22368 = CARTESIAN_POINT ( 'NONE',  ( 8.957392219593000249, 2.678331728353000152, 8.735281589464001684 ) ) ;
#22369 = ORIENTED_EDGE ( 'NONE', *, *, #59783, .T. ) ;
#22370 = FILL_AREA_STYLE ('',( #32529 ) ) ;
#22371 = CARTESIAN_POINT ( 'NONE',  ( 8.225195096046189036, -2.649880853682571313, 7.500010424662522546 ) ) ;
#22372 = CARTESIAN_POINT ( 'NONE',  ( 7.000000000000000000, -9.370210309074998634, 5.370210309075000410 ) ) ;
#22373 = CARTESIAN_POINT ( 'NONE',  ( 11.44730853405000204, 12.38161968051000095, 1.492087993499999987 ) ) ;
#22374 = CARTESIAN_POINT ( 'NONE',  ( 18.14595306053280410, 2.897894011715723472, 12.26224306838060407 ) ) ;
#22375 = CARTESIAN_POINT ( 'NONE',  ( 17.55505043854144276, -0.6250000000000001110, 13.88107975066923316 ) ) ;
#22376 = CARTESIAN_POINT ( 'NONE',  ( 11.01438209788000044, 8.148461013471999692, 6.594582989364000447 ) ) ;
#22377 = DIRECTION ( 'NONE',  ( 0.000000000000000000, -0.7071067811865475727, 0.7071067811865475727 ) ) ;
#22378 = FACE_OUTER_BOUND ( 'NONE', #49146, .T. ) ;
#22379 = ORIENTED_EDGE ( 'NONE', *, *, #35057, .F. ) ;
#22380 = CARTESIAN_POINT ( 'NONE',  ( 12.25024874575448308, -2.943737818075154777, 12.25130580795035051 ) ) ;
#22381 = CARTESIAN_POINT ( 'NONE',  ( 10.41488779216199845, -3.070969952137800441, -7.835030859477799758 ) ) ;
#22382 = CARTESIAN_POINT ( 'NONE',  ( 24.41555930013399944, -3.181808913646000381, -12.02251225967000003 ) ) ;
#22383 = VECTOR ( 'NONE', #9085, 1000.000000000000000 ) ;
#22384 = DIRECTION ( 'NONE',  ( 0.000000000000000000, -0.6555644356537908557, -0.7551392392836745460 ) ) ;
#22385 = B_SPLINE_SURFACE_WITH_KNOTS ( 'NONE', 3, 3, ( 
 ( #54867, #48237, #54166, #23044, #27265, #22003, #44394, #17816, #39131, #12565, #53826, #42992, #64301, #16419, #37747, #59074, #11174, #38438, #6266, #5924, #48588, #59760, #38085, #691, #43351, #64651, #59411, #11511, #27607, #48935, #1043, #22354, #43693, #17104, #14290 ),
 ( #40503, #2081, #44737, #35619, #35273, #61150, #13268, #50316, #19526, #8353, #24433, #29699, #34594, #8011, #45077, #56590, #40174, #51342, #2760, #61828, #51001, #30039, #13609, #3435, #60802, #13947, #55562, #66383, #3099, #2415, #66729, #8696, #7312, #55908, #24772 ),
 ( #23398, #23739, #28654, #39829, #49966, #46099, #67405, #45419, #45758, #29348, #50660, #66035, #34931, #61491, #40847, #62168, #24086, #18159, #39481, #12914, #34242, #18505, #56246, #67067, #7663, #18848, #29009, #19180, #15654, #52367, #15992, #56930, #31057, #26150, #9028 ),
 ( #19868, #69135, #46443, #41199, #25800, #47133, #36987, #68783, #4460, #46785, #26495, #30368, #3775, #14627, #5162, #52712, #47825, #20208, #57962, #51677, #68090, #9712, #62508, #62846, #47475, #58299, #31396, #63880, #25111, #57607, #4809, #20899, #42238, #67744, #63543 ) ),
 .UNSPECIFIED., .F., .F., .F.,
 ( 4, 4 ),
 ( 4, 1, 1, 1, 1, 1, 1, 1, 1, 1, 1, 1, 1, 1, 1, 1, 1, 1, 1, 1, 1, 1, 1, 1, 1, 1, 1, 1, 1, 1, 1, 1, 4 ),
 ( -0.1039086239011999951, 1.103908623900999864 ),
 ( -0.02000000000000000042, 0.01250000000000000069, 0.04499999999999999833, 0.07749999999999999944, 0.1100000000000000006, 0.1424999999999999878, 0.1749999999999999889, 0.2074999999999999900, 0.2399999999999999911, 0.2725000000000000200, 0.3049999999999999933, 0.3375000000000000222, 0.3699999999999999956, 0.4025000000000000244, 0.4349999999999999978, 0.4675000000000000266, 0.5000000000000000000, 0.5324999999999999734, 0.5649999999999999467, 0.5975000000000000311, 0.6300000000000000044, 0.6624999999999999778, 0.6949999999999999512, 0.7275000000000000355, 0.7600000000000000089, 0.7924999999999999822, 0.8249999999999999556, 0.8575000000000000400, 0.8900000000000000133, 0.9224999999999999867, 0.9549999999999999600, 0.9875000000000000444, 1.020000000000000018 ),
 .UNSPECIFIED. ) ;
#22386 = CARTESIAN_POINT ( 'NONE',  ( 11.67918044953561996, 5.011483761127000669, -8.027436060358800418 ) ) ;
#22387 = CARTESIAN_POINT ( 'NONE',  ( 12.08466115484542946, -0.08185661189466741927, 12.59973963693671806 ) ) ;
#22388 = ADVANCED_FACE ( 'NONE', ( #31009 ), #25773, .T. ) ;
#22389 = EDGE_CURVE ( 'NONE', #54418, #54024, #31954, .T. ) ;
#22390 = CARTESIAN_POINT ( 'NONE',  ( 7.507482780409000078, 3.501518846194999757, 9.055971388486000251 ) ) ;
#22391 = CARTESIAN_POINT ( 'NONE',  ( 8.807788144226000426, -3.909067355573210278, -8.453461841935100196 ) ) ;
#22392 = CARTESIAN_POINT ( 'NONE',  ( 12.61477885367309604, 1.785717119372573825, 12.47282100101237212 ) ) ;
#22393 = ORIENTED_EDGE ( 'NONE', *, *, #26671, .T. ) ;
#22394 = CARTESIAN_POINT ( 'NONE',  ( 4.599999999999999645, 0.000000000000000000, 0.000000000000000000 ) ) ;
#22395 = CARTESIAN_POINT ( 'NONE',  ( 10.86687616594229944, 3.655053560864600204, -6.412662853391999818 ) ) ;
#22396 = CARTESIAN_POINT ( 'NONE',  ( 17.77668021070434889, -0.6849607937330753904, 12.58136878870645248 ) ) ;
#22397 = CARTESIAN_POINT ( 'NONE',  ( 11.33810207955129812, 4.796537143354000499, 7.174999999999999822 ) ) ;
#22399 = CARTESIAN_POINT ( 'NONE',  ( 24.37816199240487691, 8.911180165120670793, -9.054574436677963689 ) ) ;
#22398 = CARTESIAN_POINT ( 'NONE',  ( 7.591358119366002022, 4.587777998512997613, 6.499953102827994655 ) ) ;
#22400 = DIRECTION ( 'NONE',  ( -0.9999999999848602217, -4.443944959675825629E-06, 3.245118986823870102E-06 ) ) ;
#22401 = ORIENTED_EDGE ( 'NONE', *, *, #35079, .T. ) ;
#22402 = CARTESIAN_POINT ( 'NONE',  ( 0.7968663363676999900, 2.744051942617999895, -1.815777288092999875 ) ) ;
#22403 = CARTESIAN_POINT ( 'NONE',  ( 23.99447187923627567, -9.375551851464123843, -9.276312528594363727 ) ) ;
#22404 = CARTESIAN_POINT ( 'NONE',  ( 12.52002425203546920, -12.10842255864623240, 3.203403679956746242 ) ) ;
#22405 = CARTESIAN_POINT ( 'NONE',  ( 23.50387503050299998, 0.000000000000000000, 0.000000000000000000 ) ) ;
#22406 = CARTESIAN_POINT ( 'NONE',  ( 12.19498122944103713, -2.912558373969576397, 13.69368860183518599 ) ) ;
#22407 = CARTESIAN_POINT ( 'NONE',  ( 11.13729092314000013, 2.663668339045000000, 5.186744572171000378 ) ) ;
#22408 = CARTESIAN_POINT ( 'NONE',  ( 23.95121877702899837, 3.419245466583000326, -12.90028367964000111 ) ) ;
#22409 = VERTEX_POINT ( 'NONE', #4759 ) ;
#22410 = FACE_OUTER_BOUND ( 'NONE', #28941, .T. ) ;
#22411 = CARTESIAN_POINT ( 'NONE',  ( 17.91920925550954991, -10.80976535601232413, 4.345114692423678981 ) ) ;
#22412 = CARTESIAN_POINT ( 'NONE',  ( 8.064958992852089281, 5.350069970865218849, -7.500002487662858819 ) ) ;
#22413 = CARTESIAN_POINT ( 'NONE',  ( 0.9851098981878999572, -0.3635854775007999473, -3.573745162754999871 ) ) ;
#22414 = B_SPLINE_CURVE_WITH_KNOTS ( 'NONE', 3,
 ( #33491, #22636, #22985, #54804, #60052, #12853, #17401, #49556, #1668 ),
 .UNSPECIFIED., .F., .F.,
 ( 4, 1, 1, 1, 1, 1, 4 ),
 ( 0.000000000000000000, 0.1176715969261408201, 0.3173201826739890374, 0.5169687684225858781, 0.7166173541704341510, 0.9162659399182827569, 1.000000000000000000 ),
 .UNSPECIFIED. ) ;
#22415 = CARTESIAN_POINT ( 'NONE',  ( 17.98087424867483008, -3.330341796647162234, 11.16384340189062740 ) ) ;
#22416 = ADVANCED_FACE ( 'NONE', ( #42186 ), #21334, .F. ) ;
#22417 = AXIS2_PLACEMENT_3D ( 'NONE', #53844, #6637, #5942 ) ;
#22418 = CARTESIAN_POINT ( 'NONE',  ( 17.88838831427747778, 1.971212373206994384, -12.55919681887186101 ) ) ;
#22419 = CARTESIAN_POINT ( 'NONE',  ( 9.883499245234512287, -5.249996043174972371, 7.663630899194568080 ) ) ;
#22420 = CARTESIAN_POINT ( 'NONE',  ( 10.53057053952199951, 3.659587858614300249, 8.296503712697200328 ) ) ;
#22422 = PLANE ( 'NONE',  #23395 ) ;
#22421 = AXIS2_PLACEMENT_3D ( 'NONE', #44266, #11051, #65561 ) ;
#22423 = CARTESIAN_POINT ( 'NONE',  ( 10.01676935320999995, -4.324998011277000565, -9.154075058362000306 ) ) ;
#22424 = DIRECTION ( 'NONE',  ( 0.7071067811865475727, 0.7071067811865475727, 0.000000000000000000 ) ) ;
#22425 = CARTESIAN_POINT ( 'NONE',  ( 6.570886616771333344, -1.393043258182016686, 0.6426200619446901241 ) ) ;
#22426 = CARTESIAN_POINT ( 'NONE',  ( 12.38745432767040633, -10.82911002787651533, 4.296468796485326536 ) ) ;
#22427 = CARTESIAN_POINT ( 'NONE',  ( 11.08810207955139937, -4.796537143354000499, -7.174999999999999822 ) ) ;
#22428 = ORIENTED_EDGE ( 'NONE', *, *, #41572, .T. ) ;
#22429 = CARTESIAN_POINT ( 'NONE',  ( 7.392787521145388396, 2.688866882091175192, 8.641971157071431264 ) ) ;
#22430 = VERTEX_POINT ( 'NONE', #14919 ) ;
#22431 = CARTESIAN_POINT ( 'NONE',  ( 17.93750432894415070, -2.994741171281513736, 13.55599983589037372 ) ) ;
#22432 = CARTESIAN_POINT ( 'NONE',  ( 10.44426222744799837, -4.986443098259000450, -8.312555471636301263 ) ) ;
#22433 = VERTEX_POINT ( 'NONE', #53358 ) ;
#22434 = CARTESIAN_POINT ( 'NONE',  ( 10.39969598649000027, 4.888000489779200208, 6.971269690999399415 ) ) ;
#22435 = CARTESIAN_POINT ( 'NONE',  ( 6.132296051549998239, 0.8934716322868129224, 0.6963138618532788149 ) ) ;
#22436 = ADVANCED_FACE ( 'NONE', ( #68735 ), #47426, .T. ) ;
#22437 = CARTESIAN_POINT ( 'NONE',  ( 8.755358248830999557, -3.910012670022149806, -8.350279134800100422 ) ) ;
#22438 = CARTESIAN_POINT ( 'NONE',  ( 18.44383669537300108, -2.795303817231000298, 11.36579926027000020 ) ) ;
#22439 = DIRECTION ( 'NONE',  ( 1.000000000000000000, 0.000000000000000000, 0.000000000000000000 ) ) ;
#22440 = DIRECTION ( 'NONE',  ( 0.000000000000000000, -0.9989394889116069987, -0.04604234456473054599 ) ) ;
#22441 = CARTESIAN_POINT ( 'NONE',  ( 8.100000113405998903, -3.446132268436000216E-13, -3.324929372075999932E-14 ) ) ;
#22442 = CARTESIAN_POINT ( 'NONE',  ( 10.66852499011999988, -4.435470817312999969, -5.866470266317000082 ) ) ;
#22443 = CARTESIAN_POINT ( 'NONE',  ( 11.56441235500451015, -4.638700978900200056, -6.914884925939399629 ) ) ;
#22444 = ORIENTED_EDGE ( 'NONE', *, *, #11430, .T. ) ;
#22445 = CARTESIAN_POINT ( 'NONE',  ( 9.865910841232000905, 2.685250982074999904, -7.026194612421999608 ) ) ;
#22446 = ORIENTED_EDGE ( 'NONE', *, *, #38346, .F. ) ;
#22447 = CARTESIAN_POINT ( 'NONE',  ( 9.947306532704999427, 4.892812229297999416, -9.067756197920999739 ) ) ;
#22448 = ORIENTED_EDGE ( 'NONE', *, *, #29229, .T. ) ;
#22449 = DIRECTION ( 'NONE',  ( -1.000000000000000000, 0.000000000000000000, 0.000000000000000000 ) ) ;
#22450 = CARTESIAN_POINT ( 'NONE',  ( 10.26390815928000144, -4.634708712637999994, 4.688349230856999839 ) ) ;
#22451 = CARTESIAN_POINT ( 'NONE',  ( 10.69674062800671166, -2.930427565545544066, 5.070473834605100372 ) ) ;
#22452 = CARTESIAN_POINT ( 'NONE',  ( 9.373082992855458428, 2.782568642349716459, 7.827172124334915715 ) ) ;
#22453 = CARTESIAN_POINT ( 'NONE',  ( 12.46419745175922955, 3.023973028971910004, 13.54820305185629259 ) ) ;
#22454 = CARTESIAN_POINT ( 'NONE',  ( 17.56547987801838318, -1.875000035136120458, 12.57545641098306000 ) ) ;
#22455 = DIRECTION ( 'NONE',  ( -0.8987684456439055669, 0.000000000000000000, 0.4384236320214022764 ) ) ;
#22456 = CARTESIAN_POINT ( 'NONE',  ( 12.24892445252029205, 0.2854033456632657506, 13.89606078824648172 ) ) ;
#22457 = ORIENTED_EDGE ( 'NONE', *, *, #13413, .F. ) ;
#22458 = CARTESIAN_POINT ( 'NONE',  ( 7.307590560818999492, 4.037115771921000018, -6.023232697733999608 ) ) ;
#22459 = CARTESIAN_POINT ( 'NONE',  ( 5.500000000000000000, -13.94845324556000143, -4.312847325879000770 ) ) ;
#22460 = CARTESIAN_POINT ( 'NONE',  ( 9.758812222687625493, 4.162730299909893183, 6.640319176431033199 ) ) ;
#22461 = CARTESIAN_POINT ( 'NONE',  ( 5.142503212292999670, 0.8998068448443999889, 0.7742560839445998822 ) ) ;
#22462 = CARTESIAN_POINT ( 'NONE',  ( 9.286929719595001131, 4.102804347295999854, -5.770625657082999460 ) ) ;
#22463 = CARTESIAN_POINT ( 'NONE',  ( 3.999971066382000284, -2.149963194831999935, 0.000000000000000000 ) ) ;
#22464 = CARTESIAN_POINT ( 'NONE',  ( 9.947300131853999972, -4.892806669161000599, -9.067746434455999704 ) ) ;
#22465 = EDGE_CURVE ( 'NONE', #31041, #16661, #26447, .T. ) ;
#22466 = EDGE_CURVE ( 'NONE', #51230, #873, #60307, .T. ) ;
#22467 = ORIENTED_EDGE ( 'NONE', *, *, #35465, .F. ) ;
#22468 = CARTESIAN_POINT ( 'NONE',  ( 9.472537864290000442, -2.899999999999999911, -6.571291218949999902 ) ) ;
#22469 = B_SPLINE_CURVE_WITH_KNOTS ( 'NONE', 3,
 ( #25914, #60145, #22033, #27989 ),
 .UNSPECIFIED., .F., .F.,
 ( 4, 4 ),
 ( 0.000000000000000000, 1.000000000000000000 ),
 .UNSPECIFIED. ) ;
#22470 = CARTESIAN_POINT ( 'NONE',  ( 8.316694573732000606, -2.898380360490000029, 6.611503418275999522 ) ) ;
#22471 = B_SPLINE_CURVE_WITH_KNOTS ( 'NONE', 3,
 ( #48300, #36787, #10895, #53203, #42379, #4963 ),
 .UNSPECIFIED., .F., .F.,
 ( 4, 2, 4 ),
 ( 0.000000000000000000, 0.5000000000000000000, 1.000000000000000000 ),
 .UNSPECIFIED. ) ;
#22472 = CARTESIAN_POINT ( 'NONE',  ( 17.55505043854147118, -1.787816316115923954, 13.88537766212463254 ) ) ;
#22473 = ADVANCED_FACE ( 'NONE', ( #58596 ), #41399, .T. ) ;
#22474 = EDGE_CURVE ( 'NONE', #32857, #47524, #46932, .T. ) ;
#22475 = CARTESIAN_POINT ( 'NONE',  ( 8.576923877145999242, -3.399999999999999911, 5.924121105096999962 ) ) ;
#22476 = FACE_BOUND ( 'NONE', #16268, .T. ) ;
#22477 = CARTESIAN_POINT ( 'NONE',  ( 11.30878751119029957, 2.958974835389999836, -8.044634158732998586 ) ) ;
#22478 = CARTESIAN_POINT ( 'NONE',  ( 9.153405316139998860, 3.786750623988900166, -8.481512610189300361 ) ) ;
#22480 = CARTESIAN_POINT ( 'NONE',  ( 11.08388352126999976, -2.665717300265999956, 4.955856577691999831 ) ) ;
#22479 = CARTESIAN_POINT ( 'NONE',  ( 10.27964655415099848, -3.580250267348600079, 6.741370903243699253 ) ) ;
#22481 = CARTESIAN_POINT ( 'NONE',  ( 11.24809687351632448, -3.672815144550895194, 8.717465845835393523 ) ) ;
#22482 = ORIENTED_EDGE ( 'NONE', *, *, #29769, .T. ) ;
#22483 = CARTESIAN_POINT ( 'NONE',  ( 10.81524174883999834, 3.971581146373189597, 6.466884287543999577 ) ) ;
#22484 = CARTESIAN_POINT ( 'NONE',  ( 9.781666627457001439, -5.464740618746000145, 8.817321229216000589 ) ) ;
#22485 = CARTESIAN_POINT ( 'NONE',  ( 10.16360887879199915, 3.741427262966100287, 8.612148635591999835 ) ) ;
#22486 = CARTESIAN_POINT ( 'NONE',  ( 11.53926809187918856, -3.396911444218373877, 11.84566364033329400 ) ) ;
#22487 = CARTESIAN_POINT ( 'NONE',  ( 9.261668853699999815, -2.944250413017999612, 6.507387951280999339 ) ) ;
#22488 = CARTESIAN_POINT ( 'NONE',  ( 9.938536681611822132, -2.240210568168245597, 7.748637171123511358 ) ) ;
#22489 = CARTESIAN_POINT ( 'NONE',  ( 11.68591862085600219, 3.663505620393999962, -12.01771987839999944 ) ) ;
#22490 = EDGE_CURVE ( 'NONE', #53037, #57647, #12762, .T. ) ;
#22491 = CARTESIAN_POINT ( 'NONE',  ( 8.798797255587999189, -2.996487526130999779, -7.457514444071209780 ) ) ;
#22492 = CARTESIAN_POINT ( 'NONE',  ( 9.593930206849998754, -2.750000000000000000, -7.500000000000000000 ) ) ;
#22493 = CARTESIAN_POINT ( 'NONE',  ( 5.404173046211999676, -0.7698221690009998674, -0.8891327474049000035 ) ) ;
#22494 = CARTESIAN_POINT ( 'NONE',  ( 8.896907940197010589, -2.871668805576999883, -6.751846157836005169 ) ) ;
#22495 = CARTESIAN_POINT ( 'NONE',  ( 24.54687940532799928, -3.662828524876999836, 12.34579568540000061 ) ) ;
#22496 = CARTESIAN_POINT ( 'NONE',  ( 9.433536308085933797, 2.899999999999999911, -6.665341197419093255 ) ) ;
#22497 = CARTESIAN_POINT ( 'NONE',  ( 11.19518313518939934, 3.462699341914400097, -8.179416362154199760 ) ) ;
#22498 = CARTESIAN_POINT ( 'NONE',  ( 12.41737123625420125, 2.003119782516696645, -13.76653501054599893 ) ) ;
#22499 = PLANE ( 'NONE',  #35679 ) ;
#22500 = CARTESIAN_POINT ( 'NONE',  ( 5.500000000000000000, 12.87590651766999983, 2.791353855799999728 ) ) ;
#22501 = ORIENTED_EDGE ( 'NONE', *, *, #58555, .F. ) ;
#22502 = CARTESIAN_POINT ( 'NONE',  ( 25.59994555223600088, 10.09686240769121568, -5.033199831113227773 ) ) ;
#22503 = ITEM_DEFINED_TRANSFORMATION ( 'NONE', 'NONE', #68622,  #9676 ) ;
#22504 = CARTESIAN_POINT ( 'NONE',  ( 10.28014141025500017, -3.582647672488299850, -8.243346240911998635 ) ) ;
#22505 = DIRECTION ( 'NONE',  ( -1.000000000000000000, 0.000000000000000000, 0.000000000000000000 ) ) ;
#22506 = CARTESIAN_POINT ( 'NONE',  ( 25.59997277611800115, 2.578802611042650509E-13, -11.19994871957399241 ) ) ;
#22507 = CARTESIAN_POINT ( 'NONE',  ( 10.51720455737510562, 5.205742106671379155, 8.206130011351980613 ) ) ;
#22508 = CARTESIAN_POINT ( 'NONE',  ( 5.500000000000000000, 12.22293997673000021, -3.800173559029999648 ) ) ;
#22509 = ORIENTED_EDGE ( 'NONE', *, *, #56907, .F. ) ;
#22510 = FACE_OUTER_BOUND ( 'NONE', #12742, .T. ) ;
#22511 = CARTESIAN_POINT ( 'NONE',  ( 18.14722095428668780, 2.700912180127440720, -13.62881044890620785 ) ) ;
#22512 = EDGE_LOOP ( 'NONE', ( #36886, #887, #45663, #4290 ) ) ;
#22513 = PLANE ( 'NONE',  #20590 ) ;
#22514 = CARTESIAN_POINT ( 'NONE',  ( 8.802620559624999785, -3.975070057433999438, 9.483761758588999058 ) ) ;
#22515 = ADVANCED_FACE ( 'NONE', ( #36242 ), #27835, .T. ) ;
#22516 = CARTESIAN_POINT ( 'NONE',  ( 15.36937411412500154, 8.827864207275998965, 7.821779713377999599 ) ) ;
#22517 = CARTESIAN_POINT ( 'NONE',  ( 15.40000000005200143, -9.187454762873001002, -8.213177997099000649 ) ) ;
#22518 = CARTESIAN_POINT ( 'NONE',  ( 11.11486084871780022, 5.207010770456999893, -7.174999999999999822 ) ) ;
#22519 = AXIS2_PLACEMENT_3D ( 'NONE', #36872, #10290, #31625 ) ;
#22520 = CARTESIAN_POINT ( 'NONE',  ( 8.409260841228999084, 5.592690705327999723, -8.535639167491000379 ) ) ;
#22521 = ADVANCED_FACE ( 'NONE', ( #17328 ), #12088, .T. ) ;
#22522 = CARTESIAN_POINT ( 'NONE',  ( 10.22934687351566829, -4.163624617374463099, -6.249999999999998224 ) ) ;
#22523 = CARTESIAN_POINT ( 'NONE',  ( 4.888359839683332098, 0.7554284705563452107, 1.310679582531388609 ) ) ;
#22524 = ORIENTED_EDGE ( 'NONE', *, *, #33542, .F. ) ;
#22525 = CARTESIAN_POINT ( 'NONE',  ( -0.2999999999999999889, -1.649999999999999911, 0.000000000000000000 ) ) ;
#22526 = B_SPLINE_CURVE_WITH_KNOTS ( 'NONE', 3,
 ( #52069, #13999, #46153, #40903, #46498, #58015, #56642, #62898, #46839, #30090, #41589, #62560, #36343, #42290, #4860, #15018, #35665, #57659, #25164, #56980, #63241, #67802, #31114, #14342 ),
 .UNSPECIFIED., .F., .F.,
 ( 4, 2, 2, 1, 2, 2, 2, 2, 2, 2, 1, 2, 4 ),
 ( 0.000000000000000000, 0.1249999999999996669, 0.1874999999999996947, 0.2499999999999997224, 0.3124999999999997224, 0.3749999999999997780, 0.4999999999999997780, 0.6249999999999995559, 0.7499999999999993339, 0.8124999999999994449, 0.8749999999999996669, 0.9374999999999997780, 1.000000000000000000 ),
 .UNSPECIFIED. ) ;
#22527 = CARTESIAN_POINT ( 'NONE',  ( 17.63827777595935231, -3.120766739611795071, -13.52195882727504106 ) ) ;
#22528 = LINE ( 'NONE', #21161, #17121 ) ;
#22529 = ORIENTED_EDGE ( 'NONE', *, *, #55169, .F. ) ;
#22530 = CARTESIAN_POINT ( 'NONE',  ( 9.075651506909604649, 5.234436409784954947, -7.567790861611047859 ) ) ;
#22531 = DIRECTION ( 'NONE',  ( 0.5000000000000169864, 0.000000000000000000, -0.8660254037844288266 ) ) ;
#22532 = EDGE_LOOP ( 'NONE', ( #50901, #34172, #2252, #28994 ) ) ;
#22533 = CARTESIAN_POINT ( 'NONE',  ( 9.887950584426999256, 4.398663815465100768, 8.421905343605699201 ) ) ;
#22534 = CARTESIAN_POINT ( 'NONE',  ( 17.82422846108294578, -1.812210939693179368, -12.46899807711483987 ) ) ;
#22535 = CARTESIAN_POINT ( 'NONE',  ( 5.126958905526000088, 0.3514838302171000017, -1.372182189413999831 ) ) ;
#22536 = AXIS2_PLACEMENT_3D ( 'NONE', #7235, #60717, #28928 ) ;
#22537 = CARTESIAN_POINT ( 'NONE',  ( 8.367699215443000327, 5.101426577346004798, -6.644016792819001260 ) ) ;
#22538 = CARTESIAN_POINT ( 'NONE',  ( 16.42341781689399838, 3.643648243171000001, 12.02373124034999918 ) ) ;
#22539 = FACE_OUTER_BOUND ( 'NONE', #27014, .T. ) ;
#22540 = CARTESIAN_POINT ( 'NONE',  ( 9.864633995697998259, 4.861719613449499988, 7.404358731173799946 ) ) ;
#22541 = CARTESIAN_POINT ( 'NONE',  ( 8.755358248830999557, 4.089987329977850194, -8.350279134800100422 ) ) ;
#22542 = VERTEX_POINT ( 'NONE', #39010 ) ;
#22543 = CARTESIAN_POINT ( 'NONE',  ( 10.57892463485000079, 4.649960478797999563, 5.681084732956000138 ) ) ;
#22544 = CARTESIAN_POINT ( 'NONE',  ( 11.12964528040999923, 3.869081149487999749, -9.017143166339000260 ) ) ;
#22545 = CARTESIAN_POINT ( 'NONE',  ( 25.30000327618300204, 0.7080256801165658587, 11.56241914337144472 ) ) ;
#22546 = CARTESIAN_POINT ( 'NONE',  ( 12.63821499911163038, 1.807008444693749771, -13.88289391573714227 ) ) ;
#22547 = CARTESIAN_POINT ( 'NONE',  ( 10.56244474310100045, -2.862064370975999861, -8.052229793103100164 ) ) ;
#22548 = B_SPLINE_CURVE_WITH_KNOTS ( 'NONE', 3,
 ( #45772, #9722, #62521, #4130, #13960, #3115, #45432, #50677, #19884, #19542, #3448, #40189 ),
 .UNSPECIFIED., .F., .F.,
 ( 4, 2, 2, 2, 2, 4 ),
 ( 0.000000000000000000, 0.2500000000000020539, 0.3750000000000017208, 0.4375000000000028866, 0.5000000000000039968, 1.000000000000000000 ),
 .UNSPECIFIED. ) ;
#22549 = CARTESIAN_POINT ( 'NONE',  ( 10.02990552045999983, -2.506467134554999809, 6.215414506835998942 ) ) ;
#22550 = CARTESIAN_POINT ( 'NONE',  ( 18.08498662421417791, -0.4989076128645613117, 13.99111800451625243 ) ) ;
#22551 = FACE_OUTER_BOUND ( 'NONE', #62755, .T. ) ;
#22552 = ORIENTED_EDGE ( 'NONE', *, *, #21785, .F. ) ;
#22553 = ORIENTED_EDGE ( 'NONE', *, *, #16658, .T. ) ;
#22554 = FACE_OUTER_BOUND ( 'NONE', #65911, .T. ) ;
#22555 = CARTESIAN_POINT ( 'NONE',  ( 1.746770393513999881E-07, 2.400000174626000238, -7.471637644860000521E-10 ) ) ;
#22556 = ADVANCED_FACE ( 'NONE', ( #1252 ), #34012, .F. ) ;
#22557 = CARTESIAN_POINT ( 'NONE',  ( 12.27274360190958191, -0.3282986408113108268, -13.89479914614070211 ) ) ;
#22558 = EDGE_CURVE ( 'NONE', #11948, #51764, #33562, .T. ) ;
#22559 = CARTESIAN_POINT ( 'NONE',  ( 7.267328493169560311, -2.819480080816116896, 6.820320496870126981 ) ) ;
#22560 = CARTESIAN_POINT ( 'NONE',  ( 15.96647867633519802, 8.895858221259695497, 8.626805212950838353 ) ) ;
#22561 = CARTESIAN_POINT ( 'NONE',  ( 7.358058059621999547, -4.561648098548999997, 6.153050355516999304 ) ) ;
#22562 = LINE ( 'NONE', #43904, #27064 ) ;
#22564 = CARTESIAN_POINT ( 'NONE',  ( 10.29353630810780018, -2.899999999999999911, 6.665341197265856721 ) ) ;
#22563 = CARTESIAN_POINT ( 'NONE',  ( 10.81759632033899976, -5.184381781355999586, 7.983346856269500691 ) ) ;
#22565 = CARTESIAN_POINT ( 'NONE',  ( 11.01041369783139956, 3.935522326596939902, -8.776385133971000840 ) ) ;
#22566 = AXIS2_PLACEMENT_3D ( 'NONE', #2751, #61141, #7652 ) ;
#22567 = CARTESIAN_POINT ( 'NONE',  ( 24.62774583285499830, -8.736962890587999908, -9.042103898172999976 ) ) ;
#22568 = CARTESIAN_POINT ( 'NONE',  ( 8.677306202554058601, 2.980089076194122999, -6.115478653393680908 ) ) ;
#22569 = CARTESIAN_POINT ( 'NONE',  ( 18.17177216100527914, -0.1019009512359500130, 12.69945530929771493 ) ) ;
#22570 = CARTESIAN_POINT ( 'NONE',  ( 8.474485200571999499, 5.100000000000000533, 6.560614371780999043 ) ) ;
#22571 = CARTESIAN_POINT ( 'NONE',  ( 18.14655301452571834, -2.701944876743755053, -12.40222020716218410 ) ) ;
#22572 = ORIENTED_EDGE ( 'NONE', *, *, #50968, .F. ) ;
#22574 = CARTESIAN_POINT ( 'NONE',  ( 9.198551576885758863, 4.680098380207501130, -8.679821298980339606 ) ) ;
#22573 = CARTESIAN_POINT ( 'NONE',  ( 7.968183059622999664, -2.280579276705999803, 6.510290672242000198 ) ) ;
#22575 = CARTESIAN_POINT ( 'NONE',  ( 9.251970280414001380, 5.673443217382001080, -7.051790060464000476 ) ) ;
#22576 = DIRECTION ( 'NONE',  ( -1.000000000000000000, 0.000000000000000000, 0.000000000000000000 ) ) ;
#22577 = ADVANCED_FACE ( 'NONE', ( #59977 ), #11728, .F. ) ;
#22578 = CARTESIAN_POINT ( 'NONE',  ( 23.60205915885299888, 9.377218989194005871, -8.305825996818995804 ) ) ;
#22579 = CIRCLE ( 'NONE', #1377, 0.6999999999999992895 ) ;
#22580 = CARTESIAN_POINT ( 'NONE',  ( 17.55505043854143565, 3.125000000000000000, -13.52084414783465682 ) ) ;
#22581 = DIRECTION ( 'NONE',  ( 1.000000000000000000, 0.000000000000000000, 0.000000000000000000 ) ) ;
#22582 = CONICAL_SURFACE ( 'NONE', #51583, 0.4311160744474001327, 0.7853981633972997312 ) ;
#22583 = CARTESIAN_POINT ( 'NONE',  ( 2.695429889327000339, -1.927268832017999811, 3.227074855961999944 ) ) ;
#22584 = VERTEX_POINT ( 'NONE', #33767 ) ;
#22585 = CARTESIAN_POINT ( 'NONE',  ( 12.08006680260081467, -0.02395120399004109155, -12.59999907117299855 ) ) ;
#22586 = DIRECTION ( 'NONE',  ( -1.000000000000000000, -5.693641285695000080E-09, 1.583067011023000022E-09 ) ) ;
#22587 = CARTESIAN_POINT ( 'NONE',  ( 17.65081963855157099, 3.193844305817326479, -12.18849311783432654 ) ) ;
#22588 = CARTESIAN_POINT ( 'NONE',  ( 23.81723327626561471, -12.99655882303040855, -3.682219191457393848 ) ) ;
#22589 = CARTESIAN_POINT ( 'NONE',  ( 7.988545280410000338, 3.566637212418000136, 5.743604853744000316 ) ) ;
#22590 = ORIENTED_EDGE ( 'NONE', *, *, #47917, .T. ) ;
#22591 = CARTESIAN_POINT ( 'NONE',  ( 6.407261061822000059, -0.8669997925267000083, 1.185259004083000001 ) ) ;
#22592 = CARTESIAN_POINT ( 'NONE',  ( 7.151370280410000113, 3.450042761745999886, -8.965148246193999526 ) ) ;
#22594 = CARTESIAN_POINT ( 'NONE',  ( 9.632179190069999564, 5.638172764974000550, 6.476627236431999890 ) ) ;
#22593 = CARTESIAN_POINT ( 'NONE',  ( 8.380370550424483866, -2.884289483078743555, 8.834819442766946196 ) ) ;
#22595 = CARTESIAN_POINT ( 'NONE',  ( 10.37837607040047594, -3.132032243413395367, -7.396454632467190926 ) ) ;
#22596 = ORIENTED_EDGE ( 'NONE', *, *, #20628, .T. ) ;
#22597 = DIRECTION ( 'NONE',  ( -1.000000000000000000, 0.000000000000000000, 0.000000000000000000 ) ) ;
#22598 = CARTESIAN_POINT ( 'NONE',  ( 10.18239901426000138, -2.607725299334000102, 7.783410967795999724 ) ) ;
#22599 = ORIENTED_EDGE ( 'NONE', *, *, #35079, .F. ) ;
#22600 = CARTESIAN_POINT ( 'NONE',  ( 1.700000811628999964, -1.775000326287000219, 0.000000000000000000 ) ) ;
#22601 = CARTESIAN_POINT ( 'NONE',  ( 25.46375152665800101, -2.879425814940999917, -11.30951176145000048 ) ) ;
#22602 = CARTESIAN_POINT ( 'NONE',  ( 18.01141113125041571, -0.4275223103465174423, -13.89116040406442032 ) ) ;
#22603 = EDGE_LOOP ( 'NONE', ( #61844, #30167, #48560, #55070 ) ) ;
#22604 = CARTESIAN_POINT ( 'NONE',  ( 16.06714147702597728, -8.497559733040684904, -7.969681199759283352 ) ) ;
#22605 = CARTESIAN_POINT ( 'NONE',  ( 11.23589666366019912, 3.960399224793059947, -8.391246537305399045 ) ) ;
#22606 = EDGE_CURVE ( 'NONE', #22744, #18238, #61910, .T. ) ;
#22607 = B_SPLINE_CURVE_WITH_KNOTS ( 'NONE', 3,
 ( #6419, #21812, #44201, #43844 ),
 .UNSPECIFIED., .F., .F.,
 ( 4, 4 ),
 ( 0.8747102644739949140, 1.000000000000000000 ),
 .UNSPECIFIED. ) ;
#22608 = DIRECTION ( 'NONE',  ( 0.000000000000000000, 0.000000000000000000, -1.000000000000000000 ) ) ;
#22609 = CARTESIAN_POINT ( 'NONE',  ( 9.440795537696432760, -5.100000000000000533, 6.662590550605512085 ) ) ;
#22610 = ORIENTED_EDGE ( 'NONE', *, *, #7743, .T. ) ;
#22611 = CARTESIAN_POINT ( 'NONE',  ( 8.128301658772999261, 3.117378429069999957, 8.662179062556001341 ) ) ;
#22612 = CARTESIAN_POINT ( 'NONE',  ( 12.40004937879933067, -2.976133613074172679, -13.56081502232354907 ) ) ;
#22613 = LINE ( 'NONE', #63877, #32929 ) ;
#22614 = VECTOR ( 'NONE', #27831, 999.9999999999998863 ) ;
#22615 = CARTESIAN_POINT ( 'NONE',  ( 16.08724299200000019, -9.224388201582000235, -8.529033888242999240 ) ) ;
#22616 = ORIENTED_EDGE ( 'NONE', *, *, #23183, .F. ) ;
#22617 = CARTESIAN_POINT ( 'NONE',  ( 12.35269809054582701, -2.068595867586759951, -12.54166796000261108 ) ) ;
#22618 = CARTESIAN_POINT ( 'NONE',  ( 10.66684687351590277, 4.768183399968648040, -6.500416447002280051 ) ) ;
#22619 = CARTESIAN_POINT ( 'NONE',  ( 7.988347165043021114, 3.468997027298886149, -9.279625640052284297 ) ) ;
#22620 = DIRECTION ( 'NONE',  ( -0.000000000000000000, -0.000000000000000000, 1.000000000000000000 ) ) ;
#22621 = DIRECTION ( 'NONE',  ( -1.000000000000000000, 0.000000000000000000, 0.000000000000000000 ) ) ;
#22622 = CARTESIAN_POINT ( 'NONE',  ( 10.62487750876920067, -4.543557328885200697, -8.343502390669698343 ) ) ;
#22623 = CARTESIAN_POINT ( 'NONE',  ( 5.919609839683875663, 0.1963495408493571848, 1.500000000000000666 ) ) ;
#22624 = CARTESIAN_POINT ( 'NONE',  ( 17.86072591669553944, -3.045244688009580702, 12.30767216807748987 ) ) ;
#22625 = ORIENTED_EDGE ( 'NONE', *, *, #20430, .T. ) ;
#22626 = CARTESIAN_POINT ( 'NONE',  ( 11.34523293495530005, -5.315205473512000012, -7.447129085684729866 ) ) ;
#22627 = ORIENTED_EDGE ( 'NONE', *, *, #33224, .F. ) ;
#22628 = VECTOR ( 'NONE', #14705, 1000.000000000000114 ) ;
#22629 = CARTESIAN_POINT ( 'NONE',  ( 19.89999890908300273, -12.52500000000000036, 0.000000000000000000 ) ) ;
#22630 = CARTESIAN_POINT ( 'NONE',  ( 8.599639158772999892, 2.261390688294000029, -6.733978371730000134 ) ) ;
#22631 = CARTESIAN_POINT ( 'NONE',  ( 2.335490869717000262, 3.363656811547999670, -0.3259338917754999732 ) ) ;
#22632 = B_SPLINE_CURVE_WITH_KNOTS ( 'NONE', 3,
 ( #37525, #10268, #41744, #15856 ),
 .UNSPECIFIED., .F., .F.,
 ( 4, 4 ),
 ( 0.000000000000000000, 1.000000000000000000 ),
 .UNSPECIFIED. ) ;
#22633 = CARTESIAN_POINT ( 'NONE',  ( 10.49937632700000023, -2.985311165300999825, -6.358653174814000053 ) ) ;
#22634 = CARTESIAN_POINT ( 'NONE',  ( 23.85395532197026469, -13.23045631795083921, -3.489573210166486472 ) ) ;
#22635 = CARTESIAN_POINT ( 'NONE',  ( 24.13648151864700253, 12.33467166542999927, 3.394534719267999989 ) ) ;
#22636 = CARTESIAN_POINT ( 'NONE',  ( 11.56493925477931128, 5.173530340702487962, 7.051164236119339179 ) ) ;
#22637 = ORIENTED_EDGE ( 'NONE', *, *, #3466, .F. ) ;
#22638 = CARTESIAN_POINT ( 'NONE',  ( 18.35481756226800343, 2.723642650930000020, 11.47750709399999991 ) ) ;
#22639 = EDGE_CURVE ( 'NONE', #39722, #10018, #59256, .T. ) ;
#22640 = CARTESIAN_POINT ( 'NONE',  ( 9.380783851237000093, 2.204242311415999911, 7.545378292079000460 ) ) ;
#22641 = EDGE_CURVE ( 'NONE', #21130, #44214, #27747, .T. ) ;
#22642 = CARTESIAN_POINT ( 'NONE',  ( 2.061390132542666898, 3.499999999999999112, 0.4581489286485193602 ) ) ;
#22643 = DIRECTION ( 'NONE',  ( 0.000000000000000000, 0.000000000000000000, -1.000000000000000000 ) ) ;
#22644 = CARTESIAN_POINT ( 'NONE',  ( 18.40429364930200151, 2.938801558760000265, -11.32979830910000096 ) ) ;
#22645 = CARTESIAN_POINT ( 'NONE',  ( 11.56025819896753859, 3.013900664291200293, -7.685900384398899554 ) ) ;
#22646 = CARTESIAN_POINT ( 'NONE',  ( 10.26817165544659893, 5.148139224407167980, 8.818277135132042588 ) ) ;
#22647 = CARTESIAN_POINT ( 'NONE',  ( 23.63093901041600020, -10.04490667398999904, -9.752327919465999528 ) ) ;
#22648 = CARTESIAN_POINT ( 'NONE',  ( 23.62923211109600174, -10.04860736350999950, 9.751346780839998729 ) ) ;
#22649 = SURFACE_SIDE_STYLE ('',( #11816 ) ) ;
#22650 = VERTEX_POINT ( 'NONE', #24298 ) ;
#22651 = CARTESIAN_POINT ( 'NONE',  ( 8.913566940379999082, -2.550589632307000088, 8.854674225901000284 ) ) ;
#22652 = CARTESIAN_POINT ( 'NONE',  ( 9.663732219486000474, -2.297586052318000061, -7.360088033824999876 ) ) ;
#22653 = CARTESIAN_POINT ( 'NONE',  ( 17.93716281226432230, 2.994693044426598671, 13.55594923565224974 ) ) ;
#22654 = EDGE_CURVE ( 'NONE', #64219, #35557, #24393, .T. ) ;
#22655 = CARTESIAN_POINT ( 'NONE',  ( 8.073148997456000231, 5.167567567567999731, -6.822293592207000934 ) ) ;
#22656 = CARTESIAN_POINT ( 'NONE',  ( 10.91195257254739914, -5.227167235646000165, -7.856899084262298771 ) ) ;
#22657 = ORIENTED_EDGE ( 'NONE', *, *, #33621, .F. ) ;
#22658 = CIRCLE ( 'NONE', #29382, 13.92493900951000718 ) ;
#22659 = CARTESIAN_POINT ( 'NONE',  ( 25.40548268214499927, 3.091940963388000174, -11.38328889108999853 ) ) ;
#22660 = ADVANCED_FACE ( 'NONE', ( #12784 ), #19049, .F. ) ;
#22661 = CARTESIAN_POINT ( 'NONE',  ( 7.603420280409000753, 5.687206835507000235, 6.847268999608999707 ) ) ;
#22664 = CIRCLE ( 'NONE', #53910, 11.30000000000000604 ) ;
#22663 = CARTESIAN_POINT ( 'NONE',  ( 9.226787239609999247, -4.219532685969900498, 6.659501631675699862 ) ) ;
#22662 = CARTESIAN_POINT ( 'NONE',  ( 9.211104719594999324, 5.462898983065000102, -8.055936939571999744 ) ) ;
#22665 = CARTESIAN_POINT ( 'NONE',  ( 2.981121534451109945, -2.748581895732221003, 1.749100406568057986 ) ) ;
#22666 = EDGE_LOOP ( 'NONE', ( #8591, #27454, #16341, #55726, #20070, #4254, #344, #50599, #63801, #35462 ) ) ;
#22667 = CARTESIAN_POINT ( 'NONE',  ( 10.69030645188999884, 5.903031974240000146, 7.830710565751001440 ) ) ;
#22668 = CARTESIAN_POINT ( 'NONE',  ( 17.74755423490966066, -3.094705742910454305, -13.52911976267489713 ) ) ;
#22669 = CARTESIAN_POINT ( 'NONE',  ( 11.78179573085659904, 4.973133828855400118, 7.331616337578100051 ) ) ;
#22670 = CARTESIAN_POINT ( 'NONE',  ( 9.646285452541999206, -2.591464128784999765, 6.760053199270999791 ) ) ;
#22671 = CARTESIAN_POINT ( 'NONE',  ( 8.328793652375997780, 2.897388771918001371, 6.655272502545993341 ) ) ;
#22672 = ORIENTED_EDGE ( 'NONE', *, *, #11389, .T. ) ;
#22673 = CYLINDRICAL_SURFACE ( 'NONE', #2027, 11.65000000000000036 ) ;
#22674 = CARTESIAN_POINT ( 'NONE',  ( 0.1499942179679999987, -2.750000000000000000, 0.000000000000000000 ) ) ;
#22676 = CARTESIAN_POINT ( 'NONE',  ( 10.16821935321000048, -2.330398934821000356, -7.267462182607999921 ) ) ;
#22675 = CARTESIAN_POINT ( 'NONE',  ( 12.26982956731400165, -11.56648533137999912, 4.655999611355000845 ) ) ;
#22677 = CARTESIAN_POINT ( 'NONE',  ( 7.751324872093176666, -5.382780984143693992, 8.555630740302449411 ) ) ;
#22678 = STYLED_ITEM ( 'NONE', ( #42655 ), #30272 ) ;
#22679 = CARTESIAN_POINT ( 'NONE',  ( 24.52306328725676821, 12.12196666327097638, 3.142986865081914605 ) ) ;
#22680 = CARTESIAN_POINT ( 'NONE',  ( 11.42834208742529967, -4.706521750018099581, -8.610579932818998472 ) ) ;
#22681 = CARTESIAN_POINT ( 'NONE',  ( 10.30995058442699985, -3.546800160410199965, 8.548019252390998801 ) ) ;
#22682 = ORIENTED_EDGE ( 'NONE', *, *, #14369, .F. ) ;
#22683 = CARTESIAN_POINT ( 'NONE',  ( 9.048601287889788125, -3.999999532294070459, -8.698595322193611423 ) ) ;
#22684 = CARTESIAN_POINT ( 'NONE',  ( 11.78118179236250107, -4.267047616085000605, 8.749800764654999341 ) ) ;
#22685 = CARTESIAN_POINT ( 'NONE',  ( 7.640464943433003420, 3.216280862983999622, 6.362631827276998386 ) ) ;
#22686 = CARTESIAN_POINT ( 'NONE',  ( 10.81349144726329925, 3.261052100888700345, 8.542723541016000510 ) ) ;
#22687 = AXIS2_PLACEMENT_3D ( 'NONE', #58494, #58153, #10256 ) ;
#22688 = VERTEX_POINT ( 'NONE', #23608 ) ;
#22689 = CARTESIAN_POINT ( 'NONE',  ( 9.111654719595000174, 4.989193221215000307, -6.287302145481000082 ) ) ;
#22690 = CARTESIAN_POINT ( 'NONE',  ( 24.33740888733500185, 12.30440757811000019, -3.219246934404999649 ) ) ;
#22691 = CARTESIAN_POINT ( 'NONE',  ( 12.44969725703162311, 3.107561633766895426, -12.21077779329595359 ) ) ;
#22692 = CARTESIAN_POINT ( 'NONE',  ( 11.27879632507499963, -3.576455950783300253, 6.714825466131699727 ) ) ;
#22693 = VERTEX_POINT ( 'NONE', #34464 ) ;
#22694 = CARTESIAN_POINT ( 'NONE',  ( 8.960616452296999768, -2.899999999999999911, 6.279946362737000243 ) ) ;
#22695 = CARTESIAN_POINT ( 'NONE',  ( 10.50851354018319128, 3.836375382625529795, -8.749999999999998224 ) ) ;
#22696 = ORIENTED_EDGE ( 'NONE', *, *, #14055, .T. ) ;
#22697 = CARTESIAN_POINT ( 'NONE',  ( 23.67741884366763117, 9.992396248498485178, 9.459260079125268561 ) ) ;
#22698 = ORIENTED_EDGE ( 'NONE', *, *, #20348, .T. ) ;
#22699 = CARTESIAN_POINT ( 'NONE',  ( 12.68571266918098317, -3.190282694684599907, -12.18942654693561067 ) ) ;
#22700 = CARTESIAN_POINT ( 'NONE',  ( 11.53148876160955005, 3.209326035813000022, 6.677731919207799294 ) ) ;
#22701 = PRODUCT_RELATED_PRODUCT_CATEGORY ( 'part', '', ( #18770 ) ) ;
#22702 = LINE ( 'NONE', #44399, #15280 ) ;
#22703 = CARTESIAN_POINT ( 'NONE',  ( 10.16989991304999918, 2.594216849811000092, -6.291257009166999481 ) ) ;
#22704 = CARTESIAN_POINT ( 'NONE',  ( 18.13429499374400322, -12.00402196696999901, 3.371453313192000145 ) ) ;
#22705 = DIRECTION ( 'NONE',  ( 0.9999999999999987788, 4.835300621521984030E-08, 1.472962709867996247E-08 ) ) ;
#22706 = CARTESIAN_POINT ( 'NONE',  ( 13.99967273502900156, 9.525279043350998620, 8.192384979499998110 ) ) ;
#22707 = CARTESIAN_POINT ( 'NONE',  ( 18.08578179881429193, 0.3302353423713645375, -12.69422546839061461 ) ) ;
#22708 = CARTESIAN_POINT ( 'NONE',  ( 12.18136627099982405, 2.541785745017987264, -12.44176459540348922 ) ) ;
#22709 = CARTESIAN_POINT ( 'NONE',  ( 11.06379841651039797, -4.401637675674300532, -8.567697191971999970 ) ) ;
#22710 = CARTESIAN_POINT ( 'NONE',  ( 7.262114158771001193, 4.847807297114000491, 9.065373753110998578 ) ) ;
#22711 = ORIENTED_EDGE ( 'NONE', *, *, #19573, .F. ) ;
#22712 = VECTOR ( 'NONE', #48586, 1000.000000000000114 ) ;
#22713 = AXIS2_PLACEMENT_3D ( 'NONE', #60332, #65566, #55085 ) ;
#22714 = FILL_AREA_STYLE ('',( #7682 ) ) ;
#22715 = CARTESIAN_POINT ( 'NONE',  ( 7.444482658958142984, 5.271178084961285926, 6.970094358920671418 ) ) ;
#22716 = CARTESIAN_POINT ( 'NONE',  ( 16.39999999231800132, 3.216285993016000155, 11.40340220863999932 ) ) ;
#22717 = CARTESIAN_POINT ( 'NONE',  ( 18.10358258445729973, 2.009225442943100681, 12.43878435193939858 ) ) ;
#22718 = CARTESIAN_POINT ( 'NONE',  ( 11.09999999999999964, -2.649999999999999911, 7.500000000000000000 ) ) ;
#22719 = CARTESIAN_POINT ( 'NONE',  ( 9.595493858556999101, 3.928424745541000185, 5.531312048131000303 ) ) ;
#22720 = CARTESIAN_POINT ( 'NONE',  ( 10.18282478114062606, -4.607703288839251954, 6.870532779523098377 ) ) ;
#22721 = CARTESIAN_POINT ( 'NONE',  ( 12.08019350287876037, -0.1887961028407837971, -12.59999260960569245 ) ) ;
#22722 = ADVANCED_FACE ( 'NONE', ( #66598 ), #62044, .T. ) ;
#22723 = VERTEX_POINT ( 'NONE', #44950 ) ;
#22724 = CARTESIAN_POINT ( 'NONE',  ( 12.40918755490010739, -3.083210392534605937, 12.21694967330944692 ) ) ;
#22725 = EDGE_CURVE ( 'NONE', #68087, #27711, #1948, .T. ) ;
#22726 = CARTESIAN_POINT ( 'NONE',  ( 9.201101285863998669, -4.735211557675400584, -6.626387721327399838 ) ) ;
#22727 = CARTESIAN_POINT ( 'NONE',  ( 24.56046482271400322, -3.658438515550000325, -12.32938606307999940 ) ) ;
#22728 = CARTESIAN_POINT ( 'NONE',  ( 11.79999999684100054, 3.345264396959000130, -11.86064773189999855 ) ) ;
#22729 = CARTESIAN_POINT ( 'NONE',  ( 10.25564828895399927, 4.880669054351300495, -7.981013126389099099 ) ) ;
#22730 = CARTESIAN_POINT ( 'NONE',  ( 12.21516876105738802, -0.4188397444781318257, 12.59305179380755213 ) ) ;
#22731 = VECTOR ( 'NONE', #44332, 1000.000000000000114 ) ;
#22732 = CARTESIAN_POINT ( 'NONE',  ( 7.700045280408999382, 3.346262376537000094, 6.002251090845000192 ) ) ;
#22733 = CARTESIAN_POINT ( 'NONE',  ( 5.700000000399000122, -0.2999999996014000025, -3.150000003758000044 ) ) ;
#22734 = CARTESIAN_POINT ( 'NONE',  ( 12.61225881068683918, 3.094544630460535739, 12.29295341835051047 ) ) ;
#22735 = ORIENTED_EDGE ( 'NONE', *, *, #56185, .T. ) ;
#22736 = CARTESIAN_POINT ( 'NONE',  ( 7.790635841228000125, 3.416213390569000197, 6.162512717529000206 ) ) ;
#22737 = CARTESIAN_POINT ( 'NONE',  ( 11.16225954179439839, 4.877394611789299894, -8.229019074832200076 ) ) ;
#22738 = CARTESIAN_POINT ( 'NONE',  ( 30.60000000000000142, 0.000000000000000000, 0.000000000000000000 ) ) ;
#22740 = DIRECTION ( 'NONE',  ( 0.000000000000000000, 0.000000000000000000, -1.000000000000000000 ) ) ;
#22739 = CARTESIAN_POINT ( 'NONE',  ( 12.38745432786477529, 10.82911002781349374, -4.296468796670141366 ) ) ;
#22741 = B_SPLINE_CURVE_WITH_KNOTS ( 'NONE', 3,
 ( #25430, #14603, #35923, #57236 ),
 .UNSPECIFIED., .F., .F.,
 ( 4, 4 ),
 ( 0.000000000000000000, 1.000000000000000000 ),
 .UNSPECIFIED. ) ;
#22742 = CARTESIAN_POINT ( 'NONE',  ( 10.99826088462129903, -3.998156935320088756, -6.633804182961699603 ) ) ;
#22743 = CARTESIAN_POINT ( 'NONE',  ( 8.933148997457999840, 5.167567567567999731, 6.822293592207000934 ) ) ;
#22744 = VERTEX_POINT ( 'NONE', #34113 ) ;
#22745 = CARTESIAN_POINT ( 'NONE',  ( 1.787066629541000040, 2.957881470139000157, 1.368292308076999975 ) ) ;
#22746 = EDGE_CURVE ( 'NONE', #49595, #48149, #2289, .T. ) ;
#22747 = CARTESIAN_POINT ( 'NONE',  ( 24.13789899383552395, -9.157240139151127778, -9.130332070236796937 ) ) ;
#22748 = CARTESIAN_POINT ( 'NONE',  ( 25.59994555223599733, -8.527741194213000142, -7.260611644044000279 ) ) ;
#22749 = CARTESIAN_POINT ( 'NONE',  ( 8.994442991499997930, 3.945420918055940085, 8.365291319916600798 ) ) ;
#22750 = B_SPLINE_CURVE_WITH_KNOTS ( 'NONE', 3,
 ( #54688, #43859, #64130, #28124, #37567, #37916, #58901, #48408, #21831, #59236 ),
 .UNSPECIFIED., .F., .F.,
 ( 4, 2, 2, 2, 4 ),
 ( 0.000000000000000000, 0.2500000000000000000, 0.5000000000000000000, 0.7500000000000000000, 1.000000000000000000 ),
 .UNSPECIFIED. ) ;
#22751 = CARTESIAN_POINT ( 'NONE',  ( 24.72545694048500309, -12.30753067676000079, 2.942917560468000460 ) ) ;
#22752 = CARTESIAN_POINT ( 'NONE',  ( 12.12912605232854801, -2.253778109953310516, 13.81740241363613642 ) ) ;
#22753 = CARTESIAN_POINT ( 'NONE',  ( 11.01927318630899855, -3.243547362524661359, 6.473854711408037588 ) ) ;
#22754 = CARTESIAN_POINT ( 'NONE',  ( 9.041999884715581359, -4.156896875802718050, -8.691999950321772417 ) ) ;
#22755 = CARTESIAN_POINT ( 'NONE',  ( 12.80505043854146940, -1.875000000000000444, -12.57541666120756396 ) ) ;
#22756 = ORIENTED_EDGE ( 'NONE', *, *, #8931, .T. ) ;
#22757 = CARTESIAN_POINT ( 'NONE',  ( 8.571413182548997867, -4.600000000000999734, 5.927302706106000407 ) ) ;
#22758 = AXIS2_PLACEMENT_3D ( 'NONE', #69081, #58246, #37269 ) ;
#22759 = CARTESIAN_POINT ( 'NONE',  ( 10.84393020684979980, -5.250000000000000000, -7.500000000000000000 ) ) ;
#22760 = CARTESIAN_POINT ( 'NONE',  ( 11.18220574173929904, -2.863826994586552210, -6.911917091190550089 ) ) ;
#22761 = VECTOR ( 'NONE', #56526, 1000.000000000000114 ) ;
#22762 = CARTESIAN_POINT ( 'NONE',  ( 10.76947109217999810, 5.100000000000000533, -6.152188490330000370 ) ) ;
#22763 = CARTESIAN_POINT ( 'NONE',  ( 1.562066629540999951, 3.411444769430000079, 1.578107062294999974 ) ) ;
#22764 = CARTESIAN_POINT ( 'NONE',  ( 1.771806799206333327, -3.408904368339104263, -0.9161175952574814874 ) ) ;
#22765 = CARTESIAN_POINT ( 'NONE',  ( 17.94368558191668939, -11.44474291118125109, 4.547324402811248056 ) ) ;
#22766 = CARTESIAN_POINT ( 'NONE',  ( 10.29378723213999969, 3.483632952461999999, 6.176337842045999338 ) ) ;
#22767 = CARTESIAN_POINT ( 'NONE',  ( 11.14595257254739913, 3.168263696564200149, 7.258104750172799768 ) ) ;
#22768 = CARTESIAN_POINT ( 'NONE',  ( 25.44994989278600173, -2.258942858049999725, -12.29419282279000036 ) ) ;
#22769 = CARTESIAN_POINT ( 'NONE',  ( 11.12964314679000033, -3.869080819553999628, -9.017146989745999264 ) ) ;
#22770 = CARTESIAN_POINT ( 'NONE',  ( 11.64452052416184102, 3.625675607363949116, -11.98888626465023854 ) ) ;
#22771 = DIRECTION ( 'NONE',  ( 0.000000000000000000, -0.7914851585299630399, 0.6111883865280813843 ) ) ;
#22772 = CARTESIAN_POINT ( 'NONE',  ( 8.736413463905998711, -3.915843685459630574, -8.382409559052598880 ) ) ;
#22773 = ORIENTED_EDGE ( 'NONE', *, *, #47710, .T. ) ;
#22774 = CARTESIAN_POINT ( 'NONE',  ( 8.944760841233000193, 4.990139824845000405, -9.121472988377998803 ) ) ;
#22775 = PRESENTATION_LAYER_ASSIGNMENT (  '', '', ( #44002 ) ) ;
#22776 = ORIENTED_EDGE ( 'NONE', *, *, #16412, .F. ) ;
#22777 = CARTESIAN_POINT ( 'NONE',  ( 18.17537916830627864, -2.421093501972792605, 13.68989611939600159 ) ) ;
#22778 = CARTESIAN_POINT ( 'NONE',  ( 10.12426357027499790, -2.745128867668000350, -7.742104041724699570 ) ) ;
#22779 = VERTEX_POINT ( 'NONE', #40717 ) ;
#22780 = CARTESIAN_POINT ( 'NONE',  ( 10.89835090130999973, 4.878966983716200190, 6.956352367771000189 ) ) ;
#22781 = CARTESIAN_POINT ( 'NONE',  ( 6.406992135612348704, -0.6435990042915642473, -0.9328669330701386819 ) ) ;
#22782 = LINE ( 'NONE', #32595, #35565 ) ;
#22783 = EDGE_CURVE ( 'NONE', #25073, #54494, #61517, .T. ) ;
#22784 = CARTESIAN_POINT ( 'NONE',  ( 11.08492721656000057, 3.668390701878999849, 5.558148445539999649 ) ) ;
#22785 = EDGE_CURVE ( 'NONE', #59750, #58906, #5701, .T. ) ;
#22786 = CARTESIAN_POINT ( 'NONE',  ( 8.610944094208999644, 5.100000000000000533, -6.571291218949999902 ) ) ;
#22787 = CARTESIAN_POINT ( 'NONE',  ( 27.64127793187000037, -13.87069231928999891, 4.225386915259999654 ) ) ;
#22788 = CARTESIAN_POINT ( 'NONE',  ( 17.71955056974170617, 0.7009231686363512903, -12.58048995873114073 ) ) ;
#22789 = CARTESIAN_POINT ( 'NONE',  ( 11.07336076184000007, -2.375557098086999996, -8.393541296344000813 ) ) ;
#22790 = CIRCLE ( 'NONE', #40657, 10.55000000000000426 ) ;
#22791 = CARTESIAN_POINT ( 'NONE',  ( 11.85979573085659844, -3.159987984332300215, -7.645349278262099979 ) ) ;
#22792 = VERTEX_POINT ( 'NONE', #58174 ) ;
#22793 = CARTESIAN_POINT ( 'NONE',  ( 10.75905508291875989, -2.921956017810039441, -5.082778843723144924 ) ) ;
#22794 = EDGE_LOOP ( 'NONE', ( #3449, #50289, #27944, #61218 ) ) ;
#22795 = CARTESIAN_POINT ( 'NONE',  ( 0.6325562371681370255, -0.7533924460659336964, -3.163756291279751220 ) ) ;
#22796 = ORIENTED_EDGE ( 'NONE', *, *, #45150, .F. ) ;
#22797 = CARTESIAN_POINT ( 'NONE',  ( 17.74540238971360750, -1.811773551562723350, -13.88227535917553546 ) ) ;
#22798 = CARTESIAN_POINT ( 'NONE',  ( 11.09999999999999964, -7.940796613052000019, 6.945951997396999644 ) ) ;
#22799 = CARTESIAN_POINT ( 'NONE',  ( 10.45746920027980487, -3.052701587494784263, 4.998914760967365645 ) ) ;
#22800 = CARTESIAN_POINT ( 'NONE',  ( 12.80505043854144276, -0.6600719421079697113, 13.91436771118226012 ) ) ;
#22801 = CARTESIAN_POINT ( 'NONE',  ( 12.64211699103822539, 1.896258653787259885, 13.78307619201600431 ) ) ;
#22802 = B_SPLINE_SURFACE_WITH_KNOTS ( 'NONE', 3, 3, ( 
 ( #28360, #12621, #44102, #49676 ),
 ( #32908, #65401, #44452, #33950 ),
 ( #43051, #59126, #17520, #55273 ),
 ( #12279, #38850, #398, #60173 ),
 ( #746, #32567, #59816, #53879 ),
 ( #22407, #1785, #33605, #5979 ) ),
 .UNSPECIFIED., .F., .F., .F.,
 ( 4, 1, 1, 4 ),
 ( 4, 4 ),
 ( 0.8990818836185000551, 0.9285714285714000704, 1.000000000000000000, 1.007603470889000041 ),
 ( -0.1835655572433000093, 1.183565557057000062 ),
 .UNSPECIFIED. ) ;
#22803 = CARTESIAN_POINT ( 'NONE',  ( 9.834153701540001791, -5.173926576843999925, 8.813045240277000758 ) ) ;
#22804 = CARTESIAN_POINT ( 'NONE',  ( 23.56666365135700403, -9.114812703021994977, -8.684180617873007435 ) ) ;
#22805 = CARTESIAN_POINT ( 'NONE',  ( 12.38211732427673972, 0.5935699150349409425, 13.98741755999924763 ) ) ;
#22806 = ORIENTED_EDGE ( 'NONE', *, *, #47320, .T. ) ;
#22807 = FACE_OUTER_BOUND ( 'NONE', #50030, .T. ) ;
#22808 = ADVANCED_FACE ( 'NONE', ( #67968 ), #42439, .F. ) ;
#22809 = CARTESIAN_POINT ( 'NONE',  ( 9.269471092183000138, 5.100000000000000533, -6.152188490330000370 ) ) ;
#22810 = CARTESIAN_POINT ( 'NONE',  ( 23.68231877376700112, -3.146678492433000240, -13.35242067877000061 ) ) ;
#22811 = CARTESIAN_POINT ( 'NONE',  ( 4.389380990064000621, -0.8613159615020000714, -0.6842232203413000091 ) ) ;
#22812 = AXIS2_PLACEMENT_3D ( 'NONE', #51289, #19472, #31347 ) ;
#22813 = EDGE_CURVE ( 'NONE', #3577, #44210, #20082, .T. ) ;
#22814 = B_SPLINE_SURFACE_WITH_KNOTS ( 'NONE', 3, 3, ( 
 ( #64158, #26428, #4737, #58577, #53683, #15926, #37258, #10680, #47759, #69069, #36920, #37595, #58236, #32028, #64495, #21175, #47410, #42506, #22203, #48782, #27119, #63814, #53341, #5443, #16615, #37940, #26780, #48093, #48434, #59262, #27456, #32703, #68714, #889, #64840 ),
 ( #16952, #59610, #11708, #26081, #15591, #1926, #60306, #6813, #12761, #60994, #33398, #29193, #55410, #55757, #34443, #2268, #38987, #50166, #23586, #44927, #18011, #27813, #28149, #66231, #66575, #28502, #43886, #18352, #23247, #39675, #13114, #49461, #18694, #1233, #55061 ),
 ( #7502, #2605, #1574, #28857, #44590, #22544, #39327, #54363, #7859, #50504, #23934, #22892, #49119, #45269, #65883, #60648, #44243, #40028, #65188, #49815, #6467, #17308, #7162, #34090, #61340, #13458, #38633, #59955, #12066, #33746, #54713, #65539, #17663, #12413, #57115 ),
 ( #67947, #34781, #51198, #14483, #62364, #62698, #3626, #40693, #50850, #20403, #20062, #24625, #25650, #56090, #46979, #8200, #35801, #14818, #24962, #46294, #56439, #63031, #19372, #9216, #45946, #67256, #62023, #51868, #14137, #30554, #3966, #25303, #67596, #29550, #8540 ) ),
 .UNSPECIFIED., .F., .F., .F.,
 ( 4, 4 ),
 ( 4, 1, 1, 1, 1, 1, 1, 1, 1, 1, 1, 1, 1, 1, 1, 1, 1, 1, 1, 1, 1, 1, 1, 1, 1, 1, 1, 1, 1, 1, 1, 1, 4 ),
 ( -0.1039370721279000015, 1.103937072127999963 ),
 ( 0.2233333333344000027, 0.2480800653604999795, 0.2728267973865999840, 0.2975735294126999886, 0.3223202614387999931, 0.3470669934649999733, 0.3718137254910999778, 0.3965604575171999824, 0.4213071895433000424, 0.4460539215694000470, 0.4708006535954999960, 0.4955473856216000006, 0.5202941176476999496, 0.5450408496738000652, 0.5697875816999000698, 0.5945343137260000743, 0.6192810457521999989, 0.6440277777783000035, 0.6687745098044000081, 0.6935212418305000126, 0.7182679738566000172, 0.7430147058827000217, 0.7677614379088000263, 0.7925081699349000308, 0.8172549019609999243, 0.8420016339870999289, 0.8667483660132000445, 0.8914950980394000801, 0.9162418300655000847, 0.9409885620915999782, 0.9657352941176999828, 0.9904820261437999873, 1.015228758169999912 ),
 .UNSPECIFIED. ) ;
#22815 = CARTESIAN_POINT ( 'NONE',  ( 9.137754719594999742, 2.319062457810000311, -7.919229449146000022 ) ) ;
#22816 = CARTESIAN_POINT ( 'NONE',  ( 17.77423364829699892, -3.297060500158999652, 11.83473586442999981 ) ) ;
#22817 = CARTESIAN_POINT ( 'NONE',  ( 10.27571314244999989, -5.689440078020999714, -7.562019725378000601 ) ) ;
#22818 = CARTESIAN_POINT ( 'NONE',  ( 8.314979508587148516, 2.649972834346558059, -7.499998738096613771 ) ) ;
#22819 = CARTESIAN_POINT ( 'NONE',  ( 10.53706676393821162, -5.286158710546942530, -7.027080267280065407 ) ) ;
#22820 = FILL_AREA_STYLE_COLOUR ( '', #61206 ) ;
#22821 = CARTESIAN_POINT ( 'NONE',  ( 4.500000484264000455, -12.99999951562999989, -2.124868964128000431E-09 ) ) ;
#22822 = DIRECTION ( 'NONE',  ( 0.9999999999990064614, 1.235604878859008709E-06, -6.784100806884041873E-07 ) ) ;
#22823 = DIRECTION ( 'NONE',  ( -1.000000000000000000, 0.000000000000000000, 1.554312234491000161E-14 ) ) ;
#22824 = CARTESIAN_POINT ( 'NONE',  ( 10.48280513895999988, 4.903310631086600146, -6.997844089834400094 ) ) ;
#22825 = CARTESIAN_POINT ( 'NONE',  ( 9.558671671056998775, 3.009461603020800347, -7.666361006367900188 ) ) ;
#22827 = CARTESIAN_POINT ( 'NONE',  ( 10.75590824504000054, -2.705649759953999922, 4.786982446041000649 ) ) ;
#22826 = CARTESIAN_POINT ( 'NONE',  ( 9.950367640780999778, -3.591293244209800228, 8.264635032075899446 ) ) ;
#22828 = CARTESIAN_POINT ( 'NONE',  ( 8.062814847549001129, -3.480055400096998319, 6.228346641557002350 ) ) ;
#22829 = ORIENTED_EDGE ( 'NONE', *, *, #67775, .F. ) ;
#22830 = EDGE_CURVE ( 'NONE', #16060, #21890, #20769, .T. ) ;
#22831 = CARTESIAN_POINT ( 'NONE',  ( 10.98146005378009882, 4.911671201000399556, 7.986817550794899745 ) ) ;
#22832 = AXIS2_PLACEMENT_3D ( 'NONE', #27452, #65183, #6458 ) ;
#22833 = CARTESIAN_POINT ( 'NONE',  ( 17.55505043854143565, 3.125000000000000000, -12.28374638332999602 ) ) ;
#22834 = CARTESIAN_POINT ( 'NONE',  ( 8.949822372493999367, 3.632306086542600010, 6.297150255604999636 ) ) ;
#22835 = CARTESIAN_POINT ( 'NONE',  ( 9.809470517051625649, 4.641899585206984646, -8.094556297950068924 ) ) ;
#22836 = CARTESIAN_POINT ( 'NONE',  ( 10.31668414895000119, -3.819528725844000494, 6.062183754159999438 ) ) ;
#22837 = CARTESIAN_POINT ( 'NONE',  ( 9.685974049303974098, -5.723140299379433138, 7.204273367287987284 ) ) ;
#22838 = CARTESIAN_POINT ( 'NONE',  ( 10.50851354018319128, 3.836375382625529795, 6.250000000000000888 ) ) ;
#22839 = VERTEX_POINT ( 'NONE', #5026 ) ;
#22840 = CONICAL_SURFACE ( 'NONE', #65263, 1.150082671338000129, 0.7854605808793618804 ) ;
#22841 = CARTESIAN_POINT ( 'NONE',  ( 9.254721904869999349, -3.124169273628900179, -7.991693846894699860 ) ) ;
#22842 = CARTESIAN_POINT ( 'NONE',  ( 9.729346873516668381, -4.163624617374463099, -6.249999999999998224 ) ) ;
#22843 = CARTESIAN_POINT ( 'NONE',  ( 5.368964071046000264, 1.564645433990000001, 0.3990237390554000063 ) ) ;
#22844 = DIRECTION ( 'NONE',  ( 0.000000000000000000, 1.000000000000000000, 0.000000000000000000 ) ) ;
#22845 = LINE ( 'NONE', #17963, #61868 ) ;
#22846 = CARTESIAN_POINT ( 'NONE',  ( 13.50018479229797208, -9.763984779744566467, -6.782114604289273707 ) ) ;
#22847 = CARTESIAN_POINT ( 'NONE',  ( 11.11718313518939816, 3.377550038693600154, -8.287087605365499599 ) ) ;
#22848 = DIRECTION ( 'NONE',  ( 0.9999999999999998890, -3.212307467389999644E-09, -9.519589316684998912E-09 ) ) ;
#22849 = CARTESIAN_POINT ( 'NONE',  ( 2.210247277619000084, 2.108360286353999413, -2.286637680308000409 ) ) ;
#22850 = CARTESIAN_POINT ( 'NONE',  ( 5.699999999999998401, 13.03908314205310681, 1.889202640492164242 ) ) ;
#22851 = ORIENTED_EDGE ( 'NONE', *, *, #16865, .T. ) ;
#22852 = DIRECTION ( 'NONE',  ( 0.000000000000000000, -1.000000000000000000, 0.000000000000000000 ) ) ;
#22853 = CARTESIAN_POINT ( 'NONE',  ( 12.08612513405891953, -0.09509187666555325713, -13.99968209810982067 ) ) ;
#22854 = CARTESIAN_POINT ( 'NONE',  ( 13.82809631267600103, -8.844623397843001555, -7.663863542600000578 ) ) ;
#22855 = CARTESIAN_POINT ( 'NONE',  ( 25.19967722607600180, -8.371103897856000842, -8.687405657236000778 ) ) ;
#22856 = LINE ( 'NONE', #65851, #28792 ) ;
#22857 = CARTESIAN_POINT ( 'NONE',  ( 9.856851002545999663, 2.832432432432000269, -6.822293592207000934 ) ) ;
#22858 = CARTESIAN_POINT ( 'NONE',  ( 10.23921655905618699, 2.650856495401566093, 7.263814070341827467 ) ) ;
#22859 = ORIENTED_EDGE ( 'NONE', *, *, #28984, .T. ) ;
#22860 = VECTOR ( 'NONE', #54910, 1000.000000000000000 ) ;
#22861 = CARTESIAN_POINT ( 'NONE',  ( 17.96968152693878551, 2.032227188856707389, -13.76161273592455103 ) ) ;
#22862 = ORIENTED_EDGE ( 'NONE', *, *, #40479, .T. ) ;
#22863 = FACE_OUTER_BOUND ( 'NONE', #39448, .T. ) ;
#22864 = CARTESIAN_POINT ( 'NONE',  ( 8.417495559623999313, -2.029110377978999846, 7.726994002375999315 ) ) ;
#22865 = CARTESIAN_POINT ( 'NONE',  ( 15.62410434383600055, 8.799879896029001003, 7.715564795277000343 ) ) ;
#22866 = PRODUCT_DEFINITION_FORMATION_WITH_SPECIFIED_SOURCE ( 'ANY', '', #13747, .NOT_KNOWN. ) ;
#22867 = EDGE_CURVE ( 'NONE', #39380, #19742, #18582, .T. ) ;
#22868 = CARTESIAN_POINT ( 'NONE',  ( 13.50006915090078152, -9.429349056561928677, -7.934633652400466808 ) ) ;
#22869 = EDGE_CURVE ( 'NONE', #19259, #29376, #53613, .T. ) ;
#22870 = CARTESIAN_POINT ( 'NONE',  ( 10.55569598648999907, -2.869047858956000230, -8.173387776112500447 ) ) ;
#22871 = SHAPE_REPRESENTATION ( 'O Ring Seal 1', ( #9676 ), #49917 ) ;
#22872 = CARTESIAN_POINT ( 'NONE',  ( 18.08719379937744165, 0.3285641700854472491, -12.69429818673162202 ) ) ;
#22873 = EDGE_CURVE ( 'NONE', #28388, #40655, #66116, .T. ) ;
#22874 = CARTESIAN_POINT ( 'NONE',  ( 10.18559687351566723, -2.907767014557174790, 8.129523725463618788 ) ) ;
#22875 = EDGE_LOOP ( 'NONE', ( #40081, #4384, #47645 ) ) ;
#22876 = CARTESIAN_POINT ( 'NONE',  ( 8.819055905797000605, 2.899999999999999911, -6.571291218949999902 ) ) ;
#22877 = CARTESIAN_POINT ( 'NONE',  ( 18.17052368435256682, -2.609308838451334100, -13.64962199044944491 ) ) ;
#22878 = CARTESIAN_POINT ( 'NONE',  ( 9.444964158775000840, 3.920043641733999884, -9.398198753036000497 ) ) ;
#22879 = VERTEX_POINT ( 'NONE', #10276 ) ;
#22880 = CARTESIAN_POINT ( 'NONE',  ( 10.99693586709999948, 2.980605808171000071, -6.418617723582000778 ) ) ;
#22881 = DIRECTION ( 'NONE',  ( 1.000000000000000000, 0.000000000000000000, 0.000000000000000000 ) ) ;
#22882 = ORIENTED_EDGE ( 'NONE', *, *, #56965, .F. ) ;
#22883 = CARTESIAN_POINT ( 'NONE',  ( 9.356038493598999750, 4.726907342723099426, 8.193143574899998782 ) ) ;
#22884 = CARTESIAN_POINT ( 'NONE',  ( 17.94092590763760242, -3.089486433945226374, -12.21536380989863524 ) ) ;
#22885 = CARTESIAN_POINT ( 'NONE',  ( 17.55505043854144631, 0.7192913403693005359, 12.57945229203838267 ) ) ;
#22886 = CARTESIAN_POINT ( 'NONE',  ( 16.13854177342199847, 3.630911166246999944, 11.92992564462999994 ) ) ;
#22887 = CARTESIAN_POINT ( 'NONE',  ( 23.60205915885299888, 2.338900754103997670, 12.00073634675999834 ) ) ;
#22888 = CARTESIAN_POINT ( 'NONE',  ( 9.079430433046999482, 3.262177192690499883, 7.955330044604899342 ) ) ;
#22889 = CARTESIAN_POINT ( 'NONE',  ( 8.719734573340000239, 3.777330902948500047, -8.352506367884300786 ) ) ;
#22890 = ORIENTED_EDGE ( 'NONE', *, *, #32833, .T. ) ;
#22891 = FACE_OUTER_BOUND ( 'NONE', #13875, .T. ) ;
#22892 = CARTESIAN_POINT ( 'NONE',  ( 10.90247028041000021, 4.554785930130000438, -6.081876607904999510 ) ) ;
#22893 = CARTESIAN_POINT ( 'NONE',  ( 18.38353273094886120, -11.69886204264012974, 4.474905155505553012 ) ) ;
#22894 = CARTESIAN_POINT ( 'NONE',  ( 12.42293806700074832, 2.994693046128884539, -13.55600569395198995 ) ) ;
#22895 = CARTESIAN_POINT ( 'NONE',  ( 9.861671671056999600, -5.261543809652999393, -7.711876388024100137 ) ) ;
#22896 = CARTESIAN_POINT ( 'NONE',  ( 25.40243967972899952, 3.096345258848000270, 11.38620991970000063 ) ) ;
#22897 = CARTESIAN_POINT ( 'NONE',  ( 17.95947766544255586, 0.4766231184928877984, 13.88900205690512735 ) ) ;
#22898 = CARTESIAN_POINT ( 'NONE',  ( 25.19966679887500050, -3.337966940464999865, 11.59330421545000078 ) ) ;
#22899 = ORIENTED_EDGE ( 'NONE', *, *, #23459, .F. ) ;
#22900 = ORIENTED_EDGE ( 'NONE', *, *, #58104, .F. ) ;
#22901 = CARTESIAN_POINT ( 'NONE',  ( 8.549914158773001205, 2.141799395716999843, -7.895788736628000848 ) ) ;
#22902 = CARTESIAN_POINT ( 'NONE',  ( 12.33073330760568176, -0.4072264708333818151, 13.89197624347111848 ) ) ;
#22903 = CARTESIAN_POINT ( 'NONE',  ( 12.43800705101901372, -0.5060514260813850917, -13.88760251447818206 ) ) ;
#22904 = CARTESIAN_POINT ( 'NONE',  ( 9.637133777480245911, -2.899999999999999911, -6.201439514950156884 ) ) ;
#22905 = DIRECTION ( 'NONE',  ( -0.000000000000000000, 1.000000000000000000, 0.000000000000000000 ) ) ;
#22906 = CARTESIAN_POINT ( 'NONE',  ( 8.604019353210000887, -5.165500668528999917, 8.645534272955000432 ) ) ;
#22907 = CARTESIAN_POINT ( 'NONE',  ( 25.37956771155745272, 8.342526067244204313, -8.311497089906559665 ) ) ;
#22909 = CARTESIAN_POINT ( 'NONE',  ( 23.59999445750599989, -13.22316420035999940, -4.267800004853000040 ) ) ;
#22908 = CARTESIAN_POINT ( 'NONE',  ( 8.753601108638063621, 2.714205948350784325, 7.027810827039986386 ) ) ;
#22910 = CARTESIAN_POINT ( 'NONE',  ( 8.736375959668992053, -5.159793961343003055, -6.817201505920002624 ) ) ;
#22911 = CARTESIAN_POINT ( 'NONE',  ( 12.10000000000000320, -4.874497702741446226, 7.130791426018634027 ) ) ;
#22912 = EDGE_CURVE ( 'NONE', #38413, #57550, #41117, .T. ) ;
#22913 = PRODUCT_DEFINITION_FORMATION_WITH_SPECIFIED_SOURCE ( 'ANY', '', #61747, .NOT_KNOWN. ) ;
#22914 = CARTESIAN_POINT ( 'NONE',  ( 8.715822372493999382, 3.750788346126100237, -8.315254653915399530 ) ) ;
#22915 = CARTESIAN_POINT ( 'NONE',  ( 17.77555300520474546, 0.5848996845204763595, 12.68186405703078989 ) ) ;
#22916 = CARTESIAN_POINT ( 'NONE',  ( 6.988896813636456429, -12.37529600717038214, -2.766866756147773998 ) ) ;
#22917 = EDGE_CURVE ( 'NONE', #62021, #15326, #14502, .T. ) ;
#22918 = CARTESIAN_POINT ( 'NONE',  ( 4.149992563291999836, -0.5234817089163712467, 1.947893036340041961 ) ) ;
#22919 = ORIENTED_EDGE ( 'NONE', *, *, #46261, .T. ) ;
#22921 = CARTESIAN_POINT ( 'NONE',  ( 11.01837338474678063, 3.735675910162961078, 8.333200082717626245 ) ) ;
#22920 = CARTESIAN_POINT ( 'NONE',  ( 7.903995559621998623, -2.095727472214000020, 8.056487497515000484 ) ) ;
#22922 = CARTESIAN_POINT ( 'NONE',  ( 8.763579719593998618, 4.815598936798999752, -8.835641302565999666 ) ) ;
#22923 = B_SPLINE_CURVE_WITH_KNOTS ( 'NONE', 3,
 ( #19859, #68771, #62837, #30695, #41190, #56920, #14955, #20545, #62160, #57953, #36280, #57596, #35938, #14619, #46434, #63176, #15304, #10052 ),
 .UNSPECIFIED., .F., .F.,
 ( 4, 2, 2, 2, 2, 2, 2, 2, 4 ),
 ( 0.000000000000000000, 0.1250000000000000000, 0.2500000000000000000, 0.3750000000000000000, 0.5000000000000000000, 0.6250000000000000000, 0.7500000000000000000, 0.8750000000000000000, 1.000000000000000000 ),
 .UNSPECIFIED. ) ;
#22924 = CARTESIAN_POINT ( 'NONE',  ( 12.66121447289699553, -1.891428313113427961, 13.78385349382386060 ) ) ;
#22925 = DIRECTION ( 'NONE',  ( 1.000000000000000000, 0.000000000000000000, 0.000000000000000000 ) ) ;
#22926 = CARTESIAN_POINT ( 'NONE',  ( 0.3597486600377999832, -1.720643726402999896, -3.153834707638000001 ) ) ;
#22927 = VECTOR ( 'NONE', #33946, 1000.000000000000000 ) ;
#22928 = DIRECTION ( 'NONE',  ( -1.000000000000000000, 0.000000000000000000, 0.000000000000000000 ) ) ;
#22929 = CARTESIAN_POINT ( 'NONE',  ( 2.542837364878999917, -1.685321747336000264, -2.982366387278999831 ) ) ;
#22930 = ORIENTED_EDGE ( 'NONE', *, *, #65099, .F. ) ;
#22931 = CARTESIAN_POINT ( 'NONE',  ( 12.11457469949690591, 0.2196334679052245331, -12.59809060309703277 ) ) ;
#22932 = CARTESIAN_POINT ( 'NONE',  ( 18.29991931957795259, -1.031823913341759950E-13, -12.32514597914127563 ) ) ;
#22933 = CARTESIAN_POINT ( 'NONE',  ( 24.26256940594572242, -12.27508747190780625, -3.289098842859198069 ) ) ;
#22934 = CARTESIAN_POINT ( 'NONE',  ( 7.897954719591000483, 3.608525622520999843, 5.913376237674000002 ) ) ;
#22935 = ORIENTED_EDGE ( 'NONE', *, *, #21208, .T. ) ;
#22936 = CARTESIAN_POINT ( 'NONE',  ( 5.881244644296000246, 1.024801514603000063, 1.247845015360000032 ) ) ;
#22937 = CARTESIAN_POINT ( 'NONE',  ( 7.540310841227999994, 5.150153908582999485, -6.706147112165000479 ) ) ;
#22939 = DIRECTION ( 'NONE',  ( 0.000000000000000000, 0.000000000000000000, -1.000000000000000000 ) ) ;
#22938 = DIRECTION ( 'NONE',  ( 1.000000000000000000, 0.000000000000000000, 0.000000000000000000 ) ) ;
#22940 = FACE_OUTER_BOUND ( 'NONE', #27798, .T. ) ;
#22941 = ORIENTED_EDGE ( 'NONE', *, *, #2991, .F. ) ;
#22942 = CARTESIAN_POINT ( 'NONE',  ( 11.09999999999999964, -2.700000000000000178, 5.160242730440000258 ) ) ;
#22943 = PLANE ( 'NONE',  #30572 ) ;
#22944 = ORIENTED_EDGE ( 'NONE', *, *, #27728, .T. ) ;
#22945 = CARTESIAN_POINT ( 'NONE',  ( -2.444943969992999916E-05, 2.899969545325999931, 0.000000000000000000 ) ) ;
#22946 = CARTESIAN_POINT ( 'NONE',  ( 15.95436146409600120, 3.609635682399999546, 11.22945631340000006 ) ) ;
#22947 = CARTESIAN_POINT ( 'NONE',  ( 18.18005725403618911, 0.009762789003249052952, -13.90000041479088289 ) ) ;
#22948 = ORIENTED_EDGE ( 'NONE', *, *, #20743, .T. ) ;
#22949 = CARTESIAN_POINT ( 'NONE',  ( -0.2999999999999999889, -0.5773502691895999739, 1.000000000000000000 ) ) ;
#22950 = EDGE_CURVE ( 'NONE', #56062, #41132, #40304, .T. ) ;
#22951 = CARTESIAN_POINT ( 'NONE',  ( 18.30017264560541790, 1.838307228690110540, 11.74271423064807962 ) ) ;
#22952 = CARTESIAN_POINT ( 'NONE',  ( 10.13559687351666483, -2.907767014557175678, 8.129523725463618788 ) ) ;
#22953 = CARTESIAN_POINT ( 'NONE',  ( 8.793505787816332742, -5.100000000000000533, 6.515557531858333640 ) ) ;
#22954 = EDGE_CURVE ( 'NONE', #33345, #64314, #58560, .T. ) ;
#22955 = DIRECTION ( 'NONE',  ( 1.000000000000000000, 1.736057635237000010E-14, 9.258974054599999947E-14 ) ) ;
#22956 = ORIENTED_EDGE ( 'NONE', *, *, #49188, .F. ) ;
#22957 = CARTESIAN_POINT ( 'NONE',  ( 12.80505043854146940, -1.760910691117821614, -12.47634535983622683 ) ) ;
#22958 = EDGE_CURVE ( 'NONE', #29557, #61812, #26874, .T. ) ;
#22959 = CARTESIAN_POINT ( 'NONE',  ( 23.52062907214899923, -13.48732121207000034, -4.206199075609999838 ) ) ;
#22960 = CARTESIAN_POINT ( 'NONE',  ( 9.321001730958842657, -4.768205771526717207, -6.500403846372137195 ) ) ;
#22961 = COLOUR_RGB ( '', 0.31764706, 0.68627451, 0.89019608) ;
#22962 = FACE_OUTER_BOUND ( 'NONE', #67394, .T. ) ;
#22963 = ORIENTED_EDGE ( 'NONE', *, *, #29463, .T. ) ;
#22964 = B_SPLINE_SURFACE_WITH_KNOTS ( 'NONE', 3, 3, ( 
 ( #47348, #67970, #16208, #25326, #63752, #15531, #52237, #31960, #32308, #52583, #48029, #41754, #37196, #41413, #68653, #20084, #62719, #26018, #20771, #31611, #135, #21449, #10278, #57476, #26367, #47004, #10618, #9583, #5378, #63054, #4676, #42443, #30927, #4338, #68306, #15182, #26716, #42785, #36505, #58176, #63408, #47693, #57827, #69005, #21117, #36856, #15864, #64094, #37883, #59895, #1515, #11306, #5715, #53956, #44531, #6059, #17603, #6404, #65825, #65479, #7103, #16894, #27396, #65127, #28441, #64432, #22834 ),
 ( #43827, #59203, #27058, #27752, #44180, #28089, #38223, #48725, #60592, #49755, #17248, #55002, #6750, #38928, #22485, #54655, #32986, #49064, #826, #48371, #16554, #17951, #49403, #59551, #60250, #12352, #33685, #53618, #22143, #33340, #479, #1865, #39269, #11651, #32644, #12698, #38571, #23184, #21795, #43128, #43483, #64781, #54302, #1171, #12002, #56733, #19312, #67201, #35069, #29137, #3240, #23528, #24567, #2214, #3572, #55348, #50108, #60939, #7445, #67543, #66174, #39968, #13055, #50445, #24215, #18294, #28795 ),
 ( #44870, #8487, #34382, #45890, #62310, #40636, #45558, #29833, #24905, #40987, #14082, #66864, #46238, #13401, #61971, #35407, #8827, #18638, #55700, #39614, #18977, #56385, #30170, #51138, #51475, #2547, #50799, #34724, #19666, #34036, #29492, #7798, #23874, #61285, #45213, #66515, #8143, #56035, #2891, #40302, #61623, #13736, #15789, #57398, #42371, #47266, #58435, #9853, #4259, #25938, #26288, #36083, #68226, #57744, #9163, #26638, #14427, #4950, #68571, #62640, #63672, #42708, #41672, #5296, #47614, #37120, #46923 ),
 ( #25245, #31533, #67890, #10539, #4602, #68924, #52504, #9503, #30845, #46583, #20008, #58098, #41333, #52853, #35744, #21038, #20694, #10201, #47955, #21374, #31880, #42023, #54, #62978, #53196, #57063, #30500, #20345, #14766, #52156, #63324, #15453, #51813, #36776, #3911, #25597, #31199, #15105, #36427, #38846, #59465, #16132, #54575, #48643, #48291, #58777, #38138, #12275, #32231, #11916, #65398, #10886, #17517, #37801, #22749, #27667, #60170, #11562, #53877, #6318, #6671, #16470, #743, #32906, #53544, #7022, #64013 ) ),
 .UNSPECIFIED., .F., .F., .F.,
 ( 4, 4 ),
 ( 4, 1, 1, 1, 1, 1, 1, 1, 1, 1, 1, 1, 1, 1, 1, 1, 1, 1, 1, 1, 1, 1, 1, 1, 1, 1, 1, 1, 1, 1, 1, 1, 1, 1, 1, 1, 1, 1, 1, 1, 1, 1, 1, 1, 1, 1, 1, 1, 1, 1, 1, 1, 1, 1, 1, 1, 1, 1, 1, 1, 1, 1, 1, 1, 4 ),
 ( -0.02000000000000000042, 1.020000000000000018 ),
 ( -0.02000000000000000042, -0.003749999999999999861, 0.01250000000000000069, 0.02875000000000000125, 0.04499999999999999833, 0.06124999999999999889, 0.07749999999999999944, 0.09375000000000000000, 0.1100000000000000006, 0.1262500000000000011, 0.1424999999999999878, 0.1587500000000000022, 0.1749999999999999889, 0.1912500000000000033, 0.2074999999999999900, 0.2237500000000000044, 0.2399999999999999911, 0.2562499999999999778, 0.2725000000000000200, 0.2887500000000000067, 0.3049999999999999933, 0.3212499999999999800, 0.3375000000000000222, 0.3537500000000000089, 0.3699999999999999956, 0.3862499999999999822, 0.4025000000000000244, 0.4187500000000000111, 0.4349999999999999978, 0.4512499999999999845, 0.4675000000000000266, 0.4837500000000000133, 0.5000000000000000000, 0.5162499999999999867, 0.5324999999999999734, 0.5487499999999999600, 0.5649999999999999467, 0.5812500000000000444, 0.5975000000000000311, 0.6137500000000000178, 0.6300000000000000044, 0.6462499999999999911, 0.6624999999999999778, 0.6787499999999999645, 0.6949999999999999512, 0.7112500000000000488, 0.7275000000000000355, 0.7437500000000000222, 0.7600000000000000089, 0.7762499999999999956, 0.7924999999999999822, 0.8087499999999999689, 0.8249999999999999556, 0.8412500000000000533, 0.8575000000000000400, 0.8737500000000000266, 0.8900000000000000133, 0.9062500000000000000, 0.9224999999999999867, 0.9387499999999999734, 0.9549999999999999600, 0.9712499999999999467, 0.9875000000000000444, 1.003749999999999920, 1.020000000000000018 ),
 .UNSPECIFIED. ) ;
#22965 = FACE_OUTER_BOUND ( 'NONE', #45531, .T. ) ;
#22966 = AXIS2_PLACEMENT_3D ( 'NONE', #43908, #65210, #38653 ) ;
#22967 = CARTESIAN_POINT ( 'NONE',  ( 16.09992084546400193, -8.991497430826001391, -8.719551690569000257 ) ) ;
#22968 = DIRECTION ( 'NONE',  ( 1.000000000000000000, 0.000000000000000000, 0.000000000000000000 ) ) ;
#22969 = CARTESIAN_POINT ( 'NONE',  ( 5.000030787343000327, 1.057581170753191913, 1.834918991542626943 ) ) ;
#22970 = DIRECTION ( 'NONE',  ( 1.000000000000000000, 0.000000000000000000, 0.000000000000000000 ) ) ;
#22971 = LINE ( 'NONE', #2002, #6285 ) ;
#22972 = CARTESIAN_POINT ( 'NONE',  ( 17.94181191902913852, -1.871597878487309297, 12.46022310877027195 ) ) ;
#22973 = ORIENTED_EDGE ( 'NONE', *, *, #18227, .F. ) ;
#22974 = CARTESIAN_POINT ( 'NONE',  ( 11.13746005378019888, -2.838900981960999825, -6.879992063401499713 ) ) ;
#22975 = VERTEX_POINT ( 'NONE', #41751 ) ;
#22976 = ADVANCED_FACE ( 'NONE', ( #63052 ), #35727, .F. ) ;
#22977 = CARTESIAN_POINT ( 'NONE',  ( 11.35563386585000067, -12.29158615273999899, -1.473028240582999970 ) ) ;
#22978 = VECTOR ( 'NONE', #12980, 1000.000000000000000 ) ;
#22979 = CARTESIAN_POINT ( 'NONE',  ( 9.246064158776000852, 5.200883864107000321, -6.027780766890000308 ) ) ;
#22980 = CARTESIAN_POINT ( 'NONE',  ( 2.754660504490999973, 1.495576858855999891, -3.030426860594000349 ) ) ;
#22981 = CARTESIAN_POINT ( 'NONE',  ( 10.06728329455999926, -4.192861215955000276, -5.985050974557999837 ) ) ;
#22982 = VECTOR ( 'NONE', #63886, 1000.000000000000000 ) ;
#22983 = LINE ( 'NONE', #44331, #55159 ) ;
#22984 = CARTESIAN_POINT ( 'NONE',  ( 23.85163940690300066, 13.16376717049999989, 3.535832831874000437 ) ) ;
#22985 = CARTESIAN_POINT ( 'NONE',  ( 11.54292372906208897, 5.032542535543790052, 6.730835578941808173 ) ) ;
#22986 = ORIENTED_EDGE ( 'NONE', *, *, #25174, .F. ) ;
#22987 = DIRECTION ( 'NONE',  ( 0.000000000000000000, 0.2588190451024934280, -0.9659258262890756397 ) ) ;
#22988 = CARTESIAN_POINT ( 'NONE',  ( 11.00180110216400031, -4.856393875115199599, 8.023010882787499298 ) ) ;
#22989 = CARTESIAN_POINT ( 'NONE',  ( 10.96080777006000062, 2.054568739078000306, 7.810084630238000258 ) ) ;
#22990 = CARTESIAN_POINT ( 'NONE',  ( 25.59994555223599733, 8.527741194213000142, 7.260611644044000279 ) ) ;
#22991 = CARTESIAN_POINT ( 'NONE',  ( 10.40769129028899975, 3.110563525881361535, -8.413289387078531689 ) ) ;
#22992 = CARTESIAN_POINT ( 'NONE',  ( 11.09999999999999964, 2.646159083949000124, 6.745271721726000536 ) ) ;
#22993 = CARTESIAN_POINT ( 'NONE',  ( 11.28949010443639978, 5.000675062740000065, -7.574834962826040297 ) ) ;
#22994 = CARTESIAN_POINT ( 'NONE',  ( 10.35791745203637326, 3.287858841512209640, 9.125997197693916263 ) ) ;
#22995 = CARTESIAN_POINT ( 'NONE',  ( 10.46755864497999866, 4.898932057185599653, -8.204026508301600629 ) ) ;
#22996 = CARTESIAN_POINT ( 'NONE',  ( 24.63807785274300244, -8.801136568184000808, -9.346917357783997460 ) ) ;
#22997 = CARTESIAN_POINT ( 'NONE',  ( 23.66463366901000143, -10.00963801616000026, 9.517991018344002185 ) ) ;
#22998 = CARTESIAN_POINT ( 'NONE',  ( 11.56566386073000174, -3.232480401124999680, 11.43828361194000109 ) ) ;
#22999 = ADVANCED_FACE ( 'NONE', ( #40462 ), #61792, .T. ) ;
#23000 = ORIENTED_EDGE ( 'NONE', *, *, #564, .F. ) ;
#23001 = CARTESIAN_POINT ( 'NONE',  ( 7.667605646792000407, -5.638700495537999124, 8.266402903491000487 ) ) ;
#23002 = CARTESIAN_POINT ( 'NONE',  ( 9.837156140204001531, -5.811247906278000031, -7.978055797018001272 ) ) ;
#23003 = CARTESIAN_POINT ( 'NONE',  ( 18.20194470744735327, 2.188139888162242475, 13.82794850388582653 ) ) ;
#23004 = CARTESIAN_POINT ( 'NONE',  ( 24.35365242081699932, -3.253466243134998326, 12.21167519469000240 ) ) ;
#23005 = CARTESIAN_POINT ( 'NONE',  ( 10.69041504065829962, -2.975441626403999784, -6.736065107693399945 ) ) ;
#23006 = B_SPLINE_CURVE_WITH_KNOTS ( 'NONE', 3,
 ( #67745, #10404, #68784, #36640, #57963 ),
 .UNSPECIFIED., .F., .F.,
 ( 4, 1, 4 ),
 ( 0.000000000000000000, 0.5000000000000000000, 1.000000000000000000 ),
 .UNSPECIFIED. ) ;
#23007 = ORIENTED_EDGE ( 'NONE', *, *, #14957, .F. ) ;
#23008 = FACE_OUTER_BOUND ( 'NONE', #50987, .T. ) ;
#23009 = CARTESIAN_POINT ( 'NONE',  ( 8.116920280410999666, 5.773189794777000117, 7.141495931231999883 ) ) ;
#23010 = CONICAL_SURFACE ( 'NONE', #62091, 2.074968475931999734, 0.7853828752794411727 ) ;
#23012 = CARTESIAN_POINT ( 'NONE',  ( 0.6472501130994691154, 1.225110017767339077, 3.318548330844829142 ) ) ;
#23011 = CARTESIAN_POINT ( 'NONE',  ( 9.292835841232999883, 5.200883864107000321, -6.027780766890000308 ) ) ;
#23013 = CARTESIAN_POINT ( 'NONE',  ( 11.58810207955109917, 3.203462856645999945, -7.174999999999999822 ) ) ;
#23014 = ORIENTED_EDGE ( 'NONE', *, *, #45342, .T. ) ;
#23015 = CARTESIAN_POINT ( 'NONE',  ( 25.29995758267499895, -11.13046986584000031, -3.427500733308000314 ) ) ;
#23017 = CARTESIAN_POINT ( 'NONE',  ( 17.78650313621487200, -3.080655036186602747, -13.53295239609827050 ) ) ;
#23016 = B_SPLINE_CURVE_WITH_KNOTS ( 'NONE', 3,
 ( #33596, #27659, #16463, #48979, #54213, #11911 ),
 .UNSPECIFIED., .F., .F.,
 ( 4, 2, 4 ),
 ( 0.000000000000000000, 0.5000000000000000000, 1.000000000000000000 ),
 .UNSPECIFIED. ) ;
#23018 = CARTESIAN_POINT ( 'NONE',  ( 11.46179707368349909, 3.501542828836900156, 8.370914060838998694 ) ) ;
#23019 = CARTESIAN_POINT ( 'NONE',  ( 11.18706725482999964, -3.186788126275999833, 6.232699537089999353 ) ) ;
#23020 = CARTESIAN_POINT ( 'NONE',  ( 8.212416242268998801, 3.104180772687998857, 6.104177153569003700 ) ) ;
#23021 = VERTEX_POINT ( 'NONE', #18464 ) ;
#23022 = CARTESIAN_POINT ( 'NONE',  ( 8.193904585095999948, -3.399974355387999747, 6.145257543266000155 ) ) ;
#23024 = CARTESIAN_POINT ( 'NONE',  ( 1.261390132541624576, -3.499999999999999556, -0.4581489286485119772 ) ) ;
#23023 = CARTESIAN_POINT ( 'NONE',  ( 12.08926246520500136, -11.62544123506999938, 4.252388861798999997 ) ) ;
#23025 = CARTESIAN_POINT ( 'NONE',  ( 8.093307509540114353, -4.415759437142675381, 5.811247418746839699 ) ) ;
#23026 = CARTESIAN_POINT ( 'NONE',  ( 9.939319226872999735, -2.638101016021999978, 6.328632621050000573 ) ) ;
#23028 = CARTESIAN_POINT ( 'NONE',  ( 23.58312595175700466, 2.942241311944000071, 13.62812806436000024 ) ) ;
#23027 = VECTOR ( 'NONE', #45813, 1000.000000000000000 ) ;
#23029 = CARTESIAN_POINT ( 'NONE',  ( 10.25929229006299970, -3.012566816337000297, 8.073332500201798823 ) ) ;
#23030 = EDGE_LOOP ( 'NONE', ( #19148, #8961, #35301, #3756 ) ) ;
#23031 = CARTESIAN_POINT ( 'NONE',  ( 23.78808826920356978, -9.744861260223199650, 9.430304542841936311 ) ) ;
#23032 = CARTESIAN_POINT ( 'NONE',  ( 10.87457053952200070, -4.448306506338299826, 8.548957288282998945 ) ) ;
#23033 = VERTEX_POINT ( 'NONE', #66690 ) ;
#23034 = CARTESIAN_POINT ( 'NONE',  ( 10.13351354018233330, -2.750000000000000000, 7.336375382625529795 ) ) ;
#23035 = ORIENTED_EDGE ( 'NONE', *, *, #55487, .T. ) ;
#23036 = CARTESIAN_POINT ( 'NONE',  ( 9.690635841230999858, 2.927176851028000293, -5.932007155957999878 ) ) ;
#23037 = CARTESIAN_POINT ( 'NONE',  ( 23.55360001510700130, 13.39037920836000062, -4.197254571800000278 ) ) ;
#23038 = CARTESIAN_POINT ( 'NONE',  ( 12.70216005901004586, 1.883184384472671891, -12.57411343304723594 ) ) ;
#23039 = EDGE_CURVE ( 'NONE', #62256, #4104, #30002, .T. ) ;
#23040 = CARTESIAN_POINT ( 'NONE',  ( 10.94125056272499918, -2.966599088466999934, 7.484684486284700178 ) ) ;
#23041 = EDGE_CURVE ( 'NONE', #28824, #18161, #68228, .T. ) ;
#23042 = CARTESIAN_POINT ( 'NONE',  ( 23.58888755872254706, 2.922214055433252522, 13.61647863770148703 ) ) ;
#23043 = ORIENTED_EDGE ( 'NONE', *, *, #55635, .T. ) ;
#23044 = CARTESIAN_POINT ( 'NONE',  ( 7.662254440376999653, -2.688354259407999880, 8.140021027181001401 ) ) ;
#23045 = DIRECTION ( 'NONE',  ( -1.000000000000000000, 0.000000000000000000, 0.000000000000000000 ) ) ;
#23046 = ORIENTED_EDGE ( 'NONE', *, *, #47435, .T. ) ;
#23047 = CARTESIAN_POINT ( 'NONE',  ( 10.06646012162292969, -2.291509473315214596, -8.026256863629807725 ) ) ;
#23048 = CARTESIAN_POINT ( 'NONE',  ( 10.71918447801630059, 5.140463864104999558, 7.525145395936648995 ) ) ;
#23049 = CARTESIAN_POINT ( 'NONE',  ( 11.02419555961999897, -2.407899345275000158, -8.439548421502999886 ) ) ;
#23050 = FACE_OUTER_BOUND ( 'NONE', #19834, .T. ) ;
#23051 = CARTESIAN_POINT ( 'NONE',  ( 7.591358119366002022, 4.587777998512997613, 6.499953102827994655 ) ) ;
#23052 = CARTESIAN_POINT ( 'NONE',  ( 8.121343566036618000, -3.646810248691512601, 8.848457998379473111 ) ) ;
#23053 = CARTESIAN_POINT ( 'NONE',  ( 12.32706758141029368, -2.902815230603663643, -13.57967619870183640 ) ) ;
#23054 = CARTESIAN_POINT ( 'NONE',  ( 18.15598060823833038, 0.1720826094844778720, -12.69843621396829292 ) ) ;
#23055 = CARTESIAN_POINT ( 'NONE',  ( 6.966665954281333839, -12.09896498756869576, 3.276379939815991627 ) ) ;
#23056 = CARTESIAN_POINT ( 'NONE',  ( 10.25149413291699929, -2.962184842772000337, -7.026470926762800495 ) ) ;
#23057 = CARTESIAN_POINT ( 'NONE',  ( 8.187142219590999304, 4.968147183437999992, 5.971792472497999604 ) ) ;
#23058 = VERTEX_POINT ( 'NONE', #13229 ) ;
#23059 = B_SPLINE_CURVE_WITH_KNOTS ( 'NONE', 3,
 ( #27586, #17081, #44714, #60434 ),
 .UNSPECIFIED., .F., .F.,
 ( 4, 4 ),
 ( 0.000000000000000000, 1.000000000000000000 ),
 .UNSPECIFIED. ) ;
#23060 = EDGE_CURVE ( 'NONE', #26251, #30301, #43587, .T. ) ;
#23061 = VECTOR ( 'NONE', #30967, 1000.000000000000114 ) ;
#23062 = DIRECTION ( 'NONE',  ( 1.000000000000000000, 0.000000000000000000, 0.000000000000000000 ) ) ;
#23063 = CARTESIAN_POINT ( 'NONE',  ( 9.705773468360421319, 5.100000000000000533, -6.304440313841762844 ) ) ;
#23064 = CARTESIAN_POINT ( 'NONE',  ( 11.80427293869800032, 12.43391773449000048, 1.801004847141999932 ) ) ;
#23065 = CARTESIAN_POINT ( 'NONE',  ( 23.55780568386700224, -3.266395970825999751, 13.70080015052999833 ) ) ;
#23066 = EDGE_CURVE ( 'NONE', #31174, #66219, #30222, .T. ) ;
#23067 = CARTESIAN_POINT ( 'NONE',  ( 17.80610932905893407, 1.927548246225502471, 12.56666212246289582 ) ) ;
#23068 = CARTESIAN_POINT ( 'NONE',  ( 10.96499058814000094, 5.558059231066999395, 4.905737858409000118 ) ) ;
#23069 = CARTESIAN_POINT ( 'NONE',  ( 10.83668832355999889, 4.288537082977999404, 9.448742031664000507 ) ) ;
#23070 = AXIS2_PLACEMENT_3D ( 'NONE', #48047, #21467, #495 ) ;
#23071 = CARTESIAN_POINT ( 'NONE',  ( 9.828216720588628164, -3.237060173287368503, 7.071683423462644669 ) ) ;
#23072 = CARTESIAN_POINT ( 'NONE',  ( 8.924662153698962541, -5.350575487761723537, 7.500021879703682615 ) ) ;
#23073 = ORIENTED_EDGE ( 'NONE', *, *, #37864, .T. ) ;
#23074 = CARTESIAN_POINT ( 'NONE',  ( 12.15423239032309866, -2.797846099084075000, 12.28544569950199516 ) ) ;
#23075 = CARTESIAN_POINT ( 'NONE',  ( 10.28622949779699880, -3.519000825516800379, -8.221351791991999391 ) ) ;
#23076 = CARTESIAN_POINT ( 'NONE',  ( 11.09999999999999964, -4.000000000000000000, 7.500000000000000000 ) ) ;
#23077 = APPLICATION_CONTEXT ( 'automotive_design' ) ;
#23078 = CARTESIAN_POINT ( 'NONE',  ( 1.700000000000000178, 0.000000000000000000, 0.000000000000000000 ) ) ;
#23079 = AXIS2_PLACEMENT_3D ( 'NONE', #33776, #13490, #65915 ) ;
#23080 = CARTESIAN_POINT ( 'NONE',  ( 11.13349010443639919, 5.274453806861999716, -7.595309363461700158 ) ) ;
#23081 = ORIENTED_EDGE ( 'NONE', *, *, #16865, .F. ) ;
#23082 = CARTESIAN_POINT ( 'NONE',  ( 12.41154142318501385, -0.6042324041877022989, 12.58550538354983672 ) ) ;
#23083 = CARTESIAN_POINT ( 'NONE',  ( 9.266948341230998309, 3.049618631524000367, 6.392542946894000266 ) ) ;
#23084 = CARTESIAN_POINT ( 'NONE',  ( 9.843732751558000871, 4.115124343450999866, 9.466620196856998959 ) ) ;
#23085 = CARTESIAN_POINT ( 'NONE',  ( 12.47303194318975450, 3.029615900428510145, 12.31225512782603282 ) ) ;
#23086 = VERTEX_POINT ( 'NONE', #35236 ) ;
#23087 = CARTESIAN_POINT ( 'NONE',  ( 9.925639158771000226, 4.357364160690000432, -9.282962013144999247 ) ) ;
#23088 = CARTESIAN_POINT ( 'NONE',  ( 10.27195525820100031, 3.879327850572200198, -6.227697122196000024 ) ) ;
#23089 = LINE ( 'NONE', #43039, #33815 ) ;
#23091 = CARTESIAN_POINT ( 'NONE',  ( 24.30001685126999789, 8.938702716825000394, -8.938676159935001309 ) ) ;
#23090 = DIRECTION ( 'NONE',  ( 0.9925497095595060548, 0.000000000000000000, 0.1218403629892008122 ) ) ;
#23092 = CARTESIAN_POINT ( 'NONE',  ( 10.64124205625000030, -4.360201998293100623, 6.562398383267799673 ) ) ;
#23093 = CARTESIAN_POINT ( 'NONE',  ( 10.30903300763299946, -3.402282662142699809, -8.126922218169600143 ) ) ;
#23094 = VERTEX_POINT ( 'NONE', #8993 ) ;
#23095 = CARTESIAN_POINT ( 'NONE',  ( 1.973021089241999704, -0.2083462584559999942, 3.419270530009000275 ) ) ;
#23096 = LINE ( 'NONE', #27663, #13258 ) ;
#23097 = CARTESIAN_POINT ( 'NONE',  ( 5.000000000000000000, 0.6769230769231000533, 2.665384615385000266 ) ) ;
#23098 = CARTESIAN_POINT ( 'NONE',  ( 18.20569531736705216, 2.110314541875505157, -12.42277286985108731 ) ) ;
#23099 = CARTESIAN_POINT ( 'NONE',  ( 24.46225079093600385, -12.39903786166000010, 3.098987673017999711 ) ) ;
#23100 = CARTESIAN_POINT ( 'NONE',  ( 12.48119050255588292, -1.864280969780530928, 13.87532308892432553 ) ) ;
#23101 = CARTESIAN_POINT ( 'NONE',  ( 10.97145237372900084, -3.956267952212243255, 6.225919055146349912 ) ) ;
#23102 = DIRECTION ( 'NONE',  ( 1.000000000000000000, 0.000000000000000000, 0.000000000000000000 ) ) ;
#23103 = CARTESIAN_POINT ( 'NONE',  ( 12.99046541331000171, -12.43411100708999939, -1.799680151465999911 ) ) ;
#23104 = VERTEX_POINT ( 'NONE', #40809 ) ;
#23105 = CARTESIAN_POINT ( 'NONE',  ( 7.385833333331250472, 2.685136886497773379, -7.146640356114973613 ) ) ;
#23106 = DIRECTION ( 'NONE',  ( 0.000000000000000000, 0.1862490057674050514, 0.9825025739664263735 ) ) ;
#23107 = DIRECTION ( 'NONE',  ( 0.000000000000000000, -1.000000000000000000, 0.000000000000000000 ) ) ;
#23108 = CIRCLE ( 'NONE', #2998, 1.000000000000000444 ) ;
#23109 = DIRECTION ( 'NONE',  ( 0.000000000000000000, 0.000000000000000000, -1.000000000000000000 ) ) ;
#23110 = LINE ( 'NONE', #44463, #37681 ) ;
#23111 = ORIENTED_EDGE ( 'NONE', *, *, #47998, .F. ) ;
#23112 = CARTESIAN_POINT ( 'NONE',  ( 10.84419170916004660, 2.685373094371836356, -7.853312882625375302 ) ) ;
#23113 = B_SPLINE_CURVE_WITH_KNOTS ( 'NONE', 3,
 ( #42877, #54051, #26110, #4768 ),
 .UNSPECIFIED., .F., .F.,
 ( 4, 4 ),
 ( 0.000000000000000000, 1.000000000000000000 ),
 .UNSPECIFIED. ) ;
#23114 = CARTESIAN_POINT ( 'NONE',  ( 14.70000000000000107, 9.329726667597000755, 8.204053922562998480 ) ) ;
#23115 = CARTESIAN_POINT ( 'NONE',  ( 10.68362359175999998, 2.603561947343000060, 7.762063351517999976 ) ) ;
#23116 = CARTESIAN_POINT ( 'NONE',  ( 10.92441504065829960, 4.694414232677499577, 8.017771632862299214 ) ) ;
#23117 = CARTESIAN_POINT ( 'NONE',  ( 7.105195101234886401, 5.342010355555824930, -7.330391889570061714 ) ) ;
#23118 = CARTESIAN_POINT ( 'NONE',  ( 10.46297944037999983, -3.993164663709000362, -6.140164943008000087 ) ) ;
#23119 = AXIS2_PLACEMENT_3D ( 'NONE', #48963, #42353, #11894 ) ;
#23120 = CARTESIAN_POINT ( 'NONE',  ( 18.27990784067586105, -0.1916560647366354619, -13.99999316327169829 ) ) ;
#23121 = CARTESIAN_POINT ( 'NONE',  ( 3.400000000000000355, -1.000000000000000000, 0.000000000000000000 ) ) ;
#23122 = ADVANCED_FACE ( 'NONE', ( #13570 ), #65805, .F. ) ;
#23123 = CARTESIAN_POINT ( 'NONE',  ( 12.24916108028120831, -2.785825388767152688, 12.38039059669299569 ) ) ;
#23124 = EDGE_CURVE ( 'NONE', #27875, #44844, #35902, .T. ) ;
#23125 = ORIENTED_EDGE ( 'NONE', *, *, #21432, .F. ) ;
#23126 = CARTESIAN_POINT ( 'NONE',  ( 11.02939238023000001, -8.053283849414000883, -6.898628641089999292 ) ) ;
#23127 = ORIENTED_EDGE ( 'NONE', *, *, #64083, .T. ) ;
#23128 = CONICAL_SURFACE ( 'NONE', #45450, 12.44999944941000081, 0.7853981146832407223 ) ;
#23129 = CARTESIAN_POINT ( 'NONE',  ( 18.11595230660373090, -2.775896237034515490, 13.61106543307220207 ) ) ;
#23130 = CARTESIAN_POINT ( 'NONE',  ( 11.03502897915239878, -3.672866099873000056, -8.735435061820998826 ) ) ;
#23131 = ORIENTED_EDGE ( 'NONE', *, *, #66488, .F. ) ;
#23132 = CARTESIAN_POINT ( 'NONE',  ( 11.39700581613019992, 4.869652672166700391, 6.941573685175900010 ) ) ;
#23133 = CARTESIAN_POINT ( 'NONE',  ( 6.552419474232656249, 1.065422820183789865, -0.3854643328078556919 ) ) ;
#23134 = CARTESIAN_POINT ( 'NONE',  ( 8.719734573340000239, -4.222669097051499953, -8.352506367884300786 ) ) ;
#23135 = CARTESIAN_POINT ( 'NONE',  ( 11.14698693981000055, 5.129806801114000336, 5.886034047559999927 ) ) ;
#23136 = DIRECTION ( 'NONE',  ( 1.000000000000000000, 0.000000000000000000, 0.000000000000000000 ) ) ;
#23137 = CARTESIAN_POINT ( 'NONE',  ( 10.71684687351595855, -3.231816600031351516, 8.499583552997721725 ) ) ;
#23138 = CARTESIAN_POINT ( 'NONE',  ( 11.71289336965100070, 3.191014699919000108, -11.45041132747999946 ) ) ;
#23139 = CIRCLE ( 'NONE', #16442, 0.5000000000000000000 ) ;
#23140 = CARTESIAN_POINT ( 'NONE',  ( 10.00074484908000194, -2.373896846742000299, -7.962434077545999855 ) ) ;
#23141 = CARTESIAN_POINT ( 'NONE',  ( 4.000000000000000000, -2.081773110051108322, -0.5564988119414342460 ) ) ;
#23142 = CARTESIAN_POINT ( 'NONE',  ( 5.452606837613999780, -0.4199405305951999789, 1.440017343911000003 ) ) ;
#23143 = ORIENTED_EDGE ( 'NONE', *, *, #50757, .T. ) ;
#23144 = CARTESIAN_POINT ( 'NONE',  ( 8.863694533038728451, 4.511314481744639338, -6.614578276768176224 ) ) ;
#23145 = EDGE_LOOP ( 'NONE', ( #38822, #40056, #31659, #57576 ) ) ;
#23146 = CARTESIAN_POINT ( 'NONE',  ( 10.69798710243586548, 3.113013961156086751, -4.803896147529662208 ) ) ;
#23147 = CARTESIAN_POINT ( 'NONE',  ( 19.94999927679900154, 0.000000000000000000, -12.47499939739994979 ) ) ;
#23148 = EDGE_CURVE ( 'NONE', #1641, #27849, #66986, .T. ) ;
#23149 = CARTESIAN_POINT ( 'NONE',  ( 11.04384236319999957, -5.374613432488000164, -5.035088906224999938 ) ) ;
#23150 = CARTESIAN_POINT ( 'NONE',  ( 9.988317406969001055, 4.237919115995800290, -8.756892549790999070 ) ) ;
#23151 = CARTESIAN_POINT ( 'NONE',  ( 12.27782020686940534, 2.164202955609506152, 13.73892120162924968 ) ) ;
#23152 = CARTESIAN_POINT ( 'NONE',  ( 10.39106278671000005, -4.025320977579999848, 9.261121875182000807 ) ) ;
#23153 = VERTEX_POINT ( 'NONE', #27363 ) ;
#23154 = CARTESIAN_POINT ( 'NONE',  ( 10.26685100253999927, 2.832432432432000269, 6.822293592207000934 ) ) ;
#23155 = CARTESIAN_POINT ( 'NONE',  ( 12.15994429558105949, 0.3334496638227513188, 13.99603244703262739 ) ) ;
#23156 =( BOUNDED_SURFACE ( )  B_SPLINE_SURFACE ( 3, 3, ( 
 ( #40316, #61635, #56397, #8500, #29847, #8843, #3584, #46252, #11500, #43680, #21054 ),
 ( #62993, #6956, #65333, #27947, #68586, #47284, #4969, #38423, #28288, #32844, #64977 ),
 ( #16747, #15121, #49607, #17452, #22685, #6605, #31214, #10215, #63341, #38778, #57758 ),
 ( #54156, #20708, #52519, #59748, #4618, #68939, #17091, #38074, #43335, #12208, #59401 ) ),
 .UNSPECIFIED., .F., .F., .T. ) 
 B_SPLINE_SURFACE_WITH_KNOTS ( ( 4, 4 ),
 ( 4, 1, 1, 1, 1, 1, 1, 1, 4 ),
 ( 0.000000000000000000, 1.000000000000000000 ),
 ( 0.8312902889582000077, 0.8338388411866000105, 0.8555869174461000481, 0.8794646334507000285, 0.9056938526918999477, 0.9344431701381999966, 0.9658387281735000274, 1.000000000000000000, 1.004668145018999814 ),
 .UNSPECIFIED. ) 
 GEOMETRIC_REPRESENTATION_ITEM ( )  RATIONAL_B_SPLINE_SURFACE ( (
 ( 1.221026506593000160, 1.221026506593000160, 1.221026506593000160, 1.221026506593000160, 1.221026506593000160, 1.221026506593000160, 1.221026506593000160, 1.221026506593000160, 1.221026506593000160, 1.221026506593000160, 1.221026506593000160),
 ( 0.9263244978021999421, 0.9263244978021999421, 0.9263244978021999421, 0.9263244978021999421, 0.9263244978021999421, 0.9263244978021999421, 0.9263244978021999421, 0.9263244978021999421, 0.9263244978021999421, 0.9263244978021999421, 0.9263244978021999421),
 ( 0.9263244978021999421, 0.9263244978021999421, 0.9263244978021999421, 0.9263244978021999421, 0.9263244978021999421, 0.9263244978021999421, 0.9263244978021999421, 0.9263244978021999421, 0.9263244978021999421, 0.9263244978021999421, 0.9263244978021999421),
 ( 1.221026506593000160, 1.221026506593000160, 1.221026506593000160, 1.221026506593000160, 1.221026506593000160, 1.221026506593000160, 1.221026506593000160, 1.221026506593000160, 1.221026506593000160, 1.221026506593000160, 1.221026506593000160) ) ) 
 REPRESENTATION_ITEM ( '' )  SURFACE ( )  );
#23157 = ORIENTED_EDGE ( 'NONE', *, *, #57431, .T. ) ;
#23158 = CARTESIAN_POINT ( 'NONE',  ( 7.073590560819000395, 3.668692617901999853, -8.939602259005999585 ) ) ;
#23159 = CARTESIAN_POINT ( 'NONE',  ( 21.49999863197000138, -14.00000000000000000, 0.000000000000000000 ) ) ;
#23160 = CARTESIAN_POINT ( 'NONE',  ( 23.61807773383599951, -2.886089390029999535, -13.53865479462000110 ) ) ;
#23161 = CARTESIAN_POINT ( 'NONE',  ( 8.461669748674118807, 3.016807879086336630, 6.195864493290629049 ) ) ;
#23162 = AXIS2_PLACEMENT_3D ( 'NONE', #4877, #41606, #25866 ) ;
#23163 = CARTESIAN_POINT ( 'NONE',  ( 9.038304719595000591, 3.867331042029999999, -9.227339949050001877 ) ) ;
#23164 = CARTESIAN_POINT ( 'NONE',  ( 4.649999478197380576, 0.000000000000000000, -9.325873406851000657E-14 ) ) ;
#23165 = CARTESIAN_POINT ( 'NONE',  ( 10.86493091395000121, -4.678465004315999209, -9.048463592221999363 ) ) ;
#23166 = CYLINDRICAL_SURFACE ( 'NONE', #63269, 11.84999999999999964 ) ;
#23167 = CARTESIAN_POINT ( 'NONE',  ( 17.55505043854143565, 3.125000000000000000, -25.00000000000000000 ) ) ;
#23168 = AXIS2_PLACEMENT_3D ( 'NONE', #64499, #9997, #15252 ) ;
#23169 = CARTESIAN_POINT ( 'NONE',  ( 4.542107630820832576, -1.500000000000000888, 0.2435150667312298567 ) ) ;
#23170 = CARTESIAN_POINT ( 'NONE',  ( 9.306727112333998519, -4.009302068291999532, -9.043024413115999138 ) ) ;
#23171 = CARTESIAN_POINT ( 'NONE',  ( 11.21979841651039855, 3.695024856201900132, -8.310733465454200442 ) ) ;
#23172 = CARTESIAN_POINT ( 'NONE',  ( 11.62299956498149989, -2.792989229543000107, 7.174999999999999822 ) ) ;
#23173 = CARTESIAN_POINT ( 'NONE',  ( 11.52166954483529793, 4.562096242626500597, -6.632714178206799538 ) ) ;
#23174 = CARTESIAN_POINT ( 'NONE',  ( 9.634659112603999986, 3.563556310301200014, -8.404632083253700259 ) ) ;
#23176 = CARTESIAN_POINT ( 'NONE',  ( 10.33091365668000172, -3.119355846288000222, 4.717868057528999515 ) ) ;
#23175 = CARTESIAN_POINT ( 'NONE',  ( 10.71024205624999937, -4.310927436352299580, 6.690659495528099576 ) ) ;
#23177 = CARTESIAN_POINT ( 'NONE',  ( 9.906851002540999929, -2.832432432432000269, -6.822293592207000934 ) ) ;
#23178 = EDGE_LOOP ( 'NONE', ( #38631, #61322 ) ) ;
#23179 = TOROIDAL_SURFACE ( 'NONE', #6449, 11.15000000000000036, 0.5000000000000000000 ) ;
#23180 = CARTESIAN_POINT ( 'NONE',  ( 10.72702344389999851, 2.995605560827999891, 8.109550315577399360 ) ) ;
#23181 = CARTESIAN_POINT ( 'NONE',  ( 10.90374822854000136, -3.726845778959999578, 5.900452123196999743 ) ) ;
#23182 = EDGE_CURVE ( 'NONE', #13672, #15974, #11271, .T. ) ;
#23183 = EDGE_CURVE ( 'NONE', #10762, #40405, #31092, .T. ) ;
#23184 = CARTESIAN_POINT ( 'NONE',  ( 9.581038493598999395, 4.826346105011899645, 8.287963554181398962 ) ) ;
#23185 = CARTESIAN_POINT ( 'NONE',  ( 10.72726354018300121, -3.370476274536371442, -6.407767014557179230 ) ) ;
#23186 = VECTOR ( 'NONE', #8669, 1000.000000000000114 ) ;
#23187 = CARTESIAN_POINT ( 'NONE',  ( 10.09697182628999990, -5.253379538902000156, 8.530665717066000298 ) ) ;
#23188 = CARTESIAN_POINT ( 'NONE',  ( 9.694121230991363802, -5.744981173682874420, 7.383335460396494909 ) ) ;
#23190 = UNCERTAINTY_MEASURE_WITH_UNIT (LENGTH_MEASURE( 1.000000000000000082E-05 ), #12731, 'distance_accuracy_value', 'NONE');
#23189 = CARTESIAN_POINT ( 'NONE',  ( 5.399998535875000449, -12.98068687585000092, -1.765643277146000001 ) ) ;
#23191 = ORIENTED_EDGE ( 'NONE', *, *, #24620, .T. ) ;
#23192 = CARTESIAN_POINT ( 'NONE',  ( 8.646822372493998543, -4.288705740401799638, -8.444453017408701356 ) ) ;
#23193 = FACE_OUTER_BOUND ( 'NONE', #3633, .T. ) ;
#23194 = CARTESIAN_POINT ( 'NONE',  ( 5.066478153344000646, -1.481027812490000040, 0.6434334968688999457 ) ) ;
#23195 = DIRECTION ( 'NONE',  ( -1.000000000000000000, 0.000000000000000000, 0.000000000000000000 ) ) ;
#23196 = CARTESIAN_POINT ( 'NONE',  ( 24.36809152945900081, -3.197172894633000251, 12.07984101077999917 ) ) ;
#23197 = CARTESIAN_POINT ( 'NONE',  ( 12.18748876160954886, -4.600381688599499697, 6.875627981711399883 ) ) ;
#23198 = CARTESIAN_POINT ( 'NONE',  ( 10.33364828895399867, 4.760196147278000112, -7.915211961479200475 ) ) ;
#23199 = CARTESIAN_POINT ( 'NONE',  ( 8.616332388160998335, -5.167567399848000065, -6.822293593032000558 ) ) ;
#23200 = CARTESIAN_POINT ( 'NONE',  ( 24.37847035506199944, -8.840951746222000196, 8.761877451061000244 ) ) ;
#23201 = CARTESIAN_POINT ( 'NONE',  ( 5.500000000000000000, 0.8000000000000000444, -3.149999999999999911 ) ) ;
#23202 = VERTEX_POINT ( 'NONE', #16859 ) ;
#23203 = CARTESIAN_POINT ( 'NONE',  ( 7.856851002541000106, 2.832432432432000269, -6.822293592207000934 ) ) ;
#23204 = CIRCLE ( 'NONE', #68967, 13.17499999999999538 ) ;
#23205 = CARTESIAN_POINT ( 'NONE',  ( 12.08032335320030093, -0.02332822437944849850, -13.99998565365491388 ) ) ;
#23206 = CARTESIAN_POINT ( 'NONE',  ( 13.78329442975000063, -8.859672882948000705, -7.785394853692999995 ) ) ;
#23207 = EDGE_CURVE ( 'NONE', #61459, #26174, #37847, .T. ) ;
#23208 = ADVANCED_FACE ( 'NONE', ( #6023 ), #20235, .T. ) ;
#23209 = PLANE ( 'NONE',  #11383 ) ;
#23210 = CARTESIAN_POINT ( 'NONE',  ( 10.49809687351654297, -4.327184855449103473, -8.717465845835393523 ) ) ;
#23211 = CARTESIAN_POINT ( 'NONE',  ( 7.000000000000000000, 10.80467225524999897, 3.475853594956999970 ) ) ;
#23212 = CARTESIAN_POINT ( 'NONE',  ( 13.50830001818700055, 12.29143783039000049, 2.111693202397000313 ) ) ;
#23213 = VERTEX_POINT ( 'NONE', #49368 ) ;
#23214 = EDGE_CURVE ( 'NONE', #25719, #4446, #6366, .T. ) ;
#23215 = DIRECTION ( 'NONE',  ( -1.000000000000000000, 0.000000000000000000, 0.000000000000000000 ) ) ;
#23216 = CARTESIAN_POINT ( 'NONE',  ( 17.81260085050721287, 3.200899519495046697, -13.62917211583035026 ) ) ;
#23217 = EDGE_LOOP ( 'NONE', ( #20687, #40664, #12402, #30591, #985, #65427, #1382, #18465, #12870 ) ) ;
#23218 = CARTESIAN_POINT ( 'NONE',  ( 10.42819717211483521, -5.125396288440269288, 6.749639981106747122 ) ) ;
#23219 = CARTESIAN_POINT ( 'NONE',  ( 25.02481001335046074, 8.536659555490478724, -8.299428667226347756 ) ) ;
#23220 = AXIS2_PLACEMENT_3D ( 'NONE', #40230, #34991, #7370 ) ;
#23221 = CARTESIAN_POINT ( 'NONE',  ( 9.401145280412999128, 3.927090956378999742, -9.230892435423001530 ) ) ;
#23222 = CARTESIAN_POINT ( 'NONE',  ( 8.801820635884373800, 4.060146622106553416, -8.450403350428134175 ) ) ;
#23223 = CARTESIAN_POINT ( 'NONE',  ( 11.03443712336079940, 5.057168833716702672, -7.175021320887989162 ) ) ;
#23224 = CARTESIAN_POINT ( 'NONE',  ( 17.92176999529980819, 0.5062894560746492578, -12.68641719396730316 ) ) ;
#23225 = AXIS2_PLACEMENT_3D ( 'NONE', #58258, #59638, #64180 ) ;
#23226 = CARTESIAN_POINT ( 'NONE',  ( 11.06666666666870746, -2.480181672121660519, 7.732127511715526147 ) ) ;
#23227 = ORIENTED_EDGE ( 'NONE', *, *, #7818, .F. ) ;
#23228 = CARTESIAN_POINT ( 'NONE',  ( 10.81316193496000011, -3.756072284922999938, 6.071597915422999314 ) ) ;
#23229 = CARTESIAN_POINT ( 'NONE',  ( 18.18005044575085449, -2.500000006795658702, -13.67340643792831401 ) ) ;
#23230 = CARTESIAN_POINT ( 'NONE',  ( 9.246064158776000852, 5.200883864107000321, -6.027780766890000308 ) ) ;
#23231 = ORIENTED_EDGE ( 'NONE', *, *, #68553, .T. ) ;
#23232 = AXIS2_PLACEMENT_3D ( 'NONE', #25615, #61989, #14101 ) ;
#23233 = CARTESIAN_POINT ( 'NONE',  ( 9.937409415358999354, 3.510662261693000108, -6.227052446266999830 ) ) ;
#23234 = SURFACE_STYLE_USAGE ( .BOTH. , #1913 ) ;
#23235 = ORIENTED_EDGE ( 'NONE', *, *, #43571, .F. ) ;
#23236 = CARTESIAN_POINT ( 'NONE',  ( 9.077417874593999514, 3.075647715286899953, 7.107043063332000088 ) ) ;
#23237 = CARTESIAN_POINT ( 'NONE',  ( 18.03667146358278117, -1.942392957153856514, -12.44938452643338955 ) ) ;
#23238 = ADVANCED_FACE ( 'NONE', ( #17566 ), #54621, .T. ) ;
#23239 = DIRECTION ( 'NONE',  ( 1.000000000000000000, 0.000000000000000000, 0.000000000000000000 ) ) ;
#23240 = LINE ( 'NONE', #13103, #13769 ) ;
#23241 = CARTESIAN_POINT ( 'NONE',  ( 11.29998636608000062, 3.695122995756999984, -11.25914041192000070 ) ) ;
#23242 = AXIS2_PLACEMENT_3D ( 'NONE', #30438, #62578, #40919 ) ;
#23243 = CARTESIAN_POINT ( 'NONE',  ( 9.256734463322999318, 4.090312251411050148, 6.637705594503099604 ) ) ;
#23244 = CARTESIAN_POINT ( 'NONE',  ( 9.474491361279490320, -2.332153331583475264, 6.968217119213045763 ) ) ;
#23245 = ORIENTED_EDGE ( 'NONE', *, *, #27877, .T. ) ;
#23246 = LINE ( 'NONE', #12412, #50387 ) ;
#23247 = CARTESIAN_POINT ( 'NONE',  ( 10.16821721959000158, 2.330395133894000548, -7.267461653224000173 ) ) ;
#23248 = LINE ( 'NONE', #40357, #36335 ) ;
#23249 = CARTESIAN_POINT ( 'NONE',  ( 12.37605701841384409, 2.954974367521622458, -13.56637846613975462 ) ) ;
#23250 = CARTESIAN_POINT ( 'NONE',  ( 10.21627973160999936, -3.885210315895700095, -6.225948307210999566 ) ) ;
#23251 = B_SPLINE_CURVE_WITH_KNOTS ( 'NONE', 3,
 ( #42034, #58793, #10552, #64362 ),
 .UNSPECIFIED., .F., .F.,
 ( 4, 4 ),
 ( 0.000000000000000000, 1.000000000000000000 ),
 .UNSPECIFIED. ) ;
#23252 = CARTESIAN_POINT ( 'NONE',  ( 11.02286109245999945, -2.398753588646000079, 6.352476128646999065 ) ) ;
#23253 = CARTESIAN_POINT ( 'NONE',  ( 17.78490373093669774, 0.5812901181791684246, 13.88363587338390559 ) ) ;
#23254 = CARTESIAN_POINT ( 'NONE',  ( 25.40550217044300041, -3.091918942015000393, 11.38326880256000173 ) ) ;
#23255 = ORIENTED_EDGE ( 'NONE', *, *, #12143, .F. ) ;
#23256 = ORIENTED_EDGE ( 'NONE', *, *, #31105, .T. ) ;
#23257 = CARTESIAN_POINT ( 'NONE',  ( 8.938854719593997800, 5.597201461420000967, -8.171008079894999554 ) ) ;
#23258 = CARTESIAN_POINT ( 'NONE',  ( 25.29987654162099986, -8.533547851352999203, -7.925583806936000286 ) ) ;
#23259 = CARTESIAN_POINT ( 'NONE',  ( 12.64394750692856917, -0.6042238833877793258, -13.88232004407405462 ) ) ;
#23260 = CARTESIAN_POINT ( 'NONE',  ( 10.13050497920000126, -3.092053006542000215, 8.629388195475000245 ) ) ;
#23261 = CARTESIAN_POINT ( 'NONE',  ( 23.64966114303629041, 3.378619448667885550, -13.52224079656408229 ) ) ;
#23262 = CARTESIAN_POINT ( 'NONE',  ( 8.256683059623998844, -2.876278577719999952, 6.568889245344999850 ) ) ;
#23263 = DIRECTION ( 'NONE',  ( 1.000000000000000000, 0.000000000000000000, 0.000000000000000000 ) ) ;
#23265 = DIRECTION ( 'NONE',  ( -1.000000000000000000, 0.000000000000000000, 0.000000000000000000 ) ) ;
#23264 = CARTESIAN_POINT ( 'NONE',  ( 9.677784697135001224, -3.305825103746500293, 8.574479223074998657 ) ) ;
#23266 = CARTESIAN_POINT ( 'NONE',  ( 10.78887616594230003, 3.613544262574699850, -6.281817606595999415 ) ) ;
#23267 = DIRECTION ( 'NONE',  ( 1.239633395933026350E-11, -1.000000000000000000, 7.155734338404329264E-12 ) ) ;
#23268 = CARTESIAN_POINT ( 'NONE',  ( 8.693164714044028685, 2.945149437845938856, -6.183674439331818817 ) ) ;
#23269 = EDGE_CURVE ( 'NONE', #53475, #60701, #38184, .T. ) ;
#23270 = EDGE_CURVE ( 'NONE', #19975, #27999, #443, .T. ) ;
#23271 = CARTESIAN_POINT ( 'NONE',  ( 10.90291315457000110, -5.099848460227999425, 5.141818958950999274 ) ) ;
#23272 = CARTESIAN_POINT ( 'NONE',  ( 11.09999999999999964, -5.538898460221000519, 7.685179721164000277 ) ) ;
#23273 = CIRCLE ( 'NONE', #32213, 14.00000000000000000 ) ;
#23274 = CARTESIAN_POINT ( 'NONE',  ( 18.12908148756441307, -2.747269642056539229, -12.39050915965749766 ) ) ;
#23275 = EDGE_LOOP ( 'NONE', ( #2454, #51947, #10676, #57262 ) ) ;
#23277 = CARTESIAN_POINT ( 'NONE',  ( 10.77222057153667656, 4.304280767886410786, 6.680547245655227506 ) ) ;
#23276 = CARTESIAN_POINT ( 'NONE',  ( 19.94999927679900154, 0.000000000000000000, 5.040412531797999279E-14 ) ) ;
#23278 = CARTESIAN_POINT ( 'NONE',  ( 9.600045280412000892, 3.021734963141999852, -6.070209284876999511 ) ) ;
#23279 = EDGE_CURVE ( 'NONE', #44670, #22409, #14704, .T. ) ;
#23280 = B_SPLINE_CURVE_WITH_KNOTS ( 'NONE', 3,
 ( #64687, #64335, #5963, #4933, #59107, #380, #58418, #68906, #26619, #42357, #728, #42689, #42008, #31183, #31863, #52837, #5278, #21359, #31516 ),
 .UNSPECIFIED., .F., .F.,
 ( 4, 1, 1, 1, 1, 1, 1, 1, 1, 1, 1, 1, 1, 1, 1, 1, 4 ),
 ( 0.000000000000000000, 0.04500315983054108820, 0.1100028832174083232, 0.1750026066042755235, 0.2400023299912177610, 0.3050020533779163046, 0.3700017767648023370, 0.4350015001516882585, 0.5000012235385741244, 0.5650009469254601013, 0.6300006703123461893, 0.6950003936992321663, 0.7600001170861181432, 0.8249998404730040091, 0.8899995638597026915, 0.9549992872465886684, 1.000000000000000000 ),
 .UNSPECIFIED. ) ;
#23281 = PLANE ( 'NONE',  #23079 ) ;
#23282 = FACE_OUTER_BOUND ( 'NONE', #2613, .T. ) ;
#23283 = VECTOR ( 'NONE', #14169, 1000.000000000000000 ) ;
#23284 = CARTESIAN_POINT ( 'NONE',  ( 24.30001697352500045, -3.271769158411000245, -12.21048181092999840 ) ) ;
#23285 = CARTESIAN_POINT ( 'NONE',  ( 8.571413182548997867, -4.600000000000999734, 5.927302706106000407 ) ) ;
#23286 = CARTESIAN_POINT ( 'NONE',  ( 3.267613282616999903, -3.729289631816000039, 0.4698937791177000278 ) ) ;
#23287 = ORIENTED_EDGE ( 'NONE', *, *, #36389, .F. ) ;
#23288 = CONICAL_SURFACE ( 'NONE', #2088, 0.3796172482170003804, 0.7853981633972997312 ) ;
#23289 = CARTESIAN_POINT ( 'NONE',  ( 12.08617037725597143, -0.09400131084488008715, -12.59965472429369093 ) ) ;
#23290 = CARTESIAN_POINT ( 'NONE',  ( 12.48752230513397343, -1.955425561953247682, -12.56195022951900775 ) ) ;
#23291 = CARTESIAN_POINT ( 'NONE',  ( 24.14075163639471455, -12.48103446967273378, -3.363283332670145231 ) ) ;
#23292 = CARTESIAN_POINT ( 'NONE',  ( 9.015545280411000562, 4.175915362023999933, 5.699506188181000077 ) ) ;
#23293 = VERTEX_POINT ( 'NONE', #44148 ) ;
#23294 = CARTESIAN_POINT ( 'NONE',  ( 5.795621349514000542, -1.101608967510000037, 0.4118716830840000176 ) ) ;
#23295 = CARTESIAN_POINT ( 'NONE',  ( 10.94048160847601991, 9.309402769125675547, 6.237066211927379200 ) ) ;
#23297 = CARTESIAN_POINT ( 'NONE',  ( 10.70039988502543871, 3.823246508712561109, -8.849946088921042175 ) ) ;
#23296 = CARTESIAN_POINT ( 'NONE',  ( 8.575831600094877771, -4.020817762796284889, 5.760477547183362468 ) ) ;
#23298 = VECTOR ( 'NONE', #27200, 1000.000000000000000 ) ;
#23299 = DIRECTION ( 'NONE',  ( -1.000000000000000000, 0.000000000000000000, 0.000000000000000000 ) ) ;
#23300 = EDGE_LOOP ( 'NONE', ( #55590, #6893, #24414, #53393 ) ) ;
#23301 = EDGE_CURVE ( 'NONE', #40281, #14597, #9395, .T. ) ;
#23302 = CARTESIAN_POINT ( 'NONE',  ( 9.903944471677000649, -5.205019707614999547, 6.747219600580999455 ) ) ;
#23303 = VERTEX_POINT ( 'NONE', #66481 ) ;
#23304 = CARTESIAN_POINT ( 'NONE',  ( 9.481861110199060860, -5.015380455770686474, 8.392903197087751010 ) ) ;
#23305 = FACE_OUTER_BOUND ( 'NONE', #19556, .T. ) ;
#23306 = CARTESIAN_POINT ( 'NONE',  ( 17.93540541742265049, -0.4960449563116382521, -13.88808666890936827 ) ) ;
#23307 = ORIENTED_EDGE ( 'NONE', *, *, #43087, .T. ) ;
#23308 = CARTESIAN_POINT ( 'NONE',  ( 10.97312085988376928, 8.562142776844346770, -6.539677800798914475 ) ) ;
#23309 = CARTESIAN_POINT ( 'NONE',  ( 11.09999999999999964, -2.899999999999999911, -4.336547745386999608 ) ) ;
#23310 = DIRECTION ( 'NONE',  ( 0.000000000000000000, -0.1218274111675001353, -0.9925512993736016476 ) ) ;
#23311 = CARTESIAN_POINT ( 'NONE',  ( 8.188938565157510396, 2.652235273545433092, 7.263344527950063245 ) ) ;
#23312 = CARTESIAN_POINT ( 'NONE',  ( 18.15933590972274558, -2.660621711755056573, 12.41273490637200894 ) ) ;
#23313 = VERTEX_POINT ( 'NONE', #45522 ) ;
#23314 = CARTESIAN_POINT ( 'NONE',  ( 24.30001694670299983, 8.938702829764999080, 8.938676122491999720 ) ) ;
#23315 = CARTESIAN_POINT ( 'NONE',  ( 23.58312609496700318, -13.27342582440000029, -4.266007375089999165 ) ) ;
#23316 = CYLINDRICAL_SURFACE ( 'NONE', #56458, 2.250000000000000000 ) ;
#23317 = CARTESIAN_POINT ( 'NONE',  ( 8.099999999999999645, 0.000000000000000000, 0.000000000000000000 ) ) ;
#23318 = ORIENTED_EDGE ( 'NONE', *, *, #34361, .T. ) ;
#23319 = CARTESIAN_POINT ( 'NONE',  ( 7.100000000000000533, 4.000000000000000000, 8.849999999999999645 ) ) ;
#23320 = ADVANCED_FACE ( 'NONE', ( #2515 ), #13018, .F. ) ;
#23321 = CARTESIAN_POINT ( 'NONE',  ( 4.900006121741999898, -6.122517096885939548E-17, -1.999970730383187734 ) ) ;
#23322 = DIRECTION ( 'NONE',  ( 1.000000000000000000, 0.000000000000000000, 0.000000000000000000 ) ) ;
#23323 = DIRECTION ( 'NONE',  ( 1.000000000000000000, 0.000000000000000000, 0.000000000000000000 ) ) ;
#23324 = CARTESIAN_POINT ( 'NONE',  ( 24.30001683570900184, 3.271769286791000209, 12.21048169671000139 ) ) ;
#23325 = VECTOR ( 'NONE', #42111, 1000.000000000000000 ) ;
#23326 = FACE_OUTER_BOUND ( 'NONE', #34270, .T. ) ;
#23327 = CARTESIAN_POINT ( 'NONE',  ( 18.00033872679592051, -1.911966235111655310, 12.45410047071287529 ) ) ;
#23328 = ORIENTED_EDGE ( 'NONE', *, *, #17460, .T. ) ;
#23329 = CARTESIAN_POINT ( 'NONE',  ( 11.48011496860029901, -3.080230834057799960, -7.028661263734299780 ) ) ;
#23330 = ORIENTED_EDGE ( 'NONE', *, *, #16823, .F. ) ;
#23331 = CARTESIAN_POINT ( 'NONE',  ( 18.18005043875541560, 2.480307850574838380, 13.67758270212689276 ) ) ;
#23332 = CARTESIAN_POINT ( 'NONE',  ( 8.997439158776000312, 2.773858540272000184, -8.951250717848999727 ) ) ;
#23333 = CARTESIAN_POINT ( 'NONE',  ( 3.292824395831999595, 2.812750220982000116, 1.557238109803000148 ) ) ;
#23334 = CARTESIAN_POINT ( 'NONE',  ( 11.08752429429999964, -2.871531501602999636, -6.302910744985999791 ) ) ;
#23335 = CARTESIAN_POINT ( 'NONE',  ( 6.801647950796354536, 1.188027738384418219, -0.9443810485859288617 ) ) ;
#23336 = CARTESIAN_POINT ( 'NONE',  ( -0.2999999999999999889, -0.5773502691895999739, -1.000000000000000000 ) ) ;
#23337 = CARTESIAN_POINT ( 'NONE',  ( 0.7000000000000000666, 0.000000000000000000, -0.5999999999999999778 ) ) ;
#23338 = VERTEX_POINT ( 'NONE', #23841 ) ;
#23339 = CARTESIAN_POINT ( 'NONE',  ( 10.08070436339981768, -5.349944892048520195, -7.768717962862259796 ) ) ;
#23340 = CARTESIAN_POINT ( 'NONE',  ( 12.06025819896753859, -4.986099335708799707, 7.314099615601099558 ) ) ;
#23341 = CARTESIAN_POINT ( 'NONE',  ( 10.28314886242000092, 2.387776420306999992, 7.684265965147999644 ) ) ;
#23342 = CARTESIAN_POINT ( 'NONE',  ( 10.75046352948140438, -3.823292445202751466, -8.850187295431151568 ) ) ;
#23343 = CARTESIAN_POINT ( 'NONE',  ( 10.51927318630899855, 4.756452637475340417, -8.526145288591962412 ) ) ;
#23344 = CARTESIAN_POINT ( 'NONE',  ( 9.215336765710809175, 2.659996753869333208, 7.664888201578709648 ) ) ;
#23345 = CARTESIAN_POINT ( 'NONE',  ( 11.77359063708300013, 4.955772084214699724, -7.768721787835699999 ) ) ;
#23346 = CARTESIAN_POINT ( 'NONE',  ( 7.100000000000000533, 5.221516520829000640, -8.074802043613001246 ) ) ;
#23347 = CARTESIAN_POINT ( 'NONE',  ( 9.631696787963999640, 4.196076320588900010, -6.375149554610999303 ) ) ;
#23348 = EDGE_CURVE ( 'NONE', #67676, #33524, #29364, .T. ) ;
#23349 = EDGE_CURVE ( 'NONE', #54348, #42489, #59292, .T. ) ;
#23350 = CARTESIAN_POINT ( 'NONE',  ( 23.62001506143800000, -10.21680080108000155, 9.338901190890000592 ) ) ;
#23351 = CARTESIAN_POINT ( 'NONE',  ( 8.104887188112282814, 4.724403967564894558, -6.210088579440072643 ) ) ;
#23352 = CARTESIAN_POINT ( 'NONE',  ( 10.41025778040999938, 4.690688562647999937, -6.142866736126999960 ) ) ;
#23353 = EDGE_LOOP ( 'NONE', ( #43548, #14953, #36275, #11877 ) ) ;
#23354 = CARTESIAN_POINT ( 'NONE',  ( 7.239688980126000040, -4.389298280625000714, 9.135255728583000945 ) ) ;
#23355 = B_SPLINE_CURVE_WITH_KNOTS ( 'NONE', 3,
 ( #25140, #26523, #26177, #15342 ),
 .UNSPECIFIED., .F., .F.,
 ( 4, 4 ),
 ( 0.000000000000000000, 0.4999999894681322887 ),
 .UNSPECIFIED. ) ;
#23356 = ADVANCED_FACE ( 'NONE', ( #19632 ), #45177, .T. ) ;
#23357 = EDGE_CURVE ( 'NONE', #42217, #11817, #45859, .T. ) ;
#23358 = CARTESIAN_POINT ( 'NONE',  ( 17.63745110450239295, 3.119885622577724504, 13.52219988749413737 ) ) ;
#23359 = LINE ( 'NONE', #22655, #67972 ) ;
#23360 = CARTESIAN_POINT ( 'NONE',  ( 10.25149413291699929, -2.962184842772000337, -7.026470926762800495 ) ) ;
#23361 = ORIENTED_EDGE ( 'NONE', *, *, #28344, .F. ) ;
#23362 = CARTESIAN_POINT ( 'NONE',  ( 10.57538794102227264, -5.349775832304747070, -7.676723066621575775 ) ) ;
#23363 = CARTESIAN_POINT ( 'NONE',  ( 8.320864158774000430, 3.894644548817000285, 6.044465307984999924 ) ) ;
#23365 = CARTESIAN_POINT ( 'NONE',  ( 0.7415127311769281748, -2.608895429637665853, 2.390477409079596161 ) ) ;
#23364 = CARTESIAN_POINT ( 'NONE',  ( 10.29522949779699914, -3.519000825516800379, -8.221351791991999391 ) ) ;
#23366 = CARTESIAN_POINT ( 'NONE',  ( 11.06205165877000063, 2.154392227069000132, -7.605898171884000192 ) ) ;
#23367 = VERTEX_POINT ( 'NONE', #7410 ) ;
#23368 = CARTESIAN_POINT ( 'NONE',  ( 10.18908827523999960, 5.907871695079999874, 7.801541097952000570 ) ) ;
#23369 = CARTESIAN_POINT ( 'NONE',  ( 18.10159474502875554, -2.998280829653927615, -13.67518427740799325 ) ) ;
#23370 = CARTESIAN_POINT ( 'NONE',  ( 11.26072066707849828, 4.976067344118500380, 8.090408888831799317 ) ) ;
#23371 = CARTESIAN_POINT ( 'NONE',  ( 10.50244460374000077, -2.268915328469999881, 7.824865002012999504 ) ) ;
#23372 = FACE_OUTER_BOUND ( 'NONE', #54947, .T. ) ;
#23373 = ORIENTED_EDGE ( 'NONE', *, *, #11139, .F. ) ;
#23374 = LINE ( 'NONE', #54146, #53325 ) ;
#23375 = EDGE_CURVE ( 'NONE', #31711, #53691, #11290, .T. ) ;
#23376 = CARTESIAN_POINT ( 'NONE',  ( 10.99305444037999990, -4.495427106425000652, -6.233607450113000326 ) ) ;
#23377 = CARTESIAN_POINT ( 'NONE',  ( 7.917165897655459084, -2.404019642809257729, 8.192082336436831369 ) ) ;
#23378 = CARTESIAN_POINT ( 'NONE',  ( 11.08992739829000129, -5.210546653347999602, 8.327600405525998895 ) ) ;
#23379 = LINE ( 'NONE', #6601, #6428 ) ;
#23380 = CARTESIAN_POINT ( 'NONE',  ( 9.854025935145999782, -4.165792341207500193, 8.629711178834000407 ) ) ;
#23381 = VERTEX_POINT ( 'NONE', #55312 ) ;
#23382 = CARTESIAN_POINT ( 'NONE',  ( 24.16219649940969560, -9.122613423523826981, 9.103272609183665764 ) ) ;
#23383 = CARTESIAN_POINT ( 'NONE',  ( 11.65810538575740019, -2.757018958839999812, 7.797177576385699638 ) ) ;
#23384 = ORIENTED_EDGE ( 'NONE', *, *, #49921, .F. ) ;
#23385 = CARTESIAN_POINT ( 'NONE',  ( 9.002376473208927976, 3.077871436655788440, 6.792422036439461408 ) ) ;
#23386 = ORIENTED_EDGE ( 'NONE', *, *, #18427, .F. ) ;
#23387 = B_SPLINE_SURFACE_WITH_KNOTS ( 'NONE', 3, 3, ( 
 ( #58037, #47204, #25870, #52787, #46860, #41611, #41266, #62580, #68506, #31136, #9786, #36364, #15038, #15388, #52438, #20629, #52090, #14701, #41953, #36716, #36019, #68163, #3385, #67694, #30318, #20158, #4065, #35563, #25401, #51964, #19124, #40448, #35895, #34540, #68043 ),
 ( #61774, #41485, #7955, #55853, #46737, #13894, #67016, #2706, #19818, #24721, #29293, #35222, #24377, #62117, #8638, #62794, #41148, #56192, #62458, #14578, #45707, #50605, #14235, #56880, #24031, #45365, #66673, #8300, #13557, #8978, #29988, #57210, #40125, #51288, #29645 ),
 ( #46045, #67352, #9313, #40794, #18796, #19471, #61437, #51626, #34874, #50948, #3722, #30653, #25059, #3044, #46390, #56534, #21189, #26794, #53697, #5458, #209, #41827, #43207, #36238, #48453, #37610, #64171, #48109, #4413, #52659, #36584, #57910, #10009, #4755, #58941 ),
 ( #25751, #42862, #32384, #5791, #10693, #31005, #21529, #47080, #63135, #58249, #26097, #27133, #68730, #63485, #11048, #47422, #20849, #37271, #42519, #21870, #561, #5107, #52319, #16285, #15605, #68381, #63828, #20502, #15261, #42182, #31346, #14916, #57555, #10353, #15942 ) ),
 .UNSPECIFIED., .F., .F., .F.,
 ( 4, 4 ),
 ( 4, 1, 1, 1, 1, 1, 1, 1, 1, 1, 1, 1, 1, 1, 1, 1, 1, 1, 1, 1, 1, 1, 1, 1, 1, 1, 1, 1, 1, 1, 1, 1, 4 ),
 ( -0.1039370721279000015, 1.103937072127999963 ),
 ( -0.01933701211302999920, 0.01208563257065999909, 0.04350827725433999843, 0.07493092193802000645, 0.1063535666217000075, 0.1377762113054000204, 0.1691988559891000055, 0.2006215006727000150, 0.2320441453564000001, 0.2634667900400999851, 0.2948894347238000258, 0.3263120794074999553, 0.3577347240911999959, 0.3891573687748000054, 0.4205800134584999905, 0.4520026581421999756, 0.4834253028259000162, 0.5148479475096000568, 0.5462705921932000663, 0.5776932368768999959, 0.6091158815606000365, 0.6405385262443000771, 0.6719611709280000067, 0.7033838156117000473, 0.7348064602953000568, 0.7662291049789999864, 0.7976517496627000270, 0.8290743943464000676, 0.8604970390300999972, 0.8919196837138000378, 0.9233423283974000473, 0.9547649730810999769, 0.9861876177648000175 ),
 .UNSPECIFIED. ) ;
#23388 = CARTESIAN_POINT ( 'NONE',  ( 8.804445280412998898, 5.597201461420000967, -8.171008079894999554 ) ) ;
#23389 = CARTESIAN_POINT ( 'NONE',  ( 11.17901463001529905, 4.697110652903200290, -6.383488688482000128 ) ) ;
#23390 = DIRECTION ( 'NONE',  ( -1.000000000000000000, 0.000000000000000000, 0.000000000000000000 ) ) ;
#23391 = CARTESIAN_POINT ( 'NONE',  ( 12.60227161487510195, 1.908786995848723134, -12.56986146204938493 ) ) ;
#23392 = CARTESIAN_POINT ( 'NONE',  ( 10.75564828895399927, -3.119330945648699949, 7.018986873610899124 ) ) ;
#23393 = CARTESIAN_POINT ( 'NONE',  ( 10.98280513895999988, -3.096689368913399854, 8.002155910165599906 ) ) ;
#23394 = ORIENTED_EDGE ( 'NONE', *, *, #11866, .T. ) ;
#23395 = AXIS2_PLACEMENT_3D ( 'NONE', #5649, #17177, #7041 ) ;
#23396 = CARTESIAN_POINT ( 'NONE',  ( 9.174642513462172744, 2.649442673323004538, 7.499981897072118819 ) ) ;
#23397 = EDGE_LOOP ( 'NONE', ( #299, #6198, #27053, #37282 ) ) ;
#23398 = CARTESIAN_POINT ( 'NONE',  ( 7.352706853207999771, -4.773080213113000347, 8.927399220053999329 ) ) ;
#23399 = CARTESIAN_POINT ( 'NONE',  ( 18.00096209673668213, 0.5835546240207898361, 13.98799446466929197 ) ) ;
#23400 = VERTEX_POINT ( 'NONE', #18605 ) ;
#23401 = B_SPLINE_SURFACE_WITH_KNOTS ( 'NONE', 3, 3, ( 
 ( #21160, #520, #64474, #59591 ),
 ( #48073, #21837, #32686, #10321 ),
 ( #64136, #26411, #43170, #42487 ),
 ( #10661, #64823, #16598, #177 ),
 ( #52976, #37923, #59242, #31657 ),
 ( #6101, #48762, #871, #22184 ),
 ( #43524, #16933, #31313, #16252 ),
 ( #63797, #4720, #26063, #5422 ) ),
 .UNSPECIFIED., .F., .F., .F.,
 ( 4, 1, 1, 1, 1, 4 ),
 ( 4, 4 ),
 ( 0.008355907821911999489, 0.05882352941176000050, 0.1176470588234999892, 0.1764705882353000133, 0.2352941176471000095, 0.2534671684970000172 ),
 ( -0.1830857773976999892, 1.182949828738000031 ),
 .UNSPECIFIED. ) ;
#23402 = CARTESIAN_POINT ( 'NONE',  ( 12.50259176966692110, -1.826373719304919208, -12.46693171540044531 ) ) ;
#23403 = CARTESIAN_POINT ( 'NONE',  ( 10.62072335273219892, 4.397090433355999473, 6.430603299050000388 ) ) ;
#23404 = EDGE_CURVE ( 'NONE', #25841, #57495, #171, .T. ) ;
#23405 = CARTESIAN_POINT ( 'NONE',  ( 5.500000000627999874, -0.4999999993719999591, -3.150000005921999691 ) ) ;
#23406 = DIRECTION ( 'NONE',  ( 1.000000000000000000, 0.000000000000000000, 0.000000000000000000 ) ) ;
#23407 = CARTESIAN_POINT ( 'NONE',  ( 17.72081995139100030, -11.49894842141999973, 4.816072468917000471 ) ) ;
#23408 = CARTESIAN_POINT ( 'NONE',  ( 10.91307648679999964, -2.096298111716999646, 7.827187677719999570 ) ) ;
#23409 = CARTESIAN_POINT ( 'NONE',  ( 12.23130451870208013, -2.748081639521273267, -13.61765624098743466 ) ) ;
#23410 = CARTESIAN_POINT ( 'NONE',  ( 18.11105811251409037, 0.2856309244984027718, -12.69568149856438311 ) ) ;
#23411 = EDGE_CURVE ( 'NONE', #5657, #21830, #62277, .T. ) ;
#23412 = CARTESIAN_POINT ( 'NONE',  ( 12.18936456685720771, 2.391983199617983225, -12.47610573829950553 ) ) ;
#23413 = CARTESIAN_POINT ( 'NONE',  ( 11.40841235500449891, -4.841138636481000290, -6.729431436870699557 ) ) ;
#23415 = CARTESIAN_POINT ( 'NONE',  ( 9.278329719590999503, 5.791553967443999973, 7.752111263209999770 ) ) ;
#23414 = B_SPLINE_CURVE_WITH_KNOTS ( 'NONE', 3,
 ( #10913, #52882, #43072, #64379 ),
 .UNSPECIFIED., .F., .F.,
 ( 4, 4 ),
 ( 0.000000000000000000, 1.000000000000000000 ),
 .UNSPECIFIED. ) ;
#23416 = VERTEX_POINT ( 'NONE', #66139 ) ;
#23417 = CARTESIAN_POINT ( 'NONE',  ( 11.60000000000000320, -3.890364666909557734, -8.637585274955608128 ) ) ;
#23418 = CARTESIAN_POINT ( 'NONE',  ( 8.183771503764571520, 2.796787595787193492, 8.203896902613271536 ) ) ;
#23419 = CARTESIAN_POINT ( 'NONE',  ( 10.76231429546999863, 3.259156861436999897, -8.644989069184999764 ) ) ;
#23420 = CARTESIAN_POINT ( 'NONE',  ( 17.89634705932796166, 1.976313534945128847, 12.55826774113814892 ) ) ;
#23421 = B_SPLINE_CURVE_WITH_KNOTS ( 'NONE', 3,
 ( #26477, #21560, #64203, #68762, #37304, #43241 ),
 .UNSPECIFIED., .F., .F.,
 ( 4, 2, 4 ),
 ( 0.000000000000000000, 0.5000000000000000000, 1.000000000000000000 ),
 .UNSPECIFIED. ) ;
#23422 = CARTESIAN_POINT ( 'NONE',  ( 11.07202612390000063, 5.767975602871000085, 5.098339902409000146 ) ) ;
#23423 = CARTESIAN_POINT ( 'NONE',  ( 9.967852198058999136, 2.034774058634999605, 7.636878205663998997 ) ) ;
#23424 = CARTESIAN_POINT ( 'NONE',  ( 9.802887573405627109, -3.409423315843189251, 6.854437106819677439 ) ) ;
#23425 = CARTESIAN_POINT ( 'NONE',  ( 12.35913603394561733, -0.5748214923286987244, -12.58705572532422856 ) ) ;
#23426 = ORIENTED_EDGE ( 'NONE', *, *, #11200, .T. ) ;
#23427 = CARTESIAN_POINT ( 'NONE',  ( 12.18751053307003929, -2.401600969044472844, 12.47399295505823069 ) ) ;
#23428 = CARTESIAN_POINT ( 'NONE',  ( 9.731000818238999983, -4.888721525563999748, -7.967991827203400490 ) ) ;
#23429 = CARTESIAN_POINT ( 'NONE',  ( 9.625496329943999285, 3.134638325776999856, 8.626949804392001653 ) ) ;
#23430 = DIRECTION ( 'NONE',  ( 0.000000000000000000, 0.000000000000000000, 1.000000000000000000 ) ) ;
#23431 = CARTESIAN_POINT ( 'NONE',  ( 10.64533863405319991, 4.703785194191100416, -8.397761948794601139 ) ) ;
#23432 = CARTESIAN_POINT ( 'NONE',  ( 12.18894565086185189, -0.3798658283128588664, 12.59428767283704964 ) ) ;
#23433 = CARTESIAN_POINT ( 'NONE',  ( 8.085170280410000743, 2.431401017850999935, 7.958393275880999873 ) ) ;
#23434 = CARTESIAN_POINT ( 'NONE',  ( 11.14698693981000055, 5.129806801114000336, 5.886034047559999927 ) ) ;
#23435 = CARTESIAN_POINT ( 'NONE',  ( 12.21176631991875894, 2.303170217796229213, 12.49524360984840321 ) ) ;
#23436 = ORIENTED_EDGE ( 'NONE', *, *, #8691, .T. ) ;
#23437 = CARTESIAN_POINT ( 'NONE',  ( 9.096889158776001238, 2.235961884443999459, -6.794506518623999902 ) ) ;
#23438 = CARTESIAN_POINT ( 'NONE',  ( 10.29657053952199952, 3.497746311184500190, -6.324815923923999605 ) ) ;
#23439 = EDGE_CURVE ( 'NONE', #227, #46731, #32521, .T. ) ;
#23440 = EDGE_CURVE ( 'NONE', #66745, #2511, #55664, .T. ) ;
#23441 = CARTESIAN_POINT ( 'NONE',  ( 11.09999999999999964, 2.685305999535000154, 6.664030027596000494 ) ) ;
#23443 = CARTESIAN_POINT ( 'NONE',  ( 17.55505043854144276, -0.6250000000000001110, 12.67928921589117586 ) ) ;
#23442 = CARTESIAN_POINT ( 'NONE',  ( 9.074379440379999551, -3.981661727120999750, 8.959239802162999311 ) ) ;
#23444 = CARTESIAN_POINT ( 'NONE',  ( 9.957355082328000151, -4.449513475323099598, 8.398209294002699110 ) ) ;
#23445 = VECTOR ( 'NONE', #40175, 1000.000000000000000 ) ;
#23446 = CARTESIAN_POINT ( 'NONE',  ( 11.49056651104150006, -3.914543207408039738, -6.638028001068500217 ) ) ;
#23447 = ORIENTED_EDGE ( 'NONE', *, *, #41348, .F. ) ;
#23448 = CARTESIAN_POINT ( 'NONE',  ( 1.167201286810000127, 1.556166911672999920, -2.863499806755999799 ) ) ;
#23449 = CARTESIAN_POINT ( 'NONE',  ( 24.13558482227616864, -9.160566910400561369, -9.132875783579766704 ) ) ;
#23450 = CARTESIAN_POINT ( 'NONE',  ( 11.09999999999999964, 5.299316147296000423, -5.124965750789000296 ) ) ;
#23451 = CARTESIAN_POINT ( 'NONE',  ( 18.11145169124086962, -2.784830482494844439, 13.60891328693116442 ) ) ;
#23452 = LINE ( 'NONE', #28014, #14998 ) ;
#23453 = CARTESIAN_POINT ( 'NONE',  ( 16.09586749610213374, 8.411110950737114678, 8.060864562931188360 ) ) ;
#23454 = FACE_BOUND ( 'NONE', #33378, .T. ) ;
#23455 = CARTESIAN_POINT ( 'NONE',  ( 9.416239699516157913, -5.342737953096846404, 7.360744645781648998 ) ) ;
#23456 = CARTESIAN_POINT ( 'NONE',  ( 10.53521345716899837, 4.924890298941200228, 6.659120737011199331 ) ) ;
#23457 = ORIENTED_EDGE ( 'NONE', *, *, #27193, .T. ) ;
#23458 = CARTESIAN_POINT ( 'NONE',  ( 7.364999999998000035, 2.649999999999999911, -7.500000000000000000 ) ) ;
#23459 = EDGE_CURVE ( 'NONE', #47642, #10933, #5920, .T. ) ;
#23460 = CARTESIAN_POINT ( 'NONE',  ( 11.13508722347999935, 5.337982475388999504, 5.085688468496000425 ) ) ;
#23461 = DIRECTION ( 'NONE',  ( 1.636082834842964734E-07, -0.7071067247530858912, -0.7071068376199858285 ) ) ;
#23462 = DIRECTION ( 'NONE',  ( -0.000000000000000000, -0.000000000000000000, 1.000000000000000000 ) ) ;
#23463 = CARTESIAN_POINT ( 'NONE',  ( 1.943522225067000120, 1.849469983415999996, -3.272124421528999960 ) ) ;
#23464 = VERTEX_POINT ( 'NONE', #20312 ) ;
#23465 = DIRECTION ( 'NONE',  ( 0.000000000000000000, 0.000000000000000000, -1.000000000000000000 ) ) ;
#23466 = CARTESIAN_POINT ( 'NONE',  ( 8.486008579191000933, -3.399999999999999911, 5.976611076844000614 ) ) ;
#23467 = DIRECTION ( 'NONE',  ( 0.000000000000000000, -0.7455306007789014311, -0.6664713972124013397 ) ) ;
#23468 = CARTESIAN_POINT ( 'NONE',  ( 10.79718447801629999, 5.003225587801999552, 7.522119512433738997 ) ) ;
#23469 = CARTESIAN_POINT ( 'NONE',  ( 10.41104069048442149, -5.348816829097293279, 7.263526753701751382 ) ) ;
#23470 = DIRECTION ( 'NONE',  ( 0.000000000000000000, 1.000000000000000000, 0.000000000000000000 ) ) ;
#23471 = CARTESIAN_POINT ( 'NONE',  ( 10.99239898671677906, -5.801279784331776490, 4.969949983916245095 ) ) ;
#23472 = CARTESIAN_POINT ( 'NONE',  ( 4.599999999999999645, 1.760910691117812954, 12.47634535983622861 ) ) ;
#23473 = CARTESIAN_POINT ( 'NONE',  ( 12.19259201841644646, -2.624586292374573748, 12.42169361726068821 ) ) ;
#23474 = ORIENTED_EDGE ( 'NONE', *, *, #7932, .F. ) ;
#23475 = CARTESIAN_POINT ( 'NONE',  ( 7.993786007972365049, 2.489810687196663430, 6.574732386051532096 ) ) ;
#23476 = ORIENTED_EDGE ( 'NONE', *, *, #27557, .F. ) ;
#23477 = CARTESIAN_POINT ( 'NONE',  ( 17.65850582825309090, -3.116720375661584441, 13.52313201004804810 ) ) ;
#23478 = CARTESIAN_POINT ( 'NONE',  ( 10.69041504065829962, -2.975441626403999784, -6.736065107693399945 ) ) ;
#23479 = EDGE_LOOP ( 'NONE', ( #9204, #58123, #17818, #29413, #22444, #11974, #15447 ) ) ;
#23480 = ORIENTED_EDGE ( 'NONE', *, *, #4808, .F. ) ;
#23481 = CARTESIAN_POINT ( 'NONE',  ( 11.11123293495519881, 3.108594079907299967, 7.535834283667469435 ) ) ;
#23482 = CARTESIAN_POINT ( 'NONE',  ( 4.149992563292000725, 1.007210908820210360, -1.747525841223985132 ) ) ;
#23483 = CARTESIAN_POINT ( 'NONE',  ( 23.57792393660973573, 13.37377923847282268, -4.097348931089725532 ) ) ;
#23484 = CARTESIAN_POINT ( 'NONE',  ( 9.285195242305000818, 5.269680202247999823, 8.747831873285999649 ) ) ;
#23485 = CARTESIAN_POINT ( 'NONE',  ( 8.559672690406999962, 5.100000000000000533, -6.571331466262537724 ) ) ;
#23486 = CARTESIAN_POINT ( 'NONE',  ( 6.899999691988000450, 13.87069231928999891, 4.225386915259999654 ) ) ;
#23487 = DIRECTION ( 'NONE',  ( 0.000000000000000000, 0.000000000000000000, 1.000000000000000000 ) ) ;
#23488 = EDGE_CURVE ( 'NONE', #1641, #5569, #107, .T. ) ;
#23489 = CARTESIAN_POINT ( 'NONE',  ( 10.62924380535000068, -3.609488729914999805, -5.855142811286000004 ) ) ;
#23490 = FACE_OUTER_BOUND ( 'NONE', #62156, .T. ) ;
#23491 = ORIENTED_EDGE ( 'NONE', *, *, #24138, .T. ) ;
#23492 = CARTESIAN_POINT ( 'NONE',  ( 10.98768577056000062, -2.700436730051000378, -4.945210085382000464 ) ) ;
#23493 = CARTESIAN_POINT ( 'NONE',  ( 11.36486084871759950, -5.207010770456999893, -7.825000000000000178 ) ) ;
#23494 = CARTESIAN_POINT ( 'NONE',  ( 10.27736255359000062, -4.572640260524000411, 5.004092596557000228 ) ) ;
#23495 = FACE_OUTER_BOUND ( 'NONE', #3084, .T. ) ;
#23496 = CARTESIAN_POINT ( 'NONE',  ( 10.24160887879199855, 3.710311786319799854, -6.254020414961999563 ) ) ;
#23497 = CARTESIAN_POINT ( 'NONE',  ( 12.19623795424363344, 2.642762699020543504, 13.64211084970869514 ) ) ;
#23498 = CARTESIAN_POINT ( 'NONE',  ( 10.66951732929000052, -4.592671928130000580, 5.841406818427000047 ) ) ;
#23499 = VERTEX_POINT ( 'NONE', #20 ) ;
#23500 = CARTESIAN_POINT ( 'NONE',  ( 11.21022026213526601, 5.045753393512712570, -7.824998325091605977 ) ) ;
#23501 = CARTESIAN_POINT ( 'NONE',  ( 12.27511425286870406, 0.4989076128645561492, 13.99111800451625243 ) ) ;
#23502 = ORIENTED_EDGE ( 'NONE', *, *, #39621, .F. ) ;
#23503 = CARTESIAN_POINT ( 'NONE',  ( 6.775409439180998916, 5.278582711742999756, -7.933273873238999130 ) ) ;
#23504 = CARTESIAN_POINT ( 'NONE',  ( 10.90000000000000036, 5.599999999999999645, 6.571291218949999902 ) ) ;
#23505 = CARTESIAN_POINT ( 'NONE',  ( 23.73665640592300363, -3.437546595577999575, -13.35043945363000084 ) ) ;
#23506 = CARTESIAN_POINT ( 'NONE',  ( 1.700000379347999857, -1.775000379263000028, 7.150861857908999773E-10 ) ) ;
#23507 = B_SPLINE_CURVE_WITH_KNOTS ( 'NONE', 3,
 ( #462, #58163, #5703, #63741 ),
 .UNSPECIFIED., .F., .F.,
 ( 4, 4 ),
 ( 0.000000000000000000, 0.1254918003289636208 ),
 .UNSPECIFIED. ) ;
#23508 = CARTESIAN_POINT ( 'NONE',  ( 8.789679719592999874, 4.162493982103000256, -5.775210092227999858 ) ) ;
#23509 = DIRECTION ( 'NONE',  ( 1.000000000000000000, 0.000000000000000000, 0.000000000000000000 ) ) ;
#23510 = CARTESIAN_POINT ( 'NONE',  ( 11.09999999999999964, -6.593648099371000271, -5.598803483715999896 ) ) ;
#23511 = CARTESIAN_POINT ( 'NONE',  ( 20.75138802851920161, 0.000000000000000000, 0.000000000000000000 ) ) ;
#23512 = CARTESIAN_POINT ( 'NONE',  ( 18.30017264560542145, 1.838307227263772159, -11.74271423084882571 ) ) ;
#23513 = CARTESIAN_POINT ( 'NONE',  ( 10.50333291544900050, -3.468906853242413657, -8.658936933361777832 ) ) ;
#23514 = CARTESIAN_POINT ( 'NONE',  ( 9.040134009213000255, -5.099406281193999746, -6.669356233738001016 ) ) ;
#23515 = CARTESIAN_POINT ( 'NONE',  ( 10.99826088462129903, 4.001843064679911244, -6.633804182961699603 ) ) ;
#23516 = CARTESIAN_POINT ( 'NONE',  ( 1.115556799208874850, 0.4581489286485002088, 3.500000000000001776 ) ) ;
#23517 = EDGE_CURVE ( 'NONE', #61050, #21198, #63293, .T. ) ;
#23518 = EDGE_CURVE ( 'NONE', #34596, #7076, #47670, .T. ) ;
#23519 = CARTESIAN_POINT ( 'NONE',  ( 11.64633327354034797, 3.135095881599500256, -6.934277916748599502 ) ) ;
#23520 = CARTESIAN_POINT ( 'NONE',  ( 9.176721904869998170, 4.995641764568400589, -8.058956102599799109 ) ) ;
#23522 = DIRECTION ( 'NONE',  ( 1.000000000000000000, 0.000000000000000000, 0.000000000000000000 ) ) ;
#23521 = CARTESIAN_POINT ( 'NONE',  ( 8.241912900173000267, -4.599999999999999645, 6.117539782833000928 ) ) ;
#23523 = CARTESIAN_POINT ( 'NONE',  ( 7.717206997734000318, 2.839603336731772565, 6.809939399899146650 ) ) ;
#23524 = VERTEX_POINT ( 'NONE', #26254 ) ;
#23525 = CIRCLE ( 'NONE', #48083, 5.000000000000000000 ) ;
#23526 = CARTESIAN_POINT ( 'NONE',  ( 11.64633327354034797, 3.135095881599500256, 8.065722083251399610 ) ) ;
#23527 = CARTESIAN_POINT ( 'NONE',  ( 10.00137895011999944, -3.855365288061999962, 5.709482985498999241 ) ) ;
#23528 = CARTESIAN_POINT ( 'NONE',  ( 9.226430433046999724, 3.028322657068899915, 8.099647887697699389 ) ) ;
#23529 = CARTESIAN_POINT ( 'NONE',  ( 9.429533309317625012, 4.633212041316643770, -6.896199718737570095 ) ) ;
#23530 = AXIS2_PLACEMENT_3D ( 'NONE', #3894, #46219, #18961 ) ;
#23531 = CARTESIAN_POINT ( 'NONE',  ( 10.46933016578999975, -4.988498232033999891, 6.213103211926000569 ) ) ;
#23532 = CARTESIAN_POINT ( 'NONE',  ( 9.669679685929221336, -5.627806328728547136, 6.860704028586689596 ) ) ;
#23533 = VERTEX_POINT ( 'NONE', #25563 ) ;
#23534 = ADVANCED_FACE ( 'NONE', ( #20659 ), #62609, .T. ) ;
#23535 = CIRCLE ( 'NONE', #14609, 1.000000000000000000 ) ;
#23536 = CARTESIAN_POINT ( 'NONE',  ( 9.708633995697999453, -2.865156490077000129, -7.625954975973699312 ) ) ;
#23537 = CARTESIAN_POINT ( 'NONE',  ( 9.635596873516670158, -2.907767014557175678, -6.870476274536380323 ) ) ;
#23538 = CARTESIAN_POINT ( 'NONE',  ( 5.800819726243000574, -0.04112960214766999550, -1.467935932961000001 ) ) ;
#23539 = EDGE_CURVE ( 'NONE', #64966, #34497, #47581, .T. ) ;
#23540 = CARTESIAN_POINT ( 'NONE',  ( 9.264851123445994929, -2.902720251407998830, -6.598525194663996452 ) ) ;
#23541 = CARTESIAN_POINT ( 'NONE',  ( 5.500000000000000000, 12.78667792605000031, 2.345384795462000405 ) ) ;
#23542 = CARTESIAN_POINT ( 'NONE',  ( 11.70794988689359961, 4.455786710255300598, -8.393984925606600811 ) ) ;
#23543 = CARTESIAN_POINT ( 'NONE',  ( 18.90826270587400160, -11.65000000000000036, 0.000000000000000000 ) ) ;
#23544 = CARTESIAN_POINT ( 'NONE',  ( 9.705325322606999094, -5.130141620686999637, -6.219151643305999677 ) ) ;
#23545 = CARTESIAN_POINT ( 'NONE',  ( 10.58422653167975902, 2.899999999999999911, 6.304440313954331465 ) ) ;
#23546 = EDGE_LOOP ( 'NONE', ( #169, #12073, #56895, #4037 ) ) ;
#23547 = CARTESIAN_POINT ( 'NONE',  ( 0.000000000000000000, -2.899969545326000375, -0.3804588500739426449 ) ) ;
#23548 = CARTESIAN_POINT ( 'NONE',  ( 12.32658172867158441, -0.5491314443420151070, -13.98923457196397635 ) ) ;
#23549 = CARTESIAN_POINT ( 'NONE',  ( 5.500000000000000000, 0.5415384615384001288, 2.132307692307999769 ) ) ;
#23550 = CARTESIAN_POINT ( 'NONE',  ( 24.67552801389400230, -8.698828566341001434, -9.015209094485999941 ) ) ;
#23551 = CARTESIAN_POINT ( 'NONE',  ( 4.900006121741999898, 1.999999999999999112, -0.2617993877991531826 ) ) ;
#23552 = CARTESIAN_POINT ( 'NONE',  ( 7.000000000000001776, 10.07825177844479647, 4.450660970158813790 ) ) ;
#23553 = CARTESIAN_POINT ( 'NONE',  ( 5.629847151467805233, 12.10477468259546896, -3.742618271631844351 ) ) ;
#23554 = ORIENTED_EDGE ( 'NONE', *, *, #60554, .F. ) ;
#23555 = CARTESIAN_POINT ( 'NONE',  ( 23.60205915885299888, 9.361474752776006270, 7.912850866691996998 ) ) ;
#23556 = CARTESIAN_POINT ( 'NONE',  ( 17.91291100103719458, 1.987489628841895062, -13.76889314140747800 ) ) ;
#23557 = ORIENTED_EDGE ( 'NONE', *, *, #22490, .F. ) ;
#23558 = DIRECTION ( 'NONE',  ( -0.000000000000000000, -0.000000000000000000, 1.000000000000000000 ) ) ;
#23559 = CARTESIAN_POINT ( 'NONE',  ( 2.717640132544332676, -1.762666431298159475, 3.058252359239895135 ) ) ;
#23560 = CARTESIAN_POINT ( 'NONE',  ( 9.053070280414001303, 2.391443348526999912, -6.856688371964000162 ) ) ;
#23561 = CARTESIAN_POINT ( 'NONE',  ( 9.099999931440999390, 5.064317881551000156, 6.844464000216799349 ) ) ;
#23562 = CARTESIAN_POINT ( 'NONE',  ( 10.97124174884019965, -4.036194082918090231, -8.815770025351000072 ) ) ;
#23563 = CARTESIAN_POINT ( 'NONE',  ( 17.82907313225565105, 0.5620966109058860294, -12.68325743355609347 ) ) ;
#23564 = CIRCLE ( 'NONE', #38078, 1.300172478116999208 ) ;
#23565 = CARTESIAN_POINT ( 'NONE',  ( 11.59999999999999964, -4.000000000000000000, -7.500000000000000000 ) ) ;
#23566 = ORIENTED_EDGE ( 'NONE', *, *, #3989, .T. ) ;
#23567 = CARTESIAN_POINT ( 'NONE',  ( 11.09999999999999964, 5.350000000000000533, -7.500000000000000000 ) ) ;
#23568 = CARTESIAN_POINT ( 'NONE',  ( -2.147830119999999621, -1.300000000000000044, -9.662944685757000940 ) ) ;
#23569 = CARTESIAN_POINT ( 'NONE',  ( 17.55505043854147118, -1.875000000000000000, 13.78631952119024895 ) ) ;
#23570 = VERTEX_POINT ( 'NONE', #31167 ) ;
#23571 = CARTESIAN_POINT ( 'NONE',  ( 9.988718791410999387, 2.842026940133999702, -6.504333051298999635 ) ) ;
#23572 = ORIENTED_EDGE ( 'NONE', *, *, #30699, .T. ) ;
#23573 = CARTESIAN_POINT ( 'NONE',  ( 10.06324205624999912, 3.590523439766200031, 6.434137271007999814 ) ) ;
#23574 = CARTESIAN_POINT ( 'NONE',  ( 18.23388167758336920, -2.733449996235739032, -12.29993400349665045 ) ) ;
#23575 = CONICAL_SURFACE ( 'NONE', #55927, 12.71246950475999959, 0.8960553845711767273 ) ;
#23576 = ADVANCED_BREP_SHAPE_REPRESENTATION ( '', ( #31992, #9676 ), #756 ) ;
#23577 = CARTESIAN_POINT ( 'NONE',  ( 10.98768472569999943, 6.720753179915999631, -5.471698458723999181 ) ) ;
#23578 = CARTESIAN_POINT ( 'NONE',  ( 5.700000000000000178, -1.433333333332999837, 10.65401593558000037 ) ) ;
#23579 = CARTESIAN_POINT ( 'NONE',  ( 11.80738107398800274, -11.64644714240999868, -1.863397721619000080 ) ) ;
#23580 = EDGE_CURVE ( 'NONE', #1011, #56588, #10145, .T. ) ;
#23581 = VECTOR ( 'NONE', #9130, 1000.000000000000000 ) ;
#23582 = CARTESIAN_POINT ( 'NONE',  ( 8.952784697134999803, 4.470490447737899942, 8.228249052908999772 ) ) ;
#23583 = CARTESIAN_POINT ( 'NONE',  ( 9.510967806033882255, -2.744763247581829990, 6.279873002373912882 ) ) ;
#23584 = ORIENTED_EDGE ( 'NONE', *, *, #33792, .T. ) ;
#23585 = CARTESIAN_POINT ( 'NONE',  ( 5.500000000000000000, 0.000000000000000000, -1.449999999999970202 ) ) ;
#23586 = CARTESIAN_POINT ( 'NONE',  ( 10.54684221959000112, 3.691673619534999951, -9.157283848447001162 ) ) ;
#23587 = CARTESIAN_POINT ( 'NONE',  ( 8.763353253171903390, 3.867553254011502961, 6.586646690369097890 ) ) ;
#23588 = CARTESIAN_POINT ( 'NONE',  ( 12.08553199184720128, 2.425689856710291803, -13.78827816593211786 ) ) ;
#23589 = CARTESIAN_POINT ( 'NONE',  ( 11.23976354018279977, -4.327184855449098144, 8.717465845835395299 ) ) ;
#23590 = CARTESIAN_POINT ( 'NONE',  ( 24.45998324064000329, 3.150049453514000231, 11.96533647240999976 ) ) ;
#23591 = CARTESIAN_POINT ( 'NONE',  ( 17.55505043854143921, -0.7302158263239079128, 13.98094363220831227 ) ) ;
#23592 = CARTESIAN_POINT ( 'NONE',  ( 25.39410189985537514, -8.421101446676589219, 8.066020039750368298 ) ) ;
#23593 = VERTEX_POINT ( 'NONE', #3880 ) ;
#23594 = VERTEX_POINT ( 'NONE', #36048 ) ;
#23595 = CARTESIAN_POINT ( 'NONE',  ( 9.047164158776000775, 2.156584729807999867, -7.959751745006000689 ) ) ;
#23596 = CARTESIAN_POINT ( 'NONE',  ( 12.80505043854144276, -0.6250000000000001110, 13.88107975066923316 ) ) ;
#23597 = CARTESIAN_POINT ( 'NONE',  ( 12.18203530713735816, -2.449198598491955536, 13.68410320369877731 ) ) ;
#23598 = CARTESIAN_POINT ( 'NONE',  ( 9.185618987146705550, -5.739014642741299355, 7.194290269894461964 ) ) ;
#23599 = EDGE_CURVE ( 'NONE', #28041, #6018, #67707, .T. ) ;
#23600 = EDGE_CURVE ( 'NONE', #28855, #31101, #30809, .T. ) ;
#23601 = CARTESIAN_POINT ( 'NONE',  ( 8.320870559624999885, -3.894643656844000379, 6.044452984962999764 ) ) ;
#23602 = CARTESIAN_POINT ( 'NONE',  ( 11.53111947020579819, -4.908799224006100026, 7.825000000000000178 ) ) ;
#23604 = CARTESIAN_POINT ( 'NONE',  ( 10.96873203361999849, -6.471573332185999838, 5.204310805270999651 ) ) ;
#23603 = CARTESIAN_POINT ( 'NONE',  ( 10.64029229006299992, -2.893743561734000380, 8.142324746736500529 ) ) ;
#23605 = CARTESIAN_POINT ( 'NONE',  ( 10.86272200990529946, 2.793294545435000220, -7.079074440652799893 ) ) ;
#23606 = ORIENTED_EDGE ( 'NONE', *, *, #47292, .T. ) ;
#23607 = EDGE_CURVE ( 'NONE', #43113, #50410, #22023, .T. ) ;
#23608 = CARTESIAN_POINT ( 'NONE',  ( 11.09999999999999964, 6.593648131501000265, 5.598803515845999890 ) ) ;
#23609 = CARTESIAN_POINT ( 'NONE',  ( 11.13327849887000021, -2.674582802342999610, -4.980994678569999223 ) ) ;
#23610 = CARTESIAN_POINT ( 'NONE',  ( 18.14710087547454975, 0.2005123242923287363, 12.69787478206144016 ) ) ;
#23611 = DIRECTION ( 'NONE',  ( -1.000000000000000000, 0.000000000000000000, 0.000000000000000000 ) ) ;
#23612 = CARTESIAN_POINT ( 'NONE',  ( 4.149992563291998948, -1.007210908820212358, 1.747525841223983800 ) ) ;
#23613 = ORIENTED_EDGE ( 'NONE', *, *, #63736, .F. ) ;
#23615 = CARTESIAN_POINT ( 'NONE',  ( 9.883148997457000817, 5.167567567567999731, 6.822293592207000934 ) ) ;
#23614 = CARTESIAN_POINT ( 'NONE',  ( 11.80565467195988916, -5.136173005413446013, 8.088082908809447247 ) ) ;
#23616 = CARTESIAN_POINT ( 'NONE',  ( 8.564679719593000229, 4.146787477634999775, -5.941926545671999627 ) ) ;
#23617 = B_SPLINE_CURVE_WITH_KNOTS ( 'NONE', 3,
 ( #55819, #7922, #61060, #29610 ),
 .UNSPECIFIED., .F., .F.,
 ( 4, 4 ),
 ( 0.000000000000000000, 1.000000000000000000 ),
 .UNSPECIFIED. ) ;
#23618 = CARTESIAN_POINT ( 'NONE',  ( 12.37517135966890258, -2.046199321548340500, 13.75929785978298270 ) ) ;
#23619 = B_SPLINE_CURVE_WITH_KNOTS ( 'NONE', 3,
 ( #57533, #46717, #40427, #51602, #25038, #13871, #20479, #67331, #68019, #35202, #62095, #19450, #56512, #8618, #30634, #59254, #53677, #5771 ),
 .UNSPECIFIED., .F., .F.,
 ( 4, 2, 2, 2, 2, 2, 2, 2, 4 ),
 ( 0.000000000000000000, 0.1250000000000000000, 0.2500000000000000000, 0.3750000000000000000, 0.5000000000000000000, 0.6250000000000000000, 0.7500000000000000000, 0.8750000000000000000, 1.000000000000000000 ),
 .UNSPECIFIED. ) ;
#23620 = CARTESIAN_POINT ( 'NONE',  ( 10.27195525820100031, 3.879327850572200198, 8.772302877803999976 ) ) ;
#23621 = SURFACE_STYLE_USAGE ( .BOTH. , #66951 ) ;
#23622 = EDGE_CURVE ( 'NONE', #34052, #66938, #11741, .T. ) ;
#23623 = FACE_OUTER_BOUND ( 'NONE', #63264, .T. ) ;
#23624 = CARTESIAN_POINT ( 'NONE',  ( 3.310521893996000387, -2.689871800245000610, 2.380848019370000124 ) ) ;
#23625 = ORIENTED_EDGE ( 'NONE', *, *, #58868, .F. ) ;
#23626 = CARTESIAN_POINT ( 'NONE',  ( 12.08004251007353957, 0.01123479547582826449, -12.60000044989513590 ) ) ;
#23629 = AXIS2_PLACEMENT_3D ( 'NONE', #37502, #25987, #68620 ) ;
#23628 = DIRECTION ( 'NONE',  ( -1.000000000000000000, 0.000000000000000000, 0.000000000000000000 ) ) ;
#23627 = B_SPLINE_CURVE_WITH_KNOTS ( 'NONE', 3,
 ( #5416, #16592, #42821, #58549 ),
 .UNSPECIFIED., .F., .F.,
 ( 4, 4 ),
 ( 0.000000000000000000, 1.000000000000000000 ),
 .UNSPECIFIED. ) ;
#23630 = CARTESIAN_POINT ( 'NONE',  ( 23.85842837956922580, -12.93469165770115481, -3.627720848801395448 ) ) ;
#23631 = CARTESIAN_POINT ( 'NONE',  ( 24.56351374471499938, 3.482977112968999922, -12.16506632497999973 ) ) ;
#23632 = ORIENTED_EDGE ( 'NONE', *, *, #4743, .T. ) ;
#23633 = CARTESIAN_POINT ( 'NONE',  ( 6.098107267216000160, 1.122942780917999928, 0.3495427174121999991 ) ) ;
#23634 = CARTESIAN_POINT ( 'NONE',  ( 7.639760841226999943, 5.116254232901999544, -8.340852485897000790 ) ) ;
#23636 = FACE_OUTER_BOUND ( 'NONE', #33851, .T. ) ;
#23635 = CARTESIAN_POINT ( 'NONE',  ( 44.24148000000000280, -2.258942858049999725, -12.29419282279000036 ) ) ;
#23637 = CARTESIAN_POINT ( 'NONE',  ( 11.71922412107039868, 4.069539071394910223, -6.185573549454999487 ) ) ;
#23638 = ORIENTED_EDGE ( 'NONE', *, *, #66913, .F. ) ;
#23639 = FACE_OUTER_BOUND ( 'NONE', #18425, .T. ) ;
#23640 = ORIENTED_EDGE ( 'NONE', *, *, #43257, .T. ) ;
#23641 = CARTESIAN_POINT ( 'NONE',  ( 9.766851002543001314, 2.832432432432000269, 6.822293592207000934 ) ) ;
#23642 = CARTESIAN_POINT ( 'NONE',  ( 24.76776046854388724, -8.625624972805100654, -8.557838011048463756 ) ) ;
#23643 = AXIS2_PLACEMENT_3D ( 'NONE', #62088, #52288, #63455 ) ;
#23644 = CARTESIAN_POINT ( 'NONE',  ( 17.91845017417216113, 0.6323113780857140265, -13.98571806661953154 ) ) ;
#23645 = ORIENTED_EDGE ( 'NONE', *, *, #16807, .T. ) ;
#23646 = CARTESIAN_POINT ( 'NONE',  ( 10.94168356394703601, 9.287995240817338072, -6.252185766115418097 ) ) ;
#23647 = CARTESIAN_POINT ( 'NONE',  ( 8.331682176603999679, 5.101289360622999425, 6.607176324693000424 ) ) ;
#23648 = CARTESIAN_POINT ( 'NONE',  ( 7.540789158769000800, 5.122039080790999677, -6.666882531104000087 ) ) ;
#23649 = CARTESIAN_POINT ( 'NONE',  ( 10.17500046684965120, 2.650307855385062972, 7.500001770945063484 ) ) ;
#23650 = CARTESIAN_POINT ( 'NONE',  ( 18.14127614474869787, -2.717147700817308831, 12.39835379065202225 ) ) ;
#23651 = ORIENTED_EDGE ( 'NONE', *, *, #47045, .F. ) ;
#23652 = CARTESIAN_POINT ( 'NONE',  ( 9.660528907822998335, 2.899999999999999911, -6.152188490330000370 ) ) ;
#23653 = CARTESIAN_POINT ( 'NONE',  ( 23.81982929170500185, -12.91659203753999918, -3.707450659729000453 ) ) ;
#23654 = CARTESIAN_POINT ( 'NONE',  ( 10.97843137008999825, 5.235400103863000254, 6.782920672145000829 ) ) ;
#23655 = CARTESIAN_POINT ( 'NONE',  ( 11.09999999999999964, -5.538898460221000519, 7.685179721164000277 ) ) ;
#23656 = VERTEX_POINT ( 'NONE', #1061 ) ;
#23657 = DIRECTION ( 'NONE',  ( -1.000000000000000000, 0.000000000000000000, 0.000000000000000000 ) ) ;
#23658 = CARTESIAN_POINT ( 'NONE',  ( 8.857090631127384484, -3.380484464318182614, -6.695274228472992917 ) ) ;
#23659 = CARTESIAN_POINT ( 'NONE',  ( 23.60000000000000142, -11.85420044612000012, 3.901016762742000488 ) ) ;
#23660 = ADVANCED_FACE ( 'NONE', ( #6987 ), #44043, .F. ) ;
#23661 = CARTESIAN_POINT ( 'NONE',  ( 5.500000000000000000, -12.87590651766999983, -2.791353855799999728 ) ) ;
#23662 = LINE ( 'NONE', #12839, #14260 ) ;
#23663 = EDGE_CURVE ( 'NONE', #16917, #7065, #53484, .T. ) ;
#23664 = CARTESIAN_POINT ( 'NONE',  ( 12.23548570231569066, -0.2575405707509104136, -13.89679341043304106 ) ) ;
#23665 = CARTESIAN_POINT ( 'NONE',  ( 17.78683280784129650, -3.080523647204256754, 12.29718062304645620 ) ) ;
#23666 = ORIENTED_EDGE ( 'NONE', *, *, #50052, .T. ) ;
#23667 = CARTESIAN_POINT ( 'NONE',  ( 10.35814141025499957, -3.516507310755200066, -8.361148840840000318 ) ) ;
#23668 = B_SPLINE_CURVE_WITH_KNOTS ( 'NONE', 3,
 ( #23994, #7225, #60707, #45329, #22951, #12825 ),
 .UNSPECIFIED., .F., .F.,
 ( 4, 2, 4 ),
 ( 0.000000000000000000, 0.5000000000000000000, 1.000000000000000000 ),
 .UNSPECIFIED. ) ;
#23669 = B_SPLINE_CURVE_WITH_KNOTS ( 'NONE', 3,
 ( #8262, #33809, #45332, #29611 ),
 .UNSPECIFIED., .F., .F.,
 ( 4, 4 ),
 ( 0.000000000000000000, 1.000000000000000000 ),
 .UNSPECIFIED. ) ;
#23670 = ORIENTED_EDGE ( 'NONE', *, *, #48470, .F. ) ;
#23671 = CARTESIAN_POINT ( 'NONE',  ( 0.1499942179680000265, 0.7197945678028339067, 2.678379783547567339 ) ) ;
#23672 = CARTESIAN_POINT ( 'NONE',  ( 8.541054719591000932, 3.807713920470999991, -9.221758713517999695 ) ) ;
#23673 = AXIS2_PLACEMENT_3D ( 'NONE', #50651, #56582, #60793 ) ;
#23674 = CARTESIAN_POINT ( 'NONE',  ( 3.334741359309999709, 1.648620317156999970, 2.760184582139999954 ) ) ;
#23675 = CARTESIAN_POINT ( 'NONE',  ( 10.94349328348999961, -3.081618981425999770, -8.919377696680001577 ) ) ;
#23676 = CARTESIAN_POINT ( 'NONE',  ( 6.838517237264255755, 1.484920755282000515, -0.3138429810103637307 ) ) ;
#23677 = DIRECTION ( 'NONE',  ( 0.000000000000000000, 0.000000000000000000, -1.000000000000000000 ) ) ;
#23678 = B_SPLINE_CURVE_WITH_KNOTS ( 'NONE', 3,
 ( #17382, #65613, #64572, #12141, #53752, #22618, #5510, #32779, #17027, #38360, #16343, #27884, #59685, #33471, #54787, #43619, #1649, #11785 ),
 .UNSPECIFIED., .F., .F.,
 ( 4, 2, 2, 2, 2, 2, 2, 2, 4 ),
 ( 0.000000000000000000, 0.1249999999999996669, 0.2499999999999993339, 0.3749999999999990008, 0.4999999999999986677, 0.6249999999999990008, 0.7499999999999993339, 0.8749999999999996669, 1.000000000000000000 ),
 .UNSPECIFIED. ) ;
#23679 = DIRECTION ( 'NONE',  ( 0.000000000000000000, 0.8648648648648717963, 0.5020047465136827647 ) ) ;
#23680 = ORIENTED_EDGE ( 'NONE', *, *, #53316, .T. ) ;
#23681 = CARTESIAN_POINT ( 'NONE',  ( 10.85826357027499967, -3.149486845331399998, 7.335909308151700614 ) ) ;
#23682 = CARTESIAN_POINT ( 'NONE',  ( 10.66052890781999984, 2.899999999999999911, -6.152188490330000370 ) ) ;
#23683 = CARTESIAN_POINT ( 'NONE',  ( 18.50013789939208664, 2.065999734462983189E-14, -11.64999999999999325 ) ) ;
#23684 = EDGE_CURVE ( 'NONE', #16325, #37501, #16774, .T. ) ;
#23685 = CARTESIAN_POINT ( 'NONE',  ( 12.80505043854144276, -0.6250000000000001110, -12.67928921589118652 ) ) ;
#23686 = CARTESIAN_POINT ( 'NONE',  ( 9.169143502787418853, 2.970327438714448931, 8.373611167771709773 ) ) ;
#23687 = CONICAL_SURFACE ( 'NONE', #66101, 12.42518894556000042, 0.7854133338342391690 ) ;
#23688 = CARTESIAN_POINT ( 'NONE',  ( 10.65364694612719809, 3.195501139158400061, -7.821061011719899980 ) ) ;
#23689 = EDGE_CURVE ( 'NONE', #56100, #38774, #38106, .T. ) ;
#23690 = DIRECTION ( 'NONE',  ( 0.000000000000000000, -1.000000000000000000, 0.000000000000000000 ) ) ;
#23691 = CARTESIAN_POINT ( 'NONE',  ( 10.41488779216199845, 4.929030047862200448, -7.835030859477799758 ) ) ;
#23692 = B_SPLINE_CURVE_WITH_KNOTS ( 'NONE', 3,
 ( #2652, #24325, #45658, #7213, #28194, #19071, #39724, #61042, #49860, #40399, #44291, #50211, #33443, #60350, #13163, #7904, #23980, #61721, #55107, #28550, #23295, #44636, #65928, #18056, #60694, #12809, #34138, #35510, #47026, #13841, #30267, #62742, #8930, #63079, #4699, #25348, #29937, #68677, #68329, #3668, #19419, #62067 ),
 .UNSPECIFIED., .F., .F.,
 ( 4, 2, 2, 1, 2, 2, 2, 2, 1, 1, 1, 2, 2, 2, 2, 2, 2, 2, 2, 2, 2, 2, 4 ),
 ( 0.000000000000000000, 0.06250000000000227596, 0.09375000000000296985, 0.1093750000000033168, 0.1171875000000036221, 0.1250000000000039413, 0.1875000000000053013, 0.2187500000000060230, 0.2343750000000058564, 0.2421875000000067724, 0.2460937500000072164, 0.2480468750000070222, 0.2500000000000068279, 0.3125000000000048295, 0.3437500000000036082, 0.3593750000000036082, 0.3750000000000035527, 0.4374999999999996669, 0.4687499999999985012, 0.4999999999999973910, 0.6249999999999982236, 0.7499999999999990008, 1.000000000000000000 ),
 .UNSPECIFIED. ) ;
#23693 = CARTESIAN_POINT ( 'NONE',  ( 17.96742813929298421, -0.5917181940048611422, 12.58609996267493081 ) ) ;
#23694 = FACE_OUTER_BOUND ( 'NONE', #4775, .T. ) ;
#23695 = DIRECTION ( 'NONE',  ( 0.8843050093870579165, 0.1786785976936114684, 0.4313682986720279167 ) ) ;
#23696 = CARTESIAN_POINT ( 'NONE',  ( 10.25880778041000063, 2.491777456852000139, -7.289938575364999451 ) ) ;
#23697 = ORIENTED_EDGE ( 'NONE', *, *, #59217, .F. ) ;
#23698 = CARTESIAN_POINT ( 'NONE',  ( 9.362879440377000151, -3.677416446733000388, 9.250734868033999803 ) ) ;
#23699 = CARTESIAN_POINT ( 'NONE',  ( 17.65134488495969123, 1.793858269351531254, 13.88459860980089644 ) ) ;
#23700 = CARTESIAN_POINT ( 'NONE',  ( 23.56682227024313647, 2.990440059702627273, 13.66659919071918772 ) ) ;
#23701 = CARTESIAN_POINT ( 'NONE',  ( 10.26990035061499817, 4.231093494672100164, 6.664354444139199529 ) ) ;
#23702 = ORIENTED_EDGE ( 'NONE', *, *, #7257, .F. ) ;
#23703 = CARTESIAN_POINT ( 'NONE',  ( 8.989142219592000771, 5.284130523641000110, 6.489275570566000795 ) ) ;
#23704 = EDGE_CURVE ( 'NONE', #65709, #25033, #63791, .T. ) ;
#23706 = DIRECTION ( 'NONE',  ( 1.000000000000000000, -2.612724851285000276E-14, -1.006602208993000106E-14 ) ) ;
#23705 = FACE_OUTER_BOUND ( 'NONE', #65145, .T. ) ;
#23707 = CARTESIAN_POINT ( 'NONE',  ( 16.10005255078199937, 3.632778330393000132, 11.06917548872000090 ) ) ;
#23708 = ORIENTED_EDGE ( 'NONE', *, *, #67689, .T. ) ;
#23709 = CARTESIAN_POINT ( 'NONE',  ( 10.61382428715999993, 3.385080336122999967, 5.849521480782000182 ) ) ;
#23710 = CARTESIAN_POINT ( 'NONE',  ( 17.82352195865856714, -3.196339915866920123, -13.63023968027430755 ) ) ;
#23711 = CARTESIAN_POINT ( 'NONE',  ( 11.65456516821461008, 4.802916961510000249, 6.689681884064299311 ) ) ;
#23712 = CARTESIAN_POINT ( 'NONE',  ( 10.83659005484000026, -5.133183563847000030, 8.848364935581999546 ) ) ;
#23713 = CARTESIAN_POINT ( 'NONE',  ( 7.581295643773000137, 2.929975047062999050, 6.543750339501001712 ) ) ;
#23714 = VERTEX_POINT ( 'NONE', #363 ) ;
#23715 = DIRECTION ( 'NONE',  ( 0.000000000000000000, -0.7158784314710769925, 0.6982249432342778617 ) ) ;
#23716 = CARTESIAN_POINT ( 'NONE',  ( 1.490556799207374716, 3.500000000000001776, -0.4581489286485044832 ) ) ;
#23717 = CARTESIAN_POINT ( 'NONE',  ( 7.902908229829841424, -2.546181505345110008, 8.455233271057512212 ) ) ;
#23718 = CARTESIAN_POINT ( 'NONE',  ( 10.46933016578999975, -4.988498232033999891, 6.213103211926000569 ) ) ;
#23719 = CARTESIAN_POINT ( 'NONE',  ( 10.72191429142990060, -3.974927396630719922, -6.183971186511000084 ) ) ;
#23720 = CARTESIAN_POINT ( 'NONE',  ( 9.155265421555000671, -4.188500707411799695, 6.524915741324599949 ) ) ;
#23721 = ORIENTED_EDGE ( 'NONE', *, *, #38342, .F. ) ;
#23723 = CARTESIAN_POINT ( 'NONE',  ( 7.975339216757242333, 5.350090185752605976, 7.499980949462685231 ) ) ;
#23722 = CIRCLE ( 'NONE', #58346, 0.5999999999999999778 ) ;
#23724 = CARTESIAN_POINT ( 'NONE',  ( 11.31764560330029923, -3.650429500487800460, 8.585859374935999710 ) ) ;
#23725 = VERTEX_POINT ( 'NONE', #59432 ) ;
#23726 = CARTESIAN_POINT ( 'NONE',  ( 9.231616107288068918, -3.999997736744774546, 6.618420992905502231 ) ) ;
#23727 = ORIENTED_EDGE ( 'NONE', *, *, #42056, .F. ) ;
#23728 = CARTESIAN_POINT ( 'NONE',  ( 10.06233042975999936, -5.062748727288000516, -8.618689820632001286 ) ) ;
#23729 = CARTESIAN_POINT ( 'NONE',  ( 8.233179719589999834, 5.203550244299999683, -8.391678825488000371 ) ) ;
#23730 = CARTESIAN_POINT ( 'NONE',  ( 9.411640687503366465, -2.873222873813585654, -6.752018918873797126 ) ) ;
#23731 = CARTESIAN_POINT ( 'NONE',  ( 24.96666885022796478, 8.756202917673951092, 7.455126455300256083 ) ) ;
#23732 = CARTESIAN_POINT ( 'NONE',  ( 12.52605318029421078, 1.940633248599431537, -12.56447441435821943 ) ) ;
#23733 = CARTESIAN_POINT ( 'NONE',  ( 11.66641369783139837, -4.050626550392200542, 6.497808498716000081 ) ) ;
#23734 = CARTESIAN_POINT ( 'NONE',  ( 11.35679632507500081, -3.509334349252600127, 6.590394082213600235 ) ) ;
#23735 = ORIENTED_EDGE ( 'NONE', *, *, #42168, .T. ) ;
#23736 = CARTESIAN_POINT ( 'NONE',  ( 7.645558129953747617, 3.263515245515704155, 8.650331983164434746 ) ) ;
#23737 = TOROIDAL_SURFACE ( 'NONE', #29346, 7.720759220056000238, 1.000000000000000000 ) ;
#23738 = ORIENTED_EDGE ( 'NONE', *, *, #39585, .F. ) ;
#23739 = CARTESIAN_POINT ( 'NONE',  ( 7.374102686541000651, -4.389298280625000714, 9.135255728583000945 ) ) ;
#23740 = CARTESIAN_POINT ( 'NONE',  ( 7.950512946206999665, 3.409920107335999706, -6.285779624696999690 ) ) ;
#23741 = ORIENTED_EDGE ( 'NONE', *, *, #37638, .T. ) ;
#23742 = CARTESIAN_POINT ( 'NONE',  ( 12.08117318674012708, -2.436835578774661837, -12.36211850556986214 ) ) ;
#23743 = CARTESIAN_POINT ( 'NONE',  ( 11.67918044953561996, 5.011483761127000669, 6.972563939641199582 ) ) ;
#23744 = FACE_OUTER_BOUND ( 'NONE', #55294, .T. ) ;
#23745 = CARTESIAN_POINT ( 'NONE',  ( 6.305026506349999948, 1.500000000000000000, 0.000000000000000000 ) ) ;
#23746 = CARTESIAN_POINT ( 'NONE',  ( 17.93509931767800225, -11.57247339239000006, 4.892741173462999527 ) ) ;
#23747 = ADVANCED_FACE ( 'NONE', ( #11531 ), #45761, .F. ) ;
#23748 = CARTESIAN_POINT ( 'NONE',  ( 7.000000000000000000, -0.2392304845412999981, -3.000000000000000000 ) ) ;
#23749 = CARTESIAN_POINT ( 'NONE',  ( 12.54503913623225131, -3.068442045733653867, -13.53626685534801588 ) ) ;
#23750 = EDGE_CURVE ( 'NONE', #42176, #57880, #12065, .T. ) ;
#23751 = CARTESIAN_POINT ( 'NONE',  ( 18.08617525414963723, -0.3300695133819651073, -12.69424233780836531 ) ) ;
#23752 =( NAMED_UNIT ( * ) SI_UNIT ( $, .STERADIAN. ) SOLID_ANGLE_UNIT ( ) );
#23753 = CARTESIAN_POINT ( 'NONE',  ( 11.33041235500449950, -4.942357465271699724, -6.636704692336500067 ) ) ;
#23754 = EDGE_CURVE ( 'NONE', #26667, #63941, #44341, .T. ) ;
#23755 = EDGE_CURVE ( 'NONE', #51860, #7219, #23246, .T. ) ;
#23756 = CARTESIAN_POINT ( 'NONE',  ( 7.583051658771000625, 4.763536573491999881, 5.668879554882000349 ) ) ;
#23757 = VERTEX_POINT ( 'NONE', #27455 ) ;
#23758 = B_SPLINE_CURVE_WITH_KNOTS ( 'NONE', 3,
 ( #33327, #65112, #53943, #16543, #32299, #44170, #11635, #65466, #43817, #17591, #59539, #22475 ),
 .UNSPECIFIED., .F., .F.,
 ( 4, 2, 2, 2, 2, 4 ),
 ( 0.000000000000000000, 0.2499999999999977240, 0.3749999999999977796, 0.4999999999999978906, 0.7499999999999988898, 1.000000000000000000 ),
 .UNSPECIFIED. ) ;
#23759 = DIRECTION ( 'NONE',  ( 1.000000000000000000, -1.234748485291000148E-09, -3.354312113616000052E-09 ) ) ;
#23760 = CARTESIAN_POINT ( 'NONE',  ( 5.500000000000000000, -1.449999999999999956, 0.000000000000000000 ) ) ;
#23761 = CARTESIAN_POINT ( 'NONE',  ( 24.22109243572800352, -3.760953175020000039, 12.77804564811999910 ) ) ;
#23762 = CARTESIAN_POINT ( 'NONE',  ( 17.84610786052055076, 3.139226446220193978, 12.20267444563224579 ) ) ;
#23763 = CARTESIAN_POINT ( 'NONE',  ( 18.23019412026599895, 3.031170125296999807, -11.90979123982999965 ) ) ;
#23764 = CARTESIAN_POINT ( 'NONE',  ( 10.21609109105999913, 5.961715741921000067, 7.319666990313999477 ) ) ;
#23765 = CARTESIAN_POINT ( 'NONE',  ( 11.46550210169813511, -4.058074521742473628, -8.807012707104282967 ) ) ;
#23766 = CARTESIAN_POINT ( 'NONE',  ( 25.29987333571600061, -11.77655473258999841, -4.190794510628000680 ) ) ;
#23767 = ORIENTED_EDGE ( 'NONE', *, *, #42317, .F. ) ;
#23768 = CARTESIAN_POINT ( 'NONE',  ( 12.27745450063685162, -2.164896879444428546, 12.52337953207688237 ) ) ;
#23769 = CARTESIAN_POINT ( 'NONE',  ( 8.895138961223999274, -3.167792625045000143, -8.062381800110799190 ) ) ;
#23770 = CARTESIAN_POINT ( 'NONE',  ( 11.24053267693000002, 2.774035422596999645, 6.782113650547000105 ) ) ;
#23771 = CARTESIAN_POINT ( 'NONE',  ( 8.455992358812000731, -5.100000000000000533, 6.571291218949999902 ) ) ;
#23772 = CIRCLE ( 'NONE', #4788, 0.7499999936418002555 ) ;
#23773 = PRODUCT ( 'O Ring Seal 2', 'O Ring Seal 2', '', ( #41434 ) ) ;
#23774 = CARTESIAN_POINT ( 'NONE',  ( 10.71918447801630059, 5.140463864104999558, -7.474854604063350116 ) ) ;
#23775 = CARTESIAN_POINT ( 'NONE',  ( 12.52850951125299872, 0.5605836838512540110, 12.68334204399184273 ) ) ;
#23776 = CARTESIAN_POINT ( 'NONE',  ( 7.390489158771000433, 2.216873702600000051, 8.370081218683999680 ) ) ;
#23777 = CARTESIAN_POINT ( 'NONE',  ( 9.504903297738000134, 3.934733353759999552, 5.704831249548000471 ) ) ;
#23778 = CARTESIAN_POINT ( 'NONE',  ( 12.36723811880910340, 2.053846804184053632, 12.54438404081591862 ) ) ;
#23779 = ORIENTED_EDGE ( 'NONE', *, *, #40188, .T. ) ;
#23780 = CARTESIAN_POINT ( 'NONE',  ( 9.436104719595000745, 5.619431609641999614, -8.115423117607999615 ) ) ;
#23781 = CARTESIAN_POINT ( 'NONE',  ( 11.10887482311539998, 5.184953745778000389, -7.978749413531599721 ) ) ;
#23782 = CARTESIAN_POINT ( 'NONE',  ( 5.317324867288666823, 1.499999999999999778, 0.2318186422567637683 ) ) ;
#23784 = CARTESIAN_POINT ( 'NONE',  ( 24.83136329184668156, 11.65947310412830618, 3.197453827145718463 ) ) ;
#23783 = CARTESIAN_POINT ( 'NONE',  ( 7.956793146791999227, -4.524489047957000132, 9.047757046927999980 ) ) ;
#23785 = CARTESIAN_POINT ( 'NONE',  ( 10.23597570133300039, -3.263119632394099856, 6.817468224793199916 ) ) ;
#23786 = CARTESIAN_POINT ( 'NONE',  ( 11.76133460557259980, -3.860150918677800025, -8.354833838171700222 ) ) ;
#23787 = ORIENTED_EDGE ( 'NONE', *, *, #25108, .T. ) ;
#23788 =( GEOMETRIC_REPRESENTATION_CONTEXT ( 3 ) GLOBAL_UNCERTAINTY_ASSIGNED_CONTEXT ( ( #33690 ) ) GLOBAL_UNIT_ASSIGNED_CONTEXT ( ( #59323, #53738, #42906 ) ) REPRESENTATION_CONTEXT ( 'NONE', 'WORKASPACE' ) );
#23789 = CARTESIAN_POINT ( 'NONE',  ( 1.877657190359999895, 3.109069236570999539, 1.438230559479999782 ) ) ;
#23790 = CARTESIAN_POINT ( 'NONE',  ( 17.83819980924002024, -0.5572757172051777674, -12.68354006032887327 ) ) ;
#23791 = EDGE_CURVE ( 'NONE', #43345, #52427, #29188, .T. ) ;
#23792 = CARTESIAN_POINT ( 'NONE',  ( 12.09999999999999964, -2.792989229543000107, 7.174999999999999822 ) ) ;
#23793 = CARTESIAN_POINT ( 'NONE',  ( 17.71839800377770047, -3.104623491297848314, 13.52646211264960563 ) ) ;
#23794 = CARTESIAN_POINT ( 'NONE',  ( 24.53003472522999928, -12.09081557276999952, 3.147842171698999714 ) ) ;
#23795 = EDGE_CURVE ( 'NONE', #35633, #36490, #42595, .T. ) ;
#23796 = CARTESIAN_POINT ( 'NONE',  ( 17.63806710036372749, -1.880187906035670764, -13.78549581173514937 ) ) ;
#23797 = DIRECTION ( 'NONE',  ( -0.000000000000000000, -0.000000000000000000, 1.000000000000000000 ) ) ;
#23798 = CARTESIAN_POINT ( 'NONE',  ( 23.60000000000000142, 11.49391741900999975, -4.090215442373000165 ) ) ;
#23799 = CARTESIAN_POINT ( 'NONE',  ( 10.38528584683667866, 4.732620749361601931, 6.833918148925947733 ) ) ;
#23800 = ORIENTED_EDGE ( 'NONE', *, *, #11337, .T. ) ;
#23801 = CARTESIAN_POINT ( 'NONE',  ( 8.727045280411999784, 3.882020551409000042, 5.870058896428999695 ) ) ;
#23802 = B_SPLINE_CURVE_WITH_KNOTS ( 'NONE', 3,
 ( #34401, #29156, #50126, #8504, #29851, #34740, #66881, #60610, #24585, #56402, #7124, #13421, #51159, #40320, #45229, #1887 ),
 .UNSPECIFIED., .F., .F.,
 ( 4, 2, 2, 2, 2, 2, 2, 4 ),
 ( 0.000000000000000000, 0.06250000000000098532, 0.1250000000000019706, 0.2499999999999998890, 0.4999999999999988898, 0.7499999999999977796, 0.8749999999999988898, 1.000000000000000000 ),
 .UNSPECIFIED. ) ;
#23803 = CARTESIAN_POINT ( 'NONE',  ( 10.40685100253999984, -2.832432432432000269, -6.822293592207000934 ) ) ;
#23804 = CARTESIAN_POINT ( 'NONE',  ( 7.432385141095590342, -2.300021307827942341, 7.868234740325537047 ) ) ;
#23805 = CARTESIAN_POINT ( 'NONE',  ( 7.674792391072008613, -2.650477653308784376, 7.499986425013215552 ) ) ;
#23806 = CARTESIAN_POINT ( 'NONE',  ( 0.7943821004246000017, -2.155162080922000012, 2.873869168568000010 ) ) ;
#23807 = VERTEX_POINT ( 'NONE', #28856 ) ;
#23808 = CARTESIAN_POINT ( 'NONE',  ( 1.990556799206333105, 3.500000000000001776, -0.4581489286485044832 ) ) ;
#23809 = CARTESIAN_POINT ( 'NONE',  ( 10.78315545572531065, -5.333388898808085088, -6.342471701929282446 ) ) ;
#23810 = CARTESIAN_POINT ( 'NONE',  ( 9.388624299788999039, 4.079402096444999515, 9.259357173634999327 ) ) ;
#23811 = CARTESIAN_POINT ( 'NONE',  ( 10.64949279009019989, 3.739015461786900030, 6.531063508962500208 ) ) ;
#23812 = CARTESIAN_POINT ( 'NONE',  ( 9.587263606520540549, -3.377808641630456243, 8.716806737538737693 ) ) ;
#23813 = CARTESIAN_POINT ( 'NONE',  ( 10.53870444038000009, -5.103398787993000063, -6.705198626796000205 ) ) ;
#23814 = DIRECTION ( 'NONE',  ( -0.9999999999997783995, -6.656251680840855499E-07, 7.419214651740835408E-10 ) ) ;
#23815 = DIRECTION ( 'NONE',  ( 0.000000000000000000, -1.000000000000000000, 0.000000000000000000 ) ) ;
#23816 = CARTESIAN_POINT ( 'NONE',  ( 12.17997668546738410, -2.480562828864417924, 12.45612489593431249 ) ) ;
#23817 = CARTESIAN_POINT ( 'NONE',  ( 8.314631905207910734, 4.229903678034249381, 9.254809312259414611 ) ) ;
#23818 = ORIENTED_EDGE ( 'NONE', *, *, #6773, .F. ) ;
#23819 = AXIS2_PLACEMENT_3D ( 'NONE', #48806, #1255, #21879 ) ;
#23820 = CARTESIAN_POINT ( 'NONE',  ( 18.27043923978330753, -2.638421884002154716, 13.74915584829237858 ) ) ;
#23821 = CARTESIAN_POINT ( 'NONE',  ( 10.88733729122639993, -5.277570687708000641, -7.466391690027689876 ) ) ;
#23822 = ORIENTED_EDGE ( 'NONE', *, *, #21995, .T. ) ;
#23823 = ORIENTED_EDGE ( 'NONE', *, *, #39063, .T. ) ;
#23824 = CARTESIAN_POINT ( 'NONE',  ( 8.281163468719427101, -9.408291950837330830, 6.292115732828488461 ) ) ;
#23825 = CARTESIAN_POINT ( 'NONE',  ( 9.791846873516664829, 3.000416447002276943, -6.731816600031355513 ) ) ;
#23826 = DIRECTION ( 'NONE',  ( -1.000000000000000000, 0.000000000000000000, 4.629487027166999918E-14 ) ) ;
#23827 = DIRECTION ( 'NONE',  ( 0.000000000000000000, 1.000000000000000000, 0.000000000000000000 ) ) ;
#23828 = CARTESIAN_POINT ( 'NONE',  ( 10.64447074117000014, 5.073827170570999634, -8.340679549192000053 ) ) ;
#23829 = CARTESIAN_POINT ( 'NONE',  ( 7.100000000000000533, 0.000000000000000000, 11.84999999999999964 ) ) ;
#23830 = CARTESIAN_POINT ( 'NONE',  ( 11.09999999999999964, 7.357009467662000368, -6.362164853100000350 ) ) ;
#23832 = EDGE_CURVE ( 'NONE', #21742, #65069, #60305, .T. ) ;
#23831 = B_SPLINE_CURVE_WITH_KNOTS ( 'NONE', 3,
 ( #23615, #44273, #50880, #61369 ),
 .UNSPECIFIED., .F., .F.,
 ( 4, 4 ),
 ( 0.000000000000000000, 0.1253704142480318307 ),
 .UNSPECIFIED. ) ;
#23833 = CARTESIAN_POINT ( 'NONE',  ( 11.82349952450200270, 3.378095173501999948, -11.11014980558000076 ) ) ;
#23834 = DIRECTION ( 'NONE',  ( -1.000000000000000000, 0.000000000000000000, 0.000000000000000000 ) ) ;
#23835 = CARTESIAN_POINT ( 'NONE',  ( 3.999985533191000364, -6.914809019160056625E-16, -2.149963194831858715 ) ) ;
#23836 = ADVANCED_FACE ( 'NONE', ( #17662 ), #39326, .F. ) ;
#23837 = ADVANCED_FACE ( 'NONE', ( #22891 ), #1271, .F. ) ;
#23838 = ORIENTED_EDGE ( 'NONE', *, *, #42713, .F. ) ;
#23839 = AXIS2_PLACEMENT_3D ( 'NONE', #40395, #55799, #34823 ) ;
#23840 = CARTESIAN_POINT ( 'NONE',  ( 10.90000000000000036, -8.091325576830000088, 7.077637346582999811 ) ) ;
#23841 = CARTESIAN_POINT ( 'NONE',  ( 7.900104261408000816, 3.351183067932000270, -6.316134894229000096 ) ) ;
#23842 = AXIS2_PLACEMENT_3D ( 'NONE', #55230, #44753, #49989 ) ;
#23843 = CARTESIAN_POINT ( 'NONE',  ( 11.05626362482999880, 7.348667259608998137, 6.145046404742999790 ) ) ;
#23844 = CARTESIAN_POINT ( 'NONE',  ( 12.80505043854144276, -0.7302158263239078018, 13.98094363220830871 ) ) ;
#23845 = CARTESIAN_POINT ( 'NONE',  ( 12.29504137777687056, 2.138585174375768450, 13.74345269122308721 ) ) ;
#23846 = CARTESIAN_POINT ( 'NONE',  ( 11.03855816545999957, -2.974093234901999949, 8.716125417860000724 ) ) ;
#23847 = ORIENTED_EDGE ( 'NONE', *, *, #10819, .F. ) ;
#23848 = CARTESIAN_POINT ( 'NONE',  ( 12.30788008554897672, 0.3788802689573961824, -12.69239629739823449 ) ) ;
#23849 = CARTESIAN_POINT ( 'NONE',  ( 12.50529577747504639, 0.6653129401483712790, 13.98418548573915743 ) ) ;
#23850 = VERTEX_POINT ( 'NONE', #23585 ) ;
#23851 = PLANE ( 'NONE',  #25353 ) ;
#23852 = CARTESIAN_POINT ( 'NONE',  ( 5.700000000000000178, 13.94845324556000143, 4.312847325879000770 ) ) ;
#23853 = EDGE_CURVE ( 'NONE', #10703, #8532, #16818, .T. ) ;
#23854 = CARTESIAN_POINT ( 'NONE',  ( 24.13646806689900259, -3.227588194705000024, -12.37943302943000035 ) ) ;
#23855 = CARTESIAN_POINT ( 'NONE',  ( 4.260103625319000109, 0.7126091724783999437, -1.465752069756999898 ) ) ;
#23856 = B_SPLINE_CURVE_WITH_KNOTS ( 'NONE', 3,
 ( #63159, #26120, #24747, #4436, #57235, #30680 ),
 .UNSPECIFIED., .F., .F.,
 ( 4, 1, 1, 4 ),
 ( 0.000000000000000000, 0.2305484560606776978, 0.8346924746771972048, 1.000000000000000000 ),
 .UNSPECIFIED. ) ;
#23857 = CARTESIAN_POINT ( 'NONE',  ( 7.474999999999999645, -5.349999999999999645, 7.500000000000000000 ) ) ;
#23858 = CARTESIAN_POINT ( 'NONE',  ( 9.378359312500634815, 5.126777126186428113, 6.752018918873821107 ) ) ;
#23859 = CARTESIAN_POINT ( 'NONE',  ( 0.02212111259145000189, 1.258511261458999941, -3.306246502378999974 ) ) ;
#23860 = CARTESIAN_POINT ( 'NONE',  ( 10.32322128467999889, -4.600000125420001140, -4.621083553505000552 ) ) ;
#23861 = CARTESIAN_POINT ( 'NONE',  ( 8.314979508587148516, 2.649972834346558059, -7.499998738096613771 ) ) ;
#23862 = CARTESIAN_POINT ( 'NONE',  ( 9.793328727373999953, -5.651611919872999934, -7.935921913274999184 ) ) ;
#23863 = CARTESIAN_POINT ( 'NONE',  ( 11.56441235500451015, 3.361299021099800388, -6.914884925939399629 ) ) ;
#23864 = DIRECTION ( 'NONE',  ( 0.7071067811866525998, 0.000000000000000000, -0.7071067811864425456 ) ) ;
#23865 = CARTESIAN_POINT ( 'NONE',  ( 11.06967835872019812, 3.245266201729799960, -7.024326263066900111 ) ) ;
#23866 = CARTESIAN_POINT ( 'NONE',  ( 8.847442991499999465, 3.928121959910110483, -6.360452723514999462 ) ) ;
#23868 = CARTESIAN_POINT ( 'NONE',  ( 10.73288376472999950, -2.790050529699000137, 4.894999077959000466 ) ) ;
#23867 = CARTESIAN_POINT ( 'NONE',  ( 9.266480666858999626, -3.710922827228400056, 6.682599852064000423 ) ) ;
#23869 = CARTESIAN_POINT ( 'NONE',  ( 23.61172379773616115, -13.39866229807703313, 3.948922985516912565 ) ) ;
#23870 = VERTEX_POINT ( 'NONE', #1573 ) ;
#23871 = VECTOR ( 'NONE', #19810, 1000.000000000000000 ) ;
#23872 = CARTESIAN_POINT ( 'NONE',  ( 11.56833327354034857, 3.253412192327699959, 7.988332985010599963 ) ) ;
#23873 = CARTESIAN_POINT ( 'NONE',  ( 9.662553763536999796, -4.094830574823999925, 9.119950378356000087 ) ) ;
#23874 = CARTESIAN_POINT ( 'NONE',  ( 9.629684229509999582, 3.291972602441000095, 8.212418068717900255 ) ) ;
#23875 = DIRECTION ( 'NONE',  ( 1.000000000000000000, 0.000000000000000000, 0.000000000000000000 ) ) ;
#23876 = CARTESIAN_POINT ( 'NONE',  ( 24.35365242081700288, 10.90899669668998584, -3.315896191951999583 ) ) ;
#23877 = ADVANCED_FACE ( 'NONE', ( #44242 ), #55756, .F. ) ;
#23878 = CARTESIAN_POINT ( 'NONE',  ( 11.09999999999999964, 4.000000000000000000, -7.500000000000000000 ) ) ;
#23879 = UNCERTAINTY_MEASURE_WITH_UNIT (LENGTH_MEASURE( 1.000000000000000082E-05 ), #62404, 'distance_accuracy_value', 'NONE');
#23880 = ORIENTED_EDGE ( 'NONE', *, *, #21455, .F. ) ;
#23881 = B_SPLINE_CURVE_WITH_KNOTS ( 'NONE', 3,
 ( #36030, #57014, #46871, #25197 ),
 .UNSPECIFIED., .F., .F.,
 ( 4, 4 ),
 ( 0.000000000000000000, 1.000000000000000000 ),
 .UNSPECIFIED. ) ;
#23882 = VECTOR ( 'NONE', #51313, 1000.000000000000227 ) ;
#23883 = CARTESIAN_POINT ( 'NONE',  ( 9.809950584426999853, -3.546800160410199965, -6.451980747609000311 ) ) ;
#23884 = DIRECTION ( 'NONE',  ( -0.7071067811865952013, 0.7071067811864951702, -8.251256364954943451E-08 ) ) ;
#23885 = CARTESIAN_POINT ( 'NONE',  ( 17.61541550669253198, 1.763241988052385745, -12.47601615708916434 ) ) ;
#23886 = CARTESIAN_POINT ( 'NONE',  ( 11.04677151279999947, -2.764386413791999786, -5.039776830043000366 ) ) ;
#23887 = AXIS2_PLACEMENT_3D ( 'NONE', #12679, #61947, #40285 ) ;
#23888 = CARTESIAN_POINT ( 'NONE',  ( 10.94076550314999885, -5.140765503144999471, -6.571291218949999902 ) ) ;
#23889 = CARTESIAN_POINT ( 'NONE',  ( 10.62903166480609940, 3.135947233695900227, -7.560921321260908989 ) ) ;
#23890 = CARTESIAN_POINT ( 'NONE',  ( 14.46666666157666903, 8.833279249958289725, 7.896561128163720689 ) ) ;
#23891 = CARTESIAN_POINT ( 'NONE',  ( 9.010799540956998754, -4.699533657262000119, -6.366989705700999203 ) ) ;
#23892 = CARTESIAN_POINT ( 'NONE',  ( 25.48370546149499916, 11.09850153045000098, 3.318332408913000187 ) ) ;
#23893 = ORIENTED_EDGE ( 'NONE', *, *, #14023, .T. ) ;
#23894 = CARTESIAN_POINT ( 'NONE',  ( -0.000000000000000000, -2.533832635911827502, -1.460960874862264225 ) ) ;
#23895 = VECTOR ( 'NONE', #62731, 1000.000000000000000 ) ;
#23896 = CARTESIAN_POINT ( 'NONE',  ( 12.27511425286869695, -0.4989076128645703045, -13.99111800451625065 ) ) ;
#23897 = LINE ( 'NONE', #33707, #11979 ) ;
#23898 = CARTESIAN_POINT ( 'NONE',  ( 11.53828694957233481, 4.309606737214646266, -8.735060943529676436 ) ) ;
#23899 = CARTESIAN_POINT ( 'NONE',  ( 3.499999999999999556, -2.703350975099395814, 1.634640570342158705 ) ) ;
#23900 = CARTESIAN_POINT ( 'NONE',  ( 8.126014158770999529, 5.189036231907000030, -8.048606212067999977 ) ) ;
#23901 = DIRECTION ( 'NONE',  ( 0.4384236320213994453, -0.6355252626312994924, 0.6355252626312996034 ) ) ;
#23902 = EDGE_LOOP ( 'NONE', ( #61338, #44865, #51049, #11825 ) ) ;
#23903 = CARTESIAN_POINT ( 'NONE',  ( 4.000000000000000000, 1.719326598156197372, 1.321078631445046669 ) ) ;
#23904 = CARTESIAN_POINT ( 'NONE',  ( 17.83362577474377986, 1.940423258991959443, -13.77633750067930229 ) ) ;
#23905 = ORIENTED_EDGE ( 'NONE', *, *, #27386, .F. ) ;
#23906 = DIRECTION ( 'NONE',  ( -1.000000000000000000, 0.000000000000000000, 0.000000000000000000 ) ) ;
#23907 = CARTESIAN_POINT ( 'NONE',  ( 24.72672956147405898, 3.119036157890411332, 11.78404790340006336 ) ) ;
#23908 = CARTESIAN_POINT ( 'NONE',  ( 8.813304719595000947, 3.880154689736000417, -9.060377011187000562 ) ) ;
#23909 = CARTESIAN_POINT ( 'NONE',  ( 23.91429168771849945, -12.84854223911260185, 3.562185587916466556 ) ) ;
#23910 = CARTESIAN_POINT ( 'NONE',  ( 10.44999293566599974, -3.279967330949900450, -8.383280442119700027 ) ) ;
#23911 = CARTESIAN_POINT ( 'NONE',  ( 17.59542495529381512, 0.6250000000000000000, -12.67928922306854211 ) ) ;
#23912 = CARTESIAN_POINT ( 'NONE',  ( 10.39393020684899938, -5.250000000000000000, 7.500000000000000000 ) ) ;
#23913 = ORIENTED_EDGE ( 'NONE', *, *, #25663, .F. ) ;
#23914 = CARTESIAN_POINT ( 'NONE',  ( 7.639326144738664226, 5.301174781770192190, -7.912266426404620745 ) ) ;
#23915 = ADVANCED_FACE ( 'NONE', ( #54362 ), #67139, .T. ) ;
#23916 = EDGE_CURVE ( 'NONE', #34596, #19886, #50849, .T. ) ;
#23917 = DIRECTION ( 'NONE',  ( 0.000000000000000000, 0.000000000000000000, -1.000000000000000000 ) ) ;
#23918 = CARTESIAN_POINT ( 'NONE',  ( 9.295789158775001226, 5.835196551504000517, -7.008466539623000813 ) ) ;
#23919 = ORIENTED_EDGE ( 'NONE', *, *, #67572, .F. ) ;
#23920 = CONICAL_SURFACE ( 'NONE', #455, 2.049966935984999683, 0.7853819979415218588 ) ;
#23921 = CARTESIAN_POINT ( 'NONE',  ( 10.52662718686000076, 4.933722097448000277, -6.506013113666999637 ) ) ;
#23922 = CARTESIAN_POINT ( 'NONE',  ( 25.49995889272035399, 10.64590475540159886, 3.788442452821807471 ) ) ;
#23923 = VERTEX_POINT ( 'NONE', #41043 ) ;
#23924 = CARTESIAN_POINT ( 'NONE',  ( 9.075405316139999456, 3.757578743663700038, 6.384219384258999597 ) ) ;
#23925 = CARTESIAN_POINT ( 'NONE',  ( 18.14725124545929091, -2.065010783240470271, -12.42963489304855251 ) ) ;
#23926 = DIRECTION ( 'NONE',  ( -1.000000000000000000, 0.000000000000000000, 0.000000000000000000 ) ) ;
#23927 = CARTESIAN_POINT ( 'NONE',  ( -14.79345512259999929, 10.48174933044999868, -5.405686454350000503 ) ) ;
#23928 = CARTESIAN_POINT ( 'NONE',  ( 11.55275411606000269, -11.58372484989999940, -1.667203446842000059 ) ) ;
#23929 = CARTESIAN_POINT ( 'NONE',  ( 9.915292290062998504, 4.749786674456300872, 7.935348007132199122 ) ) ;
#23930 = FACE_OUTER_BOUND ( 'NONE', #3950, .T. ) ;
#23931 = ORIENTED_EDGE ( 'NONE', *, *, #30100, .F. ) ;
#23932 = CARTESIAN_POINT ( 'NONE',  ( 11.41486084871699802, 2.792989229543000107, 7.174999999999999822 ) ) ;
#23933 = B_SPLINE_CURVE_WITH_KNOTS ( 'NONE', 1,
 ( #15632, #31718 ),
 .UNSPECIFIED., .F., .F.,
 ( 2, 2 ),
 ( 0.000000000000000000, 1.000000000000000000 ),
 .UNSPECIFIED. ) ;
#23934 = CARTESIAN_POINT ( 'NONE',  ( 10.94033278040999946, 5.142729166069000435, -6.493505370358000128 ) ) ;
#23935 = EDGE_CURVE ( 'NONE', #67995, #18236, #41842, .T. ) ;
#23936 = AXIS2_PLACEMENT_3D ( 'NONE', #58127, #15816, #63005 ) ;
#23937 = FACE_OUTER_BOUND ( 'NONE', #3789, .T. ) ;
#23938 = CARTESIAN_POINT ( 'NONE',  ( 12.20814394425992866, 2.932476687367332691, -13.68943695263252103 ) ) ;
#23939 = CARTESIAN_POINT ( 'NONE',  ( 11.32309687351640193, -5.217465845835395299, 7.827184855449101697 ) ) ;
#23940 = EDGE_CURVE ( 'NONE', #4878, #69017, #63500, .T. ) ;
#23941 = CARTESIAN_POINT ( 'NONE',  ( 10.22109127278999807, -2.983266195621000261, 8.764707262515999631 ) ) ;
#23942 = CARTESIAN_POINT ( 'NONE',  ( 18.08024975107899124, 0.3389646381316565038, 13.89444110642641661 ) ) ;
#23943 = AXIS2_PLACEMENT_3D ( 'NONE', #36625, #20194, #4105 ) ;
#23944 = CARTESIAN_POINT ( 'NONE',  ( 18.18005043890192596, -2.480435635901940383, 12.45614914577398835 ) ) ;
#23945 = ORIENTED_EDGE ( 'NONE', *, *, #22641, .T. ) ;
#23946 = ORIENTED_EDGE ( 'NONE', *, *, #53954, .F. ) ;
#23947 = CARTESIAN_POINT ( 'NONE',  ( 9.743314158772999889, 5.149303692842000402, -5.987168472229000393 ) ) ;
#23948 = CARTESIAN_POINT ( 'NONE',  ( 6.433333127195900225, 12.43895222601385697, 2.828919834970925251 ) ) ;
#23949 = CARTESIAN_POINT ( 'NONE',  ( 12.18135539520747201, -2.541609601506828131, 13.66455050636339230 ) ) ;
#23950 = CARTESIAN_POINT ( 'NONE',  ( 7.307500000000000107, -0.2999999999999999889, 3.149999999999999911 ) ) ;
#23951 = CARTESIAN_POINT ( 'NONE',  ( 23.61806548148500084, 10.28147268658000080, -9.269149798642001059 ) ) ;
#23952 = CARTESIAN_POINT ( 'NONE',  ( 16.13895793972310599, -3.268072512451278389, -11.38828084065380608 ) ) ;
#23954 = CARTESIAN_POINT ( 'NONE',  ( 23.60000000000000142, -11.85420044612000012, -3.901016762742000488 ) ) ;
#23953 = CARTESIAN_POINT ( 'NONE',  ( 10.66360887879199915, -4.258572737033900601, 8.612148635591999835 ) ) ;
#23955 = CARTESIAN_POINT ( 'NONE',  ( 9.048601287889788125, 4.000000467705929985, -8.698595322193607871 ) ) ;
#23956 = VERTEX_POINT ( 'NONE', #56089 ) ;
#23957 = CARTESIAN_POINT ( 'NONE',  ( 12.35923975622791993, 0.5837697427126086192, 13.98798827748084683 ) ) ;
#23958 = DIRECTION ( 'NONE',  ( 0.000000000000000000, 1.000000000000000000, 0.000000000000000000 ) ) ;
#23959 = CARTESIAN_POINT ( 'NONE',  ( 18.12876220047771270, 0.2481623978058146718, 12.69674179789668678 ) ) ;
#23960 = CARTESIAN_POINT ( 'NONE',  ( 11.59999999999999964, 4.000000000000000000, -7.500000000000000000 ) ) ;
#23961 = CARTESIAN_POINT ( 'NONE',  ( -0.2999999999999999889, 0.000000000000000000, 0.000000000000000000 ) ) ;
#23962 = VERTEX_POINT ( 'NONE', #67595 ) ;
#23964 = CARTESIAN_POINT ( 'NONE',  ( 12.35662541763808697, -3.053258836671836729, -12.22465729756448205 ) ) ;
#23963 = CARTESIAN_POINT ( 'NONE',  ( 10.86324669354999983, -5.065490477172999384, 5.172188879882000379 ) ) ;
#23965 = CARTESIAN_POINT ( 'NONE',  ( 8.754720280412998434, 5.687930027805999877, -7.109876198051000351 ) ) ;
#23966 = CARTESIAN_POINT ( 'NONE',  ( 8.610944094208999644, 5.100000000000000533, -6.571291218949999902 ) ) ;
#23967 = CARTESIAN_POINT ( 'NONE',  ( 10.34580110216399973, 2.909301855364999856, 8.166103548914600552 ) ) ;
#23968 = AXIS2_PLACEMENT_3D ( 'NONE', #47867, #63232, #68826 ) ;
#23969 = DIRECTION ( 'NONE',  ( 1.000000000000000000, 0.000000000000000000, 0.000000000000000000 ) ) ;
#23970 = B_SPLINE_SURFACE_WITH_KNOTS ( 'NONE', 3, 3, ( 
 ( #28435, #45552, #67884, #9495 ),
 ( #2886, #29826, #61964, #56726 ),
 ( #40981, #57057, #3234, #57390 ),
 ( #19661, #24209, #62970, #41327 ) ),
 .UNSPECIFIED., .F., .F., .F.,
 ( 4, 4 ),
 ( 4, 4 ),
 ( 0.7363163806532000422, 1.013499456067999960 ),
 ( -0.0005287450254680999126, 0.02696599629895000266 ),
 .UNSPECIFIED. ) ;
#23971 = DIRECTION ( 'NONE',  ( 0.000000000000000000, 1.000000000000000000, 0.000000000000000000 ) ) ;
#23972 = CARTESIAN_POINT ( 'NONE',  ( 2.738338500705999934, 0.2183327149865000039, 3.585551516645999914 ) ) ;
#23973 = ORIENTED_EDGE ( 'NONE', *, *, #24869, .T. ) ;
#23974 = CARTESIAN_POINT ( 'NONE',  ( 12.31563516348837872, -0.3888461597108449630, -12.69199065798141568 ) ) ;
#23975 = CARTESIAN_POINT ( 'NONE',  ( 24.67921580316900076, -12.29514843751999997, 2.979196179828000002 ) ) ;
#23976 = CARTESIAN_POINT ( 'NONE',  ( 11.02452225494999993, -2.775477745048999800, -6.571291218949999902 ) ) ;
#23977 = CARTESIAN_POINT ( 'NONE',  ( 8.192489158772998437, 2.550241116032999855, 7.666973618349000041 ) ) ;
#23978 = EDGE_LOOP ( 'NONE', ( #24949, #58301, #4706, #54699 ) ) ;
#23979 = CARTESIAN_POINT ( 'NONE',  ( 5.521676530072999967, -0.1057711097905999903, -1.318062398728999884 ) ) ;
#23980 = CARTESIAN_POINT ( 'NONE',  ( 10.93980696525934171, 9.321087494126425455, 6.228652191884624045 ) ) ;
#23982 = CARTESIAN_POINT ( 'NONE',  ( 24.66807826147336513, -8.737531165310779002, 9.168167557060799666 ) ) ;
#23981 = CYLINDRICAL_SURFACE ( 'NONE', #62017, 1.350000000000000089 ) ;
#23983 = CIRCLE ( 'NONE', #12813, 2.000000000000000000 ) ;
#23984 = CARTESIAN_POINT ( 'NONE',  ( 10.14887885159599890, 5.269014563305000287, 7.651388779553199626 ) ) ;
#23985 = CARTESIAN_POINT ( 'NONE',  ( 11.09999999999999964, 3.512324525112999751, -8.971282648301999174 ) ) ;
#23986 = ORIENTED_EDGE ( 'NONE', *, *, #4429, .F. ) ;
#23987 = CARTESIAN_POINT ( 'NONE',  ( 9.959635380193999410, -5.406637819064000539, 7.700301345050000634 ) ) ;
#23988 = ORIENTED_EDGE ( 'NONE', *, *, #27471, .F. ) ;
#23989 = CYLINDRICAL_SURFACE ( 'NONE', #44005, 3.500000000000000000 ) ;
#23990 = CARTESIAN_POINT ( 'NONE',  ( 8.020980646792999380, -3.245532552444000185, 8.949627348471000943 ) ) ;
#23991 = CARTESIAN_POINT ( 'NONE',  ( 17.87656099625190365, 0.6549277419692614011, -13.98467727287827067 ) ) ;
#23992 = VERTEX_POINT ( 'NONE', #45268 ) ;
#23993 = CARTESIAN_POINT ( 'NONE',  ( 10.91202604904536777, 9.732768313057503562, -5.831340146199694985 ) ) ;
#23994 = CARTESIAN_POINT ( 'NONE',  ( 18.30003129334700063, -2.732683817159999862, 11.53064095410000078 ) ) ;
#23995 = CARTESIAN_POINT ( 'NONE',  ( 7.988314158770000617, 4.376386084436000523, -6.154119786874999498 ) ) ;
#23996 = CARTESIAN_POINT ( 'NONE',  ( 10.21612608405689038, 2.826342078250798195, 6.832754235737262150 ) ) ;
#23997 = CARTESIAN_POINT ( 'NONE',  ( 18.16648463839231198, -2.629536980443115013, 12.42046771388698723 ) ) ;
#23998 = VERTEX_POINT ( 'NONE', #67255 ) ;
#23999 = CARTESIAN_POINT ( 'NONE',  ( 12.80505043854146940, -1.798940460745208636, -12.50936912696000469 ) ) ;
#24000 = EDGE_CURVE ( 'NONE', #16502, #12996, #58211, .T. ) ;
#24001 = ADVANCED_FACE ( 'NONE', ( #20061 ), #50503, .T. ) ;
#24002 = CARTESIAN_POINT ( 'NONE',  ( 23.51693423744300304, -13.43920603419999971, -4.372108587443999994 ) ) ;
#24003 = DIRECTION ( 'NONE',  ( -1.000000000000000000, 0.000000000000000000, 0.000000000000000000 ) ) ;
#24005 = CIRCLE ( 'NONE', #63047, 13.27499874714999883 ) ;
#24004 = B_SPLINE_CURVE_WITH_KNOTS ( 'NONE', 3,
 ( #22463, #60232, #1847, #43809 ),
 .UNSPECIFIED., .F., .F.,
 ( 4, 4 ),
 ( 0.000000000000000000, 1.000000000000000000 ),
 .UNSPECIFIED. ) ;
#24006 = DIRECTION ( 'NONE',  ( 0.000000000000000000, -1.000000000000000000, 0.000000000000000000 ) ) ;
#24007 = EDGE_LOOP ( 'NONE', ( #25311, #66312, #13071 ) ) ;
#24008 = DIRECTION ( 'NONE',  ( 0.000000000000000000, -1.000000000000000000, 0.000000000000000000 ) ) ;
#24009 = CARTESIAN_POINT ( 'NONE',  ( 0.04997405931212996200, -2.849971983161023292, -1.472631476147704172E-09 ) ) ;
#24010 = CARTESIAN_POINT ( 'NONE',  ( 3.499999999999999556, 1.045906356845314189, 3.160857899937222992 ) ) ;
#24011 = CARTESIAN_POINT ( 'NONE',  ( 10.44773515094007799, -5.286251723462822127, 7.027580072218823304 ) ) ;
#24012 = CARTESIAN_POINT ( 'NONE',  ( 9.030800552329743880, -2.902287361240535102, 6.174410955705745607 ) ) ;
#24013 = CARTESIAN_POINT ( 'NONE',  ( 12.30917092924264722, 0.3809766167652363644, -13.89298487834588514 ) ) ;
#24014 = CARTESIAN_POINT ( 'NONE',  ( 17.93883077754968625, -2.006280984399066103, 12.55302554764000789 ) ) ;
#24015 = ORIENTED_EDGE ( 'NONE', *, *, #50968, .T. ) ;
#24016 = CARTESIAN_POINT ( 'NONE',  ( 11.48522412107029922, -3.952868550833580130, -6.609122077774299164 ) ) ;
#24017 = ORIENTED_EDGE ( 'NONE', *, *, #46397, .F. ) ;
#24018 = CARTESIAN_POINT ( 'NONE',  ( 5.700000000000000178, -10.75000000000000000, 0.000000000000000000 ) ) ;
#24019 = CARTESIAN_POINT ( 'NONE',  ( 9.038304719595000591, 3.867331042029999999, -9.227339949050001877 ) ) ;
#24020 = CARTESIAN_POINT ( 'NONE',  ( 2.838494431446000110, 3.373532321960999614, -0.1987882563307999950 ) ) ;
#24021 = EDGE_CURVE ( 'NONE', #23213, #14147, #27602, .T. ) ;
#24022 = CARTESIAN_POINT ( 'NONE',  ( 11.17811058788999823, -2.762459764047000110, -6.187206491620000470 ) ) ;
#24023 = LINE ( 'NONE', #45358, #64020 ) ;
#24024 = PRODUCT_DEFINITION_FORMATION_WITH_SPECIFIED_SOURCE ( 'ANY', '', #56164, .NOT_KNOWN. ) ;
#24025 = CARTESIAN_POINT ( 'NONE',  ( 23.68234916609000251, 13.13683194047999869, 3.951035445327000240 ) ) ;
#24026 = ORIENTED_EDGE ( 'NONE', *, *, #23755, .T. ) ;
#24027 = CARTESIAN_POINT ( 'NONE',  ( 10.73103300763300005, -3.307558760216100069, 6.773725604892799623 ) ) ;
#24028 = CARTESIAN_POINT ( 'NONE',  ( 9.261662452849000360, 2.944259351255000379, 6.507396354981000108 ) ) ;
#24029 = CARTESIAN_POINT ( 'NONE',  ( 10.16052890781999984, -2.899999999999999911, -6.152188490330000370 ) ) ;
#24030 = CARTESIAN_POINT ( 'NONE',  ( 18.50003594170800270, -2.686563649653999963, 11.33603604535000109 ) ) ;
#24032 = CARTESIAN_POINT ( 'NONE',  ( 11.06666666666770382, 2.480181672120659986, 7.732127511715679802 ) ) ;
#24031 = CARTESIAN_POINT ( 'NONE',  ( 10.62197831623999988, 5.779783227492000464, 7.256572995198999898 ) ) ;
#24033 = CARTESIAN_POINT ( 'NONE',  ( 10.23103300763299828, 4.692441239783899931, -8.226274395107198600 ) ) ;
#24034 = CARTESIAN_POINT ( 'NONE',  ( 8.610875063856999745, 4.757997781751000410, 5.934102420827000124 ) ) ;
#24035 = AXIS2_PLACEMENT_3D ( 'NONE', #37850, #53242, #64748 ) ;
#24036 = CARTESIAN_POINT ( 'NONE',  ( 10.26291290906799958, 3.364470222553300083, -8.277781595084700683 ) ) ;
#24037 = CARTESIAN_POINT ( 'NONE',  ( 18.05935420056438190, -0.5168989769797245337, 12.58939571008426839 ) ) ;
#24038 = PLANE ( 'NONE',  #48367 ) ;
#24039 = CARTESIAN_POINT ( 'NONE',  ( 10.90000000011000125, 2.899999999889000257, -6.571291220762999430 ) ) ;
#24040 = CARTESIAN_POINT ( 'NONE',  ( 10.37239528041000014, 3.992345698584000235, -5.977238432995000572 ) ) ;
#24041 = EDGE_LOOP ( 'NONE', ( #450, #21402 ) ) ;
#24042 = CARTESIAN_POINT ( 'NONE',  ( 8.400066940379998570, -2.800111029801999774, 9.079936276749000612 ) ) ;
#24043 = CARTESIAN_POINT ( 'NONE',  ( 17.55505043854143565, 1.787797342887043284, 13.88538010501571129 ) ) ;
#24044 = CARTESIAN_POINT ( 'NONE',  ( 23.58926396079670340, 3.186602112811154797, 13.61293272293995571 ) ) ;
#24045 = CARTESIAN_POINT ( 'NONE',  ( 24.30000560748793959, -8.853233204563331071, -8.853233204563331071 ) ) ;
#24046 = VERTEX_POINT ( 'NONE', #40692 ) ;
#24047 = CARTESIAN_POINT ( 'NONE',  ( 7.614801658771000348, 3.326263523254000098, 8.794511546544999447 ) ) ;
#24049 = CARTESIAN_POINT ( 'NONE',  ( 0.7061642493978850244, -1.328001061679412009, 3.278594772182098271 ) ) ;
#24048 = CARTESIAN_POINT ( 'NONE',  ( 8.456370280410999030, 2.836879604150999601, -8.783908972046001296 ) ) ;
#24050 = CARTESIAN_POINT ( 'NONE',  ( 10.68342665876999931, 3.810131921595000026, -5.661115150006999386 ) ) ;
#24051 = EDGE_CURVE ( 'NONE', #3478, #53120, #18693, .T. ) ;
#24052 = ORIENTED_EDGE ( 'NONE', *, *, #43405, .F. ) ;
#24053 = EDGE_CURVE ( 'NONE', #21968, #10113, #40124, .T. ) ;
#24054 = FACE_OUTER_BOUND ( 'NONE', #46281, .T. ) ;
#24055 = CARTESIAN_POINT ( 'NONE',  ( 0.000000000000000000, 0.000000000000000000, 0.000000000000000000 ) ) ;
#24056 = CARTESIAN_POINT ( 'NONE',  ( 10.96533729122639933, 2.859653469230999612, 7.529998433785960010 ) ) ;
#24057 = CARTESIAN_POINT ( 'NONE',  ( 10.89228096335999929, -3.998355205482000851, 9.261304730013998565 ) ) ;
#24058 = CARTESIAN_POINT ( 'NONE',  ( 8.789886373836322875, 4.000007821194417446, -8.439846342473931173 ) ) ;
#24059 = VERTEX_POINT ( 'NONE', #13457 ) ;
#24060 = CARTESIAN_POINT ( 'NONE',  ( 9.050000000000000711, -7.679126935408000065, 5.093340497782000043 ) ) ;
#24061 = CARTESIAN_POINT ( 'NONE',  ( 11.06877944038000017, -5.318813217120000658, -7.168443364726000411 ) ) ;
#24062 = CARTESIAN_POINT ( 'NONE',  ( 7.913001903775949586, -2.440633479413790052, 8.271164008384964461 ) ) ;
#24063 = VECTOR ( 'NONE', #39144, 1000.000000000000114 ) ;
#24064 = CARTESIAN_POINT ( 'NONE',  ( 11.11845396862999991, -5.767021056207999763, 7.178419201465000121 ) ) ;
#24065 = CARTESIAN_POINT ( 'NONE',  ( 11.09590547754519996, -2.684394667508000154, -7.541753805330609239 ) ) ;
#24066 = CARTESIAN_POINT ( 'NONE',  ( 9.501430433047000079, -4.854750075120300323, 8.027488966151301142 ) ) ;
#24067 = ORIENTED_EDGE ( 'NONE', *, *, #1178, .T. ) ;
#24068 = CARTESIAN_POINT ( 'NONE',  ( 10.38718558795000035, -4.935364245016000240, -4.601021236483000543 ) ) ;
#24069 = CARTESIAN_POINT ( 'NONE',  ( 12.12579573085663043, -2.760622544769000264, 7.285547569258399747 ) ) ;
#24070 = ORIENTED_EDGE ( 'NONE', *, *, #44371, .F. ) ;
#24071 = CARTESIAN_POINT ( 'NONE',  ( 9.048601287889788125, 4.000000467705929985, 6.301404677806389465 ) ) ;
#24072 = ORIENTED_EDGE ( 'NONE', *, *, #19486, .F. ) ;
#24073 = CARTESIAN_POINT ( 'NONE',  ( 9.749152735436000583, -5.239375073306999475, -6.095351682555999240 ) ) ;
#24074 = CARTESIAN_POINT ( 'NONE',  ( 9.044210841233001119, 2.773858540272000184, -8.951250717848999727 ) ) ;
#24075 = CYLINDRICAL_SURFACE ( 'NONE', #14744, 11.79499999999999993 ) ;
#24076 = CARTESIAN_POINT ( 'NONE',  ( 8.288053023084509974, 5.073577879423888604, 6.476688461073075054 ) ) ;
#24077 = CARTESIAN_POINT ( 'NONE',  ( 12.34709291757827820, 2.925445075551588836, -12.34221984780394088 ) ) ;
#24078 = CARTESIAN_POINT ( 'NONE',  ( 11.34641504065830020, -3.195537720350400068, 8.099826052678000821 ) ) ;
#24079 = CARTESIAN_POINT ( 'NONE',  ( 11.90211496860029960, -3.206052520092899982, 7.906860999147899527 ) ) ;
#24080 = EDGE_CURVE ( 'NONE', #64075, #49128, #30326, .T. ) ;
#24081 = ORIENTED_EDGE ( 'NONE', *, *, #67374, .F. ) ;
#24082 = CARTESIAN_POINT ( 'NONE',  ( 9.666846873516668381, 4.768183399968648040, 8.499583552997725278 ) ) ;
#24083 = VECTOR ( 'NONE', #16123, 1000.000000000000000 ) ;
#24084 = EDGE_CURVE ( 'NONE', #68576, #68176, #39374, .T. ) ;
#24085 = ORIENTED_EDGE ( 'NONE', *, *, #32740, .F. ) ;
#24086 = CARTESIAN_POINT ( 'NONE',  ( 8.315519353208999931, -5.485781663882000281, 8.532068390166999805 ) ) ;
#24087 = CARTESIAN_POINT ( 'NONE',  ( 24.13227430146345043, 9.165337429710305628, 9.136502937412682712 ) ) ;
#24088 = ORIENTED_EDGE ( 'NONE', *, *, #38342, .T. ) ;
#24089 = CARTESIAN_POINT ( 'NONE',  ( 12.08628615590300015, -2.575951425301590714, -12.33388065128748146 ) ) ;
#24091 = CARTESIAN_POINT ( 'NONE',  ( 11.55610404293055993, 3.497163090439000310, 6.476063885290000322 ) ) ;
#24090 = AXIS2_PLACEMENT_3D ( 'NONE', #38145, #21720, #54584 ) ;
#24092 = CARTESIAN_POINT ( 'NONE',  ( 11.07691935321000010, -3.101896674955000321, -8.926549689995999515 ) ) ;
#24093 = CARTESIAN_POINT ( 'NONE',  ( 10.70851354018270030, 4.163624617374472869, 8.749999999999996447 ) ) ;
#24094 = CARTESIAN_POINT ( 'NONE',  ( 2.500973465876000112, 3.500000000000000000, 0.000000000000000000 ) ) ;
#24095 = CARTESIAN_POINT ( 'NONE',  ( 24.46275371595800152, -8.882876216795999369, 9.187943390076000583 ) ) ;
#24096 = CARTESIAN_POINT ( 'NONE',  ( 7.399999923048000028, 0.000000000000000000, 0.000000000000000000 ) ) ;
#24097 = CARTESIAN_POINT ( 'NONE',  ( 17.71747088695469330, -0.6038699852804519930, -12.68066884516331783 ) ) ;
#24098 = B_SPLINE_CURVE_WITH_KNOTS ( 'NONE', 3,
 ( #33997, #34348, #29107, #50413, #44836, #60560, #29456, #61251, #40608, #29801 ),
 .UNSPECIFIED., .F., .F.,
 ( 4, 2, 2, 2, 4 ),
 ( 0.5000000000000005551, 0.6250000000000004441, 0.7500000000000002220, 0.8750000000000001110, 1.000000000000000000 ),
 .UNSPECIFIED. ) ;
#24099 = CARTESIAN_POINT ( 'NONE',  ( 11.34287482311539996, -3.196874704906699893, -7.824481664695199790 ) ) ;
#24100 = FACE_OUTER_BOUND ( 'NONE', #11457, .T. ) ;
#24101 = DIRECTION ( 'NONE',  ( -1.000000000000000000, 0.000000000000000000, 0.000000000000000000 ) ) ;
#24102 = ORIENTED_EDGE ( 'NONE', *, *, #19396, .F. ) ;
#24103 = CARTESIAN_POINT ( 'NONE',  ( 12.22252627658614976, -11.15475449693722076, 3.361665977429223684 ) ) ;
#24104 = CARTESIAN_POINT ( 'NONE',  ( 17.63827777591714252, 3.120766739620285612, 13.52195882727199994 ) ) ;
#24105 = CARTESIAN_POINT ( 'NONE',  ( 23.68333487548100180, -3.148023544630999648, 13.34998892770999923 ) ) ;
#24106 = EDGE_CURVE ( 'NONE', #24944, #68576, #7680, .T. ) ;
#24107 = CARTESIAN_POINT ( 'NONE',  ( 18.04714676118036110, 2.114551447792224703, 12.53305202231724635 ) ) ;
#24108 = CARTESIAN_POINT ( 'NONE',  ( 18.17677363193000062, 3.419785592864999835, -11.99291007725999947 ) ) ;
#24109 = FACE_OUTER_BOUND ( 'NONE', #56796, .T. ) ;
#24110 = CARTESIAN_POINT ( 'NONE',  ( 9.422950365671626471, -3.319061674888539315, 8.049413566043876145 ) ) ;
#24111 = ORIENTED_EDGE ( 'NONE', *, *, #34269, .T. ) ;
#24112 = CARTESIAN_POINT ( 'NONE',  ( 12.55399154093078806, -1.927548249315101492, 12.56670145065455024 ) ) ;
#24113 = CARTESIAN_POINT ( 'NONE',  ( 8.819151519676999840, -3.978278301382419890, -8.504175633905001419 ) ) ;
#24114 = CARTESIAN_POINT ( 'NONE',  ( 9.500006116823001889, 2.279680316922000127, 7.877692351087999256 ) ) ;
#24115 = CARTESIAN_POINT ( 'NONE',  ( 12.13611496860034933, -2.828587461987000395, 8.100294210499798808 ) ) ;
#24116 = B_SPLINE_CURVE_WITH_KNOTS ( 'NONE', 3,
 ( #23886, #7115, #59906, #6413 ),
 .UNSPECIFIED., .F., .F.,
 ( 4, 4 ),
 ( 0.000000000000000000, 1.000000000000000000 ),
 .UNSPECIFIED. ) ;
#24117 = CARTESIAN_POINT ( 'NONE',  ( 10.74379975933729980, 5.078682052940000524, -7.128873141726999485 ) ) ;
#24118 = CARTESIAN_POINT ( 'NONE',  ( 12.18006454708593544, 0.02081145935391313928, 12.69999906470293283 ) ) ;
#24119 = VECTOR ( 'NONE', #31194, 1000.000000000000000 ) ;
#24120 = CARTESIAN_POINT ( 'NONE',  ( 7.374100552923999352, 4.389299166881000858, 9.135259451319999613 ) ) ;
#24121 = CARTESIAN_POINT ( 'NONE',  ( 10.31167969999000000, 2.874476822401000220, 8.900029516786000627 ) ) ;
#24122 = CARTESIAN_POINT ( 'NONE',  ( 12.46308409927488903, 1.976751580904479555, 12.55819113744975191 ) ) ;
#24123 = VERTEX_POINT ( 'NONE', #48006 ) ;
#24124 = CARTESIAN_POINT ( 'NONE',  ( 8.599639158772999892, 2.261390688294000029, -6.733978371730000134 ) ) ;
#24125 = CARTESIAN_POINT ( 'NONE',  ( 10.86272200990529946, 2.793294545435000220, -7.079074440652799893 ) ) ;
#24126 = CARTESIAN_POINT ( 'NONE',  ( 10.82056172568756303, -4.095931573296573980, 9.237050133684192588 ) ) ;
#24128 = CARTESIAN_POINT ( 'NONE',  ( 10.09393020684899867, 5.250000000000000000, 7.500000000000000000 ) ) ;
#24127 = DIRECTION ( 'NONE',  ( -1.000000000000000000, 0.000000000000000000, 0.000000000000000000 ) ) ;
#24129 = CARTESIAN_POINT ( 'NONE',  ( 9.731405316140000039, -4.184077495686000958, 6.652755395362000002 ) ) ;
#24130 = CARTESIAN_POINT ( 'NONE',  ( 11.09256785386839894, -4.832509746210599921, -8.060248494254899754 ) ) ;
#24131 = ORIENTED_EDGE ( 'NONE', *, *, #53705, .F. ) ;
#24132 = AXIS2_PLACEMENT_3D ( 'NONE', #54936, #33963, #55285 ) ;
#24133 = CARTESIAN_POINT ( 'NONE',  ( 1.825201902854999947, 0.7365451747729999665, -3.515871166463000019 ) ) ;
#24134 = CARTESIAN_POINT ( 'NONE',  ( 18.15698397287705035, -0.1703900907606387127, -12.69849596185835239 ) ) ;
#24135 = VECTOR ( 'NONE', #52294, 1000.000000000000000 ) ;
#24136 = CARTESIAN_POINT ( 'NONE',  ( 9.363694533038728451, -3.488685518255361551, 8.385421723231827329 ) ) ;
#24137 = CARTESIAN_POINT ( 'NONE',  ( 18.12893921138742570, -2.747599606323546606, 13.61782120253034023 ) ) ;
#24138 = EDGE_CURVE ( 'NONE', #12771, #25486, #30900, .T. ) ;
#24139 = ADVANCED_FACE ( 'NONE', ( #26691 ), #67525, .F. ) ;
#24140 = DIRECTION ( 'NONE',  ( -1.000000000000000000, 0.000000000000000000, 0.000000000000000000 ) ) ;
#24141 = CARTESIAN_POINT ( 'NONE',  ( 5.499999999523999428, -0.5000000004757000349, 9.662944681389999957 ) ) ;
#24142 = LINE ( 'NONE', #50371, #25277 ) ;
#24143 = CARTESIAN_POINT ( 'NONE',  ( 9.584226531641581559, 2.899999999999999911, 6.304440313841761068 ) ) ;
#24144 = CARTESIAN_POINT ( 'NONE',  ( 7.629816940376999312, -4.763531818439999732, 5.668890958491999754 ) ) ;
#24145 = ORIENTED_EDGE ( 'NONE', *, *, #64064, .T. ) ;
#24146 = ADVANCED_FACE ( 'NONE', ( #22807 ), #34007, .T. ) ;
#24147 = CARTESIAN_POINT ( 'NONE',  ( 9.010198341230998054, 5.040787533781999841, 8.522957620707000359 ) ) ;
#24148 = LINE ( 'NONE', #45135, #57441 ) ;
#24149 = LINE ( 'NONE', #18218, #53081 ) ;
#24150 = CARTESIAN_POINT ( 'NONE',  ( 10.72510394928771227, -2.650147065043205519, 7.500007457243348163 ) ) ;
#24151 = CARTESIAN_POINT ( 'NONE',  ( 1.652657190360000028, 3.260257002997999809, 1.508168810892000167 ) ) ;
#24152 = ORIENTED_EDGE ( 'NONE', *, *, #24998, .F. ) ;
#24153 = CARTESIAN_POINT ( 'NONE',  ( 1.865556799206333549, -0.4581489286485082579, -3.500000000000000888 ) ) ;
#24154 = CARTESIAN_POINT ( 'NONE',  ( 24.30000000000000071, 10.83443035398000021, 3.855530949778000149 ) ) ;
#24155 = CARTESIAN_POINT ( 'NONE',  ( 10.05691520198999989, 2.453477278391000382, 6.657104391228999773 ) ) ;
#24156 = CARTESIAN_POINT ( 'NONE',  ( 10.45257053952200010, 3.605640676136899980, 8.422730500489899796 ) ) ;
#24157 = CARTESIAN_POINT ( 'NONE',  ( 11.01811411617009817, -5.026960591456000493, -7.825000000000000178 ) ) ;
#24158 = CARTESIAN_POINT ( 'NONE',  ( 10.91732944037999964, -3.256268970540999952, -6.361552695759000287 ) ) ;
#24159 = CARTESIAN_POINT ( 'NONE',  ( 17.92010247872368822, -0.6380582629978912568, -13.98550026811524738 ) ) ;
#24160 = CARTESIAN_POINT ( 'NONE',  ( 16.03331929146652257, -3.865558715575581505, -11.84348844988198834 ) ) ;
#24161 = CARTESIAN_POINT ( 'NONE',  ( 12.20163823188996055, -2.663908709744649883, 12.41191052568941267 ) ) ;
#24162 = CARTESIAN_POINT ( 'NONE',  ( 7.682133832350131364, 5.705319479758692580, 7.108996016928172956 ) ) ;
#24163 = ORIENTED_EDGE ( 'NONE', *, *, #8215, .F. ) ;
#24164 = AXIS2_PLACEMENT_3D ( 'NONE', #10657, #9621, #21490 ) ;
#24165 = CARTESIAN_POINT ( 'NONE',  ( 18.07784313215200456, -3.023931901684169699, 13.66952493495815624 ) ) ;
#24166 = CARTESIAN_POINT ( 'NONE',  ( 25.29996559941400136, -2.596925179230000325, -11.35302181744000016 ) ) ;
#24167 = ORIENTED_EDGE ( 'NONE', *, *, #36236, .F. ) ;
#24168 = CARTESIAN_POINT ( 'NONE',  ( 17.55505043854144276, -0.7192913403693006469, 12.57945229203838444 ) ) ;
#24169 = CARTESIAN_POINT ( 'NONE',  ( 18.49996808500599954, 1.807259461993230287, 11.54438823538759351 ) ) ;
#24170 = CARTESIAN_POINT ( 'NONE',  ( 4.149992563291999836, 4.286198015044692593E-16, -1.999973142472143861 ) ) ;
#24171 = CARTESIAN_POINT ( 'NONE',  ( 8.710288521113000115, -4.352953559891299840, -8.284550957747498501 ) ) ;
#24172 = CARTESIAN_POINT ( 'NONE',  ( 10.40227026081000083, 2.765684886876999649, 9.035354958280999327 ) ) ;
#24173 = B_SPLINE_CURVE_WITH_KNOTS ( 'NONE', 3,
 ( #45652, #40392, #1967, #23290, #44631, #7544, #2307, #47018, #41084, #51907, #24661, #52948, #67636, #3661, #25686, #20100, #26035, #30260, #41426, #19759, #62735, #9599, #40736, #46679, #36522, #31628, #35837, #46334, #52597, #14520, #45983, #62061, #57155, #62401, #41768, #63071, #67295, #30941, #57845, #9251, #30593, #14857, #19412, #14175, #67983, #36179, #52257, #20786, #42117, #4353, #35502, #56823, #68320, #63423, #20441, #9952, #15197, #8923, #31289, #51565, #25001, #4692, #4004, #25341, #47364, #57491, #68669 ),
 .UNSPECIFIED., .F., .F.,
 ( 4, 2, 2, 2, 2, 2, 2, 2, 2, 2, 2, 2, 2, 2, 1, 1, 1, 2, 2, 2, 2, 2, 2, 2, 2, 2, 2, 2, 2, 2, 2, 2, 2, 2, 4 ),
 ( 0.000000000000000000, 0.1250000000000327793, 0.2500000000000655587, 0.3125000000000821010, 0.3437500000000908718, 0.3750000000000996425, 0.4062500000001083578, 0.4218750000001123546, 0.4375000000001163514, 0.4687500000001243450, 0.4843750000001280642, 0.5000000000001317835, 0.5156250000001355582, 0.5312500000001393330, 0.5468750000001431077, 0.5546875000001444400, 0.5585937500001448841, 0.5605468750001451061, 0.5625000000001453282, 0.5781250000001366685, 0.5859375000001322276, 0.5898437500001300071, 0.5937500000001277867, 0.6093750000001217915, 0.6171875000001194600, 0.6250000000001170175, 0.6406250000001136868, 0.6562500000001103562, 0.6718750000001070255, 0.6875000000001036948, 0.7187500000000964784, 0.7343750000000918154, 0.7500000000000870415, 0.8750000000000436318, 1.000000000000000000 ),
 .UNSPECIFIED. ) ;
#24174 = CARTESIAN_POINT ( 'NONE',  ( 9.780284676292000157, 3.021596928575999819, -8.450035627617001666 ) ) ;
#24175 = CARTESIAN_POINT ( 'NONE',  ( 8.784042939651088844, 2.728506136107232471, -8.022165079612438632 ) ) ;
#24176 = CARTESIAN_POINT ( 'NONE',  ( 10.81579453138999902, -5.374572909254000663, 6.698726302909000729 ) ) ;
#24177 = CARTESIAN_POINT ( 'NONE',  ( 9.099999999999999645, 11.84999999999999964, 0.000000000000000000 ) ) ;
#24178 = DIRECTION ( 'NONE',  ( -0.7071067811865474617, 0.7071067811865474617, -3.640778010129241947E-09 ) ) ;
#24179 = CARTESIAN_POINT ( 'NONE',  ( 11.48641235500450009, -4.739919807690899489, -6.822158181405299615 ) ) ;
#24180 = CARTESIAN_POINT ( 'NONE',  ( 5.469676782403334769, -0.7288346947182943181, 1.349937054441817219 ) ) ;
#24181 = ORIENTED_EDGE ( 'NONE', *, *, #68504, .F. ) ;
#24182 = VECTOR ( 'NONE', #22586, 1000.000000000000000 ) ;
#24183 = CARTESIAN_POINT ( 'NONE',  ( 10.02145237372899800, 4.043732047787757189, 6.225919055146348136 ) ) ;
#24184 = CARTESIAN_POINT ( 'NONE',  ( 10.60679199295805475, 3.308080241071473360, -4.759410728272197133 ) ) ;
#24185 = ADVANCED_FACE ( 'NONE', ( #49730 ), #2763, .T. ) ;
#24186 = CARTESIAN_POINT ( 'NONE',  ( 9.991825906548994496, 7.624304478282991404, 5.686370327077997722 ) ) ;
#24187 = CARTESIAN_POINT ( 'NONE',  ( 9.760355082327999199, 3.427502311996299955, -6.356045986629998978 ) ) ;
#24188 = CARTESIAN_POINT ( 'NONE',  ( 12.47274432058961047, 1.970265487500628465, 13.77159998682696340 ) ) ;
#24189 = CARTESIAN_POINT ( 'NONE',  ( 9.442085454646999665, -4.742494605615999781, 8.809986937145000141 ) ) ;
#24190 = ORIENTED_EDGE ( 'NONE', *, *, #63956, .T. ) ;
#24191 = EDGE_CURVE ( 'NONE', #36211, #53667, #45206, .T. ) ;
#24192 = CARTESIAN_POINT ( 'NONE',  ( 12.72336162088762457, 0.6199801057749227962, -12.67962184309742923 ) ) ;
#24193 = CARTESIAN_POINT ( 'NONE',  ( 12.33502240264713379, -0.4124479947379854905, 13.89177559470776302 ) ) ;
#24194 = ORIENTED_EDGE ( 'NONE', *, *, #1974, .T. ) ;
#24195 = DIRECTION ( 'NONE',  ( 0.000000000000000000, 0.000000000000000000, 1.000000000000000000 ) ) ;
#24196 = CARTESIAN_POINT ( 'NONE',  ( 6.899999691988000450, 12.43893545635000031, 2.828937028792000152 ) ) ;
#24197 = CARTESIAN_POINT ( 'NONE',  ( 23.81893538673600119, -3.247264533092999894, -13.04177392601999941 ) ) ;
#24198 = LINE ( 'NONE', #23506, #19348 ) ;
#24199 = CARTESIAN_POINT ( 'NONE',  ( 15.96663488596630742, -8.445622082970141165, -8.216900471613381995 ) ) ;
#24200 = FACE_OUTER_BOUND ( 'NONE', #39963, .T. ) ;
#24201 = CARTESIAN_POINT ( 'NONE',  ( 11.30565467195989093, 2.863826994586553099, 8.088082908809447247 ) ) ;
#24202 = CARTESIAN_POINT ( 'NONE',  ( 12.32444827497856110, 3.019497106116454610, 12.23286052727262607 ) ) ;
#24203 = CARTESIAN_POINT ( 'NONE',  ( 8.996132306828998892, -4.474581801608000120, -6.279517683005999551 ) ) ;
#24204 = CARTESIAN_POINT ( 'NONE',  ( 11.71210404293059959, 3.618181340822599790, -8.277504409418298792 ) ) ;
#24205 = FACE_OUTER_BOUND ( 'NONE', #12567, .T. ) ;
#24206 = CARTESIAN_POINT ( 'NONE',  ( 10.98656920625009903, 4.032067152264009913, -6.608450613814399688 ) ) ;
#24207 = CARTESIAN_POINT ( 'NONE',  ( 9.252709346416999381, 5.031430618794000331, -7.010219103474399915 ) ) ;
#24209 = CARTESIAN_POINT ( 'NONE',  ( 9.234997988989999129, -4.062652182992059657, 6.633566614602599998 ) ) ;
#24208 = FACE_OUTER_BOUND ( 'NONE', #49471, .T. ) ;
#24210 = CARTESIAN_POINT ( 'NONE',  ( 10.98768472567999943, 6.720753181080999283, 5.471698459870999898 ) ) ;
#24211 = ORIENTED_EDGE ( 'NONE', *, *, #38767, .T. ) ;
#24212 = AXIS2_PLACEMENT_3D ( 'NONE', #41289, #46192, #29791 ) ;
#24213 = DIRECTION ( 'NONE',  ( 1.000000000000000000, 0.000000000000000000, 0.000000000000000000 ) ) ;
#24214 = CARTESIAN_POINT ( 'NONE',  ( 9.910792656537999790, -3.869344906782000049, 5.882544796414999944 ) ) ;
#24215 = CARTESIAN_POINT ( 'NONE',  ( 8.897151519676997466, 4.024693162376980382, 6.358456126310000123 ) ) ;
#24216 = CARTESIAN_POINT ( 'NONE',  ( 10.66476354018302608, -2.782534154164604256, -7.172815144550905408 ) ) ;
#24217 = EDGE_CURVE ( 'NONE', #54214, #62492, #45532, .T. ) ;
#24218 = CARTESIAN_POINT ( 'NONE',  ( 9.110944094209999733, 5.100000000000000533, -6.571291218949999902 ) ) ;
#24219 = AXIS2_PLACEMENT_3D ( 'NONE', #30942, #62062, #15198 ) ;
#24220 = DIRECTION ( 'NONE',  ( 0.000000000000000000, 0.000000000000000000, 1.000000000000000000 ) ) ;
#24221 = CARTESIAN_POINT ( 'NONE',  ( 10.22452454188782767, -3.422561976923117477, -8.739574331469325941 ) ) ;
#24222 = B_SPLINE_CURVE_WITH_KNOTS ( 'NONE', 3,
 ( #5080, #47744, #69059, #28451 ),
 .UNSPECIFIED., .F., .F.,
 ( 4, 4 ),
 ( 0.8745842163858279505, 1.000000000000000000 ),
 .UNSPECIFIED. ) ;
#24223 = ORIENTED_EDGE ( 'NONE', *, *, #19173, .F. ) ;
#24224 = EDGE_CURVE ( 'NONE', #47324, #27393, #31821, .T. ) ;
#24225 = ADVANCED_FACE ( 'NONE', ( #8120, #7774 ), #18269, .T. ) ;
#24226 = CARTESIAN_POINT ( 'NONE',  ( 10.06324205624999912, -4.409476560233800413, -8.565862728991998409 ) ) ;
#24227 = CONICAL_SURFACE ( 'NONE', #42098, 0.9999998338055000602, 0.7853981908209605178 ) ;
#24228 = DIRECTION ( 'NONE',  ( 0.000000000000000000, 0.000000000000000000, -1.000000000000000000 ) ) ;
#24229 = CARTESIAN_POINT ( 'NONE',  ( 18.24341944916325886, 2.253723043306036455, -12.39680838072757751 ) ) ;
#24230 = CARTESIAN_POINT ( 'NONE',  ( 10.88079290149999956, -2.937478892754000093, 5.081605332078000359 ) ) ;
#24231 = CARTESIAN_POINT ( 'NONE',  ( 10.97843137008999825, 5.235400103863000254, 6.782920672145000829 ) ) ;
#24233 = VECTOR ( 'NONE', #61063, 999.9999999999998863 ) ;
#24232 = CARTESIAN_POINT ( 'NONE',  ( 12.80505043854143388, 3.124999999999999556, -13.52084414783465505 ) ) ;
#24234 = CARTESIAN_POINT ( 'NONE',  ( 9.839913318575998602, -5.792391408692000532, -6.955579396894000510 ) ) ;
#24235 = DIRECTION ( 'NONE',  ( 0.000000000000000000, -1.000000000000000000, 0.000000000000000000 ) ) ;
#24236 = ORIENTED_EDGE ( 'NONE', *, *, #29547, .T. ) ;
#24237 = DIRECTION ( 'NONE',  ( -0.5298945030328949812, -4.148149686514954961E-09, 0.8480635681689911998 ) ) ;
#24238 = CARTESIAN_POINT ( 'NONE',  ( 12.21516724099298834, -0.4251989115648944773, -13.99355557726514476 ) ) ;
#24239 = FACE_OUTER_BOUND ( 'NONE', #63273, .T. ) ;
#24240 = CARTESIAN_POINT ( 'NONE',  ( 18.17227403027940724, -2.399493853283785949, -13.69423063306952670 ) ) ;
#24241 = CARTESIAN_POINT ( 'NONE',  ( 2.358466522725250147, -0.7663246491380458769, -3.431732421873642469 ) ) ;
#24242 = EDGE_CURVE ( 'NONE', #15717, #3814, #1911, .T. ) ;
#24243 = CARTESIAN_POINT ( 'NONE',  ( 9.459729719592999686, 2.527713920559999661, -6.969421869128999525 ) ) ;
#24244 = CYLINDRICAL_SURFACE ( 'NONE', #58567, 1.999999999999999556 ) ;
#24245 = ORIENTED_EDGE ( 'NONE', *, *, #38112, .T. ) ;
#24246 = CARTESIAN_POINT ( 'NONE',  ( 4.000000000000000000, -0.2816038378556620092, 2.150035234257813954 ) ) ;
#24247 = CARTESIAN_POINT ( 'NONE',  ( 17.55505043854143565, 3.248109929747637015, -13.61799478206225444 ) ) ;
#24248 = VERTEX_POINT ( 'NONE', #24543 ) ;
#24249 = CARTESIAN_POINT ( 'NONE',  ( 10.21265911260399939, -4.376739491155700712, 6.719118894894999805 ) ) ;
#24250 = DIRECTION ( 'NONE',  ( 0.7071090068939822615, 0.000000000000000000, -0.7071045554721071547 ) ) ;
#24251 = CARTESIAN_POINT ( 'NONE',  ( 8.804445280412998898, 5.597201461420000967, -8.171008079894999554 ) ) ;
#24252 = CARTESIAN_POINT ( 'NONE',  ( 11.09999999999999964, -2.409623100499390436, -8.041736326814033831 ) ) ;
#24253 = CARTESIAN_POINT ( 'NONE',  ( 11.67403632436368888, -4.976178716761900489, -7.272033745815799755 ) ) ;
#24254 = CARTESIAN_POINT ( 'NONE',  ( 17.75497146383150948, 0.5922552425849882951, -12.68140545289945642 ) ) ;
#24255 = CARTESIAN_POINT ( 'NONE',  ( 4.971693173016667799, -0.7554284705563540925, 1.310679582531384391 ) ) ;
#24256 = VERTEX_POINT ( 'NONE', #56707 ) ;
#24257 = CARTESIAN_POINT ( 'NONE',  ( 7.846076405120456343, 2.673882995022637932, -7.823504703768565882 ) ) ;
#24258 = CARTESIAN_POINT ( 'NONE',  ( 10.76059687351566652, -4.629523725463621453, 8.592232985442825210 ) ) ;
#24259 = CARTESIAN_POINT ( 'NONE',  ( 18.11654246900412701, -2.224740281559051791, 13.72801203774633549 ) ) ;
#24260 = ORIENTED_EDGE ( 'NONE', *, *, #46002, .F. ) ;
#24261 = B_SPLINE_CURVE_WITH_KNOTS ( 'NONE', 3,
 ( #40569, #51406, #61216, #34306, #39545, #66798, #8418, #35340, #29761, #67131, #45138, #24150 ),
 .UNSPECIFIED., .F., .F.,
 ( 4, 2, 2, 2, 2, 4 ),
 ( 0.1254754252289749794, 0.3127772825098947829, 0.5000791397908146418, 0.6873809970717346118, 0.7810319257121947079, 0.8746828543526545818 ),
 .UNSPECIFIED. ) ;
#24262 = AXIS2_PLACEMENT_3D ( 'NONE', #57299, #42606, #58334 ) ;
#24263 = CARTESIAN_POINT ( 'NONE',  ( 10.77434248675000106, 4.612886656332999991, -8.898793847069001117 ) ) ;
#24264 =( NAMED_UNIT ( * ) SI_UNIT ( $, .STERADIAN. ) SOLID_ANGLE_UNIT ( ) );
#24265 = ORIENTED_EDGE ( 'NONE', *, *, #11042, .T. ) ;
#24266 = CARTESIAN_POINT ( 'NONE',  ( 8.746126402770999064, 5.068373778467000434, 7.902879529556599891 ) ) ;
#24267 = CARTESIAN_POINT ( 'NONE',  ( 18.20050923854816816, -2.808308534135717682, -12.28305809155435746 ) ) ;
#24268 = ADVANCED_FACE ( 'NONE', ( #34702 ), #61096, .T. ) ;
#24269 = MECHANICAL_DESIGN_GEOMETRIC_PRESENTATION_REPRESENTATION (  '', ( #35457 ), #33206 ) ;
#24270 = CARTESIAN_POINT ( 'NONE',  ( 7.100000000000000533, 0.000000000000000000, 0.000000000000000000 ) ) ;
#24271 = CARTESIAN_POINT ( 'NONE',  ( 17.55505043854144276, 0.6250000000000001110, -25.00000000000000000 ) ) ;
#24272 = EDGE_CURVE ( 'NONE', #8437, #30840, #56833, .T. ) ;
#24273 = AXIS2_PLACEMENT_3D ( 'NONE', #23078, #44426, #2447 ) ;
#24274 = CARTESIAN_POINT ( 'NONE',  ( 4.400048358572151486, 0.2121380062687552304, 1.494606510256098364 ) ) ;
#24275 = CARTESIAN_POINT ( 'NONE',  ( 9.408510579921751216, -2.486340047029418798, 8.356969995776358573 ) ) ;
#24276 = VERTEX_POINT ( 'NONE', #29810 ) ;
#24277 = CARTESIAN_POINT ( 'NONE',  ( 8.061933748689000367, 4.603465626214999773, -6.221450782568999749 ) ) ;
#24278 = CARTESIAN_POINT ( 'NONE',  ( 8.732935610179060504, 4.384544241869580361, -5.799574763991691917 ) ) ;
#24279 = CARTESIAN_POINT ( 'NONE',  ( 11.04391448624000027, -5.244599162544999693, -5.180563645961999697 ) ) ;
#24280 = AXIS2_PLACEMENT_3D ( 'NONE', #58199, #10301, #502 ) ;
#24281 = CARTESIAN_POINT ( 'NONE',  ( 12.08020514495812847, 2.544320517268823245, -13.76688091865072749 ) ) ;
#24282 = CARTESIAN_POINT ( 'NONE',  ( 10.39157120343299923, -4.055348968344419269, -8.640469672413999547 ) ) ;
#24283 = CARTESIAN_POINT ( 'NONE',  ( 9.290195424034999760, -2.377814350880000038, 7.540992175424999999 ) ) ;
#24284 = CARTESIAN_POINT ( 'NONE',  ( 18.25531185377811383, 0.1895042076700463041, 13.99872220539657164 ) ) ;
#24285 = CARTESIAN_POINT ( 'NONE',  ( 25.29995737991200144, -8.533537546129998930, 7.925519566782000425 ) ) ;
#24286 = ORIENTED_EDGE ( 'NONE', *, *, #68270, .T. ) ;
#24287 = VERTEX_POINT ( 'NONE', #61944 ) ;
#24288 = CARTESIAN_POINT ( 'NONE',  ( 8.400739158770999637, 4.933589693325000525, -9.154576215408999573 ) ) ;
#24289 = CARTESIAN_POINT ( 'NONE',  ( 4.900006121741999010, -2.000000000000000000, 0.000000000000000000 ) ) ;
#24290 = CARTESIAN_POINT ( 'NONE',  ( 12.63945631780195988, -1.891770379292689874, 13.78384844198601122 ) ) ;
#24291 = CARTESIAN_POINT ( 'NONE',  ( 25.59036983458399916, 8.351023420428999700, -7.983780165365000236 ) ) ;
#24292 = CARTESIAN_POINT ( 'NONE',  ( 23.58312598483500011, 10.33118764019999958, -9.362116027220000802 ) ) ;
#24293 = CARTESIAN_POINT ( 'NONE',  ( 18.26001156276199922, -2.811979134698999960, -11.55266638147999991 ) ) ;
#24295 = LINE ( 'NONE', #44609, #2708 ) ;
#24294 = CARTESIAN_POINT ( 'NONE',  ( 9.601797255588000013, -2.721932483203000075, 7.554109351283189611 ) ) ;
#24296 = CARTESIAN_POINT ( 'NONE',  ( 10.44773515093974403, 5.286251723462902952, 7.027580072218848173 ) ) ;
#24297 = ORIENTED_EDGE ( 'NONE', *, *, #64210, .F. ) ;
#24298 = CARTESIAN_POINT ( 'NONE',  ( 0.1359928592618749876, 2.324556273228959184E-06, -3.136013406113613122 ) ) ;
#24299 = CARTESIAN_POINT ( 'NONE',  ( 10.88830300260000072, -2.841398431944000436, -5.064211128354999758 ) ) ;
#24300 = CARTESIAN_POINT ( 'NONE',  ( 9.235799540957000175, -4.950980172046000050, -5.959730545597000884 ) ) ;
#24301 = CARTESIAN_POINT ( 'NONE',  ( 10.90437023801000116, -5.099522774867000230, 5.132565236215000049 ) ) ;
#24302 = DIRECTION ( 'NONE',  ( -1.000000000000000000, 0.000000000000000000, 0.000000000000000000 ) ) ;
#24303 = CARTESIAN_POINT ( 'NONE',  ( 5.500000000000000000, 2.200000000000000178, 0.000000000000000000 ) ) ;
#24304 = ORIENTED_EDGE ( 'NONE', *, *, #44335, .T. ) ;
#24305 = CARTESIAN_POINT ( 'NONE',  ( 8.587349144951568647, 5.286378939600184346, -7.027172277035280246 ) ) ;
#24306 = CARTESIAN_POINT ( 'NONE',  ( 10.90000000000000036, -0.2999999999999999889, 4.902439024389999567 ) ) ;
#24308 = ADVANCED_FACE ( 'NONE', ( #46560 ), #51453, .T. ) ;
#24307 = CIRCLE ( 'NONE', #63367, 13.10000000000000142 ) ;
#24309 = ADVANCED_FACE ( 'NONE', ( #14059, #40616 ), #35385, .T. ) ;
#24310 = CARTESIAN_POINT ( 'NONE',  ( 10.96118313518939935, 3.207251432249800249, 6.497569908212999401 ) ) ;
#24311 = CONICAL_SURFACE ( 'NONE', #33252, 13.94999927503000059, 0.7853981058017837080 ) ;
#24312 = CARTESIAN_POINT ( 'NONE',  ( 13.63350196149396609, -9.056970873722326232, -7.433404858428114714 ) ) ;
#24313 = AXIS2_PLACEMENT_3D ( 'NONE', #1607, #28535, #49498 ) ;
#24314 = DIRECTION ( 'NONE',  ( 0.000000000000000000, 1.000000000000000000, 0.000000000000000000 ) ) ;
#24315 = CARTESIAN_POINT ( 'NONE',  ( 2.786020450147000282, -1.841856495097000002, 3.084057960614999594 ) ) ;
#24316 = ORIENTED_EDGE ( 'NONE', *, *, #2564, .F. ) ;
#24317 = CARTESIAN_POINT ( 'NONE',  ( 12.57154173166082778, 0.6810629908227098239, -12.58158054216573518 ) ) ;
#24318 = DIRECTION ( 'NONE',  ( -1.000000000000000000, 0.000000000000000000, -3.663735981262999544E-14 ) ) ;
#24319 = PLANE ( 'NONE',  #63283 ) ;
#24321 = CARTESIAN_POINT ( 'NONE',  ( 24.25374608244500152, 3.234182954713999969, -12.21793987376999979 ) ) ;
#24320 = AXIS2_PLACEMENT_3D ( 'NONE', #51553, #57142, #68308 ) ;
#24322 = FACE_OUTER_BOUND ( 'NONE', #47549, .T. ) ;
#24323 = ORIENTED_EDGE ( 'NONE', *, *, #1822, .T. ) ;
#24324 = CARTESIAN_POINT ( 'NONE',  ( 5.320019251605000221, -0.6654033835843000677, 1.142600628630999982 ) ) ;
#24325 = CARTESIAN_POINT ( 'NONE',  ( 10.90258158703495006, 9.831149648873696023, 5.672179247097546728 ) ) ;
#24326 = ADVANCED_FACE ( 'NONE', ( #24884 ), #46214, .T. ) ;
#24327 = CARTESIAN_POINT ( 'NONE',  ( 7.000000000000000000, 6.255435840762999966, -3.000000000000000000 ) ) ;
#24328 = CARTESIAN_POINT ( 'NONE',  ( 1.500973465873999935, 3.500000000000000000, 0.000000000000000000 ) ) ;
#24329 = AXIS2_PLACEMENT_3D ( 'NONE', #62996, #9522, #15471 ) ;
#24330 = CARTESIAN_POINT ( 'NONE',  ( 11.22567835872029995, 3.006051690924700370, -6.873560442659099046 ) ) ;
#24331 = ORIENTED_EDGE ( 'NONE', *, *, #2275, .F. ) ;
#24332 = CARTESIAN_POINT ( 'NONE',  ( 10.79499900793999956, -3.503951165873000040, 6.168577387731000172 ) ) ;
#24333 = ORIENTED_EDGE ( 'NONE', *, *, #56717, .T. ) ;
#24334 = DIRECTION ( 'NONE',  ( 1.000000000000000000, 0.000000000000000000, 0.000000000000000000 ) ) ;
#24335 = CARTESIAN_POINT ( 'NONE',  ( 8.753441940380000119, -2.876278577719999952, 6.568889245344999850 ) ) ;
#24336 = CARTESIAN_POINT ( 'NONE',  ( 17.97713831050997513, -0.5938246120522460147, -13.98740230410798091 ) ) ;
#24337 = ORIENTED_EDGE ( 'NONE', *, *, #60529, .T. ) ;
#24338 = CARTESIAN_POINT ( 'NONE',  ( 10.96923347446639774, 8.678024018201968559, -6.520394081641061490 ) ) ;
#24339 = FACE_OUTER_BOUND ( 'NONE', #45915, .T. ) ;
#24340 = AXIS2_PLACEMENT_3D ( 'NONE', #53130, #332, #5230 ) ;
#24341 = CARTESIAN_POINT ( 'NONE',  ( 10.26059687351666661, -4.629523725463621453, 8.592232985442825210 ) ) ;
#24342 = CARTESIAN_POINT ( 'NONE',  ( 9.396013540183334456, -4.999583552997726166, -8.268183399968641822 ) ) ;
#24343 = LINE ( 'NONE', #44654, #59713 ) ;
#24344 = ORIENTED_EDGE ( 'NONE', *, *, #13975, .F. ) ;
#24345 = CARTESIAN_POINT ( 'NONE',  ( 2.073890132539958131, 2.150913519912194705, 2.798833948393636639 ) ) ;
#24346 = CARTESIAN_POINT ( 'NONE',  ( 12.22437278969013263, -2.731306219322056528, -13.62162349208237089 ) ) ;
#24347 = CARTESIAN_POINT ( 'NONE',  ( 5.500000000000000000, -13.17499999999999893, 0.000000000000000000 ) ) ;
#24348 = FACE_OUTER_BOUND ( 'NONE', #59414, .T. ) ;
#24349 = VERTEX_POINT ( 'NONE', #57039 ) ;
#24350 = PRODUCT_DEFINITION_SHAPE ( 'NONE', 'NONE',  #69197 ) ;
#24351 = DIRECTION ( 'NONE',  ( -0.7071067759742961645, 0.7071067863987962054, 5.966942998097971758E-08 ) ) ;
#24352 = CARTESIAN_POINT ( 'NONE',  ( 8.936337454063531638, -4.868096831666449908, -6.831783586538417552 ) ) ;
#24353 = CARTESIAN_POINT ( 'NONE',  ( 6.875000000000000000, 5.574137966889000317, -8.240733100917999820 ) ) ;
#24354 = CARTESIAN_POINT ( 'NONE',  ( 18.18005044575085449, -2.500000006795658702, -13.67340643792831401 ) ) ;
#24355 = CARTESIAN_POINT ( 'NONE',  ( 12.80505043854144276, 0.7192913403693015351, 12.57945229203838267 ) ) ;
#24356 = ADVANCED_FACE ( 'NONE', ( #9141 ), #55509, .T. ) ;
#24357 = CARTESIAN_POINT ( 'NONE',  ( 12.19636843800076775, 0.1422577892986776338, -13.89902525486550466 ) ) ;
#24358 = CARTESIAN_POINT ( 'NONE',  ( 17.84375123822105991, -1.945578272181329504, 12.56362807389522018 ) ) ;
#24359 = VERTEX_POINT ( 'NONE', #51792 ) ;
#24360 = CARTESIAN_POINT ( 'NONE',  ( 10.72702344389999851, -5.004394439171999664, -6.890449684422599752 ) ) ;
#24361 = ORIENTED_EDGE ( 'NONE', *, *, #41059, .T. ) ;
#24362 = CARTESIAN_POINT ( 'NONE',  ( 9.534905769125000319, 3.030948166328000237, 8.761984216465000586 ) ) ;
#24363 = B_SPLINE_CURVE_WITH_KNOTS ( 'NONE', 3,
 ( #41770, #30943, #46682, #31291, #5396, #4355, #26385, #58530, #47020, #10636 ),
 .UNSPECIFIED., .F., .F.,
 ( 4, 2, 2, 2, 4 ),
 ( 0.000000000000000000, 0.2500000000000000000, 0.5000000000000000000, 0.7500000000000000000, 1.000000000000000000 ),
 .UNSPECIFIED. ) ;
#24364 = DIRECTION ( 'NONE',  ( 0.000000000000000000, 0.000000000000000000, -1.000000000000000000 ) ) ;
#24365 = CARTESIAN_POINT ( 'NONE',  ( 10.06481084123000080, 5.336630274082000192, -7.092011739486999922 ) ) ;
#24366 = CARTESIAN_POINT ( 'NONE',  ( 3.019675553083999819, 3.701628467739999984, -0.2181216002955000122 ) ) ;
#24367 = CARTESIAN_POINT ( 'NONE',  ( 10.87695483801000051, -5.827068285690999438, -7.814745128155998977 ) ) ;
#24368 = FACE_OUTER_BOUND ( 'NONE', #29797, .T. ) ;
#24369 = CARTESIAN_POINT ( 'NONE',  ( 9.044057935147195693, -4.875277019998068617, 8.528246069510029059 ) ) ;
#24370 = ADVANCED_BREP_SHAPE_REPRESENTATION ( '', ( #7958, #9676 ), #3105 ) ;
#24371 = ORIENTED_EDGE ( 'NONE', *, *, #37441, .F. ) ;
#24372 =( GEOMETRIC_REPRESENTATION_CONTEXT ( 3 ) GLOBAL_UNCERTAINTY_ASSIGNED_CONTEXT ( ( #49759 ) ) GLOBAL_UNIT_ASSIGNED_CONTEXT ( ( #64260, #58682, #32130 ) ) REPRESENTATION_CONTEXT ( 'NONE', 'WORKASPACE' ) );
#24373 = CARTESIAN_POINT ( 'NONE',  ( 10.97303166480599934, -5.137916160623999140, 7.419769534118209720 ) ) ;
#24374 = CARTESIAN_POINT ( 'NONE',  ( 10.87521525736000072, 4.831064930369000088, 6.312796576761000367 ) ) ;
#24375 = DIRECTION ( 'NONE',  ( 0.000000000000000000, 0.9999285272608851027, -0.01195576722244981981 ) ) ;
#24376 = CARTESIAN_POINT ( 'NONE',  ( 7.150000208772000043, 0.000000000000000000, 0.000000000000000000 ) ) ;
#24378 = CARTESIAN_POINT ( 'NONE',  ( 9.160383927730638476, 3.070077541678596589, 8.479412441495636443 ) ) ;
#24377 = CARTESIAN_POINT ( 'NONE',  ( 9.877261637240000169, 2.207988120125000009, 7.624813826992999921 ) ) ;
#24379 = CARTESIAN_POINT ( 'NONE',  ( 10.35410941423799791, 4.742797679580299963, -6.825313060354999628 ) ) ;
#24380 = DIRECTION ( 'NONE',  ( 0.000000000000000000, -0.2588190451024934835, 0.9659258262890757507 ) ) ;
#24381 = CARTESIAN_POINT ( 'NONE',  ( 9.275076168957998135, 3.490299597736799875, -8.365475476407400635 ) ) ;
#24382 = CARTESIAN_POINT ( 'NONE',  ( 17.60275121352128025, -0.7181168112306479667, 12.57951960855070261 ) ) ;
#24383 = CARTESIAN_POINT ( 'NONE',  ( 11.04752711762115780, 5.162390711389719833, -7.824990536777686856 ) ) ;
#24384 = CARTESIAN_POINT ( 'NONE',  ( 12.80505043854146940, -3.199751711897561801, 12.18694338143115452 ) ) ;
#24385 = DIRECTION ( 'NONE',  ( -1.000000000000000000, 0.000000000000000000, 0.000000000000000000 ) ) ;
#24386 = ORIENTED_EDGE ( 'NONE', *, *, #24951, .T. ) ;
#24387 = CARTESIAN_POINT ( 'NONE',  ( 8.924956853209002006, -4.158911960977000000, 5.873536005760000123 ) ) ;
#24388 = EDGE_CURVE ( 'NONE', #40252, #67674, #26703, .T. ) ;
#24389 = ADVANCED_FACE ( 'NONE', ( #2525 ), #23851, .T. ) ;
#24390 = CARTESIAN_POINT ( 'NONE',  ( 18.24173484165867976, 2.753291453986174808, 13.72661349255300856 ) ) ;
#24391 = CARTESIAN_POINT ( 'NONE',  ( 7.777775979742000523, -3.623726805927396821, 6.172770137145197289 ) ) ;
#24392 = CARTESIAN_POINT ( 'NONE',  ( 10.09259632033899834, 3.197262364844699611, 7.827597670336898794 ) ) ;
#24393 = B_SPLINE_CURVE_WITH_KNOTS ( 'NONE', 3,
 ( #45968, #61360, #67278, #45635, #13817, #40049, #66939, #2628, #45291, #13136 ),
 .UNSPECIFIED., .F., .F.,
 ( 4, 1, 1, 1, 1, 1, 1, 4 ),
 ( 0.000000000000000000, 0.1626725439853999866, 0.3253459288523000148, 0.4880193137191000119, 0.6506926985859999846, 0.8133660834529000683, 0.9760394683197000099, 1.000000000000000000 ),
 .UNSPECIFIED. ) ;
#24394 = ORIENTED_EDGE ( 'NONE', *, *, #17034, .T. ) ;
#24395 = CARTESIAN_POINT ( 'NONE',  ( 8.962739158771999115, 5.445214367171999470, 7.703373622193999459 ) ) ;
#24397 = CARTESIAN_POINT ( 'NONE',  ( 11.55300581613033906, 5.107584469683000172, 6.788791567531699656 ) ) ;
#24396 = CARTESIAN_POINT ( 'NONE',  ( 9.180747021775998107, -4.651672637235799712, -8.071865996877098937 ) ) ;
#24398 = CARTESIAN_POINT ( 'NONE',  ( 11.11477971959000044, 2.548217283716999848, -8.356742414746999970 ) ) ;
#24399 = ORIENTED_EDGE ( 'NONE', *, *, #50518, .F. ) ;
#24400 = CARTESIAN_POINT ( 'NONE',  ( 11.79999999497874796, 3.261294161473140107, -11.32146851427815193 ) ) ;
#24401 = CARTESIAN_POINT ( 'NONE',  ( 17.65063036598055390, -3.242172222319712471, -13.61940987276824799 ) ) ;
#24402 = CARTESIAN_POINT ( 'NONE',  ( 11.38379707368349969, 3.433355370490100533, 8.490052513816499058 ) ) ;
#24403 = CARTESIAN_POINT ( 'NONE',  ( 10.18909467608999897, -5.907859813488999912, 7.801539220053999912 ) ) ;
#24404 = CARTESIAN_POINT ( 'NONE',  ( 8.763353253171903390, 3.867553254011501629, -8.413353309630901222 ) ) ;
#24405 = ORIENTED_EDGE ( 'NONE', *, *, #18898, .F. ) ;
#24406 = PLANE ( 'NONE',  #10945 ) ;
#24407 = CARTESIAN_POINT ( 'NONE',  ( 1.396806799207750194, 0.9161175952574848180, -3.408904368339103819 ) ) ;
#24408 = APPLICATION_CONTEXT ( 'automotive_design' ) ;
#24409 = ADVANCED_FACE ( 'NONE', ( #18614 ), #60805, .F. ) ;
#24410 = CARTESIAN_POINT ( 'NONE',  ( 8.059688117792761730, -3.668144782959516181, 5.792266635259295526 ) ) ;
#24411 = CARTESIAN_POINT ( 'NONE',  ( 10.59344961228999971, -5.297755890367000120, 8.474197994416998725 ) ) ;
#24412 = CARTESIAN_POINT ( 'NONE',  ( 11.55811496860034815, -2.954409148022000053, -6.964183526617899744 ) ) ;
#24413 = CARTESIAN_POINT ( 'NONE',  ( 9.752709346416999381, -2.968569381205999669, 7.989780896525600085 ) ) ;
#24414 = ORIENTED_EDGE ( 'NONE', *, *, #49391, .F. ) ;
#24415 = CARTESIAN_POINT ( 'NONE',  ( 10.36994085745000049, -4.628299740363999604, -5.009923106717000252 ) ) ;
#24416 = B_SPLINE_CURVE_WITH_KNOTS ( 'NONE', 3,
 ( #44521, #27742, #49055, #43818, #33328, #28431, #49745, #1854, #23516, #65814, #17939, #39258, #34025, #55338, #39603, #7434, #35735, #29822 ),
 .UNSPECIFIED., .F., .F.,
 ( 4, 2, 2, 2, 2, 2, 2, 2, 4 ),
 ( 0.000000000000000000, 0.1250000000000000000, 0.2500000000000000000, 0.3750000000000000000, 0.5000000000000000000, 0.6250000000000000000, 0.7500000000000000000, 0.8750000000000000000, 1.000000000000000000 ),
 .UNSPECIFIED. ) ;
#24417 = CARTESIAN_POINT ( 'NONE',  ( 10.55041772631200026, -3.450375740502100275, 6.368647051112000135 ) ) ;
#24418 = EDGE_LOOP ( 'NONE', ( #3266, #11607, #58063, #18342, #25867 ) ) ;
#24419 = ADVANCED_FACE ( 'NONE', ( #29 ), #40177, .T. ) ;
#24420 = CARTESIAN_POINT ( 'NONE',  ( 8.975960865537832234, 2.874039072694928088, 7.353476508004328061 ) ) ;
#24421 = AXIS2_PLACEMENT_3D ( 'NONE', #3542, #51787, #19982 ) ;
#24422 = ORIENTED_EDGE ( 'NONE', *, *, #64955, .T. ) ;
#24423 = CARTESIAN_POINT ( 'NONE',  ( 6.605026506349999771, -1.500000000000000000, 0.000000000000000000 ) ) ;
#24424 = CARTESIAN_POINT ( 'NONE',  ( 9.881820280408998514, 4.325866256860000369, -9.125812605905000652 ) ) ;
#24425 = AXIS2_PLACEMENT_3D ( 'NONE', #52326, #4421, #43125 ) ;
#24426 = CARTESIAN_POINT ( 'NONE',  ( 3.799999782336999754, 0.000000000000000000, 0.000000000000000000 ) ) ;
#24427 = CARTESIAN_POINT ( 'NONE',  ( 1.699999999999999956, 0.000000000000000000, 0.000000000000000000 ) ) ;
#24428 = CARTESIAN_POINT ( 'NONE',  ( 12.18529561036834608, 2.583342615503332773, -12.43180850209203392 ) ) ;
#24429 = CARTESIAN_POINT ( 'NONE',  ( 11.19872335273220010, -3.650693637952500126, 6.559289673553299060 ) ) ;
#24430 = CARTESIAN_POINT ( 'NONE',  ( 7.860170280410000210, 2.263558315407000254, 8.007442119518000112 ) ) ;
#24431 = ORIENTED_EDGE ( 'NONE', *, *, #48777, .F. ) ;
#24432 = DIRECTION ( 'NONE',  ( 0.000000000000000000, 0.000000000000000000, 1.000000000000000000 ) ) ;
#24433 = CARTESIAN_POINT ( 'NONE',  ( 8.020980646792999380, -3.245532552444000185, 8.949627348471000943 ) ) ;
#24434 = CARTESIAN_POINT ( 'NONE',  ( 17.55505043854143921, -0.7302158263239086899, 13.98094363220831049 ) ) ;
#24435 = VERTEX_POINT ( 'NONE', #67777 ) ;
#24436 = CARTESIAN_POINT ( 'NONE',  ( 12.21438802940097901, -2.898246740288921153, -12.26216014320957015 ) ) ;
#24437 = CARTESIAN_POINT ( 'NONE',  ( 10.17764828895399809, 5.001141961424000471, 6.953185708700699408 ) ) ;
#24438 = CARTESIAN_POINT ( 'NONE',  ( 11.12964314679000033, -3.869080819553999628, -9.017146989745999264 ) ) ;
#24439 = CARTESIAN_POINT ( 'NONE',  ( 6.450859839683333874, -0.3926218265389256890, 1.460959015002472050 ) ) ;
#24440 = CARTESIAN_POINT ( 'NONE',  ( 17.75481218032700070, -12.16597452523000022, 3.139308580624999845 ) ) ;
#24441 = CARTESIAN_POINT ( 'NONE',  ( 9.797119508974258650, 5.515971184441423425, -6.595903550150567618 ) ) ;
#24442 = CARTESIAN_POINT ( 'NONE',  ( 12.24873136391195416, -2.785023419893231988, -13.60881341097601371 ) ) ;
#24443 = B_SPLINE_CURVE_WITH_KNOTS ( 'NONE', 3,
 ( #32003, #54690, #64469, #26405, #69046, #16245, #16593, #862, #7481, #60975, #22872, #28834, #18672, #13773, #17986, #28479, #34759, #65863, #35106, #44221, #39305, #49796, #29173, #60628, #45592, #50145, #23224, #40004, #65515, #2250, #6788, #1550, #23563, #44904, #34421, #2926, #24254, #13088, #55735, #17643, #23911, #38967 ),
 .UNSPECIFIED., .F., .F.,
 ( 4, 2, 2, 2, 2, 2, 2, 2, 2, 2, 2, 2, 2, 1, 2, 2, 2, 2, 2, 1, 2, 4 ),
 ( 0.4997863768847486954, 0.5623130797741535680, 0.6248397826635585517, 0.6404714583859092425, 0.6561031341082600443, 0.6873664855529640905, 0.7029981612753175568, 0.7186298369976709122, 0.7264456748588475898, 0.7342615127200242675, 0.7498931884423775118, 0.7811565398870811139, 0.7889723777482554601, 0.7967882156094298063, 0.8124198913317783877, 0.8280515670541268580, 0.8436832427764753284, 0.8749465942211771541, 0.8905782699435280669, 0.9062099456658790908, 0.9374732971105860235, 1.000000000000000000 ),
 .UNSPECIFIED. ) ;
#24444 = CARTESIAN_POINT ( 'NONE',  ( 11.36486084871759950, 2.792989229543000107, -7.825000000000000178 ) ) ;
#24445 = CARTESIAN_POINT ( 'NONE',  ( 10.69041504065829962, -2.975441626403999784, -6.736065107693399945 ) ) ;
#24446 = LINE ( 'NONE', #41548, #43403 ) ;
#24447 = ORIENTED_EDGE ( 'NONE', *, *, #3274, .T. ) ;
#24448 = ORIENTED_EDGE ( 'NONE', *, *, #26995, .F. ) ;
#24449 = AXIS2_PLACEMENT_3D ( 'NONE', #41814, #14566, #35883 ) ;
#24450 = CARTESIAN_POINT ( 'NONE',  ( 10.32891357011167166, 2.649873868442942371, -7.263327745080984776 ) ) ;
#24451 = CARTESIAN_POINT ( 'NONE',  ( 7.975339216757242333, 5.350090185752605976, 7.499980949462685231 ) ) ;
#24452 = CARTESIAN_POINT ( 'NONE',  ( 23.52038360246099913, -3.100182920209999970, 13.78394459507999947 ) ) ;
#24453 = CARTESIAN_POINT ( 'NONE',  ( 13.50018479229300006, 11.60142623882999935, 2.415183939829000259 ) ) ;
#24454 = CARTESIAN_POINT ( 'NONE',  ( 17.77742128654737286, 1.915804696728241163, 12.56864479336925200 ) ) ;
#24455 = EDGE_CURVE ( 'NONE', #27357, #42427, #23355, .T. ) ;
#24456 = DIRECTION ( 'NONE',  ( -1.000000000000000000, 0.000000000000000000, 0.000000000000000000 ) ) ;
#24457 = ADVANCED_FACE ( 'NONE', ( #47851 ), #51900, .F. ) ;
#24458 = CARTESIAN_POINT ( 'NONE',  ( 11.18051582549000145, 5.340073783367000892, 8.416152717850000187 ) ) ;
#24459 = CARTESIAN_POINT ( 'NONE',  ( 10.35465597998723553, -2.649863840850919416, -7.676734101936328436 ) ) ;
#24460 = ORIENTED_EDGE ( 'NONE', *, *, #21522, .F. ) ;
#24461 = CARTESIAN_POINT ( 'NONE',  ( 12.39767999896657003, -2.025889534879409037, 12.54950459294602894 ) ) ;
#24462 = CARTESIAN_POINT ( 'NONE',  ( 10.32844474310100047, -3.228742141949900279, -7.874284411628199365 ) ) ;
#24463 = CARTESIAN_POINT ( 'NONE',  ( 11.01776904286000125, 4.914120883409999863, 8.587704221454000475 ) ) ;
#24464 = CARTESIAN_POINT ( 'NONE',  ( 11.72056920625029974, -3.952687217764870198, 8.815417147437999645 ) ) ;
#24465 = CARTESIAN_POINT ( 'NONE',  ( 11.28118179236249929, 3.732952383914999839, -6.250199235344999771 ) ) ;
#24466 = CARTESIAN_POINT ( 'NONE',  ( 12.80505043854144276, 0.6249999999999995559, 12.67928921589117586 ) ) ;
#24467 = CARTESIAN_POINT ( 'NONE',  ( 8.224926658773000554, 5.629399530851999955, 8.631829656822000985 ) ) ;
#24468 = CARTESIAN_POINT ( 'NONE',  ( 10.09696969267000100, 5.253376380222999131, 8.530663119653999260 ) ) ;
#24469 = CIRCLE ( 'NONE', #18886, 0.5000000000000000000 ) ;
#24470 = CARTESIAN_POINT ( 'NONE',  ( 12.80505043854143388, 1.874999999999998890, 12.57541666120756041 ) ) ;
#24471 = VERTEX_POINT ( 'NONE', #39424 ) ;
#24472 = CARTESIAN_POINT ( 'NONE',  ( 8.699089158774000907, 4.178200486578000472, -5.608493638783999202 ) ) ;
#24473 = CARTESIAN_POINT ( 'NONE',  ( 10.76426088462129904, 4.002719309691810778, -6.221990224628999755 ) ) ;
#24474 = EDGE_CURVE ( 'NONE', #8000, #44629, #28446, .T. ) ;
#24475 = EDGE_CURVE ( 'NONE', #62424, #44629, #35861, .T. ) ;
#24476 = DIRECTION ( 'NONE',  ( -1.000000000000000000, 0.000000000000000000, 0.000000000000000000 ) ) ;
#24478 = DIRECTION ( 'NONE',  ( 0.000000000000000000, 0.7270098363383213913, -0.6866270442294909460 ) ) ;
#24477 = CARTESIAN_POINT ( 'NONE',  ( 7.828418146791999099, -5.524126964933000927, 6.910359834012999691 ) ) ;
#24479 = CARTESIAN_POINT ( 'NONE',  ( 9.275480666858999967, -3.710922827228400056, 6.682599852064000423 ) ) ;
#24480 = CARTESIAN_POINT ( 'NONE',  ( 10.62487750876920067, -4.543557328885200697, -8.343502390669698343 ) ) ;
#24481 = ORIENTED_EDGE ( 'NONE', *, *, #46838, .T. ) ;
#24482 = EDGE_CURVE ( 'NONE', #14271, #60041, #45896, .T. ) ;
#24483 = CARTESIAN_POINT ( 'NONE',  ( 1.343609070385000104, -2.423129934138000152, -2.873468012158999940 ) ) ;
#24484 = CARTESIAN_POINT ( 'NONE',  ( 10.98768472639999949, 2.860903110339000133, 4.945212061661000469 ) ) ;
#24486 = CARTESIAN_POINT ( 'NONE',  ( 15.86376629110799996, -3.753680978508000088, -11.28125155222999787 ) ) ;
#24485 = CARTESIAN_POINT ( 'NONE',  ( 8.767879976495999372, -3.394455611366999914, -6.293427637271999942 ) ) ;
#24487 = CARTESIAN_POINT ( 'NONE',  ( 7.000000000000000000, -7.526486366024999874, 3.526486366024999874 ) ) ;
#24488 = CARTESIAN_POINT ( 'NONE',  ( 10.01533268956000100, 4.946987614118000032, 8.559212393557999121 ) ) ;
#24489 = CARTESIAN_POINT ( 'NONE',  ( 12.80505043854146940, -3.248109929747638347, 13.61799478206225444 ) ) ;
#24490 = DIRECTION ( 'NONE',  ( 1.000000000000000000, 0.000000000000000000, 0.000000000000000000 ) ) ;
#24491 = DIRECTION ( 'NONE',  ( 0.000000000000000000, -1.000000000000000000, 0.000000000000000000 ) ) ;
#24492 = CARTESIAN_POINT ( 'NONE',  ( 7.667605646792000407, -5.638700495537999124, 8.266402903491000487 ) ) ;
#24493 = VERTEX_POINT ( 'NONE', #51961 ) ;
#24494 = CARTESIAN_POINT ( 'NONE',  ( 7.609454719589999527, 3.276311362504999991, 5.841989464160999290 ) ) ;
#24495 = DIRECTION ( 'NONE',  ( -1.000000000000000000, -2.893429392047000287E-14, 4.629487027275000025E-14 ) ) ;
#24496 = B_SPLINE_CURVE_WITH_KNOTS ( 'NONE', 3,
 ( #23456, #44793, #23799, #56987 ),
 .UNSPECIFIED., .F., .F.,
 ( 4, 4 ),
 ( 0.000000000000000000, 1.000000000000000000 ),
 .UNSPECIFIED. ) ;
#24497 = CARTESIAN_POINT ( 'NONE',  ( 7.362367228725729795, -3.210354122145276712, 9.056218515521349488 ) ) ;
#24498 = CARTESIAN_POINT ( 'NONE',  ( 17.55505043854144276, -0.6250000000000001110, -12.67928921589118474 ) ) ;
#24499 = CARTESIAN_POINT ( 'NONE',  ( 1.986430836446000159, -0.3042438094541999871, -3.579344195347000213 ) ) ;
#24500 = EDGE_LOOP ( 'NONE', ( #31411, #44369, #67026, #37033, #30892, #18407, #10399, #28007, #47766, #11793, #33177, #27509 ) ) ;
#24501 = FACE_BOUND ( 'NONE', #64142, .T. ) ;
#24502 = CARTESIAN_POINT ( 'NONE',  ( 12.80505043854144276, 0.6249999999999995559, -12.67928921589118652 ) ) ;
#24503 = EDGE_CURVE ( 'NONE', #46988, #54418, #55057, .T. ) ;
#24504 = DIRECTION ( 'NONE',  ( -1.000000000000000000, -0.000000000000000000, -0.000000000000000000 ) ) ;
#24505 = CARTESIAN_POINT ( 'NONE',  ( 11.14994211610999919, 2.627136771666999771, 6.696094414592000277 ) ) ;
#24506 = CARTESIAN_POINT ( 'NONE',  ( 11.51102763632551884, 3.088851714329700293, 7.920427941950599404 ) ) ;
#24507 = DIRECTION ( 'NONE',  ( 0.000000000000000000, -1.000000000000000000, 0.000000000000000000 ) ) ;
#24508 = CARTESIAN_POINT ( 'NONE',  ( 11.06877944038000017, -5.318813217120000658, -7.168443364726000411 ) ) ;
#24509 = CARTESIAN_POINT ( 'NONE',  ( 7.831326693633717362, -3.674448254819469017, 6.164223331809817630 ) ) ;
#24510 = CARTESIAN_POINT ( 'NONE',  ( 18.46577960220267300, 3.126461091534826320, -12.12859619074303552 ) ) ;
#24511 = CARTESIAN_POINT ( 'NONE',  ( 12.18798377888046502, -2.400256349692730495, 12.47427327512308359 ) ) ;
#24512 = CARTESIAN_POINT ( 'NONE',  ( 7.836291913262656728, 3.773376814137977320, 9.261296850680157178 ) ) ;
#24513 = VERTEX_POINT ( 'NONE', #25397 ) ;
#24514 = CARTESIAN_POINT ( 'NONE',  ( 17.99865897956992811, -3.095937021190230620, 13.65340307249647545 ) ) ;
#24515 = CARTESIAN_POINT ( 'NONE',  ( 5.700000000000000178, -12.50865771883999855, 2.924687089724999911 ) ) ;
#24516 = VERTEX_POINT ( 'NONE', #41823 ) ;
#24517 = VERTEX_POINT ( 'NONE', #46733 ) ;
#24518 = CARTESIAN_POINT ( 'NONE',  ( 10.44635971519499940, 4.459622816450200311, 8.264615166761799969 ) ) ;
#24519 = CARTESIAN_POINT ( 'NONE',  ( 5.227606837614000135, -0.3108367803229999948, 1.065889863396000115 ) ) ;
#24520 = CYLINDRICAL_SURFACE ( 'NONE', #14355, 1.500000000000000000 ) ;
#24521 = CARTESIAN_POINT ( 'NONE',  ( 9.034110134264999203, 4.695345051283999815, 8.660667941667000491 ) ) ;
#24522 = CARTESIAN_POINT ( 'NONE',  ( 10.81905590578999998, 2.899999999999999911, -6.571291218949999902 ) ) ;
#24523 = CARTESIAN_POINT ( 'NONE',  ( 9.809470517051625649, -3.358100414793015354, -8.094556297950068924 ) ) ;
#24524 = CARTESIAN_POINT ( 'NONE',  ( 9.701976361057999654, -3.399137684422000039, 6.026753338319999820 ) ) ;
#24525 = CARTESIAN_POINT ( 'NONE',  ( 18.05078025084783278, 0.5250004125410518974, -12.58906021966016020 ) ) ;
#24526 = LINE ( 'NONE', #40601, #2856 ) ;
#24527 = CARTESIAN_POINT ( 'NONE',  ( 11.07210672858429845, -4.692204557952299737, -6.979277962544199632 ) ) ;
#24528 = CARTESIAN_POINT ( 'NONE',  ( 5.500000000000000000, 0.000000000000000000, 0.000000000000000000 ) ) ;
#24529 = ORIENTED_EDGE ( 'NONE', *, *, #36782, .T. ) ;
#24530 = CARTESIAN_POINT ( 'NONE',  ( 9.433148997456999751, -5.167567567567999731, 6.822293592207000934 ) ) ;
#24531 =( NAMED_UNIT ( * ) SI_UNIT ( $, .STERADIAN. ) SOLID_ANGLE_UNIT ( ) );
#24532 = CARTESIAN_POINT ( 'NONE',  ( 24.71803171219655582, 8.650025487060094775, 8.600693273006482897 ) ) ;
#24533 = DIRECTION ( 'NONE',  ( -1.000000000000000000, 0.000000000000000000, 0.000000000000000000 ) ) ;
#24534 = CARTESIAN_POINT ( 'NONE',  ( 9.228442991499999692, 3.919472480837189909, -6.223324745230999433 ) ) ;
#24535 = EDGE_CURVE ( 'NONE', #66219, #20189, #68039, .T. ) ;
#24536 = CARTESIAN_POINT ( 'NONE',  ( 12.09815554886058386, 2.355526959511344387, 13.80042145504355311 ) ) ;
#24537 = ADVANCED_FACE ( 'NONE', ( #4752 ), #35403, .T. ) ;
#24538 = CARTESIAN_POINT ( 'NONE',  ( 10.02202195053999922, -3.298019507654999849, 5.700533868754000366 ) ) ;
#24539 = ORIENTED_EDGE ( 'NONE', *, *, #11126, .F. ) ;
#24540 = CARTESIAN_POINT ( 'NONE',  ( 12.57406965109622909, 0.5808252089534533535, -12.68211610571899861 ) ) ;
#24541 = CARTESIAN_POINT ( 'NONE',  ( 12.08472014176158282, -0.08359636179364632325, 13.99975542440154186 ) ) ;
#24542 = ORIENTED_EDGE ( 'NONE', *, *, #30702, .T. ) ;
#24543 = CARTESIAN_POINT ( 'NONE',  ( 24.30000000000000071, -12.03537377768999939, -3.224868684338999980 ) ) ;
#24544 = DIRECTION ( 'NONE',  ( -1.000000000000000000, 0.000000000000000000, 0.000000000000000000 ) ) ;
#24545 = VECTOR ( 'NONE', #32922, 999.9999999999998863 ) ;
#24546 = PLANE ( 'NONE',  #59786 ) ;
#24547 = DIRECTION ( 'NONE',  ( -1.000000000000000000, 0.000000000000000000, 0.000000000000000000 ) ) ;
#24548 = B_SPLINE_CURVE_WITH_KNOTS ( 'NONE', 3,
 ( #35375, #30467, #67511, #25559 ),
 .UNSPECIFIED., .F., .F.,
 ( 4, 4 ),
 ( 0.5000000026798849806, 1.000000000000000000 ),
 .UNSPECIFIED. ) ;
#24549 = B_SPLINE_SURFACE_WITH_KNOTS ( 'NONE', 1, 3, ( 
 ( #48319, #424, #16500, #37827, #23477, #6004, #59839, #44127, #27344, #11946, #1809, #66119, #1118, #11590, #17897, #49011, #18239, #48666, #22431, #54245, #7050, #43773, #49700, #771, #32590, #65067, #6347, #59148, #12646, #49347, #60540, #12300, #23129, #28039, #60196, #38518, #33284, #17187, #27695, #54948, #33633, #54600, #6698, #33976, #1462, #22777, #65425, #17547, #32934, #28386, #38874, #39214, #11252, #65771, #7392, #44479, #55297, #28738, #50054, #2161, #44816, #53904, #22086, #43431, #64725, #16841, #38163, #59493, #45157, #35016, #13347, #55986, #34672, #29781, #8091, #19260, #29435, #40250, #45501, #3857, #67147, #56330, #66814, #61231, #40588, #46183, #18585, #14375, #61913, #40932 ),
 ( #35355, #56677, #8777, #3186, #13000, #50741, #30119, #51761, #13686, #29085, #51422, #8434, #3517, #67492, #2838, #25192, #55645, #61571, #24514, #7745, #51084, #24855, #46526, #24165, #18925, #19611, #45835, #67834, #50395, #14029, #62254, #35694, #57010, #9110, #2495, #34326, #30448, #39560, #60884, #23820, #66463, #39913, #42321, #31823, #58045, #20985, #68516, #63271, #25883, #36372, #15738, #63622, #47212, #57687, #43609, #20637, #54084, #19955, #9797, #68864, #47562, #48850, #10147, #41963, #41279, #68174, #15401, #49187, #11776, #62587, #33118, #14709, #37066, #957, #31477, #52799, #41618, #36026, #4543, #58378, #31147, #52448, #62926, #10485, #36726, #22268, #27879, #27522, #38351, #4892 ) ),
 .UNSPECIFIED., .F., .F., .F.,
 ( 2, 2 ),
 ( 4, 2, 2, 2, 2, 2, 2, 2, 2, 2, 2, 2, 2, 2, 2, 2, 2, 2, 2, 2, 2, 2, 2, 2, 2, 2, 2, 2, 2, 2, 2, 2, 2, 2, 2, 2, 2, 2, 2, 2, 2, 2, 2, 2, 4 ),
 ( 0.000000000000000000, 1.000000000000000000 ),
 ( 0.000000000000000000, 7.142752612018008851E-05, 0.0001428550522403601770, 0.0002142825783605402791, 0.0002857101044807203540, 0.0003214238675408103915, 0.0003571376306009004832, 0.0003928513936609905207, 0.0004285651567210805582, 0.0004999926828412606331, 0.0005357064459013507248, 0.0005714202089614407081, 0.0006071339720215306913, 0.0006428477350816207830, 0.0007142752612018009664, 0.0007857027873219810414, 0.0008214165503820710246, 0.0008571303134421611163, 0.0009285578395623411913, 0.0009999853656825212662, 0.001071412891802701450, 0.001142840417922881416, 0.001214267944043061383, 0.001285695470163241566, 0.001321409233223331658, 0.001357122996283421749, 0.001428550522403601933, 0.001499978048523782116, 0.001535691811583872208, 0.001571405574643962083, 0.001607119337704051958, 0.001642833100764142049, 0.001714260626884322233, 0.001749974389944412324, 0.001785688153004502416, 0.001821401916064592508, 0.001857115679124682383, 0.001928543205244862349, 0.001964256968304952441, 0.001999970731365042532, 0.002035684494425132624, 0.002071398257485222716, 0.002142825783605402899, 0.002214253309725583083, 0.002285680835845762832 ),
 .UNSPECIFIED. ) ;
#24550 = CARTESIAN_POINT ( 'NONE',  ( 8.813083809908729194, 2.920641027582035143, -8.329586155797288782 ) ) ;
#24551 = B_SPLINE_CURVE_WITH_KNOTS ( 'NONE', 3,
 ( #36216, #57531, #4041, #19794, #25723, #41122, #52988, #31321, #35540, #5083, #35873, #3698, #25036, #9985, #63460, #68017, #41465, #20477 ),
 .UNSPECIFIED., .F., .F.,
 ( 4, 2, 2, 2, 2, 2, 2, 2, 4 ),
 ( 0.000000000000000000, 0.1250000000000000000, 0.2500000000000000000, 0.3750000000000000000, 0.5000000000000000000, 0.6250000000000000000, 0.7500000000000000000, 0.8750000000000000000, 1.000000000000000000 ),
 .UNSPECIFIED. ) ;
#24552 = CARTESIAN_POINT ( 'NONE',  ( 0.3511782687132000147, -3.457229061792999936, 0.7500022461462000356 ) ) ;
#24553 = CARTESIAN_POINT ( 'NONE',  ( 11.07766112459999874, 2.724913093130999719, 5.089213754333000495 ) ) ;
#24554 = CARTESIAN_POINT ( 'NONE',  ( 10.35987047770899672, -5.250000000000000000, -7.750389189149368363 ) ) ;
#24555 = DIRECTION ( 'NONE',  ( 0.000000000000000000, -1.000000000000000000, 0.000000000000000000 ) ) ;
#24556 = CARTESIAN_POINT ( 'NONE',  ( 10.85056919669530018, 4.830699382454300306, -7.745432529082900253 ) ) ;
#24557 = CARTESIAN_POINT ( 'NONE',  ( 6.999998782146999332, -11.95749337870000062, -3.642574926947999892 ) ) ;
#24558 = CARTESIAN_POINT ( 'NONE',  ( 10.90346005378009941, 4.786957292481900161, -7.079777642108599167 ) ) ;
#24559 = CARTESIAN_POINT ( 'NONE',  ( 9.100734463322998735, 4.118936914955599882, -8.635600483553998785 ) ) ;
#24561 = DIRECTION ( 'NONE',  ( 0.000000000000000000, -0.2714570858282905341, -0.9624505444715651947 ) ) ;
#24560 = CARTESIAN_POINT ( 'NONE',  ( 9.291809814040998816, -3.469640109842400122, 6.814123855771700100 ) ) ;
#24562 = CARTESIAN_POINT ( 'NONE',  ( 23.59542428366313871, -13.38815799942825180, 4.017037056778253401 ) ) ;
#24563 = ORIENTED_EDGE ( 'NONE', *, *, #59648, .T. ) ;
#24564 = EDGE_CURVE ( 'NONE', #66838, #49580, #34305, .T. ) ;
#24565 = CARTESIAN_POINT ( 'NONE',  ( 11.44366954483529852, 4.485203148598100320, 8.248643701125299543 ) ) ;
#24566 = CARTESIAN_POINT ( 'NONE',  ( 9.815199780373001559, -2.813634733202999616, 8.848854270764999086 ) ) ;
#24567 = CARTESIAN_POINT ( 'NONE',  ( 9.201101285863998669, 3.264788442324599860, 8.373612278672599274 ) ) ;
#24568 = FACE_OUTER_BOUND ( 'NONE', #22875, .T. ) ;
#24569 = B_SPLINE_CURVE_WITH_KNOTS ( 'NONE', 3,
 ( #5718, #42106, #63411, #58866, #9586, #21798, #21121, #26370, #68656, #138, #63755, #20774, #9938, #37535, #48374, #15535, #15867, #57830, #64097, #36509, #32311, #31615, #16558, #16212, #31275, #10972, #53621, #36859, #43132, #37199, #58518, #27061, #25675, #30931, #52586, #4680, #10621, #5031, #31964, #58179, #64436, #53280, #10281, #26021, #483, #52241, #47697 ),
 .UNSPECIFIED., .F., .F.,
 ( 4, 2, 2, 2, 2, 2, 2, 2, 1, 2, 2, 2, 2, 2, 2, 1, 2, 2, 1, 2, 2, 2, 2, 2, 4 ),
 ( 0.4985961975200040586, 0.5299339351750088634, 0.5456028040025113768, 0.5612716728300137792, 0.5691061072437652024, 0.5769405416575167367, 0.5926094104850196942, 0.6004438448987712285, 0.6082782793125226517, 0.6239471481400227226, 0.6396160169675227936, 0.6552848857950228645, 0.6709537546225230464, 0.6866226234500231174, 0.7022914922775231883, 0.7179603611050232592, 0.7492980987600234011, 0.7649669675875218067, 0.7806358364150202123, 0.8119735740700166904, 0.8433113117250129465, 0.8746490493800094246, 0.9059867870350057917, 0.9373245246900021588, 1.000000000000000000 ),
 .UNSPECIFIED. ) ;
#24570 = CARTESIAN_POINT ( 'NONE',  ( 10.97865453029000093, -5.273142482194999481, 7.958032781726000593 ) ) ;
#24571 = FACE_OUTER_BOUND ( 'NONE', #26464, .T. ) ;
#24572 = CARTESIAN_POINT ( 'NONE',  ( 23.58885226882633290, 2.922211860835754127, -13.61647608845786372 ) ) ;
#24573 = VERTEX_POINT ( 'NONE', #14232 ) ;
#24574 = CARTESIAN_POINT ( 'NONE',  ( 9.404684229509999938, -4.804883439508000897, -6.690125258578699885 ) ) ;
#24575 = CARTESIAN_POINT ( 'NONE',  ( 24.30000000000000071, 8.810505093353000916, 8.810505093353000916 ) ) ;
#24576 = CARTESIAN_POINT ( 'NONE',  ( 11.81389666366019853, -4.045876550911099656, 6.467512203247999913 ) ) ;
#24577 = ADVANCED_FACE ( 'NONE', ( #4408 ), #3718, .F. ) ;
#24578 = CARTESIAN_POINT ( 'NONE',  ( 18.27887336143457375, 2.529852868668377663, -12.34343546511471246 ) ) ;
#24579 = CARTESIAN_POINT ( 'NONE',  ( 11.04628392526000091, -2.754466683149000339, 5.119640974370000208 ) ) ;
#24580 = DIRECTION ( 'NONE',  ( 0.000000000000000000, 0.000000000000000000, -1.000000000000000000 ) ) ;
#24581 = CARTESIAN_POINT ( 'NONE',  ( 12.18033707851134650, 2.521449564491300421, -13.66889060753329055 ) ) ;
#24582 = CARTESIAN_POINT ( 'NONE',  ( 9.614739029020999084, -5.020908168068000776, -6.342951604057000203 ) ) ;
#24583 = CARTESIAN_POINT ( 'NONE',  ( 10.20000099824999928, 0.000000000000000000, 0.000000000000000000 ) ) ;
#24584 = ORIENTED_EDGE ( 'NONE', *, *, #60890, .T. ) ;
#24585 = CARTESIAN_POINT ( 'NONE',  ( 18.28051081950323820, 2.330210462401051785, -13.80606256597729775 ) ) ;
#24586 = CARTESIAN_POINT ( 'NONE',  ( 12.30074708396108285, 0.5247499651446917435, -13.99016470477802443 ) ) ;
#24588 = DIRECTION ( 'NONE',  ( 0.000000000000000000, 1.000000000000000000, 0.000000000000000000 ) ) ;
#24587 = SHAPE_REPRESENTATION ( 'Terminal Screw 2', ( #9676 ), #38794 ) ;
#24589 = CARTESIAN_POINT ( 'NONE',  ( 18.14737500097629663, -2.299536442346259424, -13.71390152310622845 ) ) ;
#24590 = CARTESIAN_POINT ( 'NONE',  ( 18.18000379063191474, 2.491959044446622862, 12.45343158198893008 ) ) ;
#24591 = AXIS2_PLACEMENT_3D ( 'NONE', #45587, #18325, #40670 ) ;
#24592 = CARTESIAN_POINT ( 'NONE',  ( 8.374639158773000247, 2.721111233225000259, -6.936528696292000085 ) ) ;
#24593 = CARTESIAN_POINT ( 'NONE',  ( 6.627181666795220139, -0.9418933528413754308, -1.199469319010407542 ) ) ;
#24594 = ORIENTED_EDGE ( 'NONE', *, *, #39900, .T. ) ;
#24595 = B_SPLINE_CURVE_WITH_KNOTS ( 'NONE', 3,
 ( #56576, #13597, #56233, #8341, #30027, #7999 ),
 .UNSPECIFIED., .F., .F.,
 ( 4, 2, 4 ),
 ( 0.000000000000000000, 0.5000000000000000000, 1.000000000000000000 ),
 .UNSPECIFIED. ) ;
#24596 = CARTESIAN_POINT ( 'NONE',  ( 4.000000000000000000, 0.2816038378556620092, 2.149891155406186805 ) ) ;
#24597 = CARTESIAN_POINT ( 'NONE',  ( 18.08598429698832888, 3.015255620044098084, -13.67144160714441803 ) ) ;
#24598 = ORIENTED_EDGE ( 'NONE', *, *, #61441, .T. ) ;
#24599 = CARTESIAN_POINT ( 'NONE',  ( 10.69391290906799874, -4.548591194283900130, 6.828616613600999585 ) ) ;
#24600 = CARTESIAN_POINT ( 'NONE',  ( 0.2500098862125000321, 0.000000000000000000, -3.249989426617000188 ) ) ;
#24601 = CARTESIAN_POINT ( 'NONE',  ( 9.003345280414000840, 2.319062457810000311, -7.919229449146000022 ) ) ;
#24602 = CARTESIAN_POINT ( 'NONE',  ( 15.89979320885400327, 3.824231472901999496, 11.71686814605000038 ) ) ;
#24603 = CARTESIAN_POINT ( 'NONE',  ( 11.72433327354039889, -4.983220429128399687, -6.856888818507299810 ) ) ;
#24604 = LINE ( 'NONE', #25977, #13654 ) ;
#24605 = DIRECTION ( 'NONE',  ( -1.000000000000000000, 0.000000000000000000, 0.000000000000000000 ) ) ;
#24606 = VERTEX_POINT ( 'NONE', #12683 ) ;
#24607 = DIRECTION ( 'NONE',  ( 1.000000000000000000, 0.000000000000000000, 0.000000000000000000 ) ) ;
#24608 = CARTESIAN_POINT ( 'NONE',  ( 5.699999545467999695, 12.03770622561999915, -3.722046322334000124 ) ) ;
#24609 = CARTESIAN_POINT ( 'NONE',  ( 10.01622971959000097, 4.325866256860000369, -9.125812605905000652 ) ) ;
#24610 = ORIENTED_EDGE ( 'NONE', *, *, #61702, .F. ) ;
#24611 = CARTESIAN_POINT ( 'NONE',  ( 10.11859053700000111, 3.393394511985999618, -5.921995869926000466 ) ) ;
#24612 = FILL_AREA_STYLE_COLOUR ( '', #17534 ) ;
#24613 = ORIENTED_EDGE ( 'NONE', *, *, #62349, .T. ) ;
#24614 = CARTESIAN_POINT ( 'NONE',  ( 9.531329965421999617, 3.206942993865000258, 6.678540912152799436 ) ) ;
#24615 = CARTESIAN_POINT ( 'NONE',  ( 17.76275439675993084, -1.910499210220269362, -12.56953514877129763 ) ) ;
#24616 = CARTESIAN_POINT ( 'NONE',  ( 23.56665676678700194, 3.767123864185000533E-06, -13.98989063586000015 ) ) ;
#24617 = EDGE_CURVE ( 'NONE', #56214, #18715, #46579, .T. ) ;
#24618 = EDGE_CURVE ( 'NONE', #30029, #23303, #5241, .T. ) ;
#24619 = LINE ( 'NONE', #57111, #43597 ) ;
#24620 = EDGE_CURVE ( 'NONE', #4443, #44819, #51704, .T. ) ;
#24621 = EDGE_CURVE ( 'NONE', #38467, #48923, #13095, .T. ) ;
#24622 = CARTESIAN_POINT ( 'NONE',  ( 9.404541696082119984, -2.531018779588075862, 8.431930544983709197 ) ) ;
#24623 = VERTEX_POINT ( 'NONE', #6386 ) ;
#24624 = CARTESIAN_POINT ( 'NONE',  ( 11.60000000000000142, 3.254367469151916659, 6.836536274993708417 ) ) ;
#24625 = CARTESIAN_POINT ( 'NONE',  ( 10.99306084123000105, 4.495422912016000083, -6.233618171705999522 ) ) ;
#24626 = B_SPLINE_CURVE_WITH_KNOTS ( 'NONE', 3,
 ( #13989, #52409, #46486, #46142 ),
 .UNSPECIFIED., .F., .F.,
 ( 4, 4 ),
 ( 0.000000000000000000, 1.000000000000000000 ),
 .UNSPECIFIED. ) ;
#24627 = DIRECTION ( 'NONE',  ( 0.000000000000000000, 1.000000000000000000, 0.000000000000000000 ) ) ;
#24628 = CARTESIAN_POINT ( 'NONE',  ( 12.47175297079831147, 3.166474622353412816, -13.63720910406327036 ) ) ;
#24629 = CARTESIAN_POINT ( 'NONE',  ( 9.481734463323000739, -3.866750753272200303, -8.772253522581999974 ) ) ;
#24630 = VECTOR ( 'NONE', #9907, 1000.000000000000000 ) ;
#24631 = CARTESIAN_POINT ( 'NONE',  ( 18.16428164030674708, 0.3960277493246572855, 13.99440111282555499 ) ) ;
#24632 = DIRECTION ( 'NONE',  ( 0.000000000000000000, 0.000000000000000000, 1.000000000000000000 ) ) ;
#24633 = CARTESIAN_POINT ( 'NONE',  ( 7.836395553874887732, 4.967689597840368343, 6.498195682940909101 ) ) ;
#24634 = VERTEX_POINT ( 'NONE', #60234 ) ;
#24635 = EDGE_LOOP ( 'NONE', ( #19712, #5518, #10120 ) ) ;
#24636 = CARTESIAN_POINT ( 'NONE',  ( 9.526695280414001488, 5.462898983065000102, -8.055936939571999744 ) ) ;
#24637 = CARTESIAN_POINT ( 'NONE',  ( 10.75304154458338424, -2.714670728013225176, 7.026954893539181235 ) ) ;
#24638 = CARTESIAN_POINT ( 'NONE',  ( 7.474999999999999645, -5.349999999999999645, 7.500000000000000000 ) ) ;
#24639 = CARTESIAN_POINT ( 'NONE',  ( 24.26256944702610241, 3.289100563212026263, 12.27508693394269734 ) ) ;
#24640 = CARTESIAN_POINT ( 'NONE',  ( 24.45284658036600334, 8.898487387712000540, -9.226082598753000852 ) ) ;
#24642 = VECTOR ( 'NONE', #59372, 1000.000000000000000 ) ;
#24641 = CARTESIAN_POINT ( 'NONE',  ( 11.49977531252999974, 12.52500000000000213, 0.5112815185527809225 ) ) ;
#24644 = CARTESIAN_POINT ( 'NONE',  ( 8.987367436956978040, 2.413693647671283138, 6.702895723592559030 ) ) ;
#24643 = CARTESIAN_POINT ( 'NONE',  ( 10.51163399569799850, -2.865156490077000129, 7.374045024026299799 ) ) ;
#24645 = CARTESIAN_POINT ( 'NONE',  ( 10.43314899746000002, 5.167567567567999731, 6.822293592207000934 ) ) ;
#24646 = EDGE_LOOP ( 'NONE', ( #53025, #28803, #54297, #6617 ) ) ;
#24647 = CARTESIAN_POINT ( 'NONE',  ( 12.08019303639033737, -0.1916560649207423583, 13.99999316327168941 ) ) ;
#24648 = LINE ( 'NONE', #30247, #8425 ) ;
#24649 = CARTESIAN_POINT ( 'NONE',  ( 9.971744136172999262, -5.176458967229000230, -8.738385553646999426 ) ) ;
#24650 = DIRECTION ( 'NONE',  ( -1.000000000000000000, 0.000000000000000000, 0.000000000000000000 ) ) ;
#24651 = DIRECTION ( 'NONE',  ( 1.083438471561000184E-09, -7.356835621337999415E-11, -1.000000000000000000 ) ) ;
#24652 = CARTESIAN_POINT ( 'NONE',  ( 11.04399668386999878, -5.244518219639999757, 5.182772251997000090 ) ) ;
#24653 = CARTESIAN_POINT ( 'NONE',  ( 8.895035841232999729, 5.751585344281000545, -8.235867044345999588 ) ) ;
#24654 = CARTESIAN_POINT ( 'NONE',  ( 10.05041772631199848, 4.549624259497900169, 6.368647051112000135 ) ) ;
#24655 = CARTESIAN_POINT ( 'NONE',  ( 7.000000000000000000, 0.000000000000000000, 0.000000000000000000 ) ) ;
#24656 = EDGE_CURVE ( 'NONE', #8263, #37501, #37590, .T. ) ;
#24657 = CARTESIAN_POINT ( 'NONE',  ( 0.2219399104530190292, 3.221919627416792054, 0.4208838488400382660 ) ) ;
#24658 = CARTESIAN_POINT ( 'NONE',  ( 3.253293268430000218, 2.728051603523000246, -1.782980944594999784 ) ) ;
#24659 = ORIENTED_EDGE ( 'NONE', *, *, #52896, .F. ) ;
#24660 = CARTESIAN_POINT ( 'NONE',  ( 12.30913258640365804, 0.5248261352964559423, -12.58906749861124119 ) ) ;
#24661 = CARTESIAN_POINT ( 'NONE',  ( 12.23322259331983197, -2.246983130391676298, -12.50693187469075163 ) ) ;
#24662 = EDGE_CURVE ( 'NONE', #62522, #67932, #39598, .T. ) ;
#24663 = CARTESIAN_POINT ( 'NONE',  ( 5.500000000000000000, 0.000000000000000000, 0.000000000000000000 ) ) ;
#24664 = CARTESIAN_POINT ( 'NONE',  ( 7.743176658771999676, 2.735218126362000124, 6.771983639047999937 ) ) ;
#24665 = CARTESIAN_POINT ( 'NONE',  ( 17.80000000009400196, -3.216307036143000175, -11.40341376487999980 ) ) ;
#24666 = ORIENTED_EDGE ( 'NONE', *, *, #45423, .F. ) ;
#24667 = CARTESIAN_POINT ( 'NONE',  ( 5.572090849689999459, 0.6950325411885999172, -1.124902434106000104 ) ) ;
#24668 = VECTOR ( 'NONE', #27397, 1000.000000000000227 ) ;
#24669 = APPLICATION_PROTOCOL_DEFINITION ( 'draft international standard', 'automotive_design', 1998, #51657 ) ;
#24670 = CARTESIAN_POINT ( 'NONE',  ( 17.93438960674995997, 0.4968201168833306092, 12.68691926186746599 ) ) ;
#24671 = CARTESIAN_POINT ( 'NONE',  ( 13.36715644869600084, -11.69666705770999826, -2.137627928029000035 ) ) ;
#24672 = CARTESIAN_POINT ( 'NONE',  ( 1.646806799206750105, -0.9161175952574931447, 3.408904368339100710 ) ) ;
#24673 = CARTESIAN_POINT ( 'NONE',  ( 11.43856039236529831, 5.032284719763000069, -7.550239075043479353 ) ) ;
#24674 = ORIENTED_EDGE ( 'NONE', *, *, #10275, .T. ) ;
#24675 = B_SPLINE_CURVE_WITH_KNOTS ( 'NONE', 3,
 ( #34516, #55826, #50576, #2678 ),
 .UNSPECIFIED., .F., .F.,
 ( 4, 4 ),
 ( 0.000000000000000000, 1.000000000000000000 ),
 .UNSPECIFIED. ) ;
#24676 = CARTESIAN_POINT ( 'NONE',  ( 9.701976361057999654, -3.399137684422000039, 6.026753338319999820 ) ) ;
#24677 = ORIENTED_EDGE ( 'NONE', *, *, #7571, .F. ) ;
#24678 = AXIS2_PLACEMENT_3D ( 'NONE', #24270, #45605, #34435 ) ;
#24679 = CARTESIAN_POINT ( 'NONE',  ( 8.503174978518606153, -3.164505085781523785, 6.034520370687764590 ) ) ;
#24680 = CARTESIAN_POINT ( 'NONE',  ( 7.726441940376999717, -2.630475685621000093, 6.995953627589999613 ) ) ;
#24681 = CARTESIAN_POINT ( 'NONE',  ( 18.20553441509224868, 0.3226776716457254168, -13.99628514671255886 ) ) ;
#24682 = ORIENTED_EDGE ( 'NONE', *, *, #50915, .T. ) ;
#24683 = CARTESIAN_POINT ( 'NONE',  ( 7.724131401290000198, -9.034333619270000781, 5.486219533306999629 ) ) ;
#24684 = CARTESIAN_POINT ( 'NONE',  ( 7.998183527237331170, 4.138725758259847787, -6.144309761568537809 ) ) ;
#24685 = AXIS2_PLACEMENT_3D ( 'NONE', #51549, #63750, #24983 ) ;
#24686 = FACE_OUTER_BOUND ( 'NONE', #29548, .T. ) ;
#24687 = DIRECTION ( 'NONE',  ( 1.000000000000000000, 0.000000000000000000, 0.000000000000000000 ) ) ;
#24688 = CARTESIAN_POINT ( 'NONE',  ( 18.03251246676483888, -2.904216811341680415, 12.34819510225881523 ) ) ;
#24689 = VERTEX_POINT ( 'NONE', #22468 ) ;
#24690 = CARTESIAN_POINT ( 'NONE',  ( 2.209306799207166883, -3.058252359239909790, 1.762666431298136382 ) ) ;
#24691 = CARTESIAN_POINT ( 'NONE',  ( 12.22105292107917762, -2.722876829297403489, -13.62360956001007573 ) ) ;
#24692 = DIRECTION ( 'NONE',  ( 0.000000000000000000, 1.000000000000000000, 0.000000000000000000 ) ) ;
#24693 = CARTESIAN_POINT ( 'NONE',  ( 10.40879003340999986, -3.093879171920000282, -6.480773124728999690 ) ) ;
#24694 = CARTESIAN_POINT ( 'NONE',  ( 11.59999999999999964, 4.000000000000000000, 7.500000000000000000 ) ) ;
#24695 = EDGE_LOOP ( 'NONE', ( #2063, #12783, #48835, #23373 ) ) ;
#24696 = CARTESIAN_POINT ( 'NONE',  ( 17.93438719463079423, 0.4968219663173571443, -13.88804946349586977 ) ) ;
#24697 = CARTESIAN_POINT ( 'NONE',  ( 10.97755399909358154, 4.133346405062088280, -8.778526265510096849 ) ) ;
#24698 = CARTESIAN_POINT ( 'NONE',  ( 24.67921569845699992, 12.29514839105000057, -2.979196030862000022 ) ) ;
#24699 = CARTESIAN_POINT ( 'NONE',  ( 10.90000000296000060, 5.100000000009000445, -5.160242730682999657 ) ) ;
#24700 = B_SPLINE_CURVE_WITH_KNOTS ( 'NONE', 3,
 ( #16099, #63643, #10172, #4919 ),
 .UNSPECIFIED., .F., .F.,
 ( 4, 4 ),
 ( 0.000000000000000000, 1.000000000000000000 ),
 .UNSPECIFIED. ) ;
#24701 = CARTESIAN_POINT ( 'NONE',  ( 12.18127378141864980, -0.04040202251154306756, -13.89992604541789589 ) ) ;
#24702 = EDGE_CURVE ( 'NONE', #41793, #59855, #39895, .T. ) ;
#24704 = EDGE_CURVE ( 'NONE', #67791, #43366, #61736, .T. ) ;
#24703 = CARTESIAN_POINT ( 'NONE',  ( 18.12629019086307025, -2.246197018143532009, 12.50711533121134522 ) ) ;
#24705 = ORIENTED_EDGE ( 'NONE', *, *, #2140, .T. ) ;
#24706 = CARTESIAN_POINT ( 'NONE',  ( 10.43614141025499897, -3.450366949021700158, -8.478951440767898973 ) ) ;
#24707 = VERTEX_POINT ( 'NONE', #16880 ) ;
#24708 = CARTESIAN_POINT ( 'NONE',  ( 10.23809632363000155, 2.752447932331000047, 6.820051270595000048 ) ) ;
#24709 = DIRECTION ( 'NONE',  ( -1.000000000000000000, 0.000000000000000000, 0.000000000000000000 ) ) ;
#24710 = CARTESIAN_POINT ( 'NONE',  ( 9.626145280412998773, 3.934138271021000222, -9.063586117809000697 ) ) ;
#24711 = CARTESIAN_POINT ( 'NONE',  ( 3.396928224380999950, -0.1132628685336000002, -3.706319183960999908 ) ) ;
#24712 = CARTESIAN_POINT ( 'NONE',  ( 10.24845588172999911, -4.234132110154000372, -5.660862927546999934 ) ) ;
#24713 = LINE ( 'NONE', #46037, #13846 ) ;
#24714 = CARTESIAN_POINT ( 'NONE',  ( 23.58679329660199997, 13.29300756424000163, 4.188721108045000641 ) ) ;
#24715 = VERTEX_POINT ( 'NONE', #38556 ) ;
#24716 = CARTESIAN_POINT ( 'NONE',  ( 10.89918582084299992, -4.746348444722899629, 8.362701637490498996 ) ) ;
#24717 = CARTESIAN_POINT ( 'NONE',  ( 9.509901345851000443, 5.077442745148000647, 8.469003100811999474 ) ) ;
#24718 = CARTESIAN_POINT ( 'NONE',  ( 15.83043922992600017, 9.441080823466998950, 8.288885697152998944 ) ) ;
#24719 = EDGE_CURVE ( 'NONE', #61548, #63587, #33198, .T. ) ;
#24720 = CARTESIAN_POINT ( 'NONE',  ( 8.143316940379001778, -5.061720701958000390, 5.824087910811999613 ) ) ;
#24722 = CARTESIAN_POINT ( 'NONE',  ( 12.80505043854143388, 3.248109929747637015, -13.61799478206225444 ) ) ;
#24721 = CARTESIAN_POINT ( 'NONE',  ( 9.691082467489000152, 5.335647408863999352, 8.701220655673999715 ) ) ;
#24723 = CARTESIAN_POINT ( 'NONE',  ( 10.20641772631199906, 4.431553727090300043, -8.388315195900499788 ) ) ;
#24724 = CARTESIAN_POINT ( 'NONE',  ( 5.500000000000000000, 0.000000000000000000, 0.000000000000000000 ) ) ;
#24725 = CARTESIAN_POINT ( 'NONE',  ( 9.781659112603998452, 3.563556310301200014, -8.404632083253700259 ) ) ;
#24726 = CARTESIAN_POINT ( 'NONE',  ( 17.97714073376501531, -0.5849390254007678092, 12.58641711472857594 ) ) ;
#24727 = CARTESIAN_POINT ( 'NONE',  ( 11.57299956498156845, -2.792989229543000107, -7.825000000000000178 ) ) ;
#24728 = VECTOR ( 'NONE', #34692, 1000.000000000000000 ) ;
#24729 = CARTESIAN_POINT ( 'NONE',  ( 10.84657802013509986, 2.684088780794000151, 7.530633716161349689 ) ) ;
#24730 = CARTESIAN_POINT ( 'NONE',  ( 23.61813716456500245, 10.28283487008000030, 9.267309039017000316 ) ) ;
#24731 = ORIENTED_EDGE ( 'NONE', *, *, #25485, .T. ) ;
#24732 = CARTESIAN_POINT ( 'NONE',  ( 9.143918146793000190, -5.791549888895000109, 7.752110689268000954 ) ) ;
#24733 = DIRECTION ( 'NONE',  ( -5.668025694556021242E-06, 0.2588381829991006078, -0.9659206980853023428 ) ) ;
#24734 = CARTESIAN_POINT ( 'NONE',  ( 7.827987191645501497, -4.479149983889610276, 6.206347837179650995 ) ) ;
#24735 = CARTESIAN_POINT ( 'NONE',  ( 10.29522949779699914, 4.480999174483200065, 6.778648208007999720 ) ) ;
#24736 = ORIENTED_EDGE ( 'NONE', *, *, #67774, .F. ) ;
#24737 = CARTESIAN_POINT ( 'NONE',  ( 8.577614158774000686, 3.981661882377999895, 8.959227447876999761 ) ) ;
#24739 = CARTESIAN_POINT ( 'NONE',  ( 11.10612378248509913, 3.517039242046199998, 8.413720204863100349 ) ) ;
#24738 = CARTESIAN_POINT ( 'NONE',  ( 10.26788779216199821, -3.070969952137800441, -7.835030859477799758 ) ) ;
#24740 = VECTOR ( 'NONE', #62432, 1000.000000000000114 ) ;
#24741 = CARTESIAN_POINT ( 'NONE',  ( 10.56170778040999991, 5.057487376164999660, -8.595710652231000282 ) ) ;
#24742 = EDGE_LOOP ( 'NONE', ( #56549, #16910, #37975, #19444, #61976 ) ) ;
#24743 = CARTESIAN_POINT ( 'NONE',  ( 24.44496483130000186, -3.224879855413000040, 12.03535978074999946 ) ) ;
#24744 = CARTESIAN_POINT ( 'NONE',  ( 17.57920672810400831, -3.248146558128260697, -13.61798601073640747 ) ) ;
#24745 = CARTESIAN_POINT ( 'NONE',  ( 10.23103300763299828, 4.692441239783899931, 6.773725604892799623 ) ) ;
#24746 = ADVANCED_FACE ( 'NONE', ( #65462 ), #23166, .F. ) ;
#24747 = CARTESIAN_POINT ( 'NONE',  ( 24.62769666311906036, 8.773247286767267283, -9.203857928692515955 ) ) ;
#24748 = CARTESIAN_POINT ( 'NONE',  ( 11.09999999999999964, -5.299999998684000069, -5.146420581040999309 ) ) ;
#24749 = ORIENTED_EDGE ( 'NONE', *, *, #16130, .T. ) ;
#24750 = CARTESIAN_POINT ( 'NONE',  ( 11.26489721861000248, -3.710193004830000252, 11.71182445734000055 ) ) ;
#24751 = CARTESIAN_POINT ( 'NONE',  ( 7.517164158767000615, 2.455281733534999677, -8.606072783617999988 ) ) ;
#24752 = CARTESIAN_POINT ( 'NONE',  ( 8.218889947459839362, -5.685407169154115259, 7.929140997506675781 ) ) ;
#24753 = CARTESIAN_POINT ( 'NONE',  ( 10.88813259637009878, -5.155817667926999803, -8.129798612793599943 ) ) ;
#24754 = CARTESIAN_POINT ( 'NONE',  ( 10.23195058442700045, -3.492264136285500253, 8.674133161175999973 ) ) ;
#24755 = ORIENTED_EDGE ( 'NONE', *, *, #3297, .T. ) ;
#24756 = CARTESIAN_POINT ( 'NONE',  ( 10.49744223918999886, -4.907449962201999583, -5.047071811637001026 ) ) ;
#24757 = CARTESIAN_POINT ( 'NONE',  ( 10.99349279008999858, -4.332388355267299929, 6.265968249244999733 ) ) ;
#24758 = ORIENTED_EDGE ( 'NONE', *, *, #48697, .T. ) ;
#24759 = CARTESIAN_POINT ( 'NONE',  ( 9.518359312502500558, 5.126777126186113698, -6.752018918873279318 ) ) ;
#24760 = VERTEX_POINT ( 'NONE', #22126 ) ;
#24761 = CARTESIAN_POINT ( 'NONE',  ( 9.485142521132999605, -3.025808284870999731, -9.100010361367001366 ) ) ;
#24762 = CARTESIAN_POINT ( 'NONE',  ( 10.90054769436000015, -2.705757430156999988, -4.902711565806999516 ) ) ;
#24763 = B_SPLINE_CURVE_WITH_KNOTS ( 'NONE', 3,
 ( #19047, #2625, #57136, #35485 ),
 .UNSPECIFIED., .F., .F.,
 ( 4, 4 ),
 ( 0.000000000000000000, 1.000000000000000000 ),
 .UNSPECIFIED. ) ;
#24764 = CARTESIAN_POINT ( 'NONE',  ( 11.34523293495530005, 2.684794526488000432, -7.447129085684729866 ) ) ;
#24765 = CARTESIAN_POINT ( 'NONE',  ( 11.76212378248530044, -4.615095948180499619, 8.663708617168998316 ) ) ;
#24766 = CARTESIAN_POINT ( 'NONE',  ( 12.33348197901552901, 2.910306952023486549, -12.34646687328217141 ) ) ;
#24767 = CARTESIAN_POINT ( 'NONE',  ( 11.78533594839949927, -3.249987070165300196, 8.359517726022600570 ) ) ;
#24768 = CARTESIAN_POINT ( 'NONE',  ( 7.218295280410000458, 4.773081973066999772, 8.927402469597002010 ) ) ;
#24769 = ORIENTED_EDGE ( 'NONE', *, *, #28627, .T. ) ;
#24770 = CARTESIAN_POINT ( 'NONE',  ( 7.681946225801584482, 2.830976189063534321, 8.204262802077490591 ) ) ;
#24771 = AXIS2_PLACEMENT_3D ( 'NONE', #12376, #33362, #34405 ) ;
#24772 = CARTESIAN_POINT ( 'NONE',  ( 9.497293146791999874, -3.734278838175999482, 8.942129638874000364 ) ) ;
#24773 = CARTESIAN_POINT ( 'NONE',  ( 9.864763540183249191, 2.782534154164605589, 7.172815144550902744 ) ) ;
#24774 = ORIENTED_EDGE ( 'NONE', *, *, #43256, .F. ) ;
#24775 = CARTESIAN_POINT ( 'NONE',  ( 12.15765997487498140, -2.156065442695497048, -12.41416509552196956 ) ) ;
#24776 = CARTESIAN_POINT ( 'NONE',  ( 11.15810538575740019, 5.242981041160000188, 7.797177576385699638 ) ) ;
#24777 = CARTESIAN_POINT ( 'NONE',  ( 11.20536814679000059, -2.688541832249000230, -8.273932507170000505 ) ) ;
#24778 = CYLINDRICAL_SURFACE ( 'NONE', #13194, 0.5000000000000004441 ) ;
#24779 = CARTESIAN_POINT ( 'NONE',  ( 18.26005557146100244, -2.925549590147000334, -11.93525498079000080 ) ) ;
#24780 = CARTESIAN_POINT ( 'NONE',  ( 24.25375554908000097, -8.963946465867000057, 8.909846166044999904 ) ) ;
#24781 = CARTESIAN_POINT ( 'NONE',  ( 12.24262961005306849, -2.226644062380152445, -13.72761226533214618 ) ) ;
#24782 = FACE_OUTER_BOUND ( 'NONE', #54424, .T. ) ;
#24783 = CARTESIAN_POINT ( 'NONE',  ( 10.19810941423799910, -3.053977294209000437, -6.640722727400100389 ) ) ;
#24784 = EDGE_CURVE ( 'NONE', #49271, #35912, #53250, .T. ) ;
#24786 = EDGE_CURVE ( 'NONE', #52595, #19719, #8382, .T. ) ;
#24785 = CARTESIAN_POINT ( 'NONE',  ( 11.02038275177999971, 5.599999999999999645, -6.571291218949999902 ) ) ;
#24787 = VERTEX_POINT ( 'NONE', #54641 ) ;
#24788 = VERTEX_POINT ( 'NONE', #6734 ) ;
#24789 = CARTESIAN_POINT ( 'NONE',  ( 10.91949602487000170, -5.247971730353000019, 4.977236201457000853 ) ) ;
#24790 = AXIS2_PLACEMENT_3D ( 'NONE', #23076, #17495, #7342 ) ;
#24791 = CARTESIAN_POINT ( 'NONE',  ( 8.571413182548997867, -4.600000000000999734, 5.927302706106000407 ) ) ;
#24792 = CARTESIAN_POINT ( 'NONE',  ( 17.55505043854143565, 3.125000000000000000, 13.52078605991414939 ) ) ;
#24793 = CARTESIAN_POINT ( 'NONE',  ( 10.65649893244999902, 5.448184228579000532, -7.015214795518000201 ) ) ;
#24794 = CARTESIAN_POINT ( 'NONE',  ( 15.90000000000000036, 0.000000000000000000, 0.000000000000000000 ) ) ;
#24795 = CARTESIAN_POINT ( 'NONE',  ( 17.83408408707288473, 3.059349868707512687, 12.30347716376230416 ) ) ;
#24796 = VECTOR ( 'NONE', #28152, 1000.000000000000000 ) ;
#24797 = CARTESIAN_POINT ( 'NONE',  ( 25.46375345652300126, 2.879422156700999658, -11.30951020355999859 ) ) ;
#24798 = CARTESIAN_POINT ( 'NONE',  ( 10.46932803217000085, 4.988495740890000363, 6.213106455073000411 ) ) ;
#24799 = CARTESIAN_POINT ( 'NONE',  ( 11.57299956498156845, -2.792989229543000107, -7.825000000000000178 ) ) ;
#24800 = VERTEX_POINT ( 'NONE', #44166 ) ;
#24801 = CARTESIAN_POINT ( 'NONE',  ( 12.28874679351410215, -2.147634260983757315, 12.52674262693622609 ) ) ;
#24802 = CARTESIAN_POINT ( 'NONE',  ( 9.247734463322998977, -3.909687748588960066, -8.362294405496898619 ) ) ;
#24803 = B_SPLINE_CURVE_WITH_KNOTS ( 'NONE', 3,
 ( #17271, #13076, #34057, #2237, #34407, #55723, #12377, #45235, #23551, #38955 ),
 .UNSPECIFIED., .F., .F.,
 ( 4, 2, 2, 2, 4 ),
 ( 0.5000000000000011102, 0.6250000000000008882, 0.7500000000000005551, 0.8750000000000002220, 1.000000000000000000 ),
 .UNSPECIFIED. ) ;
#24804 = CARTESIAN_POINT ( 'NONE',  ( 10.68362359175999998, 2.603561947343000060, 7.762063351517999976 ) ) ;
#24805 = EDGE_CURVE ( 'NONE', #11166, #24880, #46565, .T. ) ;
#24806 = CARTESIAN_POINT ( 'NONE',  ( 10.93614141025500075, -3.450366949021700158, 6.521048559232099251 ) ) ;
#24807 = CARTESIAN_POINT ( 'NONE',  ( 8.548770280408998445, 5.203550244299999683, -8.391678825488000371 ) ) ;
#24808 = EDGE_CURVE ( 'NONE', #54071, #13468, #43423, .T. ) ;
#24809 = CARTESIAN_POINT ( 'NONE',  ( 10.56733863405299800, 4.788475529394700558, -8.505794571537999005 ) ) ;
#24810 = CARTESIAN_POINT ( 'NONE',  ( 12.66323998097240278, 0.6090396975623076914, 12.68033511803395363 ) ) ;
#24811 = CARTESIAN_POINT ( 'NONE',  ( 8.353301658773000682, 2.800103557244999930, 9.079946116129001155 ) ) ;
#24812 = CARTESIAN_POINT ( 'NONE',  ( 10.55991859298999991, 5.094266430778000121, 6.075406703384000018 ) ) ;
#24813 = CARTESIAN_POINT ( 'NONE',  ( 12.57288091590946166, 1.919630123611446360, 12.56800073041603483 ) ) ;
#24814 = ORIENTED_EDGE ( 'NONE', *, *, #36528, .F. ) ;
#24815 = CARTESIAN_POINT ( 'NONE',  ( 9.526695280414001488, 5.462898983065000102, -8.055936939571999744 ) ) ;
#24816 = CARTESIAN_POINT ( 'NONE',  ( 10.05862282008599884, 4.666276081381299790, -8.574682153725998290 ) ) ;
#24817 = CARTESIAN_POINT ( 'NONE',  ( 10.70424414268935287, -5.750615589152155316, 7.605733149126583825 ) ) ;
#24819 = CARTESIAN_POINT ( 'NONE',  ( 10.29184687351566652, 3.000416447002276943, 8.268183399968645375 ) ) ;
#24818 = CARTESIAN_POINT ( 'NONE',  ( 9.266941940380000631, -3.049610585291000042, 6.392533570808999421 ) ) ;
#24820 = CARTESIAN_POINT ( 'NONE',  ( 7.099999886593999499, 1.243449787579999883E-13, -12.39999890530017446 ) ) ;
#24821 = CARTESIAN_POINT ( 'NONE',  ( 10.50180110216399854, -4.856393875115199599, -6.976989117212499814 ) ) ;
#24822 = EDGE_LOOP ( 'NONE', ( #38420, #48950, #55211, #16404 ) ) ;
#24823 = AXIS2_PLACEMENT_3D ( 'NONE', #38856, #64706, #27674 ) ;
#24824 = CARTESIAN_POINT ( 'NONE',  ( 1.868110514233000119, -1.438367618452000007, -3.472675606904999768 ) ) ;
#24825 = CARTESIAN_POINT ( 'NONE',  ( 21.00000012402660232, -1.355091984497000173E-13, 1.088018564133000035E-14 ) ) ;
#24827 = CARTESIAN_POINT ( 'NONE',  ( 13.99967273502900156, -9.525279043350998620, -8.192384979499998110 ) ) ;
#24826 = CARTESIAN_POINT ( 'NONE',  ( 9.617764158771999305, 5.322769172805999816, -7.951018786192998178 ) ) ;
#24828 = CARTESIAN_POINT ( 'NONE',  ( 10.77164068750943393, 2.873222873819646583, 6.752018918863353925 ) ) ;
#24829 = DIRECTION ( 'NONE',  ( 0.000000000000000000, 1.000000000000000000, 0.000000000000000000 ) ) ;
#24830 = CARTESIAN_POINT ( 'NONE',  ( 15.71007343404014200, 8.769519461636436475, 7.669310999670703843 ) ) ;
#24831 = CYLINDRICAL_SURFACE ( 'NONE', #67680, 12.59999999999999964 ) ;
#24832 = CARTESIAN_POINT ( 'NONE',  ( 24.68357798603522113, -11.80735008096011285, 3.191230140235593371 ) ) ;
#24833 = CARTESIAN_POINT ( 'NONE',  ( 7.410855646792000151, -2.302293129340000188, 6.875167727519000849 ) ) ;
#24834 = ORIENTED_EDGE ( 'NONE', *, *, #59699, .F. ) ;
#24835 = CARTESIAN_POINT ( 'NONE',  ( 8.598670280411999656, 2.376526778640999815, 7.686980884243000745 ) ) ;
#24837 = CARTESIAN_POINT ( 'NONE',  ( 13.12913653430045002, -11.69120254989815599, -1.923246422712994397 ) ) ;
#24836 = CARTESIAN_POINT ( 'NONE',  ( 5.296676530072999434, -0.1174666901181000006, -1.463806399069999875 ) ) ;
#24838 = CARTESIAN_POINT ( 'NONE',  ( 18.12577783848187352, 2.244501219363363997, -13.72435250368102366 ) ) ;
#24839 = AXIS2_PLACEMENT_3D ( 'NONE', #44808, #8771, #61563 ) ;
#24840 = DIRECTION ( 'NONE',  ( 0.8231338744408063235, 0.000000000000000000, -0.5678473604306591982 ) ) ;
#24841 = CARTESIAN_POINT ( 'NONE',  ( 2.065900752180000133, 2.737733327009000295, -2.100062873276000275 ) ) ;
#24842 = ORIENTED_EDGE ( 'NONE', *, *, #4719, .F. ) ;
#24843 = CARTESIAN_POINT ( 'NONE',  ( 10.99999999997000089, 4.000000000000000000, -7.500000000000000000 ) ) ;
#24844 = CARTESIAN_POINT ( 'NONE',  ( 12.15871932425157098, -4.147141405561299621, 6.507377093516500288 ) ) ;
#24845 = CARTESIAN_POINT ( 'NONE',  ( 10.67745206237895417, -5.060860780720525476, 5.064629868885281105 ) ) ;
#24846 = CARTESIAN_POINT ( 'NONE',  ( 10.33536974457000035, 5.153692264686000613, 8.830864265869999841 ) ) ;
#24847 = CARTESIAN_POINT ( 'NONE',  ( 11.33872066707849768, 4.858611803369300652, 8.019361746728900897 ) ) ;
#24848 = CONICAL_SURFACE ( 'NONE', #12570, 0.9999998338055000602, 0.7853981908209605178 ) ;
#24849 = CARTESIAN_POINT ( 'NONE',  ( 24.04053350272573653, -3.344386409696779694, 12.67226691567676866 ) ) ;
#24850 = DIRECTION ( 'NONE',  ( -1.000000000000000000, 0.000000000000000000, 0.000000000000000000 ) ) ;
#24851 = CARTESIAN_POINT ( 'NONE',  ( 8.654006363155202664, -3.802134689411699853, 5.879617511049518797 ) ) ;
#24852 = CARTESIAN_POINT ( 'NONE',  ( 12.30233513030085035, -2.119611855452840032, 12.53231127769699782 ) ) ;
#24853 = CARTESIAN_POINT ( 'NONE',  ( 8.495025031241056013, 2.494743783266746284, 6.576609861288141623 ) ) ;
#24854 = VERTEX_POINT ( 'NONE', #51120 ) ;
#24855 = CARTESIAN_POINT ( 'NONE',  ( 18.05244152647599165, -3.049274110449837760, 13.66389386579125897 ) ) ;
#24856 = CARTESIAN_POINT ( 'NONE',  ( 15.40000000009400161, -8.833277835210999740, -7.896561221812000930 ) ) ;
#24857 = ORIENTED_EDGE ( 'NONE', *, *, #30699, .F. ) ;
#24858 = ORIENTED_EDGE ( 'NONE', *, *, #35668, .F. ) ;
#24859 = CARTESIAN_POINT ( 'NONE',  ( 8.766851002546001581, -2.832432432432000269, 6.822293592207000934 ) ) ;
#24860 = CARTESIAN_POINT ( 'NONE',  ( 17.80000000001300009, 3.351264566333000072, -11.15757590352999884 ) ) ;
#24861 = CARTESIAN_POINT ( 'NONE',  ( 11.21979841651039855, 3.695024856201900132, 6.689266534545799558 ) ) ;
#24862 = CARTESIAN_POINT ( 'NONE',  ( 10.22108913916999917, 2.983268757921999637, 8.764704075288999974 ) ) ;
#24863 = CARTESIAN_POINT ( 'NONE',  ( 9.662441121991999893, 4.824173073626999653, -8.517602418144999632 ) ) ;
#24864 = CARTESIAN_POINT ( 'NONE',  ( 9.100254395947628083, -4.850975458930337325, -7.296596368717002790 ) ) ;
#24865 = CARTESIAN_POINT ( 'NONE',  ( 9.736871746126999128, -2.742172332680000046, 6.839224809731999422 ) ) ;
#24866 = CARTESIAN_POINT ( 'NONE',  ( 18.10028187597348293, 0.4746736627229694583, -12.59106879393900513 ) ) ;
#24867 = CARTESIAN_POINT ( 'NONE',  ( 10.16989351219999982, -2.594225604561000154, -6.291264536816999708 ) ) ;
#24868 = CARTESIAN_POINT ( 'NONE',  ( 11.09672200990539892, -4.817867935977999672, -7.214709569664399247 ) ) ;
#24869 = EDGE_CURVE ( 'NONE', #43147, #38133, #42548, .T. ) ;
#24871 = ADVANCED_FACE ( 'NONE', ( #62623 ), #67873, .F. ) ;
#24870 = PLANE ( 'NONE',  #64590 ) ;
#24872 = ORIENTED_EDGE ( 'NONE', *, *, #56578, .T. ) ;
#24873 = CARTESIAN_POINT ( 'NONE',  ( 11.07071157029000119, -5.425561924405000624, -5.078387321380000152 ) ) ;
#24874 =( LENGTH_UNIT ( ) NAMED_UNIT ( * ) SI_UNIT ( .MILLI., .METRE. ) );
#24875 = CARTESIAN_POINT ( 'NONE',  ( 11.20596535229475776, -4.908912176279685013, -7.824984935920127782 ) ) ;
#24876 = CARTESIAN_POINT ( 'NONE',  ( 6.950330780312001799, 10.43291458946000461, 4.786367813216996225 ) ) ;
#24877 = CARTESIAN_POINT ( 'NONE',  ( 9.912329965421998068, 3.111510091554099855, -8.420309768537698858 ) ) ;
#24878 = CARTESIAN_POINT ( 'NONE',  ( 12.27297424062789588, 2.021448577728815366, 13.85330429709570943 ) ) ;
#24879 = CARTESIAN_POINT ( 'NONE',  ( 10.13340376756999994, -5.653635692335999607, 6.501829690795999817 ) ) ;
#24880 = VERTEX_POINT ( 'NONE', #24891 ) ;
#24881 = CARTESIAN_POINT ( 'NONE',  ( 12.18504239630149577, -0.08143391448655303011, -12.69966978411006053 ) ) ;
#24882 = CARTESIAN_POINT ( 'NONE',  ( 12.80505043854144276, -0.7302158263239079128, 13.98094363220831049 ) ) ;
#24883 = ORIENTED_EDGE ( 'NONE', *, *, #62314, .T. ) ;
#24884 = FACE_OUTER_BOUND ( 'NONE', #9249, .T. ) ;
#24885 = CARTESIAN_POINT ( 'NONE',  ( 12.80505043854144276, -0.6250000000000001110, 12.67928921589117586 ) ) ;
#24886 = CARTESIAN_POINT ( 'NONE',  ( 10.67726354018259727, -3.370476274536371442, -6.407767014557179230 ) ) ;
#24887 = CARTESIAN_POINT ( 'NONE',  ( 11.03057053952199951, -4.340412141385700195, 8.296503712697200328 ) ) ;
#24888 = CIRCLE ( 'NONE', #39411, 1.000000000000000222 ) ;
#24889 = EDGE_CURVE ( 'NONE', #42930, #36918, #41317, .T. ) ;
#24890 = CARTESIAN_POINT ( 'NONE',  ( 23.60000000000000142, 10.96648613208696688, -8.588734463056562518 ) ) ;
#24891 = CARTESIAN_POINT ( 'NONE',  ( 7.307500000000000107, -0.2500000000000000000, 3.149999999999999911 ) ) ;
#24892 = CARTESIAN_POINT ( 'NONE',  ( 7.000000000000000000, -7.526486366024999874, -3.526486366024999874 ) ) ;
#24893 = CARTESIAN_POINT ( 'NONE',  ( 10.47145237372899906, -3.956267952212243255, -8.774080944853650976 ) ) ;
#24894 = CARTESIAN_POINT ( 'NONE',  ( 17.80000000009400196, -3.216307036143000175, 11.40341376487999980 ) ) ;
#24895 = CARTESIAN_POINT ( 'NONE',  ( 10.84641504065830020, 4.804462279649600376, -6.900173947321999179 ) ) ;
#24896 = LINE ( 'NONE', #4246, #9040 ) ;
#24897 = CARTESIAN_POINT ( 'NONE',  ( 10.68342665876999931, 3.810131921595000026, -5.661115150006999386 ) ) ;
#24898 = CARTESIAN_POINT ( 'NONE',  ( 9.936596320338999533, 2.942832934044000037, -7.068569539041399175 ) ) ;
#24900 = CARTESIAN_POINT ( 'NONE',  ( 12.19038559396453003, 2.613250548423018405, 12.42445786899044791 ) ) ;
#24899 = CARTESIAN_POINT ( 'NONE',  ( 16.13959992722299930, -8.325816698831998153, -8.094004264449001340 ) ) ;
#24901 = CARTESIAN_POINT ( 'NONE',  ( 23.56734670131549336, -13.32877617996445352, 4.249149195638875831 ) ) ;
#24902 = VERTEX_POINT ( 'NONE', #8812 ) ;
#24903 = DIRECTION ( 'NONE',  ( 0.000000000000000000, -0.7198977633595244896, -0.6940801180771238865 ) ) ;
#24904 = CARTESIAN_POINT ( 'NONE',  ( 9.383549168937532770, 5.519605098629036810, -8.419222652796641171 ) ) ;
#24905 = CARTESIAN_POINT ( 'NONE',  ( 10.23758376188599861, 3.152987476450699766, 6.960174024681499816 ) ) ;
#24906 = CARTESIAN_POINT ( 'NONE',  ( 9.302887573405627109, 4.590576684156811638, -8.145562893180322561 ) ) ;
#24907 = LINE ( 'NONE', #40989, #41037 ) ;
#24908 = FACE_OUTER_BOUND ( 'NONE', #37571, .T. ) ;
#24909 = CARTESIAN_POINT ( 'NONE',  ( 9.384624721950221016, -2.899999999999999911, 6.445686799063069294 ) ) ;
#24910 = ORIENTED_EDGE ( 'NONE', *, *, #40926, .T. ) ;
#24911 = CARTESIAN_POINT ( 'NONE',  ( 9.455342523874998406, -5.128664655368000425, -7.327226901081999699 ) ) ;
#24912 = VECTOR ( 'NONE', #66420, 1000.000000000000000 ) ;
#24913 = FACE_OUTER_BOUND ( 'NONE', #46459, .T. ) ;
#24914 = CARTESIAN_POINT ( 'NONE',  ( 12.18788784977535933, -4.985985832792199979, 7.556342205905759890 ) ) ;
#24915 = PRODUCT_DEFINITION_SHAPE ( 'NONE', 'NONE',  #50496 ) ;
#24916 = CARTESIAN_POINT ( 'NONE',  ( 17.98134286629677092, 1.897806848213327457, -12.45626380386397791 ) ) ;
#24917 = CARTESIAN_POINT ( 'NONE',  ( 2.500973465876000112, 3.500000000000000000, 0.000000000000000000 ) ) ;
#24918 = CARTESIAN_POINT ( 'NONE',  ( 24.43232361759900328, -3.176382763002000509, 12.00226528444000174 ) ) ;
#24919 = EDGE_CURVE ( 'NONE', #47463, #20699, #23108, .T. ) ;
#24920 = ADVANCED_FACE ( 'NONE', ( #24200 ), #49621, .F. ) ;
#24921 = CARTESIAN_POINT ( 'NONE',  ( 12.19034750719933236, 2.613044105544683582, -13.64883414298571296 ) ) ;
#24922 = CARTESIAN_POINT ( 'NONE',  ( 9.438732219486000830, -2.462132291381999849, -7.373611177161000008 ) ) ;
#24923 = CARTESIAN_POINT ( 'NONE',  ( 10.26947109217999810, -5.100000000000000533, -6.152188490330000370 ) ) ;
#24924 = DIRECTION ( 'NONE',  ( 0.7071149608238868067, -0.7070986014545870280, -9.105180035418829085E-10 ) ) ;
#24925 = CARTESIAN_POINT ( 'NONE',  ( 12.11831821888144844, 0.2353130933619010101, -13.99804086085458898 ) ) ;
#24926 = CARTESIAN_POINT ( 'NONE',  ( 10.72510394928502286, 2.650147065043140238, 7.500007457243191844 ) ) ;
#24927 = CARTESIAN_POINT ( 'NONE',  ( 12.80505043854144276, -0.6250000000000001110, -25.00000000000000000 ) ) ;
#24928 = CARTESIAN_POINT ( 'NONE',  ( 18.14750831224828431, 2.299919532987898751, 12.49594326304257486 ) ) ;
#24929 = CARTESIAN_POINT ( 'NONE',  ( 23.59999467231800097, -10.30760443253999981, -9.317695455237998914 ) ) ;
#24931 = AXIS2_PLACEMENT_3D ( 'NONE', #40864, #62187, #14307 ) ;
#24930 = LINE ( 'NONE', #36108, #39612 ) ;
#24932 = ORIENTED_EDGE ( 'NONE', *, *, #13546, .T. ) ;
#24933 = CARTESIAN_POINT ( 'NONE',  ( 4.000000000000000000, -1.321078631445433471, 1.719326598155805463 ) ) ;
#24934 = CARTESIAN_POINT ( 'NONE',  ( 18.14661026972999736, 2.095745652224534794, -13.84225217829565580 ) ) ;
#24935 = EDGE_LOOP ( 'NONE', ( #17649, #45693, #19510, #65028, #8622, #68649, #32048 ) ) ;
#24936 = CARTESIAN_POINT ( 'NONE',  ( 10.31397570133299979, -3.363922674822000136, 6.910836541441499392 ) ) ;
#24937 = CYLINDRICAL_SURFACE ( 'NONE', #24591, 1.350000000000000089 ) ;
#24939 = CARTESIAN_POINT ( 'NONE',  ( 17.80000000001300009, 3.351264566333000072, -11.15757590352999884 ) ) ;
#24938 = AXIS2_PLACEMENT_3D ( 'NONE', #50159, #39321, #41639 ) ;
#24940 = CARTESIAN_POINT ( 'NONE',  ( 9.764472292182821533, 3.575760007354200187, -8.840577379916510381 ) ) ;
#24941 = CARTESIAN_POINT ( 'NONE',  ( 11.39189666366029918, -4.052152326617509459, -8.673729056199000809 ) ) ;
#24942 = CARTESIAN_POINT ( 'NONE',  ( 11.09999999999999964, -2.649999999999999911, -7.500000000000000000 ) ) ;
#24943 = CARTESIAN_POINT ( 'NONE',  ( 5.013359839683332986, -1.310679582531389276, 0.7554284705563443225 ) ) ;
#24944 = VERTEX_POINT ( 'NONE', #38 ) ;
#24945 = CARTESIAN_POINT ( 'NONE',  ( 25.30000327618300204, 1.393126554761430436, -11.43653827017141111 ) ) ;
#24946 = CARTESIAN_POINT ( 'NONE',  ( 8.733215486276282746, 4.027942412209718270, -8.383215533252753815 ) ) ;
#24948 = EDGE_CURVE ( 'NONE', #22779, #47838, #26271, .T. ) ;
#24947 = CARTESIAN_POINT ( 'NONE',  ( 9.825045280412000537, 3.116293075258000478, -6.208411413796000033 ) ) ;
#24949 = ORIENTED_EDGE ( 'NONE', *, *, #14370, .T. ) ;
#24950 = CARTESIAN_POINT ( 'NONE',  ( 10.83768005408999890, 5.758100475276000552, -6.911469147650000977 ) ) ;
#24951 = EDGE_CURVE ( 'NONE', #25295, #24276, #30913, .T. ) ;
#24952 = ORIENTED_EDGE ( 'NONE', *, *, #52036, .T. ) ;
#24953 = CARTESIAN_POINT ( 'NONE',  ( 9.657975701332999208, 4.837683410033799980, 6.724099908144899551 ) ) ;
#24954 = CARTESIAN_POINT ( 'NONE',  ( 17.74302412089502567, -1.903914349118853488, -12.57063651914289792 ) ) ;
#24955 = CARTESIAN_POINT ( 'NONE',  ( 8.734814475091132735, -3.943962993865710587, -8.383485082298649971 ) ) ;
#24956 = B_SPLINE_CURVE_WITH_KNOTS ( 'NONE', 3,
 ( #12183, #6231, #54829, #11478 ),
 .UNSPECIFIED., .F., .F.,
 ( 4, 4 ),
 ( 0.000000000000000000, 1.000000000000000000 ),
 .UNSPECIFIED. ) ;
#24957 = CARTESIAN_POINT ( 'NONE',  ( 24.43231275843400141, -11.98247113617999915, -3.250307990934000024 ) ) ;
#24958 = B_SPLINE_CURVE_WITH_KNOTS ( 'NONE', 3,
 ( #48650, #9864, #32240, #16483, #752, #64021, #58107, #64709 ),
 .UNSPECIFIED., .F., .F.,
 ( 4, 2, 2, 4 ),
 ( 0.000000000000000000, 0.5000000000000045519, 0.7500000000000022204, 1.000000000000000000 ),
 .UNSPECIFIED. ) ;
#24959 = CARTESIAN_POINT ( 'NONE',  ( 25.55262180961353380, 2.866482437163034636, 11.19816644711434606 ) ) ;
#24960 = ORIENTED_EDGE ( 'NONE', *, *, #20355, .T. ) ;
#24961 = CARTESIAN_POINT ( 'NONE',  ( 11.43028911132391556, 2.855999340945334808, 6.940988051967042161 ) ) ;
#24962 = CARTESIAN_POINT ( 'NONE',  ( 10.72802334123000101, 3.751278653658999929, -8.836901076820000256 ) ) ;
#24963 = CARTESIAN_POINT ( 'NONE',  ( 9.961660622463165637, -5.351629337096486694, 7.263483964539670268 ) ) ;
#24964 = CARTESIAN_POINT ( 'NONE',  ( 12.17655141950252329, 2.882034090924098457, -13.70014555608276119 ) ) ;
#24965 = VECTOR ( 'NONE', #53768, 1000.000000000000227 ) ;
#24966 = EDGE_CURVE ( 'NONE', #7034, #129, #52836, .T. ) ;
#24967 = CARTESIAN_POINT ( 'NONE',  ( 18.27863135987957222, -0.04720351400548002813, 13.99992551180917388 ) ) ;
#24968 = CARTESIAN_POINT ( 'NONE',  ( 10.06493315628555862, -5.349942305088194239, -7.500003965376651038 ) ) ;
#24969 = CARTESIAN_POINT ( 'NONE',  ( 10.60519595724999853, -5.343977295764999802, -7.731524081231999190 ) ) ;
#24970 = ORIENTED_EDGE ( 'NONE', *, *, #38370, .F. ) ;
#24971 = EDGE_LOOP ( 'NONE', ( #2672, #56099, #32024, #13877, #1689 ) ) ;
#24972 = CARTESIAN_POINT ( 'NONE',  ( 8.458179719589999479, 5.332332124071999857, -8.487089944253000340 ) ) ;
#24973 = DIRECTION ( 'NONE',  ( 0.000000000000000000, 0.000000000000000000, 1.000000000000000000 ) ) ;
#24974 = CARTESIAN_POINT ( 'NONE',  ( 12.18026105735682663, -2.480641341388361454, 13.67754910898214149 ) ) ;
#24975 = LINE ( 'NONE', #25661, #43983 ) ;
#24976 = CARTESIAN_POINT ( 'NONE',  ( 23.55381026917600096, 10.32939677816000135, -9.498137881527000559 ) ) ;
#24977 = CARTESIAN_POINT ( 'NONE',  ( 18.18404792230800382, -3.205001206845999651, -11.25648540289999922 ) ) ;
#24979 = FACE_BOUND ( 'NONE', #43790, .T. ) ;
#24978 = CARTESIAN_POINT ( 'NONE',  ( 10.00505105205199818, -2.879444846832000415, 7.280704316743199733 ) ) ;
#24980 = AXIS2_PLACEMENT_3D ( 'NONE', #46337, #19068, #67298 ) ;
#24981 = CARTESIAN_POINT ( 'NONE',  ( 8.248511556582998949, -4.520635131647999572, -6.809650021909999573 ) ) ;
#24982 = ORIENTED_EDGE ( 'NONE', *, *, #17439, .F. ) ;
#24983 = DIRECTION ( 'NONE',  ( 0.000000000000000000, -1.000000000000000000, 0.000000000000000000 ) ) ;
#24984 = CIRCLE ( 'NONE', #33929, 0.2000000000000009270 ) ;
#24985 = CARTESIAN_POINT ( 'NONE',  ( 10.49202233201000034, -3.034490706411000271, -4.914423043680000269 ) ) ;
#24986 = CARTESIAN_POINT ( 'NONE',  ( 9.443723707566000769, -5.531435376468999188, -8.256621485025000595 ) ) ;
#24987 = CARTESIAN_POINT ( 'NONE',  ( 10.98768472639999949, 5.139096889661000311, -4.945212061661000469 ) ) ;
#24988 = DIRECTION ( 'NONE',  ( 0.000000000000000000, -1.000000000000000000, 0.000000000000000000 ) ) ;
#24989 = CARTESIAN_POINT ( 'NONE',  ( 11.59999999999999964, -4.000000000000000000, -7.500000000000000000 ) ) ;
#24990 = CARTESIAN_POINT ( 'NONE',  ( 9.790085841230000696, 5.149303692842000402, -5.987168472229000393 ) ) ;
#24991 =( BOUNDED_SURFACE ( )  B_SPLINE_SURFACE ( 3, 3, ( 
 ( #23843, #39580, #35377, #24186, #56698, #7412, #28761, #45523, #60904, #66832 ),
 ( #62945, #4918, #25905, #15422, #41641, #4569, #52123, #46891, #47236, #21007 ),
 ( #68539, #36747, #41987, #10508, #63294, #9132, #40955, #24876, #52822, #20660 ),
 ( #51785, #42343, #63642, #58068, #19634, #10171, #35715, #3882, #68195, #36396 ) ),
 .UNSPECIFIED., .F., .F., .T. ) 
 B_SPLINE_SURFACE_WITH_KNOTS ( ( 4, 4 ),
 ( 4, 1, 1, 1, 1, 1, 1, 4 ),
 ( 0.000000000000000000, 1.000000000000000000 ),
 ( 0.2001824097869999985, 0.2006924593532999901, 0.2158499230326000051, 0.2291387176639999856, 0.2408062938197000069, 0.2510851730549999994, 0.2605211562811999837, 0.2678345471516999643 ),
 .UNSPECIFIED. ) 
 GEOMETRIC_REPRESENTATION_ITEM ( )  RATIONAL_B_SPLINE_SURFACE ( (
 ( 1.325324361584000021, 1.325324361584000021, 1.325324361584000021, 1.325324361584000021, 1.325324361584000021, 1.325324361584000021, 1.325324361584000021, 1.325324361584000021, 1.325324361584000021, 1.325324361584000021),
 ( 0.8915585461385999722, 0.8915585461385999722, 0.8915585461385999722, 0.8915585461385999722, 0.8915585461385999722, 0.8915585461385999722, 0.8915585461385999722, 0.8915585461385999722, 0.8915585461385999722, 0.8915585461385999722),
 ( 0.8915585461385999722, 0.8915585461385999722, 0.8915585461385999722, 0.8915585461385999722, 0.8915585461385999722, 0.8915585461385999722, 0.8915585461385999722, 0.8915585461385999722, 0.8915585461385999722, 0.8915585461385999722),
 ( 1.325324361584000021, 1.325324361584000021, 1.325324361584000021, 1.325324361584000021, 1.325324361584000021, 1.325324361584000021, 1.325324361584000021, 1.325324361584000021, 1.325324361584000021, 1.325324361584000021) ) ) 
 REPRESENTATION_ITEM ( '' )  SURFACE ( )  );
#24992 = DIRECTION ( 'NONE',  ( 0.000000000000000000, -0.7651299950380209269, 0.6438758348417170652 ) ) ;
#24993 = CARTESIAN_POINT ( 'NONE',  ( 8.164397154371004106, -4.665396042252996978, 6.167056685642003266 ) ) ;
#24994 = CARTESIAN_POINT ( 'NONE',  ( 6.160387840465999965, 0.6981053669911999604, 0.9464826977047000600 ) ) ;
#24995 = CARTESIAN_POINT ( 'NONE',  ( 0.1823164064783775740, 2.544165622319755293, -1.956281073432186712 ) ) ;
#24996 = CARTESIAN_POINT ( 'NONE',  ( 3.014883521226000340, -2.957936814457999830, 1.368172651669000039 ) ) ;
#24997 = ORIENTED_EDGE ( 'NONE', *, *, #33105, .T. ) ;
#24998 = EDGE_CURVE ( 'NONE', #11391, #21776, #68208, .T. ) ;
#24999 = EDGE_CURVE ( 'NONE', #23153, #20104, #36740, .T. ) ;
#25000 = CARTESIAN_POINT ( 'NONE',  ( 12.72331806630340978, -0.6199686954221036439, -12.67962180225518942 ) ) ;
#25001 = CARTESIAN_POINT ( 'NONE',  ( 12.34829947333263256, -2.926730327383867181, -12.34183739588157458 ) ) ;
#25002 = DIRECTION ( 'NONE',  ( 0.000000000000000000, 1.000000000000000000, 0.000000000000000000 ) ) ;
#25003 = CARTESIAN_POINT ( 'NONE',  ( 23.60000000000000142, 9.305479840184000651, 8.315530346521999405 ) ) ;
#25004 = DIRECTION ( 'NONE',  ( 0.000000000000000000, 1.000000000000000000, 0.000000000000000000 ) ) ;
#25005 = VERTEX_POINT ( 'NONE', #9834 ) ;
#25006 = CARTESIAN_POINT ( 'NONE',  ( 9.716851002543000604, 2.832432432432000269, 6.822293592207000934 ) ) ;
#25007 = ADVANCED_FACE ( 'NONE', ( #31182 ), #18960, .F. ) ;
#25008 = SHAPE_DEFINITION_REPRESENTATION ( #24915, #19687 ) ;
#25009 = CARTESIAN_POINT ( 'NONE',  ( 10.86501009699162701, 2.649983380500041008, -7.500000587580665901 ) ) ;
#25010 = CARTESIAN_POINT ( 'NONE',  ( 13.27439970770000066, -11.71097706365999969, -2.049245155247000127 ) ) ;
#25011 = CARTESIAN_POINT ( 'NONE',  ( 7.812760732415217291, 3.078855207953160367, 6.461200734285722724 ) ) ;
#25012 = CARTESIAN_POINT ( 'NONE',  ( 11.72433327354039889, 3.016779570871600313, -6.856888818507299810 ) ) ;
#25013 = EDGE_LOOP ( 'NONE', ( #30889, #61661, #63882, #2744, #30175 ) ) ;
#25014 = TOROIDAL_SURFACE ( 'NONE', #11571, 13.79999999999999893, 0.2000000000000000111 ) ;
#25015 = CARTESIAN_POINT ( 'NONE',  ( 10.81579453138999902, -5.374572909254000663, 6.698726302909000729 ) ) ;
#25016 = VERTEX_POINT ( 'NONE', #20248 ) ;
#25017 = CARTESIAN_POINT ( 'NONE',  ( 7.653716352205310436, -2.685215128838110310, 7.854066585618749485 ) ) ;
#25018 = CARTESIAN_POINT ( 'NONE',  ( 15.95563472374800185, 3.716697538693999991, 11.19594450203000058 ) ) ;
#25019 = CARTESIAN_POINT ( 'NONE',  ( 18.24178265820144773, -0.2353130933619061449, -13.99804086085459254 ) ) ;
#25020 = B_SPLINE_CURVE_WITH_KNOTS ( 'NONE', 3,
 ( #57332, #8421, #62242, #40572, #19943, #47202, #9099, #51749, #67478, #35343, #41264, #56659, #68503, #46858, #51069, #20626, #30106, #19245, #51409, #19599, #3505, #35684, #52088, #46170, #14359, #3172, #56997, #9784, #3843, #4192, #62915, #25181, #15036, #14698, #20281 ),
 .UNSPECIFIED., .F., .F.,
 ( 4, 1, 1, 1, 1, 1, 1, 1, 1, 1, 1, 1, 1, 1, 1, 1, 1, 1, 1, 1, 1, 1, 1, 1, 1, 1, 1, 1, 1, 1, 1, 1, 4 ),
 ( 0.000000000000000000, 0.01250527213657373973, 0.04500493301836113597, 0.07750459390014853567, 0.1100042547819059385, 0.1425039156636933313, 0.1750035765454807379, 0.2075032374272681168, 0.2400028983090555235, 0.2725025591908429856, 0.3050022200726303367, 0.3375018809544177989, 0.3700015418362051500, 0.4025012027179926122, 0.4350008635997799633, 0.4675005244815674255, 0.5000001853633546656, 0.5324998462451421277, 0.5649995071269294789, 0.5974991680087169410, 0.6299988288905042921, 0.6624984897722917543, 0.6949981506540791054, 0.7274978115358665676, 0.7599974724176539187, 0.7924971332994412698, 0.8249967941812287320, 0.8574964550630161941, 0.8899961159448035453, 0.9224957768265908964, 0.9549954377083782475, 0.9874950985901658207, 1.000000000000000000 ),
 .UNSPECIFIED. ) ;
#25021 = ORIENTED_EDGE ( 'NONE', *, *, #51778, .T. ) ;
#25022 = CARTESIAN_POINT ( 'NONE',  ( 23.64705884711741035, 10.02690164441486687, 9.685979275716718462 ) ) ;
#25023 = CARTESIAN_POINT ( 'NONE',  ( 7.716851002542999716, 2.832432432432000269, 6.822293592207000934 ) ) ;
#25024 = CARTESIAN_POINT ( 'NONE',  ( 7.681104719587999341, 5.564823112884000444, -7.478368060284999785 ) ) ;
#25025 = DIRECTION ( 'NONE',  ( 0.000000000000000000, -1.000000000000000000, 0.000000000000000000 ) ) ;
#25026 = CARTESIAN_POINT ( 'NONE',  ( 8.161249603540388975, -2.987768769759142629, 6.407057936808166154 ) ) ;
#25027 = ORIENTED_EDGE ( 'NONE', *, *, #67774, .T. ) ;
#25028 = CARTESIAN_POINT ( 'NONE',  ( 9.409308287954999628, -2.634700736117999931, 8.920302460802998823 ) ) ;
#25029 = CARTESIAN_POINT ( 'NONE',  ( 12.21057441424792422, -2.692955410772802871, -13.63058632108330137 ) ) ;
#25030 = CARTESIAN_POINT ( 'NONE',  ( 5.355026506350999860, 1.500000000000000000, 0.000000000000000000 ) ) ;
#25031 = CARTESIAN_POINT ( 'NONE',  ( 10.84088306584999906, -2.636277440143000472, -7.512643837511999934 ) ) ;
#25032 = CARTESIAN_POINT ( 'NONE',  ( 9.702862956261629535, -2.713451880143079809, 7.026479373627134706 ) ) ;
#25033 = VERTEX_POINT ( 'NONE', #57998 ) ;
#25034 = CARTESIAN_POINT ( 'NONE',  ( 24.13225289473700386, 12.49514845794176843, -3.369178721750599070 ) ) ;
#25035 = AXIS2_PLACEMENT_3D ( 'NONE', #55730, #34754, #34413 ) ;
#25036 = CARTESIAN_POINT ( 'NONE',  ( 5.177943173016958944, -0.9218200799623716968, -1.199500263597270910 ) ) ;
#25037 = CARTESIAN_POINT ( 'NONE',  ( 10.47530200610951034, -5.350262918594152595, 7.499984559551212904 ) ) ;
#25038 = CARTESIAN_POINT ( 'NONE',  ( 3.053056799210541072, 2.798833948393625537, 2.150913519912209360 ) ) ;
#25039 = CIRCLE ( 'NONE', #8280, 1.250000000000000666 ) ;
#25040 = CARTESIAN_POINT ( 'NONE',  ( 12.29698918160474186, 0.3645810575750328963, -13.89357890581303501 ) ) ;
#25041 = CARTESIAN_POINT ( 'NONE',  ( 18.14999129509867259, -2.691763112583330564, 12.40484894414121975 ) ) ;
#25042 = VERTEX_POINT ( 'NONE', #68130 ) ;
#25043 = CARTESIAN_POINT ( 'NONE',  ( 7.729221580034996819, -5.085115902530001897, 6.553339126910996626 ) ) ;
#25044 = ORIENTED_EDGE ( 'NONE', *, *, #6125, .F. ) ;
#25045 = CARTESIAN_POINT ( 'NONE',  ( 10.85069631730999973, 4.478098874537000285, 6.162039661770999821 ) ) ;
#25046 = CARTESIAN_POINT ( 'NONE',  ( 11.22823073745748168, -4.169674042210387732, -8.360328963510957223 ) ) ;
#25047 = CARTESIAN_POINT ( 'NONE',  ( 10.02394528041000044, 5.481267232667000222, -8.005061172455999241 ) ) ;
#25048 = CARTESIAN_POINT ( 'NONE',  ( 2.474755027877999947, 3.010559775858999920, -2.164644249678000509 ) ) ;
#25049 = CARTESIAN_POINT ( 'NONE',  ( 10.23643195768000069, -5.517145045299000294, -6.754127937316000363 ) ) ;
#25050 = EDGE_CURVE ( 'NONE', #34762, #62430, #19273, .T. ) ;
#25051 = CARTESIAN_POINT ( 'NONE',  ( 17.55505043854147118, -3.125000000000000000, 12.28374638332999780 ) ) ;
#25052 = CARTESIAN_POINT ( 'NONE',  ( 25.29987261391899978, -8.756202924575998026, 7.455126447192999883 ) ) ;
#25053 = ORIENTED_EDGE ( 'NONE', *, *, #41784, .T. ) ;
#25054 = ADVANCED_FACE ( 'NONE', ( #41574 ), #54398, .T. ) ;
#25055 = CARTESIAN_POINT ( 'NONE',  ( 11.53918313518939875, -4.707599264529200411, 6.605241151424599444 ) ) ;
#25056 = CARTESIAN_POINT ( 'NONE',  ( 10.64424812522415920, 2.623953476961054410, -6.377174817668581852 ) ) ;
#25057 = CARTESIAN_POINT ( 'NONE',  ( 15.86122879894100102, 8.802595411723000751, 8.571496522999998646 ) ) ;
#25058 = CARTESIAN_POINT ( 'NONE',  ( 7.694004440376999376, -5.850279024084999335, 6.784181137144999596 ) ) ;
#25060 = FACE_OUTER_BOUND ( 'NONE', #36950, .T. ) ;
#25059 = CARTESIAN_POINT ( 'NONE',  ( 9.786671076420999427, 2.381202181614999525, 7.612749448318000489 ) ) ;
#25061 = CARTESIAN_POINT ( 'NONE',  ( 10.87103032197929942, 4.583685623598699799, -6.683751296690399357 ) ) ;
#25062 = LINE ( 'NONE', #50609, #19088 ) ;
#25063 = CARTESIAN_POINT ( 'NONE',  ( 10.38955864497999926, 4.790758628877400227, -8.119307134446700047 ) ) ;
#25064 = CARTESIAN_POINT ( 'NONE',  ( 17.94855945389787166, 0.6042324041877016327, 12.58550538354983672 ) ) ;
#25065 = CARTESIAN_POINT ( 'NONE',  ( 25.30000327618300204, -10.83443035398000021, 3.855530949778000149 ) ) ;
#25066 = CARTESIAN_POINT ( 'NONE',  ( 9.523148997461001741, 5.167567567567999731, -6.822293592207000934 ) ) ;
#25067 = CARTESIAN_POINT ( 'NONE',  ( 23.73415186908400187, 9.844559812508000718, 9.786437184986999327 ) ) ;
#25068 = ORIENTED_EDGE ( 'NONE', *, *, #62365, .F. ) ;
#25069 = CARTESIAN_POINT ( 'NONE',  ( 7.807370559623000084, -3.650411072918999800, 6.083135626079000602 ) ) ;
#25070 = DIRECTION ( 'NONE',  ( 0.000000000000000000, 0.7158784314710769925, 0.6982249432342777506 ) ) ;
#25071 = CARTESIAN_POINT ( 'NONE',  ( 9.048601287889788125, 4.000000467705929985, 6.301404677806389465 ) ) ;
#25072 = CARTESIAN_POINT ( 'NONE',  ( 24.30001121497594596, -8.895961315773666556, -8.895961315773666556 ) ) ;
#25073 = VERTEX_POINT ( 'NONE', #14667 ) ;
#25074 = AXIS2_PLACEMENT_3D ( 'NONE', #55032, #49785, #2241 ) ;
#25075 = CARTESIAN_POINT ( 'NONE',  ( 18.31587707750999883, 3.089759977613000252, 11.98885651319999823 ) ) ;
#25076 = AXIS2_PLACEMENT_3D ( 'NONE', #50146, #60629, #12044 ) ;
#25077 = CARTESIAN_POINT ( 'NONE',  ( 10.80502344389999791, 2.874741265256000489, 8.182900850620900002 ) ) ;
#25078 = CARTESIAN_POINT ( 'NONE',  ( 10.24394221959000184, 3.220342255699999878, -6.005413528376000620 ) ) ;
#25079 = VERTEX_POINT ( 'NONE', #10438 ) ;
#25080 = EDGE_CURVE ( 'NONE', #48333, #12771, #21730, .T. ) ;
#25081 = CARTESIAN_POINT ( 'NONE',  ( 1.446806799207333905, 0.9161175952574844850, -3.408904368339102930 ) ) ;
#25082 = DIRECTION ( 'NONE',  ( 0.000000000000000000, 1.000000000000000000, 0.000000000000000000 ) ) ;
#25083 = CARTESIAN_POINT ( 'NONE',  ( 10.83810672858429847, 2.978701842912999886, 8.268288002587098617 ) ) ;
#25084 = CARTESIAN_POINT ( 'NONE',  ( 13.84418086765596811, -9.492976300313964444, -8.170822042159171517 ) ) ;
#25085 = CARTESIAN_POINT ( 'NONE',  ( 10.02052890782000105, 2.899999999999999911, 6.152188490330000370 ) ) ;
#25086 = ORIENTED_EDGE ( 'NONE', *, *, #6551, .F. ) ;
#25087 = DIRECTION ( 'NONE',  ( 0.4384236320214023874, 0.000000000000000000, 0.8987684456439055669 ) ) ;
#25088 = B_SPLINE_CURVE_WITH_KNOTS ( 'NONE', 3,
 ( #14891, #68703, #63802, #63105 ),
 .UNSPECIFIED., .F., .F.,
 ( 4, 4 ),
 ( 0.000000000000000000, 1.000000000000000000 ),
 .UNSPECIFIED. ) ;
#25089 = EDGE_CURVE ( 'NONE', #20133, #24634, #70, .T. ) ;
#25090 = ADVANCED_FACE ( 'NONE', ( #647 ), #60230, .F. ) ;
#25091 = DIRECTION ( 'NONE',  ( 1.000000000000000000, 0.000000000000000000, 0.000000000000000000 ) ) ;
#25092 = COLOUR_RGB ( '', 0.66274510, 0.83137255, 0.94901961) ;
#25093 = CARTESIAN_POINT ( 'NONE',  ( 8.125618316923414852, -5.037132069328078998, 6.102874426331527324 ) ) ;
#25094 = CARTESIAN_POINT ( 'NONE',  ( 9.246126402770999064, -2.931626221533000010, 7.902879529556599891 ) ) ;
#25095 = ORIENTED_EDGE ( 'NONE', *, *, #41759, .F. ) ;
#25096 = CARTESIAN_POINT ( 'NONE',  ( 10.31494349883999995, -4.644418916688000110, -4.564229129027999932 ) ) ;
#25097 = CARTESIAN_POINT ( 'NONE',  ( 10.72272469555899832, -3.360453478306600239, 8.606479382885998675 ) ) ;
#25098 = ORIENTED_EDGE ( 'NONE', *, *, #67246, .F. ) ;
#25099 = DIRECTION ( 'NONE',  ( 0.000000000000000000, -0.9925108176925444559, -0.1221567712543053241 ) ) ;
#25100 = ORIENTED_EDGE ( 'NONE', *, *, #5054, .F. ) ;
#25101 = CARTESIAN_POINT ( 'NONE',  ( 9.622313405920001728, -4.009302068291999532, -9.043024413115999138 ) ) ;
#25102 = DIRECTION ( 'NONE',  ( -1.000000000000000000, 0.000000000000000000, -5.786858784063000233E-14 ) ) ;
#25103 = CARTESIAN_POINT ( 'NONE',  ( 10.98146005378009882, 4.911671201000399556, -7.013182449205100255 ) ) ;
#25104 = CARTESIAN_POINT ( 'NONE',  ( 8.817462135714999150, 5.100000000000000533, 6.571291218949999902 ) ) ;
#25105 = CARTESIAN_POINT ( 'NONE',  ( 12.29572644340311349, 2.862796356722883573, -12.35963739789472804 ) ) ;
#25106 = CARTESIAN_POINT ( 'NONE',  ( 11.12072335273220069, -3.602909566644000083, 6.430603299050000388 ) ) ;
#25107 = CARTESIAN_POINT ( 'NONE',  ( 7.410857780409000561, 2.302289264429000504, 6.875166305059000393 ) ) ;
#25108 = EDGE_CURVE ( 'NONE', #66643, #44271, #12591, .T. ) ;
#25109 = ORIENTED_EDGE ( 'NONE', *, *, #30018, .T. ) ;
#25110 = DIRECTION ( 'NONE',  ( 0.000000000000000000, 1.000000000000000000, 2.114232622412000242E-14 ) ) ;
#25111 = CARTESIAN_POINT ( 'NONE',  ( 8.995183059623999000, -2.707994276285999646, 5.994456121676999594 ) ) ;
#25112 = DIRECTION ( 'NONE',  ( 0.7071067486699967874, -0.7071068137030968037, 9.022793105466955192E-11 ) ) ;
#25113 = VERTEX_POINT ( 'NONE', #44346 ) ;
#25114 = B_SPLINE_SURFACE_WITH_KNOTS ( 'NONE', 3, 3, ( 
 ( #44048, #50667, #28304, #2089 ),
 ( #39836, #64996, #29356, #60465 ),
 ( #17472, #23407, #29017, #61158 ),
 ( #23746, #34250, #44401, #33554 ),
 ( #60810, #12573, #13276, #22362 ),
 ( #33209, #66042, #17111, #55570 ),
 ( #38445, #55220, #49627, #7320 ),
 ( #59768, #65701, #1732, #11869 ),
 ( #39138, #17824, #54874, #49974 ),
 ( #1388, #54527, #18166, #33903 ),
 ( #7671, #28661, #39488, #12923 ),
 ( #6629, #22704, #50324, #2422 ),
 ( #61498, #41206, #19536, #67751 ),
 ( #24440, #36294, #62516, #45427 ),
 ( #19187, #3782, #13616, #9035 ),
 ( #45766, #30713, #61836, #9717 ) ),
 .UNSPECIFIED., .F., .F., .F.,
 ( 4, 1, 1, 1, 1, 1, 1, 1, 1, 1, 1, 1, 1, 4 ),
 ( 4, 4 ),
 ( 0.02893036654739999936, 0.07692307692307999434, 0.1538461538461999845, 0.2307692307692000011, 0.3076923076922999933, 0.3846153846154000133, 0.4615384615385000333, 0.5384615384614999112, 0.6153846153845999867, 0.6923076923076999512, 0.7692307692308000266, 0.8461538461537999600, 0.9230769230769000355, 0.9829517739831000744 ),
 ( -0.1837382356070000056, 1.183731649722000068 ),
 .UNSPECIFIED. ) ;
#25115 = CARTESIAN_POINT ( 'NONE',  ( 12.54493252275451454, -3.068391087487185587, -12.30078773432380324 ) ) ;
#25116 = CARTESIAN_POINT ( 'NONE',  ( 10.42380110216399913, 3.026453990125600235, 8.094557215852098864 ) ) ;
#25117 =( GEOMETRIC_REPRESENTATION_CONTEXT ( 3 ) GLOBAL_UNCERTAINTY_ASSIGNED_CONTEXT ( ( #10116 ) ) GLOBAL_UNIT_ASSIGNED_CONTEXT ( ( #20568, #34949, #57276 ) ) REPRESENTATION_CONTEXT ( 'NONE', 'WORKASPACE' ) );
#25118 = CARTESIAN_POINT ( 'NONE',  ( 11.11478185320999934, -2.548220588762000194, -8.356740464335999263 ) ) ;
#25119 = CARTESIAN_POINT ( 'NONE',  ( 7.016658217992999269, 10.82163639346000394, -3.419280833082998683 ) ) ;
#25120 = CARTESIAN_POINT ( 'NONE',  ( 17.79284288850699980, -3.413161633892000335, -11.89755489758000095 ) ) ;
#25121 = CARTESIAN_POINT ( 'NONE',  ( 24.50549018619200226, -8.845081872398999678, 9.150167881427000438 ) ) ;
#25122 = CARTESIAN_POINT ( 'NONE',  ( 12.78422741110794192, -1.875000586273901870, -13.78627160872173185 ) ) ;
#25123 = CARTESIAN_POINT ( 'NONE',  ( 11.56441235500451015, -4.638700978900200056, -6.914884925939399629 ) ) ;
#25124 = CARTESIAN_POINT ( 'NONE',  ( 10.98579841651039857, -4.449968941611500028, -8.696179055230999211 ) ) ;
#25125 = DIRECTION ( 'NONE',  ( 1.000000000000000000, 0.000000000000000000, 0.000000000000000000 ) ) ;
#25126 = VERTEX_POINT ( 'NONE', #21501 ) ;
#25127 = ORIENTED_EDGE ( 'NONE', *, *, #59446, .F. ) ;
#25128 = CARTESIAN_POINT ( 'NONE',  ( 11.33810207955129812, -3.203462856645999945, -7.825000000000000178 ) ) ;
#25129 = FACE_OUTER_BOUND ( 'NONE', #65231, .T. ) ;
#25130 = CARTESIAN_POINT ( 'NONE',  ( 18.15005478418062523, 2.691381137403321855, 13.63095209219456905 ) ) ;
#25131 = CARTESIAN_POINT ( 'NONE',  ( 10.86493304757000011, 4.678466548873998931, -9.048467117372998914 ) ) ;
#25132 = CARTESIAN_POINT ( 'NONE',  ( 8.745593092018999926, 5.100000000000000533, 6.404090157675000228 ) ) ;
#25133 = CIRCLE ( 'NONE', #3909, 1.300177795737000874 ) ;
#25134 = CARTESIAN_POINT ( 'NONE',  ( 18.17892392841393345, 2.542707335428990412, 12.44153274845740142 ) ) ;
#25135 = CARTESIAN_POINT ( 'NONE',  ( 18.01722669115800102, 3.499390932422000056, -11.96939125376999868 ) ) ;
#25136 = CARTESIAN_POINT ( 'NONE',  ( 9.034110134264999203, 4.695345051283999815, 8.660667941667000491 ) ) ;
#25137 = EDGE_CURVE ( 'NONE', #19063, #45676, #41802, .T. ) ;
#25138 = CARTESIAN_POINT ( 'NONE',  ( 9.296304629759626792, -3.464785522094639969, 6.807845768027799060 ) ) ;
#25139 = ORIENTED_EDGE ( 'NONE', *, *, #47453, .F. ) ;
#25140 = CARTESIAN_POINT ( 'NONE',  ( 18.29995268966800026, -2.861739928647000220, -11.98821236628000086 ) ) ;
#25141 = CARTESIAN_POINT ( 'NONE',  ( 8.918455549952998496, -3.325238030324599858, -6.955569812538500152 ) ) ;
#25142 = CARTESIAN_POINT ( 'NONE',  ( 10.37026939687000038, 5.571553923009999743, 7.748385725654999945 ) ) ;
#25143 = CARTESIAN_POINT ( 'NONE',  ( 12.05811496860034993, -2.954409148022000053, 8.035816473382100256 ) ) ;
#25144 = CARTESIAN_POINT ( 'NONE',  ( 7.245399458952341831, -0.2246543155497662536, 1.160034907470290699 ) ) ;
#25145 = CARTESIAN_POINT ( 'NONE',  ( 11.01863125001000121, 7.596591408283000391, -6.386077099867999429 ) ) ;
#25146 = CARTESIAN_POINT ( 'NONE',  ( 10.88733729122639993, 2.722429312291999803, -7.466391690027689876 ) ) ;
#25147 = CARTESIAN_POINT ( 'NONE',  ( 12.18107318252211435, 0.04114048977874578544, 12.69993211551498469 ) ) ;
#25148 = B_SPLINE_CURVE_WITH_KNOTS ( 'NONE', 3,
 ( #50852, #34782, #23587, #55411 ),
 .UNSPECIFIED., .F., .F.,
 ( 4, 4 ),
 ( 0.000000000000000000, 0.8163836489557156906 ),
 .UNSPECIFIED. ) ;
#25149 = CARTESIAN_POINT ( 'NONE',  ( 7.839801658770999992, 3.084076314893000159, 9.259847992573000397 ) ) ;
#25150 = CARTESIAN_POINT ( 'NONE',  ( 10.06344080699000010, 5.156228702401000952, 6.125219923432000613 ) ) ;
#25151 = CARTESIAN_POINT ( 'NONE',  ( 9.175271089438615135, -2.907098125219630624, 8.295045686540735375 ) ) ;
#25152 = ORIENTED_EDGE ( 'NONE', *, *, #57794, .T. ) ;
#25153 = CARTESIAN_POINT ( 'NONE',  ( 9.038304719595000591, 3.867331042029999999, -9.227339949050001877 ) ) ;
#25154 = CARTESIAN_POINT ( 'NONE',  ( 7.027948440668999375, -1.484077041169999944, -0.09315860241765000493 ) ) ;
#25155 = AXIS2_PLACEMENT_3D ( 'NONE', #62367, #68982, #63386 ) ;
#25156 = CARTESIAN_POINT ( 'NONE',  ( 17.87051611373833637, 1.960066664249855206, 13.77321273358846021 ) ) ;
#25157 = LINE ( 'NONE', #56973, #41829 ) ;
#25158 = CARTESIAN_POINT ( 'NONE',  ( 10.33351354018233081, 2.750000000000000000, -7.336375382625529795 ) ) ;
#25159 = CARTESIAN_POINT ( 'NONE',  ( 10.64949279009019989, -4.260984538213099526, -8.468936491037499792 ) ) ;
#25160 = ORIENTED_EDGE ( 'NONE', *, *, #67732, .T. ) ;
#25161 = B_SPLINE_CURVE_WITH_KNOTS ( 'NONE', 3,
 ( #26935, #15753, #48248, #46881, #68188, #36385, #4560, #25898, #37080, #5256, #47227, #57355, #20652, #354, #21669, #42664, #41978, #64311, #47915, #36039, #15413, #36739, #9459, #12, #10162, #26248, #47575, #58393, #25555, #43363, #17115, #5935, #38449, #6633, #49980, #6277, #28308, #33213, #64663, #48600, #60470, #59772, #33558, #54879, #32866, #1392, #60126, #54533, #43705, #44406, #16767, #22708, #2093, #27971, #49282, #22366, #38099, #44052, #59424, #23412, #49631, #6981, #11522, #65357, #65000, #44748, #17476, #59084, #27278 ),
 .UNSPECIFIED., .F., .F.,
 ( 4, 2, 2, 2, 2, 2, 2, 2, 2, 2, 2, 2, 2, 1, 2, 2, 2, 1, 2, 2, 2, 2, 1, 2, 2, 2, 2, 2, 2, 2, 2, 2, 2, 2, 2, 4 ),
 ( 0.000000000000000000, 0.06249999999997735145, 0.1249999999999547029, 0.1562499999999433786, 0.1874999999999320544, 0.2187499999999207301, 0.2343749999999142908, 0.2499999999999078515, 0.2812499999998929745, 0.2968749999998860356, 0.3124999999998790967, 0.3281249999998721578, 0.3437499999998652189, 0.3593749999998582800, 0.3671874999998542277, 0.3749999999998501754, 0.3906249999998412936, 0.3984374999998368527, 0.4023437499998346878, 0.4062499999998324673, 0.4218749999998229749, 0.4296874999998182010, 0.4335937499998163136, 0.4355468749998162026, 0.4374999999998160916, 0.4531249999998210876, 0.4687499999998260836, 0.4843749999998310796, 0.4999999999998361311, 0.5312499999998461231, 0.5468749999998507860, 0.5624999999998554490, 0.5937499999998658851, 0.6249999999998763212, 0.7499999999999168443, 1.000000000000000000 ),
 .UNSPECIFIED. ) ;
#25162 = CARTESIAN_POINT ( 'NONE',  ( 1.152881272621999909, -0.1662993809364999853, 3.755095982464999871 ) ) ;
#25163 = CARTESIAN_POINT ( 'NONE',  ( 17.71610594244102188, -0.6042361944557627096, -12.68064620454363478 ) ) ;
#25165 = CARTESIAN_POINT ( 'NONE',  ( 7.716851002542999716, 2.832432432432000269, 6.822293592207000934 ) ) ;
#25164 = CARTESIAN_POINT ( 'NONE',  ( 9.955712514275658620, 2.254889933401060809, 7.383222385005002053 ) ) ;
#25166 = DIRECTION ( 'NONE',  ( 0.7071082394066938726, -0.7071053229633939008, 3.720439694272969466E-11 ) ) ;
#25167 =( NAMED_UNIT ( * ) SI_UNIT ( $, .STERADIAN. ) SOLID_ANGLE_UNIT ( ) );
#25168 = CARTESIAN_POINT ( 'NONE',  ( 17.81540764135920440, -1.931433452195108869, -13.77768866547343407 ) ) ;
#25169 = CARTESIAN_POINT ( 'NONE',  ( 11.36749010443639918, 4.863785690678500195, 7.435402237490909449 ) ) ;
#25170 = FACE_OUTER_BOUND ( 'NONE', #6089, .T. ) ;
#25171 = CARTESIAN_POINT ( 'NONE',  ( 8.758793146794999984, -3.977267280662000193, 9.308921106447000327 ) ) ;
#25172 = ORIENTED_EDGE ( 'NONE', *, *, #51392, .F. ) ;
#25173 = CARTESIAN_POINT ( 'NONE',  ( 9.112170280412000167, 2.368264398678999516, 7.410200237937000445 ) ) ;
#25174 = EDGE_CURVE ( 'NONE', #146, #49400, #9226, .T. ) ;
#25176 = CARTESIAN_POINT ( 'NONE',  ( 10.00190805961999807, -2.729654112791000120, -8.843024969850999284 ) ) ;
#25175 = CARTESIAN_POINT ( 'NONE',  ( 6.899999691988000450, -13.87069231928999891, 4.225386915259999654 ) ) ;
#25177 = CARTESIAN_POINT ( 'NONE',  ( 7.481712774526203091, -2.396946871456744788, 6.823884033406665495 ) ) ;
#25178 = CARTESIAN_POINT ( 'NONE',  ( 18.17180742357672685, -0.1030366931642786449, 13.89950396794448473 ) ) ;
#25179 = CARTESIAN_POINT ( 'NONE',  ( 2.156491312998999987, 2.610776529918000133, -2.002676742402000443 ) ) ;
#25180 = EDGE_LOOP ( 'NONE', ( #23905, #39796, #16600, #8529 ) ) ;
#25181 = CARTESIAN_POINT ( 'NONE',  ( 2.144642041300283353, -0.2797333540616577241, -3.290985472785137755 ) ) ;
#25182 = CARTESIAN_POINT ( 'NONE',  ( 12.18333460557258974, -3.837988184179999873, 6.509695444280099608 ) ) ;
#25183 = FACE_OUTER_BOUND ( 'NONE', #26506, .T. ) ;
#25184 = CARTESIAN_POINT ( 'NONE',  ( 9.351497027444999333, 4.821940693094999730, 8.950154065657999425 ) ) ;
#25185 = TOROIDAL_SURFACE ( 'NONE', #33021, 11.15000000000000036, 0.5000000000000000000 ) ;
#25186 = CARTESIAN_POINT ( 'NONE',  ( 11.28533594839949750, 4.750012929834699804, 8.359517726022600570 ) ) ;
#25187 = CARTESIAN_POINT ( 'NONE',  ( 11.50029455687000102, -11.65000000000000036, 0.000000000000000000 ) ) ;
#25188 = CARTESIAN_POINT ( 'NONE',  ( 15.89979320885400327, -3.824231472901999496, -11.71686814605000038 ) ) ;
#25189 = CARTESIAN_POINT ( 'NONE',  ( 12.19537138483621064, -2.360847786584734820, 12.48294616049498629 ) ) ;
#25190 = EDGE_CURVE ( 'NONE', #58690, #47043, #25088, .T. ) ;
#25191 = CARTESIAN_POINT ( 'NONE',  ( 9.475279990687656806, -5.350441389720279162, 7.499985493516659218 ) ) ;
#25192 = CARTESIAN_POINT ( 'NONE',  ( 17.94045008455787382, -3.136494811772694735, 13.64413575143460911 ) ) ;
#25193 = CARTESIAN_POINT ( 'NONE',  ( 17.63932472559542930, 3.120604413325762216, -13.52206336586467295 ) ) ;
#25194 = ORIENTED_EDGE ( 'NONE', *, *, #14957, .T. ) ;
#25195 = VERTEX_POINT ( 'NONE', #48080 ) ;
#25196 = ADVANCED_FACE ( 'NONE', ( #58222 ), #42834, .F. ) ;
#25197 = CARTESIAN_POINT ( 'NONE',  ( 23.56664311700400205, 13.31365802054999925, 4.296923094388999331 ) ) ;
#25198 = ORIENTED_EDGE ( 'NONE', *, *, #36528, .T. ) ;
#25199 = SURFACE_STYLE_USAGE ( .BOTH. , #30794 ) ;
#25200 = CARTESIAN_POINT ( 'NONE',  ( 11.83518044953559922, 4.768048975940600620, 7.099502491684900107 ) ) ;
#25201 = CARTESIAN_POINT ( 'NONE',  ( 10.80815748598999981, 2.937526572573000205, 8.948458885032000154 ) ) ;
#25202 = CARTESIAN_POINT ( 'NONE',  ( 10.76231429546999863, 3.259156861436999897, -8.644989069184999764 ) ) ;
#25203 = CARTESIAN_POINT ( 'NONE',  ( 10.26539516633362759, -3.766791217824746241, -8.343294540545050708 ) ) ;
#25204 = CARTESIAN_POINT ( 'NONE',  ( 10.31457635473999979, -5.362146312020000138, 6.677778992223999843 ) ) ;
#25205 = CARTESIAN_POINT ( 'NONE',  ( 18.13005353941771958, 0.4382646521645942594, -12.59237917444261434 ) ) ;
#25206 = CARTESIAN_POINT ( 'NONE',  ( 24.30001122408866721, -12.15210915335040909, -3.256147833976223538 ) ) ;
#25207 = CARTESIAN_POINT ( 'NONE',  ( 10.50595525820100029, -4.081787880721680750, -6.637672143048099827 ) ) ;
#25208 = CARTESIAN_POINT ( 'NONE',  ( 8.368323341230000878, 4.780986922229000236, 6.267222470044999660 ) ) ;
#25209 = ORIENTED_EDGE ( 'NONE', *, *, #53095, .F. ) ;
#25210 = CIRCLE ( 'NONE', #7344, 12.99999854704999969 ) ;
#25211 = CARTESIAN_POINT ( 'NONE',  ( 6.799999045260999964, -9.295457794069999835, 5.399713664196000629 ) ) ;
#25212 = CARTESIAN_POINT ( 'NONE',  ( 11.09999999999999964, 4.000000000000000000, -7.500000000000000000 ) ) ;
#25213 = CARTESIAN_POINT ( 'NONE',  ( 10.21684687351595677, -3.231816600031351516, -6.500416447002277387 ) ) ;
#25214 = AXIS2_PLACEMENT_3D ( 'NONE', #22050, #64346, #38132 ) ;
#25215 = LINE ( 'NONE', #62611, #17167 ) ;
#25216 = CARTESIAN_POINT ( 'NONE',  ( 12.32410271629023057, 1.971482746313077516, 13.86049503924169279 ) ) ;
#25217 = CARTESIAN_POINT ( 'NONE',  ( 13.69997185827399733, 10.91304490500502666, 4.183762365652748727 ) ) ;
#25218 = ORIENTED_EDGE ( 'NONE', *, *, #9133, .F. ) ;
#25219 = EDGE_CURVE ( 'NONE', #31587, #47463, #34267, .T. ) ;
#25220 = CARTESIAN_POINT ( 'NONE',  ( 12.50368198879321824, 0.5476376383131742465, -12.68410501634012988 ) ) ;
#25221 = B_SPLINE_CURVE_WITH_KNOTS ( 'NONE', 3,
 ( #58213, #21156, #58551, #5418 ),
 .UNSPECIFIED., .F., .F.,
 ( 4, 4 ),
 ( 0.000000000000000000, 1.000000000000000000 ),
 .UNSPECIFIED. ) ;
#25222 = CARTESIAN_POINT ( 'NONE',  ( 12.57207325926688846, -0.6915911779535657278, 13.98290807251246726 ) ) ;
#25223 = ORIENTED_EDGE ( 'NONE', *, *, #4999, .T. ) ;
#25224 = CARTESIAN_POINT ( 'NONE',  ( 23.66004879239100234, 13.39256445865000167, -3.813547382634999483 ) ) ;
#25225 = DIRECTION ( 'NONE',  ( 0.000000000000000000, 1.000000000000000000, 0.000000000000000000 ) ) ;
#25226 = CARTESIAN_POINT ( 'NONE',  ( 12.80505043854143388, 3.248109929747637015, -13.61799478206225444 ) ) ;
#25227 = CARTESIAN_POINT ( 'NONE',  ( 12.16287348028854964, -4.761955701524100526, 7.088026579158399620 ) ) ;
#25228 = VECTOR ( 'NONE', #42699, 1000.000000000000114 ) ;
#25229 = CARTESIAN_POINT ( 'NONE',  ( 8.940795537697432849, -5.100000000000000533, 6.662590550605505868 ) ) ;
#25230 = CARTESIAN_POINT ( 'NONE',  ( -0.1507337372581999957, -2.198759671591000053, -2.775001775783000113 ) ) ;
#25231 = B_SPLINE_CURVE_WITH_KNOTS ( 'NONE', 3,
 ( #41709, #30201, #3604, #24940, #46273, #30536, #9537, #51848 ),
 .UNSPECIFIED., .F., .F.,
 ( 4, 1, 1, 1, 1, 4 ),
 ( 0.000000000000000000, 0.07676470621494888014, 0.2763109384346265074, 0.4758571706543032187, 0.6754034028747566420, 0.7874025540483345909 ),
 .UNSPECIFIED. ) ;
#25232 = DIRECTION ( 'NONE',  ( 0.9999999999938153916, 3.516990153967782703E-06, 1.152484550329262306E-11 ) ) ;
#25233 = CARTESIAN_POINT ( 'NONE',  ( 12.14231515301101005, 2.188169521966901954, 12.40854677421460472 ) ) ;
#25234 = DIRECTION ( 'NONE',  ( -1.000000000000000000, 0.000000000000000000, 0.000000000000000000 ) ) ;
#25235 = CARTESIAN_POINT ( 'NONE',  ( 11.48641235500450009, 3.260080192309100067, -6.822158181405299615 ) ) ;
#25236 = CARTESIAN_POINT ( 'NONE',  ( 21.60000000000000142, 0.000000000000000000, 0.000000000000000000 ) ) ;
#25237 = CARTESIAN_POINT ( 'NONE',  ( 12.80505043854144276, 0.6564304467897706941, -12.64601024127358286 ) ) ;
#25238 = CARTESIAN_POINT ( 'NONE',  ( 9.402671671056999969, 2.738456190347000163, -7.711876388024100137 ) ) ;
#25240 = CARTESIAN_POINT ( 'NONE',  ( 12.20324964191634898, 2.330992520694229686, 12.48933099340106700 ) ) ;
#25239 = CARTESIAN_POINT ( 'NONE',  ( 10.04762433003745414, 4.043475630241087693, 8.964144173642713653 ) ) ;
#25241 = CARTESIAN_POINT ( 'NONE',  ( 10.07314899745999881, 5.167567567567999731, -6.822293592207000934 ) ) ;
#25242 = ORIENTED_EDGE ( 'NONE', *, *, #66522, .F. ) ;
#25243 = CARTESIAN_POINT ( 'NONE',  ( 10.73724174883999893, 3.975468761016990094, 6.608211443991299561 ) ) ;
#25244 = DIRECTION ( 'NONE',  ( 0.000000000000000000, 1.000000000000000000, 0.000000000000000000 ) ) ;
#25245 = CARTESIAN_POINT ( 'NONE',  ( 10.33688779216199904, 4.801941500727100021, 7.210800365544999480 ) ) ;
#25246 = CARTESIAN_POINT ( 'NONE',  ( 23.51508327619200145, -2.987169178960999982, 13.81528548245999843 ) ) ;
#25247 = CARTESIAN_POINT ( 'NONE',  ( 5.000000000000000000, 0.05000000000000000278, -3.149999999999999911 ) ) ;
#25248 = CARTESIAN_POINT ( 'NONE',  ( 12.72203378256782358, -1.880187905311242691, 13.78554362285501789 ) ) ;
#25249 = DIRECTION ( 'NONE',  ( 1.000000000000000000, 0.000000000000000000, 0.000000000000000000 ) ) ;
#25250 = CARTESIAN_POINT ( 'NONE',  ( 23.51511192986600207, 2.985795376826999803, -13.81554990515000014 ) ) ;
#25251 = VERTEX_POINT ( 'NONE', #57881 ) ;
#25252 = EDGE_CURVE ( 'NONE', #64156, #21338, #10668, .T. ) ;
#25253 = EDGE_CURVE ( 'NONE', #27541, #25841, #9982, .T. ) ;
#25254 = CARTESIAN_POINT ( 'NONE',  ( 4.490111958656000546, 0.5591895818894999648, -0.9870222206389998032 ) ) ;
#25255 = CARTESIAN_POINT ( 'NONE',  ( 9.706621437244999484, -3.150324864944999970, -6.543738240676099771 ) ) ;
#25256 = ADVANCED_FACE ( 'NONE', ( #58564 ), #25720, .T. ) ;
#25257 = CARTESIAN_POINT ( 'NONE',  ( 4.074968078372999791, 0.000000000000000000, 0.000000000000000000 ) ) ;
#25258 = CARTESIAN_POINT ( 'NONE',  ( 10.87199293566600034, -3.366612813978900220, 6.723009541442299231 ) ) ;
#25259 = CARTESIAN_POINT ( 'NONE',  ( 17.82442946238793624, 1.812220263014552746, -12.46899672597967346 ) ) ;
#25260 = CARTESIAN_POINT ( 'NONE',  ( 8.267078902232004367, -3.206627312864001489, -6.583550664415995790 ) ) ;
#25261 = AXIS2_PLACEMENT_3D ( 'NONE', #64231, #59006, #52722 ) ;
#25262 = CARTESIAN_POINT ( 'NONE',  ( 18.08152692720025101, 2.836954189442855601, 12.36664858736386741 ) ) ;
#25263 = CARTESIAN_POINT ( 'NONE',  ( 12.18233509006103610, 2.554099910133862394, -13.66183974826738279 ) ) ;
#25264 = LINE ( 'NONE', #31549, #42410 ) ;
#25265 = CARTESIAN_POINT ( 'NONE',  ( 10.38053305961999939, -5.283785200568999585, -8.830188095997000275 ) ) ;
#25266 = CARTESIAN_POINT ( 'NONE',  ( 8.945154276125833803, -5.350566776863196594, 7.852883605855081051 ) ) ;
#25267 = CARTESIAN_POINT ( 'NONE',  ( 12.64055492385137391, 0.7115697451012049646, -13.98190580764195978 ) ) ;
#25268 = CARTESIAN_POINT ( 'NONE',  ( 23.59510617619071482, 13.38784577629162342, 4.018474608037379880 ) ) ;
#25269 = CARTESIAN_POINT ( 'NONE',  ( 9.174642513462206495, -2.649442673322992103, 7.499981897072125925 ) ) ;
#25270 = B_SPLINE_CURVE_WITH_KNOTS ( 'NONE', 3,
 ( #67840, #19961, #10154, #31482, #57015, #31830, #26238, #53146, #5247, #26586, #36032, #17107, #64654, #59415, #32514, #37408, #26927, #28300 ),
 .UNSPECIFIED., .F., .F.,
 ( 4, 2, 2, 2, 2, 2, 2, 2, 4 ),
 ( 0.000000000000000000, 0.1250000000000000000, 0.2500000000000000000, 0.3750000000000000000, 0.5000000000000000000, 0.6250000000000000000, 0.7500000000000000000, 0.8750000000000000000, 1.000000000000000000 ),
 .UNSPECIFIED. ) ;
#25271 = B_SPLINE_CURVE_WITH_KNOTS ( 'NONE', 3,
 ( #44309, #34154, #18417, #18072, #39389, #65605, #55125, #13523, #28565, #23997, #49880, #1990, #23312, #12828, #28922, #50227, #23650, #39742, #35186, #62760, #56499, #25710, #61738, #31310, #40415, #47042, #9622, #13858, #57179, #24688, #66980, #67658, #52622, #19092, #63096, #8604, #51931, #4715, #45675, #35863, #29953, #3686, #30968, #41110, #51257, #8946, #9274 ),
 .UNSPECIFIED., .F., .F.,
 ( 4, 2, 2, 2, 2, 2, 2, 2, 1, 2, 2, 2, 2, 2, 2, 1, 2, 2, 1, 2, 2, 2, 2, 2, 4 ),
 ( 0.4985961975199688090, 0.5299339351749688953, 0.5456028040024686332, 0.5612716728299683711, 0.5691061072437181290, 0.5769405416574677758, 0.5926094104849677358, 0.6004438448987177157, 0.6082782793124676957, 0.6239471481399688768, 0.6396160169674700580, 0.6552848857949711281, 0.6709537546224723092, 0.6866226234499734904, 0.7022914922774745605, 0.7179603611049757417, 0.7492980987599813236, 0.7649669675874821717, 0.7806358364149829088, 0.8119735740699847160, 0.8433113117249863011, 0.8746490493799881083, 0.9059867870349896934, 0.9373245246899915006, 1.000000000000000000 ),
 .UNSPECIFIED. ) ;
#25272 = CARTESIAN_POINT ( 'NONE',  ( 2.936390132544666187, 0.4581489286485155299, -3.499999999999999556 ) ) ;
#25273 = EDGE_CURVE ( 'NONE', #16735, #16938, #65059, .T. ) ;
#25274 = CARTESIAN_POINT ( 'NONE',  ( 9.559179719593000613, 4.038835765825999680, -5.935509327774999733 ) ) ;
#25275 = CARTESIAN_POINT ( 'NONE',  ( 8.716851002545999094, 2.832432432432000269, 6.822293592207000934 ) ) ;
#25276 = ORIENTED_EDGE ( 'NONE', *, *, #56357, .T. ) ;
#25277 = VECTOR ( 'NONE', #24490, 1000.000000000000000 ) ;
#25278 = CARTESIAN_POINT ( 'NONE',  ( 8.476519155276850626, -5.080278632455760501, 8.330433920098281320 ) ) ;
#25279 = CARTESIAN_POINT ( 'NONE',  ( 18.05353730554811520, 1.987694103345767127, -13.85817950142402033 ) ) ;
#25280 = VERTEX_POINT ( 'NONE', #31663 ) ;
#25281 = EDGE_CURVE ( 'NONE', #2324, #2854, #24222, .T. ) ;
#25282 = CARTESIAN_POINT ( 'NONE',  ( 10.08601337669299980, -4.772923352651200268, 7.892807122431200639 ) ) ;
#25283 = CARTESIAN_POINT ( 'NONE',  ( 10.80502344389999791, 2.874741265256000489, 8.182900850620900002 ) ) ;
#25284 = CARTESIAN_POINT ( 'NONE',  ( 4.149992563292000725, -1.999946284944287722, -0.2617923565148043141 ) ) ;
#25285 = CARTESIAN_POINT ( 'NONE',  ( 10.02877429409719667, 2.700021399671855615, -8.762287518837057476 ) ) ;
#25286 = CARTESIAN_POINT ( 'NONE',  ( 10.81013259637009938, -5.031671030421000168, -8.062151801142800167 ) ) ;
#25287 = CARTESIAN_POINT ( 'NONE',  ( 11.60000000000000142, -3.064876132552084353, -6.791171049664777470 ) ) ;
#25288 = CARTESIAN_POINT ( 'NONE',  ( 9.099999931440999390, -2.753634353389999845, -7.404749409716440134 ) ) ;
#25289 = ORIENTED_EDGE ( 'NONE', *, *, #45588, .T. ) ;
#25290 = PLANE ( 'NONE',  #26485 ) ;
#25291 = CARTESIAN_POINT ( 'NONE',  ( 9.734454719592999794, 3.021734963141999852, -6.070209284876999511 ) ) ;
#25292 = VERTEX_POINT ( 'NONE', #60258 ) ;
#25293 = CARTESIAN_POINT ( 'NONE',  ( 10.40558702164999971, 5.599341344818000721, -8.437759619346000051 ) ) ;
#25294 = SURFACE_SIDE_STYLE ('',( #46283 ) ) ;
#25295 = VERTEX_POINT ( 'NONE', #34044 ) ;
#25296 = CARTESIAN_POINT ( 'NONE',  ( 9.807938025973999885, 3.334935831489500124, 8.592736948783000983 ) ) ;
#25297 = CARTESIAN_POINT ( 'NONE',  ( 17.60340893540761797, -3.198498114537105419, -12.18727270072288604 ) ) ;
#25298 = CARTESIAN_POINT ( 'NONE',  ( 8.736413463905998711, -3.915843685459630574, -8.382409559052598880 ) ) ;
#25299 = CARTESIAN_POINT ( 'NONE',  ( 24.72544608131600086, -12.30754379070000049, -2.942921080080999729 ) ) ;
#25300 = CARTESIAN_POINT ( 'NONE',  ( 10.52657390975000062, -8.217615421285000110, -6.595888977210999649 ) ) ;
#25301 = ORIENTED_EDGE ( 'NONE', *, *, #55846, .F. ) ;
#25302 = CARTESIAN_POINT ( 'NONE',  ( 11.49200216175158396, 3.580169417146517485, 6.297929225185963098 ) ) ;
#25303 = CARTESIAN_POINT ( 'NONE',  ( 10.23581084123000018, 3.621841509808999771, -8.806208131805998818 ) ) ;
#25304 = DIRECTION ( 'NONE',  ( 0.000000000000000000, 1.000000000000000000, 0.000000000000000000 ) ) ;
#25305 = CARTESIAN_POINT ( 'NONE',  ( 12.70947385406807406, 3.242135136469467049, -13.61941870117945541 ) ) ;
#25306 = FACE_OUTER_BOUND ( 'NONE', #30142, .T. ) ;
#25307 = DIRECTION ( 'NONE',  ( -1.000000000000000000, 0.000000000000000000, 0.000000000000000000 ) ) ;
#25308 = CARTESIAN_POINT ( 'NONE',  ( 9.792315001194999979, -4.284154785471999460, -9.000488933596999530 ) ) ;
#25309 = EDGE_CURVE ( 'NONE', #13611, #15150, #7454, .T. ) ;
#25310 = EDGE_CURVE ( 'NONE', #37989, #23021, #11567, .T. ) ;
#25311 = ORIENTED_EDGE ( 'NONE', *, *, #35969, .T. ) ;
#25312 = ORIENTED_EDGE ( 'NONE', *, *, #16388, .T. ) ;
#25313 = CARTESIAN_POINT ( 'NONE',  ( 9.278070280414000948, 2.546924812613000189, -6.918870225297999887 ) ) ;
#25314 = CIRCLE ( 'NONE', #14149, 0.3000000000000000444 ) ;
#25315 = CARTESIAN_POINT ( 'NONE',  ( 7.102406491832000235, -0.2966009291953999871, 3.049954386258999950 ) ) ;
#25316 = CARTESIAN_POINT ( 'NONE',  ( 8.241912900173000267, -4.599999999999999645, 6.117539782833000928 ) ) ;
#25317 = CARTESIAN_POINT ( 'NONE',  ( 25.19550552243000041, 8.372893704327999842, -8.693236786278001560 ) ) ;
#25318 = DIRECTION ( 'NONE',  ( -1.000000000000000000, 0.000000000000000000, 0.000000000000000000 ) ) ;
#25319 = CARTESIAN_POINT ( 'NONE',  ( 18.31386961183700279, -3.086648833569000328, -11.29009770192999973 ) ) ;
#25321 = CARTESIAN_POINT ( 'NONE',  ( 8.920125482160894848, 2.358211129006373863, 8.150900180138641815 ) ) ;
#25320 = CARTESIAN_POINT ( 'NONE',  ( 10.05369678796300015, -3.827518619249500098, 8.489491017455099708 ) ) ;
#25322 = CARTESIAN_POINT ( 'NONE',  ( 8.914833952003988315, -4.559940160807997245, -6.172232737057998797 ) ) ;
#25323 = ORIENTED_EDGE ( 'NONE', *, *, #18148, .T. ) ;
#25324 = CARTESIAN_POINT ( 'NONE',  ( 11.05581126733999930, -2.753616725312000302, 5.054244401329000880 ) ) ;
#25325 = CARTESIAN_POINT ( 'NONE',  ( 10.36275829612999821, -3.274066978825000085, -4.865563198160999470 ) ) ;
#25326 = CARTESIAN_POINT ( 'NONE',  ( 10.52022949779799887, 4.709679768527199606, 6.435697190503999465 ) ) ;
#25327 = CARTESIAN_POINT ( 'NONE',  ( 7.936333771302000351, 5.123034328734999754, 6.721303713258000023 ) ) ;
#25328 = DIRECTION ( 'NONE',  ( 0.000000000000000000, -0.9624505444715651947, -0.2714570858282905341 ) ) ;
#25329 = DIRECTION ( 'NONE',  ( 0.000000000000000000, 0.000000000000000000, -1.000000000000000000 ) ) ;
#25330 = CARTESIAN_POINT ( 'NONE',  ( 8.546960841229999772, 2.724453559418999582, -8.908010318766001134 ) ) ;
#25331 = ADVANCED_FACE ( 'NONE', ( #23193 ), #59939, .T. ) ;
#25332 = EDGE_CURVE ( 'NONE', #26903, #4716, #58838, .T. ) ;
#25333 = FACE_OUTER_BOUND ( 'NONE', #7511, .T. ) ;
#25334 = PLANE ( 'NONE',  #17699 ) ;
#25335 = ADVANCED_FACE ( 'NONE', ( #17960 ), #55707, .T. ) ;
#25336 = CARTESIAN_POINT ( 'NONE',  ( 5.958730561998000219, -0.03293945794144000072, -1.175625617539999945 ) ) ;
#25337 = CARTESIAN_POINT ( 'NONE',  ( 0.3077908348429792551, -0.8650031602613956760, 3.222008420499449688 ) ) ;
#25338 = CARTESIAN_POINT ( 'NONE',  ( 18.50005573548403959, -2.729642361723122246, -11.32578974454799337 ) ) ;
#25339 = ORIENTED_EDGE ( 'NONE', *, *, #4803, .F. ) ;
#25340 = CARTESIAN_POINT ( 'NONE',  ( 12.34869027095183469, -0.4275228316712924581, -12.69032453495386648 ) ) ;
#25341 = CARTESIAN_POINT ( 'NONE',  ( 12.48631554272197874, -3.044136704961547757, -12.30804282041571085 ) ) ;
#25342 = CARTESIAN_POINT ( 'NONE',  ( 8.599999952505998024, -4.000000000000000000, -7.500000000000000000 ) ) ;
#25343 = PLANE ( 'NONE',  #36823 ) ;
#25344 = CARTESIAN_POINT ( 'NONE',  ( 3.500000000000000888, -0.4453636064423555641, 3.246405014819000900 ) ) ;
#25345 = EDGE_LOOP ( 'NONE', ( #15416, #22343, #44528, #27084 ) ) ;
#25346 = CARTESIAN_POINT ( 'NONE',  ( 8.455992358785000107, -3.399999999999999911, 6.571291218964999459 ) ) ;
#25347 = PRODUCT_CONTEXT ( 'NONE', #17253, 'mechanical' ) ;
#25348 = CARTESIAN_POINT ( 'NONE',  ( 10.97540928332104215, 8.495318605243999954, 6.551665373225851852 ) ) ;
#25349 = CARTESIAN_POINT ( 'NONE',  ( 13.73573769406200107, -11.39043216638999922, -2.256426478477000064 ) ) ;
#25350 = CARTESIAN_POINT ( 'NONE',  ( 1.667640132540000097, -1.762666431298160141, 3.058252359239895579 ) ) ;
#25351 = CARTESIAN_POINT ( 'NONE',  ( 11.02301463001509774, 4.547357026650399980, -6.623338154204899908 ) ) ;
#25352 = EDGE_LOOP ( 'NONE', ( #36971, #34218, #17367, #37095 ) ) ;
#25353 = AXIS2_PLACEMENT_3D ( 'NONE', #45186, #66493, #39942 ) ;
#25354 = CARTESIAN_POINT ( 'NONE',  ( 10.57223537388000167, -4.020426196685999543, 8.920680607665000039 ) ) ;
#25355 = VERTEX_POINT ( 'NONE', #45220 ) ;
#25356 = EDGE_CURVE ( 'NONE', #27849, #49580, #63329, .T. ) ;
#25357 = FACE_OUTER_BOUND ( 'NONE', #39371, .T. ) ;
#25358 = CARTESIAN_POINT ( 'NONE',  ( 16.04514873068900016, 3.655338946640000142, 11.11851555082999887 ) ) ;
#25359 = CARTESIAN_POINT ( 'NONE',  ( 17.55505043854144276, -0.7302158263239267866, -13.98094363220830871 ) ) ;
#25360 = ORIENTED_EDGE ( 'NONE', *, *, #32656, .T. ) ;
#25361 = CARTESIAN_POINT ( 'NONE',  ( 0.000000000000000000, 2.533699434757234137, -1.460905701136922197 ) ) ;
#25362 = DIRECTION ( 'NONE',  ( 0.000000000000000000, 0.000000000000000000, 1.000000000000000000 ) ) ;
#25363 = CARTESIAN_POINT ( 'NONE',  ( 6.786054719591000151, 4.411055010497999973, -9.010057343561001630 ) ) ;
#25364 = VECTOR ( 'NONE', #49912, 999.9999999999998863 ) ;
#25365 = LINE ( 'NONE', #26407, #16369 ) ;
#25366 = DIRECTION ( 'NONE',  ( 1.000000000000000000, 0.000000000000000000, 0.000000000000000000 ) ) ;
#25367 = ORIENTED_EDGE ( 'NONE', *, *, #6525, .F. ) ;
#25368 = CARTESIAN_POINT ( 'NONE',  ( 10.21608469020999976, -5.961703525007000515, 7.319668113368000384 ) ) ;
#25369 = CARTESIAN_POINT ( 'NONE',  ( 12.63953418767025205, -1.875000000000001110, -13.78627077332612316 ) ) ;
#25370 = CARTESIAN_POINT ( 'NONE',  ( 5.490443173017126810, -0.1963495408493673433, 1.499999999999999334 ) ) ;
#25371 = EDGE_LOOP ( 'NONE', ( #9551, #38873, #25634, #15035, #39562 ) ) ;
#25372 = CARTESIAN_POINT ( 'NONE',  ( 10.05525937050999907, -5.223866772223000332, -6.898311956607000361 ) ) ;
#25373 = AXIS2_PLACEMENT_3D ( 'NONE', #4515, #36001, #63591 ) ;
#25374 = CARTESIAN_POINT ( 'NONE',  ( 11.02319144466311052, 5.119973997747526262, 7.175010281093781472 ) ) ;
#25375 = EDGE_LOOP ( 'NONE', ( #44478, #32103, #33803, #62153, #30118, #15670, #22337, #50860, #23738, #57822 ) ) ;
#25376 = CARTESIAN_POINT ( 'NONE',  ( 10.80572075886704653, 4.425289333137247816, 9.224018707921255000 ) ) ;
#25377 = LINE ( 'NONE', #41806, #10928 ) ;
#25378 = DIRECTION ( 'NONE',  ( 1.000000000000000000, 0.000000000000000000, 0.000000000000000000 ) ) ;
#25379 = CARTESIAN_POINT ( 'NONE',  ( 11.72003495742762169, 3.351648276371850699, -11.15746180793245657 ) ) ;
#25380 = VECTOR ( 'NONE', #7841, 1000.000000000000000 ) ;
#25381 = CARTESIAN_POINT ( 'NONE',  ( 12.35432851685904332, 2.933105360581561349, 13.57195094675647873 ) ) ;
#25382 = CARTESIAN_POINT ( 'NONE',  ( 17.80628805164909423, -1.927626392034356595, 12.56668820897845507 ) ) ;
#25383 = ORIENTED_EDGE ( 'NONE', *, *, #13666, .F. ) ;
#25384 = CARTESIAN_POINT ( 'NONE',  ( 7.613711861438999584, -4.858906194260998568, 6.437673909214002954 ) ) ;
#25385 = VERTEX_POINT ( 'NONE', #39976 ) ;
#25386 = CARTESIAN_POINT ( 'NONE',  ( 9.479214860607999782, 4.071727169861000029, 9.089299483126000112 ) ) ;
#25387 = DIRECTION ( 'NONE',  ( 0.000000000000000000, -0.9916377111174248249, 0.1290528957048032721 ) ) ;
#25388 = CARTESIAN_POINT ( 'NONE',  ( 8.722235841230000730, 3.844886277615000125, -8.888911790991000927 ) ) ;
#25389 = CARTESIAN_POINT ( 'NONE',  ( 2.803334101832999803, -0.2418256465843999781, -3.535455962752999781 ) ) ;
#25390 = CARTESIAN_POINT ( 'NONE',  ( 9.961463664312999455, -2.787129471086000176, -8.677705025472000955 ) ) ;
#25391 = CARTESIAN_POINT ( 'NONE',  ( -15.86200481174999943, 2.399999999999999911, -6.571291218949999902 ) ) ;
#25392 = CARTESIAN_POINT ( 'NONE',  ( 9.040000584825472529, -4.926967860734864146, 8.481257932625776874 ) ) ;
#25393 = ADVANCED_FACE ( 'NONE', ( #55013 ), #24311, .T. ) ;
#25394 = EDGE_CURVE ( 'NONE', #37746, #39911, #6759, .T. ) ;
#25395 = ORIENTED_EDGE ( 'NONE', *, *, #46597, .F. ) ;
#25396 = CARTESIAN_POINT ( 'NONE',  ( 11.44072200990529886, -5.077092948368999714, 7.875713849677398848 ) ) ;
#25397 = CARTESIAN_POINT ( 'NONE',  ( 10.90000000000000036, -1.315736040608999957, 10.71955403322999878 ) ) ;
#25399 = DIRECTION ( 'NONE',  ( -0.5000000000000150990, 0.08222066253632250021, -0.8621135439442261239 ) ) ;
#25398 =( BOUNDED_SURFACE ( )  B_SPLINE_SURFACE ( 3, 3, ( 
 ( #1947, #12086, #59976, #6835, #49484, #1595, #22910, #65560, #17684 ),
 ( #56109, #67965, #45965, #66595, #67275, #8562, #51547, #8221, #34798 ),
 ( #19741, #46314, #9233, #61696, #19391, #14500, #3643, #20080, #29568 ),
 ( #25322, #67614, #35145, #14158, #56457, #61358, #30573, #30243, #24981 ) ),
 .UNSPECIFIED., .F., .F., .T. ) 
 B_SPLINE_SURFACE_WITH_KNOTS ( ( 4, 4 ),
 ( 4, 1, 1, 1, 1, 1, 4 ),
 ( 0.000000000000000000, 1.000000000000000000 ),
 ( -0.006083171280208000097, 0.000000000000000000, 0.04308213411242000496, 0.08189950809580999469, 0.1190113006902999981, 0.1566624088843000251, 0.1888062695230000032 ),
 .UNSPECIFIED. ) 
 GEOMETRIC_REPRESENTATION_ITEM ( )  RATIONAL_B_SPLINE_SURFACE ( (
 ( 1.221012668528999923, 1.221012668528999923, 1.221012668528999923, 1.221012668528999923, 1.221012668528999923, 1.221012668528999923, 1.221012668528999923, 1.221012668528999923, 1.221012668528999923),
 ( 0.9263291104904000095, 0.9263291104904000095, 0.9263291104904000095, 0.9263291104904000095, 0.9263291104904000095, 0.9263291104904000095, 0.9263291104904000095, 0.9263291104904000095, 0.9263291104904000095),
 ( 0.9263291104904000095, 0.9263291104904000095, 0.9263291104904000095, 0.9263291104904000095, 0.9263291104904000095, 0.9263291104904000095, 0.9263291104904000095, 0.9263291104904000095, 0.9263291104904000095),
 ( 1.221012668528999923, 1.221012668528999923, 1.221012668528999923, 1.221012668528999923, 1.221012668528999923, 1.221012668528999923, 1.221012668528999923, 1.221012668528999923, 1.221012668528999923) ) ) 
 REPRESENTATION_ITEM ( '' )  SURFACE ( )  );
#25400 = CARTESIAN_POINT ( 'NONE',  ( 17.55505043854143565, 1.875000000000000000, -25.00000000000000000 ) ) ;
#25402 = CARTESIAN_POINT ( 'NONE',  ( 12.15512143692708946, 2.141660958113119850, -13.83591020988682807 ) ) ;
#25401 = CARTESIAN_POINT ( 'NONE',  ( 10.96080777006000062, 2.054568739078000306, 7.810084630238000258 ) ) ;
#25403 = CARTESIAN_POINT ( 'NONE',  ( 11.35918179236250047, 3.761636028845500412, -6.384440618559000136 ) ) ;
#25404 = VECTOR ( 'NONE', #26390, 1000.000000000000000 ) ;
#25405 = B_SPLINE_CURVE_WITH_KNOTS ( 'NONE', 3,
 ( #38534, #7761, #18604, #39930 ),
 .UNSPECIFIED., .F., .F.,
 ( 4, 4 ),
 ( 0.000000000000000000, 1.000000000000000000 ),
 .UNSPECIFIED. ) ;
#25406 = CARTESIAN_POINT ( 'NONE',  ( 8.717397846562217723, -4.245312990446880264, -8.340771899786949106 ) ) ;
#25407 = B_SPLINE_CURVE_WITH_KNOTS ( 'NONE', 3,
 ( #68009, #34845, #41454, #20124, #51259, #24345, #29613, #56850, #46359, #4029, #67660, #57181, #40417, #62084, #24690, #9276, #62762, #40762 ),
 .UNSPECIFIED., .F., .F.,
 ( 4, 2, 2, 2, 2, 2, 2, 2, 4 ),
 ( 0.000000000000000000, 0.1250000000000000000, 0.2500000000000000000, 0.3750000000000000000, 0.5000000000000000000, 0.6250000000000000000, 0.7500000000000000000, 0.8750000000000000000, 1.000000000000000000 ),
 .UNSPECIFIED. ) ;
#25408 = CARTESIAN_POINT ( 'NONE',  ( 9.323721904869998411, 4.756019688173900306, -7.924431591189499358 ) ) ;
#25409 = CARTESIAN_POINT ( 'NONE',  ( 17.77734287254348189, 0.6847469513499552241, 12.58138041838080667 ) ) ;
#25410 = CARTESIAN_POINT ( 'NONE',  ( 6.683037340858000164, -1.411194079024000070, -0.08858358730369000900 ) ) ;
#25411 = CARTESIAN_POINT ( 'NONE',  ( 11.59456039236534330, 5.314711678001000195, 7.436015812896529020 ) ) ;
#25412 = CONICAL_SURFACE ( 'NONE', #37691, 12.71246950475999959, 0.8960553845711767273 ) ;
#25413 = FACE_OUTER_BOUND ( 'NONE', #55418, .T. ) ;
#25414 = ORIENTED_EDGE ( 'NONE', *, *, #46050, .F. ) ;
#25415 = CARTESIAN_POINT ( 'NONE',  ( 8.256683059623998844, -2.876278577719999952, 6.568889245344999850 ) ) ;
#25416 = CARTESIAN_POINT ( 'NONE',  ( 17.91962727382262344, 3.149549635603924091, 13.64113161598088197 ) ) ;
#25417 = CARTESIAN_POINT ( 'NONE',  ( 8.523148997455999520, 5.167567567567999731, -6.822293592207000934 ) ) ;
#25418 = EDGE_LOOP ( 'NONE', ( #42747, #1296, #15148, #34170, #67108, #32074, #49654, #5712, #65219, #48855, #49858, #61040, #24460, #67659 ) ) ;
#25419 = CONICAL_SURFACE ( 'NONE', #26529, 1.150090567076000214, 0.7854665416972951286 ) ;
#25420 = ADVANCED_FACE ( 'NONE', ( #55357 ), #49764, .T. ) ;
#25421 = CARTESIAN_POINT ( 'NONE',  ( 10.71685100253999856, 2.832432432432000269, 6.822293592207000934 ) ) ;
#25422 = CARTESIAN_POINT ( 'NONE',  ( 10.97635090131019986, 4.999207052587699707, 6.881982988766500497 ) ) ;
#25423 = CARTESIAN_POINT ( 'NONE',  ( 10.29667028040999988, 2.755514216060999999, -6.622437150225000124 ) ) ;
#25424 = ORIENTED_EDGE ( 'NONE', *, *, #45280, .F. ) ;
#25425 = CARTESIAN_POINT ( 'NONE',  ( 1.342640132540666720, -3.058252359239902685, -1.762666431298148595 ) ) ;
#25426 = CIRCLE ( 'NONE', #10623, 1.300160336740999734 ) ;
#25427 = FACE_OUTER_BOUND ( 'NONE', #29618, .T. ) ;
#25428 = CARTESIAN_POINT ( 'NONE',  ( 11.37964291764649971, 2.731641218595000087, 7.656787697937099679 ) ) ;
#25429 = CARTESIAN_POINT ( 'NONE',  ( 7.955253088807634043, -4.981915319337616666, 6.461888573305477834 ) ) ;
#25430 = CARTESIAN_POINT ( 'NONE',  ( 13.99999999347100044, 9.187456302440001110, 8.213201953411001455 ) ) ;
#25431 = EDGE_LOOP ( 'NONE', ( #13090, #44588, #35835, #62768, #63706 ) ) ;
#25432 = CARTESIAN_POINT ( 'NONE',  ( 24.67921310950000091, -12.29514723793999842, -2.979192343402000009 ) ) ;
#25433 = CARTESIAN_POINT ( 'NONE',  ( 8.312764158770001188, 5.897697057214000615, -7.408103789850999377 ) ) ;
#25434 = CARTESIAN_POINT ( 'NONE',  ( 8.128235176271338958, -5.082034189686122971, 6.137861258929247832 ) ) ;
#25435 = CARTESIAN_POINT ( 'NONE',  ( 10.40925461470300029, -5.239722547583999912, 7.184607557167700165 ) ) ;
#25436 = ORIENTED_EDGE ( 'NONE', *, *, #40314, .T. ) ;
#25437 = CARTESIAN_POINT ( 'NONE',  ( 9.150552008289244199, -4.457243628887224141, 8.907160125525155792 ) ) ;
#25438 = CARTESIAN_POINT ( 'NONE',  ( 11.06733863405299800, -3.211524470605299886, 6.494205428462000107 ) ) ;
#25439 = ORIENTED_EDGE ( 'NONE', *, *, #57207, .T. ) ;
#25440 = EDGE_CURVE ( 'NONE', #42736, #65371, #65134, .T. ) ;
#25441 = CARTESIAN_POINT ( 'NONE',  ( 11.50029455687000102, -11.65000000000000213, -0.4692429848744596455 ) ) ;
#25442 = ORIENTED_EDGE ( 'NONE', *, *, #54920, .F. ) ;
#25443 = CARTESIAN_POINT ( 'NONE',  ( 8.610875063856999745, -4.757997781751000410, 5.934102420827000124 ) ) ;
#25444 = CARTESIAN_POINT ( 'NONE',  ( 8.745860841232000027, 4.178200486578000472, -5.608493638783999202 ) ) ;
#25445 = CARTESIAN_POINT ( 'NONE',  ( 11.75203632436369894, 2.890282938442000127, -7.240848640331599917 ) ) ;
#25446 = CARTESIAN_POINT ( 'NONE',  ( 11.84523293495530005, -5.315205473512000012, 7.552870914315270134 ) ) ;
#25447 = CARTESIAN_POINT ( 'NONE',  ( 12.18088753964548410, 2.461875156572521650, -12.46041398465086480 ) ) ;
#25448 = AXIS2_PLACEMENT_3D ( 'NONE', #33292, #43780, #49018 ) ;
#25449 = CARTESIAN_POINT ( 'NONE',  ( 11.68687482311540116, -2.942322404451000128, 7.072673169413499217 ) ) ;
#25450 = FACE_OUTER_BOUND ( 'NONE', #24935, .T. ) ;
#25451 = ORIENTED_EDGE ( 'NONE', *, *, #14154, .T. ) ;
#25452 = CARTESIAN_POINT ( 'NONE',  ( 11.32299956498189886, -5.207010770456999893, -7.174999999999999822 ) ) ;
#25453 = CARTESIAN_POINT ( 'NONE',  ( 17.92003806251651099, -0.6285461057673430441, 12.58436427553280268 ) ) ;
#25454 = CARTESIAN_POINT ( 'NONE',  ( 8.819055905797000605, 2.899999999999999911, -6.571291218949999902 ) ) ;
#25455 = ORIENTED_EDGE ( 'NONE', *, *, #58642, .T. ) ;
#25456 = CARTESIAN_POINT ( 'NONE',  ( 12.30801118402051841, -2.879457308712141117, -12.35502813289141599 ) ) ;
#25457 = CARTESIAN_POINT ( 'NONE',  ( 11.33041235500449950, 3.057642534728299832, 8.363295307663500822 ) ) ;
#25458 = CARTESIAN_POINT ( 'NONE',  ( 10.73615685320999980, -3.078046833211999900, -6.088743704655001032 ) ) ;
#25459 = CARTESIAN_POINT ( 'NONE',  ( 6.068038739436002693, 9.317488949900994299, -4.752944535109002722 ) ) ;
#25460 = CARTESIAN_POINT ( 'NONE',  ( 18.31587707750999883, -3.089759977613000252, -11.98885651319999823 ) ) ;
#25461 = LINE ( 'NONE', #47831, #3999 ) ;
#25462 = CARTESIAN_POINT ( 'NONE',  ( 12.41963733656425006, -3.136527823945748583, -13.64412816271520157 ) ) ;
#25463 = VECTOR ( 'NONE', #17235, 1000.000000000000000 ) ;
#25464 = CARTESIAN_POINT ( 'NONE',  ( 10.87518447801629939, -3.134012688501500055, -7.480906371072489236 ) ) ;
#25465 = CARTESIAN_POINT ( 'NONE',  ( 11.37299956498129916, 2.792989229543000107, 7.825000000000000178 ) ) ;
#25466 = CYLINDRICAL_SURFACE ( 'NONE', #42260, 1.250000000000000222 ) ;
#25467 = ORIENTED_EDGE ( 'NONE', *, *, #55027, .T. ) ;
#25468 = ORIENTED_EDGE ( 'NONE', *, *, #69045, .T. ) ;
#25469 = LINE ( 'NONE', #46803, #19390 ) ;
#25470 = AXIS2_PLACEMENT_3D ( 'NONE', #7636, #35250, #28983 ) ;
#25471 = FILL_AREA_STYLE ('',( #4476 ) ) ;
#25472 = CARTESIAN_POINT ( 'NONE',  ( 24.30000000000000071, -8.756202924575998026, 7.455126447192999883 ) ) ;
#25473 = CARTESIAN_POINT ( 'NONE',  ( 18.13614788748274620, 2.730255577391087929, 13.62187136670912047 ) ) ;
#25474 = CARTESIAN_POINT ( 'NONE',  ( 9.937409415358999354, 3.510662261693000108, -6.227052446266999830 ) ) ;
#25475 = CARTESIAN_POINT ( 'NONE',  ( 10.90000000000000036, -1.300000000000000044, -9.662944685757000940 ) ) ;
#25476 = CARTESIAN_POINT ( 'NONE',  ( 17.98409414022578545, 2.954502725563342480, 12.33397020297173441 ) ) ;
#25477 = CARTESIAN_POINT ( 'NONE',  ( 23.58665831531100210, -13.29306600526000004, 4.189265998478999720 ) ) ;
#25478 = EDGE_CURVE ( 'NONE', #48780, #38871, #38579, .T. ) ;
#25480 = EDGE_CURVE ( 'NONE', #53586, #53307, #15794, .T. ) ;
#25479 = CARTESIAN_POINT ( 'NONE',  ( 9.509901345851000443, 5.077442745148000647, 8.469003100811999474 ) ) ;
#25481 = AXIS2_PLACEMENT_3D ( 'NONE', #38421, #49255, #64975 ) ;
#25482 = ORIENTED_EDGE ( 'NONE', *, *, #61587, .F. ) ;
#25483 = CARTESIAN_POINT ( 'NONE',  ( 9.078327844090949839, 2.243031650800266341, -7.767462267625812267 ) ) ;
#25484 = EDGE_CURVE ( 'NONE', #65047, #5290, #28099, .T. ) ;
#25485 = EDGE_CURVE ( 'NONE', #28596, #31943, #68236, .T. ) ;
#25486 = VERTEX_POINT ( 'NONE', #20358 ) ;
#25487 = CARTESIAN_POINT ( 'NONE',  ( 12.64121575286209698, -3.103492734220866023, 12.29027329182862616 ) ) ;
#25488 = CARTESIAN_POINT ( 'NONE',  ( 13.50003721581400029, 9.159934378815998812, 7.517910889891000537 ) ) ;
#25489 = CARTESIAN_POINT ( 'NONE',  ( 9.892489158770999325, 5.099602161831000124, -9.049221499261999924 ) ) ;
#25490 = CARTESIAN_POINT ( 'NONE',  ( 11.76212378248530044, -4.615095948180499619, 8.663708617168998316 ) ) ;
#25491 = CARTESIAN_POINT ( 'NONE',  ( 7.212165791352507682, 0.5478298943403082655, 1.085172144532685401 ) ) ;
#25492 = CARTESIAN_POINT ( 'NONE',  ( 10.96421577872000164, 7.493628354714999773, -6.190747039866000279 ) ) ;
#25493 = CARTESIAN_POINT ( 'NONE',  ( 10.71503032197929883, 4.743378537856500543, -6.460430507351999196 ) ) ;
#25494 = CARTESIAN_POINT ( 'NONE',  ( 12.29653175235435825, -0.3639343692979916112, 12.69299665021503998 ) ) ;
#25495 = CARTESIAN_POINT ( 'NONE',  ( 11.60000000000000142, 3.254367469151916659, -8.163463725006291583 ) ) ;
#25496 = CARTESIAN_POINT ( 'NONE',  ( 9.476372460169001144, 5.098395626600999542, 6.305536056092000408 ) ) ;
#25497 = CARTESIAN_POINT ( 'NONE',  ( 9.210689323432788456, -2.672069879332360731, 7.743984006150673949 ) ) ;
#25498 = ORIENTED_EDGE ( 'NONE', *, *, #4605, .T. ) ;
#25499 = CARTESIAN_POINT ( 'NONE',  ( 8.441604719589999917, 5.473983809665999622, -8.180077404516000072 ) ) ;
#25500 = CYLINDRICAL_SURFACE ( 'NONE', #43612, 1.500000000000000000 ) ;
#25501 = EDGE_CURVE ( 'NONE', #37337, #35262, #38327, .T. ) ;
#25502 = CARTESIAN_POINT ( 'NONE',  ( 9.028474612548713196, 4.352782978232004218, 8.850949115404432632 ) ) ;
#25503 = CARTESIAN_POINT ( 'NONE',  ( 24.44496356299600137, 12.03536643057000077, 3.224849944858999784 ) ) ;
#25504 = CARTESIAN_POINT ( 'NONE',  ( 24.62620337099106749, 8.774568046559906520, 9.205177742000389074 ) ) ;
#25505 = CARTESIAN_POINT ( 'NONE',  ( 10.37872469555899890, -3.497841151814999883, -6.631215019384099740 ) ) ;
#25506 = EDGE_LOOP ( 'NONE', ( #28253, #61165, #7290, #11279, #50728 ) ) ;
#25507 = CARTESIAN_POINT ( 'NONE',  ( 1.348382408447000191, 1.715249283262000102, -3.156226979448999881 ) ) ;
#25508 = CARTESIAN_POINT ( 'NONE',  ( 7.437260841228000352, 2.216873702600000051, 8.370081218683999680 ) ) ;
#25509 = AXIS2_PLACEMENT_3D ( 'NONE', #49212, #2017, #6560 ) ;
#25512 = CARTESIAN_POINT ( 'NONE',  ( 11.35641146476999985, 3.755935701663000170, -11.79446980948000068 ) ) ;
#25511 = CARTESIAN_POINT ( 'NONE',  ( 9.219964158774999419, 3.941185585667000169, -8.896279800194999865 ) ) ;
#25510 = UNCERTAINTY_MEASURE_WITH_UNIT (LENGTH_MEASURE( 1.000000000000000082E-05 ), #33563, 'distance_accuracy_value', 'NONE');
#25513 = CARTESIAN_POINT ( 'NONE',  ( 18.16777246618443442, -2.623276685093039795, 13.64654026452092062 ) ) ;
#25514 = ORIENTED_EDGE ( 'NONE', *, *, #4999, .F. ) ;
#25515 = CARTESIAN_POINT ( 'NONE',  ( 16.03331929146651902, 3.865558715575580617, 11.84348844988198479 ) ) ;
#25517 = CARTESIAN_POINT ( 'NONE',  ( 17.83329178774387813, -3.059742244759365182, -13.53861815793072054 ) ) ;
#25516 = AXIS2_PLACEMENT_3D ( 'NONE', #40300, #62638, #14080 ) ;
#25518 = CARTESIAN_POINT ( 'NONE',  ( 11.31825954179440075, 4.666231193203100425, 6.946434658287599540 ) ) ;
#25519 = CARTESIAN_POINT ( 'NONE',  ( 9.637068864299580540, 2.899999999999999911, 6.444141223381761208 ) ) ;
#25520 = CARTESIAN_POINT ( 'NONE',  ( 7.282480646792000023, -3.448181789123000218, 9.222458996124998976 ) ) ;
#25521 = ORIENTED_EDGE ( 'NONE', *, *, #11924, .T. ) ;
#25522 = CARTESIAN_POINT ( 'NONE',  ( 9.709999999999999076, -4.496968146123999865, -8.755198255949000696 ) ) ;
#25524 = DIRECTION ( 'NONE',  ( -1.000000000000000000, 0.000000000000000000, 0.000000000000000000 ) ) ;
#25523 = CARTESIAN_POINT ( 'NONE',  ( 10.50145247700547557, 3.917463882723016599, -6.629783135293719099 ) ) ;
#25525 = CARTESIAN_POINT ( 'NONE',  ( 7.595193963087873534, -4.443510954364005450, 5.817927645250587254 ) ) ;
#25526 = FACE_OUTER_BOUND ( 'NONE', #49998, .T. ) ;
#25527 = CARTESIAN_POINT ( 'NONE',  ( 1.175837695950999739, 2.689776413290000168, 2.380956047316999946 ) ) ;
#25528 = ORIENTED_EDGE ( 'NONE', *, *, #44117, .F. ) ;
#25529 = DIRECTION ( 'NONE',  ( -1.000000000000000000, 0.000000000000000000, 0.000000000000000000 ) ) ;
#25530 = CARTESIAN_POINT ( 'NONE',  ( 12.03564291764652872, -4.995889373412399692, 7.623106493640399606 ) ) ;
#25531 = CARTESIAN_POINT ( 'NONE',  ( 11.39975833414730033, 4.796537143354000499, 7.825000000000000178 ) ) ;
#25532 = CARTESIAN_POINT ( 'NONE',  ( 11.64440230172174928, 12.39501812775040612, 1.800675216608106366 ) ) ;
#25533 = ADVANCED_FACE ( 'NONE', ( #24913 ), #30854, .F. ) ;
#25534 = CARTESIAN_POINT ( 'NONE',  ( 10.89149144726329865, 3.340422662105400065, 8.430724369296298093 ) ) ;
#25535 = MECHANICAL_DESIGN_GEOMETRIC_PRESENTATION_REPRESENTATION (  '', ( #50090 ), #63444 ) ;
#25536 = CARTESIAN_POINT ( 'NONE',  ( 23.91426360277828067, -3.339322956494537920, 12.90830990133917133 ) ) ;
#25537 = ADVANCED_FACE ( 'NONE', ( #51482 ), #45536, .F. ) ;
#25538 = DIRECTION ( 'NONE',  ( -1.000000000000000000, 0.000000000000000000, 0.000000000000000000 ) ) ;
#25539 = CARTESIAN_POINT ( 'NONE',  ( 24.32158596962418073, -3.683026248290266036, -12.56966772971727409 ) ) ;
#25540 = CARTESIAN_POINT ( 'NONE',  ( 24.52306329364123982, -12.12196665553936192, -3.142986863021403732 ) ) ;
#25541 = CONICAL_SURFACE ( 'NONE', #62366, 0.6499999954788998613, 0.7853981633972997312 ) ;
#25542 = CARTESIAN_POINT ( 'NONE',  ( 24.22025154479399944, -12.17221585034999976, -3.346030442038999908 ) ) ;
#25543 = DIRECTION ( 'NONE',  ( 1.000000000000000000, 0.000000000000000000, 0.000000000000000000 ) ) ;
#25544 = ORIENTED_EDGE ( 'NONE', *, *, #66348, .T. ) ;
#25545 = CARTESIAN_POINT ( 'NONE',  ( 16.03045494250125458, -9.206206171697960627, -8.492540761685251738 ) ) ;
#25546 = CARTESIAN_POINT ( 'NONE',  ( 10.58422653167975902, -2.899999999999999911, 6.304440313954331465 ) ) ;
#25547 = ORIENTED_EDGE ( 'NONE', *, *, #63373, .T. ) ;
#25548 = CARTESIAN_POINT ( 'NONE',  ( 10.26195635058000022, -4.650927364049000090, 4.591198219796000402 ) ) ;
#25549 = CARTESIAN_POINT ( 'NONE',  ( 10.65364694612719809, 3.195501139158400061, 7.178938988280099132 ) ) ;
#25550 = CARTESIAN_POINT ( 'NONE',  ( 10.12550053024000007, 5.788811067708000024, 7.335561454339999621 ) ) ;
#25551 = CARTESIAN_POINT ( 'NONE',  ( 9.910156421876999744, 2.531070993918000056, -7.917736616860999277 ) ) ;
#25552 = CARTESIAN_POINT ( 'NONE',  ( 9.176241837494625742, -4.657637647145090654, -8.077100505959180055 ) ) ;
#25553 = CARTESIAN_POINT ( 'NONE',  ( 9.792562654643999664, -3.463427761954999795, 6.184385360914999907 ) ) ;
#25554 = CARTESIAN_POINT ( 'NONE',  ( 18.15103067362390377, 0.4097539338085404714, -12.59333942654355809 ) ) ;
#25555 = CARTESIAN_POINT ( 'NONE',  ( 12.23173037681283759, 2.748912840245765654, -12.39010626689092831 ) ) ;
#25556 = CARTESIAN_POINT ( 'NONE',  ( 11.02287616594229824, -4.261927842557799551, -6.674353346984900348 ) ) ;
#25557 = CARTESIAN_POINT ( 'NONE',  ( 10.88314899746000108, 5.167567567567999731, 6.822293592207000934 ) ) ;
#25558 = ORIENTED_EDGE ( 'NONE', *, *, #6608, .F. ) ;
#25559 = CARTESIAN_POINT ( 'NONE',  ( 18.50001572531400029, 2.908166856580999937, -12.18270046149000052 ) ) ;
#25560 =( LENGTH_UNIT ( ) NAMED_UNIT ( * ) SI_UNIT ( .MILLI., .METRE. ) );
#25561 = CARTESIAN_POINT ( 'NONE',  ( 24.92738733624293346, -2.996191037697414128, 11.61850378784546933 ) ) ;
#25562 = CARTESIAN_POINT ( 'NONE',  ( 25.22251638624031855, 11.23359187701061757, -3.340255986890024786 ) ) ;
#25563 = CARTESIAN_POINT ( 'NONE',  ( 9.332537864288001472, 2.899999999999999911, 6.571291218949999902 ) ) ;
#25564 = CARTESIAN_POINT ( 'NONE',  ( 17.95101261602633613, 1.877525629946211971, 12.45933154191684444 ) ) ;
#25565 = CARTESIAN_POINT ( 'NONE',  ( 12.27409806343526100, 3.015283977741789023, 13.67143535301651447 ) ) ;
#25566 = CARTESIAN_POINT ( 'NONE',  ( 9.799258316471000541, -4.057329063942999525, 9.430691159271001212 ) ) ;
#25567 = ORIENTED_EDGE ( 'NONE', *, *, #68635, .T. ) ;
#25568 = VECTOR ( 'NONE', #45721, 1000.000000000000000 ) ;
#25569 = CARTESIAN_POINT ( 'NONE',  ( 12.60523857536293413, -0.5937411427281895637, -12.68132466675194436 ) ) ;
#25570 = EDGE_CURVE ( 'NONE', #20484, #27255, #21605, .T. ) ;
#25571 = CARTESIAN_POINT ( 'NONE',  ( 12.10797096423121566, -0.2010519787742775510, 13.99856097495847607 ) ) ;
#25572 = EDGE_CURVE ( 'NONE', #45838, #21138, #14435, .T. ) ;
#25573 = VERTEX_POINT ( 'NONE', #24575 ) ;
#25574 = CARTESIAN_POINT ( 'NONE',  ( 24.54687940532799928, 8.860358431052000938, 9.345000394951000544 ) ) ;
#25575 = CYLINDRICAL_SURFACE ( 'NONE', #14761, 3.500000000000000000 ) ;
#25576 = CARTESIAN_POINT ( 'NONE',  ( 10.46933016578999975, -4.988498232033999891, 6.213103211926000569 ) ) ;
#25577 = FACE_OUTER_BOUND ( 'NONE', #15022, .T. ) ;
#25578 = CARTESIAN_POINT ( 'NONE',  ( 11.81825954179440075, -3.333768806796900019, 6.946434658287599540 ) ) ;
#25579 = DIRECTION ( 'NONE',  ( 0.000000000000000000, -0.9659258262890756397, 0.2588190451024932059 ) ) ;
#25580 = CARTESIAN_POINT ( 'NONE',  ( 0.6146236793818999899, -2.189299194929000159, -2.346944523683000217 ) ) ;
#25581 = CARTESIAN_POINT ( 'NONE',  ( 11.14955063476181962, 4.976598135215293262, 8.326430086672807818 ) ) ;
#25582 = CARTESIAN_POINT ( 'NONE',  ( 12.13758509790269535, 2.198972988417282615, 12.40663693328272466 ) ) ;
#25583 = CARTESIAN_POINT ( 'NONE',  ( 10.66052890781999984, 2.899999999999999911, -6.152188490330000370 ) ) ;
#25584 = CARTESIAN_POINT ( 'NONE',  ( 10.30487885159599770, 4.996404279947399552, -7.381132626649399064 ) ) ;
#25585 = DIRECTION ( 'NONE',  ( -0.000000000000000000, -0.000000000000000000, 1.000000000000000000 ) ) ;
#25586 = CARTESIAN_POINT ( 'NONE',  ( 11.09178278040999999, 4.578541652803000517, -8.908598806528001290 ) ) ;
#25587 = EDGE_CURVE ( 'NONE', #42619, #14127, #66685, .T. ) ;
#25588 = CARTESIAN_POINT ( 'NONE',  ( 8.668126402770999661, 5.196937059091999878, -7.048639765412399782 ) ) ;
#25590 = CARTESIAN_POINT ( 'NONE',  ( 17.80000000000000071, 14.76315775485999993, 50.50083396221000243 ) ) ;
#25589 = CARTESIAN_POINT ( 'NONE',  ( 17.94577624695061502, -11.84175277259534731, 3.381006001198936683 ) ) ;
#25591 = DIRECTION ( 'NONE',  ( 0.5298945027589778700, -0.5996715052832758408, 0.5996714948178758497 ) ) ;
#25592 = ORIENTED_EDGE ( 'NONE', *, *, #37783, .T. ) ;
#25593 = B_SPLINE_CURVE_WITH_KNOTS ( 'NONE', 3,
 ( #37460, #33262, #48987, #57 ),
 .UNSPECIFIED., .F., .F.,
 ( 4, 4 ),
 ( 0.000000000000000000, 0.1252897476283257872 ),
 .UNSPECIFIED. ) ;
#25594 = CARTESIAN_POINT ( 'NONE',  ( 12.54851516855890381, -0.5702235047293728876, 12.68276536598237136 ) ) ;
#25595 = CARTESIAN_POINT ( 'NONE',  ( 9.140753410162000492, 5.100000000000000533, 6.175944241622000064 ) ) ;
#25596 = CARTESIAN_POINT ( 'NONE',  ( 9.758146639703001668, -2.901368778958000050, 6.555068849476000103 ) ) ;
#25597 = CARTESIAN_POINT ( 'NONE',  ( 9.475696787962998968, 4.148886440911999429, 8.354131589521699652 ) ) ;
#25598 = FACE_OUTER_BOUND ( 'NONE', #53221, .T. ) ;
#25599 = CARTESIAN_POINT ( 'NONE',  ( 23.63992230472121747, -3.364525824305894197, -13.53833436019511360 ) ) ;
#25600 = CARTESIAN_POINT ( 'NONE',  ( 12.34612353109750771, -2.075598726024750817, 13.75436385846647624 ) ) ;
#25601 = CARTESIAN_POINT ( 'NONE',  ( 12.19790361218675123, 2.648659041011996784, 13.64075350830020561 ) ) ;
#25602 = CARTESIAN_POINT ( 'NONE',  ( 23.58305236527900206, 2.939621645348999834, -13.62877849538000063 ) ) ;
#25603 = ORIENTED_EDGE ( 'NONE', *, *, #35618, .T. ) ;
#25604 = CARTESIAN_POINT ( 'NONE',  ( 4.295389598754000282, -0.2757437319869999737, 1.245290690854000015 ) ) ;
#25605 = CARTESIAN_POINT ( 'NONE',  ( 9.731950584426998674, -3.492264136285500253, -6.325866838823999139 ) ) ;
#25606 = CARTESIAN_POINT ( 'NONE',  ( 11.00000000000000000, 3.031410575668799900, -7.174999999999999822 ) ) ;
#25607 = CARTESIAN_POINT ( 'NONE',  ( 11.26857802013510046, -5.174568897094999897, 7.527343341769989316 ) ) ;
#25608 = CARTESIAN_POINT ( 'NONE',  ( 18.17062868725393088, 2.391413364859044322, -12.47623124499065383 ) ) ;
#25609 = CARTESIAN_POINT ( 'NONE',  ( 11.13352130964999809, -2.664740441716999975, 5.115464099832999878 ) ) ;
#25610 = CARTESIAN_POINT ( 'NONE',  ( 18.12474152634368707, 2.757110843030302849, 12.38793583425497147 ) ) ;
#25611 = CARTESIAN_POINT ( 'NONE',  ( 12.34854013679137275, 2.926988005533238013, -13.57357535316153019 ) ) ;
#25612 = CARTESIAN_POINT ( 'NONE',  ( 11.60328610135030125, -4.878060775730400422, 7.174999999999999822 ) ) ;
#25613 = CARTESIAN_POINT ( 'NONE',  ( 10.34267055962000015, -5.750479631840000216, -8.094412205797999249 ) ) ;
#25614 = ADVANCED_FACE ( 'NONE', ( #46934 ), #31008, .T. ) ;
#25615 = CARTESIAN_POINT ( 'NONE',  ( 1.699999999999999956, 0.000000000000000000, 0.000000000000000000 ) ) ;
#25616 = DIRECTION ( 'NONE',  ( 1.000000000000000000, 0.000000000000000000, 0.000000000000000000 ) ) ;
#25617 = DIRECTION ( 'NONE',  ( 0.000000000000000000, -1.000000000000000000, 0.000000000000000000 ) ) ;
#25618 = CARTESIAN_POINT ( 'NONE',  ( 11.09999987043000047, 9.962291482759999539, 5.845852616619999331 ) ) ;
#25619 = CARTESIAN_POINT ( 'NONE',  ( 2.905140132544666631, -0.9161175952574773795, -3.408904368339105595 ) ) ;
#25620 = ORIENTED_EDGE ( 'NONE', *, *, #57743, .F. ) ;
#25621 = CARTESIAN_POINT ( 'NONE',  ( 8.514954719592999766, 3.207599814920999659, -6.150466394809999571 ) ) ;
#25622 = CARTESIAN_POINT ( 'NONE',  ( 11.37518447801629939, -3.134012688501500055, 7.519093628927509876 ) ) ;
#25623 = ORIENTED_EDGE ( 'NONE', *, *, #60693, .F. ) ;
#25624 = CARTESIAN_POINT ( 'NONE',  ( 8.379867906070000316, -2.923743482135000349, 6.439439799216000182 ) ) ;
#25625 = CARTESIAN_POINT ( 'NONE',  ( 17.99906018690869658, 1.940665501735318932, -13.86484298168864093 ) ) ;
#25626 = ORIENTED_EDGE ( 'NONE', *, *, #60890, .F. ) ;
#25627 = FACE_OUTER_BOUND ( 'NONE', #37618, .T. ) ;
#25628 = CARTESIAN_POINT ( 'NONE',  ( 11.22056920625029974, 4.047312782235129802, 8.815417147437999645 ) ) ;
#25629 = CARTESIAN_POINT ( 'NONE',  ( 4.149992563292001613, -1.229060429538525900, -1.599290730647372927 ) ) ;
#25630 = CARTESIAN_POINT ( 'NONE',  ( 11.59999999999999964, 5.064318446328999634, 6.844464917182299324 ) ) ;
#25631 = FACE_OUTER_BOUND ( 'NONE', #13334, .T. ) ;
#25632 = LINE ( 'NONE', #24942, #212 ) ;
#25633 = CARTESIAN_POINT ( 'NONE',  ( 21.59999953993000332, -1.509903313490000218E-14, 12.84999890301438796 ) ) ;
#25634 = ORIENTED_EDGE ( 'NONE', *, *, #63516, .T. ) ;
#25635 = DIRECTION ( 'NONE',  ( 0.000000000000000000, -1.000000000000000000, 0.000000000000000000 ) ) ;
#25636 = CARTESIAN_POINT ( 'NONE',  ( 9.088029719595001055, 2.881930053949999682, -8.823338183322999129 ) ) ;
#25637 = VERTEX_POINT ( 'NONE', #45566 ) ;
#25638 = AXIS2_PLACEMENT_3D ( 'NONE', #8084, #19251, #28376 ) ;
#25639 = CARTESIAN_POINT ( 'NONE',  ( 10.66852712374000056, 4.435471808682999395, -5.866466547508000673 ) ) ;
#25640 = ORIENTED_EDGE ( 'NONE', *, *, #50938, .T. ) ;
#25641 = CARTESIAN_POINT ( 'NONE',  ( 8.516151519676999015, 4.027664626136379766, 6.221087886525999089 ) ) ;
#25642 = CARTESIAN_POINT ( 'NONE',  ( 17.57925770490775008, -3.199697828486423479, -12.18695748817155078 ) ) ;
#25643 = DIRECTION ( 'NONE',  ( -1.000000000000000000, 0.000000000000000000, 0.000000000000000000 ) ) ;
#25644 = CARTESIAN_POINT ( 'NONE',  ( 4.400041421715232381, -0.6049068342875222326, 1.258180343538149781 ) ) ;
#25645 = ADVANCED_FACE ( 'NONE', ( #8495 ), #14089, .F. ) ;
#25646 = CARTESIAN_POINT ( 'NONE',  ( 9.878359312496433731, 5.126777126183345246, 6.752018918868509800 ) ) ;
#25647 = EDGE_CURVE ( 'NONE', #52595, #62430, #8838, .T. ) ;
#25648 = ORIENTED_EDGE ( 'NONE', *, *, #7227, .T. ) ;
#25649 = CARTESIAN_POINT ( 'NONE',  ( 12.24011731813700088, 12.12177778538999995, -3.303327906653999779 ) ) ;
#25650 = CARTESIAN_POINT ( 'NONE',  ( 10.95519834123000003, 3.860336562672999960, -6.147350406894000585 ) ) ;
#25651 = DIRECTION ( 'NONE',  ( 1.000000000000000000, 0.000000000000000000, 0.000000000000000000 ) ) ;
#25652 = CARTESIAN_POINT ( 'NONE',  ( 12.78089499409913721, 3.248109241121360125, -13.61799491149521302 ) ) ;
#25653 = CARTESIAN_POINT ( 'NONE',  ( 18.13027066859324421, 0.4451122480341191956, 13.99293440828418866 ) ) ;
#25654 = CARTESIAN_POINT ( 'NONE',  ( 18.31386961183700279, 3.086648833569000328, 11.29009770192999973 ) ) ;
#25655 = CARTESIAN_POINT ( 'NONE',  ( 10.85290698989999925, -3.170384785323999921, -8.782188229854000383 ) ) ;
#25656 = VERTEX_POINT ( 'NONE', #62320 ) ;
#25657 = ORIENTED_EDGE ( 'NONE', *, *, #62271, .T. ) ;
#25658 = CARTESIAN_POINT ( 'NONE',  ( 9.029445280412998542, 5.442817578555000146, -8.106149115450000053 ) ) ;
#25659 = DIRECTION ( 'NONE',  ( 0.000000000000000000, -1.000000000000000000, 0.000000000000000000 ) ) ;
#25660 = DIRECTION ( 'NONE',  ( 0.000000000000000000, 1.000000000000000000, 4.343333852297002239E-12 ) ) ;
#25661 = CARTESIAN_POINT ( 'NONE',  ( 4.500000484264000455, 12.99999951562999989, 2.124870431850000170E-09 ) ) ;
#25662 = DIRECTION ( 'NONE',  ( 1.000000000000000000, 0.000000000000000000, 0.000000000000000000 ) ) ;
#25663 = EDGE_CURVE ( 'NONE', #27164, #10703, #3047, .T. ) ;
#25664 = CARTESIAN_POINT ( 'NONE',  ( 9.813975701332999790, 4.636077325177999420, -8.089163458558500608 ) ) ;
#25666 = FACE_OUTER_BOUND ( 'NONE', #28472, .T. ) ;
#25665 = CARTESIAN_POINT ( 'NONE',  ( 10.15501337669299886, -4.895413217368500547, 7.955057656228099461 ) ) ;
#25667 = CARTESIAN_POINT ( 'NONE',  ( 23.58334011193800350, 0.000000000000000000, -13.94232983116038227 ) ) ;
#25668 = VERTEX_POINT ( 'NONE', #43415 ) ;
#25669 = EDGE_CURVE ( 'NONE', #47578, #3072, #47963, .T. ) ;
#25670 = CARTESIAN_POINT ( 'NONE',  ( 11.09056211382000079, -2.710928475574999830, 5.109860994294000314 ) ) ;
#25671 = CARTESIAN_POINT ( 'NONE',  ( 10.32823945355000106, -3.233612306621999721, -4.570995416535999389 ) ) ;
#25672 = FACE_OUTER_BOUND ( 'NONE', #5407, .T. ) ;
#25673 = DIRECTION ( 'NONE',  ( -0.7071066712931889375, -0.7071068910798888885, 1.670512803213974822E-10 ) ) ;
#25674 = CARTESIAN_POINT ( 'NONE',  ( 10.90000000011000125, 5.100000000110999743, 6.571291220762999430 ) ) ;
#25675 = CARTESIAN_POINT ( 'NONE',  ( 17.98439275848187435, 2.954313498893424317, -12.33404747595914053 ) ) ;
#25676 = CARTESIAN_POINT ( 'NONE',  ( 9.392285841233000809, 5.775964236216999836, -8.174909295649001706 ) ) ;
#25677 = CARTESIAN_POINT ( 'NONE',  ( 13.99947726215000188, 8.835099311859000437, 7.952110511812001015 ) ) ;
#25678 = CARTESIAN_POINT ( 'NONE',  ( 7.993094057962528254, 3.103801558224323465, -6.363363910445399618 ) ) ;
#25679 = CARTESIAN_POINT ( 'NONE',  ( 0.07497316781761000082, 0.000000000000000000, 0.000000000000000000 ) ) ;
#25680 = CARTESIAN_POINT ( 'NONE',  ( 0.2615634140176161249, 2.004981734223959755, 2.607536443111408087 ) ) ;
#25681 = CARTESIAN_POINT ( 'NONE',  ( 17.65333285638452310, 3.199628934752181131, 12.18697561682395936 ) ) ;
#25682 = CARTESIAN_POINT ( 'NONE',  ( 2.871837672902999739, 1.998183433799000319, 2.574596971963000414 ) ) ;
#25683 = ORIENTED_EDGE ( 'NONE', *, *, #35059, .T. ) ;
#25684 = CARTESIAN_POINT ( 'NONE',  ( 12.46581852961811521, 0.5250240499537035532, -12.68539034781189301 ) ) ;
#25685 = B_SPLINE_CURVE_WITH_KNOTS ( 'NONE', 3,
 ( #47162, #68462, #20585, #41911, #292, #21952 ),
 .UNSPECIFIED., .F., .F.,
 ( 4, 2, 4 ),
 ( 0.000000000000000000, 0.5000000000000000000, 1.000000000000000000 ),
 .UNSPECIFIED. ) ;
#25686 = CARTESIAN_POINT ( 'NONE',  ( 12.20055951530588345, -2.340869620859903577, -12.48721223319660290 ) ) ;
#25687 = CARTESIAN_POINT ( 'NONE',  ( 13.56648734862639571, 12.13584047101458374, 2.505837749223091215 ) ) ;
#25688 = DIRECTION ( 'NONE',  ( 0.9993918455886502406, 0.000000000000000000, -0.03487031647277825247 ) ) ;
#25689 = CARTESIAN_POINT ( 'NONE',  ( 11.09999999999999964, -1.406666666667000021, 10.45580168561000001 ) ) ;
#25690 = ORIENTED_EDGE ( 'NONE', *, *, #58784, .F. ) ;
#25691 = CARTESIAN_POINT ( 'NONE',  ( 9.520528907821001141, -2.899999999999999911, 6.152188490330000370 ) ) ;
#25692 = B_SPLINE_CURVE_WITH_KNOTS ( 'NONE', 3,
 ( #66113, #38869, #33969, #18580, #44811, #22426, #1804, #7044, #43768, #44122 ),
 .UNSPECIFIED., .F., .F.,
 ( 4, 2, 2, 2, 4 ),
 ( 0.4999999997123705242, 0.6249999997842778932, 0.7499999998561852621, 0.8749999999280926311, 1.000000000000000000 ),
 .UNSPECIFIED. ) ;
#25693 = APPLICATION_PROTOCOL_DEFINITION ( 'draft international standard', 'automotive_design', 1998, #43610 ) ;
#25694 = CARTESIAN_POINT ( 'NONE',  ( 0.5420802270800906264, 3.075918330867753792, 1.732122671253175650 ) ) ;
#25695 = CARTESIAN_POINT ( 'NONE',  ( 11.09806944063140399, 2.697063473146602330, 6.634103937412520580 ) ) ;
#25696 = CARTESIAN_POINT ( 'NONE',  ( 6.999999691988000095, 12.11716380430000051, 3.069905306952999791 ) ) ;
#25697 = CARTESIAN_POINT ( 'NONE',  ( 11.31389666366019853, 3.954123449088899900, -8.532487796751999198 ) ) ;
#25698 = EDGE_LOOP ( 'NONE', ( #41281, #51637, #21310, #36627, #62907, #3117, #17454, #28511, #20265, #16728 ) ) ;
#25699 = CARTESIAN_POINT ( 'NONE',  ( 10.46085355684000007, -5.403406918566000527, 7.721809917403000156 ) ) ;
#25700 = ORIENTED_EDGE ( 'NONE', *, *, #2538, .F. ) ;
#25701 = CARTESIAN_POINT ( 'NONE',  ( 17.55505043854147118, -1.760845406083394682, 12.47635457398814829 ) ) ;
#25702 = CARTESIAN_POINT ( 'NONE',  ( 8.700644353210000403, -5.212258818969000451, 6.157189191035000064 ) ) ;
#25703 = CARTESIAN_POINT ( 'NONE',  ( 16.04504292973000190, 8.364028678926000993, 8.186631590245999845 ) ) ;
#25704 = EDGE_CURVE ( 'NONE', #62492, #19870, #24958, .T. ) ;
#25705 = ORIENTED_EDGE ( 'NONE', *, *, #59990, .F. ) ;
#25706 = CARTESIAN_POINT ( 'NONE',  ( 8.416230770385023874, 5.016073627869618079, -8.932544507081987106 ) ) ;
#25707 = CARTESIAN_POINT ( 'NONE',  ( 8.009154640314669393, 4.326009048175516902, -6.176799728275869761 ) ) ;
#25708 = CARTESIAN_POINT ( 'NONE',  ( 7.730829719587998916, 5.281793838578000333, -8.397855149904000172 ) ) ;
#25709 = FACE_OUTER_BOUND ( 'NONE', #45445, .T. ) ;
#25710 = CARTESIAN_POINT ( 'NONE',  ( 18.11183118189959274, -2.784086580389351973, 12.38085211673737085 ) ) ;
#25711 = ORIENTED_EDGE ( 'NONE', *, *, #65506, .F. ) ;
#25712 = CARTESIAN_POINT ( 'NONE',  ( 10.71756905878999966, -3.040221764047000175, 8.808455607108001573 ) ) ;
#25713 = CARTESIAN_POINT ( 'NONE',  ( 12.18106278541768894, -2.459077072136087505, -13.68201856772773972 ) ) ;
#25714 = CARTESIAN_POINT ( 'NONE',  ( 9.429547492598359781, -3.266100554355691354, 6.695580748437408580 ) ) ;
#25715 = ORIENTED_EDGE ( 'NONE', *, *, #59783, .F. ) ;
#25716 = CARTESIAN_POINT ( 'NONE',  ( 10.73506343560000076, -5.202499304193000107, -8.441414596927000247 ) ) ;
#25717 = CARTESIAN_POINT ( 'NONE',  ( 5.000000000000000000, -1.382741116750999977, -11.26545724788999969 ) ) ;
#25718 = B_SPLINE_CURVE_WITH_KNOTS ( 'NONE', 3,
 ( #47027, #63080, #25695, #35511 ),
 .UNSPECIFIED., .F., .F.,
 ( 4, 4 ),
 ( 0.000000000000000000, 1.000000000000000000 ),
 .UNSPECIFIED. ) ;
#25719 = VERTEX_POINT ( 'NONE', #10549 ) ;
#25720 = CYLINDRICAL_SURFACE ( 'NONE', #51018, 12.50000000000000000 ) ;
#25721 = CARTESIAN_POINT ( 'NONE',  ( 10.99797019513065699, 2.534916329350139552, 6.496562598600510441 ) ) ;
#25722 = CARTESIAN_POINT ( 'NONE',  ( 5.274333767848000676, 1.395439897136999896, -0.6918107995601999738 ) ) ;
#25723 = CARTESIAN_POINT ( 'NONE',  ( 5.302943173017458989, 1.199500263597271799, -0.9218200799623701425 ) ) ;
#25724 = CARTESIAN_POINT ( 'NONE',  ( 11.16486084871730000, -2.792989229543000107, -7.174999999999999822 ) ) ;
#25725 = DIRECTION ( 'NONE',  ( 0.000000000000000000, 0.8514547570628039352, -0.5244280662542016858 ) ) ;
#25726 = PLANE ( 'NONE',  #11596 ) ;
#25727 = CARTESIAN_POINT ( 'NONE',  ( 9.792562654643999664, -3.463427761954999795, 6.184385360914999907 ) ) ;
#25728 = VERTEX_POINT ( 'NONE', #10209 ) ;
#25729 = ADVANCED_FACE ( 'NONE', ( #43056 ), #5304, .T. ) ;
#25730 = CARTESIAN_POINT ( 'NONE',  ( 10.44635971519499940, -3.540377183549800133, -6.735384833238199143 ) ) ;
#25731 = EDGE_CURVE ( 'NONE', #5681, #4832, #16142, .T. ) ;
#25732 = EDGE_LOOP ( 'NONE', ( #11805, #65177, #40388 ) ) ;
#25733 = CARTESIAN_POINT ( 'NONE',  ( 9.514114512910998300, 4.887632373702999189, 8.462748516415999234 ) ) ;
#25734 = APPLICATION_CONTEXT ( 'automotive_design' ) ;
#25736 = VECTOR ( 'NONE', #62226, 1000.000000000000000 ) ;
#25735 = B_SPLINE_CURVE_WITH_KNOTS ( 'NONE', 3,
 ( #4833, #63567, #25826, #15680, #69159, #57633, #26870, #52739, #14989, #26175 ),
 .UNSPECIFIED., .F., .F.,
 ( 4, 1, 1, 1, 1, 1, 1, 4 ),
 ( 0.000000000000000000, 0.1608394309853999893, 0.3216792337757999887, 0.4825190365663000192, 0.6433588393567000185, 0.8041986421472000490, 0.9650384449376000484, 1.000000000000000000 ),
 .UNSPECIFIED. ) ;
#25737 = FACE_OUTER_BOUND ( 'NONE', #1635, .T. ) ;
#25738 = CARTESIAN_POINT ( 'NONE',  ( 9.169760841232999837, 4.728328492779000136, -8.692725459657999920 ) ) ;
#25739 = ADVANCED_FACE ( 'NONE', ( #47623 ), #15382, .F. ) ;
#25740 = CARTESIAN_POINT ( 'NONE',  ( 2.677583211399999996, -3.533016733676999976, 0.2751748379743000350 ) ) ;
#25741 = CARTESIAN_POINT ( 'NONE',  ( 7.000000000000000000, 6.495643345158865323, -2.999999999999999556 ) ) ;
#25742 = DIRECTION ( 'NONE',  ( 1.000000000000000000, 0.000000000000000000, 0.000000000000000000 ) ) ;
#25743 = CARTESIAN_POINT ( 'NONE',  ( 18.03457755489743519, 0.4008875276915725983, 13.89221989487217002 ) ) ;
#25744 = EDGE_LOOP ( 'NONE', ( #58313, #68768, #5076, #24085 ) ) ;
#25745 = CARTESIAN_POINT ( 'NONE',  ( 19.89999890908300273, 12.52500000000000036, 0.000000000000000000 ) ) ;
#25746 = CARTESIAN_POINT ( 'NONE',  ( 11.28887616594230003, -4.386455737425299262, 8.718182393403999697 ) ) ;
#25747 = CARTESIAN_POINT ( 'NONE',  ( 10.39984540795353318, 5.293498025891123504, -8.716172560647471812 ) ) ;
#25748 = B_SPLINE_CURVE_WITH_KNOTS ( 'NONE', 3,
 ( #43621, #2000, #17384, #17029 ),
 .UNSPECIFIED., .F., .F.,
 ( 4, 4 ),
 ( 0.000000000000000000, 1.000000000000000000 ),
 .UNSPECIFIED. ) ;
#25749 = CARTESIAN_POINT ( 'NONE',  ( 15.86281931570199966, 8.823480018325001950, 8.551042465543998716 ) ) ;
#25750 = CARTESIAN_POINT ( 'NONE',  ( 7.330275273710999961, -4.426925773067000414, 9.293310812901001583 ) ) ;
#25752 = CARTESIAN_POINT ( 'NONE',  ( 12.61470515272479531, 1.811791595463774662, -13.88227300399932673 ) ) ;
#25751 = CARTESIAN_POINT ( 'NONE',  ( 9.013423559847998590, 4.933953210258000155, 8.417881984655998906 ) ) ;
#25753 = CARTESIAN_POINT ( 'NONE',  ( 11.40425819896749893, 2.744109752373000255, -7.736761623643599428 ) ) ;
#25754 = EDGE_CURVE ( 'NONE', #12209, #9710, #22471, .T. ) ;
#25755 = CARTESIAN_POINT ( 'NONE',  ( 12.80505043854146940, -3.125000000000000000, 12.28374638332999780 ) ) ;
#25756 = CARTESIAN_POINT ( 'NONE',  ( 8.793822372493998785, 3.711294259598199918, -8.444453017408701356 ) ) ;
#25757 = CARTESIAN_POINT ( 'NONE',  ( 17.61479688768388741, 0.7169431667913548356, 12.57958639523259414 ) ) ;
#25758 = CARTESIAN_POINT ( 'NONE',  ( 6.749453605548000112, -0.8819252889501000281, -1.105222071258000094 ) ) ;
#25759 = DIRECTION ( 'NONE',  ( 0.000000000000000000, -1.000000000000000000, 0.000000000000000000 ) ) ;
#25760 = CARTESIAN_POINT ( 'NONE',  ( 24.30000000000000071, -2.078227429405999693, -11.31065739696999906 ) ) ;
#25761 = ORIENTED_EDGE ( 'NONE', *, *, #47772, .F. ) ;
#25762 = CARTESIAN_POINT ( 'NONE',  ( 8.090519353209000286, -5.342173944271999986, 8.432314172168000610 ) ) ;
#25763 = DIRECTION ( 'NONE',  ( -1.000000000000000000, 0.000000000000000000, 0.000000000000000000 ) ) ;
#25764 = CARTESIAN_POINT ( 'NONE',  ( 9.716851002543000604, -2.832432432432000269, 6.822293592207000934 ) ) ;
#25765 = ORIENTED_EDGE ( 'NONE', *, *, #27668, .T. ) ;
#25766 = CARTESIAN_POINT ( 'NONE',  ( 18.44331666222400301, 2.998518551215999750, 12.10579027554000042 ) ) ;
#25767 = CIRCLE ( 'NONE', #51428, 1.499999999999999334 ) ;
#25768 = CARTESIAN_POINT ( 'NONE',  ( 11.01790547754519878, 5.174295865741999734, 7.462730980357120458 ) ) ;
#25769 = CARTESIAN_POINT ( 'NONE',  ( 11.28109528040999976, 2.660125405577999924, -6.904121770750999865 ) ) ;
#25770 = ORIENTED_EDGE ( 'NONE', *, *, #16901, .F. ) ;
#25771 = DIRECTION ( 'NONE',  ( 1.000000000000000000, 0.000000000000000000, 0.000000000000000000 ) ) ;
#25773 = CONICAL_SURFACE ( 'NONE', #63739, 1.349999999768000336, 0.7853981633972997312 ) ;
#25772 = CARTESIAN_POINT ( 'NONE',  ( 18.20569531734444269, -2.110314541856637582, 12.42277286985408224 ) ) ;
#25774 = CARTESIAN_POINT ( 'NONE',  ( 11.45348876160960039, 3.114179898019400206, 6.578783887955899523 ) ) ;
#25775 = CARTESIAN_POINT ( 'NONE',  ( 7.953520338486511854, -5.020965158977404030, 6.510618665280695438 ) ) ;
#25776 = CARTESIAN_POINT ( 'NONE',  ( 7.758198341228000672, 5.797099724369999763, 8.340484548805999765 ) ) ;
#25777 = VERTEX_POINT ( 'NONE', #37464 ) ;
#25778 = CARTESIAN_POINT ( 'NONE',  ( 8.737760194560385330, 3.933854210954582431, 6.629534018758290514 ) ) ;
#25779 = LINE ( 'NONE', #58278, #51857 ) ;
#25780 = CARTESIAN_POINT ( 'NONE',  ( 8.288236139519369772, -4.758661544608824734, 9.065029047955855290 ) ) ;
#25781 = CARTESIAN_POINT ( 'NONE',  ( 9.928000818239000935, -5.131870447930000800, 6.903968392969799694 ) ) ;
#25782 = ORIENTED_EDGE ( 'NONE', *, *, #31493, .T. ) ;
#25783 = CARTESIAN_POINT ( 'NONE',  ( 16.13899430609699692, -3.920333201250000066, -11.93553532998999955 ) ) ;
#25784 = CARTESIAN_POINT ( 'NONE',  ( 10.96887750876899936, -4.692271380433699512, 6.425720373262999274 ) ) ;
#25785 = ORIENTED_EDGE ( 'NONE', *, *, #1590, .F. ) ;
#25786 = CARTESIAN_POINT ( 'NONE',  ( 16.09997386696500143, -8.350085070477001992, -8.123950967096998710 ) ) ;
#25787 = CARTESIAN_POINT ( 'NONE',  ( 7.196266048625999723, 10.76669857437999944, -3.593894311215999782 ) ) ;
#25788 = VERTEX_POINT ( 'NONE', #26984 ) ;
#25789 = ADVANCED_FACE ( 'NONE', ( #68934 ), #58790, .F. ) ;
#25790 = EDGE_CURVE ( 'NONE', #43366, #2324, #57515, .T. ) ;
#25791 = CARTESIAN_POINT ( 'NONE',  ( 11.09999999999999964, 2.649999999999999911, 7.500000000000000000 ) ) ;
#25792 = CARTESIAN_POINT ( 'NONE',  ( 8.795585841232000490, 5.251032986819000214, -6.070151079272999795 ) ) ;
#25793 = CARTESIAN_POINT ( 'NONE',  ( 10.51925056272499859, 5.174767082365999471, -7.517410630436119234 ) ) ;
#25794 = CARTESIAN_POINT ( 'NONE',  ( 11.63746005378019888, -2.838900981960999825, 8.120007936598501175 ) ) ;
#25795 = CARTESIAN_POINT ( 'NONE',  ( 8.633274456858801571, -5.179562484155885826, 6.206446419389337166 ) ) ;
#25796 = CARTESIAN_POINT ( 'NONE',  ( 11.97810404293059960, -4.563346034752700398, 6.352848032645000309 ) ) ;
#25797 = CARTESIAN_POINT ( 'NONE',  ( 10.79399293566600093, -3.453258297007899991, 6.829299525004299376 ) ) ;
#25798 = VERTEX_POINT ( 'NONE', #68580 ) ;
#25799 = CARTESIAN_POINT ( 'NONE',  ( 4.600000207916445483, 2.033928581112999763E-13, -2.806643806251999915E-13 ) ) ;
#25800 = CARTESIAN_POINT ( 'NONE',  ( 7.454683059621999952, -2.138201851198999748, 6.814774777484000623 ) ) ;
#25801 = CARTESIAN_POINT ( 'NONE',  ( 25.46372189163300348, -2.879475976718999686, 11.30953721564000070 ) ) ;
#25802 = ORIENTED_EDGE ( 'NONE', *, *, #6042, .T. ) ;
#25803 = CARTESIAN_POINT ( 'NONE',  ( 12.61225881068687471, -3.094544630460537515, -12.29295341835050870 ) ) ;
#25804 = CARTESIAN_POINT ( 'NONE',  ( 7.146208818154000220, 8.240697770480998940, -4.339685437942002899 ) ) ;
#25805 = CARTESIAN_POINT ( 'NONE',  ( 7.000000000000000000, 0.3230303992915000144, -3.000000000000000000 ) ) ;
#25806 = CARTESIAN_POINT ( 'NONE',  ( 23.56967113362556177, -13.34588780157434051, -4.192937399727497016 ) ) ;
#25807 = CARTESIAN_POINT ( 'NONE',  ( 12.27782020686944264, -2.164202955609507040, -13.73892120162925146 ) ) ;
#25808 = CARTESIAN_POINT ( 'NONE',  ( 11.11718313518939816, -4.622449961306399402, -8.287087605365499599 ) ) ;
#25809 = VECTOR ( 'NONE', #51464, 1000.000000000000000 ) ;
#25810 = CARTESIAN_POINT ( 'NONE',  ( 24.30000000000000071, -3.224868684338999980, -12.03537377768999939 ) ) ;
#25811 = CARTESIAN_POINT ( 'NONE',  ( 18.25219266138124752, -2.678721125794444546, 12.31196912072773308 ) ) ;
#25812 = ORIENTED_EDGE ( 'NONE', *, *, #57509, .F. ) ;
#25813 = ADVANCED_FACE ( 'NONE', ( #20702 ), #42031, .F. ) ;
#25814 = VERTEX_POINT ( 'NONE', #38500 ) ;
#25815 = SURFACE_STYLE_USAGE ( .BOTH. , #57624 ) ;
#25816 = CARTESIAN_POINT ( 'NONE',  ( 7.100000000000000533, 11.06886219213000011, 1.536526853569999851 ) ) ;
#25817 = CARTESIAN_POINT ( 'NONE',  ( 11.79999999471800010, -3.216299622513999701, 11.40340969442000052 ) ) ;
#25818 = EDGE_CURVE ( 'NONE', #39916, #6106, #23110, .T. ) ;
#25819 = CARTESIAN_POINT ( 'NONE',  ( 10.82565186280000091, 5.331165376905000031, -8.542144899688000947 ) ) ;
#25820 = CARTESIAN_POINT ( 'NONE',  ( 10.80160188108999897, -2.805072368922999715, -8.157282064671999677 ) ) ;
#25821 = CARTESIAN_POINT ( 'NONE',  ( 18.18011893007460600, 2.482032845566129797, 12.45575022786950825 ) ) ;
#25822 = CARTESIAN_POINT ( 'NONE',  ( 24.51193677669900239, -12.36181969389999935, 3.074607925011999754 ) ) ;
#25823 = CARTESIAN_POINT ( 'NONE',  ( 9.724611353170001138, 2.928305163963000446, 8.718478150869000132 ) ) ;
#25824 = VECTOR ( 'NONE', #67168, 1000.000000000000227 ) ;
#25825 = ORIENTED_EDGE ( 'NONE', *, *, #54535, .F. ) ;
#25826 = CARTESIAN_POINT ( 'NONE',  ( 10.33542413490000023, -4.762105522783999234, -4.627036157596999821 ) ) ;
#25827 = ORIENTED_EDGE ( 'NONE', *, *, #1197, .F. ) ;
#25828 = CARTESIAN_POINT ( 'NONE',  ( 12.54473519888579247, -3.068232154748443463, 12.30085162971233181 ) ) ;
#25829 = CARTESIAN_POINT ( 'NONE',  ( 9.399709346416997846, -3.216804796119200116, -7.128095150442700145 ) ) ;
#25830 = CARTESIAN_POINT ( 'NONE',  ( 10.94796973825000030, 2.864322365205000054, 8.846249469408000721 ) ) ;
#25831 = CARTESIAN_POINT ( 'NONE',  ( 11.84523293495530005, -5.315205473512000012, 7.552870914315270134 ) ) ;
#25832 = CARTESIAN_POINT ( 'NONE',  ( 9.667010841233000917, 4.769103072373000352, -8.666849124598000387 ) ) ;
#25833 = DIRECTION ( 'NONE',  ( 1.000000000000000000, 0.000000000000000000, 0.000000000000000000 ) ) ;
#25834 = CARTESIAN_POINT ( 'NONE',  ( 10.14887885159599890, 5.269014563305000287, -7.348611220446799486 ) ) ;
#25835 = EDGE_CURVE ( 'NONE', #12259, #24880, #65757, .T. ) ;
#25836 = CARTESIAN_POINT ( 'NONE',  ( 10.86591859237855395, 5.674200084745228523, -8.061124942614856792 ) ) ;
#25837 = CLOSED_SHELL ( 'NONE', ( #30955, #467, #30457, #7658, #53985, #1489, #8836, #60749, #67183, #31126, #24308, #27818, #14913, #35200, #40978, #60839, #35282, #13578, #12231, #16271, #18760, #42859, #66133, #45873, #51022, #58954, #51301, #39579, #53495, #15855, #12872 ) ) ;
#25838 = CARTESIAN_POINT ( 'NONE',  ( 11.59999999999999964, 4.109635333090443154, -8.637585274955606351 ) ) ;
#25839 = CARTESIAN_POINT ( 'NONE',  ( 9.944319408602000365, 5.443001719280999851, 7.367350382395000175 ) ) ;
#25840 = DIRECTION ( 'NONE',  ( 0.000000000000000000, -1.000000000000000000, -0.000000000000000000 ) ) ;
#25841 = VERTEX_POINT ( 'NONE', #33269 ) ;
#25842 = CARTESIAN_POINT ( 'NONE',  ( 8.690229719593000723, 2.414630869937000046, -6.801495146585999407 ) ) ;
#25843 = DIRECTION ( 'NONE',  ( 0.000000000000000000, -1.000000000000000000, 0.000000000000000000 ) ) ;
#25844 = FACE_OUTER_BOUND ( 'NONE', #62649, .T. ) ;
#25845 = CARTESIAN_POINT ( 'NONE',  ( 12.61551017421867371, -3.176304576338894403, -12.19307927066143549 ) ) ;
#25846 = CARTESIAN_POINT ( 'NONE',  ( 24.53429010490700080, 8.855930189872001534, 9.286429716155000236 ) ) ;
#25847 = CARTESIAN_POINT ( 'NONE',  ( 10.28026357027499849, -3.014700852776899698, -7.690095141806899903 ) ) ;
#25848 = ORIENTED_EDGE ( 'NONE', *, *, #27814, .T. ) ;
#25849 = CYLINDRICAL_SURFACE ( 'NONE', #50679, 11.29999999999999893 ) ;
#25850 = CARTESIAN_POINT ( 'NONE',  ( 8.079135841228998416, 3.524748802314000340, 5.573833469815000718 ) ) ;
#25852 = CARTESIAN_POINT ( 'NONE',  ( 13.46268444654400298, -9.428250749343998649, -7.876929641374000646 ) ) ;
#25851 = DIRECTION ( 'NONE',  ( 1.000000000000000000, 0.000000000000000000, 0.000000000000000000 ) ) ;
#25853 = CARTESIAN_POINT ( 'NONE',  ( 18.16264250297551541, -2.646798802813860263, 13.64122832078476222 ) ) ;
#25854 = ORIENTED_EDGE ( 'NONE', *, *, #21910, .T. ) ;
#25855 = CARTESIAN_POINT ( 'NONE',  ( 9.681187238460999822, 2.612249048987000055, 7.804677627401999551 ) ) ;
#25856 = CARTESIAN_POINT ( 'NONE',  ( 18.05171780850500340, -2.879539315883433481, -13.58554773987827780 ) ) ;
#25857 = CARTESIAN_POINT ( 'NONE',  ( 11.44133594839949986, 4.569506585117100173, 8.152656755002400502 ) ) ;
#25858 = CARTESIAN_POINT ( 'NONE',  ( 23.60000000000000142, -2.204728229456999866, 11.99913219504999873 ) ) ;
#25859 = CARTESIAN_POINT ( 'NONE',  ( 7.320269353207000229, -2.466384407480000096, 6.935560677555000275 ) ) ;
#25860 = ORIENTED_EDGE ( 'NONE', *, *, #56320, .T. ) ;
#25861 = CARTESIAN_POINT ( 'NONE',  ( 9.187739158772000536, 5.964723767581000757, 7.776480083716999836 ) ) ;
#25863 = CARTESIAN_POINT ( 'NONE',  ( 10.34267055962000015, -5.750479631840000216, -8.094412205797999249 ) ) ;
#25862 = CARTESIAN_POINT ( 'NONE',  ( 10.14206215041809678, -3.293869621293440630, 8.705460445251572921 ) ) ;
#25864 = CARTESIAN_POINT ( 'NONE',  ( 7.477637590078199281, -2.363906917100113692, 6.907238326532012529 ) ) ;
#25865 = CARTESIAN_POINT ( 'NONE',  ( 24.30000000000000071, -50.08530474119000075, 49.09535524753000146 ) ) ;
#25866 = DIRECTION ( 'NONE',  ( 0.000000000000000000, 0.000000000000000000, -1.000000000000000000 ) ) ;
#25867 = ORIENTED_EDGE ( 'NONE', *, *, #25959, .T. ) ;
#25868 = DIRECTION ( 'NONE',  ( -0.03487031647297116066, -1.485878521854048177E-07, -0.9993918455886323660 ) ) ;
#25869 = CARTESIAN_POINT ( 'NONE',  ( 11.91256651104150066, -3.901000349726440053, 8.498573944230598087 ) ) ;
#25870 = CARTESIAN_POINT ( 'NONE',  ( 9.347254965556000883, 4.028327103212000715, 9.469449669541999626 ) ) ;
#25871 = CARTESIAN_POINT ( 'NONE',  ( 9.854942824136999846, 2.800308224477999985, 9.013816726157999781 ) ) ;
#25872 = CARTESIAN_POINT ( 'NONE',  ( 10.54687750876899877, 3.382085645339300228, 6.541108991297599928 ) ) ;
#25873 = EDGE_LOOP ( 'NONE', ( #56977, #19093, #67373, #3128 ) ) ;
#25874 = EDGE_CURVE ( 'NONE', #6365, #20862, #61608, .T. ) ;
#25875 = ADVANCED_FACE ( 'NONE', ( #59473 ), #46328, .F. ) ;
#25876 = AXIS2_PLACEMENT_3D ( 'NONE', #18219, #62239, #45820 ) ;
#25877 = DIRECTION ( 'NONE',  ( 0.000000000000000000, 0.7071067811865475727, 0.7071067811865475727 ) ) ;
#25878 = EDGE_CURVE ( 'NONE', #49507, #45933, #42131, .T. ) ;
#25879 = CARTESIAN_POINT ( 'NONE',  ( 12.30583355256787925, 1.958333444515651278, -12.44688698484233846 ) ) ;
#25880 = PLANE ( 'NONE',  #54372 ) ;
#25881 = B_SPLINE_CURVE_WITH_KNOTS ( 'NONE', 3,
 ( #31185, #47254, #20679, #42010 ),
 .UNSPECIFIED., .F., .F.,
 ( 4, 4 ),
 ( 0.000000000000000000, 1.000000000000000000 ),
 .UNSPECIFIED. ) ;
#25882 = CARTESIAN_POINT ( 'NONE',  ( 10.98768472639999949, 2.860900986606000007, -4.945212061661000469 ) ) ;
#25883 = CARTESIAN_POINT ( 'NONE',  ( 18.26192063240349839, -2.355523948311723625, 13.80042196861912984 ) ) ;
#25884 = CARTESIAN_POINT ( 'NONE',  ( 18.18005044212792143, 2.500000099754956739, -13.67345740034994250 ) ) ;
#25885 = EDGE_LOOP ( 'NONE', ( #28447, #20517, #59913 ) ) ;
#25886 = CYLINDRICAL_SURFACE ( 'NONE', #58175, 1.350000000000000533 ) ;
#25887 = CARTESIAN_POINT ( 'NONE',  ( 13.39991752512747247, -12.13029446165151803, -2.190571078338873878 ) ) ;
#25888 = ORIENTED_EDGE ( 'NONE', *, *, #66348, .F. ) ;
#25889 = CARTESIAN_POINT ( 'NONE',  ( 8.426541430992324777, 3.894762663531519564, 6.010944450864965205 ) ) ;
#25890 = CARTESIAN_POINT ( 'NONE',  ( 11.66287348028854964, 3.238044298475899918, 7.088026579158399620 ) ) ;
#25891 = AXIS2_PLACEMENT_3D ( 'NONE', #3694, #35536, #19443 ) ;
#25892 = B_SPLINE_CURVE_WITH_KNOTS ( 'NONE', 3,
 ( #4975, #52182, #30188, #35767 ),
 .UNSPECIFIED., .F., .F.,
 ( 4, 4 ),
 ( 0.000000000000000000, 1.000000000000000000 ),
 .UNSPECIFIED. ) ;
#25893 = CARTESIAN_POINT ( 'NONE',  ( 10.90374609491999891, 3.726846467344000047, 5.900456154266000119 ) ) ;
#25894 = CARTESIAN_POINT ( 'NONE',  ( 11.17811698873999937, 2.762452057009999962, -6.187198315927000536 ) ) ;
#25895 = CARTESIAN_POINT ( 'NONE',  ( 9.910787105781626138, -3.243350240173176413, -7.060667085372605456 ) ) ;
#25896 = CARTESIAN_POINT ( 'NONE',  ( 10.18909467608999897, -5.907859813488999912, 7.801539220053999912 ) ) ;
#25897 = CARTESIAN_POINT ( 'NONE',  ( 18.19734990864321134, -0.3336735144251442020, -12.59558214381612551 ) ) ;
#25898 = CARTESIAN_POINT ( 'NONE',  ( 12.49090498480046030, 3.040702594601116360, -12.30901830445451317 ) ) ;
#25899 = CARTESIAN_POINT ( 'NONE',  ( 11.48225819896749833, -5.120994791668000090, -7.711331004020999913 ) ) ;
#25900 = CARTESIAN_POINT ( 'NONE',  ( 10.67500447327561908, -2.650284540010996004, 7.500001951671615430 ) ) ;
#25901 = ORIENTED_EDGE ( 'NONE', *, *, #60247, .F. ) ;
#25902 = CARTESIAN_POINT ( 'NONE',  ( 10.98937577273788868, 3.538822733277925181, 6.300114087089553117 ) ) ;
#25903 = CARTESIAN_POINT ( 'NONE',  ( 9.225036466121004253, 2.649952287134117235, 7.500002258928285315 ) ) ;
#25904 = CARTESIAN_POINT ( 'NONE',  ( 8.659024459946206065, 3.018043227519824345, -6.080012726073716678 ) ) ;
#25905 = CARTESIAN_POINT ( 'NONE',  ( 10.52696718958000055, 8.359475522667993985, 6.870968795365002713 ) ) ;
#25906 = CARTESIAN_POINT ( 'NONE',  ( 12.54749102628328394, 3.200935012631479726, 13.62916378024774566 ) ) ;
#25907 = B_SPLINE_CURVE_WITH_KNOTS ( 'NONE', 3,
 ( #42459, #26383, #47709, #839, #15879, #33002 ),
 .UNSPECIFIED., .F., .F.,
 ( 4, 2, 4 ),
 ( 0.000000000000000000, 0.5000000000000000000, 1.000000000000000000 ),
 .UNSPECIFIED. ) ;
#25908 = CARTESIAN_POINT ( 'NONE',  ( 9.260912867475999732, -4.901383038209000453, 9.090314591495999963 ) ) ;
#25909 = CARTESIAN_POINT ( 'NONE',  ( 12.72380912727782665, -0.6210782762608558771, -12.67955178808352201 ) ) ;
#25910 = CARTESIAN_POINT ( 'NONE',  ( 12.48412837678613663, -0.6552116771452474175, 13.98466387211990636 ) ) ;
#25911 = EDGE_LOOP ( 'NONE', ( #15899, #22182, #60023, #2256, #56489, #51610, #53762, #27882 ) ) ;
#25912 = CARTESIAN_POINT ( 'NONE',  ( 24.56351374471499938, 8.793767919668001198, 9.098879823118998900 ) ) ;
#25913 = CARTESIAN_POINT ( 'NONE',  ( 9.884988259786998910, -4.149395984695000372, -8.631996151823999597 ) ) ;
#25914 = CARTESIAN_POINT ( 'NONE',  ( 11.09999999999999964, 2.700683852703999577, 5.124965750789000296 ) ) ;
#25915 = CARTESIAN_POINT ( 'NONE',  ( 10.49785673611999925, -3.776281940467000275, 5.717636230565000588 ) ) ;
#25916 = CARTESIAN_POINT ( 'NONE',  ( 12.26133460557259980, -3.860150918677800025, 6.645166161828299778 ) ) ;
#25917 = CIRCLE ( 'NONE', #54915, 2.725000000000000089 ) ;
#25918 = EDGE_CURVE ( 'NONE', #44844, #27875, #49964, .T. ) ;
#25919 = CARTESIAN_POINT ( 'NONE',  ( 12.20907020345898708, 0.4097539338085392502, 12.59333942654355631 ) ) ;
#25920 = CARTESIAN_POINT ( 'NONE',  ( 0.1127116734105999968, 1.200150369511000070, -3.152926066752000267 ) ) ;
#25921 = PLANE ( 'NONE',  #40450 ) ;
#25922 = ADVANCED_FACE ( 'NONE', ( #41949 ), #17227, .F. ) ;
#25923 = CARTESIAN_POINT ( 'NONE',  ( 12.15236716622352553, 2.166683524422403639, 12.41231652552486686 ) ) ;
#25924 = CARTESIAN_POINT ( 'NONE',  ( 8.365056901398830291, 2.650139792115765669, -7.500003826568613086 ) ) ;
#25925 = CARTESIAN_POINT ( 'NONE',  ( 10.79718447801629999, 5.003225587801999552, -7.477880487566260115 ) ) ;
#25926 = CARTESIAN_POINT ( 'NONE',  ( 25.50736953685058594, 8.309690528669074538, 8.116381377235668992 ) ) ;
#25927 = CARTESIAN_POINT ( 'NONE',  ( 10.90247028041000021, 4.554785930130000438, -6.081876607904999510 ) ) ;
#25928 = CARTESIAN_POINT ( 'NONE',  ( 8.644809814040998575, 4.698458605182900705, -8.403266072559899769 ) ) ;
#25930 = CARTESIAN_POINT ( 'NONE',  ( 12.24474413020373120, 2.777098231215099577, 12.38267839998011333 ) ) ;
#25929 = CARTESIAN_POINT ( 'NONE',  ( 15.39229341877100232, -8.812225371893999792, -7.562487140343000291 ) ) ;
#25931 = DIRECTION ( 'NONE',  ( 1.000000000000000000, 0.000000000000000000, 0.000000000000000000 ) ) ;
#25932 = VERTEX_POINT ( 'NONE', #38070 ) ;
#25933 = VECTOR ( 'NONE', #56370, 1000.000000000000114 ) ;
#25934 = CARTESIAN_POINT ( 'NONE',  ( 12.57406965100004115, -0.5808252089135508278, 12.68211610572158676 ) ) ;
#25935 = DIRECTION ( 'NONE',  ( -1.000000000000000000, 0.000000000000000000, 0.000000000000000000 ) ) ;
#25936 = AXIS2_PLACEMENT_3D ( 'NONE', #4923, #58407, #53167 ) ;
#25937 = CARTESIAN_POINT ( 'NONE',  ( 9.571967469951999874, -4.084684048989999816, 8.946621592834999248 ) ) ;
#25938 = CARTESIAN_POINT ( 'NONE',  ( 9.199088727410998700, 2.999102593977000186, 7.416055476975279781 ) ) ;
#25939 = DIRECTION ( 'NONE',  ( 0.000000000000000000, -0.9916377111174248249, -0.1290528957048032721 ) ) ;
#25940 = CARTESIAN_POINT ( 'NONE',  ( 12.24392764853882909, -2.776000094621844383, 13.61105252602849269 ) ) ;
#25941 = CARTESIAN_POINT ( 'NONE',  ( 23.63922860583116403, -3.363517752404959538, 13.53948175984613123 ) ) ;
#25942 = CARTESIAN_POINT ( 'NONE',  ( 24.30000561190290043, 3.240508259137445446, 12.09374146544330486 ) ) ;
#25943 = ORIENTED_EDGE ( 'NONE', *, *, #2602, .F. ) ;
#25944 = CARTESIAN_POINT ( 'NONE',  ( 4.534857654310999742, 0.1089978199666000042, -1.270785081792999982 ) ) ;
#25945 = CARTESIAN_POINT ( 'NONE',  ( 9.858596320338998353, -5.184381781355999586, -7.016653143730500197 ) ) ;
#25946 = CARTESIAN_POINT ( 'NONE',  ( 9.814967517147769271, -2.649990781018497721, -7.499998108648967765 ) ) ;
#25947 = CARTESIAN_POINT ( 'NONE',  ( 11.31524174883999834, -4.028418853626810403, 6.466884287543999577 ) ) ;
#25948 = CARTESIAN_POINT ( 'NONE',  ( 18.17231130205936651, 2.401422691383823249, -12.47401593597049363 ) ) ;
#25949 = CARTESIAN_POINT ( 'NONE',  ( 8.737804660583998739, 4.491756428607999396, -5.831236541471000123 ) ) ;
#25950 = CARTESIAN_POINT ( 'NONE',  ( 18.16560600475770570, 2.633677672902523970, 12.41941284449930549 ) ) ;
#25951 = ADVANCED_FACE ( 'NONE', ( #12202 ), #59396, .T. ) ;
#25952 = CARTESIAN_POINT ( 'NONE',  ( 7.100000000000000533, 0.000000000000000000, 0.000000000000000000 ) ) ;
#25953 = FACE_OUTER_BOUND ( 'NONE', #45755, .T. ) ;
#25954 = CARTESIAN_POINT ( 'NONE',  ( 11.07691935321000010, -3.101896674955000321, -8.926549689995999515 ) ) ;
#25955 = CARTESIAN_POINT ( 'NONE',  ( 0.2000000000000000389, 1.649999999999999911, 0.000000000000000000 ) ) ;
#25956 = B_SPLINE_CURVE_WITH_KNOTS ( 'NONE', 3,
 ( #40425, #13534, #18773, #8275, #61751, #45344, #29621, #50581, #50924, #55830, #2683, #24010, #66653, #34853, #42156, #42462, #67986, #25344, #15200, #47021, #58880, #51910 ),
 .UNSPECIFIED., .F., .F.,
 ( 4, 2, 2, 2, 2, 2, 2, 2, 2, 2, 4 ),
 ( 0.000000000000000000, 0.1250000000000000278, 0.2500000000000000555, 0.3750000000000001110, 0.5000000000000001110, 0.5625000000000001110, 0.6250000000000001110, 0.6875000000000001110, 0.7500000000000002220, 0.8750000000000001110, 1.000000000000000000 ),
 .UNSPECIFIED. ) ;
#25957 = EDGE_CURVE ( 'NONE', #24787, #56474, #49981, .T. ) ;
#25958 = CARTESIAN_POINT ( 'NONE',  ( 10.90454231406000041, -5.099691312770999296, -5.130383474399000221 ) ) ;
#25959 = EDGE_CURVE ( 'NONE', #39911, #48489, #19138, .T. ) ;
#25960 = DIRECTION ( 'NONE',  ( 0.000000000000000000, -0.7158784314710769925, 0.6982249432342777506 ) ) ;
#25961 = CARTESIAN_POINT ( 'NONE',  ( 9.202182965154866778, -2.714244241233930044, 7.027734220012900934 ) ) ;
#25962 = CARTESIAN_POINT ( 'NONE',  ( 23.54905712943500262, 13.36550135992999877, -4.294179668706000541 ) ) ;
#25963 = B_SPLINE_CURVE_WITH_KNOTS ( 'NONE', 3,
 ( #46187, #2499, #67497, #34330, #45505, #51426, #19615, #33979, #56334, #2166, #66818, #61917, #55300, #7395, #40593, #8438, #28742, #61235, #13351, #7749, #3521, #34676 ),
 .UNSPECIFIED., .F., .F.,
 ( 4, 2, 2, 1, 2, 2, 2, 1, 1, 1, 2, 2, 4 ),
 ( 0.000000000000000000, 0.2499999999999992228, 0.3749999999999970024, 0.4374999999999989453, 0.4687499999999975575, 0.4999999999999961142, 0.6250000000000044409, 0.6875000000000058842, 0.7187500000000067724, 0.7343750000000085487, 0.7421875000000084377, 0.7500000000000083267, 1.000000000000000000 ),
 .UNSPECIFIED. ) ;
#25964 = ORIENTED_EDGE ( 'NONE', *, *, #18109, .T. ) ;
#25965 = CARTESIAN_POINT ( 'NONE',  ( 8.953620280414000376, 2.881930053949999682, -8.823338183322999129 ) ) ;
#25966 = CARTESIAN_POINT ( 'NONE',  ( 11.20287750876920008, -4.469200303112399908, 6.771886227364699806 ) ) ;
#25967 = VERTEX_POINT ( 'NONE', #22336 ) ;
#25968 = AXIS2_PLACEMENT_3D ( 'NONE', #34459, #45286, #40711 ) ;
#25969 = CARTESIAN_POINT ( 'NONE',  ( 12.99999999998900080, 12.39025855408000076, 1.832244667012999928 ) ) ;
#25970 = CARTESIAN_POINT ( 'NONE',  ( 18.20032535889732728, 2.850937372247256629, -13.70665064220730578 ) ) ;
#25971 = ORIENTED_EDGE ( 'NONE', *, *, #67630, .F. ) ;
#25972 = CARTESIAN_POINT ( 'NONE',  ( 11.01279632507519857, 4.624908853805600906, 6.341531314375999706 ) ) ;
#25973 = CARTESIAN_POINT ( 'NONE',  ( 8.745860841232000027, 4.178200486578000472, -5.608493638783999202 ) ) ;
#25974 = CARTESIAN_POINT ( 'NONE',  ( 10.16052890781999984, 2.899999999999999911, -6.152188490330000370 ) ) ;
#25975 = CARTESIAN_POINT ( 'NONE',  ( 11.60988784977536348, -4.851105903694400645, -7.451365240271489832 ) ) ;
#25976 = CARTESIAN_POINT ( 'NONE',  ( 12.31002172224689417, 0.3816054321151358120, -13.89295103374429452 ) ) ;
#25977 = CARTESIAN_POINT ( 'NONE',  ( 1.250973465874999802, -3.500000000000000000, 0.000000000000000000 ) ) ;
#25978 = CARTESIAN_POINT ( 'NONE',  ( 13.43887202961200167, 11.47449689335000045, 1.782105406474000064 ) ) ;
#25979 = ORIENTED_EDGE ( 'NONE', *, *, #5436, .T. ) ;
#25980 = CARTESIAN_POINT ( 'NONE',  ( 4.500000000000000000, 0.000000000000000000, 0.000000000000000000 ) ) ;
#25981 = CARTESIAN_POINT ( 'NONE',  ( 8.690229719593000723, 2.414630869937000046, -6.801495146585999407 ) ) ;
#25982 = ORIENTED_EDGE ( 'NONE', *, *, #35614, .F. ) ;
#25983 = EDGE_CURVE ( 'NONE', #38001, #12182, #23379, .T. ) ;
#25984 = AXIS2_PLACEMENT_3D ( 'NONE', #8085, #66808, #3180 ) ;
#25985 = CARTESIAN_POINT ( 'NONE',  ( 10.90421423234000109, 3.863780721621000058, -9.185084890147001246 ) ) ;
#25986 = ORIENTED_EDGE ( 'NONE', *, *, #39392, .F. ) ;
#25987 = DIRECTION ( 'NONE',  ( -1.000000000000000000, 0.000000000000000000, 0.000000000000000000 ) ) ;
#25988 = CARTESIAN_POINT ( 'NONE',  ( 18.07985789204857241, -2.160546346826200281, -12.52419258880425446 ) ) ;
#25989 = B_SPLINE_CURVE_WITH_KNOTS ( 'NONE', 3,
 ( #8135, #40627, #25237, #67880 ),
 .UNSPECIFIED., .F., .F.,
 ( 4, 4 ),
 ( 0.000000000000000000, 1.000000000000000000 ),
 .UNSPECIFIED. ) ;
#25990 = DIRECTION ( 'NONE',  ( -0.7071063750895308919, -0.7071071872833308847, 1.205024241302051880E-09 ) ) ;
#25991 = CARTESIAN_POINT ( 'NONE',  ( 18.18004831022864920, -2.496998393457253052, -12.45226267666597764 ) ) ;
#25992 = CARTESIAN_POINT ( 'NONE',  ( 8.550850940329604910, 3.105567053290974044, 6.047889655643520435 ) ) ;
#25993 = ORIENTED_EDGE ( 'NONE', *, *, #7003, .F. ) ;
#25994 = CARTESIAN_POINT ( 'NONE',  ( 12.70688507812400125, 11.81408563393000044, -3.326099274546999940 ) ) ;
#25995 = CARTESIAN_POINT ( 'NONE',  ( 17.99644948955100077, 11.78614875273999907, -3.442261952866000119 ) ) ;
#25996 = CARTESIAN_POINT ( 'NONE',  ( 7.976886985233528904, -5.078974948772455811, 8.328785302375353083 ) ) ;
#25997 = CARTESIAN_POINT ( 'NONE',  ( 8.923129650240840149, 3.341122914829670609, 8.358757503607597172 ) ) ;
#25998 = CARTESIAN_POINT ( 'NONE',  ( 9.295789158775001226, 5.835196551504000517, -7.008466539623000813 ) ) ;
#25999 = CARTESIAN_POINT ( 'NONE',  ( 18.38069952315600020, -3.381269036354999979, 12.09968217836000015 ) ) ;
#26000 = CARTESIAN_POINT ( 'NONE',  ( 9.766127544684000128, -4.735430008785999512, -8.791396910319001279 ) ) ;
#26001 = ORIENTED_EDGE ( 'NONE', *, *, #44809, .F. ) ;
#26002 = ORIENTED_EDGE ( 'NONE', *, *, #68605, .T. ) ;
#26003 = CARTESIAN_POINT ( 'NONE',  ( 9.816185841232000442, 2.656512020013999997, -7.884832994446999699 ) ) ;
#26004 = ADVANCED_FACE ( 'NONE', ( #43331 ), #17087, .F. ) ;
#26005 = DIRECTION ( 'NONE',  ( -1.000000000000000000, 0.000000000000000000, 0.000000000000000000 ) ) ;
#26006 = DIRECTION ( 'NONE',  ( -0.7660444431221081762, 4.730466324156050957E-08, -0.6427876096828072372 ) ) ;
#26007 = CARTESIAN_POINT ( 'NONE',  ( 5.969609839683333696, 0.1963495408493571015, 1.500000000000000444 ) ) ;
#26008 = B_SPLINE_CURVE_WITH_KNOTS ( 'NONE', 3,
 ( #56983, #30425, #41937, #15023 ),
 .UNSPECIFIED., .F., .F.,
 ( 4, 4 ),
 ( 0.000000000000000000, 1.000000000000000000 ),
 .UNSPECIFIED. ) ;
#26009 = B_SPLINE_CURVE_WITH_KNOTS ( 'NONE', 3,
 ( #40688, #8535, #35795, #51863, #68276, #36132 ),
 .UNSPECIFIED., .F., .F.,
 ( 4, 2, 4 ),
 ( 0.000000000000000000, 0.5000000000000000000, 1.000000000000000000 ),
 .UNSPECIFIED. ) ;
#26010 = CARTESIAN_POINT ( 'NONE',  ( 11.67766954483535891, 4.715882430684499305, -6.395429936871999566 ) ) ;
#26011 = CARTESIAN_POINT ( 'NONE',  ( 8.851468108405999402, 4.834201109053600121, -7.736255015838599647 ) ) ;
#26013 = CARTESIAN_POINT ( 'NONE',  ( 17.55505043854143565, 3.125000000000000000, 12.28373071562070074 ) ) ;
#26012 = CARTESIAN_POINT ( 'NONE',  ( 10.10435508232799862, -4.449513475323099598, 8.398209294002699110 ) ) ;
#26014 = CARTESIAN_POINT ( 'NONE',  ( 7.540373275913000661, -2.929987504175003199, 6.557984262489997995 ) ) ;
#26015 = ORIENTED_EDGE ( 'NONE', *, *, #64655, .F. ) ;
#26016 = CARTESIAN_POINT ( 'NONE',  ( 9.852263540182327972, 2.907767014557178342, -6.870476274536370553 ) ) ;
#26017 = CARTESIAN_POINT ( 'NONE',  ( 10.33329075818000042, -3.361960872129000411, -4.712792984770999283 ) ) ;
#26018 = CARTESIAN_POINT ( 'NONE',  ( 10.16562143724499911, 4.849675135054999586, 8.456261759323901117 ) ) ;
#26019 = CARTESIAN_POINT ( 'NONE',  ( 6.983163067140000457, -12.13278666557000030, -3.076795749344999997 ) ) ;
#26020 = CARTESIAN_POINT ( 'NONE',  ( 10.68403590588000007, -5.436611040123999317, 8.578433628717998971 ) ) ;
#26021 = CARTESIAN_POINT ( 'NONE',  ( 17.69835410961234601, 3.108690103397766080, -12.28870081725901464 ) ) ;
#26022 = CARTESIAN_POINT ( 'NONE',  ( 16.39965637475000193, -3.313349101483999970, -11.22428178643999885 ) ) ;
#26023 = CARTESIAN_POINT ( 'NONE',  ( 13.89314246895800231, 8.838637615320999785, 7.948101024408999571 ) ) ;
#26024 = CARTESIAN_POINT ( 'NONE',  ( 7.591287949680001645, -4.587787988499997915, 6.499994349715005448 ) ) ;
#26025 = VECTOR ( 'NONE', #28390, 1000.000000000000000 ) ;
#26026 = CARTESIAN_POINT ( 'NONE',  ( 10.14124205625000030, -4.360201998293100623, -8.437601616732200327 ) ) ;
#26027 = CARTESIAN_POINT ( 'NONE',  ( 10.91476354018331030, -5.217465845835395299, 7.172815144550902744 ) ) ;
#26028 = CARTESIAN_POINT ( 'NONE',  ( 11.07529832096848210, -4.746004694577873551, 7.955594773867785463 ) ) ;
#26029 = CONICAL_SURFACE ( 'NONE', #11546, 11.75017108327000059, 0.7854127224616339609 ) ;
#26030 = CARTESIAN_POINT ( 'NONE',  ( 5.613892321701079879, 12.94560306677573003, -2.448221637638912540 ) ) ;
#26031 = CARTESIAN_POINT ( 'NONE',  ( 18.46714228073847863, -2.893782244577476792, -11.28496185859584067 ) ) ;
#26032 = EDGE_LOOP ( 'NONE', ( #47757, #44084 ) ) ;
#26033 = B_SPLINE_CURVE_WITH_KNOTS ( 'NONE', 3,
 ( #34539, #68041, #35221, #46389, #14915, #36237 ),
 .UNSPECIFIED., .F., .F.,
 ( 4, 2, 4 ),
 ( 0.000000000000000000, 0.5000000000000000000, 1.000000000000000000 ),
 .UNSPECIFIED. ) ;
#26034 = CARTESIAN_POINT ( 'NONE',  ( 12.18402519556254582, 0.07112609253419313604, -12.69973757146476778 ) ) ;
#26035 = CARTESIAN_POINT ( 'NONE',  ( 12.19317846011760231, -2.372225799441026961, -12.48041235929229131 ) ) ;
#26036 = CARTESIAN_POINT ( 'NONE',  ( 25.60000000000000142, 0.000000000000000000, 0.000000000000000000 ) ) ;
#26037 = CARTESIAN_POINT ( 'NONE',  ( 24.62774583285499830, 3.462210234181999802, -12.08748376425999993 ) ) ;
#26038 = CARTESIAN_POINT ( 'NONE',  ( 1.780140132541583320, -3.408904368339108260, 0.9161175952574674985 ) ) ;
#26039 = ORIENTED_EDGE ( 'NONE', *, *, #42138, .F. ) ;
#26040 = CARTESIAN_POINT ( 'NONE',  ( 5.543549751428999528, 1.090514925437999993, -0.4404064970261999945 ) ) ;
#26041 = ADVANCED_FACE ( 'NONE', ( #60781 ), #51345, .F. ) ;
#26042 = SHAPE_DEFINITION_REPRESENTATION ( #67327, #60856 ) ;
#26043 = EDGE_CURVE ( 'NONE', #18846, #31306, #43847, .T. ) ;
#26044 = CARTESIAN_POINT ( 'NONE',  ( 11.43345123989529810, -3.459769760840400110, -8.543317325199000223 ) ) ;
#26045 = CARTESIAN_POINT ( 'NONE',  ( 17.96717518398639157, 0.4698982333288769242, 12.68829846774584702 ) ) ;
#26046 = CARTESIAN_POINT ( 'NONE',  ( 12.95917414208900098, -11.49387908994000007, -1.654391991822000030 ) ) ;
#26047 = CARTESIAN_POINT ( 'NONE',  ( 11.49999672495000169, -10.14910021683508390, 5.848045769722698850 ) ) ;
#26048 = CARTESIAN_POINT ( 'NONE',  ( 11.48522412107029922, 4.047131449166419870, -6.609122077774299164 ) ) ;
#26049 = EDGE_LOOP ( 'NONE', ( #44379, #40705, #24297, #8605 ) ) ;
#26050 = DIRECTION ( 'NONE',  ( 0.000000000000000000, -0.7614089499631909730, 0.6482718649732925886 ) ) ;
#26051 = EDGE_LOOP ( 'NONE', ( #43692, #40036, #66369, #33886, #54597 ) ) ;
#26052 = CARTESIAN_POINT ( 'NONE',  ( 7.601545473805123798, -3.171576391775400516, 8.578950414869172647 ) ) ;
#26053 = CARTESIAN_POINT ( 'NONE',  ( 8.855418146794999501, -5.633481712366999794, 7.451234046297000368 ) ) ;
#26054 = CARTESIAN_POINT ( 'NONE',  ( 15.84051303026600266, 8.692957937327999929, 7.975472622866001338 ) ) ;
#26055 = VERTEX_POINT ( 'NONE', #8164 ) ;
#26056 = CARTESIAN_POINT ( 'NONE',  ( 8.668369459057998938, 3.037916315484999963, -6.050520490110999461 ) ) ;
#26057 = CARTESIAN_POINT ( 'NONE',  ( 8.318670280409000028, 5.452311718892000059, -8.444358433472999081 ) ) ;
#26058 = DIRECTION ( 'NONE',  ( 1.000000000000000000, 0.000000000000000000, 0.000000000000000000 ) ) ;
#26059 = CARTESIAN_POINT ( 'NONE',  ( 9.492233239867587713, 4.893451691336926146, 8.512174158741519392 ) ) ;
#26060 = VERTEX_POINT ( 'NONE', #28819 ) ;
#26061 = CARTESIAN_POINT ( 'NONE',  ( 10.37373728961999930, -2.215269876326000364, 7.703982265807999497 ) ) ;
#26062 = AXIS2_PLACEMENT_3D ( 'NONE', #19612, #20292, #57011 ) ;
#26063 = CARTESIAN_POINT ( 'NONE',  ( 25.48313547908499999, 11.09945010898000106, -3.317479108978999669 ) ) ;
#26064 = CYLINDRICAL_SURFACE ( 'NONE', #53945, 1.350000000000000089 ) ;
#26065 = ORIENTED_EDGE ( 'NONE', *, *, #39009, .T. ) ;
#26066 = EDGE_CURVE ( 'NONE', #62430, #20015, #12458, .T. ) ;
#26067 = AXIS2_PLACEMENT_3D ( 'NONE', #29301, #3730, #61782 ) ;
#26068 = CARTESIAN_POINT ( 'NONE',  ( 10.99245660749474141, -5.807287262094808611, -4.970960764622379457 ) ) ;
#26069 = EDGE_LOOP ( 'NONE', ( #11767, #59169, #42308, #68160, #5689, #276 ) ) ;
#26070 = CARTESIAN_POINT ( 'NONE',  ( 23.64563777841849301, -10.02996334016318514, 9.685372740697550498 ) ) ;
#26071 = CARTESIAN_POINT ( 'NONE',  ( 11.01356641589999974, 2.786433584103999994, 6.253463831328000211 ) ) ;
#26072 = EDGE_CURVE ( 'NONE', #27235, #41308, #29158, .T. ) ;
#26073 = FACE_OUTER_BOUND ( 'NONE', #62716, .T. ) ;
#26074 = CARTESIAN_POINT ( 'NONE',  ( 8.002383708823000319, 5.117451078405999887, -6.702236199791999915 ) ) ;
#26075 = DIRECTION ( 'NONE',  ( -3.254772980312840162E-06, -0.9999999999757510638, -6.156644133330701524E-06 ) ) ;
#26076 = CARTESIAN_POINT ( 'NONE',  ( 12.24873136391192041, 2.785023419893231544, 13.60881341097601549 ) ) ;
#26077 = EDGE_LOOP ( 'NONE', ( #8698, #46529, #5043, #37841, #56706, #68972 ) ) ;
#26078 = CARTESIAN_POINT ( 'NONE',  ( 7.750036073563001615, -5.085252754069001568, 6.546627699621002883 ) ) ;
#26079 = VERTEX_POINT ( 'NONE', #50466 ) ;
#26080 = CARTESIAN_POINT ( 'NONE',  ( 9.444315208305999576, 2.927258006877999641, 8.897018628538001295 ) ) ;
#26081 = CARTESIAN_POINT ( 'NONE',  ( 11.11477971959000044, 2.548217283716999848, -8.356742414746999970 ) ) ;
#26082 = AXIS2_PLACEMENT_3D ( 'NONE', #40423, #18771, #18426 ) ;
#26083 = DIRECTION ( 'NONE',  ( 0.000000000000000000, -0.1333333333333049098, 0.9910712498212373989 ) ) ;
#26084 = CARTESIAN_POINT ( 'NONE',  ( 12.58276127734161420, 1.915504326815320013, -13.78019217388817275 ) ) ;
#26085 = DIRECTION ( 'NONE',  ( -1.000000000000000000, 0.000000000000000000, 0.000000000000000000 ) ) ;
#26086 = PRESENTATION_STYLE_ASSIGNMENT (( #37262 ) ) ;
#26087 = CARTESIAN_POINT ( 'NONE',  ( 18.15598102061104768, 0.1720826668005503712, 13.89857125525885095 ) ) ;
#26088 = CIRCLE ( 'NONE', #36162, 11.84999999999999964 ) ;
#26089 = CARTESIAN_POINT ( 'NONE',  ( 18.11689869022392330, 0.2739455836253519294, 13.89636968673578288 ) ) ;
#26090 = VERTEX_POINT ( 'NONE', #18657 ) ;
#26091 = CARTESIAN_POINT ( 'NONE',  ( 12.70148458879910258, 0.6166668696481631962, 13.88158203759213549 ) ) ;
#26092 = B_SPLINE_CURVE_WITH_KNOTS ( 'NONE', 3,
 ( #9706, #26144, #57957, #31052 ),
 .UNSPECIFIED., .F., .F.,
 ( 4, 4 ),
 ( 0.000000000000000000, 1.000000000000000000 ),
 .UNSPECIFIED. ) ;
#26093 = CARTESIAN_POINT ( 'NONE',  ( 11.68272066707849888, -2.906477115133000222, 8.161456030935699602 ) ) ;
#26094 = CARTESIAN_POINT ( 'NONE',  ( 10.53019352383165952, 2.722060504686575122, -8.693776886016852501 ) ) ;
#26095 = CARTESIAN_POINT ( 'NONE',  ( 15.66944243593800046, 9.081775842407999733, 8.276637282895999093 ) ) ;
#26096 = CARTESIAN_POINT ( 'NONE',  ( 7.512831853207000421, -5.524126964933000927, 6.910359834012999691 ) ) ;
#26098 = CARTESIAN_POINT ( 'NONE',  ( 12.70851731079302738, 1.792711832343931277, -13.88474979353736316 ) ) ;
#26097 = CARTESIAN_POINT ( 'NONE',  ( 9.571961069101000419, 4.084683332033999470, 8.946609345378000455 ) ) ;
#26099 = CARTESIAN_POINT ( 'NONE',  ( 10.89149144726329865, 3.340422662105400065, -6.569275630703699242 ) ) ;
#26100 = CARTESIAN_POINT ( 'NONE',  ( 5.099999999768000336, -1.199999999999999956, 9.776630298829998011 ) ) ;
#26101 = CARTESIAN_POINT ( 'NONE',  ( 9.146417874593998576, 3.202096358337300330, -7.839201596587598964 ) ) ;
#26102 = CARTESIAN_POINT ( 'NONE',  ( 18.27863132999452134, 0.04649795050485548698, 12.59991969135870349 ) ) ;
#26103 = B_SPLINE_SURFACE_WITH_KNOTS ( 'NONE', 3, 3, ( 
 ( #64047, #37492, #2849, #7403 ),
 ( #50753, #34338, #50406, #60549 ),
 ( #66474, #28748, #33642, #34684 ),
 ( #12656, #44827, #39224, #1471 ),
 ( #39924, #49712, #50064, #54609 ),
 ( #18598, #65435, #11955, #38883 ),
 ( #66130, #12309, #17906, #23138 ),
 ( #18249, #33987, #44489, #60205 ),
 ( #23833, #17557, #61243, #39571 ) ),
 .UNSPECIFIED., .F., .F., .F.,
 ( 4, 1, 1, 1, 1, 1, 4 ),
 ( 4, 4 ),
 ( 0.02166927333700999908, 0.1666666666667000196, 0.3333333333333000081, 0.5000000000000000000, 0.6666666666667000474, 0.8333333333333000637, 0.9489586827378000411 ),
 ( -0.1917159053268999991, 1.191863452461999984 ),
 .UNSPECIFIED. ) ;
#26104 = CARTESIAN_POINT ( 'NONE',  ( 7.002579511120999634, -0.5447379795254000401, 1.456200539209999922 ) ) ;
#26105 = CARTESIAN_POINT ( 'NONE',  ( 18.50001572531400029, -2.908166856580999937, 12.18270046149000052 ) ) ;
#26106 = ORIENTED_EDGE ( 'NONE', *, *, #35370, .T. ) ;
#26107 = CARTESIAN_POINT ( 'NONE',  ( 8.855418146794999501, -5.633481712366999794, 7.451234046297000368 ) ) ;
#26108 = CARTESIAN_POINT ( 'NONE',  ( 9.221802827889566956, -2.874603711571219744, 6.749639981086952290 ) ) ;
#26109 = CARTESIAN_POINT ( 'NONE',  ( 23.60000000000000142, 2.548720605937000006, -12.21654710926000220 ) ) ;
#26110 = CARTESIAN_POINT ( 'NONE',  ( 0.9900191011665666618, 3.500000000000000888, -0.4817981237445647102 ) ) ;
#26111 = VERTEX_POINT ( 'NONE', #38592 ) ;
#26112 = CIRCLE ( 'NONE', #41730, 1.449999999999999956 ) ;
#26113 = CARTESIAN_POINT ( 'NONE',  ( 18.12310803393399894, 3.320912951897000198, 11.92519506916999994 ) ) ;
#26114 = CARTESIAN_POINT ( 'NONE',  ( 11.68277869730536977, 3.468607053297499743, 8.547856079839998955 ) ) ;
#26115 = CARTESIAN_POINT ( 'NONE',  ( 10.96332971959000169, 5.283550306828000309, -8.592773337476000250 ) ) ;
#26116 = VERTEX_POINT ( 'NONE', #55721 ) ;
#26117 = CARTESIAN_POINT ( 'NONE',  ( 12.36861573454710417, -0.5743932053698046492, -12.58690132123599348 ) ) ;
#26118 = DIRECTION ( 'NONE',  ( 0.000000000000000000, 0.000000000000000000, -1.000000000000000000 ) ) ;
#26119 = CARTESIAN_POINT ( 'NONE',  ( 10.51810807141099779, 4.059045408506610109, 6.223352037434000117 ) ) ;
#26120 = CARTESIAN_POINT ( 'NONE',  ( 24.66807826070334286, 8.737531166019467221, -9.168167557861536920 ) ) ;
#26121 = DIRECTION ( 'NONE',  ( 1.000000000000000000, 0.000000000000000000, 0.000000000000000000 ) ) ;
#26122 = EDGE_LOOP ( 'NONE', ( #22627, #58314, #44970, #34136 ) ) ;
#26123 = LINE ( 'NONE', #47451, #18798 ) ;
#26124 = EDGE_CURVE ( 'NONE', #61390, #5573, #5752, .T. ) ;
#26125 = EDGE_CURVE ( 'NONE', #26585, #42419, #23897, .T. ) ;
#26126 = CARTESIAN_POINT ( 'NONE',  ( 8.163589158768997933, 3.344658122371999998, -5.716722540613000447 ) ) ;
#26127 = CARTESIAN_POINT ( 'NONE',  ( 8.097451241187362925, -4.501375107734432390, 5.833995739002847181 ) ) ;
#26128 = AXIS2_PLACEMENT_3D ( 'NONE', #16650, #25771, #37976 ) ;
#26129 = CARTESIAN_POINT ( 'NONE',  ( 11.01512623398999935, -8.057018824736999818, 6.941559373591999815 ) ) ;
#26130 = ORIENTED_EDGE ( 'NONE', *, *, #61179, .F. ) ;
#26131 = CARTESIAN_POINT ( 'NONE',  ( 16.13732479921000262, -3.901986904155000158, -11.94169104666999992 ) ) ;
#26132 = CARTESIAN_POINT ( 'NONE',  ( 11.40156680346000151, 11.68030187645999973, 1.636056047313999784 ) ) ;
#26133 = ORIENTED_EDGE ( 'NONE', *, *, #38112, .F. ) ;
#26134 = CARTESIAN_POINT ( 'NONE',  ( 10.03976354018233330, -3.672815144550900524, 6.282534154164603812 ) ) ;
#26135 = DIRECTION ( 'NONE',  ( 0.000000000000000000, 0.8648648648648717963, 0.5020047465136829867 ) ) ;
#26136 = CIRCLE ( 'NONE', #65195, 2.574999650349000024 ) ;
#26137 = ORIENTED_EDGE ( 'NONE', *, *, #64091, .F. ) ;
#26138 = CARTESIAN_POINT ( 'NONE',  ( 17.88582179699705677, 0.5306878043354081864, -13.88636785578042421 ) ) ;
#26139 = CARTESIAN_POINT ( 'NONE',  ( 9.578311703535998589, -4.818302824158000597, -8.808202952968999355 ) ) ;
#26140 = CARTESIAN_POINT ( 'NONE',  ( 10.39070086100999823, -3.082125293506999597, -4.654000461396999633 ) ) ;
#26141 = CARTESIAN_POINT ( 'NONE',  ( 11.64633327354034797, 3.135095881599500256, -6.934277916748599502 ) ) ;
#26142 = AXIS2_PLACEMENT_3D ( 'NONE', #34395, #8499, #61984 ) ;
#26143 = CARTESIAN_POINT ( 'NONE',  ( 11.39324174884020024, -4.032306468273969990, 6.325557131097000685 ) ) ;
#26144 = CARTESIAN_POINT ( 'NONE',  ( 24.39664795055900015, -12.09373373542098840, -3.240506187884208522 ) ) ;
#26145 = CARTESIAN_POINT ( 'NONE',  ( 10.92380110216399913, -4.973546009874400653, 8.094557215852098864 ) ) ;
#26146 = ORIENTED_EDGE ( 'NONE', *, *, #10142, .T. ) ;
#26147 = CARTESIAN_POINT ( 'NONE',  ( 7.897954719591000483, 3.608525622520999843, 5.913376237674000002 ) ) ;
#26148 = ORIENTED_EDGE ( 'NONE', *, *, #43451, .T. ) ;
#26149 = DIRECTION ( 'NONE',  ( 1.000000000000000000, 0.000000000000000000, 0.000000000000000000 ) ) ;
#26150 = CARTESIAN_POINT ( 'NONE',  ( 9.385311019873999072, -4.135077143711000325, 9.175520401071999288 ) ) ;
#26151 = CARTESIAN_POINT ( 'NONE',  ( 11.79999999116810727, 3.511856242852833265, -11.95218832016636945 ) ) ;
#26152 = ORIENTED_EDGE ( 'NONE', *, *, #30312, .T. ) ;
#26153 = CARTESIAN_POINT ( 'NONE',  ( 12.22372692396752214, -2.729759399082356097, -12.39506432367437228 ) ) ;
#26154 = ADVANCED_FACE ( 'NONE', ( #50128 ), #39990, .F. ) ;
#26155 = LINE ( 'NONE', #20214, #22099 ) ;
#26156 = B_SPLINE_CURVE_WITH_KNOTS ( 'NONE', 3,
 ( #21675, #31497, #47579, #18, #21339, #68885, #21004, #42339 ),
 .UNSPECIFIED., .F., .F.,
 ( 4, 2, 2, 4 ),
 ( 0.000000000000000000, 0.2499999999999993894, 0.4999999999999987788, 1.000000000000000000 ),
 .UNSPECIFIED. ) ;
#26157 = CARTESIAN_POINT ( 'NONE',  ( 23.89320776801300283, -8.862674798062995407, 7.304122743114001004 ) ) ;
#26158 = CARTESIAN_POINT ( 'NONE',  ( 10.66476354018302608, 5.217465845835396188, 7.827184855449094592 ) ) ;
#26159 = CARTESIAN_POINT ( 'NONE',  ( 12.47114117431411628, -3.166196762519386088, -13.63727363649663360 ) ) ;
#26160 = CARTESIAN_POINT ( 'NONE',  ( 11.04333729122639873, -5.003122373830000136, -7.473611442402849470 ) ) ;
#26161 = DIRECTION ( 'NONE',  ( -1.000000000000000000, 0.000000000000000000, 0.000000000000000000 ) ) ;
#26162 = CARTESIAN_POINT ( 'NONE',  ( 18.28010889142763418, -2.506697083851611385, 12.34815906022512877 ) ) ;
#26163 = VERTEX_POINT ( 'NONE', #2234 ) ;
#26164 = ORIENTED_EDGE ( 'NONE', *, *, #50321, .T. ) ;
#26165 = CIRCLE ( 'NONE', #67474, 13.10000000000000320 ) ;
#26166 = CARTESIAN_POINT ( 'NONE',  ( 0.000000000000000000, 0.000000000000000000, 0.000000000000000000 ) ) ;
#26167 = CARTESIAN_POINT ( 'NONE',  ( 10.27427156480999848, -3.399999787207999447, 4.944156960757000618 ) ) ;
#26168 = CARTESIAN_POINT ( 'NONE',  ( 11.79999999523987420, -3.306280043674564517, 11.23952258183352093 ) ) ;
#26169 = CARTESIAN_POINT ( 'NONE',  ( 10.34224945431000009, 3.348985101650000296, -8.881460768006000706 ) ) ;
#26170 = CARTESIAN_POINT ( 'NONE',  ( 11.11486084871780022, 5.207010770456999893, -7.174999999999999822 ) ) ;
#26171 = CARTESIAN_POINT ( 'NONE',  ( 17.86131849338080713, 3.044913046804099466, 12.30775201372484062 ) ) ;
#26172 = CARTESIAN_POINT ( 'NONE',  ( 8.181902110542997875, 2.891006945229997793, -6.386045997152003828 ) ) ;
#26173 = FACE_OUTER_BOUND ( 'NONE', #2443, .T. ) ;
#26174 = VERTEX_POINT ( 'NONE', #38953 ) ;
#26175 = CARTESIAN_POINT ( 'NONE',  ( 10.98768521492000083, -5.299565686336999981, -4.945211137252000455 ) ) ;
#26176 = ORIENTED_EDGE ( 'NONE', *, *, #15474, .F. ) ;
#26177 = CARTESIAN_POINT ( 'NONE',  ( 18.29983863915590447, -0.9627070671913217081, -12.32514597913991850 ) ) ;
#26178 = CARTESIAN_POINT ( 'NONE',  ( 8.724265421554999733, -4.162714371335800578, -8.341695632489900092 ) ) ;
#26179 = CARTESIAN_POINT ( 'NONE',  ( 10.89227882974000039, 3.998355201738000630, 9.261308739708001170 ) ) ;
#26180 = CARTESIAN_POINT ( 'NONE',  ( 11.77745123989519982, -3.589787500396900199, 6.707778874960499849 ) ) ;
#26181 = CARTESIAN_POINT ( 'NONE',  ( 9.567560841232999991, 5.349936549139000519, -7.138437102151999447 ) ) ;
#26182 = TOROIDAL_SURFACE ( 'NONE', #66399, 12.20000000000000107, 0.6999999999999999556 ) ;
#26183 = CARTESIAN_POINT ( 'NONE',  ( 11.71210404293059959, 3.618181340822599790, -8.277504409418298792 ) ) ;
#26184 = CARTESIAN_POINT ( 'NONE',  ( 10.64118447801629941, 5.277702140407999565, -7.471828720557429193 ) ) ;
#26185 = CARTESIAN_POINT ( 'NONE',  ( 12.73299791870420528, -0.6209187240130109586, 12.67955909024709094 ) ) ;
#26186 = VECTOR ( 'NONE', #22955, 1000.000000000000000 ) ;
#26187 = EDGE_CURVE ( 'NONE', #64377, #29725, #64460, .T. ) ;
#26188 = EDGE_CURVE ( 'NONE', #49285, #22409, #44889, .T. ) ;
#26189 = CARTESIAN_POINT ( 'NONE',  ( 8.334295743503886911, 2.728512518251676511, -8.022178723330675609 ) ) ;
#26190 = CARTESIAN_POINT ( 'NONE',  ( 10.97864812944000157, 5.273131703456000352, 7.958028903907000462 ) ) ;
#26191 = CARTESIAN_POINT ( 'NONE',  ( 9.217200371204294029, -2.656565280586873357, 7.632967396875749877 ) ) ;
#26192 = VERTEX_POINT ( 'NONE', #1889 ) ;
#26193 = CARTESIAN_POINT ( 'NONE',  ( 8.631645280409999899, 3.826300099041999747, -9.055335252254000267 ) ) ;
#26194 = CARTESIAN_POINT ( 'NONE',  ( 0.000000000000000000, -0.7585797238574915058, 2.824612379753441260 ) ) ;
#26195 = CARTESIAN_POINT ( 'NONE',  ( 9.090964864865862083, 3.294502121218171098, 8.704449896995647862 ) ) ;
#26196 = CARTESIAN_POINT ( 'NONE',  ( 17.66658675203003881, 10.78295181803898295, -4.410266442050934543 ) ) ;
#26197 = CARTESIAN_POINT ( 'NONE',  ( 24.57788509281022016, 8.817303531626452084, 9.247882801663969587 ) ) ;
#26198 = CARTESIAN_POINT ( 'NONE',  ( 10.44841638348500013, -5.108333310975999630, -7.230023356477299323 ) ) ;
#26199 = VERTEX_POINT ( 'NONE', #12375 ) ;
#26200 = CARTESIAN_POINT ( 'NONE',  ( 5.602426839032973227, -12.13128594426829743, 3.749700506050578142 ) ) ;
#26201 = CARTESIAN_POINT ( 'NONE',  ( 10.26763456158959009, -5.237072593125339459, 8.927049273773194571 ) ) ;
#26204 = CARTESIAN_POINT ( 'NONE',  ( 14.03164332880499998, -9.396061154353999356, -8.198822423776999102 ) ) ;
#26203 = CARTESIAN_POINT ( 'NONE',  ( 8.523814158775000038, 4.920236664407999783, -6.448229650796999834 ) ) ;
#26202 = UNCERTAINTY_MEASURE_WITH_UNIT (LENGTH_MEASURE( 1.000000000000000082E-05 ), #53159, 'distance_accuracy_value', 'NONE');
#26205 = DIRECTION ( 'NONE',  ( 1.000000000000000000, 0.000000000000000000, 0.000000000000000000 ) ) ;
#26206 = EDGE_LOOP ( 'NONE', ( #15136, #38903, #65003, #6607 ) ) ;
#26207 = CARTESIAN_POINT ( 'NONE',  ( 10.73931450027999901, 2.763002390638999994, 6.801034082888999244 ) ) ;
#26208 = CARTESIAN_POINT ( 'NONE',  ( 17.87051611373836835, -1.960066664249855428, -13.77321273358845843 ) ) ;
#26209 = CARTESIAN_POINT ( 'NONE',  ( 10.72749279009019929, 3.774717370312400178, 6.663611138821799784 ) ) ;
#26210 = FACE_OUTER_BOUND ( 'NONE', #16583, .T. ) ;
#26211 = CARTESIAN_POINT ( 'NONE',  ( 9.053331853208000268, -5.618388245857000030, 7.727743016644000207 ) ) ;
#26212 = VERTEX_POINT ( 'NONE', #13423 ) ;
#26213 = CARTESIAN_POINT ( 'NONE',  ( 9.085767219592000288, 2.821863697211000055, 6.127145479358000024 ) ) ;
#26214 = EDGE_CURVE ( 'NONE', #69104, #53505, #59916, .T. ) ;
#26216 = CARTESIAN_POINT ( 'NONE',  ( 10.98168094034000042, 5.114619317328000569, 4.904815184644999881 ) ) ;
#26215 = CYLINDRICAL_SURFACE ( 'NONE', #9936, 0.5000000000000002220 ) ;
#26217 = CARTESIAN_POINT ( 'NONE',  ( 7.600254814611190568, -4.545917558585252038, 5.846023085849561873 ) ) ;
#26218 = DIRECTION ( 'NONE',  ( 1.000000000000000000, 0.000000000000000000, 0.000000000000000000 ) ) ;
#26219 = CARTESIAN_POINT ( 'NONE',  ( 23.73802576740300196, 3.438769318319999879, 13.34821028306000024 ) ) ;
#26220 = ORIENTED_EDGE ( 'NONE', *, *, #16130, .F. ) ;
#26221 = CARTESIAN_POINT ( 'NONE',  ( 9.591846873515667227, 4.999583552997727054, -8.268183399968643599 ) ) ;
#26222 = ADVANCED_FACE ( 'NONE', ( #24239 ), #34404, .T. ) ;
#26223 = CARTESIAN_POINT ( 'NONE',  ( 11.71564426047340035, -3.460037133261700149, 6.654192128557399499 ) ) ;
#26224 = CARTESIAN_POINT ( 'NONE',  ( 10.41185190929999926, 2.101586107686999938, 7.856266936613998553 ) ) ;
#26225 = CARTESIAN_POINT ( 'NONE',  ( 10.47303166480599934, 2.862083839376000416, 7.419769534118209720 ) ) ;
#26226 = COLOUR_RGB ( '', 0.40784314, 0.44705882, 0.49803922) ;
#26227 = ORIENTED_EDGE ( 'NONE', *, *, #14752, .T. ) ;
#26228 = CARTESIAN_POINT ( 'NONE',  ( 10.90000000000000036, 5.100000000000000533, -6.436740704805999691 ) ) ;
#26229 = CARTESIAN_POINT ( 'NONE',  ( 12.43945954148914801, 1.858853511423154137, -12.46213071393704830 ) ) ;
#26230 = CARTESIAN_POINT ( 'NONE',  ( 11.64256920625030034, -3.957769094421040190, 8.674127893687000324 ) ) ;
#26231 = CYLINDRICAL_SURFACE ( 'NONE', #42958, 0.6250000000000005551 ) ;
#26232 = CARTESIAN_POINT ( 'NONE',  ( 11.09999999999999964, 4.000000000000000000, 7.500000000000000000 ) ) ;
#26233 = CARTESIAN_POINT ( 'NONE',  ( 18.17041169247255183, 2.609942250314817525, -13.64953311053513296 ) ) ;
#26234 = ORIENTED_EDGE ( 'NONE', *, *, #12901, .F. ) ;
#26235 = CARTESIAN_POINT ( 'NONE',  ( 9.061090930683000977, -5.103946207352000108, -6.635696954776999945 ) ) ;
#26236 = CARTESIAN_POINT ( 'NONE',  ( 13.48771849468881534, -12.09748862696537763, -2.366366213948142949 ) ) ;
#26237 = VERTEX_POINT ( 'NONE', #28464 ) ;
#26238 = CARTESIAN_POINT ( 'NONE',  ( 9.427263540183332680, 3.370476274536375438, 6.407767014557179230 ) ) ;
#26239 = ADVANCED_FACE ( 'NONE', ( #65499 ), #39594, .F. ) ;
#26241 = CARTESIAN_POINT ( 'NONE',  ( 11.51518179236248862, 3.819003318705799899, 8.347076615013298451 ) ) ;
#26240 = VECTOR ( 'NONE', #61700, 1000.000000000000000 ) ;
#26242 = CARTESIAN_POINT ( 'NONE',  ( 27.09999999999999787, -4.026362576680999827E-13, -10.75000000000000000 ) ) ;
#26243 = CARTESIAN_POINT ( 'NONE',  ( 10.53865537815000053, 3.647234352455999584, -6.014129666051999834 ) ) ;
#26244 = CARTESIAN_POINT ( 'NONE',  ( 8.897621218489625505, -3.181327125463422334, -7.191281694476484354 ) ) ;
#26245 = CARTESIAN_POINT ( 'NONE',  ( 9.611390067472999732, -3.334847606888000193, 5.869121315726000709 ) ) ;
#26246 = CARTESIAN_POINT ( 'NONE',  ( 18.03335409833309910, -0.5406785836137845136, -12.58839662496522749 ) ) ;
#26247 = B_SPLINE_CURVE_WITH_KNOTS ( 'NONE', 3,
 ( #21568, #64212, #43248, #33458, #32083, #38341, #22261, #5497, #17012, #37995, #54425, #54077, #38696, #6527, #27870, #64899, #600, #11087 ),
 .UNSPECIFIED., .F., .F.,
 ( 4, 2, 2, 2, 2, 2, 2, 2, 4 ),
 ( 0.000000000000000000, 0.1250000000000001665, 0.2500000000000003331, 0.3750000000000001665, 0.5000000000000000000, 0.6249999999999996669, 0.7499999999999994449, 0.8749999999999996669, 1.000000000000000000 ),
 .UNSPECIFIED. ) ;
#26248 = CARTESIAN_POINT ( 'NONE',  ( 12.24916108029646544, 2.785825388795849289, -12.38039059668517794 ) ) ;
#26249 = CARTESIAN_POINT ( 'NONE',  ( 10.21462282008599942, -3.476853648246800432, -8.343818446627699004 ) ) ;
#26250 = CARTESIAN_POINT ( 'NONE',  ( 9.047982780412000992, 2.806082850903000026, 8.615880516515998622 ) ) ;
#26251 = VERTEX_POINT ( 'NONE', #13757 ) ;
#26252 = CARTESIAN_POINT ( 'NONE',  ( 5.500000000000000000, -0.2500000000000000000, -3.149999999999999911 ) ) ;
#26253 = CARTESIAN_POINT ( 'NONE',  ( 11.40221299665285670, 4.908904393308908709, 7.175011619880304004 ) ) ;
#26254 = CARTESIAN_POINT ( 'NONE',  ( 10.85685100254000091, -2.832432432432000269, -6.822293592207000934 ) ) ;
#26255 = DIRECTION ( 'NONE',  ( 0.000000000000000000, -0.7071067811865474617, 0.7071067811865474617 ) ) ;
#26256 = CARTESIAN_POINT ( 'NONE',  ( 12.47131944427643013, 1.869655113073432684, 13.87459630548518064 ) ) ;
#26257 = CARTESIAN_POINT ( 'NONE',  ( 11.14975833414749928, 3.203462856645999945, -7.825000000000000178 ) ) ;
#26258 = CARTESIAN_POINT ( 'NONE',  ( 9.260955151160263910, -2.777201709903842186, 6.918164468165489467 ) ) ;
#26259 = CARTESIAN_POINT ( 'NONE',  ( 8.849999778957998942, 4.000000000000000000, -8.499999833805500060 ) ) ;
#26260 = VERTEX_POINT ( 'NONE', #15127 ) ;
#26261 = CARTESIAN_POINT ( 'NONE',  ( 12.40905465428149057, -1.877469967418637919, 12.45933993000109119 ) ) ;
#26262 = CARTESIAN_POINT ( 'NONE',  ( 8.949822372493999367, -4.367693913457399546, -8.702849744394999476 ) ) ;
#26263 = CARTESIAN_POINT ( 'NONE',  ( 8.856851002545001350, 2.832432432432000269, -6.822293592207000934 ) ) ;
#26264 = CARTESIAN_POINT ( 'NONE',  ( 10.28315099603999982, -2.387772357283999725, 7.684266429524000408 ) ) ;
#26265 = CARTESIAN_POINT ( 'NONE',  ( 11.44903032197930060, -3.496160833528699996, 8.204588308639600314 ) ) ;
#26266 = B_SPLINE_SURFACE_WITH_KNOTS ( 'NONE', 3, 3, ( 
 ( #53084, #5184, #42594, #63904 ),
 ( #16017, #37346, #58670, #10770 ),
 ( #32115, #53431, #5528, #48182 ),
 ( #12160, #27903, #54459, #65631 ) ),
 .UNSPECIFIED., .F., .F., .F.,
 ( 4, 4 ),
 ( 4, 4 ),
 ( 0.7363163806532000422, 1.013499456067999960 ),
 ( -0.0005287450254680999126, 0.02696599629895000266 ),
 .UNSPECIFIED. ) ;
#26267 = CARTESIAN_POINT ( 'NONE',  ( 12.33591545429645464, 0.5485298171726803451, 12.58805670501782181 ) ) ;
#26268 = EDGE_CURVE ( 'NONE', #42155, #8229, #29831, .T. ) ;
#26269 = EDGE_CURVE ( 'NONE', #57358, #44634, #65576, .T. ) ;
#26270 = EDGE_CURVE ( 'NONE', #7001, #56519, #53304, .T. ) ;
#26271 = LINE ( 'NONE', #63657, #27604 ) ;
#26272 = CARTESIAN_POINT ( 'NONE',  ( 9.564884880418375701, 5.349923162331274185, -7.500006638304977713 ) ) ;
#26273 = CARTESIAN_POINT ( 'NONE',  ( 12.22616922475384094, 2.046442494456562677, 12.43271557125384597 ) ) ;
#26274 = CARTESIAN_POINT ( 'NONE',  ( -15.86200481174999943, 5.599999999999999645, 6.571291218949999902 ) ) ;
#26275 = EDGE_CURVE ( 'NONE', #27371, #56572, #56670, .T. ) ;
#26276 = CARTESIAN_POINT ( 'NONE',  ( 11.26487482311540056, 4.930401445321599851, -7.875904247640098887 ) ) ;
#26277 = CARTESIAN_POINT ( 'NONE',  ( 12.79999998712400178, 11.53033693765999779, -4.891431908114999949 ) ) ;
#26278 = CARTESIAN_POINT ( 'NONE',  ( 10.96332971959000169, 5.283550306828000309, -8.592773337476000250 ) ) ;
#26279 = CARTESIAN_POINT ( 'NONE',  ( 9.605304848515999083, 5.163382381259999931, -8.031907719862799055 ) ) ;
#26281 = CARTESIAN_POINT ( 'NONE',  ( 12.23610050212269584, 2.758887154479852111, 12.38747357478535704 ) ) ;
#26280 = CARTESIAN_POINT ( 'NONE',  ( 9.082867883171827472, -3.217326796159980518, -8.474986547786114599 ) ) ;
#26282 = DIRECTION ( 'NONE',  ( 0.000000000000000000, 0.000000000000000000, -1.000000000000000000 ) ) ;
#26283 = ORIENTED_EDGE ( 'NONE', *, *, #3401, .T. ) ;
#26284 = CARTESIAN_POINT ( 'NONE',  ( 12.33074081236783037, 0.4072355409458908171, 12.69121720795053676 ) ) ;
#26285 = CARTESIAN_POINT ( 'NONE',  ( 8.642077642326000841, 2.899999999999999911, 6.463854830420999953 ) ) ;
#26286 = CIRCLE ( 'NONE', #66454, 1.825000327749000117 ) ;
#26287 = CARTESIAN_POINT ( 'NONE',  ( 14.80000000000000071, 3.283787102340999464, -11.28049554847999936 ) ) ;
#26288 = CARTESIAN_POINT ( 'NONE',  ( 9.173759580228997734, 3.023107159668900312, 7.733500918284399894 ) ) ;
#26289 = CARTESIAN_POINT ( 'NONE',  ( 23.57795415946532458, -3.116628345736323968, -13.63414192076861831 ) ) ;
#26290 = CARTESIAN_POINT ( 'NONE',  ( 12.30838305349012352, -2.879539296179474572, 13.58560287457177829 ) ) ;
#26291 = CARTESIAN_POINT ( 'NONE',  ( 12.21057441422015089, 2.692955410687026596, 13.63058632110301360 ) ) ;
#26292 = CARTESIAN_POINT ( 'NONE',  ( 8.170084835020603009, 3.293757737277087205, 6.167713512348048432 ) ) ;
#26293 = VERTEX_POINT ( 'NONE', #3931 ) ;
#26294 = CARTESIAN_POINT ( 'NONE',  ( 5.174306403104999674, 0.3476685247999999895, 1.079832850831000002 ) ) ;
#26295 = CARTESIAN_POINT ( 'NONE',  ( 8.516151519676999015, -3.972335373863620234, -8.778912113473998247 ) ) ;
#26296 = DIRECTION ( 'NONE',  ( -0.7071067811865074937, -0.7011937492414073159, -0.09125418360182094291 ) ) ;
#26297 = CARTESIAN_POINT ( 'NONE',  ( 3.250973465878000290, -3.500000000000000000, 0.000000000000000000 ) ) ;
#26298 = CARTESIAN_POINT ( 'NONE',  ( 18.17889124921891053, 2.543048589645668489, -12.44148151073661701 ) ) ;
#26299 = CARTESIAN_POINT ( 'NONE',  ( 8.616995677562000466, 4.876077402042000131, 5.996974966532000018 ) ) ;
#26300 = DIRECTION ( 'NONE',  ( -1.000000000000000000, 0.000000000000000000, 0.000000000000000000 ) ) ;
#26301 = B_SPLINE_CURVE_WITH_KNOTS ( 'NONE', 3,
 ( #3500, #8416, #29759, #61894, #66795, #19594, #24837, #18567 ),
 .UNSPECIFIED., .F., .F.,
 ( 4, 2, 2, 4 ),
 ( 0.000000000000000000, 0.2500000000000013323, 0.5000000000000026645, 1.000000000000000000 ),
 .UNSPECIFIED. ) ;
#26302 = CARTESIAN_POINT ( 'NONE',  ( 17.79094441636205914, 1.825864066358003468, 13.88043842654293769 ) ) ;
#26303 = CARTESIAN_POINT ( 'NONE',  ( 17.55505043854143565, 3.248109929747637903, -13.61799478206225444 ) ) ;
#26304 = CARTESIAN_POINT ( 'NONE',  ( 24.59181005845499968, 12.25104096035999923, 3.053504809259000030 ) ) ;
#26305 = CARTESIAN_POINT ( 'NONE',  ( 23.60000000000000142, 2.548720605937000006, -12.21654710926000220 ) ) ;
#26306 = CARTESIAN_POINT ( 'NONE',  ( 11.50001544674999820, -8.431319371640864091, 9.354420476383705108 ) ) ;
#26307 = CARTESIAN_POINT ( 'NONE',  ( 11.55391045180431675, -2.870950512581995628, 6.885461205208883051 ) ) ;
#26308 = CARTESIAN_POINT ( 'NONE',  ( 11.59999999999999964, 3.182579051151299687, 7.825000000000000178 ) ) ;
#26309 = CARTESIAN_POINT ( 'NONE',  ( 24.25970694110000281, 12.09491440691000008, -3.326705949661999728 ) ) ;
#26310 = VERTEX_POINT ( 'NONE', #67912 ) ;
#26311 = CARTESIAN_POINT ( 'NONE',  ( 9.649770280412001355, 4.042991257420999851, -5.768106221333000327 ) ) ;
#26312 = CARTESIAN_POINT ( 'NONE',  ( 12.08487348028855024, -4.882707455860599843, 7.022738645480499642 ) ) ;
#26313 = ORIENTED_EDGE ( 'NONE', *, *, #67081, .T. ) ;
#26314 = VECTOR ( 'NONE', #37759, 1000.000000000000000 ) ;
#26315 = CARTESIAN_POINT ( 'NONE',  ( 5.500000000000000000, -1.315736040608999957, -10.71955403322999878 ) ) ;
#26316 = CARTESIAN_POINT ( 'NONE',  ( 11.03918313518939875, -4.707599264529200411, -8.394758848575399668 ) ) ;
#26317 = ORIENTED_EDGE ( 'NONE', *, *, #23600, .T. ) ;
#26318 = CARTESIAN_POINT ( 'NONE',  ( 11.68277869730536977, 3.468607053297499743, 8.547856079839998955 ) ) ;
#26319 = ADVANCED_FACE ( 'NONE', ( #46944 ), #61991, .T. ) ;
#26320 = CARTESIAN_POINT ( 'NONE',  ( 18.15531827655737018, 3.266808065264576566, -11.18265383028565196 ) ) ;
#26321 = CIRCLE ( 'NONE', #19633, 0.6999999999999992895 ) ;
#26322 = CARTESIAN_POINT ( 'NONE',  ( 8.559020380274406037, -4.705862675926076655, 8.704770267039673826 ) ) ;
#26323 = DIRECTION ( 'NONE',  ( 0.000000000000000000, 0.000000000000000000, -1.000000000000000000 ) ) ;
#26324 = CARTESIAN_POINT ( 'NONE',  ( 9.821013540182335078, -4.768183399968640934, -6.500416447002272946 ) ) ;
#26325 = CARTESIAN_POINT ( 'NONE',  ( 6.805184800867738915, -1.078970173958359258, 0.3488539053363355902 ) ) ;
#26326 = DIRECTION ( 'NONE',  ( 0.000000000000000000, 1.000000000000000000, 0.000000000000000000 ) ) ;
#26327 = ORIENTED_EDGE ( 'NONE', *, *, #11208, .F. ) ;
#26328 = CARTESIAN_POINT ( 'NONE',  ( 8.642358819840294970, 3.294576102360962988, 8.704493534904408136 ) ) ;
#26329 = ORIENTED_EDGE ( 'NONE', *, *, #58744, .T. ) ;
#26330 = AXIS2_PLACEMENT_3D ( 'NONE', #66509, #7790, #14076 ) ;
#26331 = CARTESIAN_POINT ( 'NONE',  ( 10.93769853197999886, 5.063116524846000388, -4.920828787216999345 ) ) ;
#26332 = SURFACE_SIDE_STYLE ('',( #9549 ) ) ;
#26333 = B_SPLINE_CURVE_WITH_KNOTS ( 'NONE', 3,
 ( #9002, #62144, #15287, #56561 ),
 .UNSPECIFIED., .F., .F.,
 ( 4, 4 ),
 ( 0.000000000000000000, 1.000000000000000000 ),
 .UNSPECIFIED. ) ;
#26334 = ORIENTED_EDGE ( 'NONE', *, *, #29648, .T. ) ;
#26335 = CARTESIAN_POINT ( 'NONE',  ( 9.301355082327999568, 3.427502311996299955, 8.643954013369999245 ) ) ;
#26336 = CARTESIAN_POINT ( 'NONE',  ( 17.89623257347368934, -3.023758741516315407, -12.31397229722846731 ) ) ;
#26337 = AXIS2_PLACEMENT_3D ( 'NONE', #23635, #34139, #66277 ) ;
#26338 = DIRECTION ( 'NONE',  ( 0.000000000000000000, 1.000000000000000000, 0.000000000000000000 ) ) ;
#26339 = CARTESIAN_POINT ( 'NONE',  ( 18.17974523562955369, -2.479825770562639864, -12.45623811636028044 ) ) ;
#26340 = CARTESIAN_POINT ( 'NONE',  ( 8.550260823830997836, 3.169363294249995633, 6.002781648002655679 ) ) ;
#26341 = ORIENTED_EDGE ( 'NONE', *, *, #27795, .F. ) ;
#26342 = CARTESIAN_POINT ( 'NONE',  ( 12.08926246520500136, 11.62544123506999938, -4.252388861798999997 ) ) ;
#26343 = CARTESIAN_POINT ( 'NONE',  ( 17.86320573775099874, 11.40784081139999984, -4.532785132108998916 ) ) ;
#26344 = CARTESIAN_POINT ( 'NONE',  ( 17.55505043854147118, -2.500000000000000000, -25.00000000000000000 ) ) ;
#26345 = CARTESIAN_POINT ( 'NONE',  ( 12.58176516051270255, 3.212719125873748194, -13.62638797003614144 ) ) ;
#26346 = CARTESIAN_POINT ( 'NONE',  ( 12.11873369409514112, -11.72532246831141478, 3.796278118051448658 ) ) ;
#26347 = CARTESIAN_POINT ( 'NONE',  ( 18.06894639827790527, 12.08549470499584189, -3.288878289815732714 ) ) ;
#26348 = CARTESIAN_POINT ( 'NONE',  ( 10.09454055528000005, -5.362855569781999954, -7.550030734599999960 ) ) ;
#26349 = ADVANCED_FACE ( 'NONE', ( #35766 ), #28773, .F. ) ;
#26350 = EDGE_CURVE ( 'NONE', #29839, #64219, #18994, .T. ) ;
#26351 = ORIENTED_EDGE ( 'NONE', *, *, #7566, .F. ) ;
#26352 = ORIENTED_EDGE ( 'NONE', *, *, #62808, .F. ) ;
#26353 = DIRECTION ( 'NONE',  ( 1.000000000000000000, 0.000000000000000000, 0.000000000000000000 ) ) ;
#26354 = FACE_OUTER_BOUND ( 'NONE', #26381, .T. ) ;
#26355 = EDGE_CURVE ( 'NONE', #67648, #5374, #4887, .T. ) ;
#26356 = EDGE_CURVE ( 'NONE', #718, #54751, #39954, .T. ) ;
#26357 = CARTESIAN_POINT ( 'NONE',  ( 11.36656541973662016, 12.29888939610234644, 1.513729097026024650 ) ) ;
#26358 = CARTESIAN_POINT ( 'NONE',  ( 5.990443173016668510, -0.1963495408493673433, 1.499999999999999334 ) ) ;
#26359 = CARTESIAN_POINT ( 'NONE',  ( 11.75203632436369894, 2.890282938442000127, -7.240848640331599917 ) ) ;
#26360 = CARTESIAN_POINT ( 'NONE',  ( 9.383380199233998908, 4.860242402105300563, -7.391875284387199763 ) ) ;
#26362 = CARTESIAN_POINT ( 'NONE',  ( 4.399687792926640917, 1.101481271771440174, -0.7758419216000916885 ) ) ;
#26361 = CARTESIAN_POINT ( 'NONE',  ( 10.56027973160900046, -3.909869487835140323, 8.500359330993999762 ) ) ;
#26363 = CARTESIAN_POINT ( 'NONE',  ( 10.89999913120000130, 0.3000008665460999757, -9.776630266016001158 ) ) ;
#26364 = VERTEX_POINT ( 'NONE', #46258 ) ;
#26365 = CARTESIAN_POINT ( 'NONE',  ( 10.17905590578999941, 2.899999999999999911, 6.571291218949999902 ) ) ;
#26366 = CARTESIAN_POINT ( 'NONE',  ( 8.332046967449000974, -2.867486995832002616, 6.314275746166007508 ) ) ;
#26367 = CARTESIAN_POINT ( 'NONE',  ( 9.988317406969001055, 4.237919115995800290, 6.243107450209000042 ) ) ;
#26368 = CARTESIAN_POINT ( 'NONE',  ( 11.09999999999999964, 6.593648130222000248, -5.598803514566000672 ) ) ;
#26369 = CARTESIAN_POINT ( 'NONE',  ( 10.46432358320999967, -2.042767395367000027, 7.723698102088000006 ) ) ;
#26370 = CARTESIAN_POINT ( 'NONE',  ( 18.16726790532411329, 2.625885335067867921, -12.42137433334332464 ) ) ;
#26371 = CARTESIAN_POINT ( 'NONE',  ( 16.15961700471899931, -3.514971253533999640, -11.06754630474000045 ) ) ;
#26372 = EDGE_CURVE ( 'NONE', #50813, #54112, #59128, .T. ) ;
#26373 = CARTESIAN_POINT ( 'NONE',  ( 13.99965637475000158, 8.819038952442999957, 7.693330608063000398 ) ) ;
#26374 = FACE_OUTER_BOUND ( 'NONE', #35014, .T. ) ;
#26375 = CARTESIAN_POINT ( 'NONE',  ( 9.889963142879999225, -3.151633609938700342, -7.321163726496699553 ) ) ;
#26376 = VECTOR ( 'NONE', #54924, 1000.000000000000227 ) ;
#26377 = CARTESIAN_POINT ( 'NONE',  ( 11.00851354018319483, -4.163624617374471093, 6.250000000000000888 ) ) ;
#26378 = CARTESIAN_POINT ( 'NONE',  ( 11.12452888361057113, -4.871957554394390044, 7.438521339935803667 ) ) ;
#26379 = DIRECTION ( 'NONE',  ( 1.000000000000000000, 0.000000000000000000, 0.000000000000000000 ) ) ;
#26380 = CARTESIAN_POINT ( 'NONE',  ( 7.749580121866000759, -3.139119547898000295, 6.460040744864000040 ) ) ;
#26381 = EDGE_LOOP ( 'NONE', ( #37566, #24361, #62777, #27427, #17352, #45340, #35270, #63319, #67127, #49783, #48314, #12207, #32026, #6677, #37762 ) ) ;
#26382 = CARTESIAN_POINT ( 'NONE',  ( 12.22381919988786692, -0.2299973361971402452, -12.69720198919504739 ) ) ;
#26383 = CARTESIAN_POINT ( 'NONE',  ( 23.60000000000000142, 12.92131265950320973, 5.202871703995182173 ) ) ;
#26384 = CARTESIAN_POINT ( 'NONE',  ( 8.216851002544000693, -2.832432432432000269, 6.822293592207000934 ) ) ;
#26385 = CARTESIAN_POINT ( 'NONE',  ( 3.499658142331559585, -2.179804560773650479, -2.476966527028495957 ) ) ;
#26386 = CARTESIAN_POINT ( 'NONE',  ( 7.100000000000000533, 11.84999999999999964, 0.000000000000000000 ) ) ;
#26387 = ORIENTED_EDGE ( 'NONE', *, *, #3989, .F. ) ;
#26388 = CARTESIAN_POINT ( 'NONE',  ( 5.644378390663000289, 0.7464156889442000731, 0.9088697504474000377 ) ) ;
#26389 = ITEM_DEFINED_TRANSFORMATION ( 'NONE', 'NONE', #61951,  #9676 ) ;
#26390 = DIRECTION ( 'NONE',  ( 1.000000000000000000, 0.000000000000000000, 0.000000000000000000 ) ) ;
#26391 = DIRECTION ( 'NONE',  ( 0.000000000000000000, 1.000000000000000000, 0.000000000000000000 ) ) ;
#26392 = LINE ( 'NONE', #21475, #45500 ) ;
#26393 = CARTESIAN_POINT ( 'NONE',  ( 7.961495038489999843, 3.389986099490999827, -6.279439026173999849 ) ) ;
#26394 = FACE_OUTER_BOUND ( 'NONE', #55296, .T. ) ;
#26395 = ORIENTED_EDGE ( 'NONE', *, *, #55406, .T. ) ;
#26396 = CARTESIAN_POINT ( 'NONE',  ( 9.687876499438001332, -5.912252057206999645, 7.772299417761000306 ) ) ;
#26397 = CARTESIAN_POINT ( 'NONE',  ( -2.444943969992999916E-05, 2.899969545325999931, 0.000000000000000000 ) ) ;
#26398 = VERTEX_POINT ( 'NONE', #63694 ) ;
#26399 = CARTESIAN_POINT ( 'NONE',  ( 10.84393020684900044, -5.250000000000000000, 7.500000000000000000 ) ) ;
#26400 = CARTESIAN_POINT ( 'NONE',  ( 9.406706853206999952, -3.705847642455000202, 9.096432253453999195 ) ) ;
#26401 = ADVANCED_FACE ( 'NONE', ( #68946 ), #59142, .T. ) ;
#26402 = FACE_OUTER_BOUND ( 'NONE', #46712, .T. ) ;
#26403 = ORIENTED_EDGE ( 'NONE', *, *, #13990, .T. ) ;
#26404 = CARTESIAN_POINT ( 'NONE',  ( 8.299720885770000223, 3.399999999999999911, -6.084164326786999588 ) ) ;
#26405 = CARTESIAN_POINT ( 'NONE',  ( 18.16002653635654696, 0.1622975231916133354, -12.69869204565246612 ) ) ;
#26406 = EDGE_CURVE ( 'NONE', #38239, #21130, #11246, .T. ) ;
#26407 = CARTESIAN_POINT ( 'NONE',  ( 10.98768491210000064, -8.067891622241001315, 6.818837029638999958 ) ) ;
#26408 = DIRECTION ( 'NONE',  ( 1.000000000000000000, -2.684047399077999465E-14, 2.619093452019999937E-10 ) ) ;
#26409 = ORIENTED_EDGE ( 'NONE', *, *, #37396, .T. ) ;
#26410 = CARTESIAN_POINT ( 'NONE',  ( 9.939319226872999735, -2.638101016021999978, 6.328632621050000573 ) ) ;
#26411 = CARTESIAN_POINT ( 'NONE',  ( 24.74446730232600089, 11.86528397834999815, -3.111028153312999756 ) ) ;
#26412 = CARTESIAN_POINT ( 'NONE',  ( 5.375859839684249408, 1.460959015002472494, 0.3926218265389233020 ) ) ;
#26413 = ORIENTED_EDGE ( 'NONE', *, *, #32524, .F. ) ;
#26414 = CIRCLE ( 'NONE', #61048, 1.000000000000000000 ) ;
#26415 = FACE_OUTER_BOUND ( 'NONE', #50151, .T. ) ;
#26416 = ORIENTED_EDGE ( 'NONE', *, *, #60222, .F. ) ;
#26417 = CARTESIAN_POINT ( 'NONE',  ( 4.941115032920667005, 0.7145727369020858921, 1.339076430445264032 ) ) ;
#26418 = CARTESIAN_POINT ( 'NONE',  ( 18.05194036310204098, 0.3791492162054622139, -13.89304085482682360 ) ) ;
#26419 = CARTESIAN_POINT ( 'NONE',  ( 17.77555300520474191, -0.5848996845204773587, -12.68186405703079167 ) ) ;
#26420 = AXIS2_PLACEMENT_3D ( 'NONE', #26484, #68080, #4796 ) ;
#26421 = CARTESIAN_POINT ( 'NONE',  ( 10.90000154029999990, -1.382741116750999977, -11.26545724788999969 ) ) ;
#26422 = CARTESIAN_POINT ( 'NONE',  ( 8.020642159885767342, 5.146218562000625774, -6.785513053889468793 ) ) ;
#26423 = CARTESIAN_POINT ( 'NONE',  ( 24.14647602714345709, 12.47136813241617226, 3.359330280457781814 ) ) ;
#26424 = VERTEX_POINT ( 'NONE', #10221 ) ;
#26425 = CARTESIAN_POINT ( 'NONE',  ( 10.28014141025500017, -3.582647672488299850, -8.243346240911998635 ) ) ;
#26426 = ORIENTED_EDGE ( 'NONE', *, *, #59507, .F. ) ;
#26427 = CARTESIAN_POINT ( 'NONE',  ( 9.611387933856001098, 3.334846092635999959, 5.869117602953000556 ) ) ;
#26428 = CARTESIAN_POINT ( 'NONE',  ( 11.08729332543999924, 2.258658230726000138, -7.034579402814999938 ) ) ;
#26429 = FACE_OUTER_BOUND ( 'NONE', #68119, .T. ) ;
#26430 = AXIS2_PLACEMENT_3D ( 'NONE', #43302, #16377, #59371 ) ;
#26431 = CARTESIAN_POINT ( 'NONE',  ( 9.070310841232000598, 5.361622798585000460, -7.185294144754000634 ) ) ;
#26432 = CARTESIAN_POINT ( 'NONE',  ( 3.774180895676000347, -3.540496567027000108, 0.007937750490802000097 ) ) ;
#26433 = FACE_OUTER_BOUND ( 'NONE', #1464, .T. ) ;
#26434 = CARTESIAN_POINT ( 'NONE',  ( 18.14024860221783442, -0.2197089332467998812, 13.89766776387047642 ) ) ;
#26435 = DIRECTION ( 'NONE',  ( -1.000000000000000000, 0.000000000000000000, 0.000000000000000000 ) ) ;
#26436 = B_SPLINE_CURVE_WITH_KNOTS ( 'NONE', 3,
 ( #3806, #52048, #4151, #42269, #25491, #53091, #25144, #40883, #46819, #68124 ),
 .UNSPECIFIED., .F., .F.,
 ( 4, 2, 2, 2, 4 ),
 ( 0.000000000000000000, 0.2500000000000000000, 0.5000000000000000000, 0.7500000000000000000, 1.000000000000000000 ),
 .UNSPECIFIED. ) ;
#26437 = ORIENTED_EDGE ( 'NONE', *, *, #58779, .T. ) ;
#26438 = CARTESIAN_POINT ( 'NONE',  ( 12.78642148534500045, -11.38816520531000087, 4.576060180783999343 ) ) ;
#26439 = EDGE_CURVE ( 'NONE', #8238, #66745, #67416, .T. ) ;
#26440 = CARTESIAN_POINT ( 'NONE',  ( 10.75149413291699929, -2.962184842772000337, 7.973529073237199505 ) ) ;
#26441 = ADVANCED_FACE ( 'NONE', ( #16833 ), #39024, .F. ) ;
#26442 = CARTESIAN_POINT ( 'NONE',  ( 18.02801947738339194, -0.4085868565494372717, -13.89191718360344119 ) ) ;
#26443 = CARTESIAN_POINT ( 'NONE',  ( 8.566230646795000681, -5.212258818969000451, 6.157189191035000064 ) ) ;
#26445 = DIRECTION ( 'NONE',  ( 0.000000000000000000, 0.001485959642859935011, -0.9999988959613604900 ) ) ;
#26444 = CARTESIAN_POINT ( 'NONE',  ( 6.875000000000000000, 5.574137966889000317, -8.240733100917999820 ) ) ;
#26446 = CARTESIAN_POINT ( 'NONE',  ( 10.54687750876899877, 3.382085645339300228, -8.458891008702400072 ) ) ;
#26447 = LINE ( 'NONE', #63489, #6807 ) ;
#26448 = CARTESIAN_POINT ( 'NONE',  ( 10.15958376188599921, 3.268856270222099791, -7.965979387614599894 ) ) ;
#26449 = CARTESIAN_POINT ( 'NONE',  ( 17.75589797987077745, -0.5919389804100247954, 12.68142457171642157 ) ) ;
#26450 = CARTESIAN_POINT ( 'NONE',  ( 6.907364441304000735, -0.7063073661229000155, -0.8851390247125999755 ) ) ;
#26451 = CARTESIAN_POINT ( 'NONE',  ( 18.49562053141630713, -2.998066116901991762, 12.16097201970263875 ) ) ;
#26452 = VERTEX_POINT ( 'NONE', #59833 ) ;
#26453 = CARTESIAN_POINT ( 'NONE',  ( 7.866206853207000194, -4.580607464247000493, 9.213361409141999303 ) ) ;
#26454 = CARTESIAN_POINT ( 'NONE',  ( 9.568039158772000619, 5.336630274082000192, -7.092011739486999922 ) ) ;
#26455 = DIRECTION ( 'NONE',  ( 0.000000000000000000, 1.000000000000000000, 0.000000000000000000 ) ) ;
#26456 = EDGE_CURVE ( 'NONE', #2243, #37337, #60535, .T. ) ;
#26457 = CARTESIAN_POINT ( 'NONE',  ( 10.99143984058640378, 5.686599839966610226, 4.947043824675725787 ) ) ;
#26458 = EDGE_LOOP ( 'NONE', ( #4032, #32854, #5025, #30353 ) ) ;
#26459 = AXIS2_PLACEMENT_3D ( 'NONE', #47419, #58245, #5104 ) ;
#26460 = CARTESIAN_POINT ( 'NONE',  ( 18.53936233968600078, 2.923364741758000207, 12.21823820824000073 ) ) ;
#26461 = AXIS2_PLACEMENT_3D ( 'NONE', #63360, #47303, #67234 ) ;
#26462 = CARTESIAN_POINT ( 'NONE',  ( 10.32169598648999909, 4.766524664146899681, 7.043598424555200133 ) ) ;
#26463 = CARTESIAN_POINT ( 'NONE',  ( 2.027882597155000521, 3.758808678259999869, 0.01395688117858999953 ) ) ;
#26464 = EDGE_LOOP ( 'NONE', ( #49420, #25451, #58843, #4300 ) ) ;
#26465 = FACE_OUTER_BOUND ( 'NONE', #10238, .T. ) ;
#26466 = CARTESIAN_POINT ( 'NONE',  ( 25.00269881440402386, -8.478843172797441596, 8.837112395074729676 ) ) ;
#26467 = CARTESIAN_POINT ( 'NONE',  ( 11.61759063708296047, 5.217265640542000149, 7.157757529645699890 ) ) ;
#26468 = CARTESIAN_POINT ( 'NONE',  ( 7.204799779090437006, -2.684882381560841580, 7.854227636469309992 ) ) ;
#26470 = CARTESIAN_POINT ( 'NONE',  ( 8.656823341231000057, 5.329437560656000272, 6.027391099688998999 ) ) ;
#26469 = VECTOR ( 'NONE', #9253, 1000.000000000000114 ) ;
#26471 = VERTEX_POINT ( 'NONE', #11939 ) ;
#26472 = DIRECTION ( 'NONE',  ( 1.000000000000000000, 0.000000000000000000, -7.847361993451999840E-14 ) ) ;
#26473 = CARTESIAN_POINT ( 'NONE',  ( 6.928179719591000207, 5.602143124542999786, -7.927308852422999763 ) ) ;
#26474 = CARTESIAN_POINT ( 'NONE',  ( 8.473482780583216467, -2.321348858116770941, 6.962478315320627331 ) ) ;
#26475 = CARTESIAN_POINT ( 'NONE',  ( 9.573392757686999488, -3.136549968260000210, 6.556157624301499176 ) ) ;
#26476 = ORIENTED_EDGE ( 'NONE', *, *, #58578, .F. ) ;
#26477 = CARTESIAN_POINT ( 'NONE',  ( 11.79999999471800010, 11.69117318561000118, 1.923227876431999883 ) ) ;
#26478 = CARTESIAN_POINT ( 'NONE',  ( 11.42387073792000152, 11.74429294849999827, 1.827310270344000065 ) ) ;
#26479 = ORIENTED_EDGE ( 'NONE', *, *, #17843, .T. ) ;
#26480 = CARTESIAN_POINT ( 'NONE',  ( 12.08055032392396555, 2.669683454821158097, -12.31540075205778528 ) ) ;
#26481 = CARTESIAN_POINT ( 'NONE',  ( 24.68356136276056390, -8.667369894679193720, -8.629863677887273710 ) ) ;
#26482 = DIRECTION ( 'NONE',  ( 0.000000000000000000, 0.000000000000000000, 1.000000000000000000 ) ) ;
#26483 = EDGE_LOOP ( 'NONE', ( #4191, #64979, #42729, #30496 ) ) ;
#26484 = CARTESIAN_POINT ( 'NONE',  ( 11.59999999999999964, 4.000000000000000000, 7.500000000000000000 ) ) ;
#26485 = AXIS2_PLACEMENT_3D ( 'NONE', #67239, #67582, #24607 ) ;
#26486 = CARTESIAN_POINT ( 'NONE',  ( 11.10612378248509913, 3.517039242046199998, -6.586279795136899651 ) ) ;
#26487 = EDGE_CURVE ( 'NONE', #15849, #44476, #57384, .T. ) ;
#26488 = DIRECTION ( 'NONE',  ( -0.000000000000000000, -0.000000000000000000, 1.000000000000000000 ) ) ;
#26489 = CARTESIAN_POINT ( 'NONE',  ( 8.784973378479026707, -4.855539494230036723, 9.057509731918708340 ) ) ;
#26490 = CARTESIAN_POINT ( 'NONE',  ( 11.23964560330029983, -3.608363763633400279, 8.716526793355999558 ) ) ;
#26491 = ORIENTED_EDGE ( 'NONE', *, *, #12810, .F. ) ;
#26492 = CARTESIAN_POINT ( 'NONE',  ( 9.053329719590999858, 5.618384167307999277, 7.727742442702000503 ) ) ;
#26493 = EDGE_LOOP ( 'NONE', ( #30054, #34886, #26632 ) ) ;
#26494 = CARTESIAN_POINT ( 'NONE',  ( 9.541846873516668381, 4.999583552997725278, -8.268183399968640046 ) ) ;
#26495 = CARTESIAN_POINT ( 'NONE',  ( 7.839808059622000336, -3.084082018960999871, 9.259837032825000591 ) ) ;
#26496 = CARTESIAN_POINT ( 'NONE',  ( 11.12484647810999938, 6.576551162614999946, -5.637922378081000829 ) ) ;
#26497 = ORIENTED_EDGE ( 'NONE', *, *, #57915, .F. ) ;
#26498 = CARTESIAN_POINT ( 'NONE',  ( 12.75302363333809019, -1.877081947669210660, -12.57507557223851080 ) ) ;
#26499 = CARTESIAN_POINT ( 'NONE',  ( 24.30000000000000071, -9.517611874540000017, -8.103398312166000039 ) ) ;
#26500 = CARTESIAN_POINT ( 'NONE',  ( 15.89979320885400327, -3.824231472901999496, -11.71686814605000038 ) ) ;
#26501 = CARTESIAN_POINT ( 'NONE',  ( 12.80505043854146940, -3.199698446519381179, -12.18695736643652516 ) ) ;
#26502 = CARTESIAN_POINT ( 'NONE',  ( 12.08109376178932948, -2.472831159707302273, -13.77990118939880126 ) ) ;
#26503 = CARTESIAN_POINT ( 'NONE',  ( 10.55518582084299872, -4.566724035220099509, -6.844925608615599621 ) ) ;
#26504 = CARTESIAN_POINT ( 'NONE',  ( 7.084133413226945564, 0.1731109259882732954, -1.315866092581484459 ) ) ;
#26505 = CARTESIAN_POINT ( 'NONE',  ( 17.90971610687751792, -3.107943374821394045, 12.21068061720392173 ) ) ;
#26506 = EDGE_LOOP ( 'NONE', ( #17572, #59269, #6950, #9990 ) ) ;
#26507 = ORIENTED_EDGE ( 'NONE', *, *, #28063, .F. ) ;
#26508 = DIRECTION ( 'NONE',  ( 1.000000000000000000, 0.000000000000000000, 0.000000000000000000 ) ) ;
#26509 = VECTOR ( 'NONE', #26296, 1000.000000000000114 ) ;
#26510 = DIRECTION ( 'NONE',  ( 0.000000000000000000, 0.000000000000000000, -1.000000000000000000 ) ) ;
#26511 = CARTESIAN_POINT ( 'NONE',  ( 16.00017105474300294, 4.418687638008000347E-13, 6.430411758629000588E-13 ) ) ;
#26512 = B_SPLINE_CURVE_WITH_KNOTS ( 'NONE', 3,
 ( #2571, #35095, #3261, #46610, #2914, #24929 ),
 .UNSPECIFIED., .F., .F.,
 ( 4, 2, 4 ),
 ( 0.000000000000000000, 0.5000000000000000000, 1.000000000000000000 ),
 .UNSPECIFIED. ) ;
#26513 = CARTESIAN_POINT ( 'NONE',  ( 10.00074698269999907, 2.373893144840999891, -7.962435130300000274 ) ) ;
#26514 = CARTESIAN_POINT ( 'NONE',  ( 12.79999999975700042, -11.86189249994999884, 3.298671769835999967 ) ) ;
#26515 = COLOUR_RGB ( '', 0.66274510, 0.83137255, 0.94901961) ;
#26516 = CARTESIAN_POINT ( 'NONE',  ( 18.16418420726525795, 2.358504521564765533, -12.48345420460929134 ) ) ;
#26517 = CARTESIAN_POINT ( 'NONE',  ( 24.42337838643000225, -12.73360400642000023, 3.018840435665000044 ) ) ;
#26518 = CARTESIAN_POINT ( 'NONE',  ( 17.74468889437873997, -1.784327658740600508, -12.47302143557414134 ) ) ;
#26519 = ORIENTED_EDGE ( 'NONE', *, *, #12146, .T. ) ;
#26520 = AXIS2_PLACEMENT_3D ( 'NONE', #42935, #54108, #16014 ) ;
#26521 = CARTESIAN_POINT ( 'NONE',  ( 8.880743402660417729, 5.552835561677609277, -8.364321471810635344 ) ) ;
#26522 = EDGE_CURVE ( 'NONE', #11630, #22321, #45152, .T. ) ;
#26523 = CARTESIAN_POINT ( 'NONE',  ( 18.29983863915590447, -1.925365884025486807, -12.21183829392446540 ) ) ;
#26524 = ADVANCED_FACE ( 'NONE', ( #60190 ), #28034, .F. ) ;
#26525 = DIRECTION ( 'NONE',  ( 1.000000000000000000, 0.000000000000000000, 0.000000000000000000 ) ) ;
#26526 = CARTESIAN_POINT ( 'NONE',  ( 10.57892463485000079, 4.649960478797999563, 5.681084732956000138 ) ) ;
#26527 = CARTESIAN_POINT ( 'NONE',  ( 10.90480513896000048, -3.220259576336399920, 7.933462475324499330 ) ) ;
#26528 = CARTESIAN_POINT ( 'NONE',  ( 18.26242787221299935, 2.744348664398000182, -11.56741553474000028 ) ) ;
#26529 = AXIS2_PLACEMENT_3D ( 'NONE', #10288, #58873, #43493 ) ;
#26530 = CARTESIAN_POINT ( 'NONE',  ( 11.44133594839949986, 4.569506585117100173, -6.847343244997600387 ) ) ;
#26531 = CARTESIAN_POINT ( 'NONE',  ( 12.24897804304629467, -0.2853680816562785827, 12.69568625917503013 ) ) ;
#26532 = CARTESIAN_POINT ( 'NONE',  ( 5.634466645576519106, -12.10031501007063603, -3.741403512701606537 ) ) ;
#26533 = CARTESIAN_POINT ( 'NONE',  ( 8.126005914336607461, 5.349985204051306731, -7.683689342979575621 ) ) ;
#26534 = AXIS2_PLACEMENT_3D ( 'NONE', #55832, #55485, #39062 ) ;
#26535 = CARTESIAN_POINT ( 'NONE',  ( 0.9681103717476999826, 3.205765437135000173, -1.404659375816999844 ) ) ;
#26536 = B_SPLINE_SURFACE_WITH_KNOTS ( 'NONE', 3, 3, ( 
 ( #40718, #8225, #7525, #23609 ),
 ( #44951, #19744, #66255, #14163 ),
 ( #18376, #24299, #29572, #39698 ),
 ( #50874, #2971, #8906, #66940 ),
 ( #13819, #29912, #35488, #3648 ),
 ( #51550, #24985, #46317, #41067 ),
 ( #12785, #5027, #63053, #4337 ),
 ( #62386, #25325, #67969, #25671 ),
 ( #35822, #42101, #26017, #9237 ),
 ( #20424, #15528, #21448, #31959 ),
 ( #14841, #68652, #47003, #36163 ) ),
 .UNSPECIFIED., .F., .F., .F.,
 ( 4, 1, 1, 1, 1, 1, 1, 1, 4 ),
 ( 4, 4 ),
 ( 0.5665910773458999738, 0.6250000000000000000, 0.6875000000000000000, 0.7500000000000000000, 0.8125000000000000000, 0.8750000000000000000, 0.9375000000000000000, 1.000000000000000000, 1.014356664780999839 ),
 ( -0.1686987264388999930, 1.168651125902999910 ),
 .UNSPECIFIED. ) ;
#26537 = ORIENTED_EDGE ( 'NONE', *, *, #46597, .T. ) ;
#26538 = CYLINDRICAL_SURFACE ( 'NONE', #38706, 0.6999999999999992895 ) ;
#26539 = CARTESIAN_POINT ( 'NONE',  ( 6.928578894554999756, -1.109280206285000236, -0.5774939165396000273 ) ) ;
#26540 = CARTESIAN_POINT ( 'NONE',  ( 5.500000000000000000, -13.04986661130000059, 1.811520473896000016 ) ) ;
#26541 = DIRECTION ( 'NONE',  ( -1.000000000000000000, 0.000000000000000000, 0.000000000000000000 ) ) ;
#26542 = EDGE_CURVE ( 'NONE', #48552, #8563, #47778, .T. ) ;
#26543 = LINE ( 'NONE', #32138, #12191 ) ;
#26544 = CARTESIAN_POINT ( 'NONE',  ( 11.45764291764649911, -5.132124077409000229, -7.360052904210999891 ) ) ;
#26545 = VERTEX_POINT ( 'NONE', #28732 ) ;
#26546 = DIRECTION ( 'NONE',  ( 1.000000000000000000, 0.000000000000000000, 0.000000000000000000 ) ) ;
#26547 = EDGE_CURVE ( 'NONE', #21198, #41719, #8087, .T. ) ;
#26548 = CARTESIAN_POINT ( 'NONE',  ( 7.099999886593999499, 12.39999890530000037, 0.000000000000000000 ) ) ;
#26550 = CARTESIAN_POINT ( 'NONE',  ( 9.073148997461000675, 5.167567567567999731, -6.822293592207000934 ) ) ;
#26549 = CARTESIAN_POINT ( 'NONE',  ( 8.564679719593000229, 4.146787477634999775, -5.941926545671999627 ) ) ;
#26551 = CARTESIAN_POINT ( 'NONE',  ( 3.358374205747110430, 1.670603451639867121, 2.796989605246705590 ) ) ;
#26552 = VERTEX_POINT ( 'NONE', #29080 ) ;
#26553 = CARTESIAN_POINT ( 'NONE',  ( 11.18484176840999922, 2.599663474744000169, 7.740674686800000259 ) ) ;
#26554 = CARTESIAN_POINT ( 'NONE',  ( 18.17246482408074471, -2.400822122662769065, -13.69396077230720721 ) ) ;
#26555 = CARTESIAN_POINT ( 'NONE',  ( 11.66287348028854964, 3.238044298475899918, 7.088026579158399620 ) ) ;
#26556 = CARTESIAN_POINT ( 'NONE',  ( 9.869049086607999399, -5.575175898444999945, 7.724300702620999104 ) ) ;
#26557 = CARTESIAN_POINT ( 'NONE',  ( 7.165495559622000243, -2.688354259407999880, 8.140021027181001401 ) ) ;
#26558 = ORIENTED_EDGE ( 'NONE', *, *, #54484, .T. ) ;
#26559 = CARTESIAN_POINT ( 'NONE',  ( 9.123551658772999673, 5.558938731259999599, 6.272977177425000050 ) ) ;
#26560 = VECTOR ( 'NONE', #45083, 1000.000000000000114 ) ;
#26562 = CARTESIAN_POINT ( 'NONE',  ( 10.53521345716899837, -3.075109701058799772, -8.340879262988799780 ) ) ;
#26561 = CARTESIAN_POINT ( 'NONE',  ( 10.94452754078378121, 4.508448539877488059, -6.788965764111623002 ) ) ;
#26563 = CARTESIAN_POINT ( 'NONE',  ( 7.706178870840924233, -5.757700323609271642, 7.628119760989433118 ) ) ;
#26564 = VECTOR ( 'NONE', #33627, 1000.000000000000000 ) ;
#26565 = CARTESIAN_POINT ( 'NONE',  ( 8.970944094206998898, 5.100000000000000533, 6.571291218949999902 ) ) ;
#26566 = CARTESIAN_POINT ( 'NONE',  ( 1.357018817589999982, 2.440310627160000134, 2.160132089918000098 ) ) ;
#26567 = ORIENTED_EDGE ( 'NONE', *, *, #65651, .F. ) ;
#26568 = CARTESIAN_POINT ( 'NONE',  ( 25.21375202814359540, -11.24065089990825506, -3.343241695434690630 ) ) ;
#26569 = CARTESIAN_POINT ( 'NONE',  ( 11.93302763632549990, -5.035790660926999784, 7.977941233841399971 ) ) ;
#26570 = CARTESIAN_POINT ( 'NONE',  ( 10.24477918374999952, 5.265206995764999398, 8.959504263949002123 ) ) ;
#26571 = AXIS2_PLACEMENT_3D ( 'NONE', #62568, #41940, #52076 ) ;
#26572 = CARTESIAN_POINT ( 'NONE',  ( 10.64533863405319991, 4.703785194191100416, 6.602238051205399749 ) ) ;
#26573 = ORIENTED_EDGE ( 'NONE', *, *, #21994, .F. ) ;
#26574 = B_SPLINE_CURVE_WITH_KNOTS ( 'NONE', 3,
 ( #1600, #65909, #22228, #11388 ),
 .UNSPECIFIED., .F., .F.,
 ( 4, 4 ),
 ( 0.7873984553934968433, 1.000000000000000000 ),
 .UNSPECIFIED. ) ;
#26575 = CARTESIAN_POINT ( 'NONE',  ( 9.269689158774999882, 3.135494838036999798, -8.598037907310999373 ) ) ;
#26576 = AXIS2_PLACEMENT_3D ( 'NONE', #34372, #29480, #13728 ) ;
#26577 = B_SPLINE_CURVE_WITH_KNOTS ( 'NONE', 3,
 ( #40581, #67485, #19950, #19607 ),
 .UNSPECIFIED., .F., .F.,
 ( 4, 4 ),
 ( 0.000000000000000000, 1.000000000000000000 ),
 .UNSPECIFIED. ) ;
#26578 = CARTESIAN_POINT ( 'NONE',  ( 12.11326330726100586, 2.264210275637937642, -12.39489744172470509 ) ) ;
#26579 = CARTESIAN_POINT ( 'NONE',  ( 12.26588784977539959, -5.120865761890000201, 7.564049652083489228 ) ) ;
#26580 = CARTESIAN_POINT ( 'NONE',  ( 11.03613257345000065, 2.777644159685000336, -5.022749861804999938 ) ) ;
#26581 = CARTESIAN_POINT ( 'NONE',  ( 18.12893921139219344, 2.747599606312327136, -13.61782120253283956 ) ) ;
#26582 = ORIENTED_EDGE ( 'NONE', *, *, #53518, .T. ) ;
#26583 = CARTESIAN_POINT ( 'NONE',  ( 15.82725884711995157, -9.380130419263611685, -8.300201155565218869 ) ) ;
#26584 = CARTESIAN_POINT ( 'NONE',  ( 11.09999999999999964, 4.000000000000000000, -7.500000000000000000 ) ) ;
#26585 = VERTEX_POINT ( 'NONE', #49004 ) ;
#26586 = CARTESIAN_POINT ( 'NONE',  ( 9.479346873516668381, 4.163624617374466652, 6.249999999999999112 ) ) ;
#26587 = CARTESIAN_POINT ( 'NONE',  ( 11.48641235500450009, 3.260080192309100067, 8.177841818594698609 ) ) ;
#26588 = CARTESIAN_POINT ( 'NONE',  ( 9.137543006348998631, 2.995704926864999784, 8.544754656710999541 ) ) ;
#26589 = EDGE_CURVE ( 'NONE', #20805, #48851, #25692, .T. ) ;
#26590 = CARTESIAN_POINT ( 'NONE',  ( 9.766125411066999717, 4.735428155407000794, -8.791393655830999521 ) ) ;
#26591 = CARTESIAN_POINT ( 'NONE',  ( 8.772923981633081070, -3.689545703815815703, -8.314671747086004316 ) ) ;
#26592 = CARTESIAN_POINT ( 'NONE',  ( 9.555699158955999195, -2.440755924888999839, 6.680881588809999272 ) ) ;
#26593 = CARTESIAN_POINT ( 'NONE',  ( 17.68572386047929967, -0.7076089047904995377, -12.58011506138061009 ) ) ;
#26594 = AXIS2_PLACEMENT_3D ( 'NONE', #11930, #28371, #12632 ) ;
#26595 = CARTESIAN_POINT ( 'NONE',  ( 9.001480659271445361, 5.278232124331313280, 7.933979055097461597 ) ) ;
#26596 = CARTESIAN_POINT ( 'NONE',  ( 11.11718313518939816, -4.622449961306399402, -8.287087605365499599 ) ) ;
#26597 = CARTESIAN_POINT ( 'NONE',  ( 8.946010841230998878, 5.458692773671000253, 7.456452194274000078 ) ) ;
#26598 = ORIENTED_EDGE ( 'NONE', *, *, #58310, .T. ) ;
#26599 = FACE_OUTER_BOUND ( 'NONE', #32035, .T. ) ;
#26600 = CARTESIAN_POINT ( 'NONE',  ( 0.7000000000000000666, -0.5773502691895999739, -1.000000000000000000 ) ) ;
#26601 = CARTESIAN_POINT ( 'NONE',  ( 24.91840527020981000, 8.566764005888588329, 8.413212214599523620 ) ) ;
#26602 = B_SPLINE_CURVE_WITH_KNOTS ( 'NONE', 3,
 ( #13807, #56799, #19383, #35136 ),
 .UNSPECIFIED., .F., .F.,
 ( 4, 4 ),
 ( 0.000000000000000000, 1.000000000000000000 ),
 .UNSPECIFIED. ) ;
#26603 = CARTESIAN_POINT ( 'NONE',  ( 18.12596594012297757, 2.036641643015555836, 12.43431447687783020 ) ) ;
#26604 = CARTESIAN_POINT ( 'NONE',  ( 8.810863317747999801, -3.039136629551499880, -7.500000000073117512 ) ) ;
#26605 = CARTESIAN_POINT ( 'NONE',  ( 11.06523650270000125, 8.808136091477001273, 6.643946570999999857 ) ) ;
#26606 = CARTESIAN_POINT ( 'NONE',  ( 12.32101752300973629, -0.3953985757065832107, -12.69171505958691704 ) ) ;
#26607 = CARTESIAN_POINT ( 'NONE',  ( 2.000973465872999846, 3.500000000000000000, 0.000000000000000000 ) ) ;
#26608 = EDGE_CURVE ( 'NONE', #41143, #2693, #17181, .T. ) ;
#26609 = ORIENTED_EDGE ( 'NONE', *, *, #57098, .F. ) ;
#26610 = CARTESIAN_POINT ( 'NONE',  ( 12.29727795756348918, -1.966522083383877462, 12.44559612467660337 ) ) ;
#26611 = EDGE_CURVE ( 'NONE', #21492, #59329, #63195, .T. ) ;
#26612 = CARTESIAN_POINT ( 'NONE',  ( 9.127126402770999292, -2.803062940908000122, -7.048639765412399782 ) ) ;
#26613 = DIRECTION ( 'NONE',  ( -1.000000000000000000, 0.000000000000000000, 0.000000000000000000 ) ) ;
#26614 = CARTESIAN_POINT ( 'NONE',  ( 9.758146639703001668, -2.901368778958000050, 6.555068849476000103 ) ) ;
#26615 = CARTESIAN_POINT ( 'NONE',  ( 12.20794988689359961, -3.544213289744700290, 6.606015074393400077 ) ) ;
#26616 = EDGE_CURVE ( 'NONE', #54765, #24256, #12295, .T. ) ;
#26617 = CARTESIAN_POINT ( 'NONE',  ( 12.48426296206727670, 0.6451567829544476718, 12.58347320810647929 ) ) ;
#26618 = CARTESIAN_POINT ( 'NONE',  ( 0.1210379451993999905, -1.906427021235999941, -2.406055758466000061 ) ) ;
#26619 = CARTESIAN_POINT ( 'NONE',  ( 4.867399517636808781, -1.067373159170256880, -0.5450599291056540396 ) ) ;
#26620 = CIRCLE ( 'NONE', #8751, 12.42499880353999941 ) ;
#26621 = CARTESIAN_POINT ( 'NONE',  ( 12.08558010717399256, 2.390021230702581434, 12.37125449870879024 ) ) ;
#26623 = CARTESIAN_POINT ( 'NONE',  ( 17.97784399489637508, -3.574258648615100231, -12.00418160090810993 ) ) ;
#26622 = CARTESIAN_POINT ( 'NONE',  ( 9.682355082327998019, 3.488994418336600400, -6.478918346312998899 ) ) ;
#26624 = CARTESIAN_POINT ( 'NONE',  ( 10.27610941423800028, 4.844410192686099847, -6.733017893878099791 ) ) ;
#26625 = CARTESIAN_POINT ( 'NONE',  ( 7.681993940831000067, 3.468925063633002903, -6.455929610676999886 ) ) ;
#26626 = B_SPLINE_CURVE_WITH_KNOTS ( 'NONE', 3,
 ( #47483, #10409, #25806, #47139, #32098, #36295, #57969, #9718, #4467, #4125 ),
 .UNSPECIFIED., .F., .F.,
 ( 4, 2, 2, 2, 4 ),
 ( 0.000000000000000000, 0.2499999999999997780, 0.3750000000000005551, 0.5000000000000013323, 1.000000000000000000 ),
 .UNSPECIFIED. ) ;
#26627 = CARTESIAN_POINT ( 'NONE',  ( 10.16821721959000158, 2.330395133894000548, -7.267461653224000173 ) ) ;
#26628 = CARTESIAN_POINT ( 'NONE',  ( 9.174709346416998201, 5.155548326249999924, -6.951281079990299538 ) ) ;
#26630 = CARTESIAN_POINT ( 'NONE',  ( 12.21429833799748188, 2.704300905804447819, 12.40162098798462331 ) ) ;
#26629 = CARTESIAN_POINT ( 'NONE',  ( 15.39518154839200115, -8.837017240434999366, -7.949877004991000362 ) ) ;
#26631 = LINE ( 'NONE', #21032, #24119 ) ;
#26632 = ORIENTED_EDGE ( 'NONE', *, *, #9246, .T. ) ;
#26633 = AXIS2_PLACEMENT_3D ( 'NONE', #67923, #30881, #3602 ) ;
#26634 = CARTESIAN_POINT ( 'NONE',  ( 0.8811095901647999495, -0.1441893070566999946, 3.255843074068999865 ) ) ;
#26635 = EDGE_CURVE ( 'NONE', #27999, #34076, #32395, .T. ) ;
#26636 = CARTESIAN_POINT ( 'NONE',  ( 24.53429014662800256, -8.855930250654999725, 9.286429702500999639 ) ) ;
#26637 = CARTESIAN_POINT ( 'NONE',  ( 3.467799898000360592, 1.131362752643461977, -3.282759086874214027 ) ) ;
#26638 = CARTESIAN_POINT ( 'NONE',  ( 9.047113844317999920, 4.253652595614200393, 8.471855267550699509 ) ) ;
#26639 = PRESENTATION_LAYER_ASSIGNMENT (  '', '', ( #50090 ) ) ;
#26640 = CARTESIAN_POINT ( 'NONE',  ( 12.18472282150165320, -2.421014800242780929, 13.68991273180144574 ) ) ;
#26641 = CARTESIAN_POINT ( 'NONE',  ( 23.66004879239100234, -3.393653467490999720, 13.50507469661999949 ) ) ;
#26642 = CARTESIAN_POINT ( 'NONE',  ( 8.194126132207950164, 2.898246542105644696, 6.620179831079268773 ) ) ;
#26643 = ORIENTED_EDGE ( 'NONE', *, *, #54008, .T. ) ;
#26644 = CARTESIAN_POINT ( 'NONE',  ( 4.979584043203000299, -0.7296458532426999266, -1.046132007313999912 ) ) ;
#26645 = CARTESIAN_POINT ( 'NONE',  ( 8.870759580228998686, -5.244164909883999748, -7.202614619576299226 ) ) ;
#26646 = CARTESIAN_POINT ( 'NONE',  ( 9.742016541512397154, -3.170522872755219712, -8.579511628985352800 ) ) ;
#26647 = B_SPLINE_CURVE_WITH_KNOTS ( 'NONE', 3,
 ( #46361, #63453, #31314, #62086, #4722, #4379, #57877, #67662 ),
 .UNSPECIFIED., .F., .F.,
 ( 4, 2, 2, 4 ),
 ( 0.4992598756075863897, 0.7496299378037931671, 0.8748149689018966946, 1.000000000000000000 ),
 .UNSPECIFIED. ) ;
#26648 = CARTESIAN_POINT ( 'NONE',  ( 17.80000000001300009, -3.351264566333000072, 11.15757590352999884 ) ) ;
#26649 = CARTESIAN_POINT ( 'NONE',  ( 17.74290558058741496, 3.096122732672591749, -12.29249473893052347 ) ) ;
#26650 = CARTESIAN_POINT ( 'NONE',  ( 8.647266668088249730, 4.120490794148916613, -5.883508675810684707 ) ) ;
#26651 = CARTESIAN_POINT ( 'NONE',  ( 18.18005043873315785, 2.501166356630923016, 12.45128845099852199 ) ) ;
#26652 = B_SPLINE_CURVE_WITH_KNOTS ( 'NONE', 3,
 ( #64946, #6577, #32471, #55518 ),
 .UNSPECIFIED., .F., .F.,
 ( 4, 4 ),
 ( 0.000000000000000000, 1.000000000000000000 ),
 .UNSPECIFIED. ) ;
#26653 = FACE_OUTER_BOUND ( 'NONE', #4977, .T. ) ;
#26654 = CARTESIAN_POINT ( 'NONE',  ( 10.87274555961999845, -5.407608219159000029, -8.698392243238998844 ) ) ;
#26655 = CARTESIAN_POINT ( 'NONE',  ( 4.834193173016584133, 1.460959015002474048, -0.3926218265389178064 ) ) ;
#26656 = CARTESIAN_POINT ( 'NONE',  ( 18.29983863916000075, 2.861762957209999847, -11.98830831200999825 ) ) ;
#26657 = CARTESIAN_POINT ( 'NONE',  ( 24.00507652701418237, 9.358504537843028714, -9.266396259472484687 ) ) ;
#26658 = CARTESIAN_POINT ( 'NONE',  ( 9.417722590937366078, 5.345104022944846989, 7.384957899024609418 ) ) ;
#26659 = CARTESIAN_POINT ( 'NONE',  ( 23.99192795366400333, 13.00768256589000060, -3.383863472243999748 ) ) ;
#26660 = APPLICATION_CONTEXT ( 'automotive_design' ) ;
#26661 = VERTEX_POINT ( 'NONE', #67830 ) ;
#26662 = CARTESIAN_POINT ( 'NONE',  ( 8.415504719592000527, 2.469361196073999842, -7.826019481986000059 ) ) ;
#26663 = CARTESIAN_POINT ( 'NONE',  ( 10.95672469555900008, -3.566534988568399900, 8.249937779480299938 ) ) ;
#26664 = ORIENTED_EDGE ( 'NONE', *, *, #73, .T. ) ;
#26665 = PLANE ( 'NONE',  #23936 ) ;
#26666 = CARTESIAN_POINT ( 'NONE',  ( 10.37457053952199892, -4.448306506338299826, -6.451042711717000167 ) ) ;
#26667 = VERTEX_POINT ( 'NONE', #14025 ) ;
#26668 = CARTESIAN_POINT ( 'NONE',  ( 11.63611496860034933, 5.171412538012999605, 8.100294210499798808 ) ) ;
#26669 = CARTESIAN_POINT ( 'NONE',  ( 17.60000000000000142, 11.23412379136000006, -3.084957477885999833 ) ) ;
#26670 = VECTOR ( 'NONE', #26488, 1000.000000000000000 ) ;
#26671 = EDGE_CURVE ( 'NONE', #57964, #28289, #17406, .T. ) ;
#26672 = CARTESIAN_POINT ( 'NONE',  ( 18.23176382712000176, -2.916721637292999603, 11.52766586543999949 ) ) ;
#26673 = ADVANCED_FACE ( 'NONE', ( #30783 ), #19724, .F. ) ;
#26674 = CARTESIAN_POINT ( 'NONE',  ( 10.36325056272499978, -3.107965259299500183, -7.513220396995270001 ) ) ;
#26675 = CARTESIAN_POINT ( 'NONE',  ( 12.34379246210524173, 0.4226248002247757207, -13.89137006864033985 ) ) ;
#26676 = CARTESIAN_POINT ( 'NONE',  ( 11.60000000000000142, -4.254640155007241020, -6.522131813714045379 ) ) ;
#26677 = CONICAL_SURFACE ( 'NONE', #14402, 0.9346783463124002100, 0.7853981908209605178 ) ;
#26678 = LINE ( 'NONE', #53233, #55233 ) ;
#26679 = VERTEX_POINT ( 'NONE', #46522 ) ;
#26680 = CARTESIAN_POINT ( 'NONE',  ( 8.475341021510232054, 5.350570349241480450, 7.499981640446101494 ) ) ;
#26681 = VERTEX_POINT ( 'NONE', #66810 ) ;
#26682 = CARTESIAN_POINT ( 'NONE',  ( 10.64393020684969926, 5.250000000000000000, -7.500000000000000000 ) ) ;
#26683 = EDGE_LOOP ( 'NONE', ( #27088, #59221, #23384, #32607 ) ) ;
#26684 = CARTESIAN_POINT ( 'NONE',  ( 9.124051052051999733, 5.255397705012999410, 7.254315263553399618 ) ) ;
#26685 = CARTESIAN_POINT ( 'NONE',  ( 17.83408408707291670, -3.059349868707512687, -12.30347716376230238 ) ) ;
#26686 = CARTESIAN_POINT ( 'NONE',  ( 7.100000000000000533, 0.000000000000000000, 0.000000000000000000 ) ) ;
#26687 = B_SPLINE_SURFACE_WITH_KNOTS ( 'NONE', 3, 3, ( 
 ( #68821, #63579, #46827, #69168 ),
 ( #67790, #20593, #63227, #37025 ),
 ( #19911, #42609, #14331, #41236 ),
 ( #68132, #35654, #56968, #51719 ),
 ( #20250, #41576, #62884, #15005 ),
 ( #54474, #49225, #21617, #22998 ),
 ( #27219, #37360, #32809, #64944 ),
 ( #38043, #16030, #28252, #17416 ),
 ( #27915, #53444, #32469, #16374 ) ),
 .UNSPECIFIED., .F., .F., .F.,
 ( 4, 1, 1, 1, 1, 1, 4 ),
 ( 4, 4 ),
 ( 0.02166927333703000044, 0.1666666666667000196, 0.3333333333333000081, 0.5000000000000000000, 0.6666666666667000474, 0.8333333333333000637, 0.9489586827378000411 ),
 ( -0.1917159053268999991, 1.191863452461999984 ),
 .UNSPECIFIED. ) ;
#26688 = CARTESIAN_POINT ( 'NONE',  ( 8.475341021510246264, -5.350570349241358770, 7.499981640446112152 ) ) ;
#26689 = CARTESIAN_POINT ( 'NONE',  ( 12.20411985647183251, -0.1720826668005533966, 13.89857125525885095 ) ) ;
#26690 = VERTEX_POINT ( 'NONE', #13681 ) ;
#26691 = FACE_OUTER_BOUND ( 'NONE', #38183, .T. ) ;
#26692 = CARTESIAN_POINT ( 'NONE',  ( 17.61332066134400165, 11.38815944871000063, -4.576072459028000416 ) ) ;
#26693 = CARTESIAN_POINT ( 'NONE',  ( 10.24006601915162484, 3.957587222814286321, 6.626081523287773223 ) ) ;
#26694 = CARTESIAN_POINT ( 'NONE',  ( 18.30000000000000071, -2.775715947008034146, 11.68320807311170917 ) ) ;
#26695 = ADVANCED_FACE ( 'NONE', ( #18921 ), #46177, .T. ) ;
#26696 = CARTESIAN_POINT ( 'NONE',  ( 8.500189158773000742, 2.724453559418999582, -8.908010318766001134 ) ) ;
#26697 = CARTESIAN_POINT ( 'NONE',  ( 17.75883778089099962, -3.641526152925000037, 12.02434993381999995 ) ) ;
#26698 = CARTESIAN_POINT ( 'NONE',  ( 9.937415816209998809, -3.510658118802999716, -6.227041669085999764 ) ) ;
#26699 = ORIENTED_EDGE ( 'NONE', *, *, #14931, .F. ) ;
#26700 = ORIENTED_EDGE ( 'NONE', *, *, #65253, .F. ) ;
#26701 = CARTESIAN_POINT ( 'NONE',  ( 8.639360841228999277, 5.074768364528000397, -8.296267706722000312 ) ) ;
#26702 = CARTESIAN_POINT ( 'NONE',  ( 8.191498616105999275, -3.399962740672999750, 6.146646623957999545 ) ) ;
#26703 = B_SPLINE_CURVE_WITH_KNOTS ( 'NONE', 3,
 ( #25224, #39589, #34356, #61260, #55676, #50421 ),
 .UNSPECIFIED., .F., .F.,
 ( 4, 2, 4 ),
 ( 0.000000000000000000, 0.5000000000000000000, 1.000000000000000000 ),
 .UNSPECIFIED. ) ;
#26704 = CARTESIAN_POINT ( 'NONE',  ( 10.99698817424124364, -5.185245244840650081, 5.073517292121563216 ) ) ;
#26705 = CARTESIAN_POINT ( 'NONE',  ( 1.228056799207625227, -2.150913519912213800, 2.798833948393621540 ) ) ;
#26706 = CYLINDRICAL_SURFACE ( 'NONE', #32190, 3.500000000000000000 ) ;
#26707 = CARTESIAN_POINT ( 'NONE',  ( 11.46989666366029859, 3.941571897678119996, -8.814970315645998866 ) ) ;
#26708 = CARTESIAN_POINT ( 'NONE',  ( 9.864633995697998259, 4.861719613449499988, -7.595641268826199166 ) ) ;
#26710 = CARTESIAN_POINT ( 'NONE',  ( 2.007156007037999679, 3.012404793772358147, -1.845954168039164678 ) ) ;
#26709 = CARTESIAN_POINT ( 'NONE',  ( 10.66159632033899918, -4.929952350555500296, 7.879514065647800436 ) ) ;
#26711 = DIRECTION ( 'NONE',  ( -0.9999999999999893419, -1.468722421713984115E-07, -5.561711760123941642E-09 ) ) ;
#26712 = ORIENTED_EDGE ( 'NONE', *, *, #44763, .T. ) ;
#26713 = CARTESIAN_POINT ( 'NONE',  ( 11.29364426047339975, -3.533902447304699823, -8.230103870496201068 ) ) ;
#26714 = ADVANCED_FACE ( 'NONE', ( #68171 ), #2948, .F. ) ;
#26715 = DIRECTION ( 'NONE',  ( 0.000000000000000000, 1.000000000000000000, 0.000000000000000000 ) ) ;
#26716 = CARTESIAN_POINT ( 'NONE',  ( 9.684367640780997988, 4.603017491986999943, 8.628164124510998789 ) ) ;
#26717 = CARTESIAN_POINT ( 'NONE',  ( 11.79999999684100054, -3.345264396959000130, 11.86064773189999855 ) ) ;
#26718 = VECTOR ( 'NONE', #48813, 1000.000000000000114 ) ;
#26719 = CARTESIAN_POINT ( 'NONE',  ( 11.27109998545999936, -5.469594811916000054, 8.504700858852999090 ) ) ;
#26720 = CARTESIAN_POINT ( 'NONE',  ( 8.433148997460000018, -5.167567567567999731, 6.822293592207000934 ) ) ;
#26721 = CARTESIAN_POINT ( 'NONE',  ( 16.34806348789000197, -3.378436248652000096, -11.11006988061000023 ) ) ;
#26722 = CARTESIAN_POINT ( 'NONE',  ( 13.73494720760600174, -12.32760134815999997, -2.421442066891999811 ) ) ;
#26723 = CARTESIAN_POINT ( 'NONE',  ( 7.417083333331121686, 2.920449762762455492, -6.670361928033868182 ) ) ;
#26724 = CARTESIAN_POINT ( 'NONE',  ( 8.978113844317999082, -3.781046324972699768, -6.661091642253600398 ) ) ;
#26725 = CARTESIAN_POINT ( 'NONE',  ( 5.454587365828999168, -0.09407552946282000950, -1.172318398388999983 ) ) ;
#26726 = CARTESIAN_POINT ( 'NONE',  ( 11.34606641549977724, -3.161700962939955506, 7.252322131039115050 ) ) ;
#26727 = CARTESIAN_POINT ( 'NONE',  ( 0.1499942179679999987, 5.893556041935713383E-16, -2.749976859058071543 ) ) ;
#26728 = ORIENTED_EDGE ( 'NONE', *, *, #53122, .F. ) ;
#26729 = CARTESIAN_POINT ( 'NONE',  ( 12.39271969839518839, 0.4698014501121452469, -12.68830453558792826 ) ) ;
#26730 = CARTESIAN_POINT ( 'NONE',  ( 11.07210672858429845, 3.307795442047700263, -6.979277962544199632 ) ) ;
#26731 = FACE_OUTER_BOUND ( 'NONE', #22512, .T. ) ;
#26732 = CARTESIAN_POINT ( 'NONE',  ( 5.500000000595999694, -0.4999999994045000173, 3.150000007847999939 ) ) ;
#26733 = CARTESIAN_POINT ( 'NONE',  ( 10.15670292967811150, 5.179682183662283279, -8.179940953558951122 ) ) ;
#26734 = ORIENTED_EDGE ( 'NONE', *, *, #23754, .F. ) ;
#26735 = CARTESIAN_POINT ( 'NONE',  ( 25.37703116084200161, -11.10735239355999937, -3.396338630210000264 ) ) ;
#26736 = APPLICATION_PROTOCOL_DEFINITION ( 'draft international standard', 'automotive_design', 1998, #49409 ) ;
#26737 = CARTESIAN_POINT ( 'NONE',  ( 11.31900581613029821, -3.249313226592100534, -7.982035256002799173 ) ) ;
#26738 = CARTESIAN_POINT ( 'NONE',  ( 18.01651533407960670, 0.4224082573471430457, 12.69056396414930887 ) ) ;
#26739 = AXIS2_PLACEMENT_3D ( 'NONE', #47712, #63074, #42461 ) ;
#26740 = CARTESIAN_POINT ( 'NONE',  ( 10.39601354018312662, -4.999583552997726166, 6.731816600031358178 ) ) ;
#26741 = CARTESIAN_POINT ( 'NONE',  ( 11.49999672495000169, -3.632761979779000061, 11.06912554803999882 ) ) ;
#26742 = CARTESIAN_POINT ( 'NONE',  ( 10.69057802013490033, 2.966773425016000054, -7.475947032624040034 ) ) ;
#26743 = EDGE_LOOP ( 'NONE', ( #52653, #67465, #44739, #61912, #67836, #56786, #39941, #19513 ) ) ;
#26744 = CARTESIAN_POINT ( 'NONE',  ( 10.13340376756999994, -5.653635692335999607, 6.501829690795999817 ) ) ;
#26745 = CARTESIAN_POINT ( 'NONE',  ( 18.11136953712599862, 2.785023373216928277, -13.60886753798840587 ) ) ;
#26746 = EDGE_LOOP ( 'NONE', ( #61384, #60685, #21044, #56563, #45610 ) ) ;
#26747 = CARTESIAN_POINT ( 'NONE',  ( 7.000000000000000000, -9.186881099820000784, 5.186879182879000183 ) ) ;
#26748 = CARTESIAN_POINT ( 'NONE',  ( 8.443894353209000059, -2.905864338704999827, 8.940687151810998046 ) ) ;
#26749 = DIRECTION ( 'NONE',  ( 0.000000000000000000, 0.000000000000000000, -1.000000000000000000 ) ) ;
#26750 = EDGE_CURVE ( 'NONE', #34701, #6933, #26577, .T. ) ;
#26751 = ORIENTED_EDGE ( 'NONE', *, *, #54290, .T. ) ;
#26752 = DIRECTION ( 'NONE',  ( 0.000000000000000000, 0.7158784314711267305, 0.6982249432342270135 ) ) ;
#26753 = EDGE_CURVE ( 'NONE', #35889, #15208, #44905, .T. ) ;
#26754 = CARTESIAN_POINT ( 'NONE',  ( 8.442410841228998208, 4.988620887051999908, -9.026201633254999024 ) ) ;
#26755 = CARTESIAN_POINT ( 'NONE',  ( 9.583513540183334456, -2.750000000000000000, -7.663624617374468428 ) ) ;
#26756 = EDGE_CURVE ( 'NONE', #12493, #19330, #35732, .T. ) ;
#26757 = CARTESIAN_POINT ( 'NONE',  ( 8.156333095604772154, -3.177195612464926100, 6.222100672065804083 ) ) ;
#26758 = EDGE_LOOP ( 'NONE', ( #54561, #12383, #40365, #37287, #49444, #9296, #474, #26778, #5116, #64463 ) ) ;
#26759 = CARTESIAN_POINT ( 'NONE',  ( 10.77962878203999963, -2.397503436487000261, 7.755423856053000442 ) ) ;
#26760 = EDGE_CURVE ( 'NONE', #10029, #47524, #10706, .T. ) ;
#26761 = B_SPLINE_CURVE_WITH_KNOTS ( 'NONE', 3,
 ( #30529, #67569, #62337, #19343, #19695, #8857, #14454, #35774, #51842, #25278, #67918, #41363, #62672, #14792 ),
 .UNSPECIFIED., .F., .F.,
 ( 4, 2, 2, 2, 2, 2, 4 ),
 ( 0.1252897476283257872, 0.3125851014321937016, 0.4998804552360616160, 0.5935281321379953789, 0.6871758090399291419, 0.7808234859418630158, 0.8744711628437967788 ),
 .UNSPECIFIED. ) ;
#26762 = B_SPLINE_CURVE_WITH_KNOTS ( 'NONE', 3,
 ( #38306, #48804, #54738, #64862 ),
 .UNSPECIFIED., .F., .F.,
 ( 4, 4 ),
 ( 0.000000000000000000, 1.000000000000000000 ),
 .UNSPECIFIED. ) ;
#26763 = CARTESIAN_POINT ( 'NONE',  ( 10.76947109217999810, 5.100000000000000533, -6.152188490330000370 ) ) ;
#26764 = CARTESIAN_POINT ( 'NONE',  ( 11.14955063476181962, 4.976598135215293262, -6.673569913327194847 ) ) ;
#26765 = ORIENTED_EDGE ( 'NONE', *, *, #53572, .T. ) ;
#26766 = CARTESIAN_POINT ( 'NONE',  ( 15.96683822361929295, 3.674392175451481446, 11.19597380828297517 ) ) ;
#26767 = CARTESIAN_POINT ( 'NONE',  ( 10.84160444037999937, -2.641264320582999758, -7.444904971031999885 ) ) ;
#26768 = ORIENTED_EDGE ( 'NONE', *, *, #18065, .F. ) ;
#26769 = CARTESIAN_POINT ( 'NONE',  ( 4.916518311043333256, 1.085476820253131081, 1.060886400888860548 ) ) ;
#26770 = CARTESIAN_POINT ( 'NONE',  ( 17.57925147499693352, -1.760911370824147504, -12.47634522799707746 ) ) ;
#26771 = CARTESIAN_POINT ( 'NONE',  ( 4.384880990064000450, 0.9041977637900000531, 1.209694771924000101 ) ) ;
#26772 = CARTESIAN_POINT ( 'NONE',  ( 11.59999999999999964, 5.087332147730433185, -6.982348652072320583 ) ) ;
#26773 = CARTESIAN_POINT ( 'NONE',  ( 25.30000327618300204, -2.078227429405999693, 11.31065739696999906 ) ) ;
#26774 = CARTESIAN_POINT ( 'NONE',  ( 10.64659450977357658, 2.685850423140129895, 7.981710561160634931 ) ) ;
#26775 = CARTESIAN_POINT ( 'NONE',  ( 23.78808814531843296, 13.03931410352375941, 3.724145320519536728 ) ) ;
#26776 = EDGE_LOOP ( 'NONE', ( #27811, #61653, #12450, #49470, #61255 ) ) ;
#26777 = CARTESIAN_POINT ( 'NONE',  ( 8.748305582559998683, 4.091272957481129957, -8.362426869835999810 ) ) ;
#26778 = ORIENTED_EDGE ( 'NONE', *, *, #3932, .F. ) ;
#26779 = CARTESIAN_POINT ( 'NONE',  ( 9.242342830452999536, 5.206708472530999998, 8.808826521083998884 ) ) ;
#26780 = CARTESIAN_POINT ( 'NONE',  ( 10.15335165876999923, 3.144981324235999853, -5.860948306964999688 ) ) ;
#26781 = CARTESIAN_POINT ( 'NONE',  ( 18.06885190415285081, -12.08553577211657348, 3.288727606363090139 ) ) ;
#26782 = DIRECTION ( 'NONE',  ( -1.000000000000000000, 0.000000000000000000, 0.000000000000000000 ) ) ;
#26783 = CARTESIAN_POINT ( 'NONE',  ( 9.600000000000001421, 0.000000000000000000, 0.000000000000000000 ) ) ;
#26784 = CARTESIAN_POINT ( 'NONE',  ( 10.90000000000000036, -0.2999999999999999889, 9.662944685757000940 ) ) ;
#26785 = CARTESIAN_POINT ( 'NONE',  ( 18.17481363285255469, -0.08139021474669956568, 13.89968437038781524 ) ) ;
#26786 = CARTESIAN_POINT ( 'NONE',  ( 17.97806348702467005, 0.4608880372546551030, 13.88973238275223387 ) ) ;
#26787 = B_SPLINE_CURVE_WITH_KNOTS ( 'NONE', 1,
 ( #48632, #734 ),
 .UNSPECIFIED., .F., .F.,
 ( 2, 2 ),
 ( 0.000000000000000000, 1.000000000000000000 ),
 .UNSPECIFIED. ) ;
#26788 = ORIENTED_EDGE ( 'NONE', *, *, #18707, .F. ) ;
#26789 = CARTESIAN_POINT ( 'NONE',  ( 12.49453886772563038, 0.5425156946249201084, 13.88574935929170806 ) ) ;
#26790 = CARTESIAN_POINT ( 'NONE',  ( 11.73195122972050086, -3.492749840905900349, 8.673036084990000560 ) ) ;
#26791 = CARTESIAN_POINT ( 'NONE',  ( 18.17614081687046124, -0.08113699236157925765, -13.89976078940779480 ) ) ;
#26792 = CARTESIAN_POINT ( 'NONE',  ( 9.208105646793001142, -5.057079407184000175, 8.967634647348999621 ) ) ;
#26793 = VECTOR ( 'NONE', #30370, 1000.000000000000000 ) ;
#26795 = CARTESIAN_POINT ( 'NONE',  ( 7.844724262280000637, -4.719412258162999585, 6.357657668295000342 ) ) ;
#26794 = CARTESIAN_POINT ( 'NONE',  ( 10.09696969267000100, 5.253376380222999131, 8.530663119653999260 ) ) ;
#26796 = CARTESIAN_POINT ( 'NONE',  ( 10.98995257254739855, 2.904643075091000171, -7.818564472783199548 ) ) ;
#26797 = CARTESIAN_POINT ( 'NONE',  ( 10.99999999997000089, -4.000000000000000000, -7.500000000000000000 ) ) ;
#26798 = EDGE_CURVE ( 'NONE', #4475, #21968, #51572, .T. ) ;
#26799 = CARTESIAN_POINT ( 'NONE',  ( 10.28622949779699880, 4.480999174483200065, -8.221351791991999391 ) ) ;
#26800 = CARTESIAN_POINT ( 'NONE',  ( 18.18005727183074782, 0.009762034906138391047, 12.70000045436730751 ) ) ;
#26801 = CARTESIAN_POINT ( 'NONE',  ( 6.948702399619000047, 1.366611866804000153, 0.3628763661032999854 ) ) ;
#26802 = EDGE_CURVE ( 'NONE', #8614, #65865, #41546, .T. ) ;
#26803 = DIRECTION ( 'NONE',  ( 1.000000000000000000, 0.000000000000000000, 0.000000000000000000 ) ) ;
#26804 = ORIENTED_EDGE ( 'NONE', *, *, #37871, .T. ) ;
#26805 = CARTESIAN_POINT ( 'NONE',  ( 8.379706853209000883, -4.282999948634999221, 9.286791354293999490 ) ) ;
#26806 = CARTESIAN_POINT ( 'NONE',  ( 9.667489158770999680, 4.808846957865000604, -8.639578604182998944 ) ) ;
#26807 = DIRECTION ( 'NONE',  ( 0.000000000000000000, 1.000000000000000000, 0.000000000000000000 ) ) ;
#26808 = DIRECTION ( 'NONE',  ( 1.000000000000000000, 0.000000000000000000, 0.000000000000000000 ) ) ;
#26809 = VERTEX_POINT ( 'NONE', #29429 ) ;
#26810 = CARTESIAN_POINT ( 'NONE',  ( 0.6750951013211000662, -1.176389486124999939, 3.509795687408999942 ) ) ;
#26811 = CARTESIAN_POINT ( 'NONE',  ( 10.98656920625009903, 4.032067152264009913, 8.391549386185598536 ) ) ;
#26812 = CARTESIAN_POINT ( 'NONE',  ( 11.10664834123000055, 5.324188120986000250, -7.809342242343999985 ) ) ;
#26813 = ORIENTED_EDGE ( 'NONE', *, *, #4247, .T. ) ;
#26814 = CARTESIAN_POINT ( 'NONE',  ( 5.294609839683333874, 1.500000000000001110, -0.1963495408493590721 ) ) ;
#26815 = CARTESIAN_POINT ( 'NONE',  ( 18.50003594170800270, -2.686563649653999963, 11.33603604535000109 ) ) ;
#26816 = CARTESIAN_POINT ( 'NONE',  ( 17.99403275303994576, 3.052983340820297542, -12.22453705205519014 ) ) ;
#26817 = CARTESIAN_POINT ( 'NONE',  ( 5.687176560458846453, 12.04993902413980678, 3.725892264571312396 ) ) ;
#26818 = CARTESIAN_POINT ( 'NONE',  ( 9.298698341228998743, 5.159258275969999197, 9.109498396691998678 ) ) ;
#26819 = EDGE_LOOP ( 'NONE', ( #23645, #43720, #31257, #58559 ) ) ;
#26820 = CARTESIAN_POINT ( 'NONE',  ( 11.50001496185000427, 10.90724927937048783, -6.294778943961341078 ) ) ;
#26821 = CARTESIAN_POINT ( 'NONE',  ( 7.458579719585999968, 5.383759907926999766, -8.542359279933998906 ) ) ;
#26822 = CARTESIAN_POINT ( 'NONE',  ( 8.544290774020575796, -3.362597475556388105, 5.881642975893083936 ) ) ;
#26823 = CARTESIAN_POINT ( 'NONE',  ( 8.990822372493999737, -4.367693913457399546, 6.297150255604999636 ) ) ;
#26824 = EDGE_LOOP ( 'NONE', ( #19763, #11447, #44253, #59244, #15272, #28133 ) ) ;
#26825 = CARTESIAN_POINT ( 'NONE',  ( 4.900006121741999010, 2.000000000000000000, 0.000000000000000000 ) ) ;
#26826 = CARTESIAN_POINT ( 'NONE',  ( 0.5000220334827000235, 2.806761118207999672, -2.090954811877999919 ) ) ;
#26827 = ORIENTED_EDGE ( 'NONE', *, *, #56672, .T. ) ;
#26828 = CARTESIAN_POINT ( 'NONE',  ( 24.70908039369507492, 3.127826627798298897, -11.79915521905276243 ) ) ;
#26829 = CARTESIAN_POINT ( 'NONE',  ( 24.71766312773793217, -8.650208672895015383, -8.601007095493814703 ) ) ;
#26830 = CARTESIAN_POINT ( 'NONE',  ( 17.65768761389442432, 0.6168528257048864205, -13.88157091029610157 ) ) ;
#26831 = ORIENTED_EDGE ( 'NONE', *, *, #12060, .T. ) ;
#26832 = CARTESIAN_POINT ( 'NONE',  ( 15.75262483093033516, -8.754898706354207860, -7.686019545157542154 ) ) ;
#26833 = EDGE_CURVE ( 'NONE', #57248, #12470, #54048, .T. ) ;
#26834 = CARTESIAN_POINT ( 'NONE',  ( 24.53428988874600236, -8.855929874993998752, -9.286429786912000495 ) ) ;
#26835 = CARTESIAN_POINT ( 'NONE',  ( 10.20851354018333623, -3.836375382625528019, 8.749999999999996447 ) ) ;
#26836 = CARTESIAN_POINT ( 'NONE',  ( 17.55505043854143565, 1.787797342887044394, 13.88538010501570952 ) ) ;
#26837 = EDGE_CURVE ( 'NONE', #27228, #20236, #38192, .T. ) ;
#26838 = CARTESIAN_POINT ( 'NONE',  ( 10.77195525820100031, -4.120672149427799802, 8.772302877803999976 ) ) ;
#26839 = EDGE_LOOP ( 'NONE', ( #16770, #33479, #60011, #29656, #61474, #45007, #28086, #42820, #12877, #31374, #11350, #28741, #27564, #47406, #42438, #15317, #55776, #42890, #53707, #10726 ) ) ;
#26840 = CARTESIAN_POINT ( 'NONE',  ( 7.037114158771000660, 4.623631324973000112, 8.651459902566999816 ) ) ;
#26841 = EDGE_CURVE ( 'NONE', #10178, #6658, #51417, .T. ) ;
#26842 = SHAPE_REPRESENTATION ( '510 Connector Pin', ( #9676 ), #67824 ) ;
#26843 = ORIENTED_EDGE ( 'NONE', *, *, #21381, .T. ) ;
#26844 = CIRCLE ( 'NONE', #53625, 10.80000000000000249 ) ;
#26845 = CARTESIAN_POINT ( 'NONE',  ( 10.07309687351667016, -2.782534154164605589, 7.172815144550900968 ) ) ;
#26846 = CARTESIAN_POINT ( 'NONE',  ( 15.90830001818700090, -9.238654026387999707, -8.377706362734000933 ) ) ;
#26847 = CARTESIAN_POINT ( 'NONE',  ( 11.07074944260999949, 6.638253589849999692, -5.577401735838000363 ) ) ;
#26848 = EDGE_LOOP ( 'NONE', ( #32687, #44428, #66703, #32392 ) ) ;
#26849 = B_SPLINE_SURFACE_WITH_KNOTS ( 'NONE', 3, 3, ( 
 ( #1190, #12370, #33004, #27413 ),
 ( #49419, #59219, #22156, #11663 ),
 ( #49773, #37547, #28106, #49077 ),
 ( #65494, #65843, #64796, #33700 ),
 ( #1531, #5731, #54318, #6076 ),
 ( #6418, #27072, #65143, #55020 ),
 ( #43843, #1884, #17264, #11320 ),
 ( #23200, #44200, #53971, #16908 ) ),
 .UNSPECIFIED., .F., .F., .F.,
 ( 4, 1, 1, 1, 1, 4 ),
 ( 4, 4 ),
 ( 0.7453056706973000267, 0.7647058823529000460, 0.8235294117646999590, 0.8823529411764999830, 0.9411764705882000870, 0.9905827404250000523 ),
 ( -0.1830915227417000135, 1.182948991274999972 ),
 .UNSPECIFIED. ) ;
#26850 = CARTESIAN_POINT ( 'NONE',  ( 10.11501430098003773, -5.350017391163235381, -7.499999134156934311 ) ) ;
#26851 = CARTESIAN_POINT ( 'NONE',  ( 0.1103081484368000076, -1.521127753326000143, -2.712944034833999929 ) ) ;
#26852 = CARTESIAN_POINT ( 'NONE',  ( 23.60205915885299888, -9.230633470682002795, 8.204162215359994903 ) ) ;
#26853 = CARTESIAN_POINT ( 'NONE',  ( 8.447783767286768608, 5.285582108569087723, 7.027722483016013655 ) ) ;
#26854 = CARTESIAN_POINT ( 'NONE',  ( 12.09560501594675230, -2.367229839359598298, -13.79841893036761036 ) ) ;
#26855 = CARTESIAN_POINT ( 'NONE',  ( 11.69559063708295987, -2.913481137622000006, -7.805482129094999166 ) ) ;
#26856 = CARTESIAN_POINT ( 'NONE',  ( 18.35676500242969666, 3.328522075977830230, 12.07468831867923242 ) ) ;
#26857 = CARTESIAN_POINT ( 'NONE',  ( 18.14576286523421800, -2.898275280820969524, 12.26215340014708310 ) ) ;
#26858 = VERTEX_POINT ( 'NONE', #11169 ) ;
#26859 = DIRECTION ( 'NONE',  ( 0.000000000000000000, 1.000000000000000000, 0.000000000000000000 ) ) ;
#26860 = ORIENTED_EDGE ( 'NONE', *, *, #31530, .T. ) ;
#26861 = ADVANCED_FACE ( 'NONE', ( #58375 ), #29581, .T. ) ;
#26862 = DIRECTION ( 'NONE',  ( 0.7071051450805292404, 0.000000000000000000, -0.7071084172887802666 ) ) ;
#26863 = CARTESIAN_POINT ( 'NONE',  ( 4.900006121741999898, -1.947945353336631102, 0.5234957687185606279 ) ) ;
#26864 = CARTESIAN_POINT ( 'NONE',  ( 10.32702465212000043, 5.663794543395000325, -6.682030833630000721 ) ) ;
#26865 = CARTESIAN_POINT ( 'NONE',  ( 8.100000113405998903, 3.037570195374000164E-13, -3.946654265865999873E-14 ) ) ;
#26866 = PLANE ( 'NONE',  #33911 ) ;
#26867 = CARTESIAN_POINT ( 'NONE',  ( 23.64714572502700207, -13.35826560361000048, 3.867671150794999679 ) ) ;
#26868 = CARTESIAN_POINT ( 'NONE',  ( 21.05000072320139992, -1.355183834107999921E-13, 1.088018564133000035E-14 ) ) ;
#26869 = EDGE_LOOP ( 'NONE', ( #25547, #6280, #58500, #50382 ) ) ;
#26870 = CARTESIAN_POINT ( 'NONE',  ( 10.77088239901999955, -5.264131025895999905, -4.839453784185999474 ) ) ;
#26871 = CARTESIAN_POINT ( 'NONE',  ( 10.74609776273999984, 4.263105564403999459, 9.276980853981999786 ) ) ;
#26872 = FACE_BOUND ( 'NONE', #64442, .T. ) ;
#26873 = CARTESIAN_POINT ( 'NONE',  ( 11.60612378248510090, -4.482960757953799558, 8.413720204863100349 ) ) ;
#26874 = B_SPLINE_CURVE_WITH_KNOTS ( 'NONE', 3,
 ( #36161, #25324, #4335, #25670, #20423 ),
 .UNSPECIFIED., .F., .F.,
 ( 4, 1, 4 ),
 ( 0.000000000000000000, 0.5000000000000000000, 1.000000000000000000 ),
 .UNSPECIFIED. ) ;
#26875 = CARTESIAN_POINT ( 'NONE',  ( 8.807788144226000426, 4.090932644426789722, -8.453461841935100196 ) ) ;
#26876 = CARTESIAN_POINT ( 'NONE',  ( 11.29364426047339975, 4.466097552695299733, -8.230103870496201068 ) ) ;
#26877 = CARTESIAN_POINT ( 'NONE',  ( 11.00366136905836889, 3.174009385455987431, -9.060794845599636105 ) ) ;
#26878 = CARTESIAN_POINT ( 'NONE',  ( 5.598857209341685071, -12.13471601160040514, -3.750691118698022741 ) ) ;
#26879 = DIRECTION ( 'NONE',  ( 1.000000000000000000, 0.000000000000000000, 0.000000000000000000 ) ) ;
#26880 = FILL_AREA_STYLE ('',( #5541 ) ) ;
#26881 = EDGE_CURVE ( 'NONE', #65865, #1379, #7372, .T. ) ;
#26882 = VERTEX_POINT ( 'NONE', #63872 ) ;
#26883 = CARTESIAN_POINT ( 'NONE',  ( 10.17905590578999941, -2.899999999999999911, 6.571291218949999902 ) ) ;
#26884 = CARTESIAN_POINT ( 'NONE',  ( 6.906312714198000080, -1.081792471387999832, 0.7949120843246000323 ) ) ;
#26885 = CARTESIAN_POINT ( 'NONE',  ( 17.74755423490962158, 3.094705742910453861, 13.52911976267489891 ) ) ;
#26886 = CARTESIAN_POINT ( 'NONE',  ( 10.81218444446805016, 4.996894876589563772, 4.859602168033166691 ) ) ;
#26887 = CARTESIAN_POINT ( 'NONE',  ( 11.48225819896749833, -5.120994791668000090, -7.711331004020999913 ) ) ;
#26888 = ORIENTED_EDGE ( 'NONE', *, *, #14239, .F. ) ;
#26889 = B_SPLINE_CURVE_WITH_KNOTS ( 'NONE', 3,
 ( #3315, #14165, #4677, #52238 ),
 .UNSPECIFIED., .F., .F.,
 ( 4, 4 ),
 ( 0.000000000000000000, 1.000000000000000000 ),
 .UNSPECIFIED. ) ;
#26890 = DIRECTION ( 'NONE',  ( 0.000000000000000000, -1.000000000000000000, -1.110693484091000068E-14 ) ) ;
#26891 = CARTESIAN_POINT ( 'NONE',  ( 8.502045280412000139, 3.869396554003000421, 5.695652484872999466 ) ) ;
#26894 = CARTESIAN_POINT ( 'NONE',  ( 3.500000000000000000, -3.033011252059000018, -1.020217008720000207 ) ) ;
#26893 = CARTESIAN_POINT ( 'NONE',  ( 8.863029719594999634, 2.990001567622999623, -8.695425648791999862 ) ) ;
#26892 = UNCERTAINTY_MEASURE_WITH_UNIT (LENGTH_MEASURE( 1.000000000000000082E-05 ), #36045, 'distance_accuracy_value', 'NONE');
#26896 = B_SPLINE_CURVE_WITH_KNOTS ( 'NONE', 3,
 ( #53764, #64238, #17039, #17749 ),
 .UNSPECIFIED., .F., .F.,
 ( 4, 4 ),
 ( 0.000000000000000000, 1.000000000000000000 ),
 .UNSPECIFIED. ) ;
#26895 = CARTESIAN_POINT ( 'NONE',  ( 10.85685100254000091, -2.832432432432000269, -6.822293592207000934 ) ) ;
#26897 = ORIENTED_EDGE ( 'NONE', *, *, #32912, .F. ) ;
#26898 = CARTESIAN_POINT ( 'NONE',  ( 10.09181485429000169, 2.440912084162000006, 7.817367409531000177 ) ) ;
#26899 = CARTESIAN_POINT ( 'NONE',  ( 18.13331639930713735, -2.076941473624323020, -13.84509535655099199 ) ) ;
#26900 = CARTESIAN_POINT ( 'NONE',  ( 10.62487750876920067, 3.456442671114800191, 6.656497609330299881 ) ) ;
#26901 = CARTESIAN_POINT ( 'NONE',  ( 9.423521818475000700, -4.993993578306000103, 8.578110568283999982 ) ) ;
#26902 = CARTESIAN_POINT ( 'NONE',  ( 7.384456853207000293, -3.346260729029000291, 6.002247316312999459 ) ) ;
#26903 = VERTEX_POINT ( 'NONE', #41527 ) ;
#26904 = CARTESIAN_POINT ( 'NONE',  ( 8.636454719592999041, 3.869396554003000421, 5.695652484872999466 ) ) ;
#26906 = CARTESIAN_POINT ( 'NONE',  ( 10.75101814679000078, -2.478465696309000155, -7.438303690845000204 ) ) ;
#26905 = CARTESIAN_POINT ( 'NONE',  ( 10.57529832096847677, 3.253995305422127782, -7.044405226132214537 ) ) ;
#26907 = CARTESIAN_POINT ( 'NONE',  ( 7.754585461271813251, -5.335985935492750798, 8.613681351317808321 ) ) ;
#26908 = CARTESIAN_POINT ( 'NONE',  ( 10.24961784311999935, -4.184221496660999406, 9.286877953065999947 ) ) ;
#26909 = CARTESIAN_POINT ( 'NONE',  ( 2.215293907524999995, 1.603576596796000064, -2.837084241009999896 ) ) ;
#26910 = ORIENTED_EDGE ( 'NONE', *, *, #31881, .F. ) ;
#26911 = CARTESIAN_POINT ( 'NONE',  ( 24.14474040618317474, 12.92575721420310764, 3.214624011666622483 ) ) ;
#26912 = CARTESIAN_POINT ( 'NONE',  ( 10.71462282008599942, -3.476853648246800432, 6.656181553372300108 ) ) ;
#26913 = CARTESIAN_POINT ( 'NONE',  ( 11.45348876160960039, 3.114179898019400206, 6.578783887955899523 ) ) ;
#26914 = VERTEX_POINT ( 'NONE', #26836 ) ;
#26915 = CARTESIAN_POINT ( 'NONE',  ( 9.219964158774999419, 3.941185585667000169, -8.896279800194999865 ) ) ;
#26916 = CARTESIAN_POINT ( 'NONE',  ( 12.36031510016526092, 1.911905511008637149, -12.45410252665035600 ) ) ;
#26917 = EDGE_CURVE ( 'NONE', #54460, #49162, #68775, .T. ) ;
#26918 = CARTESIAN_POINT ( 'NONE',  ( 11.22191429142990060, -3.974927396630719922, 8.816028813488999916 ) ) ;
#26919 = ADVANCED_FACE ( 'NONE', ( #62840 ), #48153, .T. ) ;
#26920 = CARTESIAN_POINT ( 'NONE',  ( 7.947862523144673119, 4.896691652056699873, -6.386472708437699985 ) ) ;
#26921 = CARTESIAN_POINT ( 'NONE',  ( 18.15932194351565698, 2.660757700747661936, -13.63806486294889098 ) ) ;
#26922 = ORIENTED_EDGE ( 'NONE', *, *, #5918, .T. ) ;
#26923 = CARTESIAN_POINT ( 'NONE',  ( 23.60205915885299888, 11.56239291746998710, 3.974820703396001242 ) ) ;
#26924 = CARTESIAN_POINT ( 'NONE',  ( 5.732109839684041752, 0.9218200799623741393, -1.199500263597268690 ) ) ;
#26926 = ORIENTED_EDGE ( 'NONE', *, *, #23375, .F. ) ;
#26925 = VECTOR ( 'NONE', #29366, 1000.000000000000000 ) ;
#26927 = CARTESIAN_POINT ( 'NONE',  ( 9.583513540183334456, 5.250000000000000888, 7.336375382625531572 ) ) ;
#26928 = CARTESIAN_POINT ( 'NONE',  ( 11.58487348028854846, 3.117292544139400157, 7.022738645480499642 ) ) ;
#26929 = CARTESIAN_POINT ( 'NONE',  ( 9.634020792350998619, 3.042978295541999945, 8.588098960242001922 ) ) ;
#26930 = CARTESIAN_POINT ( 'NONE',  ( 10.48414939117999900, 4.098653981087000631, -9.351365234892998757 ) ) ;
#26931 = CARTESIAN_POINT ( 'NONE',  ( 25.59994555223600088, 1.356777910713891977, -11.13814279612289226 ) ) ;
#26932 = CARTESIAN_POINT ( 'NONE',  ( 11.03855816545999957, -2.974093234901999949, 8.716125417860000724 ) ) ;
#26933 = CARTESIAN_POINT ( 'NONE',  ( 18.05096829067923281, -0.5248261352964527227, -12.58906749861124119 ) ) ;
#26934 = AXIS2_PLACEMENT_3D ( 'NONE', #30246, #51216, #13481 ) ;
#26935 = CARTESIAN_POINT ( 'NONE',  ( 12.80505043854143388, 3.124999999999999556, -12.28374638332999602 ) ) ;
#26936 = CARTESIAN_POINT ( 'NONE',  ( 11.19102897915239936, -3.743141152489600110, -8.470038342183499935 ) ) ;
#26937 = CARTESIAN_POINT ( 'NONE',  ( 8.791232780412000736, 5.095085596809999728, 6.286981168432999922 ) ) ;
#26938 = ORIENTED_EDGE ( 'NONE', *, *, #47404, .F. ) ;
#26939 = ADVANCED_FACE ( 'NONE', ( #36981 ), #4454, .F. ) ;
#26940 = CARTESIAN_POINT ( 'NONE',  ( 10.91301932002725650, 2.749999999999998224, 7.200148911387370454 ) ) ;
#26941 = B_SPLINE_CURVE_WITH_KNOTS ( 'NONE', 3,
 ( #68336, #14536, #35853, #30608 ),
 .UNSPECIFIED., .F., .F.,
 ( 4, 4 ),
 ( 0.000000000000000000, 1.000000000000000000 ),
 .UNSPECIFIED. ) ;
#26942 = PLANE ( 'NONE',  #36116 ) ;
#26943 = CARTESIAN_POINT ( 'NONE',  ( 11.68591862085600219, 12.43715917573999974, 1.778745665763999950 ) ) ;
#26944 = EDGE_CURVE ( 'NONE', #50878, #30666, #26092, .T. ) ;
#26945 = CARTESIAN_POINT ( 'NONE',  ( 18.16715147695112620, 2.094590662098726241, 12.42468172752983868 ) ) ;
#26946 = AXIS2_PLACEMENT_3D ( 'NONE', #1724, #12219, #55212 ) ;
#26947 = CARTESIAN_POINT ( 'NONE',  ( 4.599999999999999645, 3.248109929747638347, -13.61799478206225622 ) ) ;
#26948 = CARTESIAN_POINT ( 'NONE',  ( 10.92020230602999931, 9.067058286522998500, 6.347630032935000166 ) ) ;
#26949 = CARTESIAN_POINT ( 'NONE',  ( 9.243268584279421773, -2.683782748811717855, 7.201188049543101322 ) ) ;
#26950 = CARTESIAN_POINT ( 'NONE',  ( 25.59997125372800042, -2.856414944279999979, 11.13959160109000024 ) ) ;
#26951 = ORIENTED_EDGE ( 'NONE', *, *, #27668, .F. ) ;
#26952 = CARTESIAN_POINT ( 'NONE',  ( 12.19613275390598695, -2.089545048426566964, 12.42553124896410566 ) ) ;
#26953 = CARTESIAN_POINT ( 'NONE',  ( 9.581038493598999395, -3.173653894988100355, -6.712036445818600150 ) ) ;
#26954 = DIRECTION ( 'NONE',  ( -1.000000000000000000, 0.000000000000000000, 0.000000000000000000 ) ) ;
#26955 = DIRECTION ( 'NONE',  ( 0.000000000000000000, 0.000000000000000000, 1.000000000000000000 ) ) ;
#26956 = CARTESIAN_POINT ( 'NONE',  ( 11.27256919669530077, -3.037654633983899899, 7.215672285280100517 ) ) ;
#26957 = CARTESIAN_POINT ( 'NONE',  ( 11.65456516821461008, 4.802916961510000249, -8.310318115935698913 ) ) ;
#26958 = CARTESIAN_POINT ( 'NONE',  ( 12.25981900110941503, 0.4746736627229529160, 12.59106879393900513 ) ) ;
#26959 = CARTESIAN_POINT ( 'NONE',  ( 0.2444343787449999583, 2.474918916286999782, -2.043501580946999852 ) ) ;
#26960 = CARTESIAN_POINT ( 'NONE',  ( 9.637701392160892055, 4.829637745207382871, -8.579854099904720144 ) ) ;
#26961 = CARTESIAN_POINT ( 'NONE',  ( 12.79295051314559650, 1.760910731560546116, 12.47634535177225068 ) ) ;
#26963 = CARTESIAN_POINT ( 'NONE',  ( 9.101287939753134992, 5.350063131615271139, -7.263153235713748046 ) ) ;
#26962 = CARTESIAN_POINT ( 'NONE',  ( 10.26492546752099955, 2.860918852493000486, -7.421078600323300023 ) ) ;
#26964 = CARTESIAN_POINT ( 'NONE',  ( 11.13764426047339917, 4.613828180779599997, -8.461511872390000022 ) ) ;
#26965 = CARTESIAN_POINT ( 'NONE',  ( 12.60217350508001743, 12.11433231916786823, -3.180975838886203277 ) ) ;
#26966 = CARTESIAN_POINT ( 'NONE',  ( 10.58470471959000037, 2.966809777448999874, -8.831980808885999679 ) ) ;
#26967 = CARTESIAN_POINT ( 'NONE',  ( 25.29986734212600297, -2.258942858049999725, 12.29419282279000036 ) ) ;
#26969 = CARTESIAN_POINT ( 'NONE',  ( 10.90000000164000049, -2.899999999992999733, 5.160242739040000082 ) ) ;
#26968 = CARTESIAN_POINT ( 'NONE',  ( 8.436984272513997851, 5.098716299041000433, 6.624027315230001101 ) ) ;
#26970 = CARTESIAN_POINT ( 'NONE',  ( 8.949580915942656034, 5.282157812751564485, 7.064122796597747111 ) ) ;
#26971 = ORIENTED_EDGE ( 'NONE', *, *, #67942, .F. ) ;
#26972 = DIRECTION ( 'NONE',  ( 1.000000000000000000, 0.000000000000000000, 0.000000000000000000 ) ) ;
#26973 = CARTESIAN_POINT ( 'NONE',  ( 10.19601354018254291, 4.999583552997727054, 8.268183399968641822 ) ) ;
#26974 = CARTESIAN_POINT ( 'NONE',  ( 17.64998052285767471, 0.7146386402664155479, -12.57972080578569063 ) ) ;
#26975 = DIRECTION ( 'NONE',  ( 1.000000000000000000, 0.000000000000000000, 0.000000000000000000 ) ) ;
#26977 = VECTOR ( 'NONE', #63384, 1000.000000000000000 ) ;
#26976 = B_SPLINE_CURVE_WITH_KNOTS ( 'NONE', 1,
 ( #48067, #53313 ),
 .UNSPECIFIED., .F., .F.,
 ( 2, 2 ),
 ( 0.000000000000000000, 1.000000000000000000 ),
 .UNSPECIFIED. ) ;
#26978 = CARTESIAN_POINT ( 'NONE',  ( 12.19536857401210384, -2.360987227094835106, 13.70197821715308528 ) ) ;
#26979 = CARTESIAN_POINT ( 'NONE',  ( 12.20052776708265974, 2.340020608672652269, 13.70605490524154746 ) ) ;
#26980 = CARTESIAN_POINT ( 'NONE',  ( 10.99999970531878013, 2.901368254139102376, 7.402706825368051469 ) ) ;
#26981 = EDGE_LOOP ( 'NONE', ( #26558, #11586, #64620, #44561 ) ) ;
#26982 = CARTESIAN_POINT ( 'NONE',  ( 10.89393020684999946, -5.250000000000000000, 7.500000000000000000 ) ) ;
#26983 = CARTESIAN_POINT ( 'NONE',  ( 11.41486084871699802, -5.207010770456999893, -7.825000000000000178 ) ) ;
#26984 = CARTESIAN_POINT ( 'NONE',  ( 19.39373726536100051, 11.26964301940000013, 0.000000000000000000 ) ) ;
#26985 = CARTESIAN_POINT ( 'NONE',  ( 10.82169598649000086, -3.233475335853099875, 7.043598424555200133 ) ) ;
#26986 = CARTESIAN_POINT ( 'NONE',  ( 18.15144633312240074, 2.312812061507714567, -12.49323956768624377 ) ) ;
#26987 = CARTESIAN_POINT ( 'NONE',  ( 8.611421496779771090, 4.936505472987223975, 6.052097162928508745 ) ) ;
#26988 = CARTESIAN_POINT ( 'NONE',  ( 11.46595122972049907, 4.343798595649099425, 8.295047870239098842 ) ) ;
#26989 = AXIS2_PLACEMENT_3D ( 'NONE', #61932, #4223, #14046 ) ;
#26990 = DIRECTION ( 'NONE',  ( -1.000000000000000000, 0.000000000000000000, 0.000000000000000000 ) ) ;
#26991 = CARTESIAN_POINT ( 'NONE',  ( 10.14521814679000045, -3.576528389491000048, -8.962725485696999783 ) ) ;
#26992 = CARTESIAN_POINT ( 'NONE',  ( 4.709193173016083200, -0.3926218265389190276, -1.460959015002473826 ) ) ;
#26993 = CARTESIAN_POINT ( 'NONE',  ( 11.50001544674999998, -6.312855374644978035, 10.89679704382941061 ) ) ;
#26994 = CARTESIAN_POINT ( 'NONE',  ( 24.14113557808980204, 9.152656354384584247, -9.126826426531142289 ) ) ;
#26995 = EDGE_CURVE ( 'NONE', #52199, #59620, #19403, .T. ) ;
#26996 = CARTESIAN_POINT ( 'NONE',  ( 24.30000000000000071, -2.548720605937000006, -12.21654710926000220 ) ) ;
#26997 = EDGE_CURVE ( 'NONE', #33729, #7601, #11106, .T. ) ;
#26998 = ORIENTED_EDGE ( 'NONE', *, *, #44761, .T. ) ;
#26999 = CARTESIAN_POINT ( 'NONE',  ( 8.763579719593998618, 4.815598936798999752, -8.835641302565999666 ) ) ;
#27000 = CARTESIAN_POINT ( 'NONE',  ( 11.32595391537419971, -3.283439621430300104, 7.013338090450799811 ) ) ;
#27001 = ORIENTED_EDGE ( 'NONE', *, *, #23935, .F. ) ;
#27002 = FACE_OUTER_BOUND ( 'NONE', #1811, .T. ) ;
#27003 = CARTESIAN_POINT ( 'NONE',  ( 11.50271932425157040, -4.187398418774900044, -8.764198628556998827 ) ) ;
#27004 = EDGE_LOOP ( 'NONE', ( #37241, #66283, #2785, #12883, #16038 ) ) ;
#27005 = CARTESIAN_POINT ( 'NONE',  ( 11.23078751119019891, 3.084247107206000038, 7.020904658857499925 ) ) ;
#27006 = CARTESIAN_POINT ( 'NONE',  ( 5.776807001587030754, -0.8882760547343830915, 0.7026214500576545285 ) ) ;
#27007 = CARTESIAN_POINT ( 'NONE',  ( 8.726787239609997471, -4.219532685969900498, -8.340498368324299250 ) ) ;
#27008 = CARTESIAN_POINT ( 'NONE',  ( 17.99211270977099986, -3.227071166021000082, 11.34499727797000013 ) ) ;
#27009 = CARTESIAN_POINT ( 'NONE',  ( 11.48522412107029922, -3.952868550833580130, -6.609122077774299164 ) ) ;
#27010 = CARTESIAN_POINT ( 'NONE',  ( 12.21236231059852706, -0.1994024998447188335, -13.89809293279807534 ) ) ;
#27011 = CARTESIAN_POINT ( 'NONE',  ( 7.001027640260497620, 0.6248985950805467926, -0.9570937137488223501 ) ) ;
#27012 = DIRECTION ( 'NONE',  ( -0.7071067792008891573, -0.5090928532370920800, -0.4907386978739921579 ) ) ;
#27013 = CARTESIAN_POINT ( 'NONE',  ( 13.25609597789999938, 11.48890257311000163, 1.688129671228999928 ) ) ;
#27014 = EDGE_LOOP ( 'NONE', ( #20153, #49936, #32881, #29399 ) ) ;
#27016 = FACE_BOUND ( 'NONE', #60669, .T. ) ;
#27015 = B_SPLINE_CURVE_WITH_KNOTS ( 'NONE', 3,
 ( #34850, #66302, #55481, #6884 ),
 .UNSPECIFIED., .F., .F.,
 ( 4, 4 ),
 ( 0.000000000000000000, 1.000000000000000000 ),
 .UNSPECIFIED. ) ;
#27017 = ORIENTED_EDGE ( 'NONE', *, *, #29648, .F. ) ;
#27018 = DIRECTION ( 'NONE',  ( 6.273181768770000388E-11, 6.273307657911000434E-11, -1.000000000000000000 ) ) ;
#27019 = VECTOR ( 'NONE', #36801, 1000.000000000000000 ) ;
#27020 = SURFACE_SIDE_STYLE ('',( #21756 ) ) ;
#27021 = ORIENTED_EDGE ( 'NONE', *, *, #21765, .T. ) ;
#27022 = DIRECTION ( 'NONE',  ( -0.000000000000000000, -0.000000000000000000, 1.000000000000000000 ) ) ;
#27023 = B_SPLINE_CURVE_WITH_KNOTS ( 'NONE', 3,
 ( #10774, #5872, #42600, #27210, #43290, #38732, #42942, #64936, #64595, #32120, #16021, #27907, #38382, #59023, #16364, #290, #22642, #63911 ),
 .UNSPECIFIED., .F., .F.,
 ( 4, 2, 2, 2, 2, 2, 2, 2, 4 ),
 ( 0.000000000000000000, 0.1250000000000000278, 0.2500000000000000000, 0.3749999999999999445, 0.4999999999999999445, 0.6249999999999998890, 0.7499999999999998890, 0.8750000000000000000, 1.000000000000000000 ),
 .UNSPECIFIED. ) ;
#27024 = CARTESIAN_POINT ( 'NONE',  ( 18.13653212795703595, -2.729361600744797833, -12.39516738912175242 ) ) ;
#27025 = EDGE_CURVE ( 'NONE', #12675, #44325, #65604, .T. ) ;
#27026 = CARTESIAN_POINT ( 'NONE',  ( 10.90437356726000040, -2.900476673752999890, 5.132566153004000320 ) ) ;
#27027 = CARTESIAN_POINT ( 'NONE',  ( 10.15434687351570631, 5.250000000000002665, -7.336375382625537789 ) ) ;
#27028 = CARTESIAN_POINT ( 'NONE',  ( 8.331682137624000006, -5.101289325373999262, 6.607176193198000647 ) ) ;
#27029 = CYLINDRICAL_SURFACE ( 'NONE', #58110, 1.999999999999999556 ) ;
#27030 = CARTESIAN_POINT ( 'NONE',  ( 12.27392385059252788, 0.3300666952397307008, 13.89473968862478870 ) ) ;
#27031 = ORIENTED_EDGE ( 'NONE', *, *, #50189, .F. ) ;
#27032 = CARTESIAN_POINT ( 'NONE',  ( 12.38412398422500083, 11.44428158143999852, -4.450268217599000486 ) ) ;
#27033 = CARTESIAN_POINT ( 'NONE',  ( 18.48246976263299857, 11.77475711121000224, -4.379243463657999769 ) ) ;
#27034 = CARTESIAN_POINT ( 'NONE',  ( 18.30003129334700063, 2.732683817159999862, -11.53064095410000078 ) ) ;
#27035 = CARTESIAN_POINT ( 'NONE',  ( 4.554236820976999667, -0.02212662165366999917, 1.482009051976999947 ) ) ;
#27036 = VECTOR ( 'NONE', #19643, 1000.000000000000000 ) ;
#27037 = CARTESIAN_POINT ( 'NONE',  ( 9.693589158772999426, 4.047146749018000200, -5.600703114891000034 ) ) ;
#27038 = CARTESIAN_POINT ( 'NONE',  ( 18.23590051321700400, -3.219096189435000088, 11.95421454054999977 ) ) ;
#27039 = AXIS2_PLACEMENT_3D ( 'NONE', #21609, #33841, #24375 ) ;
#27040 = CARTESIAN_POINT ( 'NONE',  ( 10.44486180556999955, -4.964082081645000422, -9.083599939499999110 ) ) ;
#27041 = EDGE_LOOP ( 'NONE', ( #65422, #10830, #25439, #37481 ) ) ;
#27042 = ORIENTED_EDGE ( 'NONE', *, *, #18008, .F. ) ;
#27043 = DIRECTION ( 'NONE',  ( 0.000000000000000000, 1.000000000000000000, 0.000000000000000000 ) ) ;
#27044 = CARTESIAN_POINT ( 'NONE',  ( 11.59999999999999964, -4.000000000000000000, -7.500000000000000000 ) ) ;
#27045 = CARTESIAN_POINT ( 'NONE',  ( 17.60411830284109058, -1.787854822559178825, 13.88537270421500658 ) ) ;
#27046 = FACE_OUTER_BOUND ( 'NONE', #50277, .T. ) ;
#27047 = CARTESIAN_POINT ( 'NONE',  ( 0.1499942179679999987, 1.689975037551097792, -2.199046806507070517 ) ) ;
#27048 = DIRECTION ( 'NONE',  ( 1.000000000000000000, 0.000000000000000000, 0.000000000000000000 ) ) ;
#27049 = CARTESIAN_POINT ( 'NONE',  ( 9.535355082327999554, 3.611978631017199959, -6.724663065681199647 ) ) ;
#27051 = CARTESIAN_POINT ( 'NONE',  ( 4.400000000000000355, -0.7080094843779000113, -0.8552562627201000245 ) ) ;
#27050 = CARTESIAN_POINT ( 'NONE',  ( 10.40629229006299816, -3.250213325543700016, 7.935348007132199122 ) ) ;
#27052 = CARTESIAN_POINT ( 'NONE',  ( 4.669609839683333874, -0.1963495408493606265, -1.500000000000000222 ) ) ;
#27053 = ORIENTED_EDGE ( 'NONE', *, *, #7400, .F. ) ;
#27054 = CARTESIAN_POINT ( 'NONE',  ( 11.26212378248529866, 3.384904051819500381, 8.663708617168998316 ) ) ;
#27055 = CARTESIAN_POINT ( 'NONE',  ( 9.256662271119999730, -4.025830307267999508, 9.295859242339000517 ) ) ;
#27056 = EDGE_CURVE ( 'NONE', #49271, #20862, #60368, .T. ) ;
#27057 = ADVANCED_FACE ( 'NONE', ( #33808 ), #68815, .T. ) ;
#27058 = CARTESIAN_POINT ( 'NONE',  ( 10.46755864497999866, 4.898932057185599653, 6.795973491698399371 ) ) ;
#27059 = CARTESIAN_POINT ( 'NONE',  ( 5.600000000706000236, 0.8000000000000000444, 3.149999999999999911 ) ) ;
#27060 = CARTESIAN_POINT ( 'NONE',  ( 9.409308287954999628, -2.634700736117999931, 8.920302460802998823 ) ) ;
#27061 = CARTESIAN_POINT ( 'NONE',  ( 17.99289217962403242, 2.946103266174030288, -12.33638055411239698 ) ) ;
#27062 = CARTESIAN_POINT ( 'NONE',  ( 16.13849254682300227, -3.245716968028000249, -11.43439984646999896 ) ) ;
#27063 = CARTESIAN_POINT ( 'NONE',  ( 9.558671671056998775, -4.990538396979200542, -7.666361006367900188 ) ) ;
#27064 = VECTOR ( 'NONE', #48798, 1000.000000000000000 ) ;
#27065 = CARTESIAN_POINT ( 'NONE',  ( 5.627703546035999871, 0.07142731211511998968, 1.320368930804000085 ) ) ;
#27066 = CARTESIAN_POINT ( 'NONE',  ( 6.999999999999999112, 8.540090292376646630, -4.496300658368356906 ) ) ;
#27067 = DIRECTION ( 'NONE',  ( -0.03487031647297116066, 1.485882206239048391E-07, -0.9993918455886323660 ) ) ;
#27068 = ORIENTED_EDGE ( 'NONE', *, *, #53256, .F. ) ;
#27069 = CARTESIAN_POINT ( 'NONE',  ( 12.23133867660517282, 0.2481623978058206392, -12.69674179789669211 ) ) ;
#27070 = CARTESIAN_POINT ( 'NONE',  ( 11.09672200990539892, 3.182132064022000328, -7.214709569664399247 ) ) ;
#27071 = CARTESIAN_POINT ( 'NONE',  ( 8.220491098714299838, -2.863432619444471250, 6.768885785334203931 ) ) ;
#27072 = CARTESIAN_POINT ( 'NONE',  ( 24.74075940428600262, -8.629078674936000226, 8.723342079101000124 ) ) ;
#27073 = CARTESIAN_POINT ( 'NONE',  ( 12.80505043854143388, 3.199698446519374517, 12.18695736643652694 ) ) ;
#27074 = ORIENTED_EDGE ( 'NONE', *, *, #50711, .T. ) ;
#27075 = CARTESIAN_POINT ( 'NONE',  ( 13.50000000000000178, -11.91410841793407194, -2.466613755756923876 ) ) ;
#27076 = ITEM_DEFINED_TRANSFORMATION ( 'NONE', 'NONE', #12851,  #9676 ) ;
#27077 = CARTESIAN_POINT ( 'NONE',  ( 10.48791429142999831, -3.983006558652820051, -6.608036045330599961 ) ) ;
#27078 = EDGE_CURVE ( 'NONE', #61078, #37966, #66948, .T. ) ;
#27079 = CARTESIAN_POINT ( 'NONE',  ( 5.500000000000000000, -1.300000000000000044, -9.662944685757000940 ) ) ;
#27080 = CARTESIAN_POINT ( 'NONE',  ( 7.975339216757299177, -5.350090185752664595, 7.499980949462679014 ) ) ;
#27081 = CYLINDRICAL_SURFACE ( 'NONE', #56289, 0.5000000000000000000 ) ;
#27083 = AXIS2_PLACEMENT_3D ( 'NONE', #23201, #48740, #497 ) ;
#27082 = CARTESIAN_POINT ( 'NONE',  ( 10.36325056272499978, 4.892034740700499817, -7.513220396995270001 ) ) ;
#27084 = ORIENTED_EDGE ( 'NONE', *, *, #30811, .T. ) ;
#27085 = EDGE_CURVE ( 'NONE', #47262, #48720, #32011, .T. ) ;
#27086 = CARTESIAN_POINT ( 'NONE',  ( 10.50244460374000077, -2.268915328469999881, 7.824865002012999504 ) ) ;
#27087 = CARTESIAN_POINT ( 'NONE',  ( 8.706426979769998908, -4.358851904410700584, -8.276078370613198842 ) ) ;
#27088 = ORIENTED_EDGE ( 'NONE', *, *, #36972, .T. ) ;
#27089 = DIRECTION ( 'NONE',  ( -3.790984134576917995E-06, 0.9659310420591794566, -0.2587995787710943851 ) ) ;
#27090 = CARTESIAN_POINT ( 'NONE',  ( 8.983793146794999629, -3.979464503892999439, 9.134080454305001595 ) ) ;
#27091 = CARTESIAN_POINT ( 'NONE',  ( 15.59211270977100128, 8.811013545169000594, 7.841491685545999069 ) ) ;
#27092 = EDGE_LOOP ( 'NONE', ( #37629, #36534, #58264, #1824 ) ) ;
#27093 = CARTESIAN_POINT ( 'NONE',  ( 14.46666666233133469, -9.187454791078211613, -8.213178404136472821 ) ) ;
#27094 = CARTESIAN_POINT ( 'NONE',  ( 7.265585841225999708, 4.636818559850000909, -5.710024136463999866 ) ) ;
#27095 = CARTESIAN_POINT ( 'NONE',  ( 10.19809687351566829, -3.672815144550895639, -6.282534154164608253 ) ) ;
#27096 = CARTESIAN_POINT ( 'NONE',  ( 9.489403898701906925, 4.927997357771009668, 8.480306757541997698 ) ) ;
#27097 = ORIENTED_EDGE ( 'NONE', *, *, #57646, .F. ) ;
#27098 = CARTESIAN_POINT ( 'NONE',  ( 9.910792656537999790, -3.869344906782000049, 5.882544796414999944 ) ) ;
#27099 = CARTESIAN_POINT ( 'NONE',  ( 11.60000000000000142, 4.072982449166800301, 8.552611010855414975 ) ) ;
#27100 = PRESENTATION_STYLE_ASSIGNMENT (( #59243 ) ) ;
#27101 = VERTEX_POINT ( 'NONE', #27518 ) ;
#27102 = B_SPLINE_CURVE_WITH_KNOTS ( 'NONE', 3,
 ( #49935, #2383, #55527, #18818, #29665, #23707 ),
 .UNSPECIFIED., .F., .F.,
 ( 4, 2, 4 ),
 ( 0.000000000000000000, 0.5000000000000000000, 1.000000000000000000 ),
 .UNSPECIFIED. ) ;
#27103 = CARTESIAN_POINT ( 'NONE',  ( 6.305026506349999948, 1.500000000000000000, 0.000000000000000000 ) ) ;
#27104 = CARTESIAN_POINT ( 'NONE',  ( 21.70000039307920048, -13.99999960683000033, -1.736066577384000004E-09 ) ) ;
#27105 = ORIENTED_EDGE ( 'NONE', *, *, #64563, .T. ) ;
#27106 = CARTESIAN_POINT ( 'NONE',  ( 5.500000000000000000, 0.000000000000000000, 0.000000000000000000 ) ) ;
#27107 = CARTESIAN_POINT ( 'NONE',  ( 18.17180742357641421, 0.1030366931658452667, -13.89950396794446874 ) ) ;
#27108 = CARTESIAN_POINT ( 'NONE',  ( 5.366426961083000435, -0.1673488337983000118, 1.406555471453999839 ) ) ;
#27109 = EDGE_CURVE ( 'NONE', #35633, #35196, #17727, .T. ) ;
#27110 = CARTESIAN_POINT ( 'NONE',  ( 11.60000000000000320, 3.905927825748640725, -6.471240206706528220 ) ) ;
#27111 = CARTESIAN_POINT ( 'NONE',  ( 16.32966272177200295, 3.529531741950000079, 11.96032165934999902 ) ) ;
#27112 = CARTESIAN_POINT ( 'NONE',  ( 11.30361999289329766, 3.455907502640805262, 8.657883396625690509 ) ) ;
#27113 = CARTESIAN_POINT ( 'NONE',  ( 7.000000000000000000, 0.000000000000000000, 0.000000000000000000 ) ) ;
#27114 = B_SPLINE_SURFACE_WITH_KNOTS ( 'NONE', 3, 3, ( 
 ( #14681, #52418, #4514, #24826, #47182, #36000, #62224, #68485, #41933, #9083, #68836, #25511, #67457, #68145, #57316, #15366, #20608, #30422, #36693, #19924, #51732, #51395, #30759, #10117, #31448, #26203, #20954, #35326, #8745, #3490, #3825, #4173, #11480, #53794, #5552 ),
 ( #1345, #6234, #21972, #59726, #11828, #661, #37036, #58351, #43312, #33168, #16725, #27575, #32820, #22662, #27925, #63590, #48901, #49235, #15708, #1006, #26893, #10453, #5212, #43660, #31793, #53111, #26549, #64957, #22318, #47875, #5891, #42622, #69180, #16385, #21291 ),
 ( #38403, #63931, #17070, #64617, #32480, #37715, #54485, #16043, #37374, #48556, #38055, #58694, #10798, #48206, #6585, #64271, #313, #27232, #32143, #53458, #21629, #42964, #59043, #11146, #59379, #54136, #18124, #65312, #8320, #66693, #24048, #7977, #33515, #12530, #65659 ),
 ( #29311, #29663, #44006, #50624, #7281, #17427, #54831, #45383, #60081, #50965, #38755, #18816, #2725, #12186, #55525, #23011, #6930, #66000, #3063, #28265, #61456, #49585, #50280, #1692, #44359, #34209, #7626, #55176, #13573, #28972, #56211, #2381, #39444, #17781, #60424 ) ),
 .UNSPECIFIED., .F., .F., .F.,
 ( 4, 4 ),
 ( 4, 1, 1, 1, 1, 1, 1, 1, 1, 1, 1, 1, 1, 1, 1, 1, 1, 1, 1, 1, 1, 1, 1, 1, 1, 1, 1, 1, 1, 1, 1, 1, 4 ),
 ( -0.1039370721279000015, 1.103937072127999963 ),
 ( -0.02000000000000000042, 0.01250000000000000069, 0.04499999999999999833, 0.07749999999999999944, 0.1100000000000000006, 0.1424999999999999878, 0.1749999999999999889, 0.2074999999999999900, 0.2399999999999999911, 0.2725000000000000200, 0.3049999999999999933, 0.3375000000000000222, 0.3699999999999999956, 0.4025000000000000244, 0.4349999999999999978, 0.4675000000000000266, 0.5000000000000000000, 0.5324999999999999734, 0.5649999999999999467, 0.5975000000000000311, 0.6300000000000000044, 0.6624999999999999778, 0.6949999999999999512, 0.7275000000000000355, 0.7600000000000000089, 0.7924999999999999822, 0.8249999999999999556, 0.8575000000000000400, 0.8900000000000000133, 0.9224999999999999867, 0.9549999999999999600, 0.9875000000000000444, 1.020000000000000018 ),
 .UNSPECIFIED. ) ;
#27115 = EDGE_LOOP ( 'NONE', ( #20611, #32014, #64037, #40327 ) ) ;
#27116 = CARTESIAN_POINT ( 'NONE',  ( 9.314550945856780118, -4.223514815909876319, 9.228465502814891863 ) ) ;
#27117 = ORIENTED_EDGE ( 'NONE', *, *, #50668, .T. ) ;
#27118 = CARTESIAN_POINT ( 'NONE',  ( 10.41185190929999926, 2.101586107686999938, 7.856266936613998553 ) ) ;
#27119 = CARTESIAN_POINT ( 'NONE',  ( 10.38052665877000003, 5.283793195606000026, -8.830196380017000024 ) ) ;
#27120 = DIRECTION ( 'NONE',  ( 1.000000000000000000, 0.000000000000000000, 0.000000000000000000 ) ) ;
#27121 = CARTESIAN_POINT ( 'NONE',  ( 12.33386765766680071, 2.911124516513513782, -13.57763168322026637 ) ) ;
#27122 = CIRCLE ( 'NONE', #20422, 11.84999999999999964 ) ;
#27123 = DIRECTION ( 'NONE',  ( -1.000000000000000000, 0.000000000000000000, 0.000000000000000000 ) ) ;
#27124 = CARTESIAN_POINT ( 'NONE',  ( 25.59037064052600030, 2.738643240522000255, 11.22408785382000040 ) ) ;
#27125 = CARTESIAN_POINT ( 'NONE',  ( 17.86832607310548937, -0.5412024733746028105, 13.88582008197803042 ) ) ;
#27126 = CARTESIAN_POINT ( 'NONE',  ( 9.400463768223922045, -5.265153800075048629, -8.707768634079092962 ) ) ;
#27127 = ORIENTED_EDGE ( 'NONE', *, *, #41790, .T. ) ;
#27128 = CARTESIAN_POINT ( 'NONE',  ( 12.32512809855874636, 0.4004137791749501352, 13.89223825656494249 ) ) ;
#27129 = CARTESIAN_POINT ( 'NONE',  ( 11.95348876160960039, -4.885820101980599794, 6.578783887955899523 ) ) ;
#27130 = DIRECTION ( 'NONE',  ( 0.000000000000000000, 0.000000000000000000, -1.000000000000000000 ) ) ;
#27131 = CARTESIAN_POINT ( 'NONE',  ( 17.55505043854144276, -0.6250000000000001110, -13.88107975066922428 ) ) ;
#27132 = CARTESIAN_POINT ( 'NONE',  ( 9.250897313459001126, -4.135077143711000325, 9.175520401071999288 ) ) ;
#27134 = DIRECTION ( 'NONE',  ( -1.000000000000000000, 0.000000000000000000, 0.000000000000000000 ) ) ;
#27133 = CARTESIAN_POINT ( 'NONE',  ( 9.634020792350998619, 3.042978295541999945, 8.588098960242001922 ) ) ;
#27135 = CARTESIAN_POINT ( 'NONE',  ( 10.15303300763299887, 4.787165141710600480, -8.325626572044798834 ) ) ;
#27136 = CARTESIAN_POINT ( 'NONE',  ( 9.099999999999999645, -4.000000000000000000, 7.500000000000000000 ) ) ;
#27137 = DIRECTION ( 'NONE',  ( 1.000000000000000000, 1.845552576849000024E-09, -8.865321528282000745E-13 ) ) ;
#27138 = EDGE_CURVE ( 'NONE', #64274, #52415, #59890, .T. ) ;
#27139 = EDGE_CURVE ( 'NONE', #8792, #4832, #47768, .T. ) ;
#27140 = CARTESIAN_POINT ( 'NONE',  ( 17.91892138177005123, -0.5082598251325827210, 12.68630931495243352 ) ) ;
#27141 = CYLINDRICAL_SURFACE ( 'NONE', #22713, 1.250000000000000222 ) ;
#27142 = DIRECTION ( 'NONE',  ( -1.000000000000000000, 0.000000000000000000, 0.000000000000000000 ) ) ;
#27143 = ORIENTED_EDGE ( 'NONE', *, *, #15530, .F. ) ;
#27144 = CARTESIAN_POINT ( 'NONE',  ( 8.572269353210000276, -2.606998386752999775, 6.345764833140000505 ) ) ;
#27145 = CARTESIAN_POINT ( 'NONE',  ( 9.070789158774999805, 5.349936549139000519, -7.138437102151999447 ) ) ;
#27146 = EDGE_CURVE ( 'NONE', #6055, #41535, #14140, .T. ) ;
#27147 = CARTESIAN_POINT ( 'NONE',  ( 5.500000000000000000, 0.000000000000000000, 0.000000000000000000 ) ) ;
#27148 = CARTESIAN_POINT ( 'NONE',  ( 5.599997304680200294, -13.94845324556000143, 4.312847325879000770 ) ) ;
#27149 = B_SPLINE_CURVE_WITH_KNOTS ( 'NONE', 3,
 ( #27713, #53584, #43446, #53920, #11608, #6021 ),
 .UNSPECIFIED., .F., .F.,
 ( 4, 1, 1, 4 ),
 ( 0.000000000000000000, 0.1550125385928093902, 0.7488612291951105560, 1.000000000000000000 ),
 .UNSPECIFIED. ) ;
#27150 = CARTESIAN_POINT ( 'NONE',  ( 0.8998509817850999237, 3.128647331775999962, -1.414269894618000123 ) ) ;
#27151 = CARTESIAN_POINT ( 'NONE',  ( 8.150000662387999029, -3.446132268436000216E-13, -3.324010876891999568E-14 ) ) ;
#27152 = CARTESIAN_POINT ( 'NONE',  ( 11.06878584122999953, 5.318802051720999735, -7.168446171767000052 ) ) ;
#27153 = VERTEX_POINT ( 'NONE', #7228 ) ;
#27154 = CARTESIAN_POINT ( 'NONE',  ( 9.373082992855458428, 2.782568642349716459, -7.172827875665085173 ) ) ;
#27155 = DIRECTION ( 'NONE',  ( 1.000000000000000000, 0.000000000000000000, 0.000000000000000000 ) ) ;
#27156 = CARTESIAN_POINT ( 'NONE',  ( 17.88886072129108840, 3.119102935781167041, -12.20783478086261020 ) ) ;
#27157 = CARTESIAN_POINT ( 'NONE',  ( 7.215222283847193552, -2.650817894710479905, 7.677089056594191163 ) ) ;
#27158 = CARTESIAN_POINT ( 'NONE',  ( 8.566232780412001091, 5.212261578733999201, 6.157186134061999994 ) ) ;
#27159 = ORIENTED_EDGE ( 'NONE', *, *, #15560, .F. ) ;
#27160 = CARTESIAN_POINT ( 'NONE',  ( 5.427515767744000463, 0.1599529892900000139, 1.501782300629000089 ) ) ;
#27161 = CARTESIAN_POINT ( 'NONE',  ( 8.303904719589001004, 4.466585441010000324, -5.831585202652000532 ) ) ;
#27162 = CARTESIAN_POINT ( 'NONE',  ( 8.427572861040259156, -2.321778634991549239, 7.972824082824569558 ) ) ;
#27163 = CARTESIAN_POINT ( 'NONE',  ( 8.999265421555000088, -4.240073379563900069, 6.258138488953999712 ) ) ;
#27164 = VERTEX_POINT ( 'NONE', #39388 ) ;
#27165 = CARTESIAN_POINT ( 'NONE',  ( 16.07057712374000147, -3.541973289920000045, -11.85942491664999920 ) ) ;
#27166 = CARTESIAN_POINT ( 'NONE',  ( 11.55275411606000269, 11.58372484989999940, 1.667203446842000059 ) ) ;
#27167 = ORIENTED_EDGE ( 'NONE', *, *, #32444, .F. ) ;
#27168 = PRODUCT_DEFINITION_SHAPE ( 'NONE', 'NONE',  #69207 ) ;
#27169 = CYLINDRICAL_SURFACE ( 'NONE', #45163, 1.350000000000000533 ) ;
#27170 = DIRECTION ( 'NONE',  ( 0.000000000000000000, -1.000000000000000000, 0.000000000000000000 ) ) ;
#27171 = CARTESIAN_POINT ( 'NONE',  ( 17.65691712177036976, -0.6169787192598745751, -13.88156336867696616 ) ) ;
#27172 = ORIENTED_EDGE ( 'NONE', *, *, #60389, .F. ) ;
#27173 = CARTESIAN_POINT ( 'NONE',  ( 16.10006098462790902, -8.380959734829355412, -8.092216891312066451 ) ) ;
#27174 = CARTESIAN_POINT ( 'NONE',  ( 8.767879976495999372, -3.394455611366999914, -6.293427637271999942 ) ) ;
#27175 = CARTESIAN_POINT ( 'NONE',  ( 10.57102344389999971, 3.237334151971200225, -7.037150754511299233 ) ) ;
#27176 = CARTESIAN_POINT ( 'NONE',  ( 12.60202002655570652, 3.091459147703855770, -12.29390037902081545 ) ) ;
#27177 = CARTESIAN_POINT ( 'NONE',  ( 11.80579707368350029, -4.634832087857400751, 8.609190966793999422 ) ) ;
#27178 = ORIENTED_EDGE ( 'NONE', *, *, #19823, .F. ) ;
#27179 = CARTESIAN_POINT ( 'NONE',  ( 8.796579719592999780, 2.368264398678999516, 7.410200237937000445 ) ) ;
#27180 = ORIENTED_EDGE ( 'NONE', *, *, #31210, .T. ) ;
#27181 = CARTESIAN_POINT ( 'NONE',  ( 9.248087964304163577, -3.672831456759381830, -6.282577178243119675 ) ) ;
#27182 = AXIS2_PLACEMENT_3D ( 'NONE', #51569, #19762, #18741 ) ;
#27183 = CARTESIAN_POINT ( 'NONE',  ( 18.28019316479975132, 0.1878083608816567551, 12.60000737103649016 ) ) ;
#27184 = CARTESIAN_POINT ( 'NONE',  ( 11.02038863743000086, 5.796704460786999746, -5.015990784938999525 ) ) ;
#27185 = ORIENTED_EDGE ( 'NONE', *, *, #19282, .F. ) ;
#27186 = CARTESIAN_POINT ( 'NONE',  ( 12.20865459317947632, -2.312811904845647248, -12.49320495213145676 ) ) ;
#27187 = EDGE_CURVE ( 'NONE', #49213, #16713, #28564, .T. ) ;
#27188 = AXIS2_PLACEMENT_3D ( 'NONE', #58401, #68886, #5597 ) ;
#27189 = DIRECTION ( 'NONE',  ( 1.000000000000000000, 0.000000000000000000, -0.000000000000000000 ) ) ;
#27190 = CARTESIAN_POINT ( 'NONE',  ( 24.35365242081699932, -8.885108761826009172, 7.331500822316997734 ) ) ;
#27191 = CARTESIAN_POINT ( 'NONE',  ( 0.1500001264883999708, -2.724999873498000103, -2.408237085193000045E-10 ) ) ;
#27192 = CARTESIAN_POINT ( 'NONE',  ( 12.17639632831540020, -2.882401473261796632, -13.70008095139100313 ) ) ;
#27193 = EDGE_CURVE ( 'NONE', #67955, #41017, #44435, .T. ) ;
#27194 = CARTESIAN_POINT ( 'NONE',  ( 10.64949279009019989, -4.260984538213099526, -8.468936491037499792 ) ) ;
#27195 = CARTESIAN_POINT ( 'NONE',  ( 11.58810207955109917, 3.203462856645999945, -7.174999999999999822 ) ) ;
#27196 = CARTESIAN_POINT ( 'NONE',  ( 17.99403275303998129, -3.052983340820298874, 12.22453705205519192 ) ) ;
#27197 = ORIENTED_EDGE ( 'NONE', *, *, #43457, .F. ) ;
#27198 = CARTESIAN_POINT ( 'NONE',  ( 11.83003632436370012, -5.243255406354000669, -7.209663534847899236 ) ) ;
#27199 = EDGE_LOOP ( 'NONE', ( #17802, #41025, #51788, #10291 ) ) ;
#27200 = DIRECTION ( 'NONE',  ( -1.000000000000000000, 3.552713678845000257E-14, -5.329070518267999577E-14 ) ) ;
#27201 = CARTESIAN_POINT ( 'NONE',  ( 12.09999999999999964, -2.935681553670999921, 6.844464917182299324 ) ) ;
#27202 = CARTESIAN_POINT ( 'NONE',  ( 10.35427764559999986, 4.879113829302000660, -8.944031201701999834 ) ) ;
#27203 = CARTESIAN_POINT ( 'NONE',  ( 10.68375832677999959, -4.547311397465000127, -8.749131152219000285 ) ) ;
#27204 = CARTESIAN_POINT ( 'NONE',  ( 12.80505043854144276, -0.6250000000000001110, 13.88107975066923316 ) ) ;
#27205 = CARTESIAN_POINT ( 'NONE',  ( 8.283628111110997949, 2.878995628920999916, -6.357604486408997779 ) ) ;
#27206 = DIRECTION ( 'NONE',  ( 1.000000000000000000, 0.000000000000000000, 0.000000000000000000 ) ) ;
#27207 = ORIENTED_EDGE ( 'NONE', *, *, #42791, .F. ) ;
#27208 = CARTESIAN_POINT ( 'NONE',  ( 18.35192027319500241, 2.803655468537999962, 11.45922931039000048 ) ) ;
#27209 = CARTESIAN_POINT ( 'NONE',  ( 9.290193290418001126, 2.377818438998999806, 7.540992072119000689 ) ) ;
#27210 = CARTESIAN_POINT ( 'NONE',  ( 2.259306799209333416, -3.058252359239909346, 1.762666431298136605 ) ) ;
#27211 = CARTESIAN_POINT ( 'NONE',  ( 11.44501463001509833, -3.527519786474400121, 8.256737112932800216 ) ) ;
#27212 = CARTESIAN_POINT ( 'NONE',  ( 18.53711938375299795, 2.638714702496000264, -11.30796021345999947 ) ) ;
#27213 = CIRCLE ( 'NONE', #12695, 1.549999999999999600 ) ;
#27214 = CARTESIAN_POINT ( 'NONE',  ( 10.87850165404999991, 9.620987454954001095, -5.906477034301000018 ) ) ;
#27215 = CARTESIAN_POINT ( 'NONE',  ( 7.100000000000317613, 2.856882225463113656, -6.715485463213433093 ) ) ;
#27216 = CARTESIAN_POINT ( 'NONE',  ( 6.628782096734860296, -1.096045291018389101, 0.8220666491861405856 ) ) ;
#27217 = EDGE_CURVE ( 'NONE', #57302, #19484, #29462, .T. ) ;
#27218 = CARTESIAN_POINT ( 'NONE',  ( 8.115081613917173087, 5.350113345104855256, -7.499995474391613293 ) ) ;
#27219 = CARTESIAN_POINT ( 'NONE',  ( 11.75766493321900086, -3.377423597792000187, 11.11036430104999972 ) ) ;
#27220 = ORIENTED_EDGE ( 'NONE', *, *, #47753, .F. ) ;
#27221 = CARTESIAN_POINT ( 'NONE',  ( 21.10000000000000142, 0.000000000000000000, 0.000000000000000000 ) ) ;
#27222 = CARTESIAN_POINT ( 'NONE',  ( 7.161163246430999330, 0.5195473280092000046, 1.006186743336999978 ) ) ;
#27223 = EDGE_CURVE ( 'NONE', #67676, #33656, #58789, .T. ) ;
#27224 = EDGE_CURVE ( 'NONE', #27749, #25016, #46525, .T. ) ;
#27225 = CARTESIAN_POINT ( 'NONE',  ( 18.17486206286450923, 2.582858869840499061, 13.65550477088448034 ) ) ;
#27226 = CARTESIAN_POINT ( 'NONE',  ( 24.25375554908000097, 8.963946465867000057, -8.909846166044999904 ) ) ;
#27227 = CARTESIAN_POINT ( 'NONE',  ( 11.01456785386839954, -4.946394603182100447, -8.136888821800198457 ) ) ;
#27228 = VERTEX_POINT ( 'NONE', #11771 ) ;
#27229 = CARTESIAN_POINT ( 'NONE',  ( 5.000000000000000000, 0.000000000000000000, 0.000000000000000000 ) ) ;
#27230 = CARTESIAN_POINT ( 'NONE',  ( 7.897954719591000483, 3.608525622520999843, 5.913376237674000002 ) ) ;
#27231 = AXIS2_PLACEMENT_3D ( 'NONE', #6902, #2354, #23677 ) ;
#27233 = DIRECTION ( 'NONE',  ( 0.000000000000000000, -1.000000000000000000, 0.000000000000000000 ) ) ;
#27232 = CARTESIAN_POINT ( 'NONE',  ( 9.102795280413999990, 3.071719032003000116, -6.037263251225000182 ) ) ;
#27234 = CARTESIAN_POINT ( 'NONE',  ( 17.55505043854147118, -3.125000000000000000, -25.00000000000000000 ) ) ;
#27235 = VERTEX_POINT ( 'NONE', #56498 ) ;
#27236 = CARTESIAN_POINT ( 'NONE',  ( 10.03612394578000000, 3.011788727150999989, 8.746962581836999817 ) ) ;
#27238 = CARTESIAN_POINT ( 'NONE',  ( 18.23517937092941921, -2.264898893658558787, -13.81558401759068744 ) ) ;
#27237 = B_SPLINE_CURVE_WITH_KNOTS ( 'NONE', 3,
 ( #46660, #13479, #29909, #50870 ),
 .UNSPECIFIED., .F., .F.,
 ( 4, 4 ),
 ( 0.000000000000000000, 1.000000000000000000 ),
 .UNSPECIFIED. ) ;
#27239 = CARTESIAN_POINT ( 'NONE',  ( 10.50180110216399854, 3.143606124884799957, 8.023010882787499298 ) ) ;
#27240 = CARTESIAN_POINT ( 'NONE',  ( 10.92717634842000152, -5.023656093247000243, 8.718039182945998888 ) ) ;
#27241 = CARTESIAN_POINT ( 'NONE',  ( 8.951355646795001064, -2.821866379289000193, 6.127148604720000336 ) ) ;
#27242 = ORIENTED_EDGE ( 'NONE', *, *, #30074, .F. ) ;
#27243 = CARTESIAN_POINT ( 'NONE',  ( 9.003209435575312725, -2.902877702503883661, 6.186420784434704778 ) ) ;
#27244 = EDGE_CURVE ( 'NONE', #53059, #24256, #26414, .T. ) ;
#27246 = CARTESIAN_POINT ( 'NONE',  ( 10.01676935320999995, -4.324998011277000565, -9.154075058362000306 ) ) ;
#27245 = LINE ( 'NONE', #17441, #20976 ) ;
#27247 = CARTESIAN_POINT ( 'NONE',  ( 7.897386357334326590, -2.614547605125981722, 8.551323849536911936 ) ) ;
#27248 = CARTESIAN_POINT ( 'NONE',  ( 10.52638330645999964, -2.451090818816000105, 6.282756943804999494 ) ) ;
#27249 = CARTESIAN_POINT ( 'NONE',  ( 23.61341080715499885, 3.134550972388999934, 13.53707874230000030 ) ) ;
#27251 = VERTEX_POINT ( 'NONE', #19435 ) ;
#27250 = B_SPLINE_CURVE_WITH_KNOTS ( 'NONE', 3,
 ( #67832, #57340, #57685, #5040 ),
 .UNSPECIFIED., .F., .F.,
 ( 4, 4 ),
 ( 0.000000000000000000, 1.000000000000000000 ),
 .UNSPECIFIED. ) ;
#27252 = CARTESIAN_POINT ( 'NONE',  ( 24.97034696419939337, -11.51453382931811475, -3.225688335446051269 ) ) ;
#27253 = CARTESIAN_POINT ( 'NONE',  ( 12.08071932425156980, -4.167269912168199753, 6.371589232479998977 ) ) ;
#27254 = CARTESIAN_POINT ( 'NONE',  ( 10.44426222744799837, 3.013556901740999994, 6.687444528363699625 ) ) ;
#27255 = VERTEX_POINT ( 'NONE', #14201 ) ;
#27256 = B_SPLINE_SURFACE_WITH_KNOTS ( 'NONE', 3, 3, ( 
 ( #56152, #61058, #39387, #55470, #60708, #23995, #7569, #18759, #28920, #13178, #2328, #65603, #8601, #34506, #23648, #17726, #39049, #60367, #18070, #44987, #19780, #68343, #9272, #15569, #68005, #62421, #9972, #14199, #41450, #46007, #40758, #20120, #62758, #4373, #42142 ),
 ( #14877, #20461, #63447, #62080, #35525, #31308, #56846, #14542, #67656, #52620, #67316, #35860, #25708, #25024, #8944, #63094, #30284, #51588, #31649, #4713, #57176, #3683, #15219, #36897, #5068, #46355, #58212, #36544, #41789, #10316, #30616, #25363, #52971, #68692, #47040 ),
 ( #57871, #19434, #26057, #47386, #36200, #57514, #20807, #9620, #51929, #41108, #4025, #30965, #46701, #52279, #10656, #22179, #49098, #58902, #37917, #63792, #16928, #27789, #5417, #21155, #48068, #11006, #5751, #59585, #59237, #47732, #32681, #48757, #1210, #32344, #53315 ),
 ( #33026, #26754, #22520, #27435, #43519, #21489, #53994, #43861, #64817, #38260, #11686, #11342, #12042, #65164, #53658, #515, #21832, #15901, #54338, #43163, #6440, #17284, #172, #59931, #42482, #27094, #6096, #37233, #48409, #38611, #33375, #37568, #42823, #58550, #64131 ) ),
 .UNSPECIFIED., .F., .F., .F.,
 ( 4, 4 ),
 ( 4, 1, 1, 1, 1, 1, 1, 1, 1, 1, 1, 1, 1, 1, 1, 1, 1, 1, 1, 1, 1, 1, 1, 1, 1, 1, 1, 1, 1, 1, 1, 1, 4 ),
 ( -0.1039370721279000015, 1.103937072127999963 ),
 ( -0.01999999999998999800, 0.01250000000001000137, 0.04499999999999999833, 0.07749999999999999944, 0.1100000000000000006, 0.1424999999999999878, 0.1749999999999999889, 0.2074999999999999900, 0.2399999999999999911, 0.2725000000000000200, 0.3049999999999999933, 0.3375000000000000222, 0.3699999999999999956, 0.4025000000000000244, 0.4349999999999999978, 0.4675000000000000266, 0.5000000000000000000, 0.5324999999999999734, 0.5649999999999999467, 0.5975000000000000311, 0.6300000000000000044, 0.6624999999999999778, 0.6949999999999999512, 0.7275000000000000355, 0.7600000000000000089, 0.7924999999999999822, 0.8249999999999999556, 0.8575000000000000400, 0.8900000000000000133, 0.9224999999999999867, 0.9549999999999999600, 0.9875000000000000444, 1.020000000000000018 ),
 .UNSPECIFIED. ) ;
#27257 = CARTESIAN_POINT ( 'NONE',  ( 9.070789158774999805, 5.349936549139000519, -7.138437102151999447 ) ) ;
#27258 = CARTESIAN_POINT ( 'NONE',  ( 12.16862919417105537, 2.135222488495307935, -12.41776696322756912 ) ) ;
#27259 = CARTESIAN_POINT ( 'NONE',  ( 11.34657802013509986, -5.315911219205999849, 7.530633716161349689 ) ) ;
#27260 = ORIENTED_EDGE ( 'NONE', *, *, #39025, .F. ) ;
#27261 = LINE ( 'NONE', #64298, #27339 ) ;
#27262 = AXIS2_PLACEMENT_3D ( 'NONE', #14917, #30319, #36239 ) ;
#27263 = CARTESIAN_POINT ( 'NONE',  ( 18.18005043852537383, 2.520325007585968002, -13.66916896904722734 ) ) ;
#27264 = VERTEX_POINT ( 'NONE', #35185 ) ;
#27265 = CARTESIAN_POINT ( 'NONE',  ( 7.726441940376999717, -2.630475685621000093, 6.995953627589999613 ) ) ;
#27266 = CARTESIAN_POINT ( 'NONE',  ( 21.35000154058000277, -12.59999999999999964, 0.000000000000000000 ) ) ;
#27267 = ORIENTED_EDGE ( 'NONE', *, *, #37397, .F. ) ;
#27268 = CARTESIAN_POINT ( 'NONE',  ( 12.61585440497584187, -3.174879747171414746, -12.19344691178323181 ) ) ;
#27269 = CARTESIAN_POINT ( 'NONE',  ( 11.28949010443639978, 5.000675062740000065, 7.425165037173959703 ) ) ;
#27270 = EDGE_CURVE ( 'NONE', #47324, #1148, #23617, .T. ) ;
#27271 = CARTESIAN_POINT ( 'NONE',  ( 10.87521525736000072, 4.831064930369000088, 6.312796576761000367 ) ) ;
#27272 = CARTESIAN_POINT ( 'NONE',  ( 11.04467482811000067, 2.754798779176999890, -5.185341710892000577 ) ) ;
#27273 = CARTESIAN_POINT ( 'NONE',  ( 7.826132327310000747, 5.086383815897999483, 6.522343373212003748 ) ) ;
#27274 = CARTESIAN_POINT ( 'NONE',  ( 9.520803773887999810, -3.270557529354000348, 5.711489293131999823 ) ) ;
#27275 = CARTESIAN_POINT ( 'NONE',  ( 14.02341781689399980, 9.526752659074999130, 8.190681853965998016 ) ) ;
#27276 = CARTESIAN_POINT ( 'NONE',  ( 17.96724410757352786, 0.4699213205053987541, -12.68829855189362732 ) ) ;
#27277 = ADVANCED_FACE ( 'NONE', ( #45331 ), #8603, .F. ) ;
#27278 = CARTESIAN_POINT ( 'NONE',  ( 12.80505043854143388, 1.875000000000000000, -12.57545641911172751 ) ) ;
#27279 = CARTESIAN_POINT ( 'NONE',  ( 11.03918313518939875, -4.707599264529200411, -8.394758848575399668 ) ) ;
#27280 = CARTESIAN_POINT ( 'NONE',  ( 8.470295280410999439, 4.255646040929000229, 9.114085578076998928 ) ) ;
#27281 = ORIENTED_EDGE ( 'NONE', *, *, #37013, .F. ) ;
#27282 = B_SPLINE_CURVE_WITH_KNOTS ( 'NONE', 1,
 ( #10991, #15556 ),
 .UNSPECIFIED., .F., .F.,
 ( 2, 2 ),
 ( 0.000000000000000000, 1.000000000000000000 ),
 .UNSPECIFIED. ) ;
#27283 = AXIS2_PLACEMENT_3D ( 'NONE', #68256, #31226, #15482 ) ;
#27284 = CARTESIAN_POINT ( 'NONE',  ( 25.29989948031900227, 2.596966625103000137, -11.35305524894999962 ) ) ;
#27285 = CARTESIAN_POINT ( 'NONE',  ( 24.57788509281863298, -8.817303531637588065, -9.247882801739393699 ) ) ;
#27286 = CARTESIAN_POINT ( 'NONE',  ( 11.61689913334100055, 12.44392429648999965, 1.730928413625999918 ) ) ;
#27287 = AXIS2_PLACEMENT_3D ( 'NONE', #62157, #14952, #25099 ) ;
#27288 = CARTESIAN_POINT ( 'NONE',  ( 18.13320831056631732, 2.045970293963734310, 12.43278322311361883 ) ) ;
#27289 = CARTESIAN_POINT ( 'NONE',  ( 5.000000000000000000, 0.6153846153845999867, -2.423076923076999734 ) ) ;
#27290 = CARTESIAN_POINT ( 'NONE',  ( 11.12453464744999998, 7.791996397176999878, 6.679342906043000738 ) ) ;
#27291 = CARTESIAN_POINT ( 'NONE',  ( 9.701570984676626708, -4.444002162597382011, 6.746080675052237297 ) ) ;
#27292 = CARTESIAN_POINT ( 'NONE',  ( 12.80505043854143388, 3.124999999999999556, -12.28374638332999602 ) ) ;
#27293 = EDGE_LOOP ( 'NONE', ( #17492, #42960, #822 ) ) ;
#27294 = CARTESIAN_POINT ( 'NONE',  ( 12.56948062052972936, -3.161141996800568066, 12.19701735778311580 ) ) ;
#27295 = CARTESIAN_POINT ( 'NONE',  ( 8.871822372493998188, -4.328199826929600036, -8.573651380901999630 ) ) ;
#27296 = CARTESIAN_POINT ( 'NONE',  ( 15.99981196018700125, -1.620925615952999665E-13, 0.000000000000000000 ) ) ;
#27297 = CARTESIAN_POINT ( 'NONE',  ( 9.236413463905998711, -3.915843685459630574, 6.617590440947399344 ) ) ;
#27298 = CARTESIAN_POINT ( 'NONE',  ( 10.35410941423799791, 4.742797679580299963, -6.825313060354999628 ) ) ;
#27299 = CARTESIAN_POINT ( 'NONE',  ( 12.58342066637853129, 0.6849607937330760565, 12.58136878870645248 ) ) ;
#27300 = CARTESIAN_POINT ( 'NONE',  ( 8.111573341229000533, 3.326263523254000098, 8.794511546544999447 ) ) ;
#27301 = FACE_OUTER_BOUND ( 'NONE', #57009, .T. ) ;
#27302 = CARTESIAN_POINT ( 'NONE',  ( 12.23528344688399017, 2.757674802278836879, 12.38780605717373184 ) ) ;
#27303 = FACE_BOUND ( 'NONE', #66259, .T. ) ;
#27304 = CARTESIAN_POINT ( 'NONE',  ( 10.22687885159599830, 5.132709421626000079, -7.364871923548499844 ) ) ;
#27305 = CARTESIAN_POINT ( 'NONE',  ( 11.89965592520902327, 11.89526654130151329, -3.923396420608070922 ) ) ;
#27306 = EDGE_CURVE ( 'NONE', #27904, #57225, #3010, .T. ) ;
#27307 = CARTESIAN_POINT ( 'NONE',  ( 10.38726084123000071, 2.888676266723000374, -6.716337836090000124 ) ) ;
#27308 = CARTESIAN_POINT ( 'NONE',  ( 11.10000000009000054, -5.300000000088999741, -6.571291220400000022 ) ) ;
#27310 = CARTESIAN_POINT ( 'NONE',  ( 12.21071179159800124, 2.693740719347354151, 12.40432020966558113 ) ) ;
#27309 = CARTESIAN_POINT ( 'NONE',  ( 7.903774407030003779, 5.139635483293002238, 6.776036904885998524 ) ) ;
#27311 = CARTESIAN_POINT ( 'NONE',  ( 10.98768472638000127, 7.408460564924999936, -6.159405844198999169 ) ) ;
#27312 = ORIENTED_EDGE ( 'NONE', *, *, #1431, .T. ) ;
#27313 = CIRCLE ( 'NONE', #23968, 1.549999999999999156 ) ;
#27314 = CARTESIAN_POINT ( 'NONE',  ( 12.44244977486500048, 0.5091670850904397305, 12.68626057781341210 ) ) ;
#27315 = DIRECTION ( 'NONE',  ( 0.5298945044129969029, -0.5996714842328959572, 0.5996715144066958603 ) ) ;
#27316 = CARTESIAN_POINT ( 'NONE',  ( 12.01640417260427007, -11.69872868927379272, 4.475294149990396875 ) ) ;
#27317 = CYLINDRICAL_SURFACE ( 'NONE', #62554, 0.5000000000000004441 ) ;
#27318 = CARTESIAN_POINT ( 'NONE',  ( 12.08020514495816400, -2.544320517268841453, 13.76688091865072572 ) ) ;
#27319 = LINE ( 'NONE', #48645, #26376 ) ;
#27320 = DIRECTION ( 'NONE',  ( -1.000000000000000000, -1.776356839465000168E-14, 0.000000000000000000 ) ) ;
#27321 = ORIENTED_EDGE ( 'NONE', *, *, #13551, .F. ) ;
#27322 = ADVANCED_FACE ( 'NONE', ( #66641 ), #30286, .T. ) ;
#27323 = DIRECTION ( 'NONE',  ( 0.000000000000000000, 0.2461538461537955691, -0.9692307692307821076 ) ) ;
#27324 = CARTESIAN_POINT ( 'NONE',  ( 13.50000000000000178, 0.000000000000000000, 0.000000000000000000 ) ) ;
#27325 = CARTESIAN_POINT ( 'NONE',  ( 9.700348830567069314, -3.823367932526878121, -8.850089092130223989 ) ) ;
#27326 = CARTESIAN_POINT ( 'NONE',  ( 18.48326398027718653, -2.855662837647996888, 11.29488646771354787 ) ) ;
#27327 = EDGE_CURVE ( 'NONE', #6268, #57158, #16054, .T. ) ;
#27328 = CARTESIAN_POINT ( 'NONE',  ( 17.62782920531150310, 1.879164230502278210, -12.57477362212319250 ) ) ;
#27329 = CARTESIAN_POINT ( 'NONE',  ( 8.615570209625364129, 4.906878460622427163, 6.021351945580431853 ) ) ;
#27330 = AXIS2_PLACEMENT_3D ( 'NONE', #52609, #11329, #10303 ) ;
#27331 = CARTESIAN_POINT ( 'NONE',  ( 11.71210404293059959, 3.618181340822599790, 6.722495590581700320 ) ) ;
#27332 = CARTESIAN_POINT ( 'NONE',  ( 11.62299956498149989, -2.792989229543000107, 7.174999999999999822 ) ) ;
#27333 = CARTESIAN_POINT ( 'NONE',  ( 10.41025564679000048, -4.690690303276999984, -6.142863315966000215 ) ) ;
#27334 = CARTESIAN_POINT ( 'NONE',  ( 12.08061556837357386, 2.709898641938862429, 13.73658242091902615 ) ) ;
#27335 = LINE ( 'NONE', #416, #21907 ) ;
#27336 = CARTESIAN_POINT ( 'NONE',  ( 23.95413598829442492, 9.440340059428892872, -9.313978351785300092 ) ) ;
#27337 = DIRECTION ( 'NONE',  ( 0.000000000000000000, -1.000000000000000000, 0.000000000000000000 ) ) ;
#27339 = VECTOR ( 'NONE', #6618, 1000.000000000000114 ) ;
#27338 = B_SPLINE_CURVE_WITH_KNOTS ( 'NONE', 3,
 ( #8811, #30152, #40970, #62294 ),
 .UNSPECIFIED., .F., .F.,
 ( 4, 4 ),
 ( 0.8746820087829817458, 1.000000000000000000 ),
 .UNSPECIFIED. ) ;
#27340 = EDGE_LOOP ( 'NONE', ( #29005, #42833, #52709, #67981 ) ) ;
#27341 = CARTESIAN_POINT ( 'NONE',  ( 7.387702836194001144, 2.764883607873137361, 8.723309566181695729 ) ) ;
#27342 = CARTESIAN_POINT ( 'NONE',  ( 11.02641638348499953, -4.974961480482700260, 7.737488872214999702 ) ) ;
#27343 = ORIENTED_EDGE ( 'NONE', *, *, #13506, .F. ) ;
#27344 = CARTESIAN_POINT ( 'NONE',  ( 17.77709566067065339, -3.084588255221574649, 13.53194174261899541 ) ) ;
#27345 = CARTESIAN_POINT ( 'NONE',  ( 10.25149413291699929, -2.962184842772000337, -7.026470926762800495 ) ) ;
#27346 = ORIENTED_EDGE ( 'NONE', *, *, #55359, .F. ) ;
#27347 = CARTESIAN_POINT ( 'NONE',  ( 10.51925056272499859, 5.174767082365999471, 7.482589369563879877 ) ) ;
#27348 = CARTESIAN_POINT ( 'NONE',  ( 6.714005406034039503, -0.1331244656375725477, 1.125151267359796536 ) ) ;
#27349 = DIRECTION ( 'NONE',  ( 0.8660254003319995952, -4.365146055948999335E-12, -0.5000000059797998775 ) ) ;
#27350 = CARTESIAN_POINT ( 'NONE',  ( 18.26242787221299935, -2.744348664398000182, 11.56741553474000028 ) ) ;
#27351 = CARTESIAN_POINT ( 'NONE',  ( 12.43745875772600584, -1.881346041095415478, -13.87306493546281239 ) ) ;
#27352 = CARTESIAN_POINT ( 'NONE',  ( 12.54858531451517223, 0.5700392133823489749, -13.88426419246400378 ) ) ;
#27353 = CARTESIAN_POINT ( 'NONE',  ( 9.548601287889788125, -3.999999532294070459, 6.301404677806389465 ) ) ;
#27354 = EDGE_CURVE ( 'NONE', #26163, #4537, #56922, .T. ) ;
#27355 = CARTESIAN_POINT ( 'NONE',  ( 10.74708735964999917, -5.603138702306000418, -6.963343193308999979 ) ) ;
#27356 = CARTESIAN_POINT ( 'NONE',  ( 13.51386961183700031, 11.53357255609999932, 1.992589078083000009 ) ) ;
#27357 = VERTEX_POINT ( 'NONE', #3684 ) ;
#27358 = CARTESIAN_POINT ( 'NONE',  ( 8.532195280408998883, 5.331510020787000315, -8.114341808290998159 ) ) ;
#27359 = ORIENTED_EDGE ( 'NONE', *, *, #40389, .T. ) ;
#27360 = CARTESIAN_POINT ( 'NONE',  ( 7.100000000000000533, 4.000000000000000000, -7.500000000000000000 ) ) ;
#27361 = FILL_AREA_STYLE ('',( #31925 ) ) ;
#27362 = ORIENTED_EDGE ( 'NONE', *, *, #50216, .T. ) ;
#27363 = CARTESIAN_POINT ( 'NONE',  ( 9.112942518363999156, 5.100000000000000533, 6.192000867487999827 ) ) ;
#27364 = CARTESIAN_POINT ( 'NONE',  ( 17.71888513161123413, -3.103492732303466450, -12.29025695670424945 ) ) ;
#27365 = CARTESIAN_POINT ( 'NONE',  ( 24.76117173203458677, -8.629364107770223669, 8.563007708072372992 ) ) ;
#27366 = DIRECTION ( 'NONE',  ( 0.000000000000000000, -1.000000000000000000, 0.000000000000000000 ) ) ;
#27367 = CARTESIAN_POINT ( 'NONE',  ( 9.591846873515667227, -3.000416447002275167, -8.268183399968643599 ) ) ;
#27368 = CARTESIAN_POINT ( 'NONE',  ( 17.74851076052204490, -1.905606517475760597, 12.57039381402181455 ) ) ;
#27369 = CARTESIAN_POINT ( 'NONE',  ( 23.60205915885299888, -9.377218989177011466, -8.305825996807000067 ) ) ;
#27370 = CARTESIAN_POINT ( 'NONE',  ( 12.27985112600388717, -0.3389646381316569479, 13.89444110642641661 ) ) ;
#27371 = VERTEX_POINT ( 'NONE', #46356 ) ;
#27372 = CARTESIAN_POINT ( 'NONE',  ( 7.249090560818999940, 3.037137096735000430, -6.379793420563999895 ) ) ;
#27373 = CARTESIAN_POINT ( 'NONE',  ( 17.83742117717700282, 11.80639483233000142, -3.358960109135999961 ) ) ;
#27374 = CARTESIAN_POINT ( 'NONE',  ( 10.11342028323962694, 3.127145521393861038, 7.560475846972328995 ) ) ;
#27375 = CARTESIAN_POINT ( 'NONE',  ( 4.661825709867000178, -1.451480533005000018, 0.3000752729519000073 ) ) ;
#27376 = CARTESIAN_POINT ( 'NONE',  ( 8.748814158775001459, 5.251032986819000214, -6.070151079272999795 ) ) ;
#27377 = AXIS2_PLACEMENT_3D ( 'NONE', #35120, #30549, #46973 ) ;
#27378 = CARTESIAN_POINT ( 'NONE',  ( 18.53682820967700451, -2.877067450793000081, 12.22924281482000097 ) ) ;
#27379 = CARTESIAN_POINT ( 'NONE',  ( 10.05204995789999955, -2.669899884077999719, -8.791535702747999892 ) ) ;
#27380 = ORIENTED_EDGE ( 'NONE', *, *, #61488, .T. ) ;
#27381 = CARTESIAN_POINT ( 'NONE',  ( 3.186390132544124842, -0.4581489286485234680, 3.499999999999998668 ) ) ;
#27382 = FACE_OUTER_BOUND ( 'NONE', #11028, .T. ) ;
#27383 = PLANE ( 'NONE',  #48641 ) ;
#27384 = CARTESIAN_POINT ( 'NONE',  ( 11.79999999471800010, 3.216299622513999701, -11.40340969442000052 ) ) ;
#27385 = CARTESIAN_POINT ( 'NONE',  ( 24.37846342710900061, 8.840949306909999805, -8.761878624573000707 ) ) ;
#27386 = EDGE_CURVE ( 'NONE', #51068, #12021, #205, .T. ) ;
#27387 = EDGE_CURVE ( 'NONE', #67334, #23850, #67317, .T. ) ;
#27388 = CARTESIAN_POINT ( 'NONE',  ( 11.27234208742519783, 3.445253572379500362, -8.372004648554700168 ) ) ;
#27389 = CARTESIAN_POINT ( 'NONE',  ( 10.24255864497999902, 4.790758628877400227, -8.119307134446700047 ) ) ;
#27391 = CARTESIAN_POINT ( 'NONE',  ( 8.447041273813589157, 5.099348809280254358, -6.546252130241257738 ) ) ;
#27390 = CARTESIAN_POINT ( 'NONE',  ( 9.849051052051999378, -3.149129950522900234, 7.333482423122699601 ) ) ;
#27392 = CARTESIAN_POINT ( 'NONE',  ( 9.209122513651813335, -5.100000000000000533, 6.320295141290149132 ) ) ;
#27393 = VERTEX_POINT ( 'NONE', #66979 ) ;
#27394 = CARTESIAN_POINT ( 'NONE',  ( 11.31389666366019853, 3.954123449088899900, 6.467512203247999913 ) ) ;
#27395 = CARTESIAN_POINT ( 'NONE',  ( 10.46432358320999967, -2.042767395367000027, 7.723698102088000006 ) ) ;
#27396 = CARTESIAN_POINT ( 'NONE',  ( 9.025809814041000578, 4.782507962695600412, 6.488038963273999649 ) ) ;
#27397 = DIRECTION ( 'NONE',  ( -0.7071060865236062920, 0.7071074758488062884, 8.142048014830070602E-10 ) ) ;
#27398 = CARTESIAN_POINT ( 'NONE',  ( 10.15402496696000156, -5.267980706381999667, 5.992344456606999437 ) ) ;
#27399 = DIRECTION ( 'NONE',  ( -6.259113923818999724E-11, 6.259176727233999437E-11, 1.000000000000000000 ) ) ;
#27400 = DIRECTION ( 'NONE',  ( 0.000000000000000000, 0.1807154286440006141, -0.9835354258236025382 ) ) ;
#27401 = AXIS2_PLACEMENT_3D ( 'NONE', #197, #6814, #54715 ) ;
#27402 = EDGE_CURVE ( 'NONE', #43200, #50051, #12722, .T. ) ;
#27403 = CARTESIAN_POINT ( 'NONE',  ( 9.482684229509999341, -4.708027397558999461, -6.787581931282099745 ) ) ;
#27404 = CARTESIAN_POINT ( 'NONE',  ( 5.303344406977999803, -1.078708783361999934, 0.4686457328678000356 ) ) ;
#27405 = B_SPLINE_SURFACE_WITH_KNOTS ( 'NONE', 3, 3, ( 
 ( #35534, #56854, #8951, #25031, #30292, #30975, #36553, #51595, #46016, #46363, #16510, #436, #32269, #19789, #24693, #58818, #21750, #30626, #62431, #4033, #3692, #19441, #35869, #25372, #14207, #46709, #14887, #59160, #51937, #10925, #41459, #68013, #20130, #43084, #64389 ),
 ( #37839, #62766, #52287, #20470, #36208, #57525, #11264, #4381, #25716, #32601, #47050, #67323, #40765, #62087, #33643, #6359, #60896, #39225, #43441, #13012, #43783, #11602, #32945, #48677, #18250, #27705, #17559, #66131, #54959, #44828, #16852, #38175, #59504, #49022, #54257 ),
 ( #28750, #60550, #12657, #7061, #1128, #55307, #17907, #49358, #65079, #39572, #27355, #22096, #22442, #23489, #1820, #34340, #38529, #28397, #782, #17199, #28049, #59851, #11958, #65783, #7404, #49713, #6015, #64737, #6709, #23140, #44490, #33295, #60207, #33988, #44137 ),
 ( #54611, #50065, #1472, #2173, #22789, #65436, #38885, #12310, #45851, #56690, #14387, #8789, #46195, #50754, #3199, #35029, #62600, #67160, #29098, #45170, #67506, #40263, #39926, #50408, #61244, #61583, #51774, #24867, #57024, #2508, #9124, #29447, #35707, #19272, #30463 ) ),
 .UNSPECIFIED., .F., .F., .F.,
 ( 4, 4 ),
 ( 4, 1, 1, 1, 1, 1, 1, 1, 1, 1, 1, 1, 1, 1, 1, 1, 1, 1, 1, 1, 1, 1, 1, 1, 1, 1, 1, 1, 1, 1, 1, 1, 4 ),
 ( -0.1039086239011999951, 1.103908623900999864 ),
 ( 0.1942321073450000157, 0.2199060843169000079, 0.2455800612886999967, 0.2712540382605999612, 0.2969280152323999777, 0.3226019922043000254, 0.3482759691761000420, 0.3739499461479999787, 0.3996239231197999953, 0.4252979000916999874, 0.4509718770635000040, 0.4766458540353999962, 0.5023198310072000128, 0.5279938079791000050, 0.5536677849509000771, 0.5793417619227999582, 0.6050157388945999193, 0.6306897158665000225, 0.6563636928382999836, 0.6820376698101999757, 0.7077116467820000478, 0.7333856237539000400, 0.7590596007256998901, 0.7847335776975999933, 0.8104075546693999543, 0.8360815316413000575, 0.8617555086131000186, 0.8874294855850000108, 0.9131034625568000829, 0.9387774395286999640, 0.9644514165004999251, 0.9901253934722999972, 1.015799370444000038 ),
 .UNSPECIFIED. ) ;
#27406 = EDGE_CURVE ( 'NONE', #51112, #5748, #61737, .T. ) ;
#27407 = CARTESIAN_POINT ( 'NONE',  ( 11.27222057153667656, -3.695719232113590547, 6.680547245655227506 ) ) ;
#27408 = CARTESIAN_POINT ( 'NONE',  ( 12.17440657078182475, 2.124933824806637173, -12.41953149444585947 ) ) ;
#27409 = CARTESIAN_POINT ( 'NONE',  ( 24.30857393632600250, -3.216436940933999900, 12.15172254432999921 ) ) ;
#27410 = CARTESIAN_POINT ( 'NONE',  ( 12.31056516821460001, -3.390321848206700128, 6.884701936848800052 ) ) ;
#27411 = CARTESIAN_POINT ( 'NONE',  ( 11.53979707368350027, 3.569730287184500472, -6.748224392138099326 ) ) ;
#27412 = DIRECTION ( 'NONE',  ( -1.000000000000000000, 0.000000000000000000, 0.000000000000000000 ) ) ;
#27413 = CARTESIAN_POINT ( 'NONE',  ( 25.59037455770100422, -8.351027012765998236, 7.983767442140998760 ) ) ;
#27414 = CARTESIAN_POINT ( 'NONE',  ( 5.667284894747531609, 12.98956018755431785, 2.203076747946188352 ) ) ;
#27415 = EDGE_LOOP ( 'NONE', ( #66800, #4500, #16157 ) ) ;
#27416 = CARTESIAN_POINT ( 'NONE',  ( 25.59994555223599733, 10.55174472786000095, -3.754934689065000164 ) ) ;
#27417 = CONTEXT_DEPENDENT_SHAPE_REPRESENTATION ( #2962, #37767 ) ;
#27418 = CARTESIAN_POINT ( 'NONE',  ( 11.23078751119019891, -4.915752892793999962, -7.979095341142500075 ) ) ;
#27419 = CARTESIAN_POINT ( 'NONE',  ( 24.37808884344924465, -3.385972260544573231, 12.24452378150168563 ) ) ;
#27420 = CARTESIAN_POINT ( 'NONE',  ( 10.41684687351637528, -4.768183399968644487, 6.500416447002274722 ) ) ;
#27421 = DIRECTION ( 'NONE',  ( 1.000000000000000000, 0.000000000000000000, 0.000000000000000000 ) ) ;
#27422 = CARTESIAN_POINT ( 'NONE',  ( 11.19434208742519843, 3.521141233577200325, -8.252717006421999457 ) ) ;
#27423 = VERTEX_POINT ( 'NONE', #50911 ) ;
#27424 = CONICAL_SURFACE ( 'NONE', #60965, 1.725000594299999968, 0.7853984795078434722 ) ;
#27425 = CARTESIAN_POINT ( 'NONE',  ( 10.52324012719000024, -3.325647021086999722, 5.689999163383999026 ) ) ;
#27426 = CARTESIAN_POINT ( 'NONE',  ( 17.96876343269822129, 2.968584057511098884, -13.56283743052908619 ) ) ;
#27427 = ORIENTED_EDGE ( 'NONE', *, *, #35668, .T. ) ;
#27428 = CARTESIAN_POINT ( 'NONE',  ( 13.00000000001300116, 11.52577654661000039, 1.696746661728000038 ) ) ;
#27429 = CARTESIAN_POINT ( 'NONE',  ( 8.096558059622999792, -5.061720701958000390, 5.824087910811999613 ) ) ;
#27430 = AXIS2_PLACEMENT_3D ( 'NONE', #52840, #4935, #9840 ) ;
#27431 = CARTESIAN_POINT ( 'NONE',  ( 15.37447410014400084, 8.836271409840000146, 7.950749727554001112 ) ) ;
#27432 = ORIENTED_EDGE ( 'NONE', *, *, #4718, .T. ) ;
#27433 = CARTESIAN_POINT ( 'NONE',  ( 13.99999999347100044, -9.187456302440001110, -8.213201953411001455 ) ) ;
#27434 = B_SPLINE_CURVE_WITH_KNOTS ( 'NONE', 3,
 ( #40870, #62194, #14314, #69155, #59016 ),
 .UNSPECIFIED., .F., .F.,
 ( 4, 1, 4 ),
 ( 0.000000000000000000, 0.5000000000000000000, 1.000000000000000000 ),
 .UNSPECIFIED. ) ;
#27435 = CARTESIAN_POINT ( 'NONE',  ( 8.359535841228000308, 5.897697057214000615, -7.408103789850999377 ) ) ;
#27436 = CARTESIAN_POINT ( 'NONE',  ( 10.11476354018233081, -2.782534154164604256, -7.172815144550903632 ) ) ;
#27437 = CARTESIAN_POINT ( 'NONE',  ( 9.511909210317325503, 4.618071422035288087, 8.703327943634770136 ) ) ;
#27438 = ORIENTED_EDGE ( 'NONE', *, *, #9160, .F. ) ;
#27439 = CARTESIAN_POINT ( 'NONE',  ( 10.44080359545000114, -5.435731278187999393, 7.303630150377999009 ) ) ;
#27440 = CARTESIAN_POINT ( 'NONE',  ( 11.60000000000000497, 3.359735910920771396, 8.191831084107850103 ) ) ;
#27441 = DIRECTION ( 'NONE',  ( -0.9709491189738370664, 0.000000000000000000, -0.2392860387986094628 ) ) ;
#27442 = EDGE_LOOP ( 'NONE', ( #55862, #17391, #62860 ) ) ;
#27443 = CARTESIAN_POINT ( 'NONE',  ( 11.29997960521318312, -3.569935952926194478, 11.29784959202356021 ) ) ;
#27444 = CARTESIAN_POINT ( 'NONE',  ( 11.50029455687000102, 11.62161504194025063, 0.9384843090728728354 ) ) ;
#27445 = ORIENTED_EDGE ( 'NONE', *, *, #28685, .F. ) ;
#27446 = CARTESIAN_POINT ( 'NONE',  ( 9.685317406968998455, 4.186809223719299311, 6.513113677132300161 ) ) ;
#27447 = CARTESIAN_POINT ( 'NONE',  ( 18.02961597915983205, 0.4069473558587370920, -13.89198745890301723 ) ) ;
#27448 = CARTESIAN_POINT ( 'NONE',  ( 5.310278024686999387, -0.4934046401541999360, 1.147847133074999748 ) ) ;
#27449 = DIRECTION ( 'NONE',  ( 1.000000000000000000, -6.763579949425000297E-11, 5.896569782073000140E-12 ) ) ;
#27450 = EDGE_CURVE ( 'NONE', #13866, #47471, #30904, .T. ) ;
#27451 = CARTESIAN_POINT ( 'NONE',  ( 24.76774735605714284, 11.72413114164001513, -3.191091186273769864 ) ) ;
#27452 = CARTESIAN_POINT ( 'NONE',  ( 6.950034089120999958, 13.87069231928999891, -4.225386915259999654 ) ) ;
#27453 = CARTESIAN_POINT ( 'NONE',  ( 9.327002446946540459, -3.954584633155211915, 9.239083166430416938 ) ) ;
#27454 = ORIENTED_EDGE ( 'NONE', *, *, #42441, .F. ) ;
#27455 = CARTESIAN_POINT ( 'NONE',  ( 5.700000000000000178, 1.250000000000000000, 0.000000000000000000 ) ) ;
#27456 = CARTESIAN_POINT ( 'NONE',  ( 10.00190165877000048, 2.729646201450000031, -8.843033333815998986 ) ) ;
#27457 = CARTESIAN_POINT ( 'NONE',  ( 25.59997036749100374, 2.856417224717999748, 11.13959153667999935 ) ) ;
#27458 = CARTESIAN_POINT ( 'NONE',  ( 12.68500746440619764, 1.797494983113959277, -13.88412888179957605 ) ) ;
#27459 = DIRECTION ( 'NONE',  ( -1.000000000000000000, -9.912705577010336396E-15, -5.699805706780943546E-14 ) ) ;
#27460 = B_SPLINE_CURVE_WITH_KNOTS ( 'NONE', 3,
 ( #63262, #59661, #62919, #64888 ),
 .UNSPECIFIED., .F., .F.,
 ( 4, 4 ),
 ( 0.8163836489557126930, 1.000000000000000000 ),
 .UNSPECIFIED. ) ;
#27461 = CARTESIAN_POINT ( 'NONE',  ( 10.65050275296000137, -5.200029647236999786, 5.937716681140000397 ) ) ;
#27462 = CARTESIAN_POINT ( 'NONE',  ( 18.02561562912593018, -0.4118363585311525799, 13.89180007025485786 ) ) ;
#27463 = CARTESIAN_POINT ( 'NONE',  ( 25.26979641699100299, -2.550139818953999882, 11.36439134171999932 ) ) ;
#27464 = ORIENTED_EDGE ( 'NONE', *, *, #17345, .F. ) ;
#27465 = VERTEX_POINT ( 'NONE', #13179 ) ;
#27466 = CARTESIAN_POINT ( 'NONE',  ( 12.49507620378167871, -0.5430989695073406009, 13.88572189919897326 ) ) ;
#27467 = CARTESIAN_POINT ( 'NONE',  ( 12.38194801265181333, -0.4608083867824254720, -13.88973595540270800 ) ) ;
#27468 = CARTESIAN_POINT ( 'NONE',  ( 9.882266086202999844, -4.932716797830999589, 6.390980246320999925 ) ) ;
#27469 = CARTESIAN_POINT ( 'NONE',  ( 18.04535492079093828, -0.3877560771919992266, -13.89272419024339733 ) ) ;
#27470 = EDGE_CURVE ( 'NONE', #22975, #28283, #14463, .T. ) ;
#27471 = EDGE_CURVE ( 'NONE', #3420, #37989, #63601, .T. ) ;
#27472 = CARTESIAN_POINT ( 'NONE',  ( 7.667605646792000407, -5.638700495537999124, 8.266402903491000487 ) ) ;
#27473 = DIRECTION ( 'NONE',  ( 0.000000000000000000, 0.000000000000000000, -1.000000000000000000 ) ) ;
#27475 = CARTESIAN_POINT ( 'NONE',  ( 17.66658663920548733, 11.23412379135927530, -3.084957477888136790 ) ) ;
#27474 = CARTESIAN_POINT ( 'NONE',  ( 11.04555864497999984, -2.992894514506000192, 6.711254117843599154 ) ) ;
#27476 = CARTESIAN_POINT ( 'NONE',  ( 10.93656785386839836, 2.939720539848000413, -8.213529149347399638 ) ) ;
#27477 = AXIS2_PLACEMENT_3D ( 'NONE', #40524, #62866, #56951 ) ;
#27478 = EDGE_CURVE ( 'NONE', #22723, #62822, #25221, .T. ) ;
#27479 = CARTESIAN_POINT ( 'NONE',  ( 24.50399615158200106, -8.846403136021999458, -9.151488484734001005 ) ) ;
#27480 = CARTESIAN_POINT ( 'NONE',  ( 23.66004879239100234, 9.998910715289998308, -9.691527791130999603 ) ) ;
#27481 = CARTESIAN_POINT ( 'NONE',  ( 18.04446571359450147, -0.3888461597108445189, 12.69199065798140680 ) ) ;
#27482 = DIRECTION ( 'NONE',  ( -1.000000000000000000, 0.000000000000000000, 0.000000000000000000 ) ) ;
#27483 = CARTESIAN_POINT ( 'NONE',  ( 18.22497476945055439, -3.457026130723240609, 12.03849088744245499 ) ) ;
#27484 = VERTEX_POINT ( 'NONE', #63793 ) ;
#27485 = CARTESIAN_POINT ( 'NONE',  ( 11.09461754388281740, -3.670987266758758416, -9.018203014671000162 ) ) ;
#27486 = CARTESIAN_POINT ( 'NONE',  ( 8.641808059624999316, -2.933824946949000090, 8.496487880080000110 ) ) ;
#27487 = B_SPLINE_CURVE_WITH_KNOTS ( 'NONE', 3,
 ( #61600, #45533, #62288, #41310 ),
 .UNSPECIFIED., .F., .F.,
 ( 4, 4 ),
 ( 0.000000000000000000, 1.000000000000000000 ),
 .UNSPECIFIED. ) ;
#27488 = DIRECTION ( 'NONE',  ( 0.000000000000000000, 0.9421243786071880066, -0.3352635608502960163 ) ) ;
#27489 = LINE ( 'NONE', #64185, #26718 ) ;
#27490 = CARTESIAN_POINT ( 'NONE',  ( 9.660601868375998436, -2.901236202253999696, -6.151180522693000086 ) ) ;
#27491 = EDGE_CURVE ( 'NONE', #29320, #3964, #57516, .T. ) ;
#27492 = CARTESIAN_POINT ( 'NONE',  ( 11.23589666366019912, 3.960399224793059947, 6.608753462694600067 ) ) ;
#27493 = CARTESIAN_POINT ( 'NONE',  ( 11.03092334123000029, 5.020455242919999783, -6.601201971309999195 ) ) ;
#27494 = ORIENTED_EDGE ( 'NONE', *, *, #62179, .T. ) ;
#27495 = CARTESIAN_POINT ( 'NONE',  ( 12.35444711458464973, -0.5635217852607019573, -12.58739276154098086 ) ) ;
#27496 = CARTESIAN_POINT ( 'NONE',  ( 6.949466529116000046, 12.16404197558000000, -3.090625629547000042 ) ) ;
#27497 = CARTESIAN_POINT ( 'NONE',  ( 17.84599613952810415, 3.139413506986218128, -12.20262697555083342 ) ) ;
#27498 = CARTESIAN_POINT ( 'NONE',  ( 5.619729929256978451, 12.11456185543956288, 3.745214083257081938 ) ) ;
#27499 = CARTESIAN_POINT ( 'NONE',  ( 7.037114158771000660, 4.623631324973000112, 8.651459902566999816 ) ) ;
#27500 = ORIENTED_EDGE ( 'NONE', *, *, #20689, .T. ) ;
#27501 = CARTESIAN_POINT ( 'NONE',  ( 6.082901922763999991, -1.553728905769999891, -0.4396155223175000071 ) ) ;
#27502 = CARTESIAN_POINT ( 'NONE',  ( 8.195595280407001582, 2.759821810153000321, -8.454514188070000102 ) ) ;
#27503 = CARTESIAN_POINT ( 'NONE',  ( 8.386090224810864413, -2.789003059333644341, 8.749111205124165735 ) ) ;
#27504 = CARTESIAN_POINT ( 'NONE',  ( 13.73125687462010447, 9.567603210582007023, 8.083310008147687853 ) ) ;
#27505 = ORIENTED_EDGE ( 'NONE', *, *, #68605, .F. ) ;
#27506 = CARTESIAN_POINT ( 'NONE',  ( 17.60000000000000142, -11.23412379136000006, 3.084957477885999833 ) ) ;
#27507 = B_SPLINE_CURVE_WITH_KNOTS ( 'NONE', 3,
 ( #28052, #11961, #55659, #22793, #39928, #54616, #34687, #2175, #50758, #39574, #29449, #44141, #65439, #17562, #60209, #38888, #66135, #7758, #33645 ),
 .UNSPECIFIED., .F., .F.,
 ( 4, 2, 2, 1, 2, 2, 2, 2, 2, 4 ),
 ( 0.000000000000000000, 0.1250000000000042188, 0.1875000000000060507, 0.2187500000000067168, 0.2343750000000068556, 0.2500000000000069944, 0.3750000000000019984, 0.4375000000000018874, 0.5000000000000017764, 1.000000000000000000 ),
 .UNSPECIFIED. ) ;
#27508 = CARTESIAN_POINT ( 'NONE',  ( 6.157109839683333696, -1.199500263597270022, -0.9218200799623730290 ) ) ;
#27509 = ORIENTED_EDGE ( 'NONE', *, *, #65013, .F. ) ;
#27510 = CARTESIAN_POINT ( 'NONE',  ( 24.71768487731727859, 3.123575521103121755, -11.79178543996698991 ) ) ;
#27511 = CARTESIAN_POINT ( 'NONE',  ( 16.32975648157900039, 3.316681689484000106, 11.22330675696999869 ) ) ;
#27512 = VECTOR ( 'NONE', #15983, 1000.000000000000000 ) ;
#27513 = CARTESIAN_POINT ( 'NONE',  ( 17.57900095810616392, 0.7302151993337242519, -13.98094363222392111 ) ) ;
#27514 = ORIENTED_EDGE ( 'NONE', *, *, #42100, .F. ) ;
#27515 = DIRECTION ( 'NONE',  ( 1.000000000000000000, 0.000000000000000000, 0.000000000000000000 ) ) ;
#27516 = CARTESIAN_POINT ( 'NONE',  ( 9.857734298427807573, -2.650109589709913838, -7.624707963951017575 ) ) ;
#27517 = CARTESIAN_POINT ( 'NONE',  ( 10.35814141025499957, 4.483492689244800822, -8.361148840840000318 ) ) ;
#27518 = CARTESIAN_POINT ( 'NONE',  ( 18.49985170088394426, -7.837663500889314729E-14, -12.52499999999998792 ) ) ;
#27519 = CARTESIAN_POINT ( 'NONE',  ( 16.09997386696500143, -8.350085070477001992, -8.123950967096998710 ) ) ;
#27520 = ORIENTED_EDGE ( 'NONE', *, *, #59755, .F. ) ;
#27521 = CARTESIAN_POINT ( 'NONE',  ( 7.127704719590999716, 4.698356649019999942, 8.789431186081998248 ) ) ;
#27522 = CARTESIAN_POINT ( 'NONE',  ( 17.60314900679416183, -1.789028854058319684, 13.88522169503354142 ) ) ;
#27523 = ORIENTED_EDGE ( 'NONE', *, *, #8467, .F. ) ;
#27524 = FILL_AREA_STYLE ('',( #54086 ) ) ;
#27525 = AXIS2_PLACEMENT_3D ( 'NONE', #54746, #12098, #56122 ) ;
#27526 = CARTESIAN_POINT ( 'NONE',  ( 16.04495723965300158, -8.927588545536998765, -8.707532029612000457 ) ) ;
#27527 = CARTESIAN_POINT ( 'NONE',  ( 11.02029022880999953, 6.435658501792000052, -5.283992956780000583 ) ) ;
#27528 = ORIENTED_EDGE ( 'NONE', *, *, #17294, .F. ) ;
#27529 = CARTESIAN_POINT ( 'NONE',  ( 12.48926758269845827, -1.960545016317334355, -12.56101064709213766 ) ) ;
#27530 = CARTESIAN_POINT ( 'NONE',  ( 0.4398691794437870617, -0.9011714948220468369, -3.349986680846007037 ) ) ;
#27531 = DIRECTION ( 'NONE',  ( 0.000000000000000000, 1.000000000000000000, 0.000000000000000000 ) ) ;
#27532 = ADVANCED_FACE ( 'NONE', ( #37569 ), #10317, .T. ) ;
#27533 = DIRECTION ( 'NONE',  ( 1.000000000000000000, 0.000000000000000000, 0.000000000000000000 ) ) ;
#27534 = CARTESIAN_POINT ( 'NONE',  ( 12.10694218860116855, -2.320713384140930202, -13.80631828123456728 ) ) ;
#27535 = EDGE_CURVE ( 'NONE', #31977, #9447, #68344, .T. ) ;
#27536 = CARTESIAN_POINT ( 'NONE',  ( 11.43302763632549990, -5.035790660926999784, -7.022058766158599141 ) ) ;
#27537 = CARTESIAN_POINT ( 'NONE',  ( 10.35987047770899672, 2.749999999999999556, 7.249610810850630749 ) ) ;
#27538 = CARTESIAN_POINT ( 'NONE',  ( 17.74290558058745049, -3.096122732672591749, 12.29249473893052524 ) ) ;
#27539 = ORIENTED_EDGE ( 'NONE', *, *, #26750, .F. ) ;
#27540 = CARTESIAN_POINT ( 'NONE',  ( 9.469356963619999235, -5.119357025014000584, 7.500000000085178087 ) ) ;
#27541 = VERTEX_POINT ( 'NONE', #53318 ) ;
#27542 = CARTESIAN_POINT ( 'NONE',  ( 13.00000000009400303, 11.69118001589999878, 1.923222888683999932 ) ) ;
#27543 = CARTESIAN_POINT ( 'NONE',  ( 9.842764158772000727, 5.798263352390999437, -8.113145944980999502 ) ) ;
#27544 = CARTESIAN_POINT ( 'NONE',  ( 10.39355883036999906, 4.089958667033000594, -9.188186800857998549 ) ) ;
#27545 = CARTESIAN_POINT ( 'NONE',  ( 11.06133683778999988, -2.503914237677999921, -6.712780725818999983 ) ) ;
#27546 = CARTESIAN_POINT ( 'NONE',  ( 24.32154984244752072, -12.72720806567605578, -3.095248367017349178 ) ) ;
#27547 = CARTESIAN_POINT ( 'NONE',  ( 24.42277064782400231, 12.73424796067999942, 3.019164715476000183 ) ) ;
#27548 = CARTESIAN_POINT ( 'NONE',  ( 10.25461802485000007, 2.860644035673999941, 6.604613005744999654 ) ) ;
#27549 = ORIENTED_EDGE ( 'NONE', *, *, #66932, .F. ) ;
#27550 = LINE ( 'NONE', #17047, #16824 ) ;
#27551 = CARTESIAN_POINT ( 'NONE',  ( 11.14698693981000055, 5.129806801114000336, 5.886034047559999927 ) ) ;
#27552 = CARTESIAN_POINT ( 'NONE',  ( 10.42819717210663555, 5.125396288445606352, 6.749639981115941545 ) ) ;
#27553 = CARTESIAN_POINT ( 'NONE',  ( 11.85545123989520100, -3.524778630617700248, 6.582230774881299595 ) ) ;
#27554 = LINE ( 'NONE', #26875, #10484 ) ;
#27555 = CARTESIAN_POINT ( 'NONE',  ( 11.85979573085659844, 4.840012015667699785, -7.645349278262099979 ) ) ;
#27556 = CIRCLE ( 'NONE', #15278, 2.199999999999999734 ) ;
#27557 = EDGE_CURVE ( 'NONE', #56639, #9679, #4374, .T. ) ;
#27558 = CARTESIAN_POINT ( 'NONE',  ( 10.48845679253054897, 2.446973213462996455, 6.696139198371997558 ) ) ;
#27559 = AXIS2_PLACEMENT_3D ( 'NONE', #18246, #6704, #7752 ) ;
#27560 = CARTESIAN_POINT ( 'NONE',  ( 23.68331123634199997, -9.987482016315999189, -9.401264431477001082 ) ) ;
#27561 = CARTESIAN_POINT ( 'NONE',  ( 11.33810207955129812, -3.203462856645999945, -7.825000000000000178 ) ) ;
#27562 = DIRECTION ( 'NONE',  ( 0.000000000000000000, 0.000000000000000000, 1.000000000000000000 ) ) ;
#27563 = AXIS2_PLACEMENT_3D ( 'NONE', #28644, #18491, #66022 ) ;
#27564 = ORIENTED_EDGE ( 'NONE', *, *, #58433, .T. ) ;
#27565 = LINE ( 'NONE', #26883, #21969 ) ;
#27566 = CARTESIAN_POINT ( 'NONE',  ( 7.293740924889999810, 0.6280046043689999635, 1.216231657070000027 ) ) ;
#27567 = CARTESIAN_POINT ( 'NONE',  ( 18.08101717074206150, 2.837770499550323233, 13.59594328884928593 ) ) ;
#27568 = CARTESIAN_POINT ( 'NONE',  ( 24.66271477989500127, 8.757902662406001681, -9.242626227026999430 ) ) ;
#27569 = CARTESIAN_POINT ( 'NONE',  ( 11.40425819896749893, -5.255890247626999745, -7.736761623643599428 ) ) ;
#27570 = EDGE_LOOP ( 'NONE', ( #21288, #2722, #13123, #15631 ) ) ;
#27571 = AXIS2_PLACEMENT_3D ( 'NONE', #20775, #9939, #10973 ) ;
#27572 = CARTESIAN_POINT ( 'NONE',  ( 24.46225899603300036, 3.149515489371000232, -11.96334157380999841 ) ) ;
#27573 = CARTESIAN_POINT ( 'NONE',  ( 9.341490007895000502, 4.148133901461999784, 9.337478696773001019 ) ) ;
#27574 = EDGE_CURVE ( 'NONE', #6237, #31811, #16246, .T. ) ;
#27576 = CARTESIAN_POINT ( 'NONE',  ( 25.59997821859199973, 2.856411258734000036, -11.13959759756999901 ) ) ;
#27575 = CARTESIAN_POINT ( 'NONE',  ( 9.310554719594000161, 3.934138271021000222, -9.063586117809000697 ) ) ;
#27577 = CARTESIAN_POINT ( 'NONE',  ( 10.93769855012999948, 2.936883479403999964, 4.920828759365000415 ) ) ;
#27578 = ORIENTED_EDGE ( 'NONE', *, *, #54038, .T. ) ;
#27579 = CARTESIAN_POINT ( 'NONE',  ( 10.62793268324000096, 3.100586971929999880, 8.599896650316999569 ) ) ;
#27580 = AXIS2_PLACEMENT_3D ( 'NONE', #26996, #48312, #418 ) ;
#27581 = CARTESIAN_POINT ( 'NONE',  ( 17.74496479089906487, -1.812889415971018048, -13.88212816151363782 ) ) ;
#27582 = CARTESIAN_POINT ( 'NONE',  ( 10.74795391537419853, 4.830118059977199785, 6.936213817702099327 ) ) ;
#27583 = CARTESIAN_POINT ( 'NONE',  ( 9.792562654643999664, -3.463427761954999795, 6.184385360914999907 ) ) ;
#27584 = CARTESIAN_POINT ( 'NONE',  ( 8.266390833065004884, 2.877128322603998534, 6.332041950470006064 ) ) ;
#27585 = EDGE_LOOP ( 'NONE', ( #34425, #41386, #22446, #47920 ) ) ;
#27586 = CARTESIAN_POINT ( 'NONE',  ( 11.09999999999999964, 5.299999999999999822, 5.160242730440000258 ) ) ;
#27588 = CARTESIAN_POINT ( 'NONE',  ( 10.43325685320999874, -5.596199512734999715, -8.042023143828998855 ) ) ;
#27587 = CARTESIAN_POINT ( 'NONE',  ( 12.49732881085200020, -12.03818693049999844, 3.242368311117000079 ) ) ;
#27589 = CARTESIAN_POINT ( 'NONE',  ( 7.754496970723887550, -5.337279552285365547, 8.612131160001228025 ) ) ;
#27590 = CARTESIAN_POINT ( 'NONE',  ( 17.55505043854147118, -1.875000000000000000, -13.78627172894481667 ) ) ;
#27591 = DIRECTION ( 'NONE',  ( 1.000000000000000000, 0.000000000000000000, 0.000000000000000000 ) ) ;
#27592 = ORIENTED_EDGE ( 'NONE', *, *, #53924, .F. ) ;
#27593 = CARTESIAN_POINT ( 'NONE',  ( 5.855026506350000659, 1.500000000000000000, 0.000000000000000000 ) ) ;
#27594 = CARTESIAN_POINT ( 'NONE',  ( 12.03148876160955005, -4.790673964186999534, 6.677731919207799294 ) ) ;
#27595 = CARTESIAN_POINT ( 'NONE',  ( 17.60412247570698341, 3.248108758003381613, 13.61799506159946382 ) ) ;
#27596 = CARTESIAN_POINT ( 'NONE',  ( 11.05964426047339799, 4.687693494822500639, 6.422784126663999338 ) ) ;
#27597 = ORIENTED_EDGE ( 'NONE', *, *, #4078, .F. ) ;
#27598 = CARTESIAN_POINT ( 'NONE',  ( 9.061929719594999710, 4.092867382745001059, -5.937785237406000505 ) ) ;
#27599 = CARTESIAN_POINT ( 'NONE',  ( 12.68481529409925379, 3.190188709592562066, -12.18945115681612101 ) ) ;
#27600 = CARTESIAN_POINT ( 'NONE',  ( 11.67901463001530082, -3.302889347096799710, 8.616511311517999872 ) ) ;
#27601 = ORIENTED_EDGE ( 'NONE', *, *, #60188, .F. ) ;
#27602 = B_SPLINE_CURVE_WITH_KNOTS ( 'NONE', 3,
 ( #40027, #61339, #14136, #45611, #62363, #46293 ),
 .UNSPECIFIED., .F., .F.,
 ( 4, 1, 1, 4 ),
 ( 0.000000000000000000, 0.1550125199349672578, 0.7488612387844387763, 1.000000000000000000 ),
 .UNSPECIFIED. ) ;
#27603 = CARTESIAN_POINT ( 'NONE',  ( 8.002383708823000319, 5.117451078405999887, -6.702236199791999915 ) ) ;
#27604 = VECTOR ( 'NONE', #16453, 1000.000000000000114 ) ;
#27605 = CYLINDRICAL_SURFACE ( 'NONE', #14883, 1.350000000000000089 ) ;
#27606 = EDGE_LOOP ( 'NONE', ( #22482, #54203, #39732, #10794 ) ) ;
#27607 = CARTESIAN_POINT ( 'NONE',  ( 9.266941940380000631, -3.049610585291000042, 6.392533570808999421 ) ) ;
#27608 = LINE ( 'NONE', #59075, #6714 ) ;
#27609 = ORIENTED_EDGE ( 'NONE', *, *, #68170, .T. ) ;
#27610 = CARTESIAN_POINT ( 'NONE',  ( 10.02887352605975124, -2.739120126747620620, -8.716523496102675850 ) ) ;
#27611 = CARTESIAN_POINT ( 'NONE',  ( 11.63410404293056999, 3.557672215630899970, 6.599279737936000423 ) ) ;
#27612 = CARTESIAN_POINT ( 'NONE',  ( 9.882259685352000389, 4.932708901218999742, 6.390989635557000170 ) ) ;
#27613 = CARTESIAN_POINT ( 'NONE',  ( 10.99480479316000014, 3.850613903518000036, -9.347963496621000345 ) ) ;
#27614 = CARTESIAN_POINT ( 'NONE',  ( 7.712330476186004979, 4.866816057961001363, 6.392636141994996635 ) ) ;
#27615 = EDGE_CURVE ( 'NONE', #12730, #8953, #9674, .T. ) ;
#27616 = DIRECTION ( 'NONE',  ( 1.000000000000000000, 0.000000000000000000, 0.000000000000000000 ) ) ;
#27617 = CARTESIAN_POINT ( 'NONE',  ( 13.46268444654400298, 9.428250749343998649, 7.876929641374000646 ) ) ;
#27618 = ADVANCED_FACE ( 'NONE', ( #25709 ), #20462, .F. ) ;
#27619 = CARTESIAN_POINT ( 'NONE',  ( 18.12461185120978868, -0.2575478136180262556, -12.69649014468030757 ) ) ;
#27620 = VECTOR ( 'NONE', #63818, 1000.000000000000114 ) ;
#27621 = CARTESIAN_POINT ( 'NONE',  ( 8.571413182547999554, 4.599999999999999645, 5.927302706106000407 ) ) ;
#27622 = CARTESIAN_POINT ( 'NONE',  ( 10.52226222744799955, -4.880489021643899861, -8.225278704382400718 ) ) ;
#27623 = EDGE_CURVE ( 'NONE', #18837, #9447, #25365, .T. ) ;
#27624 = EDGE_CURVE ( 'NONE', #26174, #10742, #7771, .T. ) ;
#27626 = CARTESIAN_POINT ( 'NONE',  ( 8.496698341230001006, 5.198556077301000222, 8.332552905512999430 ) ) ;
#27625 = B_SPLINE_CURVE_WITH_KNOTS ( 'NONE', 3,
 ( #25969, #10570, #68953, #46952, #63704, #9531, #47981, #37482, #53566, #52533, #52188, #16159, #47643, #21066 ),
 .UNSPECIFIED., .F., .F.,
 ( 4, 2, 2, 2, 2, 2, 4 ),
 ( 0.000000000000000000, 0.1249999999999996392, 0.2499999999999992784, 0.5000000000000024425, 0.6250000000000019984, 0.7500000000000014433, 1.000000000000000000 ),
 .UNSPECIFIED. ) ;
#27627 = ORIENTED_EDGE ( 'NONE', *, *, #12013, .T. ) ;
#27628 = VECTOR ( 'NONE', #23706, 1000.000000000000000 ) ;
#27629 = SURFACE_STYLE_FILL_AREA ( #42338 ) ;
#27630 = LINE ( 'NONE', #33218, #60408 ) ;
#27631 = CARTESIAN_POINT ( 'NONE',  ( 7.116206910042869538, 3.734875113800864455, 8.831328650134384617 ) ) ;
#27632 = CARTESIAN_POINT ( 'NONE',  ( 10.90000000000000036, -0.2999999999999999889, 4.902439024389999567 ) ) ;
#27633 = CARTESIAN_POINT ( 'NONE',  ( 18.21592075161430557, 2.776565552903136336, 12.29027267990593764 ) ) ;
#27634 = CARTESIAN_POINT ( 'NONE',  ( 12.80505043854143388, 1.787797342887043062, 13.88538010501570952 ) ) ;
#27635 = CARTESIAN_POINT ( 'NONE',  ( 10.85467514323000060, 9.827446706043000191, 5.589517099280000068 ) ) ;
#27636 = CIRCLE ( 'NONE', #29899, 1.250000000000000444 ) ;
#27637 = CARTESIAN_POINT ( 'NONE',  ( 9.954862456499625978, -3.587552194319129750, 8.271634030165902374 ) ) ;
#27638 = DIRECTION ( 'NONE',  ( 0.000000000000000000, 0.2461538461537955691, -0.9692307692307821076 ) ) ;
#27639 = ORIENTED_EDGE ( 'NONE', *, *, #31710, .T. ) ;
#27640 = CARTESIAN_POINT ( 'NONE',  ( 12.08853825830071038, -2.367028970089855466, 12.37569070051500653 ) ) ;
#27641 = CARTESIAN_POINT ( 'NONE',  ( 9.454392757686999715, -3.229293331742300044, -8.342464052342599246 ) ) ;
#27642 = CYLINDRICAL_SURFACE ( 'NONE', #24790, 1.350000000000000089 ) ;
#27643 = EDGE_CURVE ( 'NONE', #7930, #22245, #35354, .T. ) ;
#27644 = DIRECTION ( 'NONE',  ( 1.000000000000000000, 0.000000000000000000, 0.000000000000000000 ) ) ;
#27645 = CARTESIAN_POINT ( 'NONE',  ( 10.84641504065830020, 4.804462279649600376, -6.900173947321999179 ) ) ;
#27646 = CARTESIAN_POINT ( 'NONE',  ( 12.13047558099396284, -0.2638285456865435696, 12.59724228039519645 ) ) ;
#27647 = B_SPLINE_CURVE_WITH_KNOTS ( 'NONE', 3,
 ( #13991, #23782, #2800, #28698, #51044, #61874, #39522, #55259, #12961, #45118 ),
 .UNSPECIFIED., .F., .F.,
 ( 4, 2, 2, 2, 4 ),
 ( 0.000000000000000000, 0.2500000000000000000, 0.5000000000000000000, 0.7500000000000000000, 1.000000000000000000 ),
 .UNSPECIFIED. ) ;
#27648 = CARTESIAN_POINT ( 'NONE',  ( 8.277732780410000046, 4.874567052833000069, 6.119507471270999588 ) ) ;
#27649 = CARTESIAN_POINT ( 'NONE',  ( 9.815201913989998417, 2.813632032385000148, 8.848857341496000117 ) ) ;
#27650 = CARTESIAN_POINT ( 'NONE',  ( 12.37577160951050814, 2.954704321271699019, 12.33392404961603894 ) ) ;
#27651 = ORIENTED_EDGE ( 'NONE', *, *, #37832, .F. ) ;
#27652 = CARTESIAN_POINT ( 'NONE',  ( 7.662260841227999997, 2.688365364125000045, 8.140015608605001063 ) ) ;
#27653 = CARTESIAN_POINT ( 'NONE',  ( 11.43302763632549990, 2.964209339073000216, -7.022058766158599141 ) ) ;
#27654 = CARTESIAN_POINT ( 'NONE',  ( 18.22023691865391015, -0.2863297863804597498, 12.59675086341328409 ) ) ;
#27655 = SHAPE_REPRESENTATION ( 'Drip Tip - Airflow Cap', ( #9676 ), #42081 ) ;
#27656 = CARTESIAN_POINT ( 'NONE',  ( 8.499265421555000088, 3.759926620436100375, -8.741861511046000288 ) ) ;
#27658 = CARTESIAN_POINT ( 'NONE',  ( 17.75497146387445468, -0.5922552425703458967, 12.68140545290050802 ) ) ;
#27657 = CARTESIAN_POINT ( 'NONE',  ( 9.660528907822998335, 2.899999999999999911, -6.152188490330000370 ) ) ;
#27659 = CARTESIAN_POINT ( 'NONE',  ( 11.29997394301484093, 12.21464834955394352, 1.635338263058603303 ) ) ;
#27660 = ORIENTED_EDGE ( 'NONE', *, *, #22129, .F. ) ;
#27661 = AXIS2_PLACEMENT_3D ( 'NONE', #1709, #54152, #65675 ) ;
#27662 = CARTESIAN_POINT ( 'NONE',  ( 12.19590851926989927, 0.1412562895068591451, 12.69896251113184427 ) ) ;
#27663 = CARTESIAN_POINT ( 'NONE',  ( 12.80505043854144276, 0.6250000000000001110, 13.88107975066923494 ) ) ;
#27664 = EDGE_CURVE ( 'NONE', #64274, #42800, #36201, .T. ) ;
#27665 = COLOUR_RGB ( '', 0.40784314, 0.44705882, 0.49803922) ;
#27666 = CARTESIAN_POINT ( 'NONE',  ( 21.60000021221999944, 12.84999978760999895, 2.874107720315999839E-09 ) ) ;
#27667 = CARTESIAN_POINT ( 'NONE',  ( 8.969113844317998741, 4.218953675027299788, 8.338908357746399602 ) ) ;
#27668 = EDGE_CURVE ( 'NONE', #30122, #69104, #27556, .T. ) ;
#27670 = CARTESIAN_POINT ( 'NONE',  ( 12.18865279333487095, -2.902449960337692314, 13.69583488376822622 ) ) ;
#27669 = AXIS2_PLACEMENT_3D ( 'NONE', #13565, #34885, #24385 ) ;
#27671 = CARTESIAN_POINT ( 'NONE',  ( 11.59999999999999964, -2.935681553670999921, -8.155535082817699788 ) ) ;
#27672 = CARTESIAN_POINT ( 'NONE',  ( 24.57009630585800153, 3.716770706295000171, -12.37072133406000063 ) ) ;
#27673 = ORIENTED_EDGE ( 'NONE', *, *, #28344, .T. ) ;
#27674 = DIRECTION ( 'NONE',  ( 1.000000000000000000, 0.000000000000000000, 0.000000000000000000 ) ) ;
#27675 = CARTESIAN_POINT ( 'NONE',  ( 17.60000000000000142, -10.78295181803999903, 4.410266442048000002 ) ) ;
#27676 = AXIS2_PLACEMENT_3D ( 'NONE', #40731, #45979, #35498 ) ;
#27677 = CARTESIAN_POINT ( 'NONE',  ( 8.457129882803000598, 5.100036551512999949, -6.571411952062999440 ) ) ;
#27678 = CARTESIAN_POINT ( 'NONE',  ( 1.371338831777000111, -1.438367618452000007, -3.472675606904999768 ) ) ;
#27679 = DIRECTION ( 'NONE',  ( 0.000000000000000000, 0.000000000000000000, -1.000000000000000000 ) ) ;
#27680 = CARTESIAN_POINT ( 'NONE',  ( 17.59669571873551774, 1.876302067258580619, -12.57524312254454379 ) ) ;
#27681 = CARTESIAN_POINT ( 'NONE',  ( 9.821001730958839104, -4.768205771526717207, 8.499596153627864581 ) ) ;
#27682 = CARTESIAN_POINT ( 'NONE',  ( 10.80133863405319872, 4.534404523786000674, 6.818303296693398963 ) ) ;
#27683 = VECTOR ( 'NONE', #7306, 1000.000000000000000 ) ;
#27684 = CARTESIAN_POINT ( 'NONE',  ( 23.56664309646999911, -10.37807348783000094, 9.381504613656002078 ) ) ;
#27685 = CARTESIAN_POINT ( 'NONE',  ( 10.47111935320999976, -5.170637620872999385, -8.712950754783999940 ) ) ;
#27686 = CARTESIAN_POINT ( 'NONE',  ( 11.33810207955129812, 4.796537143354000499, -7.825000000000000178 ) ) ;
#27687 = B_SPLINE_SURFACE_WITH_KNOTS ( 'NONE', 3, 3, ( 
 ( #56445, #8550, #40702, #62029, #14145, #19727, #8892, #30228, #3632, #24969, #62372, #10261, #36839, #9917, #52916, #113, #30907, #58158, #41733, #9567, #57459, #46646, #26348, #15514, #68634, #37177, #26698, #47331, #68988, #20755, #42083, #31595, #68289, #20408, #5359 ),
 ( #21430, #5013, #4320, #47677, #63038, #25655, #31942, #42766, #36488, #21101, #52220, #41396, #64074, #15847, #52565, #42426, #4661, #46987, #48013, #63734, #58498, #10601, #53254, #16193, #31255, #37516, #58841, #15165, #57809, #10949, #51875, #3971, #25308, #26000, #67953 ),
 ( #20069, #63392, #62704, #14824, #36147, #6384, #1848, #23165, #37863, #44513, #60233, #33321, #38205, #48705, #59187, #28425, #28073, #49384, #1499, #65106, #54639, #59533, #22817, #6733, #808, #22124, #11983, #33668, #44165, #12336, #53938, #65808, #43811, #64414, #17231 ),
 ( #38554, #43467, #27735, #17933, #39251, #11288, #60576, #54987, #65461, #11629, #64760, #59876, #17584, #32293, #7083, #5698, #53601, #38910, #49739, #16878, #27040, #48351, #458, #21775, #32969, #54282, #43111, #16537, #32629, #6041, #27379, #49047, #1155, #22464, #20587 ) ),
 .UNSPECIFIED., .F., .F., .F.,
 ( 4, 4 ),
 ( 4, 1, 1, 1, 1, 1, 1, 1, 1, 1, 1, 1, 1, 1, 1, 1, 1, 1, 1, 1, 1, 1, 1, 1, 1, 1, 1, 1, 1, 1, 1, 1, 4 ),
 ( -0.1039086239011999951, 1.103908623900999864 ),
 ( 0.1942321073450000157, 0.2199060843169000079, 0.2455800612886999967, 0.2712540382605999612, 0.2969280152323999777, 0.3226019922043000254, 0.3482759691761000420, 0.3739499461479999787, 0.3996239231197999953, 0.4252979000916999874, 0.4509718770635000040, 0.4766458540353999962, 0.5023198310072000128, 0.5279938079791000050, 0.5536677849509000771, 0.5793417619227999582, 0.6050157388945999193, 0.6306897158665000225, 0.6563636928382999836, 0.6820376698101999757, 0.7077116467820000478, 0.7333856237539000400, 0.7590596007256998901, 0.7847335776975999933, 0.8104075546693999543, 0.8360815316413000575, 0.8617555086131000186, 0.8874294855850000108, 0.9131034625568000829, 0.9387774395286999640, 0.9644514165004999251, 0.9901253934722999972, 1.015799370444000038 ),
 .UNSPECIFIED. ) ;
#27688 = CARTESIAN_POINT ( 'NONE',  ( 9.707733921870000060, -2.624754973437999794, -6.486841649805000110 ) ) ;
#27689 = CARTESIAN_POINT ( 'NONE',  ( 24.05251143665766733, 9.284066128425779496, -9.220293913675572384 ) ) ;
#27690 = FACE_OUTER_BOUND ( 'NONE', #2008, .T. ) ;
#27691 = ORIENTED_EDGE ( 'NONE', *, *, #47101, .T. ) ;
#27692 = CARTESIAN_POINT ( 'NONE',  ( 11.03776249210999971, -8.050323671732000363, -6.914613055281999543 ) ) ;
#27693 = CARTESIAN_POINT ( 'NONE',  ( 12.19559063708295987, -2.913481137622000006, 7.194517870904999945 ) ) ;
#27694 = ORIENTED_EDGE ( 'NONE', *, *, #14239, .T. ) ;
#27695 = CARTESIAN_POINT ( 'NONE',  ( 18.16386294024318460, -2.642762625146028110, 13.64216358405140994 ) ) ;
#27696 = CARTESIAN_POINT ( 'NONE',  ( 10.64118447801629941, -2.722297859592000435, -7.471828720557429193 ) ) ;
#27697 = VERTEX_POINT ( 'NONE', #42144 ) ;
#27698 = CARTESIAN_POINT ( 'NONE',  ( 11.60988784977536348, 3.148894096305599799, 7.548634759728509280 ) ) ;
#27699 = CARTESIAN_POINT ( 'NONE',  ( 6.164613237910274712, 0.5517680008132791469, 0.9902087497090418244 ) ) ;
#27700 = CARTESIAN_POINT ( 'NONE',  ( 23.96072736199457154, 3.344687141702650912, -12.82061042838967779 ) ) ;
#27701 = CARTESIAN_POINT ( 'NONE',  ( 18.49055856039300139, -2.949841519493000330, 11.23086453091999992 ) ) ;
#27702 = CARTESIAN_POINT ( 'NONE',  ( 4.650000881942760067, -3.073097332162000125E-13, -5.595524044110998485E-14 ) ) ;
#27703 = DIRECTION ( 'NONE',  ( 0.000000000000000000, -0.8304044637637929549, -0.5571610418551961041 ) ) ;
#27704 = CARTESIAN_POINT ( 'NONE',  ( 7.282019735819710071, -0.9188793378149595625, 0.6322026530472603101 ) ) ;
#27705 = CARTESIAN_POINT ( 'NONE',  ( 10.06728329455999926, -4.192861215955000276, -5.985050974557999837 ) ) ;
#27706 = CARTESIAN_POINT ( 'NONE',  ( 21.00000012402660232, -1.355183834107999921E-13, -12.42499880353998876 ) ) ;
#27707 = ORIENTED_EDGE ( 'NONE', *, *, #48490, .T. ) ;
#27708 = EDGE_CURVE ( 'NONE', #68740, #12282, #1957, .T. ) ;
#27709 = EDGE_CURVE ( 'NONE', #66543, #12955, #57783, .T. ) ;
#27710 = CARTESIAN_POINT ( 'NONE',  ( 8.581920280410001212, 4.769017407621999993, -8.862909124839001507 ) ) ;
#27711 = VERTEX_POINT ( 'NONE', #63448 ) ;
#27712 = B_SPLINE_CURVE_WITH_KNOTS ( 'NONE', 3,
 ( #63426, #57157, #10295, #9601 ),
 .UNSPECIFIED., .F., .F.,
 ( 4, 4 ),
 ( 0.000000000000000000, 1.000000000000000000 ),
 .UNSPECIFIED. ) ;
#27713 = CARTESIAN_POINT ( 'NONE',  ( 24.53429010005800137, -12.47024913742999885, 3.026245653581999928 ) ) ;
#27714 =( NAMED_UNIT ( * ) PLANE_ANGLE_UNIT ( ) SI_UNIT ( $, .RADIAN. ) );
#27715 = ORIENTED_EDGE ( 'NONE', *, *, #54531, .T. ) ;
#27716 = DIRECTION ( 'NONE',  ( 1.000000000000000000, 0.000000000000000000, 3.738339622219000240E-14 ) ) ;
#27717 = CIRCLE ( 'NONE', #66784, 0.5000000000000014433 ) ;
#27718 = CARTESIAN_POINT ( 'NONE',  ( 25.26126798770998505, -8.521553306829913410, 7.991940928116512133 ) ) ;
#27719 = FACE_OUTER_BOUND ( 'NONE', #56002, .T. ) ;
#27720 = CARTESIAN_POINT ( 'NONE',  ( 12.49024380163858439, 3.040024005673538809, 13.54391858567110241 ) ) ;
#27721 = CARTESIAN_POINT ( 'NONE',  ( 10.51654446536000087, -4.930670681812999945, 8.573593359022000371 ) ) ;
#27722 = VECTOR ( 'NONE', #64766, 1000.000000000000000 ) ;
#27723 = CARTESIAN_POINT ( 'NONE',  ( 10.90000000000000036, -0.2500000000000000000, -4.902439024389999567 ) ) ;
#27724 = CARTESIAN_POINT ( 'NONE',  ( 12.20981157025896913, 0.1908382484571561621, 13.89824168789395920 ) ) ;
#27725 = ORIENTED_EDGE ( 'NONE', *, *, #68875, .T. ) ;
#27726 = CARTESIAN_POINT ( 'NONE',  ( 7.547271682458000619, 5.017953588770000195, -6.429833855306000601 ) ) ;
#27727 = DIRECTION ( 'NONE',  ( 0.000000000000000000, 1.000000000000000000, 0.000000000000000000 ) ) ;
#27728 = EDGE_CURVE ( 'NONE', #17232, #16376, #64450, .T. ) ;
#27729 = CARTESIAN_POINT ( 'NONE',  ( 4.400000000000000355, 0.000000000000000000, 0.000000000000000000 ) ) ;
#27730 = CIRCLE ( 'NONE', #14308, 12.50000000000000000 ) ;
#27731 = CARTESIAN_POINT ( 'NONE',  ( 4.905636958659999713, 1.235401976546000036, 1.063025361430000038 ) ) ;
#27732 = B_SPLINE_CURVE_WITH_KNOTS ( 'NONE', 3,
 ( #12789, #50532, #29220, #65567, #17690, #13140, #11734, #45295, #44616, #49842, #22918, #23612, #18038, #44270, #33424, #61023, #2634, #39015 ),
 .UNSPECIFIED., .F., .F.,
 ( 4, 2, 2, 2, 2, 2, 2, 2, 4 ),
 ( 0.000000000000000000, 0.1250000000000000000, 0.2500000000000000000, 0.3750000000000000000, 0.5000000000000000000, 0.6250000000000000000, 0.7500000000000000000, 0.8750000000000000000, 1.000000000000000000 ),
 .UNSPECIFIED. ) ;
#27733 = CARTESIAN_POINT ( 'NONE',  ( 9.237204719595000668, 3.071719032003000116, -6.037263251225000182 ) ) ;
#27734 = CARTESIAN_POINT ( 'NONE',  ( 10.90000000000000036, 0.2500000000000000000, -9.776630298829998011 ) ) ;
#27735 = CARTESIAN_POINT ( 'NONE',  ( 11.15192313136999935, -2.359310578948000003, -6.636692315558000210 ) ) ;
#27736 = ORIENTED_EDGE ( 'NONE', *, *, #67014, .F. ) ;
#27737 = DIRECTION ( 'NONE',  ( 0.000000000000000000, 1.000000000000000000, 0.000000000000000000 ) ) ;
#27738 = FACE_OUTER_BOUND ( 'NONE', #25418, .T. ) ;
#27739 = PLANE ( 'NONE',  #54511 ) ;
#27740 = DIRECTION ( 'NONE',  ( 1.000000000000000000, 0.000000000000000000, 0.000000000000000000 ) ) ;
#27741 = CARTESIAN_POINT ( 'NONE',  ( 11.00000000000000000, 2.799999999999999822, -5.865766984179000332 ) ) ;
#27742 = CARTESIAN_POINT ( 'NONE',  ( 1.011390132542624665, 3.499999999999998224, 0.4581489286485194157 ) ) ;
#27743 = CARTESIAN_POINT ( 'NONE',  ( 11.14256920625030034, 4.042230905578960254, -6.325872106312999676 ) ) ;
#27744 = CARTESIAN_POINT ( 'NONE',  ( 10.16657120343299958, 3.951311476804090006, -8.503230697164999796 ) ) ;
#27746 = CARTESIAN_POINT ( 'NONE',  ( 11.04200385643000182, -2.754971892945000000, 5.031215070518999966 ) ) ;
#27745 = CARTESIAN_POINT ( 'NONE',  ( 10.60892546752099896, -4.864937374655599278, 7.559927309296559983 ) ) ;
#27747 = B_SPLINE_CURVE_WITH_KNOTS ( 'NONE', 3,
 ( #44611, #40377, #65906, #61699, #18375, #2970, #60670, #29571, #24647, #50873, #61019, #23957, #35487, #18034, #7880, #50528 ),
 .UNSPECIFIED., .F., .F.,
 ( 4, 2, 2, 2, 2, 2, 2, 4 ),
 ( 0.000000000000000000, 0.06249999999999941713, 0.1249999999999988343, 0.2499999999999997224, 0.4999999999999998890, 0.7500000000000000000, 0.8749999999999998890, 1.000000000000000000 ),
 .UNSPECIFIED. ) ;
#27748 = PLANE ( 'NONE',  #52002 ) ;
#27749 = VERTEX_POINT ( 'NONE', #23829 ) ;
#27750 = CARTESIAN_POINT ( 'NONE',  ( 11.39189666366029918, 3.947847673382490541, 6.326270943800999191 ) ) ;
#27751 = CARTESIAN_POINT ( 'NONE',  ( 9.843726350706999639, -4.115123626494000320, 9.466607949400000166 ) ) ;
#27752 = CARTESIAN_POINT ( 'NONE',  ( 10.44222949779799947, 4.633452903845899584, 6.550014196338999284 ) ) ;
#27753 = CARTESIAN_POINT ( 'NONE',  ( 5.613892323500530246, -12.94560306806822503, 2.448221630819331640 ) ) ;
#27754 = CARTESIAN_POINT ( 'NONE',  ( 9.199609130449999839, -2.551382302226000487, 7.536606162076999738 ) ) ;
#27755 = EDGE_CURVE ( 'NONE', #28289, #40442, #45300, .T. ) ;
#27756 = CARTESIAN_POINT ( 'NONE',  ( 8.573148997459998810, 5.167567567567999731, -6.822293592207000934 ) ) ;
#27757 = CARTESIAN_POINT ( 'NONE',  ( 11.31944011432000075, 3.562654288336999819, -11.75631193234000094 ) ) ;
#27758 = CARTESIAN_POINT ( 'NONE',  ( 9.229392757687000071, -3.322036695224600322, -8.241085728986799808 ) ) ;
#27759 = DIRECTION ( 'NONE',  ( -1.000000000000000000, 0.000000000000000000, 0.000000000000000000 ) ) ;
#27760 = B_SPLINE_CURVE_WITH_KNOTS ( 'NONE', 3,
 ( #43474, #15520, #36847, #31601, #5019, #52923, #53608, #43117, #26358, #26007, #47684, #64771, #16885, #11295, #21107, #32977, #37874, #4667 ),
 .UNSPECIFIED., .F., .F.,
 ( 4, 2, 2, 2, 2, 2, 2, 2, 4 ),
 ( 0.000000000000000000, 0.1250000000000000833, 0.2500000000000001665, 0.3750000000000001665, 0.5000000000000002220, 0.6250000000000002220, 0.7500000000000001110, 0.8750000000000001110, 1.000000000000000000 ),
 .UNSPECIFIED. ) ;
#27761 = CARTESIAN_POINT ( 'NONE',  ( 5.757073283530000474, -0.6440133831468000114, 0.9840870706126000345 ) ) ;
#27762 = FACE_OUTER_BOUND ( 'NONE', #66171, .T. ) ;
#27763 = CONICAL_SURFACE ( 'NONE', #61250, 2.325000277643999969, 0.7853982725543797727 ) ;
#27764 = DIRECTION ( 'NONE',  ( -1.000000000000000000, -4.609710477022999584E-09, -1.269678721256999984E-09 ) ) ;
#27765 = CARTESIAN_POINT ( 'NONE',  ( 12.35979573085659844, -3.159987984332300215, 7.354650721737899133 ) ) ;
#27766 = CARTESIAN_POINT ( 'NONE',  ( 11.61364291764652812, 3.140345330584100036, -7.393734108507599601 ) ) ;
#27767 = DIRECTION ( 'NONE',  ( 1.000000000000000000, 0.000000000000000000, 0.000000000000000000 ) ) ;
#27769 = FACE_OUTER_BOUND ( 'NONE', #61966, .T. ) ;
#27768 = AXIS2_PLACEMENT_3D ( 'NONE', #24655, #61374, #66611 ) ;
#27770 = CARTESIAN_POINT ( 'NONE',  ( 1.050973465875000068, 3.500000000000000000, 0.000000000000000000 ) ) ;
#27771 = EDGE_LOOP ( 'NONE', ( #59787, #39118, #9673, #14827 ) ) ;
#27772 = CARTESIAN_POINT ( 'NONE',  ( 13.50018479229300006, -11.60142623882999935, -2.415183939829000259 ) ) ;
#27773 = ITEM_DEFINED_TRANSFORMATION ( 'NONE', 'NONE', #5000,  #9676 ) ;
#27774 = CARTESIAN_POINT ( 'NONE',  ( 11.23589666366019912, -4.039600775206940497, -8.391246537305399045 ) ) ;
#27775 = CARTESIAN_POINT ( 'NONE',  ( 8.751496707488000126, 4.081676005979390176, 6.643597378104299622 ) ) ;
#27776 = CARTESIAN_POINT ( 'NONE',  ( 16.00000002095532992, -12.11988194449493506, 3.159760537119275181 ) ) ;
#27777 = CARTESIAN_POINT ( 'NONE',  ( 7.000000000000001776, 9.718048825484419950, 4.627116016484593253 ) ) ;
#27778 = CARTESIAN_POINT ( 'NONE',  ( 13.58069952315600126, 12.39169461668999972, 2.069104550346000160 ) ) ;
#27779 = ORIENTED_EDGE ( 'NONE', *, *, #5306, .F. ) ;
#27780 = CARTESIAN_POINT ( 'NONE',  ( 24.35365242081700288, 8.355077740067001102, 8.511587483820997946 ) ) ;
#27781 = CARTESIAN_POINT ( 'NONE',  ( 8.783078676347997771, -4.247267730859300094, -8.446684196061099215 ) ) ;
#27782 = ORIENTED_EDGE ( 'NONE', *, *, #5762, .T. ) ;
#27783 = CARTESIAN_POINT ( 'NONE',  ( 11.04783424078000031, -2.764605797469000148, 5.041477660832000218 ) ) ;
#27784 = DIRECTION ( 'NONE',  ( 0.000000000000000000, 0.7071067811865474617, -0.7071067811865474617 ) ) ;
#27785 = CARTESIAN_POINT ( 'NONE',  ( 9.219964158774999419, 3.941185585667000169, -8.896279800194999865 ) ) ;
#27786 = CARTESIAN_POINT ( 'NONE',  ( 17.55505043854143565, 1.875000000000000000, -12.57545641911172751 ) ) ;
#27787 = B_SPLINE_CURVE_WITH_KNOTS ( 'NONE', 3,
 ( #30539, #51850, #14118, #35442, #25287, #52197, #3607, #41023, #14462, #35782, #57097, #41371, #9196, #67926, #20042, #36120, #47989, #58474, #64735, #26676, #43782, #16851, #11601, #10579, #59159, #91, #6357, #58817, #53232, #780 ),
 .UNSPECIFIED., .F., .F.,
 ( 4, 2, 1, 1, 2, 2, 2, 2, 2, 2, 2, 2, 2, 2, 2, 4 ),
 ( 0.000000000000000000, 0.1250000000000011102, 0.1875000000000016653, 0.2187500000000019429, 0.2343750000000018874, 0.2500000000000018319, 0.3750000000000014433, 0.4375000000000012212, 0.5000000000000009992, 0.5625000000000007772, 0.6250000000000005551, 0.6875000000000003331, 0.7500000000000001110, 0.8124999999999998890, 0.8749999999999996669, 1.000000000000000000 ),
 .UNSPECIFIED. ) ;
#27788 = CARTESIAN_POINT ( 'NONE',  ( 10.80502344389999791, -5.125258734743999511, -6.817099149379099110 ) ) ;
#27789 = CARTESIAN_POINT ( 'NONE',  ( 7.373895280404999752, 4.512523768570999572, -9.154878768564000069 ) ) ;
#27790 = CARTESIAN_POINT ( 'NONE',  ( 11.30000000000000071, 4.368599826607999503, 15.48886178036999972 ) ) ;
#27791 = CARTESIAN_POINT ( 'NONE',  ( 4.846693173016666911, 1.310679582531385501, 0.7554284705563518720 ) ) ;
#27792 = ORIENTED_EDGE ( 'NONE', *, *, #7571, .T. ) ;
#27793 = CARTESIAN_POINT ( 'NONE',  ( 6.799999999999999822, 0.000000000000000000, 0.000000000000000000 ) ) ;
#27794 = EDGE_CURVE ( 'NONE', #49128, #37678, #61007, .T. ) ;
#27795 = EDGE_CURVE ( 'NONE', #61758, #28902, #34682, .T. ) ;
#27796 = CARTESIAN_POINT ( 'NONE',  ( 17.81484293439625688, -3.068795199404298124, -13.53617370485920013 ) ) ;
#27797 =( NAMED_UNIT ( * ) SI_UNIT ( $, .STERADIAN. ) SOLID_ANGLE_UNIT ( ) );
#27798 = EDGE_LOOP ( 'NONE', ( #58441, #34239, #46018, #19014 ) ) ;
#27799 = VECTOR ( 'NONE', #32448, 1000.000000000000000 ) ;
#27800 = CYLINDRICAL_SURFACE ( 'NONE', #12468, 1.999999999999999778 ) ;
#27801 = CARTESIAN_POINT ( 'NONE',  ( 11.50029455687000102, 11.65000000000000213, 0.4692429876170854386 ) ) ;
#27802 = ORIENTED_EDGE ( 'NONE', *, *, #59093, .T. ) ;
#27803 = CARTESIAN_POINT ( 'NONE',  ( 9.052088727410998459, 2.999102593977000186, 7.416055476975279781 ) ) ;
#27804 = CARTESIAN_POINT ( 'NONE',  ( 17.81303847540711516, -1.807878129530196221, -12.46962684194071791 ) ) ;
#27805 = CARTESIAN_POINT ( 'NONE',  ( 4.545393627743999687, -0.9903479682421998387, -1.012736759802999931 ) ) ;
#27806 = CARTESIAN_POINT ( 'NONE',  ( 11.60000000000000320, 3.468809616172332078, -6.694115079111573330 ) ) ;
#27807 = DIRECTION ( 'NONE',  ( -1.000000000000000000, 0.000000000000000000, 0.000000000000000000 ) ) ;
#27808 = CARTESIAN_POINT ( 'NONE',  ( 24.30001694391200218, -12.21047201246000036, 3.271805662802000025 ) ) ;
#27809 = CARTESIAN_POINT ( 'NONE',  ( 9.813975701332999790, 4.636077325177999420, 6.910836541441499392 ) ) ;
#27810 = CARTESIAN_POINT ( 'NONE',  ( 8.726967411678998587, 3.935557623441470643, -8.391190439313799487 ) ) ;
#27811 = ORIENTED_EDGE ( 'NONE', *, *, #58396, .F. ) ;
#27812 = CARTESIAN_POINT ( 'NONE',  ( 5.600023899775999681, -13.94845324556000143, -4.312847325879000770 ) ) ;
#27813 = CARTESIAN_POINT ( 'NONE',  ( 10.43325471958999984, 5.596203146559000530, -8.042024377770999877 ) ) ;
#27814 = EDGE_CURVE ( 'NONE', #64952, #2109, #32649, .T. ) ;
#27815 = CARTESIAN_POINT ( 'NONE',  ( 9.679055905794999859, 2.899999999999999911, 6.571291218949999902 ) ) ;
#27816 = CARTESIAN_POINT ( 'NONE',  ( 12.50306195774379958, 1.853743832531304481, -13.87673314481786591 ) ) ;
#27817 = CARTESIAN_POINT ( 'NONE',  ( 11.29184687351630423, -4.999583552997724389, 8.268183399968647151 ) ) ;
#27818 = ADVANCED_FACE ( 'NONE', ( #16929 ), #11343, .T. ) ;
#27819 = CARTESIAN_POINT ( 'NONE',  ( 11.25041341105000114, -5.730771985297000271, 8.122672103119001008 ) ) ;
#27820 = CARTESIAN_POINT ( 'NONE',  ( 18.06311169547814899, 0.3645810575750376703, 13.89357890581305099 ) ) ;
#27821 = DIRECTION ( 'NONE',  ( -1.000000000000000000, 0.000000000000000000, 0.000000000000000000 ) ) ;
#27822 = ORIENTED_EDGE ( 'NONE', *, *, #26671, .F. ) ;
#27823 = EDGE_LOOP ( 'NONE', ( #49127, #19804, #2164, #68702 ) ) ;
#27824 = VECTOR ( 'NONE', #15276, 999.9999999999998863 ) ;
#27825 = CARTESIAN_POINT ( 'NONE',  ( 10.27967883605999866, 5.739712809045000697, 7.774963411801000923 ) ) ;
#27826 = CARTESIAN_POINT ( 'NONE',  ( 12.52211160811865120, -0.5573818237641869899, 13.88495700090146734 ) ) ;
#27827 = CARTESIAN_POINT ( 'NONE',  ( 12.42340929148597617, -0.4950008743047930593, -13.88813607082249035 ) ) ;
#27828 = CARTESIAN_POINT ( 'NONE',  ( 10.31668414895000119, -3.819528725844000494, 6.062183754159999438 ) ) ;
#27829 = CARTESIAN_POINT ( 'NONE',  ( 18.06407613793124511, -0.3627976900031492646, -13.89363072198946547 ) ) ;
#27830 = CARTESIAN_POINT ( 'NONE',  ( 8.766851002546001581, 2.832432432432000269, 6.822293592207000934 ) ) ;
#27831 = DIRECTION ( 'NONE',  ( -0.7071067811865605623, 0.09428090767661463645, 0.7007932009142605612 ) ) ;
#27833 = CARTESIAN_POINT ( 'NONE',  ( 18.29999330150736014, 11.02846243710159868, -3.754394858750199848 ) ) ;
#27832 = CARTESIAN_POINT ( 'NONE',  ( 9.728442991499999692, -4.080527519162810535, 8.776675254768999679 ) ) ;
#27834 = CARTESIAN_POINT ( 'NONE',  ( 10.09964828895399869, 5.121614868497999851, -8.112615456209400833 ) ) ;
#27835 = PLANE ( 'NONE',  #14600 ) ;
#27836 = CARTESIAN_POINT ( 'NONE',  ( 18.22495619086188512, 11.54180252136524487, -4.316564229370158934 ) ) ;
#27837 = CARTESIAN_POINT ( 'NONE',  ( 17.63678281077947574, -0.6199686954221033108, 12.67962180225517876 ) ) ;
#27838 = B_SPLINE_SURFACE_WITH_KNOTS ( 'NONE', 3, 3, ( 
 ( #48729, #36860, #58180, #21453 ),
 ( #21799, #26022, #15868, #10282 ),
 ( #26721, #53960, #64098, #6063 ),
 ( #5719, #48033, #37200, #27062 ),
 ( #43133, #64437, #16559, #52937 ),
 ( #26371, #20429, #53281, #47698 ),
 ( #57831, #5382, #41758, #36510 ),
 ( #139, #63059, #31276, #4681 ),
 ( #47351, #69009, #35327, #24486 ) ),
 .UNSPECIFIED., .F., .F., .F.,
 ( 4, 1, 1, 1, 1, 1, 4 ),
 ( 4, 4 ),
 ( 0.02209653170519000273, 0.1666666666667000196, 0.3333333333333000081, 0.5000000000000000000, 0.6666666666667000474, 0.8333333333333000637, 0.9492823795161999811 ),
 ( -0.1916656884162999952, 1.191851428473000185 ),
 .UNSPECIFIED. ) ;
#27839 = CARTESIAN_POINT ( 'NONE',  ( 8.473304831784332691, 5.100000000000000533, 6.564173320837334735 ) ) ;
#27840 = CARTESIAN_POINT ( 'NONE',  ( 17.55505043854147118, -3.125000000000000000, -12.28373071562070074 ) ) ;
#27841 = ORIENTED_EDGE ( 'NONE', *, *, #12706, .F. ) ;
#27843 = DIRECTION ( 'NONE',  ( 1.000000000000000000, 0.000000000000000000, 0.000000000000000000 ) ) ;
#27842 = DIRECTION ( 'NONE',  ( 1.000000000000000000, 0.000000000000000000, 0.000000000000000000 ) ) ;
#27844 = CARTESIAN_POINT ( 'NONE',  ( 8.514954719592999766, 3.207599814920999659, -6.150466394809999571 ) ) ;
#27845 = FACE_OUTER_BOUND ( 'NONE', #25371, .T. ) ;
#27846 = CARTESIAN_POINT ( 'NONE',  ( 0.7984915348666999924, -3.532786812989999969, -1.105428934477000080 ) ) ;
#27847 = CARTESIAN_POINT ( 'NONE',  ( 10.65413259636999932, 3.216622244594500302, 7.073141822156699732 ) ) ;
#27848 = CARTESIAN_POINT ( 'NONE',  ( 10.84161084123000052, 2.641275823976000137, -7.444905437480000110 ) ) ;
#27849 = VERTEX_POINT ( 'NONE', #11687 ) ;
#27850 = CARTESIAN_POINT ( 'NONE',  ( 12.08472055051100824, -0.08234928811777623980, -12.59973629603894274 ) ) ;
#27852 = DIRECTION ( 'NONE',  ( -1.000000000000000000, 0.000000000000000000, 0.000000000000000000 ) ) ;
#27851 = B_SPLINE_CURVE_WITH_KNOTS ( 'NONE', 3,
 ( #44666, #17744, #7242, #971, #34168, #33477, #11443, #54792, #22623, #39064, #22283, #43624, #18084, #55139, #60726, #55486, #27889, #7586 ),
 .UNSPECIFIED., .F., .F.,
 ( 4, 2, 2, 2, 2, 2, 2, 2, 4 ),
 ( 0.000000000000000000, 0.1249999999999999722, 0.2499999999999999445, 0.3749999999999998890, 0.4999999999999998890, 0.6249999999999998890, 0.7499999999999997780, 0.8749999999999998890, 1.000000000000000000 ),
 .UNSPECIFIED. ) ;
#27853 = CARTESIAN_POINT ( 'NONE',  ( 10.22514748322304534, -2.649941783575446408, 7.500008211948054004 ) ) ;
#27854 = CARTESIAN_POINT ( 'NONE',  ( 7.399999923048000028, 0.000000000000000000, -0.9999997023190999590 ) ) ;
#27855 = CARTESIAN_POINT ( 'NONE',  ( 8.411454719592999396, 3.882020551409000042, 5.870058896428999695 ) ) ;
#27856 = ORIENTED_EDGE ( 'NONE', *, *, #57307, .F. ) ;
#27857 = CARTESIAN_POINT ( 'NONE',  ( 5.651046267567999770, 0.7718853692621999718, -1.249287881180999982 ) ) ;
#27858 = CARTESIAN_POINT ( 'NONE',  ( 7.549170280409000178, 5.250007070404999254, -8.441605882928000071 ) ) ;
#27860 = CARTESIAN_POINT ( 'NONE',  ( 10.87835931249066768, 5.126777126180478206, 6.752018918863570640 ) ) ;
#27859 = CARTESIAN_POINT ( 'NONE',  ( 8.461280570003118839, -2.261174139539910311, 7.238226757569249159 ) ) ;
#27861 = CARTESIAN_POINT ( 'NONE',  ( 11.26212378248529866, 3.384904051819500381, -6.336291382830999908 ) ) ;
#27862 = ORIENTED_EDGE ( 'NONE', *, *, #3554, .F. ) ;
#27863 = CARTESIAN_POINT ( 'NONE',  ( 10.34393020685000053, -5.250000000000000000, 7.500000000000000000 ) ) ;
#27864 = CARTESIAN_POINT ( 'NONE',  ( 10.01532628870999986, -4.946995631616999844, 8.559221361189001342 ) ) ;
#27865 = ORIENTED_EDGE ( 'NONE', *, *, #24786, .T. ) ;
#27866 = DIRECTION ( 'NONE',  ( 0.000000000000000000, 1.000000000000000000, 0.000000000000000000 ) ) ;
#27867 = CARTESIAN_POINT ( 'NONE',  ( 24.44496482743900145, 12.03536723905999928, -3.224852005146999989 ) ) ;
#27868 = CARTESIAN_POINT ( 'NONE',  ( 17.63678025734560251, -0.6199690124688013171, -13.88138352397877462 ) ) ;
#27869 = ORIENTED_EDGE ( 'NONE', *, *, #44142, .F. ) ;
#27870 = CARTESIAN_POINT ( 'NONE',  ( 10.33455242540051522, -5.771779017986490068, -7.375668094431187427 ) ) ;
#27871 = CARTESIAN_POINT ( 'NONE',  ( 8.829015684063998393, -3.399013800391000206, -6.242130679267000382 ) ) ;
#27872 = CARTESIAN_POINT ( 'NONE',  ( 11.56833327354034857, 3.253412192327699959, -7.011667014989399149 ) ) ;
#27873 = CARTESIAN_POINT ( 'NONE',  ( 8.886105992892519012, -2.780583821594381888, 8.755311148983734526 ) ) ;
#27874 = CARTESIAN_POINT ( 'NONE',  ( 9.428197172113431890, -5.125396288428772706, 6.749639981086940743 ) ) ;
#27875 = VERTEX_POINT ( 'NONE', #53995 ) ;
#27876 = CARTESIAN_POINT ( 'NONE',  ( 7.807364158771999740, 3.650414032626000171, 6.083147621602999600 ) ) ;
#27877 = EDGE_CURVE ( 'NONE', #9091, #26424, #55188, .T. ) ;
#27878 = ADVANCED_FACE ( 'NONE', ( #54339 ), #6097, .F. ) ;
#27879 = CARTESIAN_POINT ( 'NONE',  ( 17.65064139367258988, -1.793792787906298036, 13.88460705996369349 ) ) ;
#27880 = CARTESIAN_POINT ( 'NONE',  ( 9.958513540183334456, -4.163624617374470205, 6.250000000000000000 ) ) ;
#27881 = CARTESIAN_POINT ( 'NONE',  ( 15.35870478550200069, -9.525289020731998235, -8.192348383776000276 ) ) ;
#27882 = ORIENTED_EDGE ( 'NONE', *, *, #53434, .T. ) ;
#27883 = CARTESIAN_POINT ( 'NONE',  ( 12.26133075698776942, -2.191112520879996861, -12.51819442860477416 ) ) ;
#27884 = CARTESIAN_POINT ( 'NONE',  ( 10.76059687351619765, 3.370476274536378547, -6.407767014557177454 ) ) ;
#27885 = DIRECTION ( 'NONE',  ( 0.000000000000000000, -0.2461538461540070666, 0.9692307692307283729 ) ) ;
#27886 = CARTESIAN_POINT ( 'NONE',  ( 5.000030787343002103, 1.290525307673966449, 1.679270695423617399 ) ) ;
#27887 = DIRECTION ( 'NONE',  ( 1.000000000000000000, 0.000000000000000000, 0.000000000000000000 ) ) ;
#27888 = CARTESIAN_POINT ( 'NONE',  ( 11.30995122972050027, -3.547233695387300045, -6.452959986593999275 ) ) ;
#27889 = CARTESIAN_POINT ( 'NONE',  ( 6.044609839683374730, -1.500000000000000444, 0.1963495408493560745 ) ) ;
#27890 = CARTESIAN_POINT ( 'NONE',  ( 18.07990072965513662, -1.983698511703248180, 12.44287000959587175 ) ) ;
#27891 = ORIENTED_EDGE ( 'NONE', *, *, #27450, .F. ) ;
#27892 = CARTESIAN_POINT ( 'NONE',  ( 10.93479632507519916, -3.442212747724900268, -8.534037301706000278 ) ) ;
#27893 = B_SPLINE_CURVE_WITH_KNOTS ( 'NONE', 3,
 ( #41959, #52794, #47557, #46521, #46176, #10141, #62921, #57680, #41273, #4886, #40925, #68168, #3511, #67484, #25536, #9790, #31142, #20979, #42315, #52443, #37061, #24849, #14368, #15733, #9440, #36022, #63617, #4198, #58374, #62248, #57337, #4538 ),
 .UNSPECIFIED., .F., .F.,
 ( 4, 2, 2, 2, 2, 2, 2, 2, 1, 2, 2, 2, 1, 1, 1, 2, 2, 4 ),
 ( 0.000000000000000000, 0.2500000000000091593, 0.3750000000000153211, 0.4375000000000198175, 0.4687500000000232592, 0.5000000000000267564, 0.6250000000000375255, 0.6875000000000405231, 0.7187500000000419664, 0.7343750000000426326, 0.7500000000000434097, 0.8125000000000432987, 0.8437500000000421885, 0.8593750000000426326, 0.8671875000000418554, 0.8710937500000396350, 0.8750000000000375255, 1.000000000000000000 ),
 .UNSPECIFIED. ) ;
#27894 = ORIENTED_EDGE ( 'NONE', *, *, #20937, .T. ) ;
#27895 = AXIS2_PLACEMENT_3D ( 'NONE', #22768, #54592, #6688 ) ;
#27896 = CARTESIAN_POINT ( 'NONE',  ( 11.83966971788800215, -12.22235437154000159, -1.953272420501999784 ) ) ;
#27897 = CARTESIAN_POINT ( 'NONE',  ( 9.286929719595001131, 4.102804347295999854, -5.770625657082999460 ) ) ;
#27898 = CARTESIAN_POINT ( 'NONE',  ( 10.19715290653000217, 4.982626294267999967, -6.124313696433000054 ) ) ;
#27899 = ADVANCED_FACE ( 'NONE', ( #8443, #35025 ), #35364, .F. ) ;
#27900 = CARTESIAN_POINT ( 'NONE',  ( 10.81362580514000094, -3.876947229615999913, -9.022210119840998743 ) ) ;
#27901 = DIRECTION ( 'NONE',  ( 0.000000000000000000, 0.000000000000000000, 1.000000000000000000 ) ) ;
#27902 = CARTESIAN_POINT ( 'NONE',  ( 9.610944094206999466, 5.100000000000000533, -6.571291218949999902 ) ) ;
#27903 = CARTESIAN_POINT ( 'NONE',  ( 8.734997988989999129, 3.937347817007940343, -8.366433385397400002 ) ) ;
#27904 = VERTEX_POINT ( 'NONE', #67157 ) ;
#27905 = DIRECTION ( 'NONE',  ( 0.000000000000000000, 0.000000000000000000, 1.000000000000000000 ) ) ;
#27906 = CARTESIAN_POINT ( 'NONE',  ( 9.504903297738000134, 3.934733353759999552, 5.704831249548000471 ) ) ;
#27907 = CARTESIAN_POINT ( 'NONE',  ( 2.134306799209333416, 1.762666431298139713, 3.058252359239908458 ) ) ;
#27908 = CARTESIAN_POINT ( 'NONE',  ( 10.47145237372899906, 4.043732047787757189, -8.774080944853650976 ) ) ;
#27909 = CARTESIAN_POINT ( 'NONE',  ( 17.99211270977099986, 3.227071166021000082, -11.34499727797000013 ) ) ;
#27910 = CARTESIAN_POINT ( 'NONE',  ( 11.63410404293056999, 3.557672215630899970, -8.400720262063998689 ) ) ;
#27911 = CARTESIAN_POINT ( 'NONE',  ( 10.40686970472170536, 2.482357117332503194, 8.418222078226063942 ) ) ;
#27912 = CARTESIAN_POINT ( 'NONE',  ( 11.59999999999999964, 5.064318446328999634, -8.155535082817699788 ) ) ;
#27913 = B_SPLINE_CURVE_WITH_KNOTS ( 'NONE', 3,
 ( #67623, #14845, #36167, #13487, #51222 ),
 .UNSPECIFIED., .F., .F.,
 ( 4, 1, 4 ),
 ( 0.000000000000000000, 0.5000000000000000000, 1.000000000000000000 ),
 .UNSPECIFIED. ) ;
#27914 = CARTESIAN_POINT ( 'NONE',  ( 23.86794696826499873, -9.630643803976999706, 9.781828974359999762 ) ) ;
#27915 = CARTESIAN_POINT ( 'NONE',  ( 11.82349952450200270, -3.378095173501999948, 11.11014980558000076 ) ) ;
#27916 = EDGE_LOOP ( 'NONE', ( #35808, #50644, #61867, #68399, #12045 ) ) ;
#27917 = CARTESIAN_POINT ( 'NONE',  ( 8.672510841228998402, 4.686731264770999772, -8.717075579553000608 ) ) ;
#27918 = CARTESIAN_POINT ( 'NONE',  ( 7.194371378776000192, 0.06715535307189000880, 1.130410956850999904 ) ) ;
#27919 = CARTESIAN_POINT ( 'NONE',  ( 18.14022514731436431, 2.720460039646585670, 13.62418930002215589 ) ) ;
#27920 = DIRECTION ( 'NONE',  ( 0.000000000000000000, -0.5393439587572765870, 0.8420855622512650740 ) ) ;
#27921 = CARTESIAN_POINT ( 'NONE',  ( 11.08425954179440076, -3.017023678917100327, -8.316745941391600283 ) ) ;
#27922 = ORIENTED_EDGE ( 'NONE', *, *, #68032, .T. ) ;
#27923 = CARTESIAN_POINT ( 'NONE',  ( 24.74447889200699890, 3.238408025005999669, -11.83114124653999966 ) ) ;
#27924 = CARTESIAN_POINT ( 'NONE',  ( 8.913573341230998537, 2.550580605805000012, 8.854682662413999594 ) ) ;
#27926 = CARTESIAN_POINT ( 'NONE',  ( 9.255358248830999557, -3.910012670022149806, 6.649720865199900466 ) ) ;
#27925 = CARTESIAN_POINT ( 'NONE',  ( 9.161379719595000637, 5.511689883260999956, -7.095113581311000672 ) ) ;
#27927 = CARTESIAN_POINT ( 'NONE',  ( 10.74549836952449944, 3.055340480832492656, 4.827072375377776225 ) ) ;
#27928 = EDGE_CURVE ( 'NONE', #46774, #10029, #4280, .T. ) ;
#27929 = EDGE_LOOP ( 'NONE', ( #35959, #10414, #26922, #64608, #6102, #57472, #18751, #26106 ) ) ;
#27930 = EDGE_CURVE ( 'NONE', #24707, #66054, #10495, .T. ) ;
#27931 = CARTESIAN_POINT ( 'NONE',  ( 10.02201554968999986, 3.298015135926000152, 5.700522662207000657 ) ) ;
#27932 = CARTESIAN_POINT ( 'NONE',  ( 17.99965052394119169, -1.940731178328038098, -13.86484045969604395 ) ) ;
#27933 = CARTESIAN_POINT ( 'NONE',  ( 11.60948876160955479, 3.304472173606900043, 6.776679950459500112 ) ) ;
#27934 = CARTESIAN_POINT ( 'NONE',  ( 10.20319453770999907, -3.421758889707999796, 6.017729046583999875 ) ) ;
#27935 = DIRECTION ( 'NONE',  ( 0.000000000000000000, 1.000000000000000000, 0.000000000000000000 ) ) ;
#27936 = ORIENTED_EDGE ( 'NONE', *, *, #69052, .T. ) ;
#27937 = CARTESIAN_POINT ( 'NONE',  ( 24.41456973790700147, 12.00390065640000081, -3.256048965793000516 ) ) ;
#27939 = CARTESIAN_POINT ( 'NONE',  ( 9.978906853208000527, -5.007779786185999171, -8.772596342864998675 ) ) ;
#27938 = CARTESIAN_POINT ( 'NONE',  ( 12.05989062672900047, -12.07342271643000053, 3.473919584753000223 ) ) ;
#27940 = AXIS2_PLACEMENT_3D ( 'NONE', #65937, #6522, #38692 ) ;
#27941 = CARTESIAN_POINT ( 'NONE',  ( 7.746254512012610505, -5.449976221991329695, 8.461014486623254172 ) ) ;
#27942 = CARTESIAN_POINT ( 'NONE',  ( 10.89874164595999950, -2.834836218627000193, 9.088455567997000273 ) ) ;
#27943 = CARTESIAN_POINT ( 'NONE',  ( 11.83003632436370012, -5.243255406354000669, -7.209663534847899236 ) ) ;
#27944 = ORIENTED_EDGE ( 'NONE', *, *, #8194, .F. ) ;
#27945 = CARTESIAN_POINT ( 'NONE',  ( 24.00938322038199857, -9.351644529155782593, 9.262332192104681283 ) ) ;
#27946 = CARTESIAN_POINT ( 'NONE',  ( 10.67764828895399987, -2.998858038575999974, 6.953185708700699408 ) ) ;
#27947 = CARTESIAN_POINT ( 'NONE',  ( 7.654876518126000562, 2.928962009306002479, 6.518628166992000317 ) ) ;
#27948 = CARTESIAN_POINT ( 'NONE',  ( 10.96118313518939935, 3.207251432249800249, 6.497569908212999401 ) ) ;
#27949 = ORIENTED_EDGE ( 'NONE', *, *, #38538, .T. ) ;
#27950 = CARTESIAN_POINT ( 'NONE',  ( 9.717214158771000143, 3.990126737362999609, -8.809457313313998839 ) ) ;
#27951 = CARTESIAN_POINT ( 'NONE',  ( 23.61814130164600201, 13.16711982218999921, -4.271579012135999776 ) ) ;
#27952 = CARTESIAN_POINT ( 'NONE',  ( 12.47064909367909280, 3.118799700203781722, -12.20791227269315549 ) ) ;
#27953 = CARTESIAN_POINT ( 'NONE',  ( 12.10988784977536525, -4.851105903694400645, 7.548634759728509280 ) ) ;
#27954 = ADVANCED_FACE ( 'NONE', ( #63968 ), #37755, .T. ) ;
#27955 = VERTEX_POINT ( 'NONE', #48596 ) ;
#27956 = CARTESIAN_POINT ( 'NONE',  ( 9.085607419977296928, 5.315139263812436177, -7.853694237287989210 ) ) ;
#27958 = ADVANCED_FACE ( 'NONE', ( #31835 ), #279, .F. ) ;
#27957 = CARTESIAN_POINT ( 'NONE',  ( 11.09999999999999964, -6.519062740977999759, -5.524218123981000872 ) ) ;
#27959 = ORIENTED_EDGE ( 'NONE', *, *, #15309, .T. ) ;
#27960 = CARTESIAN_POINT ( 'NONE',  ( 23.56666365135700403, 12.07812737769999245, 3.551569042642998664 ) ) ;
#27961 = CARTESIAN_POINT ( 'NONE',  ( 23.97711684283312294, 9.403743244523731448, 9.292184203824568556 ) ) ;
#27962 = ORIENTED_EDGE ( 'NONE', *, *, #55487, .F. ) ;
#27963 = CARTESIAN_POINT ( 'NONE',  ( 10.03827017495050100, -2.603767608621661900, -8.557743501763278360 ) ) ;
#27964 = CARTESIAN_POINT ( 'NONE',  ( 10.30903300763299946, 4.597717337857299746, 6.873077781830399857 ) ) ;
#27965 = CARTESIAN_POINT ( 'NONE',  ( 11.08729972629000038, -2.258669075224000178, -7.034582301298999418 ) ) ;
#27966 = CARTESIAN_POINT ( 'NONE',  ( 10.79839886931999970, 5.269366011605000288, -6.148705891248999578 ) ) ;
#27967 = CARTESIAN_POINT ( 'NONE',  ( 10.39393020684999946, -5.250000000000000000, -7.500000000000000000 ) ) ;
#27968 = LINE ( 'NONE', #43359, #38606 ) ;
#27969 = DIRECTION ( 'NONE',  ( -1.000000000000000000, 0.000000000000000000, 0.000000000000000000 ) ) ;
#27970 = CARTESIAN_POINT ( 'NONE',  ( 17.84124069827833736, -0.5557204214162416722, -12.68363025601217053 ) ) ;
#27971 = CARTESIAN_POINT ( 'NONE',  ( 12.18009334795431187, 2.513081858645665356, -12.44854102044448929 ) ) ;
#27972 = CARTESIAN_POINT ( 'NONE',  ( 10.39918582084299992, -4.746348444722899629, -6.637298362509499228 ) ) ;
#27973 = CARTESIAN_POINT ( 'NONE',  ( 9.406704719590001318, 3.705846972803000128, 9.096435887808000942 ) ) ;
#27974 = ORIENTED_EDGE ( 'NONE', *, *, #51709, .T. ) ;
#27975 = SURFACE_SIDE_STYLE ('',( #49987 ) ) ;
#27976 = FACE_OUTER_BOUND ( 'NONE', #8650, .T. ) ;
#27977 = FACE_OUTER_BOUND ( 'NONE', #27585, .T. ) ;
#27978 = CARTESIAN_POINT ( 'NONE',  ( 11.53944595909000270, 12.46266292589999836, 1.587625155185000025 ) ) ;
#27979 = EDGE_CURVE ( 'NONE', #38102, #18184, #10840, .T. ) ;
#27980 = VECTOR ( 'NONE', #54933, 999.9999999999998863 ) ;
#27981 = CARTESIAN_POINT ( 'NONE',  ( 18.27407156835991131, 2.576234207239477492, 12.33383912514346470 ) ) ;
#27982 = DIRECTION ( 'NONE',  ( 1.000000000000000000, 0.000000000000000000, 0.000000000000000000 ) ) ;
#27983 = CARTESIAN_POINT ( 'NONE',  ( 10.58844943056000076, 3.754657019866000311, 5.545350295858999523 ) ) ;
#27984 = CARTESIAN_POINT ( 'NONE',  ( 10.66407857760462541, -4.737836169116369511, 7.029755324101339298 ) ) ;
#27985 = CARTESIAN_POINT ( 'NONE',  ( 12.80505043854144276, -0.7192913403693169672, -12.57945229203838267 ) ) ;
#27986 = EDGE_LOOP ( 'NONE', ( #50222, #57977, #13593, #655 ) ) ;
#27987 = CARTESIAN_POINT ( 'NONE',  ( 12.10343314470982179, -2.298052811141204188, 12.38866778002552849 ) ) ;
#27988 = CARTESIAN_POINT ( 'NONE',  ( 8.880265421554998539, -4.214287043487900064, -8.608472884860999486 ) ) ;
#27989 = CARTESIAN_POINT ( 'NONE',  ( 11.09999999999999964, 2.700000000000000178, 5.160242713806000303 ) ) ;
#27990 =( REPRESENTATION_RELATIONSHIP ('NONE','NONE', #10823, #30050 ) REPRESENTATION_RELATIONSHIP_WITH_TRANSFORMATION ( #21472 )SHAPE_REPRESENTATION_RELATIONSHIP( ) );
#27991 = AXIS2_PLACEMENT_3D ( 'NONE', #36345, #4862, #46500 ) ;
#27992 = CARTESIAN_POINT ( 'NONE',  ( 9.099999931440999390, 5.246365646610000155, 7.595250590283559866 ) ) ;
#27993 = B_SPLINE_SURFACE_WITH_KNOTS ( 'NONE', 3, 3, ( 
 ( #40597, #66471, #3868, #30128, #50404, #25202, #34681, #2504, #23828, #66127, #18247, #14037, #55995, #56685, #3528, #66822, #9120, #39569, #45166, #18935, #8784, #18595, #8099, #39921, #61240, #51092, #13355, #29443, #50749, #2846, #24174, #40259, #61579, #51431, #24863 ),
 ( #13695, #56339, #29790, #67502, #19619, #3195, #40941, #62262, #14383, #10494, #14720, #41974, #4902, #26243, #52110, #37076, #47571, #42659, #63967, #52809, #10839, #68876, #68184, #53150, #20993, #30797, #42329, #4213, #15748, #25551, #36035, #67843, #57351, #26590, #31834 ),
 ( #63631, #20302, #31485, #46876, #46537, #20648, #58387, #19965, #47223, #41628, #5586, #8, #5252, #47911, #21330, #62934, #16080, #37412, #63279, #36381, #58733, #41288, #62596, #15058, #32181, #53496, #9455, #15409, #57697, #9807, #31156, #68526, #52458, #36735, #58054 ),
 ( #4553, #25894, #10157, #16762, #49276, #33553, #27613, #17823, #12572, #59080, #48941, #27966, #60464, #38093, #33902, #11181, #11868, #65700, #55219, #26930, #32861, #39137, #48244, #37754, #1387, #54873, #6975, #22703, #38796, #59419, #53833, #697, #28303, #48595, #17471 ) ),
 .UNSPECIFIED., .F., .F., .F.,
 ( 4, 4 ),
 ( 4, 1, 1, 1, 1, 1, 1, 1, 1, 1, 1, 1, 1, 1, 1, 1, 1, 1, 1, 1, 1, 1, 1, 1, 1, 1, 1, 1, 1, 1, 1, 1, 4 ),
 ( -0.1039370721279000015, 1.103937072127999963 ),
 ( 0.1942321073450000157, 0.2199060843169000079, 0.2455800612886999967, 0.2712540382605999612, 0.2969280152323999777, 0.3226019922043000254, 0.3482759691761000420, 0.3739499461479999787, 0.3996239231197999953, 0.4252979000916999874, 0.4509718770635000040, 0.4766458540353999962, 0.5023198310072000128, 0.5279938079791000050, 0.5536677849509000771, 0.5793417619227999582, 0.6050157388945999193, 0.6306897158665000225, 0.6563636928382999836, 0.6820376698101999757, 0.7077116467820000478, 0.7333856237539000400, 0.7590596007256998901, 0.7847335776975999933, 0.8104075546693999543, 0.8360815316413000575, 0.8617555086131000186, 0.8874294855850000108, 0.9131034625568000829, 0.9387774395286999640, 0.9644514165004999251, 0.9901253934722999972, 1.015799370444000038 ),
 .UNSPECIFIED. ) ;
#27994 = CARTESIAN_POINT ( 'NONE',  ( 10.82179975933729921, 4.948878321068100661, -7.173532873542499466 ) ) ;
#27995 = CARTESIAN_POINT ( 'NONE',  ( 12.08123681970977259, 0.04734719685816674017, 12.59993264914401045 ) ) ;
#27996 = CARTESIAN_POINT ( 'NONE',  ( 8.919607780412000864, 5.165497731316000873, 8.645531386060000045 ) ) ;
#27997 = CARTESIAN_POINT ( 'NONE',  ( 10.40227026081000083, 2.765684886876999649, 9.035354958280999327 ) ) ;
#27998 = CARTESIAN_POINT ( 'NONE',  ( 12.49937493268693878, 3.045244672522429141, 12.30765407517399446 ) ) ;
#27999 = VERTEX_POINT ( 'NONE', #41975 ) ;
#28000 = CARTESIAN_POINT ( 'NONE',  ( 18.22725926605928848, -3.461153921119815902, -12.03746648326404589 ) ) ;
#28001 = CARTESIAN_POINT ( 'NONE',  ( 10.52226222744799955, 3.119510978356100139, -8.225278704382400718 ) ) ;
#28002 = CARTESIAN_POINT ( 'NONE',  ( 11.59999999999999964, 3.116215992411100366, 7.174999999999999822 ) ) ;
#28004 = CARTESIAN_POINT ( 'NONE',  ( 25.02478270113282832, 11.45587418384018896, 3.243239995978246526 ) ) ;
#28003 = CARTESIAN_POINT ( 'NONE',  ( 8.076862807906000086, 5.120521186033995420, 6.727223554611003742 ) ) ;
#28005 = CARTESIAN_POINT ( 'NONE',  ( 10.40749413291699987, -3.211956830789300277, -7.140435631538599281 ) ) ;
#28006 = CYLINDRICAL_SURFACE ( 'NONE', #49768, 0.5000000000000002220 ) ;
#28007 = ORIENTED_EDGE ( 'NONE', *, *, #55842, .F. ) ;
#28008 = CARTESIAN_POINT ( 'NONE',  ( 0.9192448634807000030, 3.532364098973999944, -0.6521526059094999717 ) ) ;
#28009 = CARTESIAN_POINT ( 'NONE',  ( 6.965816936038000229, -1.147328252452000097, 0.8605332073374000190 ) ) ;
#28010 = DIRECTION ( 'NONE',  ( 0.000000000000000000, 1.000000000000000000, 0.000000000000000000 ) ) ;
#28011 = CARTESIAN_POINT ( 'NONE',  ( 24.30001697352500045, -3.271769158411000245, -12.21048181092999840 ) ) ;
#28012 = EDGE_CURVE ( 'NONE', #27393, #52892, #42676, .T. ) ;
#28013 = ADVANCED_FACE ( 'NONE', ( #11518 ), #1721, .F. ) ;
#28014 = CARTESIAN_POINT ( 'NONE',  ( 11.37299956498129916, 2.792989229543000107, -7.174999999999999822 ) ) ;
#28015 = CARTESIAN_POINT ( 'NONE',  ( 12.56965099582940049, -1.826966356815477255, 13.88028256676999384 ) ) ;
#28016 = CARTESIAN_POINT ( 'NONE',  ( 3.799999782336999754, -2.725000000000000089, 0.000000000000000000 ) ) ;
#28017 = CARTESIAN_POINT ( 'NONE',  ( 24.21996587171000215, 3.760918895062999923, -12.77941170050999986 ) ) ;
#28018 = CARTESIAN_POINT ( 'NONE',  ( 23.59999176271200128, 13.22318677037999812, 4.267778497637999102 ) ) ;
#28019 = ORIENTED_EDGE ( 'NONE', *, *, #21432, .T. ) ;
#28020 = EDGE_CURVE ( 'NONE', #43628, #9687, #33779, .T. ) ;
#28021 = CARTESIAN_POINT ( 'NONE',  ( 7.000000000000000000, 8.307879248642999315, -4.307879248643000203 ) ) ;
#28022 = CARTESIAN_POINT ( 'NONE',  ( 12.73341324573692290, 11.23412379136182260, -3.084957477880623689 ) ) ;
#28023 = DIRECTION ( 'NONE',  ( 1.000000000000000000, 0.000000000000000000, 0.000000000000000000 ) ) ;
#28024 = DIRECTION ( 'NONE',  ( 0.000000000000000000, 1.000000000000000000, 0.000000000000000000 ) ) ;
#28025 = CARTESIAN_POINT ( 'NONE',  ( 1.180611034013999916, -1.296472565164999979, 3.528106597684999901 ) ) ;
#28026 = CARTESIAN_POINT ( 'NONE',  ( 1.823890132539666586, -2.150913519912200478, -2.798833948393631754 ) ) ;
#28027 = AXIS2_PLACEMENT_3D ( 'NONE', #10848, #10168, #361 ) ;
#28028 = CARTESIAN_POINT ( 'NONE',  ( 17.66882634972349209, 1.885356762137523345, -12.57375482825836777 ) ) ;
#28029 = CARTESIAN_POINT ( 'NONE',  ( 9.792569055495000896, 3.463432304708999876, 6.184396499233999478 ) ) ;
#28030 = CARTESIAN_POINT ( 'NONE',  ( 11.66287348028854964, 3.238044298475899918, 7.088026579158399620 ) ) ;
#28031 = CARTESIAN_POINT ( 'NONE',  ( 8.906851002547000462, 2.832432432432000269, -6.822293592207000934 ) ) ;
#28032 = CARTESIAN_POINT ( 'NONE',  ( 10.39539435320999949, -5.667179153637999178, -7.250689665673000661 ) ) ;
#28033 = CARTESIAN_POINT ( 'NONE',  ( 11.16544712921906957, 3.267598948716616825, -7.982093405445620959 ) ) ;
#28034 = PLANE ( 'NONE',  #29919 ) ;
#28035 = DIRECTION ( 'NONE',  ( -1.901299611514599864E-27, -1.000000000000000000, 3.733732073519000081E-14 ) ) ;
#28036 = ORIENTED_EDGE ( 'NONE', *, *, #42391, .T. ) ;
#28037 = CARTESIAN_POINT ( 'NONE',  ( 21.10000000000000142, -11.84999999999999964, 0.000000000000000000 ) ) ;
#28038 = ORIENTED_EDGE ( 'NONE', *, *, #55257, .T. ) ;
#28039 = CARTESIAN_POINT ( 'NONE',  ( 18.12467946932838814, -2.757395321821673129, 13.61549383066600782 ) ) ;
#28040 = CARTESIAN_POINT ( 'NONE',  ( 10.22272469555899832, -3.360453478306600239, -6.393520617113999549 ) ) ;
#28041 = VERTEX_POINT ( 'NONE', #27967 ) ;
#28042 = CARTESIAN_POINT ( 'NONE',  ( 11.31900581613029821, 4.750686773407899466, 7.017964743997199939 ) ) ;
#28043 = CARTESIAN_POINT ( 'NONE',  ( 6.665529626493635895, 0.5345806894169679024, 0.9988415717975688279 ) ) ;
#28044 = CARTESIAN_POINT ( 'NONE',  ( 24.12729511379000513, 3.330893262555046697, -12.51461353060619786 ) ) ;
#28045 = DIRECTION ( 'NONE',  ( 0.000000000000000000, 1.000000000000000000, 0.000000000000000000 ) ) ;
#28046 = CARTESIAN_POINT ( 'NONE',  ( 12.61577834527631303, -1.811481987162395724, -13.88231333970466608 ) ) ;
#28047 = DIRECTION ( 'NONE',  ( 0.000000000000000000, 0.9565994702956990281, -0.2914059941558995726 ) ) ;
#28048 = CARTESIAN_POINT ( 'NONE',  ( 17.87583791501561237, 0.6451567829544448962, -12.58347320810647929 ) ) ;
#28049 = CARTESIAN_POINT ( 'NONE',  ( 10.35427551197999918, -4.879111827962000270, -8.944027914303999793 ) ) ;
#28050 = DIRECTION ( 'NONE',  ( 1.000000000000000000, 0.000000000000000000, 0.000000000000000000 ) ) ;
#28051 = ORIENTED_EDGE ( 'NONE', *, *, #26072, .T. ) ;
#28052 = CARTESIAN_POINT ( 'NONE',  ( 10.90453766415000025, -2.900310535872000273, -5.130381900875999435 ) ) ;
#28053 = ORIENTED_EDGE ( 'NONE', *, *, #26635, .T. ) ;
#28054 = CARTESIAN_POINT ( 'NONE',  ( 8.896714042595457173, 3.863849893574820893, -6.453285899984952501 ) ) ;
#28055 = VERTEX_POINT ( 'NONE', #55915 ) ;
#28056 = CARTESIAN_POINT ( 'NONE',  ( 10.83581759994134863, 2.987285522957833894, -4.871130536556726121 ) ) ;
#28057 = CARTESIAN_POINT ( 'NONE',  ( 10.42861756900999914, -5.068632498314999069, 4.618459570084000099 ) ) ;
#28058 = EDGE_CURVE ( 'NONE', #19641, #16280, #35986, .T. ) ;
#28059 = CARTESIAN_POINT ( 'NONE',  ( 10.27427156480999848, -3.399999787207999447, 4.944156960757000618 ) ) ;
#28060 = CARTESIAN_POINT ( 'NONE',  ( 9.099999999999999645, 0.000000000000000000, 0.000000000000000000 ) ) ;
#28061 = CARTESIAN_POINT ( 'NONE',  ( 12.21287994455106229, 2.700912243963291992, 13.62875716402589532 ) ) ;
#28062 = CARTESIAN_POINT ( 'NONE',  ( 17.69913221809301263, -1.891485217175129963, 12.57274297139331587 ) ) ;
#28063 = EDGE_CURVE ( 'NONE', #51958, #53568, #65353, .T. ) ;
#28064 = CARTESIAN_POINT ( 'NONE',  ( 11.28192504596561996, 4.908977993420656105, -7.825000185715046186 ) ) ;
#28065 = CARTESIAN_POINT ( 'NONE',  ( 12.23548570231569066, 0.2575405707509094144, 13.89679341043304994 ) ) ;
#28066 = ORIENTED_EDGE ( 'NONE', *, *, #32798, .T. ) ;
#28067 = CARTESIAN_POINT ( 'NONE',  ( 12.67430611818100061, 11.44505085583999993, -4.692779640757001047 ) ) ;
#28068 = CARTESIAN_POINT ( 'NONE',  ( 13.56663524094155804, -11.53596571847203300, -2.401556225329832817 ) ) ;
#28069 = FACE_BOUND ( 'NONE', #50662, .T. ) ;
#28070 = CARTESIAN_POINT ( 'NONE',  ( 4.981119878958000236, 0.2975160469921999673, -1.149139654934000054 ) ) ;
#28071 = CARTESIAN_POINT ( 'NONE',  ( 10.12339528040999959, 3.988943694240999704, -8.966360307350999648 ) ) ;
#28072 = CARTESIAN_POINT ( 'NONE',  ( 9.843930206850000530, 2.750000000000000000, -7.500000000000000000 ) ) ;
#28073 = CARTESIAN_POINT ( 'NONE',  ( 10.51140025105000042, -2.326718149302000160, -7.741209600718000239 ) ) ;
#28074 = DIRECTION ( 'NONE',  ( 0.000000000000000000, 2.657874803301998965E-08, -0.9999999999999996669 ) ) ;
#28075 = AXIS2_PLACEMENT_3D ( 'NONE', #54266, #17212, #59170 ) ;
#28076 = CARTESIAN_POINT ( 'NONE',  ( 18.30008632280270930, 2.887848135250621385E-14, -11.85014035451981762 ) ) ;
#28077 = CARTESIAN_POINT ( 'NONE',  ( 10.87751262143000019, -2.899999999999999911, 6.466455373849333554 ) ) ;
#28078 = CARTESIAN_POINT ( 'NONE',  ( 18.20318779774994056, -2.896782429227412692, 13.69773569391997547 ) ) ;
#28079 = FACE_OUTER_BOUND ( 'NONE', #25506, .T. ) ;
#28080 = CARTESIAN_POINT ( 'NONE',  ( 12.61731147765582328, 0.6963438834333895988, 12.58074676375310474 ) ) ;
#28081 = CARTESIAN_POINT ( 'NONE',  ( 10.64902344389989963, 3.116469856398800253, -6.963800219468099684 ) ) ;
#28082 = CARTESIAN_POINT ( 'NONE',  ( 10.11591290906799934, 3.364470222553300083, -8.277781595084700683 ) ) ;
#28084 = DIRECTION ( 'NONE',  ( 0.000000000000000000, 1.000000000000000000, 0.000000000000000000 ) ) ;
#28083 = CARTESIAN_POINT ( 'NONE',  ( 9.369809814040999996, -3.385590752329799891, 6.705428891605899722 ) ) ;
#28085 = CARTESIAN_POINT ( 'NONE',  ( 9.317462135714000837, -5.100000000000000533, 6.571291218949999902 ) ) ;
#28086 = ORIENTED_EDGE ( 'NONE', *, *, #19487, .T. ) ;
#28087 = CARTESIAN_POINT ( 'NONE',  ( 10.37199293566600034, 4.633387186021100668, 6.723009541442299231 ) ) ;
#28088 = CARTESIAN_POINT ( 'NONE',  ( 11.02286109245999945, -2.398753588646000079, 6.352476128646999065 ) ) ;
#28089 = CARTESIAN_POINT ( 'NONE',  ( 10.39157120343299923, 3.944651031655580287, 6.359530327585999565 ) ) ;
#28090 = CARTESIAN_POINT ( 'NONE',  ( 9.581508192411627434, 3.220001783077621305, -7.103597363128174358 ) ) ;
#28091 = ADVANCED_FACE ( 'NONE', ( #12227 ), #25114, .F. ) ;
#28092 = CARTESIAN_POINT ( 'NONE',  ( 10.19256470245000123, -2.560274838243000062, 7.664550593243999899 ) ) ;
#28093 = CARTESIAN_POINT ( 'NONE',  ( 9.629471092178999214, -5.100000000000000533, 6.152188490330000370 ) ) ;
#28094 = CARTESIAN_POINT ( 'NONE',  ( 12.10000000000000142, -43.96540072520999587, 14.96704326274999985 ) ) ;
#28095 = EDGE_LOOP ( 'NONE', ( #35413, #47145, #61489, #3367 ) ) ;
#28096 = ADVANCED_FACE ( 'NONE', ( #13955 ), #6624, .F. ) ;
#28097 = EDGE_CURVE ( 'NONE', #67407, #55115, #16782, .T. ) ;
#28098 = CARTESIAN_POINT ( 'NONE',  ( 9.584000818238999742, -4.888721525563999748, -7.967991827203400490 ) ) ;
#28099 = LINE ( 'NONE', #9512, #43275 ) ;
#28100 = CARTESIAN_POINT ( 'NONE',  ( 6.276421824150999917, 0.9869232226998000401, -1.278013103562000152 ) ) ;
#28101 = CARTESIAN_POINT ( 'NONE',  ( 10.42581074856899725, -5.172583146916751140, 6.999756549658379789 ) ) ;
#28102 = CARTESIAN_POINT ( 'NONE',  ( 24.30001680216799897, -3.271769318036999774, 12.21048166890999909 ) ) ;
#28103 = CARTESIAN_POINT ( 'NONE',  ( 13.50018479229797208, -11.40740214419244225, -3.347185923349857095 ) ) ;
#28104 = CARTESIAN_POINT ( 'NONE',  ( 11.16641369783139837, 3.949373449607799902, -8.502191501283999031 ) ) ;
#28105 = CARTESIAN_POINT ( 'NONE',  ( 12.21215155063535640, 2.301234877171830284, -13.71362569327517100 ) ) ;
#28106 = CARTESIAN_POINT ( 'NONE',  ( 25.41677598325400211, -8.397334373648000394, 8.092712133474000424 ) ) ;
#28107 = CARTESIAN_POINT ( 'NONE',  ( 10.62947109217999930, 5.100000000000000533, 6.152188490330000370 ) ) ;
#28108 = ORIENTED_EDGE ( 'NONE', *, *, #34465, .T. ) ;
#28109 = CARTESIAN_POINT ( 'NONE',  ( 7.496528476645853090, -5.315361133063865928, 7.854106854282135508 ) ) ;
#28110 = CARTESIAN_POINT ( 'NONE',  ( 12.41655229043184860, 0.4896942981276207196, -13.88839019180475809 ) ) ;
#28111 = CARTESIAN_POINT ( 'NONE',  ( 8.191498566858999908, 3.399962487441000381, 6.146646668338000552 ) ) ;
#28112 = CARTESIAN_POINT ( 'NONE',  ( 2.266329616852750473, -3.450786940248410151, -0.6753594422426504318 ) ) ;
#28113 = EDGE_CURVE ( 'NONE', #1557, #15559, #66736, .T. ) ;
#28114 = DIRECTION ( 'NONE',  ( 1.000000000000000000, 0.000000000000000000, 0.000000000000000000 ) ) ;
#28115 = CARTESIAN_POINT ( 'NONE',  ( 8.099999999999999645, 0.000000000000000000, 0.000000000000000000 ) ) ;
#28116 = LINE ( 'NONE', #50470, #532 ) ;
#28117 = ORIENTED_EDGE ( 'NONE', *, *, #29901, .F. ) ;
#28118 =( NAMED_UNIT ( * ) PLANE_ANGLE_UNIT ( ) SI_UNIT ( $, .RADIAN. ) );
#28119 = CARTESIAN_POINT ( 'NONE',  ( 17.71798387292786003, 1.896258650311507310, -13.78312406285443004 ) ) ;
#28120 = ORIENTED_EDGE ( 'NONE', *, *, #39785, .T. ) ;
#28121 = LINE ( 'NONE', #45242, #4917 ) ;
#28122 = CARTESIAN_POINT ( 'NONE',  ( 11.09999999999999964, 6.593648130222000248, -5.598803514566000672 ) ) ;
#28123 = CARTESIAN_POINT ( 'NONE',  ( 9.410004719593999312, 2.495531372253999791, -7.930944806125000746 ) ) ;
#28124 = CARTESIAN_POINT ( 'NONE',  ( 6.487553283437998530, -0.1491724392751367367, 1.524878087010347993 ) ) ;
#28125 = CARTESIAN_POINT ( 'NONE',  ( 17.65064139367255436, 1.793792787906293595, -13.88460705996369704 ) ) ;
#28126 = CARTESIAN_POINT ( 'NONE',  ( 11.00000000000000000, 2.941427501403999667, -7.825000000000000178 ) ) ;
#28127 = CARTESIAN_POINT ( 'NONE',  ( 10.26059687351567007, -4.629523725463621453, -6.407767014557177454 ) ) ;
#28128 = CARTESIAN_POINT ( 'NONE',  ( 4.599999999999999645, 1.760910691117812954, 12.47634535983622861 ) ) ;
#28129 = ORIENTED_EDGE ( 'NONE', *, *, #18810, .F. ) ;
#28130 = CARTESIAN_POINT ( 'NONE',  ( 9.758146639703001668, -2.901368778958000050, 6.555068849476000103 ) ) ;
#28131 = CARTESIAN_POINT ( 'NONE',  ( 18.14649830798774843, -2.702104747124480344, -13.62846271472191262 ) ) ;
#28132 = DIRECTION ( 'NONE',  ( 0.8660254037844288266, 0.000000000000000000, 0.5000000000000169864 ) ) ;
#28133 = ORIENTED_EDGE ( 'NONE', *, *, #55169, .T. ) ;
#28134 = AXIS2_PLACEMENT_3D ( 'NONE', #63740, #64417, #53259 ) ;
#28135 = CARTESIAN_POINT ( 'NONE',  ( 9.780284676292000157, 3.021596928575999819, -8.450035627617001666 ) ) ;
#28136 = LINE ( 'NONE', #27104, #55465 ) ;
#28137 = VERTEX_POINT ( 'NONE', #42576 ) ;
#28138 = CARTESIAN_POINT ( 'NONE',  ( 9.710646554150999421, 4.486270025758400060, 6.621146336197599958 ) ) ;
#28139 = CARTESIAN_POINT ( 'NONE',  ( 18.24176189833876194, -2.711585165818146681, -12.30477270241628496 ) ) ;
#28140 = AXIS2_PLACEMENT_3D ( 'NONE', #24694, #46017, #55479 ) ;
#28141 = CARTESIAN_POINT ( 'NONE',  ( 9.591846873515667227, 4.999583552997727054, 6.731816600031356401 ) ) ;
#28142 = CARTESIAN_POINT ( 'NONE',  ( 15.86268444654400156, 3.728894906265999509, 11.70612128528000007 ) ) ;
#28143 = CARTESIAN_POINT ( 'NONE',  ( 11.30000000000000071, 3.738146901528993205, -11.41167910143314579 ) ) ;
#28144 = EDGE_CURVE ( 'NONE', #64677, #23593, #13471, .T. ) ;
#28145 = CARTESIAN_POINT ( 'NONE',  ( 10.14124205625000030, 3.639798001706899822, 6.562398383267799673 ) ) ;
#28146 = CARTESIAN_POINT ( 'NONE',  ( 8.057875016312998184, -4.641725571029997610, 6.225038937488997171 ) ) ;
#28147 = ORIENTED_EDGE ( 'NONE', *, *, #49221, .F. ) ;
#28148 = CARTESIAN_POINT ( 'NONE',  ( 8.267706852541074625, -5.045576645684537453, 6.407495147014386383 ) ) ;
#28149 = CARTESIAN_POINT ( 'NONE',  ( 10.39539221959000059, 5.667182949051000840, -7.250689098107000241 ) ) ;
#28150 = DIRECTION ( 'NONE',  ( 0.000000000000000000, 0.7071067811865475727, 0.7071067811865475727 ) ) ;
#28151 = CARTESIAN_POINT ( 'NONE',  ( 12.30838305349008444, 2.879539296179473684, -13.58560287457177473 ) ) ;
#28152 = DIRECTION ( 'NONE',  ( -0.9999999999999997780, -1.366956391494999762E-09, 2.239632587909999191E-08 ) ) ;
#28153 = CARTESIAN_POINT ( 'NONE',  ( 25.08242994833700124, 2.794105277247000085, 11.47833782540000058 ) ) ;
#28154 = CARTESIAN_POINT ( 'NONE',  ( 17.98240304306455428, 0.4561791668615490236, 13.88992602861185155 ) ) ;
#28155 = CARTESIAN_POINT ( 'NONE',  ( 24.56892027611100460, -3.303734510344000341, 12.00214753008000024 ) ) ;
#28156 = VERTEX_POINT ( 'NONE', #32437 ) ;
#28157 = ORIENTED_EDGE ( 'NONE', *, *, #26269, .F. ) ;
#28158 = CARTESIAN_POINT ( 'NONE',  ( 9.833904719592002408, 5.048004622677000341, -6.120508709481000231 ) ) ;
#28159 = CARTESIAN_POINT ( 'NONE',  ( 12.28049946560828865, -0.3399327000516478847, 13.89440849577454351 ) ) ;
#28160 = CARTESIAN_POINT ( 'NONE',  ( 10.74733997688000109, -3.727636250918499705, 8.748653021963999521 ) ) ;
#28161 = CARTESIAN_POINT ( 'NONE',  ( 10.68904248846000016, -2.568964727443000307, 7.728094434513999467 ) ) ;
#28162 = CARTESIAN_POINT ( 'NONE',  ( 23.60707278462106373, 3.266495719822134713, -13.58453502575737026 ) ) ;
#28163 = CARTESIAN_POINT ( 'NONE',  ( 8.411456853209999807, -3.882020254083999866, 5.870054788755000530 ) ) ;
#28164 = CARTESIAN_POINT ( 'NONE',  ( 23.58334011193800350, 0.000000000000000000, -3.819167204710999951E-13 ) ) ;
#28166 = CARTESIAN_POINT ( 'NONE',  ( 8.620740978634000129, 4.599999999999999645, 5.898823289756999877 ) ) ;
#28165 = CARTESIAN_POINT ( 'NONE',  ( 9.880417874594000338, -5.177249570814000279, 6.999532383170999239 ) ) ;
#28167 = FACE_OUTER_BOUND ( 'NONE', #27916, .T. ) ;
#28168 = CIRCLE ( 'NONE', #3553, 13.17499999999999716 ) ;
#28169 = CARTESIAN_POINT ( 'NONE',  ( 12.09999999999999964, -3.890364666909557734, 6.362414725044391872 ) ) ;
#28170 = CARTESIAN_POINT ( 'NONE',  ( 8.742477372938900260, 2.899999999999999467, -6.356265660156537045 ) ) ;
#28171 = CARTESIAN_POINT ( 'NONE',  ( 17.78508576848220812, 0.5812174491462176462, 12.68209204657792810 ) ) ;
#28172 = B_SPLINE_CURVE_WITH_KNOTS ( 'NONE', 3,
 ( #34865, #50941, #54802, #3037 ),
 .UNSPECIFIED., .F., .F.,
 ( 4, 4 ),
 ( 0.000000000000000000, 1.000000000000000000 ),
 .UNSPECIFIED. ) ;
#28173 = CARTESIAN_POINT ( 'NONE',  ( 6.570873790634999878, -1.458001084847000195, 0.5398711174489000397 ) ) ;
#28174 = CARTESIAN_POINT ( 'NONE',  ( 17.71871529295699332, -3.104542143066329363, -12.28994062198766457 ) ) ;
#28175 = VERTEX_POINT ( 'NONE', #21584 ) ;
#28177 = CARTESIAN_POINT ( 'NONE',  ( 18.22958240948263509, 10.92137759501686034, -4.055351289589740560 ) ) ;
#28176 = CARTESIAN_POINT ( 'NONE',  ( 10.88314899746000108, 5.167567567567999731, 6.822293592207000934 ) ) ;
#28178 = CARTESIAN_POINT ( 'NONE',  ( 8.614404719593999005, 5.030502105212999453, -6.322203460290999999 ) ) ;
#28179 = EDGE_CURVE ( 'NONE', #11948, #61432, #10067, .T. ) ;
#28180 = CARTESIAN_POINT ( 'NONE',  ( 8.568197172116430949, 5.125396288428779812, -6.749639981086953178 ) ) ;
#28181 = CARTESIAN_POINT ( 'NONE',  ( 10.21160513988073149, -3.634030556546635093, -8.817876221680798210 ) ) ;
#28182 = CIRCLE ( 'NONE', #15891, 12.50000000000000000 ) ;
#28183 = CARTESIAN_POINT ( 'NONE',  ( 0.4611081069563000012, 3.330914467393999878, 1.191613524625000142 ) ) ;
#28184 = CARTESIAN_POINT ( 'NONE',  ( 9.520528907821001141, 2.899999999999999911, 6.152188490330000370 ) ) ;
#28185 = CIRCLE ( 'NONE', #67250, 2.700000000000000178 ) ;
#28186 = CARTESIAN_POINT ( 'NONE',  ( 3.410659130938999972, 0.3807847720749999998, -3.739296779731999809 ) ) ;
#28187 = ORIENTED_EDGE ( 'NONE', *, *, #58349, .T. ) ;
#28188 = CARTESIAN_POINT ( 'NONE',  ( 12.18894565086184478, 0.3798658283128608093, -12.59428767283705497 ) ) ;
#28189 = CARTESIAN_POINT ( 'NONE',  ( 10.88210843320517007, -5.137688304401064165, -8.098394516494941797 ) ) ;
#28190 = CARTESIAN_POINT ( 'NONE',  ( 24.14113398102592711, -12.48039438772169873, -3.363020802264193421 ) ) ;
#28191 = CARTESIAN_POINT ( 'NONE',  ( 7.256079719589999755, 2.531201476950000195, 8.216704145297999418 ) ) ;
#28192 = EDGE_LOOP ( 'NONE', ( #50544, #3822, #14159, #35773, #35123 ) ) ;
#28193 = CARTESIAN_POINT ( 'NONE',  ( 6.939945356251999264, -0.08083205921694999740, 1.612735633780000066 ) ) ;
#28194 = CARTESIAN_POINT ( 'NONE',  ( 10.91281150458596727, 9.717878385093197124, 5.838659047851286310 ) ) ;
#28195 = ADVANCED_FACE ( 'NONE', ( #63885 ), #64573, .F. ) ;
#28197 = CARTESIAN_POINT ( 'NONE',  ( 9.096071945540000314, -5.102479135096000817, -6.621020973615999061 ) ) ;
#28196 = CARTESIAN_POINT ( 'NONE',  ( 3.800000448357999883, 0.000000000000000000, 0.000000000000000000 ) ) ;
#28198 = CARTESIAN_POINT ( 'NONE',  ( 11.13746005378019888, 5.161099018038999731, -6.879992063401499713 ) ) ;
#28199 = ORIENTED_EDGE ( 'NONE', *, *, #67100, .T. ) ;
#28200 = CARTESIAN_POINT ( 'NONE',  ( 5.000000000000000000, 0.05000000000000000278, 9.776630298829998011 ) ) ;
#28201 = CARTESIAN_POINT ( 'NONE',  ( 12.79999999202000005, -11.41069016990000051, 4.623987642516999230 ) ) ;
#28202 = ORIENTED_EDGE ( 'NONE', *, *, #3173, .T. ) ;
#28203 = EDGE_CURVE ( 'NONE', #23594, #34256, #54307, .T. ) ;
#28204 = CARTESIAN_POINT ( 'NONE',  ( 9.957462135714001406, -5.100000000000000533, -6.571291218949999902 ) ) ;
#28205 = CARTESIAN_POINT ( 'NONE',  ( 16.13862479881500178, 3.581551568669000041, 11.04584923442999944 ) ) ;
#28206 = CARTESIAN_POINT ( 'NONE',  ( 18.08024975107899479, -0.3389646381316551715, -13.89444110642640773 ) ) ;
#28207 = VERTEX_POINT ( 'NONE', #25805 ) ;
#28208 = DIRECTION ( 'NONE',  ( 0.000000000000000000, 1.000000000000000000, 0.000000000000000000 ) ) ;
#28209 = CARTESIAN_POINT ( 'NONE',  ( 5.500000000000000000, 11.95749337870000062, -3.642574926948999980 ) ) ;
#28210 = CARTESIAN_POINT ( 'NONE',  ( 23.66004879239100234, -13.39256420742000131, 3.813548264891000183 ) ) ;
#28211 = CARTESIAN_POINT ( 'NONE',  ( 10.90000000011000125, -5.100000000110999743, 6.571291220762999430 ) ) ;
#28212 = CARTESIAN_POINT ( 'NONE',  ( 0.4529763571839853786, 3.676114825633475335E-06, -3.452897576335808072 ) ) ;
#28213 = EDGE_LOOP ( 'NONE', ( #26334, #49268, #67851, #40176, #59152 ) ) ;
#28214 = DIRECTION ( 'NONE',  ( 0.7071060865235063719, 0.7071074758489063194, 8.142185728694072879E-10 ) ) ;
#28215 = CARTESIAN_POINT ( 'NONE',  ( 12.33523313523883580, -2.912685155760744049, -13.57718188376844282 ) ) ;
#28216 = B_SPLINE_CURVE_WITH_KNOTS ( 'NONE', 3,
 ( #56017, #41316, #4239, #30827 ),
 .UNSPECIFIED., .F., .F.,
 ( 4, 4 ),
 ( 0.000000000000000000, 1.000000000000000000 ),
 .UNSPECIFIED. ) ;
#28217 = CARTESIAN_POINT ( 'NONE',  ( 9.216839207166819037, -3.231820996160964743, -6.500433908363888236 ) ) ;
#28218 = CONICAL_SURFACE ( 'NONE', #38230, 1.600003888856000200, 0.7854004771980920285 ) ;
#28219 = CARTESIAN_POINT ( 'NONE',  ( 16.13682146000800088, -8.990085112443999549, -8.775549782916998609 ) ) ;
#28220 = EDGE_LOOP ( 'NONE', ( #25098, #41263, #53099, #52000 ) ) ;
#28221 = FACE_OUTER_BOUND ( 'NONE', #29875, .T. ) ;
#28222 = CYLINDRICAL_SURFACE ( 'NONE', #17625, 1.500000000000000000 ) ;
#28223 = CARTESIAN_POINT ( 'NONE',  ( 11.09999999999999964, 4.000000000000000000, -7.500000000000000000 ) ) ;
#28224 = CARTESIAN_POINT ( 'NONE',  ( 5.000030787343000327, 2.099962892531006098, 0.2748844998327708011 ) ) ;
#28225 = CARTESIAN_POINT ( 'NONE',  ( 12.80505043854143388, 1.875000000000000000, -12.57545641911172751 ) ) ;
#28226 = CARTESIAN_POINT ( 'NONE',  ( 11.01872200990539952, -4.947480442174099657, -7.169497859994799605 ) ) ;
#28227 = CARTESIAN_POINT ( 'NONE',  ( 10.50333291544900050, 4.531093146757585899, 6.341063066638221279 ) ) ;
#28228 = CARTESIAN_POINT ( 'NONE',  ( 17.56715138999752313, -1.760845446529460512, 12.47635456592353620 ) ) ;
#28229 = ORIENTED_EDGE ( 'NONE', *, *, #60785, .T. ) ;
#28230 = CARTESIAN_POINT ( 'NONE',  ( 11.42834208742529967, -4.706521750018099581, -8.610579932818998472 ) ) ;
#28231 = VERTEX_POINT ( 'NONE', #36992 ) ;
#28232 = AXIS2_PLACEMENT_3D ( 'NONE', #48151, #32423, #22262 ) ;
#28233 = CARTESIAN_POINT ( 'NONE',  ( 11.35194613850999978, -12.28618680900000015, -1.513058913260000082 ) ) ;
#28234 = CARTESIAN_POINT ( 'NONE',  ( 9.146614158775999925, 2.981992329588000423, -5.895876591910999664 ) ) ;
#28235 = CARTESIAN_POINT ( 'NONE',  ( 3.488436892060000183, -3.068566966923000017, 0.5458777553189999576 ) ) ;
#28236 = CARTESIAN_POINT ( 'NONE',  ( 10.99693800072000016, -2.980603239157999962, -6.418614998350999912 ) ) ;
#28237 = CARTESIAN_POINT ( 'NONE',  ( 6.654170804923853488, -1.238391233191631802, -0.8776529624291122822 ) ) ;
#28238 = CARTESIAN_POINT ( 'NONE',  ( 24.08683856445600213, 12.68564027046999954, 3.367487813839999955 ) ) ;
#28239 = CARTESIAN_POINT ( 'NONE',  ( 10.90000000000000036, -4.000000000000000000, -7.500000000000000000 ) ) ;
#28240 = ORIENTED_EDGE ( 'NONE', *, *, #15162, .F. ) ;
#28241 = CARTESIAN_POINT ( 'NONE',  ( 1.946856900172333704, 0.9112004763889643977, -3.396138185504796958 ) ) ;
#28242 = CARTESIAN_POINT ( 'NONE',  ( 11.07564694612699974, -4.931992688388300294, 7.128058497017000228 ) ) ;
#28243 = CARTESIAN_POINT ( 'NONE',  ( 9.753142190738998352, 4.104977339646000090, 9.293283246364000050 ) ) ;
#28244 = CARTESIAN_POINT ( 'NONE',  ( 10.31905590579000176, -2.899999999999999911, -6.571291218949999902 ) ) ;
#28245 = LINE ( 'NONE', #43987, #67772 ) ;
#28246 = CARTESIAN_POINT ( 'NONE',  ( 25.60000000000000142, 2.258942858049999725, 10.99401502705231515 ) ) ;
#28247 = CARTESIAN_POINT ( 'NONE',  ( 11.33872066707849768, 4.858611803369300652, -6.980638253271099103 ) ) ;
#28248 = DIRECTION ( 'NONE',  ( -1.000000000000000000, 0.000000000000000000, 0.000000000000000000 ) ) ;
#28249 = CARTESIAN_POINT ( 'NONE',  ( 9.429063610504998749, 4.468346739194200445, -8.541338455964998744 ) ) ;
#28250 = CARTESIAN_POINT ( 'NONE',  ( 24.57033794412999939, -8.854779233076000011, -9.403977091059999793 ) ) ;
#28251 = CARTESIAN_POINT ( 'NONE',  ( 23.55653128217999992, -10.23594516573000135, 9.677208546218999174 ) ) ;
#28252 = CARTESIAN_POINT ( 'NONE',  ( 11.80756411264299999, -3.251511910489000012, 11.33753290789000090 ) ) ;
#28253 = ORIENTED_EDGE ( 'NONE', *, *, #52979, .T. ) ;
#28254 = CARTESIAN_POINT ( 'NONE',  ( 7.758191940376999440, -5.797088532631000213, 8.340479314546998424 ) ) ;
#28255 = CARTESIAN_POINT ( 'NONE',  ( 9.573145925901000552, -2.133039813254999917, -7.346564890486999566 ) ) ;
#28256 = ADVANCED_FACE ( 'NONE', ( #5167 ), #37671, .F. ) ;
#28257 = ADVANCED_FACE ( 'NONE', ( #617 ), #54395, .F. ) ;
#28258 = CARTESIAN_POINT ( 'NONE',  ( 18.01266241223991216, 2.926178784092880569, 13.57373383468747363 ) ) ;
#28259 = CARTESIAN_POINT ( 'NONE',  ( 15.90018573812067970, -7.829696748392007244, -8.945859267997793296 ) ) ;
#28260 = CARTESIAN_POINT ( 'NONE',  ( 10.17764828895399809, -2.998858038575999974, -8.046814291299300592 ) ) ;
#28261 = ORIENTED_EDGE ( 'NONE', *, *, #20266, .F. ) ;
#28262 = CIRCLE ( 'NONE', #18189, 1.625000000000000000 ) ;
#28263 = CARTESIAN_POINT ( 'NONE',  ( 25.31133064153000234, 2.728868305775999925, -11.35932564715999860 ) ) ;
#28264 = CARTESIAN_POINT ( 'NONE',  ( 7.667607780408999929, 5.638704226117999596, 8.266404648244000342 ) ) ;
#28266 = CARTESIAN_POINT ( 'NONE',  ( 9.219914745407999490, -4.065337473341759988, 6.596431033727998994 ) ) ;
#28265 = CARTESIAN_POINT ( 'NONE',  ( 9.093935841232999806, 2.156584729807999867, -7.959751745006000689 ) ) ;
#28267 = CARTESIAN_POINT ( 'NONE',  ( 11.02418915877000138, 2.407889430138999920, -8.439554272735000140 ) ) ;
#28268 = ORIENTED_EDGE ( 'NONE', *, *, #15501, .F. ) ;
#28269 = CARTESIAN_POINT ( 'NONE',  ( 10.63461554336999981, 5.668731883089999535, 6.527253515312000154 ) ) ;
#28270 = CARTESIAN_POINT ( 'NONE',  ( 18.28009623694103070, -2.497067955185374277, -13.77553007214568481 ) ) ;
#28271 = CARTESIAN_POINT ( 'NONE',  ( 11.63410404293056999, 3.557672215630899970, 6.599279737936000423 ) ) ;
#28272 = CARTESIAN_POINT ( 'NONE',  ( 9.945535518573000999, -2.906050966242999856, 8.880386511481999534 ) ) ;
#28273 = CARTESIAN_POINT ( 'NONE',  ( 8.834370559623998531, -4.141908960411000429, 6.047561724438000219 ) ) ;
#28274 = ORIENTED_EDGE ( 'NONE', *, *, #25918, .T. ) ;
#28275 = CARTESIAN_POINT ( 'NONE',  ( 24.35145719007200071, 12.30648751194999946, -3.205655321895999776 ) ) ;
#28277 = CARTESIAN_POINT ( 'NONE',  ( 10.96333185321000059, -5.283547384770999500, -8.592770849731000027 ) ) ;
#28276 = CARTESIAN_POINT ( 'NONE',  ( 12.04183425709900135, -11.69157926155999938, 4.070931047779999368 ) ) ;
#28278 = CARTESIAN_POINT ( 'NONE',  ( 8.089012611369920336, -4.321942129502657437, 5.789925683486281116 ) ) ;
#28279 = AXIS2_PLACEMENT_3D ( 'NONE', #23309, #18069, #12472 ) ;
#28280 = CARTESIAN_POINT ( 'NONE',  ( 9.533427734455999669, -2.564762519363000148, 6.150594768287000136 ) ) ;
#28281 = CARTESIAN_POINT ( 'NONE',  ( 9.951054409601857387, -5.324155905473885397, 7.941945900372265221 ) ) ;
#28282 = CARTESIAN_POINT ( 'NONE',  ( 9.729392757687000071, -3.322036695224600322, 6.758914271013199304 ) ) ;
#28283 = VERTEX_POINT ( 'NONE', #5850 ) ;
#28284 = CARTESIAN_POINT ( 'NONE',  ( 24.00507834543561003, -9.358513022419435501, 9.266405905701180501 ) ) ;
#28285 = CARTESIAN_POINT ( 'NONE',  ( 11.21918447801630059, -2.859536135895000442, 7.525145395936648995 ) ) ;
#28286 = ORIENTED_EDGE ( 'NONE', *, *, #2360, .F. ) ;
#28287 = EDGE_CURVE ( 'NONE', #16917, #33506, #61870, .T. ) ;
#28288 = CARTESIAN_POINT ( 'NONE',  ( 8.266390833065004884, 2.877128322603998534, 6.332041950470006064 ) ) ;
#28289 = VERTEX_POINT ( 'NONE', #26500 ) ;
#28290 = CARTESIAN_POINT ( 'NONE',  ( 9.450870280412999591, 2.928319778732999978, -8.861178115809998701 ) ) ;
#28291 = CARTESIAN_POINT ( 'NONE',  ( 23.73581876812099978, 13.39628736436000089, -3.629848242966999816 ) ) ;
#28292 = CARTESIAN_POINT ( 'NONE',  ( 12.11461379017076112, 2.700589376673574016, -12.30719081517758084 ) ) ;
#28293 = CARTESIAN_POINT ( 'NONE',  ( 11.73078751119019891, -4.915752892793999962, 7.020904658857499925 ) ) ;
#28294 = EDGE_LOOP ( 'NONE', ( #52117, #25198, #24102, #60984 ) ) ;
#28295 = CARTESIAN_POINT ( 'NONE',  ( 27.64127793187000037, 5.599999999999999645, -6.571291218949999902 ) ) ;
#28296 = ORIENTED_EDGE ( 'NONE', *, *, #21304, .T. ) ;
#28297 = CARTESIAN_POINT ( 'NONE',  ( 23.60205915885299888, 11.72032963060998867, 3.891881970952999481 ) ) ;
#28298 = CARTESIAN_POINT ( 'NONE',  ( 23.65871351072082618, 10.04305333474976081, 9.454472293059238197 ) ) ;
#28299 = EDGE_LOOP ( 'NONE', ( #23127, #20913, #27639, #51666, #60386 ) ) ;
#28300 = CARTESIAN_POINT ( 'NONE',  ( 9.593930206849998754, 5.250000000000000000, 7.500000000000000000 ) ) ;
#28301 = CARTESIAN_POINT ( 'NONE',  ( 11.23610538575739959, 5.109472165990999848, 7.765257665594799796 ) ) ;
#28302 = CARTESIAN_POINT ( 'NONE',  ( 23.56666365135700403, 2.920993777334001340, -11.72568747145000145 ) ) ;
#28303 = CARTESIAN_POINT ( 'NONE',  ( 9.973493989215999278, 4.344963986309999804, -9.321593970653999861 ) ) ;
#28304 = CARTESIAN_POINT ( 'NONE',  ( 17.56873934038800300, -11.44357731092999941, 4.696002633125000436 ) ) ;
#28305 = CARTESIAN_POINT ( 'NONE',  ( 11.00589466765999802, -3.012766713855000056, 5.961506477028999385 ) ) ;
#28306 = CARTESIAN_POINT ( 'NONE',  ( 8.957462135714999718, 5.100000000000000533, -6.571291218949999902 ) ) ;
#28307 = CARTESIAN_POINT ( 'NONE',  ( 18.18003632999695895, 0.02081145935391477686, -12.69999906470294526 ) ) ;
#28308 = CARTESIAN_POINT ( 'NONE',  ( 12.20841262068627842, 2.686198883114174762, -12.40625987438722788 ) ) ;
#28309 = CARTESIAN_POINT ( 'NONE',  ( 10.54687750876899877, -4.617914354660699772, -8.458891008702400072 ) ) ;
#28310 = CARTESIAN_POINT ( 'NONE',  ( 7.647239158771000689, 5.850290547079999293, 6.784176679236000318 ) ) ;
#28311 = VERTEX_POINT ( 'NONE', #48510 ) ;
#28312 = CIRCLE ( 'NONE', #61789, 1.000000000000000000 ) ;
#28313 = AXIS2_PLACEMENT_3D ( 'NONE', #6222, #43297, #55513 ) ;
#28314 =( NAMED_UNIT ( * ) PLANE_ANGLE_UNIT ( ) SI_UNIT ( $, .RADIAN. ) );
#28315 = CARTESIAN_POINT ( 'NONE',  ( 11.00000000000000000, 4.991767524623399233, 7.825000000000000178 ) ) ;
#28316 = DIRECTION ( 'NONE',  ( 1.000000000000000000, 0.000000000000000000, 0.000000000000000000 ) ) ;
#28317 = CARTESIAN_POINT ( 'NONE',  ( 11.53898320224999985, 12.47165320829000024, 1.511147746418000093 ) ) ;
#28318 = CARTESIAN_POINT ( 'NONE',  ( 10.29094007826000023, 2.903522982536999919, -8.310916170934000036 ) ) ;
#28319 = CARTESIAN_POINT ( 'NONE',  ( 18.07135403277170127, 2.147634186626015573, 12.52670565379012579 ) ) ;
#28320 = EDGE_CURVE ( 'NONE', #46445, #28965, #47830, .T. ) ;
#28321 = CARTESIAN_POINT ( 'NONE',  ( 18.35499787466299892, 2.879071536379000040, -12.03968120189999880 ) ) ;
#28322 = ADVANCED_FACE ( 'NONE', ( #63191 ), #15320, .F. ) ;
#28323 = CARTESIAN_POINT ( 'NONE',  ( 10.27815081430999911, 5.521603098753999461, 8.751228458888000716 ) ) ;
#28324 = CARTESIAN_POINT ( 'NONE',  ( 10.33479966423462670, -3.204277625948437347, 7.136189372949617749 ) ) ;
#28325 = DIRECTION ( 'NONE',  ( 0.000000000000000000, -1.000000000000000000, 0.000000000000000000 ) ) ;
#28326 = VERTEX_POINT ( 'NONE', #52717 ) ;
#28327 = CARTESIAN_POINT ( 'NONE',  ( 12.31158149911131794, -3.007516552431697132, 12.23580242208396562 ) ) ;
#28328 = CARTESIAN_POINT ( 'NONE',  ( 9.403734463322997783, -3.881063085044400118, -8.635600483553998785 ) ) ;
#28329 = CARTESIAN_POINT ( 'NONE',  ( 8.455992358812000731, -5.100000000000000533, 6.571291218949999902 ) ) ;
#28330 = CARTESIAN_POINT ( 'NONE',  ( 9.293111399473126255, 2.988705873519680090, 8.251846359484561688 ) ) ;
#28331 = AXIS2_PLACEMENT_3D ( 'NONE', #36305, #57622, #9725 ) ;
#28332 = B_SPLINE_CURVE_WITH_KNOTS ( 'NONE', 3,
 ( #68155, #47195, #31127, #53470, #9777, #42303, #58708, #26561, #64282, #47887, #16399, #15721, #21305, #48219, #69191, #63943, #36354, #9427, #52778, #41944, #52082, #5563, #26905, #37047, #4185, #25523, #58362, #325, #31806, #42634, #16055, #30770, #21640, #41601, #37385 ),
 .UNSPECIFIED., .F., .F.,
 ( 4, 1, 1, 1, 1, 1, 1, 1, 1, 1, 1, 1, 1, 1, 1, 1, 1, 1, 1, 1, 1, 1, 1, 1, 1, 1, 1, 1, 1, 1, 1, 1, 4 ),
 ( 0.000000000000000000, 0.02634724210002164710, 0.05799096732718461711, 0.08963469255434758365, 0.1212784177813103353, 0.1529221430084733158, 0.1845658682354360536, 0.2162095934625990201, 0.2478533186897620144, 0.2794970439167247522, 0.3111407691438877188, 0.3427844943710506853, 0.3744282195980134231, 0.4060719448251764452, 0.4377156700521391830, 0.4693593952793021495, 0.5010031205064651161, 0.5326468457334281315, 0.5642905709605910980, 0.5959342961875535583, 0.6275780214147167468, 0.6592217466418797134, 0.6908654718688422847, 0.7225091970960054732, 0.7541529223229680445, 0.7857966475501312331, 0.8174403727772941997, 0.8490840980042566599, 0.8807278232314198485, 0.9123715484585828150, 0.9440152736855453863, 0.9756589989127085749, 1.000000000000000000 ),
 .UNSPECIFIED. ) ;
#28333 = CARTESIAN_POINT ( 'NONE',  ( 11.60118044953561878, 5.133201153721000054, -8.090905336380599167 ) ) ;
#28334 = ORIENTED_EDGE ( 'NONE', *, *, #67572, .T. ) ;
#28335 = CARTESIAN_POINT ( 'NONE',  ( 12.08612546794236486, -0.09367178904474190992, 12.59965724591066483 ) ) ;
#28336 = VECTOR ( 'NONE', #66320, 1000.000000000000000 ) ;
#28337 = CARTESIAN_POINT ( 'NONE',  ( 8.881823341230997926, 4.977909614887999545, 6.416776202806000029 ) ) ;
#28338 = CARTESIAN_POINT ( 'NONE',  ( 10.58844943056000076, 3.754657019866000311, 5.545350295858999523 ) ) ;
#28339 = CARTESIAN_POINT ( 'NONE',  ( 12.70862826151950919, 1.767199679044270333, 12.47545624547677434 ) ) ;
#28340 = ORIENTED_EDGE ( 'NONE', *, *, #16471, .T. ) ;
#28341 = CARTESIAN_POINT ( 'NONE',  ( 8.367589158771000513, 5.461114003844000031, -8.582501063019000398 ) ) ;
#28342 = CARTESIAN_POINT ( 'NONE',  ( 11.28118179236249929, 3.732952383914999839, -6.250199235344999771 ) ) ;
#28343 = EDGE_CURVE ( 'NONE', #4716, #67055, #39403, .T. ) ;
#28344 = EDGE_CURVE ( 'NONE', #12675, #68596, #28182, .T. ) ;
#28345 = CARTESIAN_POINT ( 'NONE',  ( 11.14975833414749928, 3.203462856645999945, 7.174999999999999822 ) ) ;
#28347 = CARTESIAN_POINT ( 'NONE',  ( 10.99999999997000089, -4.000000000000000000, 7.500000000000000000 ) ) ;
#28346 = CARTESIAN_POINT ( 'NONE',  ( 7.643735281411005111, 4.861037469149006363, 6.423817941563998879 ) ) ;
#28348 = CARTESIAN_POINT ( 'NONE',  ( 9.630088727410999638, -4.863977618062000019, 7.427538838030949719 ) ) ;
#28349 = B_SPLINE_CURVE_WITH_KNOTS ( 'NONE', 3,
 ( #51524, #46290, #19717, #11276 ),
 .UNSPECIFIED., .F., .F.,
 ( 4, 4 ),
 ( 0.000000000000000000, 1.000000000000000000 ),
 .UNSPECIFIED. ) ;
#28350 = CARTESIAN_POINT ( 'NONE',  ( 10.57980110216399972, -4.739241740354600552, -7.048535450274799885 ) ) ;
#28351 = CARTESIAN_POINT ( 'NONE',  ( 18.30000077768849565, 11.66744147158535405, -3.971919865264926575 ) ) ;
#28352 = ORIENTED_EDGE ( 'NONE', *, *, #41458, .F. ) ;
#28353 = EDGE_CURVE ( 'NONE', #46383, #62706, #58315, .T. ) ;
#28354 = CARTESIAN_POINT ( 'NONE',  ( 1.782293291478000086, 2.470933839010999833, -2.372615558983000472 ) ) ;
#28355 = CARTESIAN_POINT ( 'NONE',  ( 24.13225745270770517, -9.165361937195044106, -9.136521564051420796 ) ) ;
#28356 = CARTESIAN_POINT ( 'NONE',  ( 11.03521345716899837, -3.075109701058799772, 6.659120737011199331 ) ) ;
#28357 = CARTESIAN_POINT ( 'NONE',  ( 17.79118476696435280, 3.162166141421089094, -12.19676423671823962 ) ) ;
#28358 = CARTESIAN_POINT ( 'NONE',  ( 21.65000086032551252, 3.970157536060000036E-13, 1.776356839399999796E-13 ) ) ;
#28359 = CARTESIAN_POINT ( 'NONE',  ( 12.11351653522384098, -2.298558756435003403, 13.81002389223456106 ) ) ;
#28360 = CARTESIAN_POINT ( 'NONE',  ( 11.12921181303999951, 2.727588019252999985, 4.816967850745000668 ) ) ;
#28361 = PLANE ( 'NONE',  #7597 ) ;
#28362 = CARTESIAN_POINT ( 'NONE',  ( 13.36350100824700071, -12.09092425779999935, -2.196870506499999820 ) ) ;
#28363 = ORIENTED_EDGE ( 'NONE', *, *, #27327, .T. ) ;
#28364 = CARTESIAN_POINT ( 'NONE',  ( 6.933501042874380182, 3.037137096735000430, -6.379793420563999895 ) ) ;
#28365 = B_SPLINE_CURVE_WITH_KNOTS ( 'NONE', 3,
 ( #22472, #27045, #21780, #54644, #37522, #59191, #10956, #53606, #64079, #16198, #28078, #11293, #43115, #5704, #6738, #814 ),
 .UNSPECIFIED., .F., .F.,
 ( 4, 2, 2, 2, 2, 2, 2, 4 ),
 ( 0.000000000000000000, 0.06250000000000162370, 0.1250000000000032474, 0.2500000000000022760, 0.5000000000000005551, 0.7499999999999987788, 0.8749999999999994449, 1.000000000000000000 ),
 .UNSPECIFIED. ) ;
#28366 = DIRECTION ( 'NONE',  ( 0.7071067811865969777, 0.7071067811864980568, 3.301816515101990092E-09 ) ) ;
#28367 = DIRECTION ( 'NONE',  ( 0.5000000000000169864, 0.000000000000000000, 0.8660254037844288266 ) ) ;
#28368 = CARTESIAN_POINT ( 'NONE',  ( 9.629471092178999214, 5.100000000000000533, 6.152188490330000370 ) ) ;
#28369 = CARTESIAN_POINT ( 'NONE',  ( 0.6561095901646999407, -0.1662993809364999853, 3.755095982464999871 ) ) ;
#28370 = EDGE_LOOP ( 'NONE', ( #58672, #18991, #16529, #55354 ) ) ;
#28371 = DIRECTION ( 'NONE',  ( -1.000000000000000000, 0.000000000000000000, 0.000000000000000000 ) ) ;
#28372 = EDGE_CURVE ( 'NONE', #51133, #40281, #43551, .T. ) ;
#28373 = LINE ( 'NONE', #53887, #49835 ) ;
#28374 = CARTESIAN_POINT ( 'NONE',  ( 10.57224177473000104, 4.020426023752999178, 8.920668579831000145 ) ) ;
#28375 = CARTESIAN_POINT ( 'NONE',  ( 10.97364560330029981, 4.265439025801100570, 8.324524538096799375 ) ) ;
#28376 = DIRECTION ( 'NONE',  ( 0.000000000000000000, -0.1333333333333049375, -0.9910712498212375099 ) ) ;
#28377 = CARTESIAN_POINT ( 'NONE',  ( 11.05391814679000184, -5.159486550382999859, -8.487149456222999433 ) ) ;
#28378 = CARTESIAN_POINT ( 'NONE',  ( 17.74534446683495048, 0.7110419930699937163, -13.98197980709423582 ) ) ;
#28379 = DIRECTION ( 'NONE',  ( 1.000000000000000000, 0.000000000000000000, 0.000000000000000000 ) ) ;
#28380 = CARTESIAN_POINT ( 'NONE',  ( 12.23173037680160569, -2.748912840219636333, 12.39010626689776196 ) ) ;
#28381 = VERTEX_POINT ( 'NONE', #60723 ) ;
#28382 = CARTESIAN_POINT ( 'NONE',  ( 9.690635841230999858, 2.927176851028000293, -5.932007155957999878 ) ) ;
#28383 = AXIS2_PLACEMENT_3D ( 'NONE', #52963, #6087, #26050 ) ;
#28384 = ORIENTED_EDGE ( 'NONE', *, *, #49752, .F. ) ;
#28385 = B_SPLINE_CURVE_WITH_KNOTS ( 'NONE', 3,
 ( #23142, #24180, #18941, #66478, #44492, #59854 ),
 .UNSPECIFIED., .F., .F.,
 ( 4, 2, 4 ),
 ( 0.000000000000000000, 0.5000000000000000000, 1.000000000000000000 ),
 .UNSPECIFIED. ) ;
#28386 = CARTESIAN_POINT ( 'NONE',  ( 18.15957959476903838, -2.341019627110876744, 13.70589624875886514 ) ) ;
#28387 = CARTESIAN_POINT ( 'NONE',  ( 10.71503032197929883, -3.256621462143499901, -6.460430507351999196 ) ) ;
#28388 = VERTEX_POINT ( 'NONE', #65614 ) ;
#28389 = CARTESIAN_POINT ( 'NONE',  ( 11.19434208742519843, 3.521141233577200325, 6.747282993577999655 ) ) ;
#28390 = DIRECTION ( 'NONE',  ( -1.000000000000000000, 0.000000000000000000, 0.000000000000000000 ) ) ;
#28391 = CARTESIAN_POINT ( 'NONE',  ( 9.679055905794999859, -2.899999999999999911, 6.571291218949999902 ) ) ;
#28392 = CARTESIAN_POINT ( 'NONE',  ( 10.21609109105999913, 5.961715741921000067, 7.319666990313999477 ) ) ;
#28393 = B_SPLINE_CURVE_WITH_KNOTS ( 'NONE', 3,
 ( #57935, #20869, #4778, #21212 ),
 .UNSPECIFIED., .F., .F.,
 ( 4, 4 ),
 ( 0.000000000000000000, 1.000000000000000000 ),
 .UNSPECIFIED. ) ;
#28394 = CARTESIAN_POINT ( 'NONE',  ( 12.80505043854146940, -1.787797342887047947, -13.88538010501570774 ) ) ;
#28395 = FACE_OUTER_BOUND ( 'NONE', #54869, .T. ) ;
#28396 = CARTESIAN_POINT ( 'NONE',  ( 10.71685100253999856, -2.832432432432000269, 6.822293592207000934 ) ) ;
#28397 = CARTESIAN_POINT ( 'NONE',  ( 10.47211906628000122, -2.640759929160000130, -8.505246563374999624 ) ) ;
#28398 = CARTESIAN_POINT ( 'NONE',  ( 3.050973465878000113, 3.500000000000000000, 0.000000000000000000 ) ) ;
#28399 = DIRECTION ( 'NONE',  ( 0.000000000000000000, 0.8648648648648717963, -0.5020047465136829867 ) ) ;
#28400 = ORIENTED_EDGE ( 'NONE', *, *, #3934, .F. ) ;
#28401 = LINE ( 'NONE', #7408, #1329 ) ;
#28402 =( LENGTH_UNIT ( ) NAMED_UNIT ( * ) SI_UNIT ( .MILLI., .METRE. ) );
#28403 = ORIENTED_EDGE ( 'NONE', *, *, #55010, .F. ) ;
#28404 = CARTESIAN_POINT ( 'NONE',  ( 11.16486084871730000, 5.207010770456999893, 7.825000000000000178 ) ) ;
#28405 = CARTESIAN_POINT ( 'NONE',  ( 25.05003896993082435, -8.531459344605563544, 8.270378173953636392 ) ) ;
#28406 = DIRECTION ( 'NONE',  ( -1.000000000000000000, 0.000000000000000000, 0.000000000000000000 ) ) ;
#28407 = ADVANCED_FACE ( 'NONE', ( #44663 ), #44318, .F. ) ;
#28408 = CARTESIAN_POINT ( 'NONE',  ( 12.19562740135367918, 2.360953413553768421, 13.70191948036521268 ) ) ;
#28409 = EDGE_CURVE ( 'NONE', #59938, #24623, #46895, .T. ) ;
#28410 = B_SPLINE_SURFACE_WITH_KNOTS ( 'NONE', 3, 3, ( 
 ( #44114, #54232, #29075, #33618, #7382, #65412, #28029, #54937, #28723, #60525, #50385, #2484, #17884, #16826, #38150, #22766, #60184, #44804, #59476, #11576, #28374, #1797, #23115, #39550, #12634, #11932, #33964, #32919, #6331, #43760, #65054, #40922, #34661, #39902, #9437 ),
 ( #35687, #55974, #2824, #67137, #35004, #62581, #8424, #3176, #46519, #61559, #29767, #46173, #30110, #30779, #52091, #14017, #57001, #57335, #62245, #9103, #51413, #61221, #13337, #51072, #40241, #41267, #67822, #19248, #3508, #45826, #8081, #19603, #24505, #14702, #8768 ),
 ( #40576, #25184, #23810, #45143, #56662, #61903, #56319, #30441, #35346, #66804, #29422, #19946, #67481, #50731, #24155, #13675, #51752, #45489, #36020, #24846, #14363, #18916, #3846, #66453, #18575, #49721, #43589, #37056, #60005, #49168, #36717, #47553, #42311, #15389, #43937 ),
 ( #6515, #9787, #68855, #68507, #15039, #36365, #1280, #65241, #22594, #63613, #31469, #57678, #25871, #58371, #17358, #33098, #5233, #10137, #20630, #26570, #58038, #38684, #26224, #41954, #38331, #41612, #20975, #4195, #68164, #15729, #10473, #31814, #12117, #33445, #53133 ) ),
 .UNSPECIFIED., .F., .F., .F.,
 ( 4, 4 ),
 ( 4, 1, 1, 1, 1, 1, 1, 1, 1, 1, 1, 1, 1, 1, 1, 1, 1, 1, 1, 1, 1, 1, 1, 1, 1, 1, 1, 1, 1, 1, 1, 1, 4 ),
 ( -0.1039370721279000015, 1.103937072127999963 ),
 ( -0.01735257130020999988, 0.01084535706264999969, 0.03904328542550000031, 0.06724121378835999641, 0.09543914215121999944, 0.1236370705141000004, 0.1518349988768999959, 0.1800329272397999947, 0.2082308556026999935, 0.2364287839655000167, 0.2646267123283999601, 0.2928246406912000110, 0.3210225690540999821, 0.3492204974169000331, 0.3774184257798000042, 0.4056163541427000307, 0.4338142825054999707, 0.4620122108683999973, 0.4902101392311999928, 0.5184080675940999638, 0.5466059959569999904, 0.5748039243197999859, 0.6030018526827000125, 0.6311997810455000080, 0.6593977094084000345, 0.6875956377712000300, 0.7157935661340999456, 0.7439914944969999722, 0.7721894228597999676, 0.8003873512226999942, 0.8285852795854999897, 0.8567832079484000163, 0.8849811363112999318 ),
 .UNSPECIFIED. ) ;
#28411 = CARTESIAN_POINT ( 'NONE',  ( 11.09424907396999949, -2.431867116603999790, 7.769513708858000633 ) ) ;
#28412 = ORIENTED_EDGE ( 'NONE', *, *, #12892, .T. ) ;
#28413 = CARTESIAN_POINT ( 'NONE',  ( 7.852796759037660834, 2.886226026955057034, -6.701059260334753631 ) ) ;
#28414 = ADVANCED_FACE ( 'NONE', ( #50237 ), #10355, .F. ) ;
#28415 = CARTESIAN_POINT ( 'NONE',  ( 12.10431174240586216, 0.1888260363403126418, 13.99874504378992413 ) ) ;
#28416 = VERTEX_POINT ( 'NONE', #2341 ) ;
#28417 = CARTESIAN_POINT ( 'NONE',  ( 12.68949153424100196, 11.39033517652999983, -4.571431300619999583 ) ) ;
#28418 = CARTESIAN_POINT ( 'NONE',  ( 10.42499241036559532, -5.349775919985432004, 7.500001834605715345 ) ) ;
#28419 = CARTESIAN_POINT ( 'NONE',  ( 24.08681017553700343, -3.426492766728000294, -12.66987775218999879 ) ) ;
#28420 = CARTESIAN_POINT ( 'NONE',  ( 4.658353212288999678, 0.7287915381420000394, 0.9369635204702000397 ) ) ;
#28421 = VECTOR ( 'NONE', #54997, 1000.000000000000000 ) ;
#28422 = B_SPLINE_SURFACE_WITH_KNOTS ( 'NONE', 3, 3, ( 
 ( #17779, #12528, #49233, #39097 ),
 ( #27572, #54482, #44702, #2042 ),
 ( #6583, #27923, #1343, #65657 ),
 ( #44003, #43658, #6928, #60422 ),
 ( #38400, #48899, #11826, #22659 ),
 ( #33859, #28263, #54134, #55174 ),
 ( #49581, #38753, #65310, #7278 ),
 ( #17424, #18122, #28617, #65997 ) ),
 .UNSPECIFIED., .F., .F., .F.,
 ( 4, 1, 1, 1, 1, 4 ),
 ( 4, 4 ),
 ( 0.008355529829647000833, 0.05882352941176000050, 0.1176470588234999892, 0.1764705882353000133, 0.2352941176471000095, 0.2534842851975999678 ),
 ( -0.1830816906711000003, 1.182949851103000105 ),
 .UNSPECIFIED. ) ;
#28423 = CARTESIAN_POINT ( 'NONE',  ( 9.585279719593998493, 2.928319778732999978, -8.861178115809998701 ) ) ;
#28424 = CARTESIAN_POINT ( 'NONE',  ( 8.331682137624000006, -5.101289325373999262, 6.607176193198000647 ) ) ;
#28425 = CARTESIAN_POINT ( 'NONE',  ( 10.55068143582000140, -2.412180768165999911, -6.919582641217999708 ) ) ;
#28426 = CARTESIAN_POINT ( 'NONE',  ( 7.000000000000000000, -9.186881182980000560, -5.186879035586000164 ) ) ;
#28427 = LINE ( 'NONE', #49050, #8074 ) ;
#28428 = DIRECTION ( 'NONE',  ( -1.000000000000000000, 0.000000000000000000, 0.000000000000000000 ) ) ;
#28429 = CARTESIAN_POINT ( 'NONE',  ( 9.010799540956998754, -4.699533657262000119, -6.366989705700999203 ) ) ;
#28430 = DIRECTION ( 'NONE',  ( 0.7071067811865475727, 0.7071067811865475727, 0.000000000000000000 ) ) ;
#28431 = CARTESIAN_POINT ( 'NONE',  ( 1.073890132542374864, 2.150913519912194705, 2.798833948393636639 ) ) ;
#28432 = CARTESIAN_POINT ( 'NONE',  ( 11.39189666366029918, 3.947847673382490541, -8.673729056199000809 ) ) ;
#28433 = CARTESIAN_POINT ( 'NONE',  ( 9.989267173155999657, 3.235527139800300045, -6.848522029265999400 ) ) ;
#28435 = CARTESIAN_POINT ( 'NONE',  ( 9.311649685568999857, -3.898643963693099845, 6.542299367266399379 ) ) ;
#28434 = CARTESIAN_POINT ( 'NONE',  ( 9.445797255587999430, -2.996487526130999779, 7.542485555928779561 ) ) ;
#28436 = AXIS2_PLACEMENT_3D ( 'NONE', #49430, #59922, #17634 ) ;
#28437 = DIRECTION ( 'NONE',  ( 1.000000000000000000, 0.000000000000000000, 0.000000000000000000 ) ) ;
#28438 = EDGE_LOOP ( 'NONE', ( #46647, #45554, #66512, #28469, #34388, #65332, #23318, #38729, #42596, #57027 ) ) ;
#28439 = CARTESIAN_POINT ( 'NONE',  ( 11.60477869730532774, 3.532552483170099844, 8.421761806503198500 ) ) ;
#28440 = CARTESIAN_POINT ( 'NONE',  ( 7.443695762906002322, -3.525420668437998728, 6.642224720921002579 ) ) ;
#28441 = CARTESIAN_POINT ( 'NONE',  ( 8.975151519677000422, 4.027664626136379766, 6.221087886525999089 ) ) ;
#28442 = CARTESIAN_POINT ( 'NONE',  ( 9.505520750864626223, 3.872956735472087964, -6.634325535862901191 ) ) ;
#28443 = CARTESIAN_POINT ( 'NONE',  ( 9.414314870535999802, -3.941041813398000304, 5.878346364186999295 ) ) ;
#28444 = CARTESIAN_POINT ( 'NONE',  ( 9.857064864738445564, -3.288037737649794234, 9.126893253094490177 ) ) ;
#28445 = CARTESIAN_POINT ( 'NONE',  ( 5.399998535875000449, -12.99045401563999924, -1.690592933733000125 ) ) ;
#28446 = B_SPLINE_CURVE_WITH_KNOTS ( 'NONE', 3,
 ( #34537, #45019, #55848, #9309 ),
 .UNSPECIFIED., .F., .F.,
 ( 4, 4 ),
 ( 0.000000000000000000, 1.000000000000000000 ),
 .UNSPECIFIED. ) ;
#28447 = ORIENTED_EDGE ( 'NONE', *, *, #5533, .F. ) ;
#28448 = CONICAL_SURFACE ( 'NONE', #52997, 13.22499948080999843, 0.7853981240402999608 ) ;
#28449 = B_SPLINE_CURVE_WITH_KNOTS ( 'NONE', 3,
 ( #9114, #36376, #9449, #31828 ),
 .UNSPECIFIED., .F., .F.,
 ( 4, 4 ),
 ( 0.000000000000000000, 1.000000000000000000 ),
 .UNSPECIFIED. ) ;
#28450 = CARTESIAN_POINT ( 'NONE',  ( 8.748138961223999033, -3.167792625045000143, -8.062381800110799190 ) ) ;
#28451 = CARTESIAN_POINT ( 'NONE',  ( 9.856851002545999663, -2.832432432432000269, -6.822293592207000934 ) ) ;
#28452 = DIRECTION ( 'NONE',  ( -1.000000000000000000, 0.000000000000000000, 0.000000000000000000 ) ) ;
#28453 = EDGE_CURVE ( 'NONE', #58820, #66385, #51628, .T. ) ;
#28454 = CARTESIAN_POINT ( 'NONE',  ( 10.52145237372899800, -3.956267952212241479, 6.225919055146348136 ) ) ;
#28455 = LINE ( 'NONE', #7117, #20547 ) ;
#28456 = CARTESIAN_POINT ( 'NONE',  ( 11.74441369783139955, -4.043700988887960257, 6.634905315059499209 ) ) ;
#28457 = CARTESIAN_POINT ( 'NONE',  ( 11.01872200990539952, 3.052519557825900343, -7.169497859994799605 ) ) ;
#28458 = CARTESIAN_POINT ( 'NONE',  ( 12.18791262560835342, 2.399397798254620628, -13.69429647071889811 ) ) ;
#28459 = CARTESIAN_POINT ( 'NONE',  ( 9.700159544970999193, -4.268950419651999617, -8.781589108989999559 ) ) ;
#28460 = CARTESIAN_POINT ( 'NONE',  ( 12.56893612372510205, 3.162115968191201443, 12.19677724224926685 ) ) ;
#28461 = EDGE_LOOP ( 'NONE', ( #7559, #69043, #56208, #43583, #7110, #3347, #45717, #6645, #28867, #9739 ) ) ;
#28462 = CARTESIAN_POINT ( 'NONE',  ( 24.59180953954000159, -12.25104150531999991, -3.053504439888000022 ) ) ;
#28463 = CARTESIAN_POINT ( 'NONE',  ( 12.08466087602982597, -0.08309727575450116810, -13.99975851644561686 ) ) ;
#28464 = CARTESIAN_POINT ( 'NONE',  ( 16.10005255078199937, 3.632778330393000132, 11.06917548872000090 ) ) ;
#28465 = CARTESIAN_POINT ( 'NONE',  ( 9.970944094204998720, -5.100000000000000533, 6.571291218949999902 ) ) ;
#28466 = CARTESIAN_POINT ( 'NONE',  ( 10.56059687351646481, -3.370476274536376771, -8.592232985442823434 ) ) ;
#28467 = DIRECTION ( 'NONE',  ( 1.000000000000000000, 0.000000000000000000, 0.000000000000000000 ) ) ;
#28468 = CARTESIAN_POINT ( 'NONE',  ( 5.601974509047820128, 12.13172069192291680, -3.749825701181556781 ) ) ;
#28469 = ORIENTED_EDGE ( 'NONE', *, *, #8914, .F. ) ;
#28470 = CARTESIAN_POINT ( 'NONE',  ( 23.89320776801300283, 8.862674798131001452, 7.304122743059000555 ) ) ;
#28471 = CARTESIAN_POINT ( 'NONE',  ( 17.72176632460244861, 3.228945123492080516, -13.62255252064306177 ) ) ;
#28472 = EDGE_LOOP ( 'NONE', ( #55126, #25127, #65926 ) ) ;
#28473 = DIRECTION ( 'NONE',  ( 1.000000000000000000, 0.000000000000000000, 0.000000000000000000 ) ) ;
#28474 = CARTESIAN_POINT ( 'NONE',  ( 24.83137806176560503, 8.598806517310384478, -8.498658647712348468 ) ) ;
#28475 = CARTESIAN_POINT ( 'NONE',  ( 23.50387503050299998, 0.01734707287875719012, -13.99998925281954065 ) ) ;
#28476 = PRODUCT_DEFINITION_FORMATION_WITH_SPECIFIED_SOURCE ( 'ANY', '', #23773, .NOT_KNOWN. ) ;
#28477 = CARTESIAN_POINT ( 'NONE',  ( 24.13560165858060813, -12.48955752925216167, 3.366833954017129482 ) ) ;
#28478 = CARTESIAN_POINT ( 'NONE',  ( 17.84579744522521239, 1.849003904486290484, -13.87736309738764540 ) ) ;
#28479 = CARTESIAN_POINT ( 'NONE',  ( 18.03457482787555577, 0.4008908244826864808, -12.69148415474307789 ) ) ;
#28480 = CARTESIAN_POINT ( 'NONE',  ( 11.09166666666872203, -2.528771982360623838, 6.972956482935448896 ) ) ;
#28481 = EDGE_LOOP ( 'NONE', ( #5338, #24481, #5173, #63250 ) ) ;
#28482 = CARTESIAN_POINT ( 'NONE',  ( 11.08992739829000129, -5.210546653347999602, 8.327600405525998895 ) ) ;
#28483 = CARTESIAN_POINT ( 'NONE',  ( 18.08141525686298579, -2.837131573376346694, -13.59610056796362088 ) ) ;
#28484 = CARTESIAN_POINT ( 'NONE',  ( 23.66004879239100234, 6.960835523577999950, -12.06029416026999890 ) ) ;
#28485 = EDGE_LOOP ( 'NONE', ( #66017, #21864, #11155, #51791 ) ) ;
#28486 = CARTESIAN_POINT ( 'NONE',  ( 10.73506130198999919, 5.202496273738000276, -8.441412224440000500 ) ) ;
#28487 = ORIENTED_EDGE ( 'NONE', *, *, #44622, .F. ) ;
#28488 = CARTESIAN_POINT ( 'NONE',  ( 9.153405316139998860, 3.786750623988900166, 6.518487389810699639 ) ) ;
#28489 = CARTESIAN_POINT ( 'NONE',  ( 18.20581337561481305, -2.797825772877925221, -12.28545032770987255 ) ) ;
#28490 = AXIS2_PLACEMENT_3D ( 'NONE', #59520, #58146, #26338 ) ;
#28491 = CARTESIAN_POINT ( 'NONE',  ( 9.602263540182329749, 5.092232985442822546, 6.870476274536374106 ) ) ;
#28492 = CARTESIAN_POINT ( 'NONE',  ( 15.95279538704000366, 3.847565940079000324, 11.76597731123000123 ) ) ;
#28493 = CARTESIAN_POINT ( 'NONE',  ( 11.64596081258699911, -11.57456368445000017, -1.729631387595999881 ) ) ;
#28494 = ADVANCED_FACE ( 'NONE', ( #49197 ), #967, .F. ) ;
#28495 = EDGE_CURVE ( 'NONE', #24471, #49930, #52704, .T. ) ;
#28496 = CARTESIAN_POINT ( 'NONE',  ( 9.763317406968999634, 4.161254277581000416, 6.648116790593900483 ) ) ;
#28497 = EDGE_CURVE ( 'NONE', #57662, #10646, #11839, .T. ) ;
#28498 = EDGE_CURVE ( 'NONE', #46731, #53432, #25956, .T. ) ;
#28499 = CARTESIAN_POINT ( 'NONE',  ( 9.382379370190513157, -2.850576913252966360, 8.805889684294008646 ) ) ;
#28500 = ORIENTED_EDGE ( 'NONE', *, *, #60579, .T. ) ;
#28501 = CARTESIAN_POINT ( 'NONE',  ( 9.440795537696265782, 5.100000000000000533, 6.662590550601107608 ) ) ;
#28502 = CARTESIAN_POINT ( 'NONE',  ( 10.28180471959000108, 3.991526675591000384, -5.814300410279999554 ) ) ;
#28503 = FACE_OUTER_BOUND ( 'NONE', #59316, .T. ) ;
#28504 = CARTESIAN_POINT ( 'NONE',  ( 12.70235978774137919, 3.116847232384802435, -13.52309701207074433 ) ) ;
#28505 = CARTESIAN_POINT ( 'NONE',  ( 11.14601354018249779, -3.000416447002271170, 8.268183399968638270 ) ) ;
#28506 = CARTESIAN_POINT ( 'NONE',  ( 24.67332306156800215, 3.458640006525999677, 12.04351266709000079 ) ) ;
#28507 = CARTESIAN_POINT ( 'NONE',  ( 18.05092994784023830, 0.3809766167652354207, 13.89298487834589402 ) ) ;
#28508 = CARTESIAN_POINT ( 'NONE',  ( 24.98632790797000069, -3.086020258067999844, 11.61344380798999865 ) ) ;
#28509 = B_SPLINE_CURVE_WITH_KNOTS ( 'NONE', 1,
 ( #18354, #33747 ),
 .UNSPECIFIED., .F., .F.,
 ( 2, 2 ),
 ( 0.000000000000000000, 1.000000000000000000 ),
 .UNSPECIFIED. ) ;
#28510 = ORIENTED_EDGE ( 'NONE', *, *, #52867, .F. ) ;
#28511 = ORIENTED_EDGE ( 'NONE', *, *, #24662, .T. ) ;
#28512 = CARTESIAN_POINT ( 'NONE',  ( 8.988579719593998263, 4.902869380824999901, -8.978557145469999057 ) ) ;
#28513 = CARTESIAN_POINT ( 'NONE',  ( 12.40587428659213387, -0.4809231526391881117, 13.88880064789875668 ) ) ;
#28514 = CARTESIAN_POINT ( 'NONE',  ( 12.34511315269137199, -0.4233056299066826345, -13.89132630015665448 ) ) ;
#28515 = AXIS2_PLACEMENT_3D ( 'NONE', #27729, #32289, #16532 ) ;
#28516 = CARTESIAN_POINT ( 'NONE',  ( 17.55505043854147118, -1.875000000000000000, -25.00000000000000000 ) ) ;
#28517 = CARTESIAN_POINT ( 'NONE',  ( 9.266851002542999538, 2.832432432432000269, 6.822293592207000934 ) ) ;
#28518 = EDGE_CURVE ( 'NONE', #37419, #38028, #49359, .T. ) ;
#28519 = CARTESIAN_POINT ( 'NONE',  ( 9.117519353207999444, -4.954907757874000396, 8.825780921426000347 ) ) ;
#28520 = CARTESIAN_POINT ( 'NONE',  ( 10.39393020684999946, -5.250000000000000000, -7.500000000000000000 ) ) ;
#28522 = CARTESIAN_POINT ( 'NONE',  ( 11.07127482541000063, -5.550092857035999749, 5.077717152805000467 ) ) ;
#28521 = CARTESIAN_POINT ( 'NONE',  ( 10.66562143724499911, -3.150324864944999970, 8.456261759323901117 ) ) ;
#28523 = FACE_OUTER_BOUND ( 'NONE', #53200, .T. ) ;
#28524 = CARTESIAN_POINT ( 'NONE',  ( 7.481658233226216481, 4.679574733145784649, -6.320553983555220690 ) ) ;
#28525 = CARTESIAN_POINT ( 'NONE',  ( 9.393930206848999376, 2.750000000000000000, -7.500000000000000000 ) ) ;
#28526 = B_SPLINE_CURVE_WITH_KNOTS ( 'NONE', 1,
 ( #43218, #40060 ),
 .UNSPECIFIED., .F., .F.,
 ( 2, 2 ),
 ( 0.000000000000000000, 1.000000000000000000 ),
 .UNSPECIFIED. ) ;
#28527 = CARTESIAN_POINT ( 'NONE',  ( 18.01167108103433279, 0.4268810874232056851, 12.69034564040269331 ) ) ;
#28528 = CARTESIAN_POINT ( 'NONE',  ( 11.09999999999999964, -5.299999999999999822, 6.469505845987999493 ) ) ;
#28529 = CARTESIAN_POINT ( 'NONE',  ( 18.10295792975328411, -2.800845226996505399, -12.37636719702903676 ) ) ;
#28530 = ORIENTED_EDGE ( 'NONE', *, *, #53401, .T. ) ;
#28532 = CARTESIAN_POINT ( 'NONE',  ( 9.601268341696789221, 5.349866766629849835, -7.263147672793892617 ) ) ;
#28531 = CARTESIAN_POINT ( 'NONE',  ( 8.802620559624999785, -3.975070057433999438, 9.483761758588999058 ) ) ;
#28533 = CARTESIAN_POINT ( 'NONE',  ( 8.316054719590999511, 3.826300099041999747, -9.055335252254000267 ) ) ;
#28534 = CARTESIAN_POINT ( 'NONE',  ( 24.96658445227665979, 10.83443034554823825, 3.855530973479976531 ) ) ;
#28535 = DIRECTION ( 'NONE',  ( -1.000000000000000000, 0.000000000000000000, 0.000000000000000000 ) ) ;
#28536 = CARTESIAN_POINT ( 'NONE',  ( 10.81349144726329925, 3.261052100888700345, 8.542723541016000510 ) ) ;
#28537 = DIRECTION ( 'NONE',  ( 0.000000000000000000, 0.000000000000000000, -1.000000000000000000 ) ) ;
#28538 = AXIS2_PLACEMENT_3D ( 'NONE', #65744, #55955, #66089 ) ;
#28539 = EDGE_CURVE ( 'NONE', #16690, #35994, #65202, .T. ) ;
#28540 = CARTESIAN_POINT ( 'NONE',  ( 9.484111209357660499, 2.372201727752532019, 6.771817387162120561 ) ) ;
#28541 = CARTESIAN_POINT ( 'NONE',  ( 2.924292960406999597, -3.109127409734000036, 1.438104787010000107 ) ) ;
#28542 = ORIENTED_EDGE ( 'NONE', *, *, #1760, .F. ) ;
#28543 = CARTESIAN_POINT ( 'NONE',  ( 12.28357442006479872, 0.4998493492227008006, -12.59008424712974872 ) ) ;
#28544 = CARTESIAN_POINT ( 'NONE',  ( 11.07928355765999839, -7.977355694624001181, -6.935622273774999513 ) ) ;
#28545 = EDGE_CURVE ( 'NONE', #22085, #65709, #68267, .T. ) ;
#28546 = DIRECTION ( 'NONE',  ( -1.000000000000000000, 0.000000000000000000, 0.000000000000000000 ) ) ;
#28547 = CARTESIAN_POINT ( 'NONE',  ( 8.283079719592000956, 2.376526778640999815, 7.686980884243000745 ) ) ;
#28548 = ORIENTED_EDGE ( 'NONE', *, *, #36095, .T. ) ;
#28549 = CARTESIAN_POINT ( 'NONE',  ( 6.703079102619000196, -0.05887414910050999678, 1.174638368522000098 ) ) ;
#28550 = CARTESIAN_POINT ( 'NONE',  ( 10.94048155334786010, 9.309399651271464293, 6.237067107879298966 ) ) ;
#28552 = CYLINDRICAL_SURFACE ( 'NONE', #874, 0.6250000000000005551 ) ;
#28551 = CARTESIAN_POINT ( 'NONE',  ( 8.559591719171793400, -3.670668999121442955, 5.791868630734976264 ) ) ;
#28553 = CARTESIAN_POINT ( 'NONE',  ( 11.30367835872029936, 2.886444435522000251, -6.798177532456199934 ) ) ;
#28554 = ORIENTED_EDGE ( 'NONE', *, *, #46050, .T. ) ;
#28555 = DIRECTION ( 'NONE',  ( 0.000000000000000000, 1.000000000000000000, 0.000000000000000000 ) ) ;
#28556 = ORIENTED_EDGE ( 'NONE', *, *, #25731, .F. ) ;
#28557 = CARTESIAN_POINT ( 'NONE',  ( 9.493541411000029129, -4.876956592064014551, 8.526784707585971290 ) ) ;
#28558 = CARTESIAN_POINT ( 'NONE',  ( 16.13849254682300227, 3.245716968028000249, 11.43439984646999896 ) ) ;
#28559 = CARTESIAN_POINT ( 'NONE',  ( 18.15913552218862037, 0.1616183441363971129, -13.89875400931294180 ) ) ;
#28560 = ORIENTED_EDGE ( 'NONE', *, *, #60528, .F. ) ;
#28561 = CARTESIAN_POINT ( 'NONE',  ( 10.48692887490000025, -8.228405771565000748, 6.845561203178999854 ) ) ;
#28562 = CARTESIAN_POINT ( 'NONE',  ( 25.39993151917486713, -2.060147809147888420, -11.21226007647768874 ) ) ;
#28563 = CARTESIAN_POINT ( 'NONE',  ( 10.34393020685000053, -5.250000000000000000, 7.500000000000000000 ) ) ;
#28564 = LINE ( 'NONE', #54774, #66629 ) ;
#28565 = CARTESIAN_POINT ( 'NONE',  ( 18.16752965499882677, -2.624502286956208685, 12.42171427751213919 ) ) ;
#28566 = ORIENTED_EDGE ( 'NONE', *, *, #11225, .T. ) ;
#28567 = DIRECTION ( 'NONE',  ( 0.000000000000000000, 0.000000000000000000, 1.000000000000000000 ) ) ;
#28568 = CARTESIAN_POINT ( 'NONE',  ( 12.52739587006843358, -3.060316261558335693, -13.53846823646701125 ) ) ;
#28569 = CARTESIAN_POINT ( 'NONE',  ( 16.10004050617000004, 3.886235259787000018, 11.90683839252000098 ) ) ;
#28570 = AXIS2_PLACEMENT_3D ( 'NONE', #17898, #12647, #35017 ) ;
#28571 = DIRECTION ( 'NONE',  ( 0.000000000000000000, 1.000000000000000000, 0.000000000000000000 ) ) ;
#28572 = VERTEX_POINT ( 'NONE', #25689 ) ;
#28573 = CARTESIAN_POINT ( 'NONE',  ( 10.08712270112374121, -5.286531262339795312, -7.026829543710682024 ) ) ;
#28574 = AXIS2_PLACEMENT_3D ( 'NONE', #41912, #47163, #12682 ) ;
#28575 = CARTESIAN_POINT ( 'NONE',  ( 10.95950272614480880, -2.825896501487262569, -6.683764319341896964 ) ) ;
#28576 = CARTESIAN_POINT ( 'NONE',  ( 7.391647165042849466, 5.483386455157001294, -8.617406009823950441 ) ) ;
#28577 = CARTESIAN_POINT ( 'NONE',  ( 11.09999999999999964, -4.000000000000000000, 7.500000000000000000 ) ) ;
#28578 = CARTESIAN_POINT ( 'NONE',  ( 24.39664325339802176, 8.810500106973549350, 8.810500106973549350 ) ) ;
#28579 = CYLINDRICAL_SURFACE ( 'NONE', #46479, 1.500000000000000000 ) ;
#28580 = EDGE_CURVE ( 'NONE', #41017, #28137, #42805, .T. ) ;
#28582 = EDGE_CURVE ( 'NONE', #25195, #26111, #36525, .T. ) ;
#28581 = CARTESIAN_POINT ( 'NONE',  ( 17.71812653075902944, -3.103437839927554176, 12.29028812931824000 ) ) ;
#28583 = ORIENTED_EDGE ( 'NONE', *, *, #48925, .F. ) ;
#28584 = CARTESIAN_POINT ( 'NONE',  ( 9.475960865537832234, -5.125960927305071024, 7.353476508004328061 ) ) ;
#28585 = EDGE_LOOP ( 'NONE', ( #8393, #14146, #48748, #62548 ) ) ;
#28586 = B_SPLINE_CURVE_WITH_KNOTS ( 'NONE', 3,
 ( #44551, #17621, #48389, #32324, #841 ),
 .UNSPECIFIED., .F., .F.,
 ( 4, 1, 4 ),
 ( 0.000000000000000000, 0.5000000000000000000, 1.000000000000000000 ),
 .UNSPECIFIED. ) ;
#28587 = CARTESIAN_POINT ( 'NONE',  ( 11.50001544675000176, -12.52500000000000036, 0.000000000000000000 ) ) ;
#28588 = AXIS2_PLACEMENT_3D ( 'NONE', #56038, #61289, #13404 ) ;
#28589 = CARTESIAN_POINT ( 'NONE',  ( 9.933354719590999693, 5.639765292528999829, -8.059103558718000215 ) ) ;
#28590 = CARTESIAN_POINT ( 'NONE',  ( 2.538319053239000311, -2.896360734409999971, -1.395582542787000113 ) ) ;
#28591 = CARTESIAN_POINT ( 'NONE',  ( 10.05525937050999907, -5.223866772223000332, -6.898311956607000361 ) ) ;
#28592 = AXIS2_PLACEMENT_3D ( 'NONE', #53754, #27533, #11103 ) ;
#28593 = CARTESIAN_POINT ( 'NONE',  ( 6.727909377860130213, -0.04179919159915057580, -1.517065169120832779 ) ) ;
#28594 = CARTESIAN_POINT ( 'NONE',  ( 9.568197172114434323, 5.125396288428782476, -6.749639981086958507 ) ) ;
#28595 = DIRECTION ( 'NONE',  ( 0.000000000000000000, -1.000000000000000000, 0.000000000000000000 ) ) ;
#28596 = VERTEX_POINT ( 'NONE', #31292 ) ;
#28597 = DIRECTION ( 'NONE',  ( 1.000000000000000000, 0.000000000000000000, 0.000000000000000000 ) ) ;
#28598 = CARTESIAN_POINT ( 'NONE',  ( 11.39564560330030041, -3.692495237344800341, 8.455191956516999952 ) ) ;
#28599 = CARTESIAN_POINT ( 'NONE',  ( 10.31667774810000004, 3.819530253758000260, 6.062195927068000145 ) ) ;
#28600 = DIRECTION ( 'NONE',  ( -8.953094821931283005E-11, -0.9867385579967302700, -0.1623176458754050089 ) ) ;
#28601 = EDGE_CURVE ( 'NONE', #54370, #26667, #4695, .T. ) ;
#28602 = CARTESIAN_POINT ( 'NONE',  ( 10.53521345716899837, 4.924890298941200228, -8.340879262988799780 ) ) ;
#28603 = CARTESIAN_POINT ( 'NONE',  ( 4.950033214355999966, 0.000000000000000000, 0.000000000000000000 ) ) ;
#28604 = CARTESIAN_POINT ( 'NONE',  ( 10.67826222744820086, 3.331419131587999960, -8.050725169876500331 ) ) ;
#28605 = DIRECTION ( 'NONE',  ( 1.000000000000000000, 0.000000000000000000, 0.000000000000000000 ) ) ;
#28606 = CARTESIAN_POINT ( 'NONE',  ( 9.783671671056998420, 2.873958896683999953, -7.689118697196099639 ) ) ;
#28607 = CARTESIAN_POINT ( 'NONE',  ( 23.54916673983900210, -10.40118575069000073, 9.428023239853999371 ) ) ;
#28608 = CARTESIAN_POINT ( 'NONE',  ( 8.107831681780405475, 5.065903857563916368, -6.531537680950162184 ) ) ;
#28609 = CARTESIAN_POINT ( 'NONE',  ( 10.31153584123000044, 2.716831823259000078, -7.950163994344000784 ) ) ;
#28610 = ORIENTED_EDGE ( 'NONE', *, *, #42525, .T. ) ;
#28611 = CARTESIAN_POINT ( 'NONE',  ( 8.014941940377999785, -2.280579276705999803, 6.510290672242000198 ) ) ;
#28612 = CARTESIAN_POINT ( 'NONE',  ( 10.10633213213999859, -4.301175052434000001, -8.935144319903001175 ) ) ;
#28613 = CARTESIAN_POINT ( 'NONE',  ( 18.27051424461482654, 2.638143613628436412, 13.74920933505747556 ) ) ;
#28614 = CARTESIAN_POINT ( 'NONE',  ( 23.58131316884520245, 3.140314540300665591, 13.62732133062536377 ) ) ;
#28615 = CARTESIAN_POINT ( 'NONE',  ( 11.25656651104150008, -3.873914634362100262, -6.228222165170999247 ) ) ;
#28616 = ORIENTED_EDGE ( 'NONE', *, *, #57765, .F. ) ;
#28617 = CARTESIAN_POINT ( 'NONE',  ( 25.48313700195200227, 2.676699651352000053, -11.27114471784999949 ) ) ;
#28618 = CARTESIAN_POINT ( 'NONE',  ( 7.678989158771000412, 2.599243720295000060, 7.909344432242998657 ) ) ;
#28619 = CONICAL_SURFACE ( 'NONE', #17485, 2.049966935984999683, 0.7853819979415218588 ) ;
#28621 = CARTESIAN_POINT ( 'NONE',  ( 9.241252916288999586, -3.907441415015589836, 6.625425395127999550 ) ) ;
#28620 = DIRECTION ( 'NONE',  ( -1.000000000000000000, 0.000000000000000000, 0.000000000000000000 ) ) ;
#28622 = CARTESIAN_POINT ( 'NONE',  ( 10.91060165877000188, 4.702351492776999820, -9.210043641106000933 ) ) ;
#28623 = ORIENTED_EDGE ( 'NONE', *, *, #56998, .T. ) ;
#28624 = CARTESIAN_POINT ( 'NONE',  ( 10.05691520198999989, 2.453477278391000382, 6.657104391228999773 ) ) ;
#28625 = CARTESIAN_POINT ( 'NONE',  ( 17.72083032727078233, -3.229203862303416717, -13.62249117442682333 ) ) ;
#28626 = CARTESIAN_POINT ( 'NONE',  ( 11.28533594839949750, 4.750012929834699804, 8.359517726022600570 ) ) ;
#28627 = EDGE_CURVE ( 'NONE', #11176, #59953, #31631, .T. ) ;
#28628 = CARTESIAN_POINT ( 'NONE',  ( 9.298040139821001304, -4.087076480742000584, 9.429402848390999736 ) ) ;
#28629 = CARTESIAN_POINT ( 'NONE',  ( 1.700000000000000178, 0.000000000000000000, 0.000000000000000000 ) ) ;
#28630 = VERTEX_POINT ( 'NONE', #60608 ) ;
#28631 = CARTESIAN_POINT ( 'NONE',  ( 6.899999689904000810, -12.43893549496000084, 2.828936992187000232 ) ) ;
#28632 = B_SPLINE_CURVE_WITH_KNOTS ( 'NONE', 3,
 ( #26850, #11100, #28573, #2680 ),
 .UNSPECIFIED., .F., .F.,
 ( 4, 4 ),
 ( 0.8745849735171273842, 1.000000000000000000 ),
 .UNSPECIFIED. ) ;
#28633 = CARTESIAN_POINT ( 'NONE',  ( 11.22022944037999892, -3.883088694641999794, -8.854817792072001481 ) ) ;
#28634 = CARTESIAN_POINT ( 'NONE',  ( 7.933152249316766103, -2.298782909427148358, 7.863666461026288523 ) ) ;
#28635 = CARTESIAN_POINT ( 'NONE',  ( 10.71756905878999966, -3.040221764047000175, 8.808455607108001573 ) ) ;
#28637 = CARTESIAN_POINT ( 'NONE',  ( 23.58435506825300010, 2.902136918182999903, 13.63397704980999947 ) ) ;
#28636 = VECTOR ( 'NONE', #30440, 1000.000000000000114 ) ;
#28638 = CARTESIAN_POINT ( 'NONE',  ( 9.930013376692999216, -5.017903082085999777, 8.017308190024898806 ) ) ;
#28639 = VERTEX_POINT ( 'NONE', #38588 ) ;
#28640 = CARTESIAN_POINT ( 'NONE',  ( 23.61469341836961533, -10.17936131679624445, 9.423452332300746193 ) ) ;
#28641 = B_SPLINE_CURVE_WITH_KNOTS ( 'NONE', 3,
 ( #57289, #10429, #9391, #30737, #52045, #25488 ),
 .UNSPECIFIED., .F., .F.,
 ( 4, 2, 4 ),
 ( 0.000000000000000000, 0.4999999999999991118, 1.000000000000000000 ),
 .UNSPECIFIED. ) ;
#28642 = CARTESIAN_POINT ( 'NONE',  ( 11.90425819896749893, -5.255890247626999745, 7.263238376356399684 ) ) ;
#28643 = ORIENTED_EDGE ( 'NONE', *, *, #10664, .F. ) ;
#28644 = CARTESIAN_POINT ( 'NONE',  ( 23.66004879239100234, 0.000000000000000000, 0.000000000000000000 ) ) ;
#28645 = ORIENTED_EDGE ( 'NONE', *, *, #29687, .T. ) ;
#28646 = CARTESIAN_POINT ( 'NONE',  ( 9.500595280412998278, 2.334550724494000029, -7.977056617806000283 ) ) ;
#28647 = DIRECTION ( 'NONE',  ( -1.000000000000000000, 0.000000000000000000, 0.000000000000000000 ) ) ;
#28648 = DIRECTION ( 'NONE',  ( -1.000000000000000000, 0.000000000000000000, 0.000000000000000000 ) ) ;
#28649 = CARTESIAN_POINT ( 'NONE',  ( 12.72249460523637410, 1.880133632676046718, -12.57461455596142841 ) ) ;
#28650 = CARTESIAN_POINT ( 'NONE',  ( 11.40346005378009941, -3.213042707518099839, 7.920222357891399945 ) ) ;
#28651 = ORIENTED_EDGE ( 'NONE', *, *, #64369, .T. ) ;
#28652 = CARTESIAN_POINT ( 'NONE',  ( 7.536393842410557653, 4.984327542422680501, 8.445161314658211182 ) ) ;
#28653 = VERTEX_POINT ( 'NONE', #44552 ) ;
#28654 = CARTESIAN_POINT ( 'NONE',  ( 7.416894353206999746, -3.448181789123000218, 9.222458996124998976 ) ) ;
#28655 = CARTESIAN_POINT ( 'NONE',  ( 24.04055934518150650, 9.302271743222915390, 9.232431401971632923 ) ) ;
#28656 = ORIENTED_EDGE ( 'NONE', *, *, #6687, .T. ) ;
#28657 = CARTESIAN_POINT ( 'NONE',  ( 12.43868857148329177, -1.859375588728228390, -12.46205283878465053 ) ) ;
#28658 = CARTESIAN_POINT ( 'NONE',  ( 10.28026357027499849, 4.985299147223100746, 7.309904858193100097 ) ) ;
#28659 = CARTESIAN_POINT ( 'NONE',  ( 10.16000000000000014, 4.496968146123999865, -8.755198255949000696 ) ) ;
#28660 = CARTESIAN_POINT ( 'NONE',  ( 6.534193173016667799, -1.460959015002474493, 0.3926218265389144757 ) ) ;
#28661 = CARTESIAN_POINT ( 'NONE',  ( 18.29014736449600420, -11.95934322008999828, 3.530971945262000311 ) ) ;
#28662 = CARTESIAN_POINT ( 'NONE',  ( 8.027701659444524296, -5.080332885338415316, 8.330387188616123595 ) ) ;
#28663 = CARTESIAN_POINT ( 'NONE',  ( 12.23542143184363695, -2.757395375068925958, -13.61543998564092028 ) ) ;
#28664 = CARTESIAN_POINT ( 'NONE',  ( 18.06882650195508333, 0.3560396104572006726, -12.69328656575056691 ) ) ;
#28665 = CARTESIAN_POINT ( 'NONE',  ( 0.07500030076246999577, 0.000000000000000000, -2.649999808707999893 ) ) ;
#28666 = CARTESIAN_POINT ( 'NONE',  ( 10.81764560330029923, -3.650429500487800460, -6.414140625063999401 ) ) ;
#28667 = EDGE_CURVE ( 'NONE', #24349, #41143, #5152, .T. ) ;
#28669 = EDGE_CURVE ( 'NONE', #55276, #56202, #5732, .T. ) ;
#28668 = CARTESIAN_POINT ( 'NONE',  ( 9.294718325437999695, 4.148133901461999784, 9.337478696773001019 ) ) ;
#28670 = ORIENTED_EDGE ( 'NONE', *, *, #68357, .T. ) ;
#28671 = SURFACE_SIDE_STYLE ('',( #34611 ) ) ;
#28672 = CARTESIAN_POINT ( 'NONE',  ( 24.35365242081700288, -10.90899669668998584, 3.315896191951999583 ) ) ;
#28673 = CARTESIAN_POINT ( 'NONE',  ( 8.099999999999999645, 0.000000000000000000, -11.84999999999999964 ) ) ;
#28674 = CARTESIAN_POINT ( 'NONE',  ( 23.73581744296999929, -3.554601233002000260, 13.41645131342000141 ) ) ;
#28675 = CARTESIAN_POINT ( 'NONE',  ( 17.92180752009628009, 1.993817408553323789, 12.55519104945816977 ) ) ;
#28676 = CARTESIAN_POINT ( 'NONE',  ( 11.02029022880999953, 5.784022792365999699, 5.014076608209000696 ) ) ;
#28677 = CARTESIAN_POINT ( 'NONE',  ( 10.96080777006000062, 2.054568739078000306, 7.810084630238000258 ) ) ;
#28678 = AXIS2_PLACEMENT_3D ( 'NONE', #65235, #41769, #46680 ) ;
#28679 = CARTESIAN_POINT ( 'NONE',  ( 10.74006601915162662, -4.042412777185713679, 6.626081523287773223 ) ) ;
#28680 = CARTESIAN_POINT ( 'NONE',  ( 3.899999681170999821, 0.000000000000000000, 0.000000000000000000 ) ) ;
#28681 = ORIENTED_EDGE ( 'NONE', *, *, #2664, .T. ) ;
#28682 = CARTESIAN_POINT ( 'NONE',  ( 12.26933621011917275, -2.178034692540640638, 12.52080028461861794 ) ) ;
#28683 = CARTESIAN_POINT ( 'NONE',  ( 9.705671671056999017, -4.990538396979200542, -7.666361006367900188 ) ) ;
#28684 = CARTESIAN_POINT ( 'NONE',  ( 24.61098151538899970, -3.467630292425999627, -12.10773253045999986 ) ) ;
#28685 = EDGE_CURVE ( 'NONE', #55873, #3842, #46023, .T. ) ;
#28686 = LINE ( 'NONE', #7696, #30966 ) ;
#28687 = AXIS2_PLACEMENT_3D ( 'NONE', #11403, #64879, #34133 ) ;
#28688 = B_SPLINE_CURVE_WITH_KNOTS ( 'NONE', 3,
 ( #56064, #23218, #17981, #49433 ),
 .UNSPECIFIED., .F., .F.,
 ( 4, 4 ),
 ( 0.000000000000000000, 1.000000000000000000 ),
 .UNSPECIFIED. ) ;
#28689 = EDGE_CURVE ( 'NONE', #66385, #57125, #38465, .T. ) ;
#28690 = CARTESIAN_POINT ( 'NONE',  ( 11.52733460557258915, 4.206337284815599986, -8.761245990815998752 ) ) ;
#28691 = CARTESIAN_POINT ( 'NONE',  ( 12.67437701660358762, -0.7076089047904881024, 12.58011506138061009 ) ) ;
#28692 = CARTESIAN_POINT ( 'NONE',  ( 7.828420280408998622, 5.524123123935000379, 6.910361319981999095 ) ) ;
#28693 = CARTESIAN_POINT ( 'NONE',  ( 9.347254965556000883, 4.028327103212000715, 9.469449669541999626 ) ) ;
#28694 = CARTESIAN_POINT ( 'NONE',  ( 12.37468788209170611, 2.046657606614539215, 12.54569895759544984 ) ) ;
#28695 = ORIENTED_EDGE ( 'NONE', *, *, #31325, .T. ) ;
#28696 = CARTESIAN_POINT ( 'NONE',  ( 9.535554719593998030, 3.927090956378999742, -9.230892435423001530 ) ) ;
#28697 = CARTESIAN_POINT ( 'NONE',  ( 10.81349144726329925, 3.261052100888700345, -6.457276458983999490 ) ) ;
#28698 = CARTESIAN_POINT ( 'NONE',  ( 5.354219950104666559, 1.237977404532700332, 0.8781525088298994808 ) ) ;
#28700 = CARTESIAN_POINT ( 'NONE',  ( 17.93439305966544950, -0.4967428619541083279, 12.68692192486686743 ) ) ;
#28699 = CARTESIAN_POINT ( 'NONE',  ( 8.625066940379999991, -3.117370956513999758, 8.662188901935000018 ) ) ;
#28701 = CARTESIAN_POINT ( 'NONE',  ( 10.56525461470299909, -4.973404788313100511, 7.252360304610999897 ) ) ;
#28702 = CARTESIAN_POINT ( 'NONE',  ( 11.39210538575740017, -3.157545584346100220, -7.298582155985900322 ) ) ;
#28703 = VERTEX_POINT ( 'NONE', #17968 ) ;
#28704 = CARTESIAN_POINT ( 'NONE',  ( 2.020703038683000052, -2.100427248507999778, 2.706108474410000131 ) ) ;
#28705 = CARTESIAN_POINT ( 'NONE',  ( 18.29983863915590803, -1.925365984851983070, 12.21183827962646085 ) ) ;
#28706 = CARTESIAN_POINT ( 'NONE',  ( 11.07435795695566583, -2.750000000000000000, 7.192559817601734906 ) ) ;
#28707 = CARTESIAN_POINT ( 'NONE',  ( 17.81487012555341209, -3.068783844980979669, 13.53623303301404590 ) ) ;
#28708 = FACE_OUTER_BOUND ( 'NONE', #43567, .T. ) ;
#28709 = CARTESIAN_POINT ( 'NONE',  ( 12.09654996457813603, -2.673023974430121630, 13.74245554503370492 ) ) ;
#28710 = CARTESIAN_POINT ( 'NONE',  ( 9.893930206848997599, 2.750000000000000000, 7.500000000000000000 ) ) ;
#28711 = DIRECTION ( 'NONE',  ( -1.000000000000000000, 0.000000000000000000, 0.000000000000000000 ) ) ;
#28712 = CARTESIAN_POINT ( 'NONE',  ( 13.32310803393400178, -12.20807901729000022, -2.049767542799999731 ) ) ;
#28713 = ORIENTED_EDGE ( 'NONE', *, *, #27244, .T. ) ;
#28714 = CARTESIAN_POINT ( 'NONE',  ( 10.98768472638000127, 7.408460564924999936, -6.159405844198999169 ) ) ;
#28715 = DIRECTION ( 'NONE',  ( -1.000000000000000000, -3.552713678732000035E-14, 3.552713678732000035E-14 ) ) ;
#28716 = CARTESIAN_POINT ( 'NONE',  ( 17.72013721789504714, 1.891648809754047367, -13.78386988243240907 ) ) ;
#28717 = AXIS2_PLACEMENT_3D ( 'NONE', #54663, #2554, #2223 ) ;
#28718 = CYLINDRICAL_SURFACE ( 'NONE', #25876, 2.000000000000001332 ) ;
#28719 = CARTESIAN_POINT ( 'NONE',  ( 5.500000000000000000, -0.2500000000000000000, 3.149999999999999911 ) ) ;
#28720 = EDGE_LOOP ( 'NONE', ( #65156, #41430, #38113 ) ) ;
#28721 = CARTESIAN_POINT ( 'NONE',  ( 14.39999999971666789, 12.11987147417543298, -3.159800697744812314 ) ) ;
#28722 = CARTESIAN_POINT ( 'NONE',  ( 18.11306383842991252, 2.218305400803588512, -12.51277866499342650 ) ) ;
#28723 = CARTESIAN_POINT ( 'NONE',  ( 9.903950872528001881, 5.205009505618999555, 6.747225973806000532 ) ) ;
#28724 = PRESENTATION_LAYER_ASSIGNMENT (  '', '', ( #5250 ) ) ;
#28725 = CARTESIAN_POINT ( 'NONE',  ( 11.48641235500450009, 3.260080192309100067, 8.177841818594698609 ) ) ;
#28726 = EDGE_CURVE ( 'NONE', #10649, #20272, #22607, .T. ) ;
#28727 = EDGE_CURVE ( 'NONE', #68990, #53568, #34930, .T. ) ;
#28728 = CARTESIAN_POINT ( 'NONE',  ( 8.640591541102308426, -5.000946319700332765, 6.106569738443371698 ) ) ;
#28729 = CARTESIAN_POINT ( 'NONE',  ( 9.392900668365001593, -2.713627063504739478, -7.026974105800378290 ) ) ;
#28730 = VECTOR ( 'NONE', #44687, 1000.000000000000000 ) ;
#28731 = CARTESIAN_POINT ( 'NONE',  ( 10.98956486188273551, -6.636233809049309151, 5.388476118166376061 ) ) ;
#28732 = CARTESIAN_POINT ( 'NONE',  ( 3.500000000000000000, -3.200000000000000178, 0.000000000000000000 ) ) ;
#28733 = CARTESIAN_POINT ( 'NONE',  ( 12.19311196923565710, -2.627115700264358367, 12.42106741838665585 ) ) ;
#28734 = ORIENTED_EDGE ( 'NONE', *, *, #65103, .T. ) ;
#28735 = CARTESIAN_POINT ( 'NONE',  ( 7.331802703852692282, 3.864187756835510967, 9.236377466553157944 ) ) ;
#28736 = ORIENTED_EDGE ( 'NONE', *, *, #57433, .T. ) ;
#28737 = AXIS2_PLACEMENT_3D ( 'NONE', #42447, #32312, #27400 ) ;
#28738 = CARTESIAN_POINT ( 'NONE',  ( 18.08776130068898524, -2.172968270232229493, 13.73740491327006197 ) ) ;
#28739 = CARTESIAN_POINT ( 'NONE',  ( 10.91195257254739914, -5.227167235646000165, -7.856899084262298771 ) ) ;
#28740 = ORIENTED_EDGE ( 'NONE', *, *, #11814, .F. ) ;
#28741 = ORIENTED_EDGE ( 'NONE', *, *, #8608, .T. ) ;
#28742 = CARTESIAN_POINT ( 'NONE',  ( 24.73255430586192816, -3.116067653016331818, -11.77907593398745867 ) ) ;
#28743 = DIRECTION ( 'NONE',  ( 1.000000000000000000, 0.000000000000000000, 0.000000000000000000 ) ) ;
#28744 = CARTESIAN_POINT ( 'NONE',  ( 23.59999462723899910, 13.22316330987000121, -4.267799687262000319 ) ) ;
#28745 = LINE ( 'NONE', #50061, #57695 ) ;
#28746 = FACE_BOUND ( 'NONE', #12053, .T. ) ;
#28747 = CARTESIAN_POINT ( 'NONE',  ( 24.30000000000000071, -11.49391741900999975, -4.090215442373000165 ) ) ;
#28748 = CARTESIAN_POINT ( 'NONE',  ( 11.44795901272999927, 3.583381594953999549, -11.14153199795000049 ) ) ;
#28749 = CIRCLE ( 'NONE', #35422, 1.350000000000000533 ) ;
#28750 = CARTESIAN_POINT ( 'NONE',  ( 11.10061802256000085, -3.093055606601000207, -6.153681532251999542 ) ) ;
#28751 = CARTESIAN_POINT ( 'NONE',  ( 17.55505043854147118, -3.125000000000000000, 13.52084414783465682 ) ) ;
#28752 = ADVANCED_FACE ( 'NONE', ( #22157 ), #23737, .T. ) ;
#28754 = EDGE_CURVE ( 'NONE', #21149, #45407, #41604, .T. ) ;
#28753 =( NAMED_UNIT ( * ) PLANE_ANGLE_UNIT ( ) SI_UNIT ( $, .RADIAN. ) );
#28755 = EDGE_LOOP ( 'NONE', ( #6969, #66097, #47878, #43606 ) ) ;
#28756 = CARTESIAN_POINT ( 'NONE',  ( 11.04677151279999947, -2.764386413791999786, -5.039776830043000366 ) ) ;
#28757 = APPLICATION_PROTOCOL_DEFINITION ( 'draft international standard', 'automotive_design', 1998, #38704 ) ;
#28758 = EDGE_CURVE ( 'NONE', #44831, #13445, #39287, .T. ) ;
#28759 = CARTESIAN_POINT ( 'NONE',  ( 10.62716797183172268, 3.242337246279118013, -4.769350230161790272 ) ) ;
#28760 = CARTESIAN_POINT ( 'NONE',  ( 10.33385424252000107, -4.803082529331999417, 5.018848833410999966 ) ) ;
#28761 = CARTESIAN_POINT ( 'NONE',  ( 7.492958774445000358, 8.174261230744999551, 4.512457914278000359 ) ) ;
#28762 = CARTESIAN_POINT ( 'NONE',  ( 10.01364655415099847, 4.619310611972400338, -8.619302797893999113 ) ) ;
#28763 = CARTESIAN_POINT ( 'NONE',  ( 12.18472169747684575, 2.421093590824782815, 13.68984525495557314 ) ) ;
#28764 = CARTESIAN_POINT ( 'NONE',  ( 10.89228096335999929, -3.998355205482000851, 9.261304730013998565 ) ) ;
#28765 = ORIENTED_EDGE ( 'NONE', *, *, #66623, .F. ) ;
#28766 = CARTESIAN_POINT ( 'NONE',  ( 7.900104261408000816, 3.351183067932000270, -6.316134894229000096 ) ) ;
#28767 = CARTESIAN_POINT ( 'NONE',  ( 12.52839348839893674, -0.5608030988280898743, 13.88477341743901938 ) ) ;
#28768 = EDGE_LOOP ( 'NONE', ( #61034, #35616, #11289, #2932 ) ) ;
#28769 = CARTESIAN_POINT ( 'NONE',  ( 12.83143828159500188, 11.44347076768000093, -4.696252053897000067 ) ) ;
#28770 = CARTESIAN_POINT ( 'NONE',  ( 10.67500447327561908, -2.650284540010996004, 7.500001951671615430 ) ) ;
#28771 = CARTESIAN_POINT ( 'NONE',  ( 23.99048274734800046, -3.573011467988000067, -12.95903152520000035 ) ) ;
#28772 = DIRECTION ( 'NONE',  ( 0.000000000000000000, 0.8648648648648720183, 0.5020047465136825426 ) ) ;
#28773 = CONICAL_SURFACE ( 'NONE', #67815, 0.6499999954790001144, 0.7853981633972997312 ) ;
#28774 = EDGE_CURVE ( 'NONE', #44210, #14053, #3720, .T. ) ;
#28775 = CARTESIAN_POINT ( 'NONE',  ( 9.635004719593998956, 2.334550724494000029, -7.977056617806000283 ) ) ;
#28776 = CARTESIAN_POINT ( 'NONE',  ( 10.01059687351599692, 4.629523725463622341, -8.592232985442825210 ) ) ;
#28777 = CARTESIAN_POINT ( 'NONE',  ( 10.95868203502999982, 8.167115842968998507, -6.508568339202000175 ) ) ;
#28778 = B_SPLINE_CURVE_WITH_KNOTS ( 'NONE', 3,
 ( #62585, #25539, #3852, #67831, #14372, #14026 ),
 .UNSPECIFIED., .F., .F.,
 ( 4, 2, 4 ),
 ( 0.000000000000000000, 0.5000000000000000000, 1.000000000000000000 ),
 .UNSPECIFIED. ) ;
#28779 = DIRECTION ( 'NONE',  ( 1.000000000000000000, 0.000000000000000000, 0.000000000000000000 ) ) ;
#28780 = DIRECTION ( 'NONE',  ( 0.000000000000000000, 1.000000000000000000, 0.000000000000000000 ) ) ;
#28781 = VECTOR ( 'NONE', #8299, 1000.000000000000000 ) ;
#28782 = LINE ( 'NONE', #38914, #31068 ) ;
#28783 = CARTESIAN_POINT ( 'NONE',  ( 9.480151033051999576, -4.233164088428999605, -6.141918726850000176 ) ) ;
#28784 = CARTESIAN_POINT ( 'NONE',  ( 10.55518582084299872, 3.433275964779900047, -6.844925608615599621 ) ) ;
#28785 = CARTESIAN_POINT ( 'NONE',  ( 12.15889392806725056, 0.3761765224702128263, 12.59508068833789451 ) ) ;
#28786 = CARTESIAN_POINT ( 'NONE',  ( 10.85168717260509830, 3.386210853237200169, -8.501809683958001074 ) ) ;
#28787 = CARTESIAN_POINT ( 'NONE',  ( 9.938608878791999501, 3.772542739612499751, -6.521682313853199631 ) ) ;
#28789 = CARTESIAN_POINT ( 'NONE',  ( 10.42441090035999984, -2.988250767850000322, 4.759068290708999172 ) ) ;
#28788 = CARTESIAN_POINT ( 'NONE',  ( 16.00429364930199938, -8.559608311085998622, -7.983357056237001537 ) ) ;
#28790 = CARTESIAN_POINT ( 'NONE',  ( 7.717918988116000634, 2.852331522235000083, 6.784355039830999523 ) ) ;
#28791 = ORIENTED_EDGE ( 'NONE', *, *, #58026, .F. ) ;
#28792 = VECTOR ( 'NONE', #17974, 1000.000000000000000 ) ;
#28793 = CARTESIAN_POINT ( 'NONE',  ( 11.27234208742519783, 3.445253572379500362, 6.627995351445298944 ) ) ;
#28794 = CARTESIAN_POINT ( 'NONE',  ( 9.877259503622999759, -2.207992199716000137, 7.624813542847999059 ) ) ;
#28795 = CARTESIAN_POINT ( 'NONE',  ( 8.871822372493998188, 3.671800173070400408, 6.426348619097999482 ) ) ;
#28796 = CARTESIAN_POINT ( 'NONE',  ( 9.961445400145626294, 4.347277725169313989, -6.696924380570436597 ) ) ;
#28797 = B_SPLINE_CURVE_WITH_KNOTS ( 'NONE', 3,
 ( #15783, #48284, #37113, #390, #63317, #58427, #42700, #32223, #64695, #11221, #16462, #16804, #37794, #9846, #7013, #39177, #17509, #12264, #12609, #55609, #54212, #60500, #2124, #7355, #45120, #28700, #43738, #6312, #59458, #18201, #33940, #49664, #17151, #7710, #29049, #55261, #27658, #50015, #1084, #38483, #33593, #23443 ),
 .UNSPECIFIED., .F., .F.,
 ( 4, 2, 2, 2, 2, 2, 2, 2, 2, 2, 2, 2, 2, 1, 2, 2, 2, 2, 2, 1, 2, 4 ),
 ( 0.4997863768847483068, 0.5623130797741622278, 0.6248397826635760932, 0.6404714583859291155, 0.6561031341082821378, 0.6873664855529879603, 0.7029981612753410936, 0.7186298369976940048, 0.7264456748588704604, 0.7342615127200470271, 0.7498931884424000494, 0.7811565398871087584, 0.7889723777482845479, 0.7967882156094603374, 0.8124198913318116944, 0.8280515670541630513, 0.8436832427765145193, 0.8749465942212126812, 0.8905782699435618177, 0.9062099456659109542, 0.9374732971106091162, 1.000000000000000000 ),
 .UNSPECIFIED. ) ;
#28798 = VECTOR ( 'NONE', #11024, 1000.000000000000227 ) ;
#28799 = CARTESIAN_POINT ( 'NONE',  ( 9.910792656537999790, -3.869344906782000049, 5.882544796414999944 ) ) ;
#28800 = DIRECTION ( 'NONE',  ( 0.000000000000000000, -0.1218274111675002047, 0.9925512993736015366 ) ) ;
#28802 = CARTESIAN_POINT ( 'NONE',  ( 11.61689913334100055, 3.709679022145000005, -12.00356807880999988 ) ) ;
#28801 = UNCERTAINTY_MEASURE_WITH_UNIT (LENGTH_MEASURE( 1.000000000000000082E-05 ), #13097, 'distance_accuracy_value', 'NONE');
#28803 = ORIENTED_EDGE ( 'NONE', *, *, #40122, .F. ) ;
#28804 = CARTESIAN_POINT ( 'NONE',  ( 9.227380199234000102, -2.867101906753999785, -7.357604921762999517 ) ) ;
#28805 = CARTESIAN_POINT ( 'NONE',  ( 9.802263540183334456, -5.092232985442821658, -6.870476274536374994 ) ) ;
#28806 = CARTESIAN_POINT ( 'NONE',  ( 5.750405406626000193, -0.9021507525358000157, -1.158728426834999992 ) ) ;
#28807 = CARTESIAN_POINT ( 'NONE',  ( 10.33253786428999987, 2.899999999999999911, 6.571291218949999902 ) ) ;
#28808 = CARTESIAN_POINT ( 'NONE',  ( 4.500000000000000000, 0.000000000000000000, 0.000000000000000000 ) ) ;
#28809 = EDGE_CURVE ( 'NONE', #67604, #8734, #62052, .T. ) ;
#28810 = EDGE_CURVE ( 'NONE', #55718, #62373, #8690, .T. ) ;
#28811 = CARTESIAN_POINT ( 'NONE',  ( 10.28441772631199846, 4.372518460886800185, -8.266796319406900295 ) ) ;
#28812 = CARTESIAN_POINT ( 'NONE',  ( 10.95319771135661391, 5.088176249045773147, 4.928389127490998334 ) ) ;
#28813 = CARTESIAN_POINT ( 'NONE',  ( 9.482733921870000415, -2.757678812098000254, -6.584768124342000206 ) ) ;
#28814 = CARTESIAN_POINT ( 'NONE',  ( 9.725191424783300675, -2.649754699899359522, 7.500009801425228773 ) ) ;
#28815 = ORIENTED_EDGE ( 'NONE', *, *, #44054, .F. ) ;
#28816 = FACE_BOUND ( 'NONE', #15076, .T. ) ;
#28817 = VECTOR ( 'NONE', #63190, 1000.000000000000000 ) ;
#28818 = CARTESIAN_POINT ( 'NONE',  ( 12.70954970454857502, -0.7242550212506043694, -13.98125389334239443 ) ) ;
#28819 = CARTESIAN_POINT ( 'NONE',  ( 8.599999952505998024, 4.000000000000000000, -8.249999993641800700 ) ) ;
#28820 = CARTESIAN_POINT ( 'NONE',  ( 11.52285868696541549, 4.059810388505518119, -8.771870505746530711 ) ) ;
#28821 = CARTESIAN_POINT ( 'NONE',  ( 13.31007343199765813, -11.51543253752115525, -1.765677284072121989 ) ) ;
#28822 = CARTESIAN_POINT ( 'NONE',  ( 6.999999999999999112, 10.39726215437233492, 4.179831230459656766 ) ) ;
#28823 = LINE ( 'NONE', #2572, #19494 ) ;
#28824 = VERTEX_POINT ( 'NONE', #14098 ) ;
#28825 = CARTESIAN_POINT ( 'NONE',  ( 24.30000000000000071, -9.289189189551001036, 7.908916752675001050 ) ) ;
#28826 = CARTESIAN_POINT ( 'NONE',  ( 17.88894803995536975, 3.166162608671027723, -13.63728156593011498 ) ) ;
#28827 = EDGE_LOOP ( 'NONE', ( #14518, #44334, #17894, #29880 ) ) ;
#28828 = CARTESIAN_POINT ( 'NONE',  ( 8.476519155276927009, 5.080278632455591747, 8.330433920097927825 ) ) ;
#28829 = CARTESIAN_POINT ( 'NONE',  ( 24.44496264144000364, 8.810483598181999554, -8.810508341310001157 ) ) ;
#28830 = AXIS2_PLACEMENT_3D ( 'NONE', #13326, #28711, #39190 ) ;
#28831 = CARTESIAN_POINT ( 'NONE',  ( 8.307195280408999238, 5.473983809665999622, -8.180077404516000072 ) ) ;
#28832 = CARTESIAN_POINT ( 'NONE',  ( 24.52306339378907296, 8.782889706257643425, -8.926437547059927979 ) ) ;
#28833 = CARTESIAN_POINT ( 'NONE',  ( 11.84388784977539899, -5.255745690988000263, -7.428242901739219306 ) ) ;
#28834 = CARTESIAN_POINT ( 'NONE',  ( 18.06844660307443817, 0.3566172609805220994, -12.69326555881922047 ) ) ;
#28835 = STYLED_ITEM ( 'NONE', ( #6575 ), #52802 ) ;
#28836 = CARTESIAN_POINT ( 'NONE',  ( 11.04166666666869467, -2.793604566011342882, 8.411630010703568416 ) ) ;
#28837 = ORIENTED_EDGE ( 'NONE', *, *, #51525, .T. ) ;
#28838 = CARTESIAN_POINT ( 'NONE',  ( 8.348093183609000434, 4.599999999999999645, -6.056236567608999977 ) ) ;
#28839 = CARTESIAN_POINT ( 'NONE',  ( 18.09719409069527885, -2.811143122832467700, -13.60247644589073879 ) ) ;
#28841 = EDGE_CURVE ( 'NONE', #69130, #60334, #15378, .T. ) ;
#28840 = CARTESIAN_POINT ( 'NONE',  ( 8.549914158773001205, 2.141799395716999843, -7.895788736628000848 ) ) ;
#28842 = ORIENTED_EDGE ( 'NONE', *, *, #63221, .T. ) ;
#28843 = AXIS2_PLACEMENT_3D ( 'NONE', #41089, #35842, #30946 ) ;
#28844 = CARTESIAN_POINT ( 'NONE',  ( 10.60518955639999916, 5.343965917319999370, -7.731522121091999544 ) ) ;
#28845 = ADVANCED_FACE ( 'NONE', ( #3586 ), #13070, .F. ) ;
#28846 = ORIENTED_EDGE ( 'NONE', *, *, #57706, .F. ) ;
#28847 = CARTESIAN_POINT ( 'NONE',  ( 9.280051052051998539, 4.985712601322500603, 7.307093369932900373 ) ) ;
#28848 = CARTESIAN_POINT ( 'NONE',  ( 18.06139486453147569, -2.995281757671043987, -12.23880324656448870 ) ) ;
#28849 = CARTESIAN_POINT ( 'NONE',  ( 9.446013540182333301, 3.000416447002273834, 6.731816600031359066 ) ) ;
#28850 = CARTESIAN_POINT ( 'NONE',  ( 24.54223752889256360, -3.611770689511173860, -12.30300795109232581 ) ) ;
#28851 = CARTESIAN_POINT ( 'NONE',  ( 11.80585503023100102, -11.57020517019000039, -1.758699328329000222 ) ) ;
#28852 = AXIS2_PLACEMENT_3D ( 'NONE', #30776, #8765, #46516 ) ;
#28853 = CARTESIAN_POINT ( 'NONE',  ( 9.358051052051999719, 4.850870049477099322, 7.333482423122699601 ) ) ;
#28854 = CARTESIAN_POINT ( 'NONE',  ( 7.682876674207999912, -9.044797463044000452, -5.468325094282000087 ) ) ;
#28855 = VERTEX_POINT ( 'NONE', #8160 ) ;
#28856 = CARTESIAN_POINT ( 'NONE',  ( 6.899999691988000450, 12.20988339176000004, 3.111064831550000243 ) ) ;
#28857 = CARTESIAN_POINT ( 'NONE',  ( 11.20537028040999949, 2.688545137295000220, -8.273930556758998023 ) ) ;
#28858 = CARTESIAN_POINT ( 'NONE',  ( 10.59393020684899867, 5.250000000000000000, -7.500000000000000000 ) ) ;
#28859 = CARTESIAN_POINT ( 'NONE',  ( 12.15817878876224434, 2.188143349582272634, -13.82794795582454483 ) ) ;
#28860 = VECTOR ( 'NONE', #21439, 1000.000000000000000 ) ;
#28861 = CARTESIAN_POINT ( 'NONE',  ( 11.34393020684979980, -5.250000000000000000, 7.500000000000000000 ) ) ;
#28862 = CARTESIAN_POINT ( 'NONE',  ( 9.657547180956999711, -5.333447643521000536, 6.049925825719999928 ) ) ;
#28863 = EDGE_CURVE ( 'NONE', #14563, #54068, #8846, .T. ) ;
#28864 = CARTESIAN_POINT ( 'NONE',  ( 18.05115593671926533, -0.5330308249010320409, 13.98985951701901520 ) ) ;
#28865 = CARTESIAN_POINT ( 'NONE',  ( 17.94293712292327925, 0.4901002083121274722, 13.88836944287485586 ) ) ;
#28866 = EDGE_LOOP ( 'NONE', ( #25021, #32497, #41457, #21573 ) ) ;
#28867 = ORIENTED_EDGE ( 'NONE', *, *, #30253, .F. ) ;
#28868 = CARTESIAN_POINT ( 'NONE',  ( 8.897989158775001073, 4.990139824845000405, -9.121472988377998803 ) ) ;
#28869 = CARTESIAN_POINT ( 'NONE',  ( 12.53102142821679976, -0.5618070541888602332, 13.88471645277480171 ) ) ;
#28870 = CARTESIAN_POINT ( 'NONE',  ( 12.21880568483910245, -2.282463263798835129, 13.71720984526819009 ) ) ;
#28871 = CARTESIAN_POINT ( 'NONE',  ( 5.100000001045000175, 0.000000000000000000, 0.000000000000000000 ) ) ;
#28872 = CARTESIAN_POINT ( 'NONE',  ( 8.924956853209002006, -4.158911960977000000, 5.873536005760000123 ) ) ;
#28873 = DIRECTION ( 'NONE',  ( 0.000000000000000000, 0.000000000000000000, -1.000000000000000000 ) ) ;
#28875 = CARTESIAN_POINT ( 'NONE',  ( 10.96239535880000027, -5.423117484767999485, 4.905496954963999734 ) ) ;
#28874 = FACE_OUTER_BOUND ( 'NONE', #10073, .T. ) ;
#28876 = CARTESIAN_POINT ( 'NONE',  ( 11.04384236319999957, -5.374509385214000012, 5.035088906224999938 ) ) ;
#28877 = VERTEX_POINT ( 'NONE', #29506 ) ;
#28878 = B_SPLINE_CURVE_WITH_KNOTS ( 'NONE', 3,
 ( #56589, #67404, #45075, #39827 ),
 .UNSPECIFIED., .F., .F.,
 ( 4, 4 ),
 ( 0.000000000000000000, 1.000000000000000000 ),
 .UNSPECIFIED. ) ;
#28879 = CARTESIAN_POINT ( 'NONE',  ( 7.315000000000000391, 2.649999999999999911, -7.500000000000000000 ) ) ;
#28880 = FACE_OUTER_BOUND ( 'NONE', #67165, .T. ) ;
#28881 = CARTESIAN_POINT ( 'NONE',  ( 10.90145123840999908, -5.099999999122000638, 5.151026147719999670 ) ) ;
#28882 = CARTESIAN_POINT ( 'NONE',  ( 12.27274573047528072, -0.3283020094990616311, 12.69430739907260630 ) ) ;
#28883 = CIRCLE ( 'NONE', #63479, 1.000000000000001332 ) ;
#28884 = CARTESIAN_POINT ( 'NONE',  ( 17.93744643711337972, -2.994789699036757735, -12.32241545780482816 ) ) ;
#28885 = ORIENTED_EDGE ( 'NONE', *, *, #44843, .F. ) ;
#28887 = DIRECTION ( 'NONE',  ( -0.7071067751363951936, 0.7071067872366950668, -8.276005153174941152E-08 ) ) ;
#28886 = CARTESIAN_POINT ( 'NONE',  ( 7.775620559622000272, -4.636725880537000855, 9.378965771357000492 ) ) ;
#28888 = CARTESIAN_POINT ( 'NONE',  ( 9.012204719595001023, 3.161445734422999809, -6.178649910536000434 ) ) ;
#28889 = CARTESIAN_POINT ( 'NONE',  ( 12.39809172042342311, -2.025537470422473785, 13.76271392731540821 ) ) ;
#28890 = AXIS2_PLACEMENT_3D ( 'NONE', #4985, #31567, #15486 ) ;
#28891 = DIRECTION ( 'NONE',  ( 0.000000000000000000, -1.000000000000000000, 0.000000000000000000 ) ) ;
#28892 = LINE ( 'NONE', #60683, #17546 ) ;
#28893 = CARTESIAN_POINT ( 'NONE',  ( 3.362977181498000512, -1.794707112228999923, -3.302705535711000007 ) ) ;
#28894 = VERTEX_POINT ( 'NONE', #56399 ) ;
#28895 = CIRCLE ( 'NONE', #41155, 13.10000000000000320 ) ;
#28896 = EDGE_CURVE ( 'NONE', #51514, #12675, #52781, .T. ) ;
#28897 = EDGE_CURVE ( 'NONE', #8552, #14358, #12562, .T. ) ;
#28898 = CARTESIAN_POINT ( 'NONE',  ( 12.12656756701885641, -0.2537702651956292854, -12.59744904646397679 ) ) ;
#28899 = CARTESIAN_POINT ( 'NONE',  ( 10.90437356726000040, -2.900476673752999890, 5.132566153004000320 ) ) ;
#28900 = CARTESIAN_POINT ( 'NONE',  ( 23.61456421552348672, -13.25068299535432459, -4.104339497028676398 ) ) ;
#28901 = CARTESIAN_POINT ( 'NONE',  ( 24.30857393632600250, 3.216436940933999900, -12.15172254432999921 ) ) ;
#28902 = VERTEX_POINT ( 'NONE', #28814 ) ;
#28903 = CARTESIAN_POINT ( 'NONE',  ( 6.782034520496999619, -0.06619345247263999643, 1.320670790275000117 ) ) ;
#28904 = EDGE_CURVE ( 'NONE', #23570, #23499, #14808, .T. ) ;
#28905 = ADVANCED_FACE ( 'NONE', ( #45227 ), #40730, .F. ) ;
#28906 = CARTESIAN_POINT ( 'NONE',  ( 7.109360841228999917, 5.292420046468999217, -7.844702366751000966 ) ) ;
#28908 = CARTESIAN_POINT ( 'NONE',  ( 10.79415884302793316, 2.685269952712994623, -7.853379249108686011 ) ) ;
#28907 = CARTESIAN_POINT ( 'NONE',  ( 8.563725384270323815, -3.755834718894938806, 5.775588430088804515 ) ) ;
#28909 = AXIS2_PLACEMENT_3D ( 'NONE', #31076, #53424, #52032 ) ;
#28910 = CARTESIAN_POINT ( 'NONE',  ( 10.63880513895979973, 5.150451045932999961, -6.860457220153399760 ) ) ;
#28911 = ORIENTED_EDGE ( 'NONE', *, *, #23539, .T. ) ;
#28912 = CARTESIAN_POINT ( 'NONE',  ( 12.79999998875598344, -11.49049412642037460, 4.802266170000438983 ) ) ;
#28913 = EDGE_LOOP ( 'NONE', ( #63039, #2145, #45503, #44233 ) ) ;
#28914 = CARTESIAN_POINT ( 'NONE',  ( 9.490131905446967053, -4.919265557633711872, 8.488500456889612522 ) ) ;
#28915 = CARTESIAN_POINT ( 'NONE',  ( 24.92743226742850382, -8.563809462501300374, -8.403983636214338304 ) ) ;
#28916 = CARTESIAN_POINT ( 'NONE',  ( 18.21574553171934596, 0.3008963210924943121, -13.99677033988233354 ) ) ;
#28917 = EDGE_LOOP ( 'NONE', ( #6700, #3096, #20577, #31578 ) ) ;
#28918 = CARTESIAN_POINT ( 'NONE',  ( 10.97828475743834531, 8.385142400385850792, -6.553559007601123199 ) ) ;
#28919 = CARTESIAN_POINT ( 'NONE',  ( 8.361784252019500485, 5.107027770526263666, 6.686924863581454659 ) ) ;
#28920 = CARTESIAN_POINT ( 'NONE',  ( 7.839139158769000026, 2.603157881926999817, -7.543458285860999979 ) ) ;
#28921 = CARTESIAN_POINT ( 'NONE',  ( 5.500000000000000000, -11.00717859340000082, -1.432487142323000118 ) ) ;
#28922 = CARTESIAN_POINT ( 'NONE',  ( 18.15015087270999672, -2.691082634310324462, 12.40501869838522708 ) ) ;
#28923 = ORIENTED_EDGE ( 'NONE', *, *, #52011, .T. ) ;
#28924 = CARTESIAN_POINT ( 'NONE',  ( 11.59999999999999964, -2.613168764257999932, -7.174999999999999822 ) ) ;
#28925 = CARTESIAN_POINT ( 'NONE',  ( 23.95204486579200420, -12.88042262741999977, -3.488172014188000158 ) ) ;
#28926 = APPLICATION_CONTEXT ( 'automotive_design' ) ;
#28927 = CARTESIAN_POINT ( 'NONE',  ( 16.10004050617000004, 4.849232186851351933, 11.59252887645442343 ) ) ;
#28928 = DIRECTION ( 'NONE',  ( 1.000000000000000000, 0.000000000000000000, 0.000000000000000000 ) ) ;
#28929 = ORIENTED_EDGE ( 'NONE', *, *, #42473, .F. ) ;
#28930 = DIRECTION ( 'NONE',  ( 0.000000000000000000, 0.000000000000000000, -1.000000000000000000 ) ) ;
#28931 = CARTESIAN_POINT ( 'NONE',  ( 8.883506238772763908, -3.863849893416519077, -6.466493704552774169 ) ) ;
#28932 = DIRECTION ( 'NONE',  ( 1.000000000000000000, 0.000000000000000000, 0.000000000000000000 ) ) ;
#28933 = CARTESIAN_POINT ( 'NONE',  ( 23.61469341658364840, -3.071268921750722303, -13.52731160624835027 ) ) ;
#28934 = CARTESIAN_POINT ( 'NONE',  ( 25.29989727901499919, -2.258942858049999725, -12.29419282279000036 ) ) ;
#28935 = B_SPLINE_CURVE_WITH_KNOTS ( 'NONE', 3,
 ( #12155, #34176, #6897, #65281 ),
 .UNSPECIFIED., .F., .F.,
 ( 4, 4 ),
 ( 0.000000000000000000, 0.8163836489557148024 ),
 .UNSPECIFIED. ) ;
#28936 = AXIS2_PLACEMENT_3D ( 'NONE', #25679, #63416, #15540 ) ;
#28937 = CARTESIAN_POINT ( 'NONE',  ( 12.37737328439355089, -0.4562271229319654342, -13.88993195058941410 ) ) ;
#28938 = CARTESIAN_POINT ( 'NONE',  ( 17.77951638133176360, -1.796077334879284892, 12.47133186514445491 ) ) ;
#28939 = ORIENTED_EDGE ( 'NONE', *, *, #9597, .T. ) ;
#28940 = CARTESIAN_POINT ( 'NONE',  ( 11.06967835872019812, -4.754733798270200928, -7.024326263066900111 ) ) ;
#28941 = EDGE_LOOP ( 'NONE', ( #59305, #6230, #62510, #28736 ) ) ;
#28942 = DIRECTION ( 'NONE',  ( -1.000000000000000000, 0.000000000000000000, 0.000000000000000000 ) ) ;
#28943 = CARTESIAN_POINT ( 'NONE',  ( 9.684729719592999331, 2.370176859044999862, -6.912649125838000508 ) ) ;
#28944 = CARTESIAN_POINT ( 'NONE',  ( 2.789820834103999836, 2.869509198118999738, 1.449990717411999919 ) ) ;
#28945 = CARTESIAN_POINT ( 'NONE',  ( 10.17310292480999934, -4.709171320598000143, -8.664883863910000983 ) ) ;
#28946 = EDGE_CURVE ( 'NONE', #67995, #23400, #40384, .T. ) ;
#28947 = CARTESIAN_POINT ( 'NONE',  ( 6.703329853547768558, -0.4976103889317664564, -1.434029154780907644 ) ) ;
#28948 = LINE ( 'NONE', #55498, #43961 ) ;
#28949 = CARTESIAN_POINT ( 'NONE',  ( 10.45746213570999927, -5.100000000000000533, -6.571291218949999902 ) ) ;
#28950 = VERTEX_POINT ( 'NONE', #68 ) ;
#28951 = EDGE_CURVE ( 'NONE', #34621, #49491, #52521, .T. ) ;
#28952 = CARTESIAN_POINT ( 'NONE',  ( 17.96012107570599881, 3.168891391480999520, 11.45723209283999999 ) ) ;
#28953 = CARTESIAN_POINT ( 'NONE',  ( 11.37103032197929942, -3.416314376401300201, 8.316248703309600643 ) ) ;
#28954 = CARTESIAN_POINT ( 'NONE',  ( 9.848730799670999403, 2.769737997918999994, 6.441853401936000090 ) ) ;
#28955 = CARTESIAN_POINT ( 'NONE',  ( 10.71922080291932033, -4.353435520373503564, -8.814860677227310148 ) ) ;
#28956 = CARTESIAN_POINT ( 'NONE',  ( 11.09999999999999964, 5.299999999999999822, 5.160242730440000258 ) ) ;
#28957 = CARTESIAN_POINT ( 'NONE',  ( 9.175261536096115833, 2.907197492737139122, 8.295168095921209073 ) ) ;
#28958 = CARTESIAN_POINT ( 'NONE',  ( 10.77672335273219950, 4.301522290735800169, -8.312023951944400579 ) ) ;
#28959 = CARTESIAN_POINT ( 'NONE',  ( 24.69899873138500013, -12.37166880149999848, 2.942311212846000057 ) ) ;
#28960 = CARTESIAN_POINT ( 'NONE',  ( 9.581038493598999395, 4.826346105011899645, -6.712036445818600150 ) ) ;
#28961 = CARTESIAN_POINT ( 'NONE',  ( 17.74252821691605320, -0.6952251598378670350, 12.58080715426405938 ) ) ;
#28962 = CARTESIAN_POINT ( 'NONE',  ( 24.46729256464000457, 3.339593025236999857, 12.12065414616999881 ) ) ;
#28963 = CARTESIAN_POINT ( 'NONE',  ( 0.9590630006697127286, 3.046066035227705804, -1.769131241224070950 ) ) ;
#28964 = CARTESIAN_POINT ( 'NONE',  ( 11.18237334122999904, 4.516636732814999888, -8.757876389238999693 ) ) ;
#28965 = VERTEX_POINT ( 'NONE', #52870 ) ;
#28966 = CARTESIAN_POINT ( 'NONE',  ( 8.849379440379999906, -3.975070057433999438, 9.483761758588999058 ) ) ;
#28967 = CARTESIAN_POINT ( 'NONE',  ( 18.25201697486997432, 2.719281809836141317, 13.73337690942506129 ) ) ;
#28968 = CARTESIAN_POINT ( 'NONE',  ( 15.89979320885400327, -3.824231472901999496, -11.71686814605000038 ) ) ;
#28969 = CARTESIAN_POINT ( 'NONE',  ( 10.32118582084299874, -4.836160649475099937, -6.533484739457099622 ) ) ;
#28970 = VERTEX_POINT ( 'NONE', #14443 ) ;
#28971 = CARTESIAN_POINT ( 'NONE',  ( 17.79403162610499933, 3.298115360370000193, 11.83441368098000090 ) ) ;
#28973 = CARTESIAN_POINT ( 'NONE',  ( 9.248305582559998683, -3.908727042518870043, 6.637573130164000190 ) ) ;
#28972 = CARTESIAN_POINT ( 'NONE',  ( 8.596685841231000325, 2.141799395716999843, -7.895788736628000848 ) ) ;
#28974 = DIRECTION ( 'NONE',  ( 1.000000000000000000, 0.000000000000000000, 0.000000000000000000 ) ) ;
#28975 = VERTEX_POINT ( 'NONE', #42038 ) ;
#28976 = ADVANCED_FACE ( 'NONE', ( #30863 ), #30151, .F. ) ;
#28977 = CARTESIAN_POINT ( 'NONE',  ( 10.44675156161000018, 2.885046387990999772, 8.863482298832000339 ) ) ;
#28978 = CARTESIAN_POINT ( 'NONE',  ( 13.63331750507211559, -9.617283495289667528, -7.919506078536236338 ) ) ;
#28979 = CARTESIAN_POINT ( 'NONE',  ( 10.20641772631199906, 4.431553727090300043, 6.611684804099500212 ) ) ;
#28980 = CARTESIAN_POINT ( 'NONE',  ( 10.11260824411999870, -3.359889198679999911, 5.859131457670000209 ) ) ;
#28981 = FACE_OUTER_BOUND ( 'NONE', #63040, .T. ) ;
#28982 = ORIENTED_EDGE ( 'NONE', *, *, #13827, .F. ) ;
#28983 = DIRECTION ( 'NONE',  ( 0.000000000000000000, -0.8648648648648720183, -0.5020047465136825426 ) ) ;
#28984 = EDGE_CURVE ( 'NONE', #59995, #17996, #60531, .T. ) ;
#28985 = EDGE_CURVE ( 'NONE', #52849, #51171, #62796, .T. ) ;
#28986 = CARTESIAN_POINT ( 'NONE',  ( 10.53870444038000009, -5.103398787993000063, -6.705198626796000205 ) ) ;
#28987 = CARTESIAN_POINT ( 'NONE',  ( 7.966450313383576010, -2.301798426562205790, 7.124576740443179901 ) ) ;
#28988 = CARTESIAN_POINT ( 'NONE',  ( 10.90374822854000136, -3.726845778959999578, 5.900452123196999743 ) ) ;
#28989 = CARTESIAN_POINT ( 'NONE',  ( 10.89324174884020024, -4.032306468273969990, -8.674442868902998427 ) ) ;
#28990 = CARTESIAN_POINT ( 'NONE',  ( 9.476101285863999024, -4.646739515667500875, 8.268485718282699182 ) ) ;
#28991 = ORIENTED_EDGE ( 'NONE', *, *, #14931, .T. ) ;
#28992 = DIRECTION ( 'NONE',  ( 1.000000000000000000, 0.000000000000000000, 0.000000000000000000 ) ) ;
#28993 = CARTESIAN_POINT ( 'NONE',  ( 11.43656785386840014, -5.060279460151999587, 6.786470850652599474 ) ) ;
#28994 = ORIENTED_EDGE ( 'NONE', *, *, #7137, .F. ) ;
#28995 = CARTESIAN_POINT ( 'NONE',  ( 9.610944094206999466, 5.100000000000000533, -6.571291218949999902 ) ) ;
#28996 = ORIENTED_EDGE ( 'NONE', *, *, #22873, .T. ) ;
#28997 = CARTESIAN_POINT ( 'NONE',  ( 9.311718600414000235, -4.588307032459999490, -5.987050435448999508 ) ) ;
#28998 = CARTESIAN_POINT ( 'NONE',  ( 9.292835841232999883, 5.200883864107000321, -6.027780766890000308 ) ) ;
#28999 = DIRECTION ( 'NONE',  ( 0.000000000000000000, 1.000000000000000000, 0.000000000000000000 ) ) ;
#29000 = FACE_OUTER_BOUND ( 'NONE', #18665, .T. ) ;
#29001 = CARTESIAN_POINT ( 'NONE',  ( 12.54459593125679362, 1.931762302728656788, -12.56598641381995307 ) ) ;
#29002 = CARTESIAN_POINT ( 'NONE',  ( 10.92795525820100089, -4.094749303624469761, 8.498986197235801399 ) ) ;
#29003 = CARTESIAN_POINT ( 'NONE',  ( 11.19568717260499824, -4.466067913030199676, 6.739296831621899742 ) ) ;
#29004 = EDGE_CURVE ( 'NONE', #63987, #27357, #9543, .T. ) ;
#29005 = ORIENTED_EDGE ( 'NONE', *, *, #8223, .T. ) ;
#29006 = AXIS2_PLACEMENT_3D ( 'NONE', #12019, #38237, #7121 ) ;
#29007 = CARTESIAN_POINT ( 'NONE',  ( 7.000000000000000000, 0.3230303992915000144, 3.000000000000000000 ) ) ;
#29008 = ORIENTED_EDGE ( 'NONE', *, *, #17439, .T. ) ;
#29009 = CARTESIAN_POINT ( 'NONE',  ( 8.957394353210000659, -2.678334737187000325, 8.735278777293000729 ) ) ;
#29010 = CARTESIAN_POINT ( 'NONE',  ( 25.49995753756256178, -8.603837101910434271, 7.325400450397203223 ) ) ;
#29011 = EDGE_LOOP ( 'NONE', ( #10930, #51877, #36606, #51379 ) ) ;
#29012 = B_SPLINE_SURFACE_WITH_KNOTS ( 'NONE', 3, 3, ( 
 ( #45128, #55957, #33603, #49321 ),
 ( #49674, #34296, #23099, #7367 ),
 ( #61543, #55618, #7718, #33948 ),
 ( #29059, #61205, #54922, #29408 ),
 ( #8064, #50715, #2469, #39186 ),
 ( #50369, #23794, #66438, #22751 ) ),
 .UNSPECIFIED., .F., .F., .F.,
 ( 4, 1, 1, 4 ),
 ( 4, 4 ),
 ( 0.1811037439853999953, 0.3333333333333000081, 0.6666666666667000474, 0.8725156478927998949 ),
 ( -0.1256563615239000009, 1.125656361510000147 ),
 .UNSPECIFIED. ) ;
#29013 = CARTESIAN_POINT ( 'NONE',  ( 12.15236716622355750, -2.166683524422402751, -12.41231652552486864 ) ) ;
#29014 = CARTESIAN_POINT ( 'NONE',  ( 10.55103166480599874, 2.999015536536000504, 7.429424106427209296 ) ) ;
#29015 = CARTESIAN_POINT ( 'NONE',  ( 10.22908305962000064, -4.838492992840000007, -5.852445959518000507 ) ) ;
#29016 = CARTESIAN_POINT ( 'NONE',  ( 10.76059687351619765, 3.370476274536378547, 8.592232985442823434 ) ) ;
#29017 = CARTESIAN_POINT ( 'NONE',  ( 17.70779401564400146, -11.44429775961999951, 4.694470971454999919 ) ) ;
#29018 = LINE ( 'NONE', #50325, #66550 ) ;
#29019 = CARTESIAN_POINT ( 'NONE',  ( 12.34730967147305591, -2.925678532231709816, -13.57385403034849425 ) ) ;
#29020 = CARTESIAN_POINT ( 'NONE',  ( 18.12876220047771270, -0.2481623978058161428, -12.69674179789669211 ) ) ;
#29021 = CYLINDRICAL_SURFACE ( 'NONE', #13912, 11.84999999999999964 ) ;
#29022 = CARTESIAN_POINT ( 'NONE',  ( 9.149954719592001240, 4.175915362023999933, 5.699506188181000077 ) ) ;
#29023 = VERTEX_POINT ( 'NONE', #55290 ) ;
#29024 = SURFACE_STYLE_USAGE ( .BOTH. , #28671 ) ;
#29025 = CARTESIAN_POINT ( 'NONE',  ( 27.64127793187000037, -2.399999999999999911, -6.571291218949999902 ) ) ;
#29026 = CARTESIAN_POINT ( 'NONE',  ( 7.178735624121773462, 2.852824245031727379, 8.262394631885278784 ) ) ;
#29027 = CARTESIAN_POINT ( 'NONE',  ( 23.86982303804800054, -3.657043654406999966, 13.22876065065999818 ) ) ;
#29028 = CARTESIAN_POINT ( 'NONE',  ( 17.94092590763757755, 3.089486433945234811, 12.21536380989863702 ) ) ;
#29029 = CARTESIAN_POINT ( 'NONE',  ( 11.09999999999999964, -4.000000000000000000, -9.049999999995968381 ) ) ;
#29030 = CARTESIAN_POINT ( 'NONE',  ( 9.629022744239000176, 5.794335169544999609, 7.414871903737999759 ) ) ;
#29031 = EDGE_CURVE ( 'NONE', #34779, #51086, #39905, .T. ) ;
#29032 = CARTESIAN_POINT ( 'NONE',  ( 11.39043504475232815, -5.070797187771876047, -8.202738646980327175 ) ) ;
#29033 = FACE_OUTER_BOUND ( 'NONE', #43124, .T. ) ;
#29034 = ORIENTED_EDGE ( 'NONE', *, *, #47518, .T. ) ;
#29035 = CARTESIAN_POINT ( 'NONE',  ( 12.46375379917807713, -1.976313547018314631, 12.55830662486076932 ) ) ;
#29036 = CARTESIAN_POINT ( 'NONE',  ( 10.03293802597399953, -4.450760089576400347, -6.759376420744099612 ) ) ;
#29037 = CARTESIAN_POINT ( 'NONE',  ( 10.90638722582999875, 5.227488226180000197, 6.784465725675999259 ) ) ;
#29038 = DIRECTION ( 'NONE',  ( -1.000000000000000000, 0.000000000000000000, 0.000000000000000000 ) ) ;
#29039 = CARTESIAN_POINT ( 'NONE',  ( 10.96533729122639933, 2.859653469230999612, -7.470001566214039990 ) ) ;
#29040 = CARTESIAN_POINT ( 'NONE',  ( 12.74530398939900167, -0.7169431667913570561, 12.57958639523259414 ) ) ;
#29041 = CARTESIAN_POINT ( 'NONE',  ( 8.893204719592999297, 3.977267228909999730, 9.308925224542001331 ) ) ;
#29042 = CARTESIAN_POINT ( 'NONE',  ( 9.442843574488000158, 2.691255504502000129, 6.269523028052000235 ) ) ;
#29043 = DIRECTION ( 'NONE',  ( 1.000000000000000000, 0.000000000000000000, 0.000000000000000000 ) ) ;
#29044 = ORIENTED_EDGE ( 'NONE', *, *, #61009, .T. ) ;
#29045 = CARTESIAN_POINT ( 'NONE',  ( 25.58980649241400229, 8.350730680791999205, 7.985153332161000428 ) ) ;
#29046 = CARTESIAN_POINT ( 'NONE',  ( 11.62579573085663043, 5.239377455231000624, -7.714452430741599365 ) ) ;
#29047 = CARTESIAN_POINT ( 'NONE',  ( 10.80231684603725917, -4.484370860713429607, 9.173854975331316552 ) ) ;
#29049 = CARTESIAN_POINT ( 'NONE',  ( 17.78594645489210890, -0.5808586469551295650, 12.68211397078189862 ) ) ;
#29048 = CARTESIAN_POINT ( 'NONE',  ( 5.500000000000000000, -12.22296174243999900, -3.800101973039000214 ) ) ;
#29050 = CARTESIAN_POINT ( 'NONE',  ( 9.376797255588000368, -3.133765047594600173, 7.536673658251589636 ) ) ;
#29051 = AXIS2_PLACEMENT_3D ( 'NONE', #29090, #30452, #20989 ) ;
#29052 = CARTESIAN_POINT ( 'NONE',  ( 10.75210807141120029, -3.959980833595939664, -8.365272822098500427 ) ) ;
#29053 = VERTEX_POINT ( 'NONE', #29426 ) ;
#29054 = CARTESIAN_POINT ( 'NONE',  ( 0.9717001509839999773, -0.1515593316830000370, 3.422260710200999867 ) ) ;
#29055 = CARTESIAN_POINT ( 'NONE',  ( 17.96717518460240726, -0.4698982327886221944, -12.68829846777228632 ) ) ;
#29056 = CARTESIAN_POINT ( 'NONE',  ( 24.84557271449745741, 12.09420847694864065, 2.925015109421550186 ) ) ;
#29057 = DIRECTION ( 'NONE',  ( 0.000000000000000000, 0.000000000000000000, -1.000000000000000000 ) ) ;
#29058 = B_SPLINE_CURVE_WITH_KNOTS ( 'NONE', 3,
 ( #6638, #54185, #23063, #11530 ),
 .UNSPECIFIED., .F., .F.,
 ( 4, 4 ),
 ( 0.000000000000000000, 1.000000000000000000 ),
 .UNSPECIFIED. ) ;
#29059 = CARTESIAN_POINT ( 'NONE',  ( 24.36809152995600058, -12.06003563572999937, 3.271087558185000077 ) ) ;
#29060 = CARTESIAN_POINT ( 'NONE',  ( 17.55505043854147118, -1.874999999999999556, -13.78627172894481845 ) ) ;
#29061 = CARTESIAN_POINT ( 'NONE',  ( 9.817462135711998883, -5.100000000000000533, 6.571291218949999902 ) ) ;
#29062 = CARTESIAN_POINT ( 'NONE',  ( 9.383148997457999130, -5.167567567567999731, 6.822293592207000934 ) ) ;
#29063 = CARTESIAN_POINT ( 'NONE',  ( 23.61469345536201558, 13.25062970456771083, 4.103859225642715103 ) ) ;
#29064 = VERTEX_POINT ( 'NONE', #56667 ) ;
#29065 = CARTESIAN_POINT ( 'NONE',  ( 7.700045280408999382, 3.346262376537000094, 6.002251090845000192 ) ) ;
#29066 = EDGE_CURVE ( 'NONE', #22260, #29486, #4757, .T. ) ;
#29067 = EDGE_CURVE ( 'NONE', #68446, #66560, #60455, .T. ) ;
#29068 = CARTESIAN_POINT ( 'NONE',  ( 11.59610237318921477, 3.189590050595149773, -7.174950768514437804 ) ) ;
#29069 = CARTESIAN_POINT ( 'NONE',  ( 18.09739622855035890, 2.188708726545602001, -13.73458559204160423 ) ) ;
#29070 = CARTESIAN_POINT ( 'NONE',  ( 7.688565988106098814, -2.650624002730362250, 7.262809006051590188 ) ) ;
#29071 = CARTESIAN_POINT ( 'NONE',  ( 0.6036543026616000285, 3.532364098973999944, -0.6521526059094999717 ) ) ;
#29072 = ORIENTED_EDGE ( 'NONE', *, *, #36220, .T. ) ;
#29073 = CARTESIAN_POINT ( 'NONE',  ( 1.792640132539665698, -3.058252359239901796, -1.762666431298149039 ) ) ;
#29074 = CARTESIAN_POINT ( 'NONE',  ( 10.83824331590383672, -5.765061639177475605, -7.465997195058596603 ) ) ;
#29075 = CARTESIAN_POINT ( 'NONE',  ( 9.569805421428000614, 4.064052243276000453, 8.919241792616000808 ) ) ;
#29076 = CARTESIAN_POINT ( 'NONE',  ( 11.43718179236249988, 3.790319673775199849, 8.481317998227099864 ) ) ;
#29077 = CARTESIAN_POINT ( 'NONE',  ( 11.05336220499919797, -4.965402920923000174, -7.825000000000000178 ) ) ;
#29078 = CARTESIAN_POINT ( 'NONE',  ( 10.65229194037999960, -4.944342461481999962, -8.478476072358999360 ) ) ;
#29079 = CARTESIAN_POINT ( 'NONE',  ( 11.50002653705205446, 3.809920415104828262, -11.93174655290500574 ) ) ;
#29080 = CARTESIAN_POINT ( 'NONE',  ( 10.10000011340999926, 12.39999890530000037, 0.000000000000000000 ) ) ;
#29081 = CARTESIAN_POINT ( 'NONE',  ( 12.27407495020797334, -2.829836729544706664, 12.36860105340724658 ) ) ;
#29082 = ADVANCED_FACE ( 'NONE', ( #7385 ), #61906, .T. ) ;
#29083 = CARTESIAN_POINT ( 'NONE',  ( 7.506887093506311892, 2.659857595113553241, 6.362335448027723217 ) ) ;
#29084 = ORIENTED_EDGE ( 'NONE', *, *, #7764, .F. ) ;
#29085 = CARTESIAN_POINT ( 'NONE',  ( 17.84567419427294155, -3.186977498899958849, 13.63243182350604243 ) ) ;
#29086 = CARTESIAN_POINT ( 'NONE',  ( 7.779445392134999082, 3.186710064579999724, 6.422248840039000761 ) ) ;
#29087 = EDGE_LOOP ( 'NONE', ( #30219, #40632, #40983, #34749 ) ) ;
#29088 = ORIENTED_EDGE ( 'NONE', *, *, #45453, .F. ) ;
#29089 = EDGE_CURVE ( 'NONE', #66241, #4821, #53761, .T. ) ;
#29090 = CARTESIAN_POINT ( 'NONE',  ( 5.500000000000000000, 13.87069231928999891, -4.225386915259999654 ) ) ;
#29091 = CARTESIAN_POINT ( 'NONE',  ( 5.308207799363945156, -1.091870064679186347, 0.3013736060501072123 ) ) ;
#29092 = AXIS2_PLACEMENT_3D ( 'NONE', #66571, #13454, #67252 ) ;
#29093 = LINE ( 'NONE', #50402, #34477 ) ;
#29094 = CARTESIAN_POINT ( 'NONE',  ( 10.71256887705999894, 5.951815279772000089, 7.233043586354999555 ) ) ;
#29095 = LINE ( 'NONE', #24522, #20965 ) ;
#29096 = CARTESIAN_POINT ( 'NONE',  ( 10.65434687351570631, -2.749999999999998668, 7.663624617374463988 ) ) ;
#29097 = FACE_OUTER_BOUND ( 'NONE', #35097, .T. ) ;
#29098 = CARTESIAN_POINT ( 'NONE',  ( 10.52342417510000061, -3.209670667763000029, -9.177087527572998837 ) ) ;
#29099 = CARTESIAN_POINT ( 'NONE',  ( 11.85159063708299954, -3.174974693948799942, -7.731961446576300467 ) ) ;
#29100 =( NAMED_UNIT ( * ) SI_UNIT ( $, .STERADIAN. ) SOLID_ANGLE_UNIT ( ) );
#29101 = ORIENTED_EDGE ( 'NONE', *, *, #57767, .F. ) ;
#29103 = CIRCLE ( 'NONE', #14565, 12.52500000000000036 ) ;
#29102 = B_SPLINE_CURVE_WITH_KNOTS ( 'NONE', 3,
 ( #66063, #1750, #49293, #54892, #28679, #11198, #17840, #27984, #48957, #59436, #64675, #43375, #12590, #43718, #38110, #716, #1405, #38814, #39159, #60138, #28324, #6290, #11536, #32879, #48612, #17130, #22720, #22028, #12246, #55239, #33919, #60482, #59784, #2107, #44068, #27637, #6992, #49643, #33226, #32536, #23071, #23424, #11887, #1066, #65369, #27291, #54546, #2784, #61518, #12941, #30394, #18182, #8721, #29724, #66409, #67095, #24110, #34266, #13295, #34619, #51367, #25138, #40875, #8381, #19555 ),
 .UNSPECIFIED., .F., .F.,
 ( 4, 1, 1, 1, 1, 1, 1, 1, 1, 1, 1, 1, 1, 1, 1, 1, 1, 1, 1, 1, 1, 1, 1, 1, 1, 1, 1, 1, 1, 1, 1, 1, 1, 1, 1, 1, 1, 1, 1, 1, 1, 1, 1, 1, 1, 1, 1, 1, 1, 1, 1, 1, 1, 1, 1, 1, 1, 1, 1, 1, 1, 1, 4 ),
 ( 0.000000000000000000, 0.01249986222369731809, 0.02874986775682975698, 0.04499987328996219588, 0.06124987882309463477, 0.07749988435622708061, 0.09374988988935951950, 0.1099998954224919584, 0.1262499009556244112, 0.1424999064887568501, 0.1587499120218892890, 0.1749999175550217279, 0.1912499230881541668, 0.2074999286212866056, 0.2237499341544190445, 0.2399999396875514834, 0.2562499452206838946, 0.2724999507538163890, 0.2887499562869488279, 0.3049999618200812668, 0.3212499673532136502, 0.3374999728863461446, 0.3537499784194785835, 0.3699999839526110224, 0.3862499894857434612, 0.4024999950188759001, 0.4187500005520083390, 0.4350000060851407779, 0.4512500116182732168, 0.4675000171514057112, 0.4837500226845380946, 0.5000000282176705335, 0.5162500337508029169, 0.5325000392839353003, 0.5487500448170677947, 0.5650000503502001781, 0.5812500558833327835, 0.5975000614164651669, 0.6137500669495975503, 0.6300000724827300447, 0.6462500780158624281, 0.6625000835489948114, 0.6787500890821273059, 0.6950000946152596892, 0.7112501001483922947, 0.7275001056815246780, 0.7437501112146570614, 0.7600001167477895558, 0.7762501222809219392, 0.7925001278140544336, 0.8087501333471868170, 0.8250001388803192004, 0.8412501444134518058, 0.8575001499465841892, 0.8737501554797166836, 0.8900001610128490670, 0.9062501665459814504, 0.9225001720791139448, 0.9387501776122463282, 0.9550001831453788226, 0.9712501886785112060, 0.9875001942116437004, 1.000000000000000000 ),
 .UNSPECIFIED. ) ;
#29104 = DIRECTION ( 'NONE',  ( 0.000000000000000000, -1.000000000000000000, 0.000000000000000000 ) ) ;
#29105 =( NAMED_UNIT ( * ) SI_UNIT ( $, .STERADIAN. ) SOLID_ANGLE_UNIT ( ) );
#29106 = CARTESIAN_POINT ( 'NONE',  ( 23.59999441188499958, 10.30760541648000128, -9.317696302454001156 ) ) ;
#29107 = CARTESIAN_POINT ( 'NONE',  ( 5.000030787343001215, 0.5496608443529860111, -2.045306479342562156 ) ) ;
#29108 = CARTESIAN_POINT ( 'NONE',  ( 9.154341692891298621, 5.250000716804954948, 7.663628708442515425 ) ) ;
#29109 = CARTESIAN_POINT ( 'NONE',  ( 12.80505043854143210, 3.248147246781388109, 13.61798588129781074 ) ) ;
#29110 = CARTESIAN_POINT ( 'NONE',  ( 9.667080975990000269, -4.541622198376999542, 5.824041840233000755 ) ) ;
#29111 = ORIENTED_EDGE ( 'NONE', *, *, #3016, .F. ) ;
#29112 = CARTESIAN_POINT ( 'NONE',  ( 12.35320888716225518, 0.4320279635882856573, -12.69011309768868934 ) ) ;
#29113 = CARTESIAN_POINT ( 'NONE',  ( 12.64343601369307279, -0.6040897852209341501, 13.88232707694115398 ) ) ;
#29114 = ORIENTED_EDGE ( 'NONE', *, *, #14414, .F. ) ;
#29115 = CARTESIAN_POINT ( 'NONE',  ( 21.00000000000000000, 0.000000000000000000, 0.000000000000000000 ) ) ;
#29116 = CARTESIAN_POINT ( 'NONE',  ( 18.43329219593509194, 2.701919656448346529, 11.40083085748005054 ) ) ;
#29117 = CARTESIAN_POINT ( 'NONE',  ( 7.115095033390245405, 5.350161709276040511, -7.499994210608702083 ) ) ;
#29118 = CARTESIAN_POINT ( 'NONE',  ( 8.491253953972980995, 3.097373565453227506, 6.091084184371706733 ) ) ;
#29119 = CARTESIAN_POINT ( 'NONE',  ( 5.500000000000000000, 0.000000000000000000, 0.000000000000000000 ) ) ;
#29120 = CARTESIAN_POINT ( 'NONE',  ( 11.01668724082999873, 7.361611265918999614, -6.178327710506999360 ) ) ;
#29121 = PRODUCT_DEFINITION ( 'UNKNOWN', '', #35160, #62559 ) ;
#29122 = CARTESIAN_POINT ( 'NONE',  ( 8.106591486974918936, 5.204875969127657598, -8.204933670002066748 ) ) ;
#29123 = CARTESIAN_POINT ( 'NONE',  ( -15.86200481174999943, 5.599999999999999645, 6.571291218949999902 ) ) ;
#29124 = CARTESIAN_POINT ( 'NONE',  ( 11.09999999999999964, 2.649999999999999911, -7.500000000000000000 ) ) ;
#29125 = CARTESIAN_POINT ( 'NONE',  ( 9.612156140204000110, -5.332339947063000629, -7.851654145788001138 ) ) ;
#29126 = CARTESIAN_POINT ( 'NONE',  ( 10.50595525820100029, 3.918212119278319694, -6.637672143048099827 ) ) ;
#29127 = LINE ( 'NONE', #12688, #58976 ) ;
#29128 = CARTESIAN_POINT ( 'NONE',  ( 11.40211496860029783, 4.793947479907100018, -7.093139000852099585 ) ) ;
#29129 = CARTESIAN_POINT ( 'NONE',  ( 9.632646554151000018, 4.552790318865400643, -8.499078230848398974 ) ) ;
#29131 = CARTESIAN_POINT ( 'NONE',  ( 10.33390208397999999, -3.197011589206999904, 5.018836569371999623 ) ) ;
#29130 = CARTESIAN_POINT ( 'NONE',  ( 9.595759580228998331, -4.843256805554699618, 7.701558687214699717 ) ) ;
#29132 = CARTESIAN_POINT ( 'NONE',  ( 23.59959168357080017, -13.39165867665727205, 3.997819989704973764 ) ) ;
#29133 = ORIENTED_EDGE ( 'NONE', *, *, #29958, .F. ) ;
#29134 = AXIS2_PLACEMENT_3D ( 'NONE', #2439, #29373, #50687 ) ;
#29135 = CARTESIAN_POINT ( 'NONE',  ( 11.60988784977536348, 3.148894096305599799, 7.548634759728509280 ) ) ;
#29136 = CARTESIAN_POINT ( 'NONE',  ( 10.84168850528999961, -2.681008214828000114, 6.554752254946000889 ) ) ;
#29137 = CARTESIAN_POINT ( 'NONE',  ( 9.277088727410998104, 2.862182806015999947, 7.404572115919599185 ) ) ;
#29138 = CARTESIAN_POINT ( 'NONE',  ( 9.885457958598628636, 4.856131813426149968, -7.319526769407151079 ) ) ;
#29139 = CIRCLE ( 'NONE', #116, 5.760713961201000544 ) ;
#29140 = CARTESIAN_POINT ( 'NONE',  ( 9.352255147285999826, -2.817754448466000206, 6.388456890282999900 ) ) ;
#29141 = DIRECTION ( 'NONE',  ( 0.000000000000000000, 1.000000000000000000, 0.000000000000000000 ) ) ;
#29142 = ORIENTED_EDGE ( 'NONE', *, *, #1965, .F. ) ;
#29143 = EDGE_CURVE ( 'NONE', #57692, #53328, #31473, .T. ) ;
#29144 = EDGE_CURVE ( 'NONE', #67057, #20353, #1430, .T. ) ;
#29145 = CARTESIAN_POINT ( 'NONE',  ( 9.657975701332999208, -3.162316589966200020, -8.275900091855099561 ) ) ;
#29146 = CARTESIAN_POINT ( 'NONE',  ( 9.760596873516668381, -4.629523725463621453, -6.407767014557177454 ) ) ;
#29147 = CARTESIAN_POINT ( 'NONE',  ( 5.721864308364999374, -0.04522467425096000221, -1.614091090670999984 ) ) ;
#29148 = CARTESIAN_POINT ( 'NONE',  ( 10.27195525820100031, 3.879327850572200198, 8.772302877803999976 ) ) ;
#29149 = DIRECTION ( 'NONE',  ( 1.000000000000000000, 0.000000000000000000, 0.000000000000000000 ) ) ;
#29150 = DIRECTION ( 'NONE',  ( -1.000000000000000000, 0.000000000000000000, 0.000000000000000000 ) ) ;
#29151 = CARTESIAN_POINT ( 'NONE',  ( 11.46179707368349909, 3.501542828836900156, -6.629085939160999530 ) ) ;
#29152 = CARTESIAN_POINT ( 'NONE',  ( 5.200000000963999724, -1.599999999036000098, 2.855876981774999784E-09 ) ) ;
#29153 = CARTESIAN_POINT ( 'NONE',  ( 9.309310001151999359, -5.531435376468999188, -8.256621485025000595 ) ) ;
#29154 = CARTESIAN_POINT ( 'NONE',  ( 0.8218067992086085516, -3.408904368339104263, -0.9161175952574813763 ) ) ;
#29155 = EDGE_LOOP ( 'NONE', ( #66813, #66037, #49924, #21687, #41032, #27936, #27627, #59382, #42991, #68153, #30356, #10688, #21975, #35602, #13376 ) ) ;
#29156 = CARTESIAN_POINT ( 'NONE',  ( 17.60411830284828483, 1.787854822559049595, -13.88537270421502612 ) ) ;
#29157 = CARTESIAN_POINT ( 'NONE',  ( 12.42135566322309081, -0.6200266137005091549, -13.98626978124057629 ) ) ;
#29158 = LINE ( 'NONE', #7465, #42185 ) ;
#29159 = DIRECTION ( 'NONE',  ( 0.000000000000000000, -0.5895247755844827964, -0.8077502949377767250 ) ) ;
#29160 = CARTESIAN_POINT ( 'NONE',  ( 10.63351354018304740, -2.750000000000000000, -7.663624617374467540 ) ) ;
#29161 = CARTESIAN_POINT ( 'NONE',  ( 8.324914158772999784, 2.633142096252999664, -7.791134854666999843 ) ) ;
#29162 = CARTESIAN_POINT ( 'NONE',  ( 5.610802430945667219, 12.12319474034293521, -3.747515530460208133 ) ) ;
#29163 = VERTEX_POINT ( 'NONE', #19949 ) ;
#29164 = CARTESIAN_POINT ( 'NONE',  ( 9.354620317202259727, -2.650257996360415369, -7.676659957281179558 ) ) ;
#29165 = CARTESIAN_POINT ( 'NONE',  ( 17.75752317324808160, 1.908613644657472408, -13.78124409819558949 ) ) ;
#29166 = ORIENTED_EDGE ( 'NONE', *, *, #64812, .F. ) ;
#29167 = EDGE_CURVE ( 'NONE', #25033, #42399, #20287, .T. ) ;
#29168 = CARTESIAN_POINT ( 'NONE',  ( 11.53192018828833731, -4.908970299435360118, -7.175001928748123703 ) ) ;
#29169 = CARTESIAN_POINT ( 'NONE',  ( 24.92845940784351555, 2.996118283957757811, 11.61748718301992156 ) ) ;
#29170 = CARTESIAN_POINT ( 'NONE',  ( 9.881820280408998514, 4.325866256860000369, -9.125812605905000652 ) ) ;
#29171 = CARTESIAN_POINT ( 'NONE',  ( 24.01911655981654548, -12.68156841354276310, 3.458532931849343850 ) ) ;
#29172 = CARTESIAN_POINT ( 'NONE',  ( 11.35034208742529849, -4.630634088820300143, -8.491292290686200062 ) ) ;
#29173 = CARTESIAN_POINT ( 'NONE',  ( 17.96217742567913334, 0.4744044024703746310, -12.68807559258215711 ) ) ;
#29174 = CIRCLE ( 'NONE', #65975, 12.39999890530000037 ) ;
#29175 = CARTESIAN_POINT ( 'NONE',  ( 11.03333333333535293, -2.969278270712975676, 8.594189652917078703 ) ) ;
#29176 = ORIENTED_EDGE ( 'NONE', *, *, #11144, .F. ) ;
#29177 = CARTESIAN_POINT ( 'NONE',  ( 8.679055905797000037, -2.899999999999999911, 6.571291218949999902 ) ) ;
#29178 = CARTESIAN_POINT ( 'NONE',  ( 18.15005478421819518, -2.691381137285254965, -13.63095209222209903 ) ) ;
#29179 = ORIENTED_EDGE ( 'NONE', *, *, #55982, .F. ) ;
#29180 = CARTESIAN_POINT ( 'NONE',  ( 10.25165889348999926, 3.418644779562000302, -8.733642166016998942 ) ) ;
#29181 = CARTESIAN_POINT ( 'NONE',  ( 11.02938691836999929, -8.053295335382999909, 6.898627764883999980 ) ) ;
#29182 = ORIENTED_EDGE ( 'NONE', *, *, #63198, .T. ) ;
#29183 = CARTESIAN_POINT ( 'NONE',  ( 9.151392757686998891, 4.770706668257700400, 6.657535947657399866 ) ) ;
#29184 = CARTESIAN_POINT ( 'NONE',  ( 18.27150181675466811, -2.367044107065576775, -12.37568780170008509 ) ) ;
#29185 = CARTESIAN_POINT ( 'NONE',  ( 8.225195096046167720, 2.649880853682612614, 7.500010424662513664 ) ) ;
#29186 = DIRECTION ( 'NONE',  ( -0.8660254037844288266, 0.000000000000000000, -0.5000000000000169864 ) ) ;
#29187 = CARTESIAN_POINT ( 'NONE',  ( 11.61719580513100247, -11.50344080059000085, -1.587150035090999722 ) ) ;
#29188 = CIRCLE ( 'NONE', #55976, 1.249999999999999778 ) ;
#29189 = CARTESIAN_POINT ( 'NONE',  ( 10.21722949779699974, 4.557226039164599563, 6.664331202173499946 ) ) ;
#29190 = CARTESIAN_POINT ( 'NONE',  ( 9.382598168139042016, -2.846997224034427898, 8.802713852305345199 ) ) ;
#29191 = ORIENTED_EDGE ( 'NONE', *, *, #66488, .T. ) ;
#29192 = CARTESIAN_POINT ( 'NONE',  ( 11.56914347478616634, 4.748726180097643912, 6.470125748842363578 ) ) ;
#29193 = CARTESIAN_POINT ( 'NONE',  ( 10.81187971959000116, 4.614148948243999904, -5.930135044105000475 ) ) ;
#29194 = CARTESIAN_POINT ( 'NONE',  ( 12.80505043854143388, 3.207073286498425269, -13.58561123731972131 ) ) ;
#29195 = CARTESIAN_POINT ( 'NONE',  ( 12.48231810865423874, 3.171873548221313843, -13.63595416837495300 ) ) ;
#29196 = CARTESIAN_POINT ( 'NONE',  ( 10.01364655415099847, -3.380689388027600106, -8.619302797893999113 ) ) ;
#29197 = CARTESIAN_POINT ( 'NONE',  ( 9.034116535116000435, -4.695350938297000454, 8.660677768253002284 ) ) ;
#29198 = CARTESIAN_POINT ( 'NONE',  ( 17.65691712177036621, 0.6169787192598746861, 13.88156336867697149 ) ) ;
#29199 = CLOSED_SHELL ( 'NONE', ( #1486, #60864, #11090, #5674, #47187, #33245 ) ) ;
#29200 = CARTESIAN_POINT ( 'NONE',  ( 10.20920446231349921, 2.899999999999999911, 6.662590550579914783 ) ) ;
#29201 = EDGE_CURVE ( 'NONE', #57124, #6268, #35448, .T. ) ;
#29202 = EDGE_CURVE ( 'NONE', #23593, #52535, #27893, .T. ) ;
#29203 = ORIENTED_EDGE ( 'NONE', *, *, #11281, .F. ) ;
#29204 = ORIENTED_EDGE ( 'NONE', *, *, #23663, .T. ) ;
#29205 = CARTESIAN_POINT ( 'NONE',  ( 8.739954719592999410, 3.122811675949999977, -6.006064052396999919 ) ) ;
#29206 = PLANE ( 'NONE',  #63533 ) ;
#29207 = CARTESIAN_POINT ( 'NONE',  ( 12.80505043854146940, -1.875000000000000444, 13.78631952119025605 ) ) ;
#29208 = CARTESIAN_POINT ( 'NONE',  ( 9.292149251564818968, -4.685486125476070463, 9.106491892308623548 ) ) ;
#29209 = CARTESIAN_POINT ( 'NONE',  ( 24.56914376165800107, 8.855803919881999775, -9.404908024782999476 ) ) ;
#29210 = CARTESIAN_POINT ( 'NONE',  ( 18.07439970769999960, -3.110573872314000177, -11.47478625844000177 ) ) ;
#29212 = CARTESIAN_POINT ( 'NONE',  ( 1.800973465875000068, -3.500000000000000000, 0.000000000000000000 ) ) ;
#29211 = CARTESIAN_POINT ( 'NONE',  ( 10.79025461470400060, -5.106563667948999630, 7.218483930889299849 ) ) ;
#29213 = CARTESIAN_POINT ( 'NONE',  ( 9.099999999999999645, 0.000000000000000000, -11.84999999999999964 ) ) ;
#29214 = VERTEX_POINT ( 'NONE', #25187 ) ;
#29215 = B_SPLINE_CURVE_WITH_KNOTS ( 'NONE', 3,
 ( #53112, #11147, #21630, #11481 ),
 .UNSPECIFIED., .F., .F.,
 ( 4, 4 ),
 ( 0.000000000000000000, 1.000000000000000000 ),
 .UNSPECIFIED. ) ;
#29216 = DIRECTION ( 'NONE',  ( 1.000000000000000000, 0.000000000000000000, 0.000000000000000000 ) ) ;
#29217 = CARTESIAN_POINT ( 'NONE',  ( 24.35365242081700288, -11.54878985765998500, -2.979915831562000239 ) ) ;
#29218 = CARTESIAN_POINT ( 'NONE',  ( 17.99001832964330916, 0.4489258298041814421, 12.68932177688764362 ) ) ;
#29219 = CARTESIAN_POINT ( 'NONE',  ( 12.53084373025215648, -0.5620101268951274154, 12.68326259363504960 ) ) ;
#29220 = CARTESIAN_POINT ( 'NONE',  ( 4.149992563292000725, 1.947893036340042627, 0.5234817089163691373 ) ) ;
#29221 = ORIENTED_EDGE ( 'NONE', *, *, #10420, .F. ) ;
#29223 = CARTESIAN_POINT ( 'NONE',  ( 10.89529697814178100, 4.826567894363762434, 7.784385510031588851 ) ) ;
#29222 = CARTESIAN_POINT ( 'NONE',  ( 11.13226790813000022, -5.329954231730000380, 5.054493266885999425 ) ) ;
#29224 = CARTESIAN_POINT ( 'NONE',  ( 9.360279719594000625, 3.031907308384000022, -8.729608011560001657 ) ) ;
#29225 = EDGE_CURVE ( 'NONE', #29433, #10252, #22045, .T. ) ;
#29226 = DIRECTION ( 'NONE',  ( 1.000000000000000000, 0.000000000000000000, 0.000000000000000000 ) ) ;
#29227 = B_SPLINE_CURVE_WITH_KNOTS ( 'NONE', 3,
 ( #29207, #29903, #24290, #61352, #8212, #66588, #13127, #19040, #61010, #46307, #19384, #28870, #19733, #50516, #66245, #18367, #2281, #13472, #45627, #23597, #61690, #24974, #60661, #34455, #7871, #23949, #35137, #2617, #34792, #12776, #34105, #7515, #56103, #14151, #29561, #45283, #66930, #35479, #55769, #18708, #40369, #56800, #56450, #55422, #8555, #51208, #50178, #8897, #30236, #44940, #39689, #4325, #36152, #48019, #31948, #120, #21106, #31260, #53265, #20414, #52922, #41742, #57815, #46993, #62709, #68642, #41403 ),
 .UNSPECIFIED., .F., .F.,
 ( 4, 2, 2, 2, 2, 2, 2, 2, 2, 2, 2, 2, 2, 2, 1, 1, 1, 2, 2, 2, 2, 2, 2, 2, 2, 2, 2, 2, 2, 2, 2, 2, 2, 2, 4 ),
 ( 0.000000000000000000, 0.1250000000000047740, 0.2500000000000094369, 0.3125000000000108247, 0.3437500000000110467, 0.3750000000000113243, 0.4062500000000115463, 0.4218750000000118239, 0.4375000000000121014, 0.4687500000000127121, 0.4843750000000134892, 0.5000000000000142109, 0.5156250000000149880, 0.5312500000000157652, 0.5468750000000164313, 0.5546875000000169864, 0.5585937500000174305, 0.5605468750000180966, 0.5625000000000186517, 0.5781250000000179856, 0.5859375000000167644, 0.5898437500000160982, 0.5937500000000154321, 0.6093750000000172085, 0.6171875000000173195, 0.6250000000000175415, 0.6406250000000172085, 0.6562500000000169864, 0.6718750000000166533, 0.6875000000000163203, 0.7187500000000149880, 0.7343750000000135447, 0.7500000000000119904, 0.8750000000000059952, 1.000000000000000000 ),
 .UNSPECIFIED. ) ;
#29228 = CARTESIAN_POINT ( 'NONE',  ( 8.361422056298998484, -5.126342729456004221, 6.365321850284000327 ) ) ;
#29229 = EDGE_CURVE ( 'NONE', #21989, #19777, #52893, .T. ) ;
#29230 = LINE ( 'NONE', #2641, #8803 ) ;
#29231 = DIRECTION ( 'NONE',  ( -0.000000000000000000, -0.000000000000000000, 1.000000000000000000 ) ) ;
#29232 = CARTESIAN_POINT ( 'NONE',  ( 2.595292652382999776, 3.444664203886000031, -1.018890266960999824 ) ) ;
#29233 = ORIENTED_EDGE ( 'NONE', *, *, #42713, .T. ) ;
#29234 = CARTESIAN_POINT ( 'NONE',  ( 12.66323998097239922, -0.6090396975623090237, -12.68033511803396252 ) ) ;
#29236 = AXIS2_PLACEMENT_3D ( 'NONE', #59824, #11572, #16820 ) ;
#29235 = CARTESIAN_POINT ( 'NONE',  ( 5.399998535875000449, 12.99045401563999924, -1.690592933733000125 ) ) ;
#29237 = CARTESIAN_POINT ( 'NONE',  ( 10.10000011340999926, -1.190159082397999942E-13, -1.214010018759999782E-13 ) ) ;
#29238 = CARTESIAN_POINT ( 'NONE',  ( 7.486426658771000220, 5.321913229613000063, 8.118244847118999630 ) ) ;
#29239 = CARTESIAN_POINT ( 'NONE',  ( 18.30003129332100187, -2.732683818840999646, -11.53064095373000164 ) ) ;
#29240 = ORIENTED_EDGE ( 'NONE', *, *, #57016, .F. ) ;
#29241 = CARTESIAN_POINT ( 'NONE',  ( 5.286409705193999997, -0.1287196877685000129, 1.257471894813999791 ) ) ;
#29242 = B_SPLINE_CURVE_WITH_KNOTS ( 'NONE', 3,
 ( #51114, #56014, #30820, #30479 ),
 .UNSPECIFIED., .F., .F.,
 ( 4, 4 ),
 ( 0.000000000000000000, 1.000000000000000000 ),
 .UNSPECIFIED. ) ;
#29243 = CARTESIAN_POINT ( 'NONE',  ( 8.186735841226001398, 4.459320617394000763, -8.819879155908999735 ) ) ;
#29245 = PLANE ( 'NONE',  #43293 ) ;
#29244 = CARTESIAN_POINT ( 'NONE',  ( 8.576404413402933358, -4.033774881259239997, 5.760694017649135468 ) ) ;
#29246 = CARTESIAN_POINT ( 'NONE',  ( 11.60118044953561878, 5.133201153721000054, 6.909094663619399945 ) ) ;
#29247 = CARTESIAN_POINT ( 'NONE',  ( 8.486008579191000933, 3.399999999999999911, 5.976611076844000614 ) ) ;
#29248 = ORIENTED_EDGE ( 'NONE', *, *, #36220, .F. ) ;
#29249 = CARTESIAN_POINT ( 'NONE',  ( 12.79999999038796688, -11.45060587895086002, 4.713120762395663910 ) ) ;
#29250 = ORIENTED_EDGE ( 'NONE', *, *, #60447, .T. ) ;
#29251 = EDGE_CURVE ( 'NONE', #47653, #10995, #54983, .T. ) ;
#29252 = CARTESIAN_POINT ( 'NONE',  ( 16.39999999393279140, -3.428567374516922506, -11.90640519000895559 ) ) ;
#29253 = CARTESIAN_POINT ( 'NONE',  ( 7.533879440377999614, -4.623636604834999275, 8.651469651195000665 ) ) ;
#29254 = CARTESIAN_POINT ( 'NONE',  ( 18.20015658150182958, 0.3334496638227510412, -13.99603244703262739 ) ) ;
#29255 = ORIENTED_EDGE ( 'NONE', *, *, #39228, .T. ) ;
#29256 = CARTESIAN_POINT ( 'NONE',  ( 10.93115808116164445, 9.461016078471338631, -6.116472974095783499 ) ) ;
#29257 = CARTESIAN_POINT ( 'NONE',  ( 18.90826270587400160, -11.15000000000000036, -4.842665157767000124E-11 ) ) ;
#29258 = CARTESIAN_POINT ( 'NONE',  ( 10.57314899745999881, 5.167567567567999731, -6.822293592207000934 ) ) ;
#29259 = CARTESIAN_POINT ( 'NONE',  ( 10.14393020684899938, 5.250000000000000000, 7.500000000000000000 ) ) ;
#29260 = CYLINDRICAL_SURFACE ( 'NONE', #64146, 1.350000000000000533 ) ;
#29261 = ORIENTED_EDGE ( 'NONE', *, *, #50603, .F. ) ;
#29262 = DIRECTION ( 'NONE',  ( 1.000000000000000000, 0.000000000000000000, 0.000000000000000000 ) ) ;
#29263 = CARTESIAN_POINT ( 'NONE',  ( 23.55381274576900097, -13.39033134663000091, -4.196426638631999495 ) ) ;
#29264 = CARTESIAN_POINT ( 'NONE',  ( 11.59999999999999964, 5.250000000000000000, 7.500000000000000000 ) ) ;
#29265 = DIRECTION ( 'NONE',  ( 0.000000000000000000, 0.8648648648648717963, -0.5020047465136829867 ) ) ;
#29266 = CARTESIAN_POINT ( 'NONE',  ( 12.75534451565735417, -1.787855198891555641, 13.88537265576021262 ) ) ;
#29267 = ORIENTED_EDGE ( 'NONE', *, *, #267, .T. ) ;
#29268 = CARTESIAN_POINT ( 'NONE',  ( 0.000000000000000000, 0.000000000000000000, 0.000000000000000000 ) ) ;
#29269 = FACE_OUTER_BOUND ( 'NONE', #38695, .T. ) ;
#29270 = CARTESIAN_POINT ( 'NONE',  ( 7.093297165044828212, 2.144184834596416511, -7.429419625897773827 ) ) ;
#29271 = CARTESIAN_POINT ( 'NONE',  ( 23.78808895316426231, -3.294453063347192234, -13.15444831767801759 ) ) ;
#29272 = CARTESIAN_POINT ( 'NONE',  ( 24.30000000000000071, -9.305479840184000651, 8.315530346521999405 ) ) ;
#29273 = CARTESIAN_POINT ( 'NONE',  ( 12.18201982513761550, -0.05063168410658510504, -13.89988098555964946 ) ) ;
#29274 = CARTESIAN_POINT ( 'NONE',  ( 18.17988829291491371, -2.482516021556980590, 12.45565317647434611 ) ) ;
#29275 = ORIENTED_EDGE ( 'NONE', *, *, #8235, .F. ) ;
#29276 = CARTESIAN_POINT ( 'NONE',  ( 11.52677869730533011, -4.403502086956500250, -6.704332466833498927 ) ) ;
#29277 = VERTEX_POINT ( 'NONE', #47208 ) ;
#29278 = CARTESIAN_POINT ( 'NONE',  ( 0.1499942179679999987, 1.689975037551096015, 2.199046806507072294 ) ) ;
#29279 = CARTESIAN_POINT ( 'NONE',  ( 8.631645280409999899, 3.826300099041999747, -9.055335252254000267 ) ) ;
#29280 = CIRCLE ( 'NONE', #53811, 0.2999999999999993228 ) ;
#29281 = CARTESIAN_POINT ( 'NONE',  ( 2.454485126283999730, -2.645348439211000269, 1.827207675772000162 ) ) ;
#29282 = CARTESIAN_POINT ( 'NONE',  ( 10.13061232742999884, -2.189322372303999842, -7.101642112140999608 ) ) ;
#29283 = CARTESIAN_POINT ( 'NONE',  ( 7.000000000000000000, 7.526486366024999874, 3.526486366024999874 ) ) ;
#29284 = CARTESIAN_POINT ( 'NONE',  ( 9.042738649950948115, -4.892150455714567414, 8.513356723856825070 ) ) ;
#29285 = ADVANCED_FACE ( 'NONE', ( #63265 ), #7203, .T. ) ;
#29286 = ADVANCED_FACE ( 'NONE', ( #20197 ), #51668, .T. ) ;
#29287 = ORIENTED_EDGE ( 'NONE', *, *, #27056, .T. ) ;
#29288 = ADVANCED_FACE ( 'NONE', ( #3427 ), #35607, .T. ) ;
#29289 = CARTESIAN_POINT ( 'NONE',  ( 11.95764291764649911, -5.132124077409000229, 7.639947095788999221 ) ) ;
#29290 = CARTESIAN_POINT ( 'NONE',  ( 9.944319408602000365, 5.443001719280999851, 7.367350382395000175 ) ) ;
#29291 = CARTESIAN_POINT ( 'NONE',  ( 25.30000327618300204, -9.659335867304680079, -6.394377797198711910 ) ) ;
#29292 = DIRECTION ( 'NONE',  ( 0.000000000000000000, -0.1333333333333049930, -0.9910712498212376209 ) ) ;
#29294 = CARTESIAN_POINT ( 'NONE',  ( 9.092672482587163429, 4.128061954255975330, 8.851215505526871752 ) ) ;
#29293 = CARTESIAN_POINT ( 'NONE',  ( 9.753142190738998352, 4.104977339646000090, 9.293283246364000050 ) ) ;
#29295 = VECTOR ( 'NONE', #26353, 1000.000000000000000 ) ;
#29296 = CARTESIAN_POINT ( 'NONE',  ( 10.60441638348510018, 3.158410350011299883, -7.294998899090099798 ) ) ;
#29297 = DIRECTION ( 'NONE',  ( -1.000000000000000000, 0.000000000000000000, 0.000000000000000000 ) ) ;
#29298 = CIRCLE ( 'NONE', #67199, 12.52500000000000036 ) ;
#29299 = CARTESIAN_POINT ( 'NONE',  ( 8.897151519676997466, 4.024693162376980382, -8.641543873690000765 ) ) ;
#29300 = CARTESIAN_POINT ( 'NONE',  ( 18.26112048795754106, -0.1637242582067935659, 12.59894148523291157 ) ) ;
#29301 = CARTESIAN_POINT ( 'NONE',  ( 24.30000000000000071, 9.240454295252998662, 8.250504801592001058 ) ) ;
#29302 = CARTESIAN_POINT ( 'NONE',  ( 5.500000000000000000, -12.22293997673000021, 3.800173559041999827 ) ) ;
#29303 = CARTESIAN_POINT ( 'NONE',  ( 10.27367334122999942, 3.065551304793999510, -8.487910413489000661 ) ) ;
#29304 = ORIENTED_EDGE ( 'NONE', *, *, #65016, .T. ) ;
#29305 = CARTESIAN_POINT ( 'NONE',  ( 9.170316940378999249, -5.558929022707999046, 6.272984818914999927 ) ) ;
#29306 = CARTESIAN_POINT ( 'NONE',  ( 17.94133460182552753, 1.899620958390740855, 13.87053073593715169 ) ) ;
#29307 = CARTESIAN_POINT ( 'NONE',  ( 15.90003771078200145, -3.695138809391000034, -11.25918926437999978 ) ) ;
#29308 = CARTESIAN_POINT ( 'NONE',  ( 10.19391290906799874, 3.451408805716100314, 6.828616613600999585 ) ) ;
#29309 = ORIENTED_EDGE ( 'NONE', *, *, #57860, .T. ) ;
#29310 = CARTESIAN_POINT ( 'NONE',  ( 9.181704719590001673, 3.734279507827999556, 8.942126004519000304 ) ) ;
#29312 = CARTESIAN_POINT ( 'NONE',  ( 0.5765531495413795948, 3.350104404781542033, 1.142356188860006228 ) ) ;
#29311 = CARTESIAN_POINT ( 'NONE',  ( 9.988985841228000595, 3.986577607995999806, -9.280166295424001177 ) ) ;
#29313 = CARTESIAN_POINT ( 'NONE',  ( 10.75915165876999957, 5.387277012365999873, -6.278112168454999420 ) ) ;
#29314 = ORIENTED_EDGE ( 'NONE', *, *, #45453, .T. ) ;
#29315 = CARTESIAN_POINT ( 'NONE',  ( 10.72520610419000064, 5.521650664120000940, 6.612990918765000004 ) ) ;
#29316 = DIRECTION ( 'NONE',  ( 1.000000000000000000, 0.000000000000000000, 0.000000000000000000 ) ) ;
#29317 = CARTESIAN_POINT ( 'NONE',  ( 11.43302763632549990, 2.964209339073000216, 7.977941233841399971 ) ) ;
#29318 = CARTESIAN_POINT ( 'NONE',  ( 9.444317341922999987, -2.927260449021000355, 8.897015448164999896 ) ) ;
#29319 = CARTESIAN_POINT ( 'NONE',  ( 8.736820887142258130, 3.746718250072767376, -8.358484985884542695 ) ) ;
#29320 = VERTEX_POINT ( 'NONE', #68423 ) ;
#29321 = CARTESIAN_POINT ( 'NONE',  ( 12.80505043854143210, 3.248147246781388553, 13.61798588129781251 ) ) ;
#29322 = CARTESIAN_POINT ( 'NONE',  ( 1.417640132541000186, 1.762666431298152370, -3.058252359239900464 ) ) ;
#29323 = B_SPLINE_CURVE_WITH_KNOTS ( 'NONE', 3,
 ( #34414, #8175, #46271, #18667, #67574, #55731, #66893, #39999, #41019, #19005, #29169, #8517, #62341, #50477, #29865, #2579, #3268, #23907, #61313, #13434, #34755, #50826 ),
 .UNSPECIFIED., .F., .F.,
 ( 4, 2, 2, 1, 2, 2, 2, 1, 1, 1, 2, 2, 4 ),
 ( 0.000000000000000000, 0.2499999999999572564, 0.3749999999999340528, 0.4374999999999227840, 0.4687499999999181211, 0.4999999999999135136, 0.6249999999999101830, 0.6874999999999068523, 0.7187499999999039657, 0.7343749999999026334, 0.7421874999999006350, 0.7499999999998986366, 1.000000000000000000 ),
 .UNSPECIFIED. ) ;
#29324 = CARTESIAN_POINT ( 'NONE',  ( 7.948545716009685513, -2.259334748069345977, 7.519046407094909235 ) ) ;
#29325 = CARTESIAN_POINT ( 'NONE',  ( 9.137549407199999862, -2.995696424181999884, 8.544763501938000161 ) ) ;
#29326 = CARTESIAN_POINT ( 'NONE',  ( 11.26723293495529887, -5.173938955706000264, -7.452807962566580180 ) ) ;
#29327 = CARTESIAN_POINT ( 'NONE',  ( 10.43659632033899953, -5.057167065956000407, 7.931430460958599049 ) ) ;
#29328 = ORIENTED_EDGE ( 'NONE', *, *, #45625, .F. ) ;
#29330 = CARTESIAN_POINT ( 'NONE',  ( 24.15455566405240617, -9.133426265715067771, 9.111863915754568666 ) ) ;
#29329 = VECTOR ( 'NONE', #67272, 1000.000000000000000 ) ;
#29331 = CARTESIAN_POINT ( 'NONE',  ( 10.62841772631199966, -3.509411006705700053, 6.490165927606000196 ) ) ;
#29332 = VERTEX_POINT ( 'NONE', #4108 ) ;
#29333 = EDGE_CURVE ( 'NONE', #65921, #17154, #62496, .T. ) ;
#29334 = DIRECTION ( 'NONE',  ( 0.000000000000000000, -0.7071067811865475727, -0.7071067811865475727 ) ) ;
#29335 = ORIENTED_EDGE ( 'NONE', *, *, #27109, .F. ) ;
#29336 = CARTESIAN_POINT ( 'NONE',  ( 9.575728814717999526, -3.111669560323000017, -8.958991988670002016 ) ) ;
#29337 = CARTESIAN_POINT ( 'NONE',  ( 9.550320280412000429, 2.370176859044999862, -6.912649125838000508 ) ) ;
#29338 = EDGE_CURVE ( 'NONE', #37404, #56515, #22923, .T. ) ;
#29339 = CARTESIAN_POINT ( 'NONE',  ( 11.55300581613033906, 5.107584469683000172, -8.211208432468300344 ) ) ;
#29340 = FACE_OUTER_BOUND ( 'NONE', #58833, .T. ) ;
#29341 = CARTESIAN_POINT ( 'NONE',  ( 12.20998423544383904, 2.691370015539682026, -12.40494896326797303 ) ) ;
#29342 = CARTESIAN_POINT ( 'NONE',  ( 11.88379707368349969, -4.566644629509899467, 8.490052513816499058 ) ) ;
#29343 = CARTESIAN_POINT ( 'NONE',  ( 11.43990547754509990, -2.967013601007999934, 7.467215766047949899 ) ) ;
#29344 = ORIENTED_EDGE ( 'NONE', *, *, #39476, .T. ) ;
#29345 = FACE_OUTER_BOUND ( 'NONE', #14711, .T. ) ;
#29346 = AXIS2_PLACEMENT_3D ( 'NONE', #38238, #53637, #11321 ) ;
#29347 = VERTEX_POINT ( 'NONE', #13938 ) ;
#29348 = CARTESIAN_POINT ( 'NONE',  ( 7.866206853207000194, -4.580607464247000493, 9.213361409141999303 ) ) ;
#29349 = B_SPLINE_CURVE_WITH_KNOTS ( 'NONE', 3,
 ( #61625, #66866, #67893, #13403 ),
 .UNSPECIFIED., .F., .F.,
 ( 4, 4 ),
 ( 0.000000000000000000, 1.000000000000000000 ),
 .UNSPECIFIED. ) ;
#29350 = CARTESIAN_POINT ( 'NONE',  ( 7.954299074928001367, 3.414461172233999697, -6.283593702261001113 ) ) ;
#29351 = ORIENTED_EDGE ( 'NONE', *, *, #22813, .T. ) ;
#29352 = CARTESIAN_POINT ( 'NONE',  ( 12.09087492024913679, -2.355317862440514887, -12.37790828721919212 ) ) ;
#29353 = CARTESIAN_POINT ( 'NONE',  ( 11.18687482311539938, 5.057677595549000316, 7.072673169413499217 ) ) ;
#29354 = FACE_OUTER_BOUND ( 'NONE', #8350, .T. ) ;
#29355 = DIRECTION ( 'NONE',  ( 1.000000000000000000, 0.000000000000000000, 0.000000000000000000 ) ) ;
#29356 = CARTESIAN_POINT ( 'NONE',  ( 17.60718180634500030, -11.44293104347999979, 4.697469793150999884 ) ) ;
#29357 = CARTESIAN_POINT ( 'NONE',  ( 9.035395982797805203, 3.688926447190845170, -8.654212551762981320 ) ) ;
#29358 = DIRECTION ( 'NONE',  ( 0.000000000000000000, 1.000000000000000000, 0.000000000000000000 ) ) ;
#29359 = CARTESIAN_POINT ( 'NONE',  ( 5.205914323403000310, 0.3864793456783000014, -1.508803618046000272 ) ) ;
#29360 = CARTESIAN_POINT ( 'NONE',  ( 11.07210672858429845, -4.692204557952299737, -6.979277962544199632 ) ) ;
#29361 = CARTESIAN_POINT ( 'NONE',  ( 11.37964291764649971, -5.268358781405000357, -7.343212302062899433 ) ) ;
#29362 = CARTESIAN_POINT ( 'NONE',  ( 8.700642219592999993, 5.212261578733999201, 6.157186134061999994 ) ) ;
#29363 = ORIENTED_EDGE ( 'NONE', *, *, #61088, .F. ) ;
#29364 = B_SPLINE_CURVE_WITH_KNOTS ( 'NONE', 3,
 ( #8796, #66831, #56696, #61589 ),
 .UNSPECIFIED., .F., .F.,
 ( 4, 4 ),
 ( 0.000000000000000000, 1.000000000000000000 ),
 .UNSPECIFIED. ) ;
#29365 =( LENGTH_UNIT ( ) NAMED_UNIT ( * ) SI_UNIT ( .MILLI., .METRE. ) );
#29366 = DIRECTION ( 'NONE',  ( -1.000000000000000000, 5.329070518330000258E-14, -1.243449787610000074E-13 ) ) ;
#29367 = CARTESIAN_POINT ( 'NONE',  ( 18.08671416524397912, 2.828730077974936030, 13.59817001273920489 ) ) ;
#29368 = CARTESIAN_POINT ( 'NONE',  ( 10.84087666499999969, 2.636288985756999992, -7.512643730465999425 ) ) ;
#29369 = CARTESIAN_POINT ( 'NONE',  ( 17.74302412089499015, 1.903914349118853488, 12.57063651914289437 ) ) ;
#29370 = CARTESIAN_POINT ( 'NONE',  ( 11.59999999999999964, 4.000000000000000000, -7.500000000000000000 ) ) ;
#29372 = EDGE_CURVE ( 'NONE', #50410, #9350, #43907, .T. ) ;
#29371 = CARTESIAN_POINT ( 'NONE',  ( 9.657553581808000942, 5.333455947841000189, 6.049916795084000043 ) ) ;
#29373 = DIRECTION ( 'NONE',  ( -1.000000000000000000, 0.000000000000000000, 0.000000000000000000 ) ) ;
#29374 = EDGE_CURVE ( 'NONE', #31101, #50410, #31388, .T. ) ;
#29375 = EDGE_CURVE ( 'NONE', #25798, #21322, #4590, .T. ) ;
#29376 = VERTEX_POINT ( 'NONE', #14281 ) ;
#29377 = CARTESIAN_POINT ( 'NONE',  ( 12.19547854351947080, -2.361608046327441812, 12.48276200957626081 ) ) ;
#29378 = B_SPLINE_CURVE_WITH_KNOTS ( 'NONE', 3,
 ( #30093, #40906, #8408, #67805 ),
 .UNSPECIFIED., .F., .F.,
 ( 4, 4 ),
 ( 0.000000000000000000, 1.000000000000000000 ),
 .UNSPECIFIED. ) ;
#29379 = CARTESIAN_POINT ( 'NONE',  ( 9.680342523874998051, -4.992846242613000030, -7.348017636355000270 ) ) ;
#29380 = CARTESIAN_POINT ( 'NONE',  ( 10.85069631730999973, 4.478098874537000285, 6.162039661770999821 ) ) ;
#29381 = CARTESIAN_POINT ( 'NONE',  ( 12.21922412107039868, -3.930460928605089777, 8.814426450544999625 ) ) ;
#29382 = AXIS2_PLACEMENT_3D ( 'NONE', #50359, #67449, #7353 ) ;
#29383 = PRODUCT_DEFINITION_SHAPE ( 'NONE', 'NONE',  #46633 ) ;
#29384 = CARTESIAN_POINT ( 'NONE',  ( 10.34995525820099971, 3.892289273474800471, -6.364355462479999836 ) ) ;
#29385 = CARTESIAN_POINT ( 'NONE',  ( 12.19008233596125379, 0.1120021961262550880, 12.69934078656687682 ) ) ;
#29386 = B_SPLINE_CURVE_WITH_KNOTS ( 'NONE', 3,
 ( #64160, #5444, #43541, #54364, #59956, #38988, #37941, #49462 ),
 .UNSPECIFIED., .F., .F.,
 ( 4, 2, 2, 4 ),
 ( 0.000000000000000000, 0.4999999999999995559, 0.7499999999999997780, 1.000000000000000000 ),
 .UNSPECIFIED. ) ;
#29387 = CARTESIAN_POINT ( 'NONE',  ( 7.994579719591000000, 2.263558315407000254, 8.007442119518000112 ) ) ;
#29388 = CARTESIAN_POINT ( 'NONE',  ( 9.034110134264999203, 4.695345051283999815, 8.660667941667000491 ) ) ;
#29389 = CARTESIAN_POINT ( 'NONE',  ( 12.18490839767382816, 2.421563015655831652, 12.46949130182971821 ) ) ;
#29390 = ORIENTED_EDGE ( 'NONE', *, *, #33538, .F. ) ;
#29391 = CARTESIAN_POINT ( 'NONE',  ( 8.500189158773000742, 2.724453559418999582, -8.908010318766001134 ) ) ;
#29392 = CARTESIAN_POINT ( 'NONE',  ( 11.33041235500449950, 3.057642534728299832, -6.636704692336500067 ) ) ;
#29393 = EDGE_CURVE ( 'NONE', #23992, #26199, #49546, .T. ) ;
#29394 = CARTESIAN_POINT ( 'NONE',  ( 9.843930206850000530, 2.750000000000000000, -7.500000000000000000 ) ) ;
#29396 = CARTESIAN_POINT ( 'NONE',  ( 11.51961669203094196, 5.030276287827526005, -7.175016092226064401 ) ) ;
#29395 = CARTESIAN_POINT ( 'NONE',  ( 7.571668146791999732, -2.531197775378000170, 8.216705951490000714 ) ) ;
#29397 = CARTESIAN_POINT ( 'NONE',  ( 10.53992546752099990, -5.002009261081000524, 7.569424354486659290 ) ) ;
#29398 = CARTESIAN_POINT ( 'NONE',  ( 11.73256516821459883, -3.293702443348299980, -8.212808089543500500 ) ) ;
#29399 = ORIENTED_EDGE ( 'NONE', *, *, #37311, .F. ) ;
#29400 = AXIS2_PLACEMENT_3D ( 'NONE', #8439, #14034, #35360 ) ;
#29401 = CARTESIAN_POINT ( 'NONE',  ( 1.162427948746999951, -2.208354302538000358, -2.618776384398000090 ) ) ;
#29402 = DIRECTION ( 'NONE',  ( 1.000000000000000000, 0.000000000000000000, 0.000000000000000000 ) ) ;
#29403 = AXIS2_PLACEMENT_3D ( 'NONE', #68031, #26782, #20147 ) ;
#29404 = CARTESIAN_POINT ( 'NONE',  ( 9.403317944506802917, -4.274905112035348509, 8.526233764311365704 ) ) ;
#29405 = CARTESIAN_POINT ( 'NONE',  ( 18.01231764196698748, -2.926478478965309105, 13.57371117741642408 ) ) ;
#29406 = B_SPLINE_CURVE_WITH_KNOTS ( 'NONE', 3,
 ( #38174, #47651, #21749, #58136, #68963, #27353 ),
 .UNSPECIFIED., .F., .F.,
 ( 4, 2, 4 ),
 ( 0.000000000000000000, 0.1967045975185045814, 0.3934091950370091628 ),
 .UNSPECIFIED. ) ;
#29407 = B_SPLINE_CURVE_WITH_KNOTS ( 'NONE', 3,
 ( #16696, #37343, #53427, #42257 ),
 .UNSPECIFIED., .F., .F.,
 ( 4, 4 ),
 ( 0.000000000000000000, 1.000000000000000000 ),
 .UNSPECIFIED. ) ;
#29408 = CARTESIAN_POINT ( 'NONE',  ( 24.66122485283899834, -12.38509973019000121, 2.963735973451999683 ) ) ;
#29409 = CARTESIAN_POINT ( 'NONE',  ( 12.48231810865427249, -3.171873548221312067, 13.63595416837495122 ) ) ;
#29410 = CARTESIAN_POINT ( 'NONE',  ( 11.50001436749000128, -11.64999275565999959, -4.104694901035999596E-10 ) ) ;
#29411 = CARTESIAN_POINT ( 'NONE',  ( 0.1499942179679999987, 5.893556041935713383E-16, -2.749976859058071543 ) ) ;
#29412 = CARTESIAN_POINT ( 'NONE',  ( 8.245293146793999384, -4.282999948634999221, 9.286791354293999490 ) ) ;
#29413 = ORIENTED_EDGE ( 'NONE', *, *, #45806, .T. ) ;
#29414 = CARTESIAN_POINT ( 'NONE',  ( 8.149357780409999918, 2.583668273793999770, 6.684750595573999199 ) ) ;
#29415 = CARTESIAN_POINT ( 'NONE',  ( 24.72675064436329606, -8.645756478877553164, 8.593170189962409111 ) ) ;
#29416 = CARTESIAN_POINT ( 'NONE',  ( 7.433354534967393512, -2.295543244304647512, 7.846514096336020927 ) ) ;
#29417 = CARTESIAN_POINT ( 'NONE',  ( 17.80428097309404833, -0.5732560958719012945, 13.88408533439657511 ) ) ;
#29418 = CARTESIAN_POINT ( 'NONE',  ( 1.891066937564000128, -3.444624976169999631, -1.019033653642999804 ) ) ;
#29419 = VERTEX_POINT ( 'NONE', #15984 ) ;
#29420 = CARTESIAN_POINT ( 'NONE',  ( 1.761390132539666808, -3.499999999999999556, -0.4581489286485119772 ) ) ;
#29421 = CARTESIAN_POINT ( 'NONE',  ( 10.98973493139468793, -3.461032840053388515, -9.181186645308331506 ) ) ;
#29422 = CARTESIAN_POINT ( 'NONE',  ( 9.834151567923001380, 5.173929249342999803, 8.813048229486998508 ) ) ;
#29423 = EDGE_CURVE ( 'NONE', #30301, #40828, #45478, .T. ) ;
#29424 = CARTESIAN_POINT ( 'NONE',  ( 11.68333460557258796, 4.162011815820000571, 6.509695444280099608 ) ) ;
#29425 = CARTESIAN_POINT ( 'NONE',  ( 5.000000000000000000, 0.2999999999999999889, 9.776630298829998011 ) ) ;
#29426 = CARTESIAN_POINT ( 'NONE',  ( 18.29983863916000075, 2.861762957209999847, -11.98830831200999825 ) ) ;
#29427 = ADVANCED_FACE ( 'NONE', ( #43249 ), #32723, .T. ) ;
#29428 = CARTESIAN_POINT ( 'NONE',  ( 11.66883611461859971, 3.345349279800629905, -11.86065815404513479 ) ) ;
#29429 = CARTESIAN_POINT ( 'NONE',  ( 8.474485200571999499, 5.100000000000000533, 6.560614371780999043 ) ) ;
#29430 = CARTESIAN_POINT ( 'NONE',  ( 12.18396690407210770, -2.429413046053483960, 12.46775848779559759 ) ) ;
#29431 = AXIS2_PLACEMENT_3D ( 'NONE', #57342, #62255, #66815 ) ;
#29432 = CARTESIAN_POINT ( 'NONE',  ( 8.536950018568271403, 3.172726136472098446, 5.956131468116810268 ) ) ;
#29433 = VERTEX_POINT ( 'NONE', #15644 ) ;
#29434 = CONICAL_SURFACE ( 'NONE', #4841, 12.44999944941000081, 0.7853981146832407223 ) ;
#29435 = CARTESIAN_POINT ( 'NONE',  ( 17.83362577474381183, -1.940423258991959665, 13.77633750067930407 ) ) ;
#29436 = FACE_OUTER_BOUND ( 'NONE', #59575, .T. ) ;
#29437 = ORIENTED_EDGE ( 'NONE', *, *, #63908, .T. ) ;
#29438 = DIRECTION ( 'NONE',  ( 1.000000000000000000, 0.000000000000000000, -4.770489558936215471E-13 ) ) ;
#29439 = CARTESIAN_POINT ( 'NONE',  ( 9.581163468719390508, -9.035708932181609754, 6.816351070799544054 ) ) ;
#29440 = CARTESIAN_POINT ( 'NONE',  ( 24.44496356232399847, -3.224881240379999792, -12.03535804424000055 ) ) ;
#29441 = CARTESIAN_POINT ( 'NONE',  ( 10.47706399772000019, -8.232249776294999322, 6.630938099616999537 ) ) ;
#29442 = CARTESIAN_POINT ( 'NONE',  ( 9.781673028307999118, 5.464749740720999505, 8.817329433105999925 ) ) ;
#29443 = CARTESIAN_POINT ( 'NONE',  ( 9.898128230592000421, 2.965931985296999862, -6.610871072364999712 ) ) ;
#29444 = CARTESIAN_POINT ( 'NONE',  ( 10.13559687351567007, -2.907767014557175678, -6.870476274536380323 ) ) ;
#29445 = CARTESIAN_POINT ( 'NONE',  ( 9.869049086607999399, -5.575175898444999945, 7.724300702620999104 ) ) ;
#29446 = CARTESIAN_POINT ( 'NONE',  ( 17.74252821691605675, 0.6952251598378719200, -12.58080715426406293 ) ) ;
#29447 = CARTESIAN_POINT ( 'NONE',  ( 10.01276877312999858, -3.440626575163999945, -9.267592337498999910 ) ) ;
#29448 = CARTESIAN_POINT ( 'NONE',  ( 11.56025819896753859, -4.986099335708799707, -7.685900384398899554 ) ) ;
#29449 = CARTESIAN_POINT ( 'NONE',  ( 10.64946917938723558, -2.962827107629537604, -5.047145064087899868 ) ) ;
#29450 = ORIENTED_EDGE ( 'NONE', *, *, #30235, .F. ) ;
#29451 = CIRCLE ( 'NONE', #42793, 2.199999999999999734 ) ;
#29452 = CARTESIAN_POINT ( 'NONE',  ( 8.810863317747999801, 4.960863370448500120, -7.500000000073117512 ) ) ;
#29453 = SURFACE_STYLE_USAGE ( .BOTH. , #44145 ) ;
#29454 = CARTESIAN_POINT ( 'NONE',  ( 24.65659314676950231, 8.681452214508958320, 8.652166108174951020 ) ) ;
#29455 = AXIS2_PLACEMENT_3D ( 'NONE', #56016, #39945, #51116 ) ;
#29456 = CARTESIAN_POINT ( 'NONE',  ( 5.000030787342999439, 1.834918991542626499, -1.057581170753191913 ) ) ;
#29457 = CARTESIAN_POINT ( 'NONE',  ( 9.203113844318000503, 4.323050436788100193, -6.262250912840999106 ) ) ;
#29458 = CARTESIAN_POINT ( 'NONE',  ( 12.51733672169663869, 1.945066915100360116, 13.77556489992940847 ) ) ;
#29459 = CARTESIAN_POINT ( 'NONE',  ( 9.778462793022999477, -5.743713977826000239, 7.748300060190000060 ) ) ;
#29460 = ORIENTED_EDGE ( 'NONE', *, *, #14445, .F. ) ;
#29461 = CARTESIAN_POINT ( 'NONE',  ( 12.44983299083951600, 0.5143225249093883455, -12.68597987476780276 ) ) ;
#29462 = B_SPLINE_CURVE_WITH_KNOTS ( 'NONE', 3,
 ( #38345, #55472, #59325, #6875 ),
 .UNSPECIFIED., .F., .F.,
 ( 4, 4 ),
 ( 0.000000000000000000, 1.000000000000000000 ),
 .UNSPECIFIED. ) ;
#29463 = EDGE_CURVE ( 'NONE', #17417, #23021, #58289, .T. ) ;
#29464 = CARTESIAN_POINT ( 'NONE',  ( 12.47502503668309615, -0.5311540453515625204, 13.88634387573209139 ) ) ;
#29465 = EDGE_CURVE ( 'NONE', #51860, #46362, #49483, .T. ) ;
#29466 = ORIENTED_EDGE ( 'NONE', *, *, #24224, .F. ) ;
#29467 = CARTESIAN_POINT ( 'NONE',  ( 11.59999999999999964, 4.000000000000000000, -7.500000000000000000 ) ) ;
#29468 = CARTESIAN_POINT ( 'NONE',  ( 12.09999999999999964, -4.817420948848700313, 7.825000000000000178 ) ) ;
#29469 = CARTESIAN_POINT ( 'NONE',  ( 8.973608660036624940, 4.220957842099207546, 8.346587208109317757 ) ) ;
#29470 = FACE_OUTER_BOUND ( 'NONE', #7857, .T. ) ;
#29471 = CARTESIAN_POINT ( 'NONE',  ( 8.761020418847346392, 3.646575901141349885, -8.850808559580910284 ) ) ;
#29472 = CARTESIAN_POINT ( 'NONE',  ( 10.55478570706233299, 5.131706358131709500, 6.886599490775120458 ) ) ;
#29473 = CARTESIAN_POINT ( 'NONE',  ( 0.4936698601467999770, 3.273731968234999901, -1.479853775367000246 ) ) ;
#29474 = DIRECTION ( 'NONE',  ( 0.000000000000000000, 0.8648648648648717963, -0.5020047465136829867 ) ) ;
#29475 = CARTESIAN_POINT ( 'NONE',  ( 10.45551210286900279, -4.217228369037729685, -8.756187319522085843 ) ) ;
#29476 = CARTESIAN_POINT ( 'NONE',  ( 21.59999953993000332, -1.509903313490000218E-14, 4.329869796037999436E-14 ) ) ;
#29477 = CARTESIAN_POINT ( 'NONE',  ( 11.75718044953559804, 4.889766368533900120, -7.963966784336999005 ) ) ;
#29478 = CARTESIAN_POINT ( 'NONE',  ( 6.999998971696826722, -12.01547034654744195, -3.452253082527627637 ) ) ;
#29479 = VECTOR ( 'NONE', #2618, 1000.000000000000227 ) ;
#29480 = DIRECTION ( 'NONE',  ( -1.000000000000000000, 0.000000000000000000, 0.000000000000000000 ) ) ;
#29481 = EDGE_CURVE ( 'NONE', #17007, #2520, #2867, .T. ) ;
#29482 = CARTESIAN_POINT ( 'NONE',  ( 8.655265421554998895, 3.811499292588199861, -8.475084258675400051 ) ) ;
#29484 = CARTESIAN_POINT ( 'NONE',  ( 12.18782402014237753, 2.399945986244715446, 12.47432385254658804 ) ) ;
#29483 = CARTESIAN_POINT ( 'NONE',  ( 17.80000000009400196, 3.216307036143000175, 11.40341376487999980 ) ) ;
#29485 = CARTESIAN_POINT ( 'NONE',  ( 6.778816671981999775, -0.8882170986559999593, 0.6661914818925001036 ) ) ;
#29486 = VERTEX_POINT ( 'NONE', #69124 ) ;
#29487 = VECTOR ( 'NONE', #35130, 1000.000000000000000 ) ;
#29488 = MANIFOLD_SOLID_BREP ( 'Stock-MAS-678-1', #3474 ) ;
#29489 = B_SPLINE_CURVE_WITH_KNOTS ( 'NONE', 3,
 ( #67610, #36154, #35481, #41058, #67960, #19737 ),
 .UNSPECIFIED., .F., .F.,
 ( 4, 2, 4 ),
 ( 0.000000000000000000, 0.4999999999999995559, 1.000000000000000000 ),
 .UNSPECIFIED. ) ;
#29490 = CARTESIAN_POINT ( 'NONE',  ( 10.65413259636999932, 3.216622244594500302, 7.073141822156699732 ) ) ;
#29491 = CARTESIAN_POINT ( 'NONE',  ( 10.74609562913000005, -4.263104965433000437, 9.276976808608999647 ) ) ;
#29492 = CARTESIAN_POINT ( 'NONE',  ( 9.680342523874998051, 3.007153757386999526, 7.651982363644999730 ) ) ;
#29493 = CARTESIAN_POINT ( 'NONE',  ( 9.733483075504627990, 3.885520926571138567, -8.367425391989351979 ) ) ;
#29494 = CARTESIAN_POINT ( 'NONE',  ( 23.60205915885299888, 11.56239291744999065, -3.974820703413998846 ) ) ;
#29495 = CARTESIAN_POINT ( 'NONE',  ( 13.50018479229797208, 11.40740214419261278, 3.347185923349937031 ) ) ;
#29496 = ORIENTED_EDGE ( 'NONE', *, *, #4347, .T. ) ;
#29497 = AXIS2_PLACEMENT_3D ( 'NONE', #21549, #15963, #53717 ) ;
#29498 = CARTESIAN_POINT ( 'NONE',  ( 9.987254614702999689, -5.106563667948999630, -7.781516069110699263 ) ) ;
#29499 = CARTESIAN_POINT ( 'NONE',  ( 10.99999975383417627, 2.937013229513552925, -7.366608021396839234 ) ) ;
#29500 = CARTESIAN_POINT ( 'NONE',  ( 18.23564136049837003, 2.231667926091399412, -12.40079771041855849 ) ) ;
#29501 = CARTESIAN_POINT ( 'NONE',  ( 11.04839869688000142, -2.759396991474999616, 5.061364986604000471 ) ) ;
#29502 = AXIS2_PLACEMENT_3D ( 'NONE', #44826, #49019, #22440 ) ;
#29503 = CARTESIAN_POINT ( 'NONE',  ( 21.60000012424471194, -13.89999856298999958, 0.000000000000000000 ) ) ;
#29504 = CARTESIAN_POINT ( 'NONE',  ( 12.22445506991028807, 2.731418686063790791, -13.62164890390593008 ) ) ;
#29505 = CARTESIAN_POINT ( 'NONE',  ( 9.927916723342999461, -5.290169207169999943, -8.858081286661999343 ) ) ;
#29506 = CARTESIAN_POINT ( 'NONE',  ( 8.433148997460000018, -5.167567567567999731, 6.822293592207000934 ) ) ;
#29507 = EDGE_CURVE ( 'NONE', #61617, #25033, #43734, .T. ) ;
#29508 = VERTEX_POINT ( 'NONE', #21569 ) ;
#29509 = CARTESIAN_POINT ( 'NONE',  ( 11.09999999999999964, -5.449702613288000208, -5.124965750789000296 ) ) ;
#29510 = CONICAL_SURFACE ( 'NONE', #26142, 12.49999584805000019, 0.7853981146832407223 ) ;
#29511 = CARTESIAN_POINT ( 'NONE',  ( 12.22921562908470072, -0.4443071882833348196, -13.99296005428181466 ) ) ;
#29512 = CARTESIAN_POINT ( 'NONE',  ( 8.406851002545000284, 2.832432432432000269, -6.822293592207000934 ) ) ;
#29513 = CARTESIAN_POINT ( 'NONE',  ( 10.05091168077847108, -5.349831496875363968, -7.263252183692045172 ) ) ;
#29514 = B_SPLINE_CURVE_WITH_KNOTS ( 'NONE', 3,
 ( #60710, #17728, #60022, #12132 ),
 .UNSPECIFIED., .F., .F.,
 ( 4, 4 ),
 ( 0.000000000000000000, 1.000000000000000000 ),
 .UNSPECIFIED. ) ;
#29515 = CARTESIAN_POINT ( 'NONE',  ( 25.41798597150000205, -8.397682312107999536, -8.090308797361000615 ) ) ;
#29516 = CARTESIAN_POINT ( 'NONE',  ( 9.617764158771999305, 5.322769172805999816, -7.951018786192998178 ) ) ;
#29517 = CARTESIAN_POINT ( 'NONE',  ( 12.35159063708299954, -3.174974693948799942, 7.268038553423699533 ) ) ;
#29518 = ORIENTED_EDGE ( 'NONE', *, *, #26269, .T. ) ;
#29519 = B_SPLINE_CURVE_WITH_KNOTS ( 'NONE', 3,
 ( #34456, #59971, #18368, #12777 ),
 .UNSPECIFIED., .F., .F.,
 ( 4, 4 ),
 ( 0.000000000000000000, 1.000000000000000000 ),
 .UNSPECIFIED. ) ;
#29520 = CARTESIAN_POINT ( 'NONE',  ( 9.292123497980924185, -3.170553882200173756, -8.579481765757963174 ) ) ;
#29521 = CARTESIAN_POINT ( 'NONE',  ( 17.59651827076216080, 1.876037923068245794, -13.78616466676677632 ) ) ;
#29522 = ORIENTED_EDGE ( 'NONE', *, *, #50997, .F. ) ;
#29523 = CARTESIAN_POINT ( 'NONE',  ( 8.528661480133287398, 4.352698949118988025, 8.815590613233503348 ) ) ;
#29524 = DIRECTION ( 'NONE',  ( -1.000000000000000000, 0.000000000000000000, 0.000000000000000000 ) ) ;
#29525 = CARTESIAN_POINT ( 'NONE',  ( 9.898395280408998076, 3.987760651117999711, -9.123263301387000368 ) ) ;
#29526 = CARTESIAN_POINT ( 'NONE',  ( 23.80820397230190011, -13.01045451829668842, 3.693343721330374141 ) ) ;
#29527 = CARTESIAN_POINT ( 'NONE',  ( 11.26723293495529887, -5.173938955706000264, -7.452807962566580180 ) ) ;
#29528 = CARTESIAN_POINT ( 'NONE',  ( 9.316292271078561171, -5.056976493916715221, -6.220632899828596685 ) ) ;
#29529 = CARTESIAN_POINT ( 'NONE',  ( 4.940443173016666023, -0.1963495408493673156, 1.499999999999999556 ) ) ;
#29530 = EDGE_LOOP ( 'NONE', ( #66596, #64945, #14028, #46113 ) ) ;
#29531 = CARTESIAN_POINT ( 'NONE',  ( 7.773105724985851950, 3.449994720449756525, -8.750200106293087643 ) ) ;
#29532 = CARTESIAN_POINT ( 'NONE',  ( 7.732053843957007899, 3.067861388767125774, 6.507875342627428950 ) ) ;
#29533 = CARTESIAN_POINT ( 'NONE',  ( 8.997439158776000312, 2.773858540272000184, -8.951250717848999727 ) ) ;
#29534 = ORIENTED_EDGE ( 'NONE', *, *, #20628, .F. ) ;
#29535 = CIRCLE ( 'NONE', #57393, 2.149999999999999911 ) ;
#29536 = CARTESIAN_POINT ( 'NONE',  ( 10.34224945431000009, 3.348985101650000296, -8.881460768006000706 ) ) ;
#29537 = FACE_OUTER_BOUND ( 'NONE', #29538, .T. ) ;
#29538 = EDGE_LOOP ( 'NONE', ( #66118, #22696, #60433, #65275 ) ) ;
#29539 = CARTESIAN_POINT ( 'NONE',  ( 8.822113844317998499, 4.288351516201100111, 8.604802177355001191 ) ) ;
#29540 = CARTESIAN_POINT ( 'NONE',  ( 18.25660817874747721, -2.298073654326284299, -12.38866391276717316 ) ) ;
#29541 = DIRECTION ( 'NONE',  ( 0.000000000000000000, -0.9586353287323918781, 0.2846371488511973413 ) ) ;
#29542 = DIRECTION ( 'NONE',  ( 0.000000000000000000, 1.000000000000000000, 0.000000000000000000 ) ) ;
#29543 = B_SPLINE_CURVE_WITH_KNOTS ( 'NONE', 3,
 ( #50014, #18547, #17860, #65737, #61534, #7354 ),
 .UNSPECIFIED., .F., .F.,
 ( 4, 2, 4 ),
 ( 0.000000000000000000, 0.5000000000000000000, 1.000000000000000000 ),
 .UNSPECIFIED. ) ;
#29544 = CARTESIAN_POINT ( 'NONE',  ( 24.31006797060300073, -12.13011445653000031, -3.289861759914999517 ) ) ;
#29545 = EDGE_CURVE ( 'NONE', #15877, #61826, #17099, .T. ) ;
#29546 = CARTESIAN_POINT ( 'NONE',  ( 9.382540076676905372, -2.847952239995268808, 8.803561693506937402 ) ) ;
#29547 = EDGE_CURVE ( 'NONE', #68281, #54071, #48811, .T. ) ;
#29548 = EDGE_LOOP ( 'NONE', ( #52627, #46515, #67520, #12269 ) ) ;
#29549 = DIRECTION ( 'NONE',  ( 1.000000000000000000, 0.000000000000000000, 0.000000000000000000 ) ) ;
#29550 = CARTESIAN_POINT ( 'NONE',  ( 10.17270667456000055, 4.650145611776999921, -8.655516756809999990 ) ) ;
#29551 = CARTESIAN_POINT ( 'NONE',  ( 9.933148997456999751, -5.167567567567999731, 6.822293592207000934 ) ) ;
#29552 = CARTESIAN_POINT ( 'NONE',  ( 12.14421144042236378, 2.819066901275890213, -13.71325475029871299 ) ) ;
#29553 = CARTESIAN_POINT ( 'NONE',  ( 9.228442991499999692, -4.080527519162810535, -6.223324745230999433 ) ) ;
#29554 = CARTESIAN_POINT ( 'NONE',  ( 10.18755811987000115, -5.387486580809999204, 8.640943191857999750 ) ) ;
#29555 = PLANE ( 'NONE',  #52913 ) ;
#29556 = CARTESIAN_POINT ( 'NONE',  ( 7.836894192211024013, 4.974970171335808544, 6.505028920865267850 ) ) ;
#29557 = VERTEX_POINT ( 'NONE', #949 ) ;
#29558 = ORIENTED_EDGE ( 'NONE', *, *, #46755, .F. ) ;
#29559 = CARTESIAN_POINT ( 'NONE',  ( 9.784179719593000257, 4.042991257420999851, -5.768106221333000327 ) ) ;
#29560 = LINE ( 'NONE', #67957, #8844 ) ;
#29561 = CARTESIAN_POINT ( 'NONE',  ( 12.19234151475259864, -2.623341432797029693, 13.64652576243516968 ) ) ;
#29562 = CARTESIAN_POINT ( 'NONE',  ( 23.61719497714241101, 3.300271013483454308, -13.56984003092980196 ) ) ;
#29563 = CARTESIAN_POINT ( 'NONE',  ( 23.95204244535300120, 9.461060432932999475, -9.410689202680000420 ) ) ;
#29564 = EDGE_CURVE ( 'NONE', #64040, #25016, #49181, .T. ) ;
#29565 = CARTESIAN_POINT ( 'NONE',  ( 17.77447410014400120, -3.189754565392000085, -11.45074580414000032 ) ) ;
#29567 = CARTESIAN_POINT ( 'NONE',  ( 11.01665874711000015, -5.432796194138000523, 4.991871746747999161 ) ) ;
#29566 = CARTESIAN_POINT ( 'NONE',  ( 10.73959632033899858, -5.057167065956000407, 7.931430460958599049 ) ) ;
#29568 = CARTESIAN_POINT ( 'NONE',  ( 8.226385565605996320, -4.797071061338999520, -6.615828105123995329 ) ) ;
#29569 = ORIENTED_EDGE ( 'NONE', *, *, #2828, .F. ) ;
#29570 = EDGE_CURVE ( 'NONE', #68067, #49685, #57976, .T. ) ;
#29571 = CARTESIAN_POINT ( 'NONE',  ( 12.15888864290852389, -0.3818843736424570312, 13.99543728850611046 ) ) ;
#29572 = CARTESIAN_POINT ( 'NONE',  ( 10.92160119059999879, -2.751730582352999832, -4.977179449700000369 ) ) ;
#29573 = CARTESIAN_POINT ( 'NONE',  ( 17.93599305328152482, 0.4959072410923922036, 12.68697406334525368 ) ) ;
#29574 = CARTESIAN_POINT ( 'NONE',  ( 12.42340696056926852, -0.4949990737637007254, 12.68701406539598331 ) ) ;
#29575 = CARTESIAN_POINT ( 'NONE',  ( 18.17603698667415202, -2.571536872247066174, -12.43461505417294077 ) ) ;
#29576 = ORIENTED_EDGE ( 'NONE', *, *, #39245, .F. ) ;
#29578 = LINE ( 'NONE', #61026, #49668 ) ;
#29577 = FACE_OUTER_BOUND ( 'NONE', #47296, .T. ) ;
#29579 = CARTESIAN_POINT ( 'NONE',  ( 9.292835841232999883, 5.200883864107000321, -6.027780766890000308 ) ) ;
#29580 = CARTESIAN_POINT ( 'NONE',  ( 10.44426222744799837, 3.013556901740999994, 6.687444528363699625 ) ) ;
#29581 = B_SPLINE_SURFACE_WITH_KNOTS ( 'NONE', 1, 3, ( 
 ( #10481, #21317, #41960, #68859, #53482, #32169, #31474, #31819, #48582, #42646, #63266, #36722, #16067, #4888, #337, #48231, #52445, #21654, #26229, #5575, #68511, #37400, #32504, #26916, #53138, #16751, #58042, #25879, #42316, #47558, #42987, #64296, #16410, #37741, #59068, #15735, #20981, #38079, #5916, #27408, #27258, #686, #21998, #47900, #43341, #5238, #26578, #63957, #31143, #20634, #64645, #58721, #9792, #4539, #47209, #10143, #52796, #6614, #39127, #17811, #18152, #28292, #65338, #59405, #38429, #12213, #18498, #50310, #11504, #2409, #32849, #55207, #17097, #64982, #34236, #44035, #59753, #22348, #54161, #17457, #49263, #60453, #49959, #54513, #6961, #38782, #60795, #49612, #22691, #27952, #11855, #6261, #12908, #12558, #33194, #1373, #60109, #33890, #33543, #27599, #65688, #1719, #48929, #54859 ),
 ( #1035, #7307, #55555, #28649, #23038, #66374, #43686, #44388, #2073, #23391, #44731, #66028, #39473, #7654, #29001, #23732, #45070, #46780, #62499, #30034, #41194, #62163, #51671, #8686, #40840, #19172, #13941, #56241, #61143, #50653, #52008, #45752, #8347, #14622, #40496, #3767, #39823, #29693, #19520, #67399, #67739, #51336, #67062, #13261, #18843, #61823, #68084, #30698, #34585, #4111, #55901, #35611, #19862, #25447, #14284, #61484, #8005, #24428, #56924, #66723, #35941, #29341, #2753, #3430, #30363, #13603, #9023, #46437, #57254, #50994, #9355, #25105, #35267, #3092, #24766, #24077, #46091, #45414, #40169, #34924, #56584, #256, #58636, #37317, #10740, #36633, #5154, #58989, #15986, #20200, #20893, #47469, #14959, #32086, #52706, #15308, #27176, #42909, #10397, #21571, #42564, #53402, #58292, #21233 ) ),
 .UNSPECIFIED., .F., .F., .F.,
 ( 2, 2 ),
 ( 4, 2, 2, 2, 2, 2, 2, 2, 2, 2, 2, 2, 2, 2, 2, 2, 2, 2, 2, 2, 2, 2, 2, 2, 2, 2, 2, 2, 2, 2, 2, 2, 2, 2, 2, 2, 2, 2, 2, 2, 2, 2, 2, 2, 2, 2, 2, 2, 2, 2, 2, 4 ),
 ( 0.000000000000000000, 1.000000000000000000 ),
 ( 0.000000000000000000, 7.157624699936004573E-05, 0.0001431524939987200915, 0.0002147287409980801372, 0.0002326228027479201486, 0.0002505168644977601600, 0.0002863049879974401829, 0.0003220931114971202058, 0.0003578812349968002286, 0.0003936693584964802515, 0.0004294574819961602744, 0.0004652456054958402972, 0.0005010337289955203201, 0.0005368218524952003429, 0.0005726099759948803658, 0.0006441862229942404115, 0.0006799743464939204344, 0.0007157624699936004573, 0.0007336565317434404687, 0.0007515505934932804801, 0.0007873387169929605030, 0.0008589149639923205487, 0.0008947030874920005716, 0.0009304912109916805944, 0.0009662793344913606173, 0.001002067457991040640, 0.001073643704990400686, 0.001145219951989760732, 0.001216796198989120777, 0.001288372445988480823, 0.001359948692987840869, 0.001395736816487520892, 0.001431524939987200915, 0.001467313063486880937, 0.001503101186986560960, 0.001574677433985921006, 0.001646253680985281052, 0.001682041804484961075, 0.001717829927984641097, 0.001735723989734481217, 0.001753618051484321120, 0.001789406174984001143, 0.001860982421983361189, 0.001896770545483041212, 0.001932558668982721235, 0.001968346792482401041, 0.001986240854232241160, 0.002004134915982081280, 0.002075711162981441326, 0.002147287409980801372, 0.002218863656980161417, 0.002290439903979521463 ),
 .UNSPECIFIED. ) ;
#29582 = CARTESIAN_POINT ( 'NONE',  ( 1.700000000000000178, 0.000000000000000000, 0.000000000000000000 ) ) ;
#29583 = AXIS2_PLACEMENT_3D ( 'NONE', #3667, #30947, #56482 ) ;
#29584 = CARTESIAN_POINT ( 'NONE',  ( 3.358203843436000202, -3.564015676669000321, 0.4490691151644999879 ) ) ;
#29585 = ORIENTED_EDGE ( 'NONE', *, *, #32281, .F. ) ;
#29586 = CARTESIAN_POINT ( 'NONE',  ( 12.48372201234962731, 0.6448943924266595795, -12.58348668657565739 ) ) ;
#29587 = CARTESIAN_POINT ( 'NONE',  ( 24.44496488041000148, -12.03536727282999941, 3.224852091355999928 ) ) ;
#29588 = CARTESIAN_POINT ( 'NONE',  ( 23.67309896701788219, -13.19585400017914267, -3.926555274927371553 ) ) ;
#29589 = CARTESIAN_POINT ( 'NONE',  ( 24.46225079000999969, 3.515716880278999756, -12.28737560831000053 ) ) ;
#29590 = DIRECTION ( 'NONE',  ( 0.000000000000000000, 0.000000000000000000, -1.000000000000000000 ) ) ;
#29591 = ORIENTED_EDGE ( 'NONE', *, *, #32912, .T. ) ;
#29592 = CARTESIAN_POINT ( 'NONE',  ( 6.047692947599000668, 1.111956540095999868, -0.3830577677631999967 ) ) ;
#29593 = CARTESIAN_POINT ( 'NONE',  ( 10.86501009699162701, 2.649983380500041008, -7.500000587580665901 ) ) ;
#29594 = B_SPLINE_CURVE_WITH_KNOTS ( 'NONE', 3,
 ( #16387, #11830, #1008, #37717, #59045, #12188, #27927, #64619, #6587, #27577 ),
 .UNSPECIFIED., .F., .F.,
 ( 4, 2, 2, 2, 4 ),
 ( 0.000000000000000000, 0.2500000000000000000, 0.5000000000000000000, 0.7500000000000000000, 1.000000000000000000 ),
 .UNSPECIFIED. ) ;
#29595 = CARTESIAN_POINT ( 'NONE',  ( 7.882273351303999753, 4.670607894679000616, 6.328281252841999382 ) ) ;
#29596 = CARTESIAN_POINT ( 'NONE',  ( 17.55505043854143565, 3.125000000000000000, -25.00000000000000000 ) ) ;
#29597 = CARTESIAN_POINT ( 'NONE',  ( 10.47769598648999967, 5.009476315410999803, -8.101059042556599366 ) ) ;
#29598 = VERTEX_POINT ( 'NONE', #50909 ) ;
#29599 = CARTESIAN_POINT ( 'NONE',  ( 9.500008250440000523, -2.279684233303000074, 7.877691491255999878 ) ) ;
#29600 = ORIENTED_EDGE ( 'NONE', *, *, #28144, .F. ) ;
#29601 = CARTESIAN_POINT ( 'NONE',  ( 9.905375278050065901, -5.100000000000000533, -6.445686799065932782 ) ) ;
#29602 = CARTESIAN_POINT ( 'NONE',  ( 7.662254440376999653, -2.688354259407999880, 8.140021027181001401 ) ) ;
#29603 = VECTOR ( 'NONE', #18762, 1000.000000000000000 ) ;
#29604 = CARTESIAN_POINT ( 'NONE',  ( 18.27044831935229752, -0.1190513140356078692, -13.99949878896183719 ) ) ;
#29605 = EDGE_CURVE ( 'NONE', #48769, #16924, #17085, .T. ) ;
#29606 = ORIENTED_EDGE ( 'NONE', *, *, #2564, .T. ) ;
#29607 = CARTESIAN_POINT ( 'NONE',  ( 10.96365577692472293, 8.824255620808143519, -6.481155636164055878 ) ) ;
#29608 = CARTESIAN_POINT ( 'NONE',  ( 8.878359312501501677, -5.126777126186120803, 6.752018918873290865 ) ) ;
#29609 = DIRECTION ( 'NONE',  ( -1.000000000000000000, 0.000000000000000000, 0.000000000000000000 ) ) ;
#29610 = CARTESIAN_POINT ( 'NONE',  ( 24.30000000000000071, 2.078227429405999693, -11.31065739696999906 ) ) ;
#29611 = CARTESIAN_POINT ( 'NONE',  ( 25.46373154986600085, 8.354608910739999672, 8.148450287869000164 ) ) ;
#29612 = ORIENTED_EDGE ( 'NONE', *, *, #59258, .F. ) ;
#29613 = CARTESIAN_POINT ( 'NONE',  ( 2.084306799206667282, 1.762666431298138825, 3.058252359239908014 ) ) ;
#29614 = CARTESIAN_POINT ( 'NONE',  ( 12.29692076505851972, -2.864061239596868536, -13.58942221846003484 ) ) ;
#29615 = CARTESIAN_POINT ( 'NONE',  ( 10.53976354018315753, 4.327184855449099921, -8.717465845835397076 ) ) ;
#29616 = CARTESIAN_POINT ( 'NONE',  ( 10.99284770222452323, 5.204191398046943640, 6.666795694131347538 ) ) ;
#29617 = CARTESIAN_POINT ( 'NONE',  ( 11.41486084871699802, 2.792989229543000107, -7.825000000000000178 ) ) ;
#29618 = EDGE_LOOP ( 'NONE', ( #42313, #57527, #65404, #25971, #25683 ) ) ;
#29619 = CARTESIAN_POINT ( 'NONE',  ( 11.09999999999999964, -5.299999999999999822, 5.160242713806000303 ) ) ;
#29620 = CARTESIAN_POINT ( 'NONE',  ( 8.969356963619999235, -5.119357025014000584, -7.499999999914821025 ) ) ;
#29621 = CARTESIAN_POINT ( 'NONE',  ( 3.500000000000000000, 2.593303125396967168, 2.221279084403522841 ) ) ;
#29622 = LINE ( 'NONE', #2684, #7362 ) ;
#29623 = CARTESIAN_POINT ( 'NONE',  ( 7.903235257726999308, -5.126111038912999796, 6.730858764360999835 ) ) ;
#29624 = CARTESIAN_POINT ( 'NONE',  ( 12.18829585510503399, -0.1017048024283968843, -13.89950429703523938 ) ) ;
#29625 = CARTESIAN_POINT ( 'NONE',  ( 18.01444767332564112, -2.076107767824256989, 12.54031350746514129 ) ) ;
#29626 = EDGE_LOOP ( 'NONE', ( #46694, #11889, #20875, #51997 ) ) ;
#29627 = ADVANCED_FACE ( 'NONE', ( #38697 ), #44986, .F. ) ;
#29628 = CARTESIAN_POINT ( 'NONE',  ( 10.64391429142989765, -3.977620450637519678, -6.325326139450999641 ) ) ;
#29629 = ADVANCED_FACE ( 'NONE', ( #66639 ), #67287, .T. ) ;
#29630 = ORIENTED_EDGE ( 'NONE', *, *, #22867, .T. ) ;
#29631 = CARTESIAN_POINT ( 'NONE',  ( 10.03612394578000000, 3.011788727150999989, 8.746962581836999817 ) ) ;
#29632 = CARTESIAN_POINT ( 'NONE',  ( 18.17227403027676758, 2.399493853270739496, 13.69423063307216282 ) ) ;
#29633 = CARTESIAN_POINT ( 'NONE',  ( 10.16426084122999995, 4.808846957865000604, -8.639578604182998944 ) ) ;
#29634 = EDGE_CURVE ( 'NONE', #10305, #2626, #33805, .T. ) ;
#29635 = CARTESIAN_POINT ( 'NONE',  ( 2.496402089761999843, -3.205343848849000032, 0.2496534946583000014 ) ) ;
#29636 = CARTESIAN_POINT ( 'NONE',  ( 10.44486180556999955, -4.964082081645000422, -9.083599939499999110 ) ) ;
#29637 = CARTESIAN_POINT ( 'NONE',  ( 25.60000000000000142, 8.131727983644998048, -8.131727983644998048 ) ) ;
#29638 = AXIS2_PLACEMENT_3D ( 'NONE', #63895, #10763, #15671 ) ;
#29639 = CARTESIAN_POINT ( 'NONE',  ( 11.59999999999999964, 4.000000000000000000, 7.500000000000000000 ) ) ;
#29640 = EDGE_LOOP ( 'NONE', ( #14124, #57440, #67291, #4364, #46096 ) ) ;
#29641 = CARTESIAN_POINT ( 'NONE',  ( 11.34226088462130022, -3.997572771977982775, 8.640738455926999961 ) ) ;
#29642 = CARTESIAN_POINT ( 'NONE',  ( 10.77962664842000073, 2.397507474987000009, 7.755423212350999407 ) ) ;
#29643 = CARTESIAN_POINT ( 'NONE',  ( 10.65673534980114923, -5.179482957637668861, -8.179835726794200568 ) ) ;
#29644 = CARTESIAN_POINT ( 'NONE',  ( 7.950754440378000609, -2.095727472214000020, 8.056487497515000484 ) ) ;
#29646 = CARTESIAN_POINT ( 'NONE',  ( 10.96666666666765622, 4.766458981285071062, 8.714450223969652853 ) ) ;
#29645 = CARTESIAN_POINT ( 'NONE',  ( 11.18051582549000145, 5.340073783367000892, 8.416152717850000187 ) ) ;
#29647 = CARTESIAN_POINT ( 'NONE',  ( 10.72333863405319931, 4.619094858989799768, -8.289729326049599223 ) ) ;
#29648 = EDGE_CURVE ( 'NONE', #19263, #40828, #42125, .T. ) ;
#29649 = CARTESIAN_POINT ( 'NONE',  ( 23.66004879239100234, 0.000000000000000000, 0.000000000000000000 ) ) ;
#29650 = CIRCLE ( 'NONE', #49690, 13.17499999999999538 ) ;
#29651 = CARTESIAN_POINT ( 'NONE',  ( 10.03495058442699950, 4.398663815465100768, -6.578094656394299911 ) ) ;
#29652 = CARTESIAN_POINT ( 'NONE',  ( 11.62299956498149989, -2.792989229543000107, 7.174999999999999822 ) ) ;
#29653 = CARTESIAN_POINT ( 'NONE',  ( 24.72544608131600086, 3.605127478668999963, 12.13010612098000074 ) ) ;
#29654 = CARTESIAN_POINT ( 'NONE',  ( 0.9047787742017877610, 1.249023173894558303, -3.293673443241941445 ) ) ;
#29655 = CARTESIAN_POINT ( 'NONE',  ( 11.03092334123000029, 5.020455242919999783, -6.601201971309999195 ) ) ;
#29656 = ORIENTED_EDGE ( 'NONE', *, *, #17610, .T. ) ;
#29657 = CARTESIAN_POINT ( 'NONE',  ( 7.229683059621999419, -2.630475685621000093, 6.995953627589999613 ) ) ;
#29658 = CARTESIAN_POINT ( 'NONE',  ( 17.59651852071652556, 3.123961849275329161, 13.52107344427228952 ) ) ;
#29659 = DIRECTION ( 'NONE',  ( -0.000000000000000000, 0.8765967884314782577, 0.4812255921203881792 ) ) ;
#29660 = CARTESIAN_POINT ( 'NONE',  ( 10.16858376188599955, 3.268856270222099791, 7.034020612385399218 ) ) ;
#29661 = EDGE_LOOP ( 'NONE', ( #47488, #61259 ) ) ;
#29662 = CARTESIAN_POINT ( 'NONE',  ( 9.053329719590999858, 5.618384167307999277, 7.727742442702000503 ) ) ;
#29664 = CARTESIAN_POINT ( 'NONE',  ( 9.219734573340000239, -4.222669097051499953, 6.647493632115700102 ) ) ;
#29663 = CARTESIAN_POINT ( 'NONE',  ( 9.972410841228999345, 4.357364160690000432, -9.282962013144999247 ) ) ;
#29665 = CARTESIAN_POINT ( 'NONE',  ( 16.10009593531633243, 3.558564495895859991, 11.09347632393068928 ) ) ;
#29666 = ORIENTED_EDGE ( 'NONE', *, *, #29202, .F. ) ;
#29667 = B_SPLINE_CURVE_WITH_KNOTS ( 'NONE', 3,
 ( #49138, #22908, #64858, #1945 ),
 .UNSPECIFIED., .F., .F.,
 ( 4, 4 ),
 ( 0.000000000000000000, 0.1254224513349476711 ),
 .UNSPECIFIED. ) ;
#29668 = CARTESIAN_POINT ( 'NONE',  ( 18.39984528086700166, -1.003641614260999896E-13, -12.42515511467992440 ) ) ;
#29669 = CYLINDRICAL_SURFACE ( 'NONE', #48784, 2.725000000000000089 ) ;
#29670 = CARTESIAN_POINT ( 'NONE',  ( 10.47303166480599934, 2.862083839376000416, 7.419769534118209720 ) ) ;
#29671 = CARTESIAN_POINT ( 'NONE',  ( 9.351499161061999743, -4.821938821912000073, 8.950150764319998231 ) ) ;
#29672 = CARTESIAN_POINT ( 'NONE',  ( 9.739312519577246974, 2.650230560758055187, 7.263871480528552915 ) ) ;
#29673 = ORIENTED_EDGE ( 'NONE', *, *, #38220, .F. ) ;
#29674 = CARTESIAN_POINT ( 'NONE',  ( 11.48828127163000268, -3.524947629324000076, 11.86450458095000116 ) ) ;
#29675 = CARTESIAN_POINT ( 'NONE',  ( 10.50084194037999907, -4.616788958496999662, -6.288071994190999270 ) ) ;
#29676 = CARTESIAN_POINT ( 'NONE',  ( 7.925145711943240023, -2.342924674265735696, 8.034557503593903860 ) ) ;
#29677 = AXIS2_PLACEMENT_3D ( 'NONE', #55477, #34515, #29265 ) ;
#29678 = CARTESIAN_POINT ( 'NONE',  ( 9.724613486786999772, -2.928302463146000179, 8.718481221599999387 ) ) ;
#29679 = CARTESIAN_POINT ( 'NONE',  ( 11.59966954483535773, -3.361010663344000005, -6.514072057539499916 ) ) ;
#29680 = CARTESIAN_POINT ( 'NONE',  ( 9.172151519676999598, -3.978278301382419890, 6.495824366094999469 ) ) ;
#29681 = ORIENTED_EDGE ( 'NONE', *, *, #40592, .F. ) ;
#29682 = FACE_OUTER_BOUND ( 'NONE', #58047, .T. ) ;
#29683 = CARTESIAN_POINT ( 'NONE',  ( 0.5181103717477000270, 3.205765437135000173, -1.404659375816999844 ) ) ;
#29684 = VERTEX_POINT ( 'NONE', #50566 ) ;
#29685 = CARTESIAN_POINT ( 'NONE',  ( 24.30000000000000071, 11.49391741900999975, 4.090215442373000165 ) ) ;
#29686 = VERTEX_POINT ( 'NONE', #28209 ) ;
#29687 = EDGE_CURVE ( 'NONE', #7601, #65525, #19456, .T. ) ;
#29688 = EDGE_CURVE ( 'NONE', #48587, #57524, #49523, .T. ) ;
#29689 = CARTESIAN_POINT ( 'NONE',  ( 6.553816671982000130, -1.199981415667000118, 0.9000247785775999931 ) ) ;
#29690 = CARTESIAN_POINT ( 'NONE',  ( 8.365779719592000063, 2.949305648881000330, -8.659807625323999503 ) ) ;
#29691 = CARTESIAN_POINT ( 'NONE',  ( 10.76346886766499900, 3.365322927604099679, -6.346853961441000003 ) ) ;
#29692 = FACE_OUTER_BOUND ( 'NONE', #37796, .T. ) ;
#29693 = CARTESIAN_POINT ( 'NONE',  ( 12.27200335545529519, 2.173637791136409092, -12.52166559990193839 ) ) ;
#29694 = CARTESIAN_POINT ( 'NONE',  ( 10.85410941423799791, -3.257202320419700037, 8.174686939644999484 ) ) ;
#29695 = CARTESIAN_POINT ( 'NONE',  ( 8.785198341231000185, 5.414918126383000185, 8.890678916765999418 ) ) ;
#29696 = VERTEX_POINT ( 'NONE', #2668 ) ;
#29697 = CARTESIAN_POINT ( 'NONE',  ( 5.087956561560668334, -1.500000000000001110, 0.3217608788839214085 ) ) ;
#29698 = AXIS2_PLACEMENT_3D ( 'NONE', #23276, #39703, #44956 ) ;
#29699 = CARTESIAN_POINT ( 'NONE',  ( 8.085168146793000332, -2.431397064767999439, 7.958394431095000776 ) ) ;
#29700 = CARTESIAN_POINT ( 'NONE',  ( 14.80000000000000071, -3.470217030164000072, 11.92928724693999953 ) ) ;
#29701 = ORIENTED_EDGE ( 'NONE', *, *, #25874, .F. ) ;
#29702 = CARTESIAN_POINT ( 'NONE',  ( 12.11481770488412657, -2.701029500518122184, -12.30709430042447750 ) ) ;
#29704 = CARTESIAN_POINT ( 'NONE',  ( 10.52641638348499953, 3.025038519517300184, 7.737488872214999702 ) ) ;
#29703 = VECTOR ( 'NONE', #29792, 1000.000000000000000 ) ;
#29705 = CARTESIAN_POINT ( 'NONE',  ( 10.50898185320999900, -4.485028460808000439, -9.114431591966999591 ) ) ;
#29706 = CARTESIAN_POINT ( 'NONE',  ( 6.409193173016666911, 0.3926218265389159745, 1.460959015002474493 ) ) ;
#29707 = CARTESIAN_POINT ( 'NONE',  ( 17.88701341325399952, -3.642483061606999861, -12.02409215997000125 ) ) ;
#29708 = CARTESIAN_POINT ( 'NONE',  ( 7.325000000000000178, -4.000000000000000000, 9.239711431703000244 ) ) ;
#29709 = CARTESIAN_POINT ( 'NONE',  ( 12.30785086506347525, -2.879247442421006387, -13.58563033715519452 ) ) ;
#29710 = CARTESIAN_POINT ( 'NONE',  ( 17.55505043854147118, -3.199698446519375850, -12.18695736643652694 ) ) ;
#29711 = CARTESIAN_POINT ( 'NONE',  ( 11.21979841651039855, -4.304975143798100312, -8.310733465454200442 ) ) ;
#29712 = CARTESIAN_POINT ( 'NONE',  ( 10.64118447801629941, -2.722297859592000435, -7.471828720557429193 ) ) ;
#29713 = DIRECTION ( 'NONE',  ( -0.7071068219128313626, 0.000000000000000000, 0.7071067404602613404 ) ) ;
#29714 = ORIENTED_EDGE ( 'NONE', *, *, #20932, .F. ) ;
#29715 = ORIENTED_EDGE ( 'NONE', *, *, #45197, .T. ) ;
#29716 = CARTESIAN_POINT ( 'NONE',  ( 8.435453087375249126, -3.606524746037642615, 6.005799303653357235 ) ) ;
#29717 = CARTESIAN_POINT ( 'NONE',  ( 18.17920330502308701, 2.539026862123676231, 13.66507545609737662 ) ) ;
#29718 = EDGE_CURVE ( 'NONE', #19870, #68412, #23668, .T. ) ;
#29719 = CARTESIAN_POINT ( 'NONE',  ( 24.51195298297300340, -3.518215509121000117, 12.24293180497000044 ) ) ;
#29720 = LINE ( 'NONE', #51023, #812 ) ;
#29721 = CARTESIAN_POINT ( 'NONE',  ( 17.99268395210757632, 2.053674450599853873, 12.54441556206896990 ) ) ;
#29722 = DIRECTION ( 'NONE',  ( 0.000000000000000000, 0.000000000000000000, 1.000000000000000000 ) ) ;
#29723 = CARTESIAN_POINT ( 'NONE',  ( 10.15902941591999920, 4.166415211384999040, 9.114163806478000396 ) ) ;
#29724 = CARTESIAN_POINT ( 'NONE',  ( 9.498937807218625906, -4.055078665241000024, 8.373211663664079651 ) ) ;
#29725 = VERTEX_POINT ( 'NONE', #61400 ) ;
#29726 = CARTESIAN_POINT ( 'NONE',  ( 12.18088753964551429, -2.461875156572522094, 12.46041398465085948 ) ) ;
#29727 = CARTESIAN_POINT ( 'NONE',  ( 9.503038493598998215, -3.273092657276900130, -6.806856425099999441 ) ) ;
#29728 = CARTESIAN_POINT ( 'NONE',  ( 9.611387933856001098, 3.334846092635999959, 5.869117602953000556 ) ) ;
#29729 = CARTESIAN_POINT ( 'NONE',  ( 12.05300581613033906, -2.892415530317000272, 6.788791567531699656 ) ) ;
#29730 = CARTESIAN_POINT ( 'NONE',  ( 11.45348876160960039, 3.114179898019400206, -8.421216112044099589 ) ) ;
#29731 = EDGE_CURVE ( 'NONE', #35162, #48584, #32834, .T. ) ;
#29732 = CARTESIAN_POINT ( 'NONE',  ( 12.44955242156041919, 0.5141503178158078891, 12.68598964581896738 ) ) ;
#29733 = AXIS2_PLACEMENT_3D ( 'NONE', #57296, #25833, #31094 ) ;
#29734 = CARTESIAN_POINT ( 'NONE',  ( 8.187142219590999304, 4.968147183437999992, 5.971792472497999604 ) ) ;
#29735 = CARTESIAN_POINT ( 'NONE',  ( 9.124700695083998170, 4.778663323155000420, 8.799742559280000265 ) ) ;
#29736 = B_SPLINE_CURVE_WITH_KNOTS ( 'NONE', 3,
 ( #8126, #9746, #18276, #2875 ),
 .UNSPECIFIED., .F., .F.,
 ( 4, 4 ),
 ( 0.000000000000000000, 1.000000000000000000 ),
 .UNSPECIFIED. ) ;
#29737 = CARTESIAN_POINT ( 'NONE',  ( 12.70145053304001515, 1.883559157534606232, 12.57401126189226304 ) ) ;
#29738 = EDGE_LOOP ( 'NONE', ( #13208, #11353, #42712 ) ) ;
#29739 = CARTESIAN_POINT ( 'NONE',  ( 9.146614158775999925, 2.981992329588000423, -5.895876591910999664 ) ) ;
#29740 = CARTESIAN_POINT ( 'NONE',  ( 11.37964291764649971, 2.731641218595000087, -7.343212302062899433 ) ) ;
#29741 = CARTESIAN_POINT ( 'NONE',  ( 11.09999058424224394, 2.671414376110711864, 6.690776694877815345 ) ) ;
#29743 = CARTESIAN_POINT ( 'NONE',  ( 11.04384236319999957, -7.396937235950000300, -6.274987567768999241 ) ) ;
#29742 = CARTESIAN_POINT ( 'NONE',  ( 8.047379440378000126, -4.468370631666999770, 8.882152684713000568 ) ) ;
#29744 = CARTESIAN_POINT ( 'NONE',  ( 10.00801337669299862, -4.895413217368500547, 7.955057656228099461 ) ) ;
#29745 = CARTESIAN_POINT ( 'NONE',  ( 11.68333460557258796, -3.837988184179999873, -8.490304555719900392 ) ) ;
#29746 = ORIENTED_EDGE ( 'NONE', *, *, #64503, .F. ) ;
#29747 = AXIS2_PLACEMENT_3D ( 'NONE', #23114, #33271, #44113 ) ;
#29748 = CARTESIAN_POINT ( 'NONE',  ( 2.015929700617999920, 1.841731729107999982, 3.084132442762999915 ) ) ;
#29749 = CARTESIAN_POINT ( 'NONE',  ( 18.14037995566704708, -0.2193687868931910034, -12.69745523514908925 ) ) ;
#29750 = CARTESIAN_POINT ( 'NONE',  ( 9.357090631127384484, -3.380484464318182170, 8.304725771527003531 ) ) ;
#29751 = CARTESIAN_POINT ( 'NONE',  ( 21.60000012424459825, -2.247091401841000284E-13, 4.272138198758000206E-13 ) ) ;
#29752 = CARTESIAN_POINT ( 'NONE',  ( 11.09999999999999964, 2.399999999999999911, 6.571291218949999902 ) ) ;
#29753 = CARTESIAN_POINT ( 'NONE',  ( 12.42020189403039154, -3.137187437229797649, 13.64398187047951794 ) ) ;
#29754 = LINE ( 'NONE', #56985, #14109 ) ;
#29755 = CARTESIAN_POINT ( 'NONE',  ( 9.251496707488000126, -3.918323994020610268, 6.643597378104299622 ) ) ;
#29756 = CARTESIAN_POINT ( 'NONE',  ( 7.950754440378000609, -2.095727472214000020, 8.056487497515000484 ) ) ;
#29757 = ORIENTED_EDGE ( 'NONE', *, *, #46900, .F. ) ;
#29758 = CARTESIAN_POINT ( 'NONE',  ( 9.266948341230998309, 3.049618631524000367, 6.392542946894000266 ) ) ;
#29759 = CARTESIAN_POINT ( 'NONE',  ( 13.48832048419380314, -11.62805077016393618, -2.291814632468948343 ) ) ;
#29760 = DIRECTION ( 'NONE',  ( -1.000000000000000000, 0.000000000000000000, 0.000000000000000000 ) ) ;
#29761 = CARTESIAN_POINT ( 'NONE',  ( 10.68360729283869581, -2.821290678668196161, 8.178873955024902997 ) ) ;
#29762 = CARTESIAN_POINT ( 'NONE',  ( 0.8849726612439999807, -2.055220836715000221, 2.740599349591000156 ) ) ;
#29763 = EDGE_LOOP ( 'NONE', ( #31228, #45458, #17461, #45897, #14258, #8515 ) ) ;
#29764 = DIRECTION ( 'NONE',  ( 1.000000000000000000, 0.000000000000000000, 0.000000000000000000 ) ) ;
#29765 = CARTESIAN_POINT ( 'NONE',  ( 11.44903032197930060, -3.496160833528699996, 8.204588308639600314 ) ) ;
#29766 = CARTESIAN_POINT ( 'NONE',  ( 23.60000000000000142, 0.000000000000000000, 0.000000000000000000 ) ) ;
#29767 = CARTESIAN_POINT ( 'NONE',  ( 9.924742128742000347, 5.060458431729999873, 8.686130311522999747 ) ) ;
#29768 = CARTESIAN_POINT ( 'NONE',  ( 11.14179841651039915, 3.646693590264900031, 6.560784671286499226 ) ) ;
#29769 = EDGE_CURVE ( 'NONE', #4993, #10018, #13176, .T. ) ;
#29770 = EDGE_CURVE ( 'NONE', #57373, #53930, #45008, .T. ) ;
#29771 = CARTESIAN_POINT ( 'NONE',  ( 9.674960421382822418, -2.650268802167429438, 7.499999178247414910 ) ) ;
#29772 = CARTESIAN_POINT ( 'NONE',  ( 9.378950334184001036, -2.649999999999999911, -7.263338156157796988 ) ) ;
#29773 = CARTESIAN_POINT ( 'NONE',  ( 17.83221471278436354, 0.5605600754933557361, -13.88478672247768664 ) ) ;
#29774 = EDGE_CURVE ( 'NONE', #46445, #23086, #57832, .T. ) ;
#29775 = ADVANCED_FACE ( 'NONE', ( #65254 ), #7018, .T. ) ;
#29776 = CARTESIAN_POINT ( 'NONE',  ( 18.14797787938944751, 3.506662021213152514, -12.02412632936462522 ) ) ;
#29777 = CARTESIAN_POINT ( 'NONE',  ( 12.47149800526937646, -3.028907606606671354, 12.31248708664185543 ) ) ;
#29778 = CARTESIAN_POINT ( 'NONE',  ( 7.597202546497848985, 4.478004213731558991, 5.818027706311307945 ) ) ;
#29779 = EDGE_LOOP ( 'NONE', ( #38249, #48399, #17523, #10224, #16194, #2797, #25242, #47678, #54927, #8493, #38533, #32271 ) ) ;
#29780 = AXIS2_PLACEMENT_3D ( 'NONE', #40759, #8945, #25025 ) ;
#29781 = CARTESIAN_POINT ( 'NONE',  ( 17.88735652878719051, -1.970265470216408410, 13.77164815731349989 ) ) ;
#29782 = CARTESIAN_POINT ( 'NONE',  ( 10.26537527815838580, -5.100000000000000533, 6.445686799303629755 ) ) ;
#29783 = EDGE_LOOP ( 'NONE', ( #4222, #58811, #57346, #10319 ) ) ;
#29784 = ORIENTED_EDGE ( 'NONE', *, *, #68328, .F. ) ;
#29785 = CARTESIAN_POINT ( 'NONE',  ( 10.90000000000000036, -0.2500000000000000000, -4.902439024389999567 ) ) ;
#29786 = CARTESIAN_POINT ( 'NONE',  ( 4.149992563292000725, 2.000000000000000000, 0.000000000000000000 ) ) ;
#29787 = DIRECTION ( 'NONE',  ( 1.000000000000000000, 0.000000000000000000, 0.000000000000000000 ) ) ;
#29788 = VECTOR ( 'NONE', #28208, 1000.000000000000000 ) ;
#29789 = CARTESIAN_POINT ( 'NONE',  ( 9.166073843917999397, 4.023333628930999772, 9.122276991855001071 ) ) ;
#29790 = CARTESIAN_POINT ( 'NONE',  ( 10.97074841058999972, 2.648521302318000092, -6.788870928221999890 ) ) ;
#29791 = DIRECTION ( 'NONE',  ( 0.000000000000000000, 0.000000000000000000, 1.000000000000000000 ) ) ;
#29792 = DIRECTION ( 'NONE',  ( -1.000000000000000000, 2.350993083155999923E-10, 3.098106116599000021E-09 ) ) ;
#29793 = CARTESIAN_POINT ( 'NONE',  ( 18.05935420056438900, 0.5168989769797246447, -12.58939571008426839 ) ) ;
#29794 = CARTESIAN_POINT ( 'NONE',  ( 11.50001544675000176, -12.52500000000000036, 0.000000000000000000 ) ) ;
#29795 = CARTESIAN_POINT ( 'NONE',  ( 11.36749010443639918, -3.136214309321499805, -7.564597762509089662 ) ) ;
#29796 = CARTESIAN_POINT ( 'NONE',  ( 7.919010841228001141, 5.361039412362000434, 6.973453640356000349 ) ) ;
#29797 = EDGE_LOOP ( 'NONE', ( #59775, #29072, #2701, #55202 ) ) ;
#29798 = AXIS2_PLACEMENT_3D ( 'NONE', #12804, #23628, #51232 ) ;
#29799 = FACE_OUTER_BOUND ( 'NONE', #32413, .T. ) ;
#29800 = DIRECTION ( 'NONE',  ( 0.000000000000000000, 0.3258275053806940491, -0.9454292341245820186 ) ) ;
#29801 = CARTESIAN_POINT ( 'NONE',  ( 5.000030787343000327, 2.099962892530999881, 0.000000000000000000 ) ) ;
#29802 = CARTESIAN_POINT ( 'NONE',  ( 9.051138961223999857, 5.059894361919000438, -8.216246114996598848 ) ) ;
#29803 = CARTESIAN_POINT ( 'NONE',  ( 12.36142641661517239, 3.095968474608999710, 13.65339594101960863 ) ) ;
#29805 = CARTESIAN_POINT ( 'NONE',  ( 10.83659005484000026, -5.133183563847000030, 8.848364935581999546 ) ) ;
#29804 = B_SPLINE_CURVE_WITH_KNOTS ( 'NONE', 3,
 ( #21773, #32626, #31593, #16535 ),
 .UNSPECIFIED., .F., .F.,
 ( 4, 4 ),
 ( 0.000000000000000000, 1.000000000000000000 ),
 .UNSPECIFIED. ) ;
#29806 = ORIENTED_EDGE ( 'NONE', *, *, #29774, .F. ) ;
#29807 = CARTESIAN_POINT ( 'NONE',  ( 12.58522439486011812, 0.5851582065079803385, -12.68184838022456340 ) ) ;
#29808 = CARTESIAN_POINT ( 'NONE',  ( 12.49249577546344447, -0.5416168188285658269, 13.88579828294358798 ) ) ;
#29809 = ORIENTED_EDGE ( 'NONE', *, *, #19973, .T. ) ;
#29810 = CARTESIAN_POINT ( 'NONE',  ( 8.710288521113000115, 3.647046440108700160, 6.715449042252499723 ) ) ;
#29811 = CYLINDRICAL_SURFACE ( 'NONE', #10257, 0.6999999999999992895 ) ;
#29812 = CARTESIAN_POINT ( 'NONE',  ( 24.22012277176100170, -3.188429784449000159, -12.21471352112000019 ) ) ;
#29813 = CARTESIAN_POINT ( 'NONE',  ( 4.313898069763999921, 1.472923203709999962, -0.6975189077233999724 ) ) ;
#29814 = ADVANCED_FACE ( 'NONE', ( #61057 ), #68431, .F. ) ;
#29815 = CARTESIAN_POINT ( 'NONE',  ( 8.928197172114431979, -5.125396288428769154, 6.749639981086935414 ) ) ;
#29816 = CARTESIAN_POINT ( 'NONE',  ( 17.60000001298399397, -11.65261404859787930, 3.227423182320804163 ) ) ;
#29817 = CARTESIAN_POINT ( 'NONE',  ( 7.935182732229910663, 5.348502701843190543, 7.676951299079826541 ) ) ;
#29818 = EDGE_CURVE ( 'NONE', #10337, #1602, #30964, .T. ) ;
#29819 = DIRECTION ( 'NONE',  ( 1.000000000000000000, 0.000000000000000000, 0.000000000000000000 ) ) ;
#29820 = CARTESIAN_POINT ( 'NONE',  ( 25.59994555223599733, 10.55174472786000095, -3.754934689065000164 ) ) ;
#29821 = CARTESIAN_POINT ( 'NONE',  ( 11.02287616594229824, 3.738072157442200005, -6.674353346984900348 ) ) ;
#29822 = CARTESIAN_POINT ( 'NONE',  ( 1.250973465874999802, -3.500000000000000000, 0.000000000000000000 ) ) ;
#29823 = CARTESIAN_POINT ( 'NONE',  ( 11.06205165877000063, 2.154392227069000132, -7.605898171884000192 ) ) ;
#29824 = CARTESIAN_POINT ( 'NONE',  ( 9.430013376692999216, 2.982096917914000223, -6.982691809975100306 ) ) ;
#29826 = CARTESIAN_POINT ( 'NONE',  ( 9.276575450301999481, -4.067929031554969654, 6.560591699025100532 ) ) ;
#29825 = LINE ( 'NONE', #29483, #39763 ) ;
#29827 = DIRECTION ( 'NONE',  ( 0.000000000000000000, 0.8648648261949251070, 0.5020048131351152465 ) ) ;
#29828 = ORIENTED_EDGE ( 'NONE', *, *, #24224, .T. ) ;
#29829 = AXIS2_PLACEMENT_3D ( 'NONE', #44877, #12011, #12710 ) ;
#29830 = CARTESIAN_POINT ( 'NONE',  ( 11.40211496860029783, 4.793947479907100018, 7.906860999147899527 ) ) ;
#29831 = CIRCLE ( 'NONE', #16371, 12.35000000006999876 ) ;
#29832 = CARTESIAN_POINT ( 'NONE',  ( 10.09697182628999990, -5.253379538902000156, 8.530665717066000298 ) ) ;
#29833 = CARTESIAN_POINT ( 'NONE',  ( 10.26291290906799958, 3.364470222553300083, 6.722218404915299317 ) ) ;
#29834 = CARTESIAN_POINT ( 'NONE',  ( 10.91620964606000044, -2.818413279081999789, -6.814156272943999504 ) ) ;
#29835 = LINE ( 'NONE', #13738, #47783 ) ;
#29836 = CIRCLE ( 'NONE', #54356, 12.39999890530000037 ) ;
#29837 = CARTESIAN_POINT ( 'NONE',  ( 7.156776345353000224, 1.243223188895000053, 2.274921040069000118E-10 ) ) ;
#29838 = DIRECTION ( 'NONE',  ( 1.000000000000000000, 0.000000000000000000, 0.000000000000000000 ) ) ;
#29839 = VERTEX_POINT ( 'NONE', #40412 ) ;
#29840 = B_SPLINE_CURVE_WITH_KNOTS ( 'NONE', 3,
 ( #43110, #68987, #31594, #63391 ),
 .UNSPECIFIED., .F., .F.,
 ( 4, 4 ),
 ( 0.000000000000000000, 1.000000000000000000 ),
 .UNSPECIFIED. ) ;
#29841 = CARTESIAN_POINT ( 'NONE',  ( 9.683304848515998486, -2.961576783819000358, -7.974775391194199869 ) ) ;
#29842 = CIRCLE ( 'NONE', #25373, 11.35000000000000497 ) ;
#29843 = CARTESIAN_POINT ( 'NONE',  ( 13.00000000000000178, -49.86679564220000316, -7.696464862566000598 ) ) ;
#29844 = CARTESIAN_POINT ( 'NONE',  ( 17.84655355976681790, 1.821424963963778954, -12.46765546240475686 ) ) ;
#29845 = CARTESIAN_POINT ( 'NONE',  ( 9.041568618727998441, -2.868050178059002420, -6.343697345132999210 ) ) ;
#29846 = CARTESIAN_POINT ( 'NONE',  ( 23.66004879239100234, -13.39256464007999980, -3.813546745462999876 ) ) ;
#29847 = CARTESIAN_POINT ( 'NONE',  ( 7.939460911587998382, 2.865023798136999922, 6.766038833998996971 ) ) ;
#29848 = CARTESIAN_POINT ( 'NONE',  ( 9.661323620223001285, -4.289037785427000316, -5.816478295321999781 ) ) ;
#29849 = CARTESIAN_POINT ( 'NONE',  ( 0.8009734658753000502, -3.500000000000000000, 0.000000000000000000 ) ) ;
#29850 = ORIENTED_EDGE ( 'NONE', *, *, #34124, .F. ) ;
#29851 = CARTESIAN_POINT ( 'NONE',  ( 17.79083366723151727, 1.825854556024153474, -13.88043960113665953 ) ) ;
#29852 = ADVANCED_FACE ( 'NONE', ( #24339 ), #46354, .T. ) ;
#29853 = DIRECTION ( 'NONE',  ( 0.000000000000000000, 0.7614089499631913061, 0.6482718649732923666 ) ) ;
#29854 = ADVANCED_FACE ( 'NONE', ( #52277 ), #3349, .T. ) ;
#29855 = CARTESIAN_POINT ( 'NONE',  ( 13.64514873068900158, -9.050862583665999495, -7.420564490681000436 ) ) ;
#29856 = CARTESIAN_POINT ( 'NONE',  ( 17.72017830064981325, -1.875000000000000666, -13.78627079974488900 ) ) ;
#29857 = DIRECTION ( 'NONE',  ( 0.7071068187612229439, 0.000000000000000000, -0.7071067436118699812 ) ) ;
#29858 = CARTESIAN_POINT ( 'NONE',  ( 9.310554719594000161, 3.934138271021000222, -9.063586117809000697 ) ) ;
#29859 = CARTESIAN_POINT ( 'NONE',  ( 11.94133594839949986, -3.430493414882899827, 8.152656755002400502 ) ) ;
#29860 = ORIENTED_EDGE ( 'NONE', *, *, #47586, .F. ) ;
#29861 = CARTESIAN_POINT ( 'NONE',  ( 4.000000000000000000, -1.082950885222932147, 1.878608423871279687 ) ) ;
#29862 = CARTESIAN_POINT ( 'NONE',  ( 17.99865897956989613, 3.095937021190220850, -13.65340307249647900 ) ) ;
#29863 = ORIENTED_EDGE ( 'NONE', *, *, #34667, .T. ) ;
#29864 = CARTESIAN_POINT ( 'NONE',  ( 9.959367640781000119, -3.591293244209800228, 8.264635032075899446 ) ) ;
#29865 = CARTESIAN_POINT ( 'NONE',  ( 24.76115083069733203, 3.101111505761503295, 11.75477011280721840 ) ) ;
#29866 = CARTESIAN_POINT ( 'NONE',  ( 9.600045280412000892, 3.021734963141999852, -6.070209284876999511 ) ) ;
#29867 = CARTESIAN_POINT ( 'NONE',  ( 18.20279897579441197, 3.027817980922571817, -11.45825916412429457 ) ) ;
#29868 = CARTESIAN_POINT ( 'NONE',  ( 11.43345123989529810, -3.459769760840400110, -8.543317325199000223 ) ) ;
#29869 = DIRECTION ( 'NONE',  ( -1.000000000000000000, -0.000000000000000000, -0.000000000000000000 ) ) ;
#29870 = CARTESIAN_POINT ( 'NONE',  ( -15.86200481174999943, 5.599999999999999645, 6.571291218949999902 ) ) ;
#29871 = ORIENTED_EDGE ( 'NONE', *, *, #25704, .F. ) ;
#29872 = CARTESIAN_POINT ( 'NONE',  ( 25.30000327618300204, 2.078227429405999693, -11.31065739696999906 ) ) ;
#29873 = CARTESIAN_POINT ( 'NONE',  ( 8.736413463905998711, 4.084156314540369870, -8.382409559052598880 ) ) ;
#29874 = CARTESIAN_POINT ( 'NONE',  ( 9.128895280414001334, 3.880154689736000417, -9.060377011187000562 ) ) ;
#29875 = EDGE_LOOP ( 'NONE', ( #45621, #4101, #13909 ) ) ;
#29876 = EDGE_CURVE ( 'NONE', #33943, #37994, #24888, .T. ) ;
#29877 = VECTOR ( 'NONE', #60959, 1000.000000000000000 ) ;
#29878 = CARTESIAN_POINT ( 'NONE',  ( 10.87696123885999810, 5.827079664135999870, -7.814747088295999511 ) ) ;
#29879 = SURFACE_STYLE_FILL_AREA ( #8531 ) ;
#29880 = ORIENTED_EDGE ( 'NONE', *, *, #11348, .T. ) ;
#29881 = CARTESIAN_POINT ( 'NONE',  ( 9.581988259785999773, 3.850604015305000072, 6.368003848175999515 ) ) ;
#29882 = CARTESIAN_POINT ( 'NONE',  ( 17.84319482158669246, -1.945290144093657192, -12.56363827966045044 ) ) ;
#29883 = COLOUR_RGB ( '', 0.31764706, 0.68627451, 0.89019608) ;
#29884 = DIRECTION ( 'NONE',  ( 0.000000000000000000, -0.1807154286440003366, -0.9835354258236024272 ) ) ;
#29885 = AXIS2_PLACEMENT_3D ( 'NONE', #18106, #66326, #13214 ) ;
#29886 = CARTESIAN_POINT ( 'NONE',  ( 24.46275371508600216, -12.39843049379000028, -3.098824767661999768 ) ) ;
#29887 = DIRECTION ( 'NONE',  ( 0.000000000000000000, -1.000000000000000000, 0.000000000000000000 ) ) ;
#29888 = ORIENTED_EDGE ( 'NONE', *, *, #64295, .T. ) ;
#29889 = CARTESIAN_POINT ( 'NONE',  ( 11.59999999999999964, 3.528833218773708591, 6.561154158729442187 ) ) ;
#29890 = CARTESIAN_POINT ( 'NONE',  ( 8.687922088694000067, 3.419384128876999718, -5.860036257779999147 ) ) ;
#29891 = DIRECTION ( 'NONE',  ( -0.4682208595142289265, -0.4682208595142289265, 0.7493586947727458591 ) ) ;
#29892 = CONICAL_SURFACE ( 'NONE', #49986, 0.8999999994071996579, 0.7853981633972997312 ) ;
#29893 = CARTESIAN_POINT ( 'NONE',  ( 12.22896558337868989, 2.961354171198296914, -13.68321881638708604 ) ) ;
#29894 = CARTESIAN_POINT ( 'NONE',  ( 9.935646554150999066, -3.447209681134600245, -8.499078230848398974 ) ) ;
#29895 = CARTESIAN_POINT ( 'NONE',  ( 18.27397574302396066, -0.09509187666555490859, 13.99968209810982600 ) ) ;
#29896 = CARTESIAN_POINT ( 'NONE',  ( 7.837706995175509839, 4.985640386982826300, 6.515278850541923461 ) ) ;
#29897 = VERTEX_POINT ( 'NONE', #62420 ) ;
#29898 = ORIENTED_EDGE ( 'NONE', *, *, #26917, .T. ) ;
#29899 = AXIS2_PLACEMENT_3D ( 'NONE', #55138, #7585, #25725 ) ;
#29900 = CARTESIAN_POINT ( 'NONE',  ( 8.441604719589999917, 5.473983809665999622, -8.180077404516000072 ) ) ;
#29901 = EDGE_CURVE ( 'NONE', #27904, #43460, #67000, .T. ) ;
#29902 = CARTESIAN_POINT ( 'NONE',  ( 9.299999999999998934, 4.537600397704999899, 9.154563893594000135 ) ) ;
#29903 = CARTESIAN_POINT ( 'NONE',  ( 12.72228957555996942, -1.875000000000000666, 13.78631905550009407 ) ) ;
#29904 = CARTESIAN_POINT ( 'NONE',  ( 25.41675762280700113, 8.397332536106999257, -8.092742924401999716 ) ) ;
#29905 = CARTESIAN_POINT ( 'NONE',  ( 25.00271319629458944, -3.413733088963054385, -11.76143375765198407 ) ) ;
#29906 = CARTESIAN_POINT ( 'NONE',  ( 18.24051303026600124, -3.055556278716000218, -11.39470302754000031 ) ) ;
#29908 = CARTESIAN_POINT ( 'NONE',  ( 8.752020595170648676, 5.414340795661968464, 8.580369625954880064 ) ) ;
#29907 = CARTESIAN_POINT ( 'NONE',  ( 10.68893802597400011, -4.593629475532499562, 8.475365825607600101 ) ) ;
#29909 = CARTESIAN_POINT ( 'NONE',  ( 0.6679169396051075624, 2.967698684047975544, -1.300341253696400301 ) ) ;
#29910 = ORIENTED_EDGE ( 'NONE', *, *, #62271, .F. ) ;
#29911 = CARTESIAN_POINT ( 'NONE',  ( 8.486008579191000933, -3.399999999999999911, 5.976611076844000614 ) ) ;
#29912 = CARTESIAN_POINT ( 'NONE',  ( 10.60232725808000076, -2.940669124847000049, -4.956116633172999997 ) ) ;
#29913 = CARTESIAN_POINT ( 'NONE',  ( 9.487725409950000355, -4.905858243509999106, -8.948175900338000588 ) ) ;
#29914 = DIRECTION ( 'NONE',  ( 0.000000000000000000, 1.000000000000000000, 0.000000000000000000 ) ) ;
#29915 = CARTESIAN_POINT ( 'NONE',  ( 5.055026506350000837, -1.500000000000000000, 0.000000000000000000 ) ) ;
#29916 = DIRECTION ( 'NONE',  ( 0.000000000000000000, 1.000000000000000000, 0.000000000000000000 ) ) ;
#29917 = CYLINDRICAL_SURFACE ( 'NONE', #28737, 1.000000000000000222 ) ;
#29918 = CARTESIAN_POINT ( 'NONE',  ( 10.41964694612699915, 2.813019656517000477, 7.026297514493899499 ) ) ;
#29919 = AXIS2_PLACEMENT_3D ( 'NONE', #49342, #22771, #28379 ) ;
#29920 = DIRECTION ( 'NONE',  ( -1.000000000000000000, 0.000000000000000000, 0.000000000000000000 ) ) ;
#29921 = VECTOR ( 'NONE', #3496, 1000.000000000000000 ) ;
#29922 = CARTESIAN_POINT ( 'NONE',  ( 0.3738300074506999970, -3.373808768376999723, -1.182108054635000026E-09 ) ) ;
#29923 = CARTESIAN_POINT ( 'NONE',  ( 3.496476353695999961, -3.048162822197999944, -1.563142635087000132 ) ) ;
#29924 = EDGE_LOOP ( 'NONE', ( #6841, #24705 ) ) ;
#29925 = CARTESIAN_POINT ( 'NONE',  ( 12.58477481432937672, -0.5849872192492366896, -12.68185863724643170 ) ) ;
#29926 = B_SPLINE_CURVE_WITH_KNOTS ( 'NONE', 3,
 ( #38025, #27546, #32794, #22634, #54109, #21263 ),
 .UNSPECIFIED., .F., .F.,
 ( 4, 2, 4 ),
 ( 0.000000000000000000, 0.5000000000000000000, 1.000000000000000000 ),
 .UNSPECIFIED. ) ;
#29927 = CARTESIAN_POINT ( 'NONE',  ( 7.773264358664000007, -2.859518314699000197, 6.768377407145999669 ) ) ;
#29928 = DIRECTION ( 'NONE',  ( -1.000000000000000000, 0.000000000000000000, 0.000000000000000000 ) ) ;
#29930 = CARTESIAN_POINT ( 'NONE',  ( 24.36453968238300050, 3.372832729159999765, -12.24475767785000002 ) ) ;
#29929 = VECTOR ( 'NONE', #1591, 1000.000000000000000 ) ;
#29931 = CARTESIAN_POINT ( 'NONE',  ( 18.20279897513207246, -3.027817981728709640, -11.45825916391119037 ) ) ;
#29932 = VERTEX_POINT ( 'NONE', #4024 ) ;
#29933 = CARTESIAN_POINT ( 'NONE',  ( 6.753493422235999688, -0.7428381837956999911, 0.9117187782023999931 ) ) ;
#29934 = EDGE_CURVE ( 'NONE', #57425, #7219, #63946, .T. ) ;
#29935 = CARTESIAN_POINT ( 'NONE',  ( 0.000000000000000000, 0.000000000000000000, 0.000000000000000000 ) ) ;
#29936 = EDGE_CURVE ( 'NONE', #10927, #11525, #46215, .T. ) ;
#29937 = CARTESIAN_POINT ( 'NONE',  ( 10.97857890969851979, 8.376940913775774433, 6.556924013712003507 ) ) ;
#29938 = CARTESIAN_POINT ( 'NONE',  ( 9.580795537697266440, -5.100000000000000533, -6.662590550601107608 ) ) ;
#29939 = CARTESIAN_POINT ( 'NONE',  ( 1.615556799206875116, 0.4581489286485002088, 3.500000000000001776 ) ) ;
#29940 = CIRCLE ( 'NONE', #24329, 1.000000000000000888 ) ;
#29941 = CARTESIAN_POINT ( 'NONE',  ( 10.89324174884020024, 3.967693531726030010, -8.674442868902998427 ) ) ;
#29942 = ORIENTED_EDGE ( 'NONE', *, *, #35140, .T. ) ;
#29943 = CARTESIAN_POINT ( 'NONE',  ( 11.24052627608000066, -2.774025043188999895, 6.782107572692000375 ) ) ;
#29944 = EDGE_LOOP ( 'NONE', ( #19177, #21835, #5428, #9559, #49557, #53899, #50056, #42939, #5235, #30552, #34229 ) ) ;
#29945 = CARTESIAN_POINT ( 'NONE',  ( 8.476294715524065992, -3.031386904610626765, 6.154469090921128149 ) ) ;
#29946 = CARTESIAN_POINT ( 'NONE',  ( 7.635855646791999796, -2.466384407480000096, 6.935560677555000275 ) ) ;
#29947 = CARTESIAN_POINT ( 'NONE',  ( 17.81092223849609724, 0.6836428945794175149, -13.98330131869062321 ) ) ;
#29948 = ORIENTED_EDGE ( 'NONE', *, *, #17923, .F. ) ;
#29949 = CARTESIAN_POINT ( 'NONE',  ( 10.97209615884046485, 8.593900732908855034, -6.535061034646649780 ) ) ;
#29950 = CARTESIAN_POINT ( 'NONE',  ( 11.02214804248387203, -5.404890988668177521, -8.010352125886161190 ) ) ;
#29951 = LINE ( 'NONE', #29258, #19226 ) ;
#29952 = DIRECTION ( 'NONE',  ( -1.000000000000000000, 0.000000000000000000, 0.000000000000000000 ) ) ;
#29953 = CARTESIAN_POINT ( 'NONE',  ( 17.77858768906186882, -3.083996659902246140, 12.29614209097516841 ) ) ;
#29954 = ORIENTED_EDGE ( 'NONE', *, *, #61529, .F. ) ;
#29955 = CARTESIAN_POINT ( 'NONE',  ( 8.716851002545999094, -2.832432432432000269, 6.822293592207000934 ) ) ;
#29956 = CARTESIAN_POINT ( 'NONE',  ( 11.60000000000000142, 4.363617849674655602, 8.530211724564095377 ) ) ;
#29957 = CARTESIAN_POINT ( 'NONE',  ( 1.849999551004999798, 0.000000000000000000, 0.000000000000000000 ) ) ;
#29958 = EDGE_CURVE ( 'NONE', #6824, #53059, #4372, .T. ) ;
#29959 = CARTESIAN_POINT ( 'NONE',  ( 9.664763540182335078, 5.217465845835396188, 7.827184855449094592 ) ) ;
#29960 = CARTESIAN_POINT ( 'NONE',  ( 5.699999999554000496, -0.3000000004460000036, 9.662944681662999358 ) ) ;
#29961 = EDGE_LOOP ( 'NONE', ( #34204, #23640, #45784, #27520, #53168, #18337, #48480, #57310 ) ) ;
#29962 = PRODUCT ( 'Terminal Screw', 'Terminal Screw', '', ( #4009 ) ) ;
#29963 = CARTESIAN_POINT ( 'NONE',  ( 17.59562484679850058, 0.6250000000000004441, -13.88107975066922783 ) ) ;
#29964 = EDGE_CURVE ( 'NONE', #69017, #62685, #6942, .T. ) ;
#29965 = CARTESIAN_POINT ( 'NONE',  ( 10.94975213449457208, -2.829972217754548325, -6.705091429376293100 ) ) ;
#29966 = CARTESIAN_POINT ( 'NONE',  ( 24.05220244970136179, -3.343001867506199432, -12.65093409602237529 ) ) ;
#29967 = DIRECTION ( 'NONE',  ( -1.000000000000000000, 0.000000000000000000, 0.000000000000000000 ) ) ;
#29968 = CARTESIAN_POINT ( 'NONE',  ( 12.76382393867146092, -0.6239806250735595583, -13.88114166035887997 ) ) ;
#29969 = CARTESIAN_POINT ( 'NONE',  ( 18.17584245753829464, -2.573100139072833414, 12.43426722069302315 ) ) ;
#29970 = ORIENTED_EDGE ( 'NONE', *, *, #25485, .F. ) ;
#29971 = CARTESIAN_POINT ( 'NONE',  ( 11.23078751119019891, -4.915752892793999962, -7.979095341142500075 ) ) ;
#29972 = ORIENTED_EDGE ( 'NONE', *, *, #40833, .F. ) ;
#29973 = CARTESIAN_POINT ( 'NONE',  ( 9.442087588264000075, 4.742492734433000123, 8.809983635807000724 ) ) ;
#29974 = B_SPLINE_CURVE_WITH_KNOTS ( 'NONE', 3,
 ( #58749, #30816, #10855, #47927, #26, #16101, #58072, #37091, #26949, #32201, #52129, #52825, #26258, #4231 ),
 .UNSPECIFIED., .F., .F.,
 ( 4, 2, 1, 1, 2, 2, 2, 4 ),
 ( 0.8006037889120940498, 0.8504528416840665406, 0.8629151048770596910, 0.8691462364735562662, 0.8722618022718046094, 0.8753773680700528415, 0.9003018944560425840, 1.000000000000000000 ),
 .UNSPECIFIED. ) ;
#29975 = DIRECTION ( 'NONE',  ( -1.000000000000000000, 0.000000000000000000, -3.164702532202999971E-14 ) ) ;
#29976 = CARTESIAN_POINT ( 'NONE',  ( 9.865910841232000905, 2.685250982074999904, -7.026194612421999608 ) ) ;
#29977 = CARTESIAN_POINT ( 'NONE',  ( 3.054835882697000127, 0.1750656501049999980, 3.539389852118999702 ) ) ;
#29978 = CARTESIAN_POINT ( 'NONE',  ( 10.16989351219999982, -2.594225604561000154, -6.291264536816999708 ) ) ;
#29979 = CARTESIAN_POINT ( 'NONE',  ( 3.500000000000000000, -2.946081722130999836, 0.9972449351501998516 ) ) ;
#29980 = CARTESIAN_POINT ( 'NONE',  ( 9.039567739507649691, -4.932484926559381755, 8.476014846726219076 ) ) ;
#29981 = ORIENTED_EDGE ( 'NONE', *, *, #19396, .T. ) ;
#29982 = STYLED_ITEM ( 'NONE', ( #32974 ), #52451 ) ;
#29983 = CARTESIAN_POINT ( 'NONE',  ( 11.21918447801630059, -2.859536135895000442, 7.525145395936648995 ) ) ;
#29984 = CARTESIAN_POINT ( 'NONE',  ( 9.013423559847998590, 4.933953210258000155, 8.417881984655998906 ) ) ;
#29985 = B_SPLINE_CURVE_WITH_KNOTS ( 'NONE', 3,
 ( #43540, #543, #20834, #21856, #11031, #10339, #42169, #33047, #54015, #63468 ),
 .UNSPECIFIED., .F., .F.,
 ( 4, 2, 2, 2, 4 ),
 ( 0.000000000000000000, 0.2500000000000000000, 0.5000000000000000000, 0.7500000000000000000, 1.000000000000000000 ),
 .UNSPECIFIED. ) ;
#29986 = CARTESIAN_POINT ( 'NONE',  ( 15.95500032369699994, 8.890098389148999303, 8.614471248541999415 ) ) ;
#29987 = DIRECTION ( 'NONE',  ( 0.000000000000000000, 0.000000000000000000, 1.000000000000000000 ) ) ;
#29989 = CARTESIAN_POINT ( 'NONE',  ( 12.75598008710589326, 3.248071441111126667, -13.61800396221869214 ) ) ;
#29988 = CARTESIAN_POINT ( 'NONE',  ( 10.99433665574000152, 3.697618584609999814, 5.729302299903000772 ) ) ;
#29990 = TOROIDAL_SURFACE ( 'NONE', #33317, 12.20000000000000107, 0.6999999999999999556 ) ;
#29991 = CARTESIAN_POINT ( 'NONE',  ( 11.08841369783139896, 3.942447888101379583, -8.639288317626999003 ) ) ;
#29992 = CARTESIAN_POINT ( 'NONE',  ( 3.999999836924999386, 2.524999836911000273, 2.479012191990000139E-10 ) ) ;
#29993 = CARTESIAN_POINT ( 'NONE',  ( 9.249747021775998945, 3.245052836381700168, -8.162493079567200382 ) ) ;
#29994 = CARTESIAN_POINT ( 'NONE',  ( 18.14418133822493928, -0.4193891200559137222, 12.59302195412780456 ) ) ;
#29995 = FACE_OUTER_BOUND ( 'NONE', #10363, .T. ) ;
#29996 = LINE ( 'NONE', #18458, #18789 ) ;
#29997 = CARTESIAN_POINT ( 'NONE',  ( 24.63329909277253194, -2.078227420229220357, -11.31065739865757536 ) ) ;
#29998 = ORIENTED_EDGE ( 'NONE', *, *, #5387, .T. ) ;
#29999 = CARTESIAN_POINT ( 'NONE',  ( 7.422245559621999611, -5.361050935357000391, 6.973449182446000094 ) ) ;
#30000 = CARTESIAN_POINT ( 'NONE',  ( 18.13331639930710537, 2.076941473624324797, 13.84509535655099199 ) ) ;
#30001 = CARTESIAN_POINT ( 'NONE',  ( 6.965816936038000229, -1.147328252452000097, 0.8605332073374000190 ) ) ;
#30002 = LINE ( 'NONE', #67030, #3510 ) ;
#30003 = VERTEX_POINT ( 'NONE', #63093 ) ;
#30004 = CARTESIAN_POINT ( 'NONE',  ( 7.807364158771999740, 3.650414032626000171, 6.083147621602999600 ) ) ;
#30006 = CARTESIAN_POINT ( 'NONE',  ( 10.72191429142990060, 4.025072603369280522, 8.816028813488999916 ) ) ;
#30005 = CARTESIAN_POINT ( 'NONE',  ( 8.750151519676999001, -3.981249765141819719, -8.366807394121199337 ) ) ;
#30007 = CARTESIAN_POINT ( 'NONE',  ( 10.47111721959000086, 5.170640285885000687, -8.712953516124999354 ) ) ;
#30008 = ORIENTED_EDGE ( 'NONE', *, *, #24455, .T. ) ;
#30009 = B_SPLINE_CURVE_WITH_KNOTS ( 'NONE', 3,
 ( #64958, #1007, #42623, #5553, #42965, #662, #64272, #16386, #48902, #37716 ),
 .UNSPECIFIED., .F., .F.,
 ( 4, 2, 2, 2, 4 ),
 ( 0.000000000000000000, 0.2499999999999997780, 0.4999999999999995559, 0.7499999999999997780, 1.000000000000000000 ),
 .UNSPECIFIED. ) ;
#30010 = CARTESIAN_POINT ( 'NONE',  ( 1.467640132540666498, 1.762666431298152148, -3.058252359239900908 ) ) ;
#30011 = LINE ( 'NONE', #61122, #68831 ) ;
#30012 = CARTESIAN_POINT ( 'NONE',  ( 10.98995257254739855, 2.904643075091000171, 7.181435527216799564 ) ) ;
#30013 = CARTESIAN_POINT ( 'NONE',  ( 24.30001129594134568, -12.15210919218037233, 3.256147844378488809 ) ) ;
#30014 = DIRECTION ( 'NONE',  ( 1.000000000000000000, 0.000000000000000000, 0.000000000000000000 ) ) ;
#30015 = ORIENTED_EDGE ( 'NONE', *, *, #7092, .T. ) ;
#30016 = CYLINDRICAL_SURFACE ( 'NONE', #17650, 2.000000000000000444 ) ;
#30017 = EDGE_CURVE ( 'NONE', #64705, #35912, #36543, .T. ) ;
#30018 = EDGE_CURVE ( 'NONE', #46752, #52724, #17857, .T. ) ;
#30019 = CARTESIAN_POINT ( 'NONE',  ( 10.17270027370999941, -4.650151116117000605, -8.655526539784000661 ) ) ;
#30020 = CARTESIAN_POINT ( 'NONE',  ( 8.127894995188555072, -5.076156598471832204, 6.133170389101868736 ) ) ;
#30021 = CARTESIAN_POINT ( 'NONE',  ( 11.30878751119029957, -5.041025164610000608, -8.044634158732998586 ) ) ;
#30022 = CARTESIAN_POINT ( 'NONE',  ( 10.60344474310099905, -2.862064370975999861, 6.947770206896899836 ) ) ;
#30023 = ORIENTED_EDGE ( 'NONE', *, *, #39500, .T. ) ;
#30024 = CARTESIAN_POINT ( 'NONE',  ( 2.865556799209791894, -0.4581489286485082579, -3.500000000000000888 ) ) ;
#30025 = CARTESIAN_POINT ( 'NONE',  ( 10.64887885159599890, -2.730985436695000157, 7.651388779553199626 ) ) ;
#30026 = ORIENTED_EDGE ( 'NONE', *, *, #10084, .T. ) ;
#30027 = CARTESIAN_POINT ( 'NONE',  ( 16.10009593531634664, -3.558564495883423273, -11.09347632393477134 ) ) ;
#30028 = VECTOR ( 'NONE', #55499, 1000.000000000000000 ) ;
#30029 = VERTEX_POINT ( 'NONE', #51587 ) ;
#30030 = CARTESIAN_POINT ( 'NONE',  ( 9.910492310842998975, -4.686746084135999801, -9.174865097765998456 ) ) ;
#30031 = CARTESIAN_POINT ( 'NONE',  ( 8.397785841227999981, 5.616457598545999907, -8.245813000738998255 ) ) ;
#30032 = CARTESIAN_POINT ( 'NONE',  ( 11.63611496860034933, 5.171412538012999605, -6.899705789500199415 ) ) ;
#30033 = FACE_OUTER_BOUND ( 'NONE', #59270, .T. ) ;
#30034 = CARTESIAN_POINT ( 'NONE',  ( 12.47240630447277709, 1.970775872724741973, -12.55927287175691198 ) ) ;
#30035 = CARTESIAN_POINT ( 'NONE',  ( 10.72687885159599830, -2.867290578374000365, 7.635128076451499268 ) ) ;
#30036 = CARTESIAN_POINT ( 'NONE',  ( 8.721010841230999233, 5.983047240001000411, 7.440798119034999658 ) ) ;
#30037 = VERTEX_POINT ( 'NONE', #3682 ) ;
#30038 = CARTESIAN_POINT ( 'NONE',  ( 9.593930206849998754, 5.250000000000000000, 7.500000000000000000 ) ) ;
#30039 = CARTESIAN_POINT ( 'NONE',  ( 8.727043146794999373, -3.882020254083999866, 5.870054788755000530 ) ) ;
#30040 = FACE_OUTER_BOUND ( 'NONE', #55022, .T. ) ;
#30041 = EDGE_LOOP ( 'NONE', ( #14058, #8679, #58620, #36655, #49617 ) ) ;
#30042 = CARTESIAN_POINT ( 'NONE',  ( 12.07989974639902542, -2.471827770301485039, -12.35516928474874554 ) ) ;
#30043 = EDGE_CURVE ( 'NONE', #54684, #37989, #54604, .T. ) ;
#30044 = CARTESIAN_POINT ( 'NONE',  ( 11.23195122972050086, 4.507250159094099651, 8.673036084990000560 ) ) ;
#30045 = CARTESIAN_POINT ( 'NONE',  ( 10.54684435321000002, -3.691674321452999674, -9.157280075569998345 ) ) ;
#30046 = CARTESIAN_POINT ( 'NONE',  ( 6.875000000000000000, 5.574137966889000317, -8.240733100917999820 ) ) ;
#30047 = CARTESIAN_POINT ( 'NONE',  ( 18.53682146000800302, -2.876943948391000205, -12.22927217127999988 ) ) ;
#30048 = CARTESIAN_POINT ( 'NONE',  ( 9.343930206849998754, 2.750000000000000000, -7.500000000000000000 ) ) ;
#30049 = CARTESIAN_POINT ( 'NONE',  ( 12.19562740135371470, -2.360953413553769309, -13.70191948036522156 ) ) ;
#30050 = SHAPE_REPRESENTATION ( 'Positive Post', ( #9676 ), #16178 ) ;
#30051 = CARTESIAN_POINT ( 'NONE',  ( 11.59999999999999964, 4.000000000000000000, 7.500000000000000000 ) ) ;
#30052 = CARTESIAN_POINT ( 'NONE',  ( 10.91195257254739914, -5.227167235646000165, -7.856899084262298771 ) ) ;
#30053 = CARTESIAN_POINT ( 'NONE',  ( 2.750973465876000557, -3.500000000000000000, 0.000000000000000000 ) ) ;
#30054 = ORIENTED_EDGE ( 'NONE', *, *, #38801, .T. ) ;
#30055 = ORIENTED_EDGE ( 'NONE', *, *, #67260, .F. ) ;
#30056 = CARTESIAN_POINT ( 'NONE',  ( 10.27194008929999924, -4.567480829194999536, 4.846795848580000232 ) ) ;
#30057 = LINE ( 'NONE', #61847, #57060 ) ;
#30058 = LINE ( 'NONE', #45436, #2629 ) ;
#30059 = CARTESIAN_POINT ( 'NONE',  ( 11.01002959534999981, 3.180718072098000171, -6.283812549199000230 ) ) ;
#30060 = DIRECTION ( 'NONE',  ( 1.000000000000000000, 0.000000000000000000, 0.000000000000000000 ) ) ;
#30061 = CARTESIAN_POINT ( 'NONE',  ( 18.03321709926671801, 2.902596714178123261, 12.34859794581418768 ) ) ;
#30062 = CARTESIAN_POINT ( 'NONE',  ( 17.87620400591499958, 3.527529948368999690, -11.96092454128000071 ) ) ;
#30063 = CARTESIAN_POINT ( 'NONE',  ( 11.11845610223999969, 5.767025078915000158, 7.178418469370999588 ) ) ;
#30064 = DIRECTION ( 'NONE',  ( -1.000000000000000000, 0.000000000000000000, 0.000000000000000000 ) ) ;
#30065 = EDGE_LOOP ( 'NONE', ( #41797, #43243, #9234, #4169, #26567 ) ) ;
#30066 = CARTESIAN_POINT ( 'NONE',  ( 12.20882029558155502, -2.312280790556522359, 12.49335225873939059 ) ) ;
#30067 = CARTESIAN_POINT ( 'NONE',  ( 9.148430433047000321, -4.854750075120300323, -6.972511033848699746 ) ) ;
#30068 = CARTESIAN_POINT ( 'NONE',  ( 9.980433037259000884, 4.047223446241999589, 9.090360698422999874 ) ) ;
#30069 = CARTESIAN_POINT ( 'NONE',  ( 11.18546886766499959, -4.566506264294200257, 8.529286361367999447 ) ) ;
#30070 = CARTESIAN_POINT ( 'NONE',  ( 8.640504719592000171, 2.305580295895999665, -7.860904109308999743 ) ) ;
#30071 = CARTESIAN_POINT ( 'NONE',  ( 10.32118582084299874, 3.163839350524900063, -6.533484739457099622 ) ) ;
#30072 = CARTESIAN_POINT ( 'NONE',  ( 12.54694134722857513, 0.5693054069933383143, 12.68281928773556366 ) ) ;
#30073 = ADVANCED_FACE ( 'NONE', ( #49704 ), #33637, .T. ) ;
#30074 = EDGE_CURVE ( 'NONE', #66643, #7462, #16965, .T. ) ;
#30075 = CARTESIAN_POINT ( 'NONE',  ( 9.021579719592999425, 2.193665972875999959, 7.400591513898000073 ) ) ;
#30076 = CARTESIAN_POINT ( 'NONE',  ( 9.600491906670001185, 5.206545077004999911, 8.585111878242999595 ) ) ;
#30077 = AXIS2_PLACEMENT_3D ( 'NONE', #67205, #22925, #67547 ) ;
#30078 = CARTESIAN_POINT ( 'NONE',  ( 12.42127013197880281, 2.006280959398175856, 12.55298695860708946 ) ) ;
#30079 = ORIENTED_EDGE ( 'NONE', *, *, #2489, .T. ) ;
#30080 = CARTESIAN_POINT ( 'NONE',  ( 10.01508584123000034, 4.845406482350000488, -6.387189183984999907 ) ) ;
#30081 = CARTESIAN_POINT ( 'NONE',  ( -2.444943969992999916E-05, 2.899969545325999931, 0.000000000000000000 ) ) ;
#30082 = CARTESIAN_POINT ( 'NONE',  ( 25.29989948031900227, 2.258942858049999725, -12.29419282279000036 ) ) ;
#30084 = CARTESIAN_POINT ( 'NONE',  ( 10.20851354018233437, 4.163624617374472869, 8.749999999999996447 ) ) ;
#30083 = CARTESIAN_POINT ( 'NONE',  ( 7.854816940377000734, -4.561648098548999997, 6.153050355516999304 ) ) ;
#30085 = CARTESIAN_POINT ( 'NONE',  ( 12.10000000000000320, -4.400439255161259666, 8.403338258880266309 ) ) ;
#30086 = CARTESIAN_POINT ( 'NONE',  ( 11.51102763632551884, -4.911148285670300595, -7.079572058049399708 ) ) ;
#30087 = ORIENTED_EDGE ( 'NONE', *, *, #10810, .F. ) ;
#30088 = CARTESIAN_POINT ( 'NONE',  ( 1.062290711803000054, -0.1589293563100999951, 3.588678346333000313 ) ) ;
#30089 = CARTESIAN_POINT ( 'NONE',  ( 5.700000000000000178, 13.04986661130000059, -1.811520473896000016 ) ) ;
#30091 = CARTESIAN_POINT ( 'NONE',  ( 9.564964385875493136, -5.350010280223940207, -7.500002129152480101 ) ) ;
#30090 = CARTESIAN_POINT ( 'NONE',  ( 9.768156128192828191, 5.148428864295390817, 8.818541960853263362 ) ) ;
#30092 = CARTESIAN_POINT ( 'NONE',  ( 17.83317199298538824, -3.060086213985775405, 13.53858764060002962 ) ) ;
#30093 = CARTESIAN_POINT ( 'NONE',  ( 13.70005190196300227, 9.005348107749998832, 7.391036106496999381 ) ) ;
#30094 = CARTESIAN_POINT ( 'NONE',  ( 16.06714147702547635, 8.497559733041605057, 7.969681199758297474 ) ) ;
#30095 = LINE ( 'NONE', #35671, #43135 ) ;
#30096 = CARTESIAN_POINT ( 'NONE',  ( 9.679055905794999859, 2.899999999999999911, 6.571291218949999902 ) ) ;
#30097 = CARTESIAN_POINT ( 'NONE',  ( 7.501441940376999185, -2.138201851198999748, 6.814774777484000623 ) ) ;
#30098 = VERTEX_POINT ( 'NONE', #24860 ) ;
#30099 = CARTESIAN_POINT ( 'NONE',  ( 9.074385841230999006, 3.981661882377999895, 8.959227447876999761 ) ) ;
#30100 = EDGE_CURVE ( 'NONE', #15615, #21235, #62779, .T. ) ;
#30101 = CARTESIAN_POINT ( 'NONE',  ( 24.57709886597293547, -8.720615828874477060, 8.720613681126877736 ) ) ;
#30102 = CARTESIAN_POINT ( 'NONE',  ( 7.325000000000000178, -4.000000000000000000, 9.239711431703000244 ) ) ;
#30103 = CARTESIAN_POINT ( 'NONE',  ( 17.55505043854144276, -0.6250000000000001110, -25.00000000000000000 ) ) ;
#30104 = CARTESIAN_POINT ( 'NONE',  ( 0.7896087623623999630, 1.804890371571000074, 2.911542930280999641 ) ) ;
#30105 = EDGE_LOOP ( 'NONE', ( #24769, #28400, #63679, #66422 ) ) ;
#30106 = CARTESIAN_POINT ( 'NONE',  ( 1.429412799688042801, -1.139198292438498017, 3.100114201899466959 ) ) ;
#30107 = ADVANCED_FACE ( 'NONE', ( #55992 ), #45506, .T. ) ;
#30108 = CARTESIAN_POINT ( 'NONE',  ( 12.13410404293056999, -4.442327784369100030, 6.599279737936000423 ) ) ;
#30109 = CARTESIAN_POINT ( 'NONE',  ( 10.64360935987385659, -5.049157587798284830, 5.054580113003310338 ) ) ;
#30110 = CARTESIAN_POINT ( 'NONE',  ( 10.03612394578000000, 3.011788727150999989, 8.746962581836999817 ) ) ;
#30111 = CARTESIAN_POINT ( 'NONE',  ( 10.94487616594229884, 3.696562859151900415, 8.456491899811199531 ) ) ;
#30112 = CARTESIAN_POINT ( 'NONE',  ( 11.18236694037999968, -4.516641106826999597, -8.757887038823000125 ) ) ;
#30113 = CARTESIAN_POINT ( 'NONE',  ( 11.79999999684100054, 12.15995044155999949, 2.000340912084999978 ) ) ;
#30114 = CARTESIAN_POINT ( 'NONE',  ( 24.30001120070703990, 12.15210914071406734, -3.256147830588134173 ) ) ;
#30115 = FACE_OUTER_BOUND ( 'NONE', #9012, .T. ) ;
#30116 = B_SPLINE_CURVE_WITH_KNOTS ( 'NONE', 3,
 ( #28356, #44447, #28706, #2130 ),
 .UNSPECIFIED., .F., .F.,
 ( 4, 4 ),
 ( 0.000000000000000000, 1.000000000000000000 ),
 .UNSPECIFIED. ) ;
#30117 = CARTESIAN_POINT ( 'NONE',  ( 7.665091595931846413, 5.584449939165478938, 6.749525577098944851 ) ) ;
#30118 = ORIENTED_EDGE ( 'NONE', *, *, #16250, .F. ) ;
#30119 = CARTESIAN_POINT ( 'NONE',  ( 17.74479774746059846, -3.223061189501819523, 13.62394687717146802 ) ) ;
#30120 = CARTESIAN_POINT ( 'NONE',  ( 5.099999999983999999, -3.441691376337999159E-14, 1.598721155459999804E-14 ) ) ;
#30121 = EDGE_LOOP ( 'NONE', ( #39466, #14794, #2400, #28815 ) ) ;
#30122 = VERTEX_POINT ( 'NONE', #18244 ) ;
#30123 = CARTESIAN_POINT ( 'NONE',  ( 18.50003594170800270, -2.686563649653999963, 11.33603604535000109 ) ) ;
#30124 = CARTESIAN_POINT ( 'NONE',  ( 9.708513540183332680, 4.163624617374472869, -6.250000000000001776 ) ) ;
#30125 = EDGE_CURVE ( 'NONE', #32067, #12035, #19616, .T. ) ;
#30126 = CARTESIAN_POINT ( 'NONE',  ( 10.85056919669530018, 4.830699382454300306, 7.254567470917099747 ) ) ;
#30127 = CARTESIAN_POINT ( 'NONE',  ( 9.691082467489000152, 5.335647408863999352, 8.701220655673999715 ) ) ;
#30128 = CARTESIAN_POINT ( 'NONE',  ( 10.84087666499999969, 2.636288985756999992, -7.512643730465999425 ) ) ;
#30129 = CARTESIAN_POINT ( 'NONE',  ( 9.404204162135625822, -3.209635909649031671, -7.124690962532754135 ) ) ;
#30130 = FACE_OUTER_BOUND ( 'NONE', #26743, .T. ) ;
#30131 = CARTESIAN_POINT ( 'NONE',  ( 18.25531039711340497, 0.1866745257715810569, -12.59862229962904401 ) ) ;
#30132 = DIRECTION ( 'NONE',  ( -1.000000000000000000, 0.000000000000000000, 0.000000000000000000 ) ) ;
#30133 = CARTESIAN_POINT ( 'NONE',  ( 11.21979841651039855, -4.304975143798100312, -8.310733465454200442 ) ) ;
#30134 = CARTESIAN_POINT ( 'NONE',  ( 10.90379229492000057, -5.099791907704999794, -5.134764377744000186 ) ) ;
#30135 = ORIENTED_EDGE ( 'NONE', *, *, #33626, .F. ) ;
#30136 = CARTESIAN_POINT ( 'NONE',  ( 9.548601287889788125, -3.999999532294070459, 6.301404677806389465 ) ) ;
#30137 = DIRECTION ( 'NONE',  ( 1.000000000000000000, 0.000000000000000000, 0.000000000000000000 ) ) ;
#30138 = CARTESIAN_POINT ( 'NONE',  ( 8.856495485442710702, 4.349453410998743941, 6.546761994161411913 ) ) ;
#30139 = CARTESIAN_POINT ( 'NONE',  ( 9.532392757686999119, 4.863450031739999346, -8.443842375698499936 ) ) ;
#30140 = CARTESIAN_POINT ( 'NONE',  ( 12.14271297744733680, 2.220151667091618819, 13.82285866607422520 ) ) ;
#30141 = DIRECTION ( 'NONE',  ( 0.000000000000000000, 1.000000000000000000, 0.000000000000000000 ) ) ;
#30142 = EDGE_LOOP ( 'NONE', ( #5926, #36577, #30962, #11112, #14288, #16998, #62008 ) ) ;
#30143 = CARTESIAN_POINT ( 'NONE',  ( 12.21931228143050774, 0.2190605494068694759, -12.69747807323824951 ) ) ;
#30144 = DIRECTION ( 'NONE',  ( 0.000000000000000000, 0.000000000000000000, -1.000000000000000000 ) ) ;
#30145 = ORIENTED_EDGE ( 'NONE', *, *, #59990, .T. ) ;
#30146 = CARTESIAN_POINT ( 'NONE',  ( 10.97499895057999986, -2.398081733189999864E-14, 0.000000000000000000 ) ) ;
#30147 = FACE_OUTER_BOUND ( 'NONE', #1038, .T. ) ;
#30148 = AXIS2_PLACEMENT_3D ( 'NONE', #53556, #26990, #59138 ) ;
#30149 = CARTESIAN_POINT ( 'NONE',  ( 5.500000000000000000, 0.000000000000000000, 0.000000000000000000 ) ) ;
#30150 = CARTESIAN_POINT ( 'NONE',  ( 4.421486958654000432, 1.000604198411000123, 1.286416736850999998 ) ) ;
#30151 = B_SPLINE_SURFACE_WITH_KNOTS ( 'NONE', 3, 3, ( 
 ( #36444, #51832, #4971, #9872, #10217, #21056, #14782, #26654, #47632, #57079, #42385, #52178, #63344, #3927, #15470, #63691, #57417, #15806, #4278, #21390, #25265, #25613, #46941, #31898, #68244, #53210, #46604, #36796, #5312, #47971, #67908, #20025, #41351, #62662, #20365 ),
 ( #41689, #62995, #57761, #4620, #25954, #54593, #43421, #53891, #11579, #11936, #32923, #38867, #60187, #6335, #53557, #65057, #49693, #6689, #54235, #16148, #27685, #17178, #28032, #16490, #38507, #64716, #48656, #7042, #1110, #59481, #760, #64366, #22423, #49340, #21727 ),
 ( #43765, #48999, #59831, #33276, #1454, #22769, #5993, #28377, #1802, #5650, #59139, #11243, #42723, #44120, #65416, #32581, #38154, #17537, #48307, #12293, #58798, #22074, #33623, #16830, #27333, #54941, #64027, #37818, #37471, #10903, #32248, #26991, #414, #43062, #67141 ),
 ( #34315, #13679, #39207, #65764, #55638, #18230, #30112, #45829, #13341, #24508, #45493, #35008, #61225, #24158, #2488, #66457, #39553, #44471, #33967, #35348, #29078, #60877, #19252, #23813, #56323, #23118, #12992, #2830, #50734, #51076, #34664, #50389, #17889, #2153, #45148 ) ),
 .UNSPECIFIED., .F., .F., .F.,
 ( 4, 4 ),
 ( 4, 1, 1, 1, 1, 1, 1, 1, 1, 1, 1, 1, 1, 1, 1, 1, 1, 1, 1, 1, 1, 1, 1, 1, 1, 1, 1, 1, 1, 1, 1, 1, 4 ),
 ( -0.1039086239011999951, 1.103908623900999864 ),
 ( 0.2233333333344000027, 0.2480800653604999795, 0.2728267973865999840, 0.2975735294126999886, 0.3223202614387999931, 0.3470669934649999733, 0.3718137254910999778, 0.3965604575171999824, 0.4213071895433000424, 0.4460539215694000470, 0.4708006535954999960, 0.4955473856216000006, 0.5202941176476999496, 0.5450408496738000652, 0.5697875816999000698, 0.5945343137260000743, 0.6192810457521999989, 0.6440277777783000035, 0.6687745098044000081, 0.6935212418305000126, 0.7182679738566000172, 0.7430147058827000217, 0.7677614379088000263, 0.7925081699349000308, 0.8172549019609999243, 0.8420016339870999289, 0.8667483660132000445, 0.8914950980394000801, 0.9162418300655000847, 0.9409885620915999782, 0.9657352941176999828, 0.9904820261437999873, 1.015228758169999912 ),
 .UNSPECIFIED. ) ;
#30152 = CARTESIAN_POINT ( 'NONE',  ( 10.23921655905610528, -2.650856495401338275, 7.263814070341720885 ) ) ;
#30153 = ADVANCED_FACE ( 'NONE', ( #50059 ), #40937, .F. ) ;
#30154 = EDGE_CURVE ( 'NONE', #47074, #50591, #64508, .T. ) ;
#30155 = CARTESIAN_POINT ( 'NONE',  ( 24.30000000000000071, 2.258942858049999725, 12.29419282279000036 ) ) ;
#30156 = CARTESIAN_POINT ( 'NONE',  ( 8.029017301488167391, 4.353549739958994635, 8.815463536202678085 ) ) ;
#30157 = CARTESIAN_POINT ( 'NONE',  ( 10.83253786428999987, -2.899999999999999911, 6.571291218949999902 ) ) ;
#30158 = CARTESIAN_POINT ( 'NONE',  ( 19.01453011999999987, 0.8000000000000000444, 3.149999999999999911 ) ) ;
#30159 = EDGE_CURVE ( 'NONE', #43855, #41213, #7819, .T. ) ;
#30160 = CARTESIAN_POINT ( 'NONE',  ( 11.36749010443639918, 4.863785690678500195, -7.564597762509089662 ) ) ;
#30161 = CARTESIAN_POINT ( 'NONE',  ( 9.709999999999999076, 4.496968146123999865, -8.755198255949000696 ) ) ;
#30162 = CARTESIAN_POINT ( 'NONE',  ( 10.60770165877000082, 2.392327800351000011, -6.587345916039000215 ) ) ;
#30163 = CARTESIAN_POINT ( 'NONE',  ( 9.075405316139999456, 3.757578743663700038, -8.615780615741000403 ) ) ;
#30165 = CARTESIAN_POINT ( 'NONE',  ( 12.18035041863818790, 2.521826826515520370, 12.44645458618487588 ) ) ;
#30164 = CARTESIAN_POINT ( 'NONE',  ( 9.342468108405999061, -3.165798890946399879, 7.263744984161399465 ) ) ;
#30166 = CARTESIAN_POINT ( 'NONE',  ( 23.59642540973940683, -13.38915559410792078, 4.012079637628372275 ) ) ;
#30167 = ORIENTED_EDGE ( 'NONE', *, *, #43344, .T. ) ;
#30168 = CARTESIAN_POINT ( 'NONE',  ( 10.57102344389999971, 3.237334151971200225, 7.962849245488699879 ) ) ;
#30169 = CARTESIAN_POINT ( 'NONE',  ( 10.71756905878999966, -3.040221764047000175, 8.808455607108001573 ) ) ;
#30170 = CARTESIAN_POINT ( 'NONE',  ( 9.882975701332998852, 4.736880367605800224, 6.817468224793199916 ) ) ;
#30171 = CARTESIAN_POINT ( 'NONE',  ( 23.61700615888999977, -2.917315259571999775, 13.53528614794999996 ) ) ;
#30172 = CARTESIAN_POINT ( 'NONE',  ( 10.93728138146000006, -5.425439422033999648, 7.240583766112999697 ) ) ;
#30173 = CARTESIAN_POINT ( 'NONE',  ( 13.50018479229797208, 10.27880801399748734, 5.973155204427849974 ) ) ;
#30174 = CARTESIAN_POINT ( 'NONE',  ( 6.916399753370999548, -12.19468927157999971, 3.104275419013000192 ) ) ;
#30175 = ORIENTED_EDGE ( 'NONE', *, *, #26275, .T. ) ;
#30176 = CARTESIAN_POINT ( 'NONE',  ( 9.607317406968999052, -3.787635830142400462, -8.621889436328999068 ) ) ;
#30177 = CARTESIAN_POINT ( 'NONE',  ( 10.67701940544685790, -5.048701884080403879, -5.056137651350367079 ) ) ;
#30178 = CARTESIAN_POINT ( 'NONE',  ( 11.19057802013490033, -5.033226574983999946, 7.524052967375959966 ) ) ;
#30179 = CARTESIAN_POINT ( 'NONE',  ( 18.27123885515668889, 2.366823750208064681, -12.37571350032474982 ) ) ;
#30180 = CARTESIAN_POINT ( 'NONE',  ( 24.30000000000000071, 9.289189189551001036, -7.908916752675001050 ) ) ;
#30181 = DIRECTION ( 'NONE',  ( 0.000000000000000000, 0.000000000000000000, -1.000000000000000000 ) ) ;
#30182 = CARTESIAN_POINT ( 'NONE',  ( 12.18135539521807509, 2.541609601666299678, -13.66455050632895585 ) ) ;
#30183 = CARTESIAN_POINT ( 'NONE',  ( 9.218723707566001124, -5.383415012847999392, -8.183490493635000362 ) ) ;
#30184 = CARTESIAN_POINT ( 'NONE',  ( 10.63706886433642573, 2.899999999999999911, 6.444141223494331605 ) ) ;
#30185 = CARTESIAN_POINT ( 'NONE',  ( 9.704564187634451500, -2.648431596117190256, 7.852956029643703317 ) ) ;
#30186 = FACE_OUTER_BOUND ( 'NONE', #61105, .T. ) ;
#30187 = DIRECTION ( 'NONE',  ( -1.000000000000000000, 0.000000000000000000, 0.000000000000000000 ) ) ;
#30188 = CARTESIAN_POINT ( 'NONE',  ( 8.270987825454401587, -2.867662898289943918, 6.761597767506805745 ) ) ;
#30189 = CARTESIAN_POINT ( 'NONE',  ( 18.17241432538235202, 2.400344151293695827, 12.47423995685674392 ) ) ;
#30190 = AXIS2_PLACEMENT_3D ( 'NONE', #26584, #4208, #62592 ) ;
#30191 = CARTESIAN_POINT ( 'NONE',  ( 8.474089158773999486, 4.131080973160000447, -6.108642999115999395 ) ) ;
#30192 = CARTESIAN_POINT ( 'NONE',  ( 6.756521017669194329, 1.248225365452464652, -0.8739435346021212636 ) ) ;
#30193 = ORIENTED_EDGE ( 'NONE', *, *, #32606, .F. ) ;
#30194 = CARTESIAN_POINT ( 'NONE',  ( 4.000000000000000000, 1.082895748633089683, 1.878475312369199957 ) ) ;
#30195 = CARTESIAN_POINT ( 'NONE',  ( 18.22053876895016344, 2.807780685761759987, -13.71555663160087235 ) ) ;
#30196 = ORIENTED_EDGE ( 'NONE', *, *, #1173, .T. ) ;
#30197 = CARTESIAN_POINT ( 'NONE',  ( 10.44062143724499947, -3.424116261072899903, 8.148124882831599081 ) ) ;
#30198 = LINE ( 'NONE', #45243, #22333 ) ;
#30199 = EDGE_CURVE ( 'NONE', #62414, #79, #51676, .T. ) ;
#30200 = CARTESIAN_POINT ( 'NONE',  ( 9.152520280414000453, 4.102804347295999854, -5.770625657082999460 ) ) ;
#30201 = CARTESIAN_POINT ( 'NONE',  ( 9.715116888608552159, 4.417514547833707894, -8.786659901436729925 ) ) ;
#30202 = CARTESIAN_POINT ( 'NONE',  ( 10.64391429142989765, -3.977620450637519678, -6.325326139450999641 ) ) ;
#30203 = CARTESIAN_POINT ( 'NONE',  ( 21.35000154058000277, -1.509903258602878808E-14, 12.59999999999999964 ) ) ;
#30204 = EDGE_CURVE ( 'NONE', #53074, #51860, #21531, .T. ) ;
#30205 = CARTESIAN_POINT ( 'NONE',  ( 5.034193173016665135, -1.460959015002474493, 0.3926218265389144757 ) ) ;
#30206 = EDGE_LOOP ( 'NONE', ( #1520, #49867, #42502 ) ) ;
#30207 = CARTESIAN_POINT ( 'NONE',  ( 7.906851002540999929, 2.832432432432000269, -6.822293592207000934 ) ) ;
#30208 = CARTESIAN_POINT ( 'NONE',  ( 8.731616107288068918, 4.000002263255227675, -8.381579007094499545 ) ) ;
#30209 = CARTESIAN_POINT ( 'NONE',  ( 8.491329719591000469, 4.851303550474000303, -9.008742670124000540 ) ) ;
#30210 = ORIENTED_EDGE ( 'NONE', *, *, #9823, .T. ) ;
#30211 = CARTESIAN_POINT ( 'NONE',  ( 9.870875237110999123, 2.904361819252000210, -8.563871667095998674 ) ) ;
#30212 = ORIENTED_EDGE ( 'NONE', *, *, #28545, .T. ) ;
#30213 = CARTESIAN_POINT ( 'NONE',  ( 9.328696787962998727, 4.196076320588900010, 8.624850445389000697 ) ) ;
#30214 = CARTESIAN_POINT ( 'NONE',  ( 17.91340230256481547, -1.987833194700776795, -12.55624649895498024 ) ) ;
#30215 = B_SPLINE_CURVE_WITH_KNOTS ( 'NONE', 3,
 ( #37521, #31599, #42430, #42089, #48356, #36151 ),
 .UNSPECIFIED., .F., .F.,
 ( 4, 2, 4 ),
 ( 0.000000000000000000, 0.3470882326038999266, 0.6941764652077998532 ),
 .UNSPECIFIED. ) ;
#30216 = CARTESIAN_POINT ( 'NONE',  ( 9.342770489224111685, 2.713249534563407561, -7.026737643655856402 ) ) ;
#30217 = CARTESIAN_POINT ( 'NONE',  ( 24.36504260745899941, -12.29008018610999819, -3.201257196435000285 ) ) ;
#30218 = CARTESIAN_POINT ( 'NONE',  ( 25.50719570236825362, 2.874190748112039895, 11.25480690672102746 ) ) ;
#30219 = ORIENTED_EDGE ( 'NONE', *, *, #53147, .T. ) ;
#30220 = CARTESIAN_POINT ( 'NONE',  ( 11.47657389914466464, 3.351225026288215947, 6.404407512144050685 ) ) ;
#30221 = DIRECTION ( 'NONE',  ( 0.000000000000000000, -1.000000000000000000, 0.000000000000000000 ) ) ;
#30222 = B_SPLINE_CURVE_WITH_KNOTS ( 'NONE', 3,
 ( #18812, #61452, #56894, #45722 ),
 .UNSPECIFIED., .F., .F.,
 ( 4, 4 ),
 ( 0.000000000000000000, 1.000000000000000000 ),
 .UNSPECIFIED. ) ;
#30223 = CYLINDRICAL_SURFACE ( 'NONE', #48460, 11.50000000000000000 ) ;
#30224 = CARTESIAN_POINT ( 'NONE',  ( 12.30746066369761138, 3.049480053538142776, -13.66385627579028572 ) ) ;
#30225 = AXIS2_PLACEMENT_3D ( 'NONE', #7256, #22987, #38379 ) ;
#30226 = LINE ( 'NONE', #13800, #29487 ) ;
#30227 = CARTESIAN_POINT ( 'NONE',  ( 9.679055905794999859, -2.899999999999999911, 6.571291218949999902 ) ) ;
#30228 = CARTESIAN_POINT ( 'NONE',  ( 10.68375832677999959, -4.547311397465000127, -8.749131152219000285 ) ) ;
#30229 = EDGE_CURVE ( 'NONE', #58875, #62483, #34457, .T. ) ;
#30230 = VERTEX_POINT ( 'NONE', #57693 ) ;
#30231 = ORIENTED_EDGE ( 'NONE', *, *, #22783, .F. ) ;
#30232 = CARTESIAN_POINT ( 'NONE',  ( 8.532195280408998883, 5.331510020787000315, -8.114341808290998159 ) ) ;
#30233 = CARTESIAN_POINT ( 'NONE',  ( 4.149992563292000725, -2.000000000000000000, 0.000000000000000000 ) ) ;
#30234 = EDGE_CURVE ( 'NONE', #29932, #37966, #53623, .T. ) ;
#30235 = EDGE_CURVE ( 'NONE', #45043, #42217, #13762, .T. ) ;
#30236 = CARTESIAN_POINT ( 'NONE',  ( 12.23181585140601868, -2.749296767780423867, 13.61742212735507351 ) ) ;
#30237 = CARTESIAN_POINT ( 'NONE',  ( 24.87549197752000296, 8.587510512484001879, -8.379258482743999537 ) ) ;
#30238 = CARTESIAN_POINT ( 'NONE',  ( 23.66565514010100202, 10.00711324362000099, -9.518238975075000496 ) ) ;
#30240 = CIRCLE ( 'NONE', #31332, 1.900000000000001021 ) ;
#30239 = CARTESIAN_POINT ( 'NONE',  ( 17.88018231457700224, -3.314507696643999690, -11.22393832560999982 ) ) ;
#30242 = DIRECTION ( 'NONE',  ( -1.000000000000000000, 0.000000000000000000, 0.000000000000000000 ) ) ;
#30241 = CARTESIAN_POINT ( 'NONE',  ( 9.625113844317999323, -3.711648483798899889, 8.604802177355001191 ) ) ;
#30243 = CARTESIAN_POINT ( 'NONE',  ( 8.285673191594010945, -4.510969308813000289, -6.771077081157996780 ) ) ;
#30244 = ORIENTED_EDGE ( 'NONE', *, *, #31402, .F. ) ;
#30245 = B_SPLINE_CURVE_WITH_KNOTS ( 'NONE', 3,
 ( #30161, #19999, #51803, #30833 ),
 .UNSPECIFIED., .F., .F.,
 ( 4, 4 ),
 ( 0.000000000000000000, 1.000000000000000000 ),
 .UNSPECIFIED. ) ;
#30246 = CARTESIAN_POINT ( 'NONE',  ( 27.64127793187000037, -2.399999999999999911, -6.571291218949999902 ) ) ;
#30247 = CARTESIAN_POINT ( 'NONE',  ( 0.7000000000000000666, -0.5773502691895999739, 1.000000000000000000 ) ) ;
#30248 = CARTESIAN_POINT ( 'NONE',  ( 9.265134009212999899, -5.494586520014999920, -6.370782351137999733 ) ) ;
#30249 = LINE ( 'NONE', #41069, #11277 ) ;
#30250 = CARTESIAN_POINT ( 'NONE',  ( 4.933367189779430895, 2.033301450227492424, -8.777144014527002974E-10 ) ) ;
#30251 = CARTESIAN_POINT ( 'NONE',  ( 8.601296034414005476, 5.350254842529069244, -7.263180132971093883 ) ) ;
#30252 = CARTESIAN_POINT ( 'NONE',  ( 8.696135841231001251, 3.038023536984999939, -5.861661709981000001 ) ) ;
#30253 = EDGE_CURVE ( 'NONE', #41719, #29839, #6065, .T. ) ;
#30254 = CARTESIAN_POINT ( 'NONE',  ( 7.674540706797001732, -4.591334964886001124, 6.448517731106997886 ) ) ;
#30255 = CARTESIAN_POINT ( 'NONE',  ( 11.14975833414749928, 3.203462856645999945, 7.174999999999999822 ) ) ;
#30256 = CARTESIAN_POINT ( 'NONE',  ( 24.84571067577687842, -3.513925179492865425, 11.93623758569678728 ) ) ;
#30257 = CARTESIAN_POINT ( 'NONE',  ( 2.299654279612000085, 3.259062154207000184, 0.01210126588865999969 ) ) ;
#30258 = ORIENTED_EDGE ( 'NONE', *, *, #23439, .F. ) ;
#30259 = CARTESIAN_POINT ( 'NONE',  ( 12.53820945512841156, 0.6689034848678672152, -12.58223305319197749 ) ) ;
#30260 = CARTESIAN_POINT ( 'NONE',  ( 12.18782402015739130, -2.399945986167177914, -12.47432385256424858 ) ) ;
#30261 = CARTESIAN_POINT ( 'NONE',  ( 8.765417767663000959, 5.029951493281999753, -6.097931603992000404 ) ) ;
#30262 = CARTESIAN_POINT ( 'NONE',  ( 7.358051658771000092, 4.561643343497000735, 6.153061759127000485 ) ) ;
#30263 = LINE ( 'NONE', #7901, #58462 ) ;
#30264 = ORIENTED_EDGE ( 'NONE', *, *, #5537, .T. ) ;
#30265 = CARTESIAN_POINT ( 'NONE',  ( 11.04384236319999957, 5.374509385214000012, -5.035088906224999938 ) ) ;
#30266 = SHAPE_DEFINITION_REPRESENTATION ( #34392, #46027 ) ;
#30267 = CARTESIAN_POINT ( 'NONE',  ( 10.96277061797134955, 8.847246680402779617, 6.474667694356146974 ) ) ;
#30268 = CARTESIAN_POINT ( 'NONE',  ( 13.55481756226799916, -11.54935041389000006, -2.400813070608000199 ) ) ;
#30269 = CARTESIAN_POINT ( 'NONE',  ( 1.750973465873000068, -3.500000000000000000, 0.000000000000000000 ) ) ;
#30270 = CARTESIAN_POINT ( 'NONE',  ( 10.76857802013509868, 2.825431102905000103, -7.472656658230009796 ) ) ;
#30271 = ORIENTED_EDGE ( 'NONE', *, *, #20371, .T. ) ;
#30272 = MANIFOLD_SOLID_BREP ( 'Stock-MAS-678-1', #19146 ) ;
#30273 = CARTESIAN_POINT ( 'NONE',  ( 11.07345355053000091, -3.998673159585000025, 8.920828114954002075 ) ) ;
#30274 = ORIENTED_EDGE ( 'NONE', *, *, #2485, .T. ) ;
#30275 = CIRCLE ( 'NONE', #9049, 12.50000000000000000 ) ;
#30276 = CARTESIAN_POINT ( 'NONE',  ( 12.07299956498157023, -2.792989229543000107, 7.174999999999999822 ) ) ;
#30278 = CARTESIAN_POINT ( 'NONE',  ( 9.074379440379999551, -3.981661727120999750, 8.959239802162999311 ) ) ;
#30277 = ADVANCED_BREP_SHAPE_REPRESENTATION ( '', ( #7037, #9676 ), #49917 ) ;
#30279 = CARTESIAN_POINT ( 'NONE',  ( 18.17115727977514439, 0.3856318793703991665, -13.99470184309726051 ) ) ;
#30280 = ORIENTED_EDGE ( 'NONE', *, *, #55318, .T. ) ;
#30281 = CARTESIAN_POINT ( 'NONE',  ( 23.56673047179102909, 10.35362056585002755, 9.408487697651425563 ) ) ;
#30282 = DIRECTION ( 'NONE',  ( 1.000000000000000000, 0.000000000000000000, 0.000000000000000000 ) ) ;
#30283 = AXIS2_PLACEMENT_3D ( 'NONE', #37276, #57214, #9316 ) ;
#30284 = CARTESIAN_POINT ( 'NONE',  ( 7.531929719588999816, 3.511256298105000173, -6.013302684100999329 ) ) ;
#30285 = ADVANCED_FACE ( 'NONE', ( #46533 ), #10491, .T. ) ;
#30286 = CYLINDRICAL_SURFACE ( 'NONE', #36482, 2.725000000000000089 ) ;
#30287 = CARTESIAN_POINT ( 'NONE',  ( 8.172783018424818025, -2.939287716552612562, 6.492393787938203431 ) ) ;
#30288 = EDGE_LOOP ( 'NONE', ( #1711, #18825, #41520, #31956 ) ) ;
#30289 = CARTESIAN_POINT ( 'NONE',  ( 10.40226385995999969, -2.765692573780999641, 9.035345396600000356 ) ) ;
#30290 = CARTESIAN_POINT ( 'NONE',  ( 11.59999999999999787, 5.087332147730433185, 8.017651347927678529 ) ) ;
#30291 = CARTESIAN_POINT ( 'NONE',  ( 11.16486084871730000, 5.207010770456999893, -7.174999999999999822 ) ) ;
#30292 = CARTESIAN_POINT ( 'NONE',  ( 10.80160188108999897, -2.805072368922999715, -8.157282064671999677 ) ) ;
#30293 = CARTESIAN_POINT ( 'NONE',  ( 11.09999999999999964, 5.299999999999999822, -5.160242713806000303 ) ) ;
#30294 = VERTEX_POINT ( 'NONE', #36732 ) ;
#30295 = CARTESIAN_POINT ( 'NONE',  ( 10.62947109217999930, 5.100000000000000533, 6.152188490330000370 ) ) ;
#30296 = CARTESIAN_POINT ( 'NONE',  ( 18.50003594167399967, 2.686563651857999613, 11.33603604486000016 ) ) ;
#30297 = DIRECTION ( 'NONE',  ( -1.000000000000000000, 0.000000000000000000, -6.365544662581999450E-14 ) ) ;
#30298 = DIRECTION ( 'NONE',  ( -1.000000000000000000, 0.000000000000000000, 0.000000000000000000 ) ) ;
#30299 = CARTESIAN_POINT ( 'NONE',  ( 12.27431752107753837, 0.3302328523437060848, -13.89472426752320899 ) ) ;
#30300 = CARTESIAN_POINT ( 'NONE',  ( 18.17639191339637250, -2.431702999347771676, 12.46724561074273652 ) ) ;
#30301 = VERTEX_POINT ( 'NONE', #58051 ) ;
#30302 = CARTESIAN_POINT ( 'NONE',  ( 7.935252636294002571, -4.895109672515001620, 6.296391117214003685 ) ) ;
#30303 = EDGE_LOOP ( 'NONE', ( #3342, #14292, #29715, #33681 ) ) ;
#30304 = CARTESIAN_POINT ( 'NONE',  ( 10.42596030538999941, 5.042177533603999784, 8.702224267793999601 ) ) ;
#30305 = DIRECTION ( 'NONE',  ( 0.000000000000000000, -1.000000000000000000, 0.000000000000000000 ) ) ;
#30306 = CARTESIAN_POINT ( 'NONE',  ( 9.178620280414001797, 2.990001567622999623, -8.695425648791999862 ) ) ;
#30307 = CARTESIAN_POINT ( 'NONE',  ( 2.446810385560000078, 2.013401216687999984, -2.977891740175000024 ) ) ;
#30308 = CARTESIAN_POINT ( 'NONE',  ( 8.767879976495999372, -3.394455611366999914, -6.293427637271999942 ) ) ;
#30309 = DIRECTION ( 'NONE',  ( 0.5298945043518936693, -0.5996714848441926371, -0.5996715138493925457 ) ) ;
#30310 = CARTESIAN_POINT ( 'NONE',  ( 23.52034478825299857, 13.48676252767000072, 4.209100417191000254 ) ) ;
#30311 = ORIENTED_EDGE ( 'NONE', *, *, #55884, .F. ) ;
#30312 = EDGE_CURVE ( 'NONE', #45966, #7152, #15745, .T. ) ;
#30313 = CARTESIAN_POINT ( 'NONE',  ( 11.58841369783139896, -4.057552111898620417, 6.360711682373000109 ) ) ;
#30314 = CARTESIAN_POINT ( 'NONE',  ( 10.33467135001178860, 5.744925381912087126, -7.383168082734888671 ) ) ;
#30315 = EDGE_CURVE ( 'NONE', #19590, #66054, #25270, .T. ) ;
#30316 = CARTESIAN_POINT ( 'NONE',  ( 15.95168611684299975, 8.949867560646000086, 8.553740745252000011 ) ) ;
#30317 = CARTESIAN_POINT ( 'NONE',  ( 18.29983863916000075, 2.861762957209999847, -11.98830831200999825 ) ) ;
#30319 = DIRECTION ( 'NONE',  ( 1.000000000000000000, 0.000000000000000000, 0.000000000000000000 ) ) ;
#30318 = CARTESIAN_POINT ( 'NONE',  ( 10.71256887705999894, 5.951815279772000089, 7.233043586354999555 ) ) ;
#30320 = CARTESIAN_POINT ( 'NONE',  ( 11.04333729122639873, 2.996877626170000308, -7.473611442402849470 ) ) ;
#30321 = CARTESIAN_POINT ( 'NONE',  ( 11.02452225494999993, 2.775477745048999800, -6.571291218949999902 ) ) ;
#30322 = CARTESIAN_POINT ( 'NONE',  ( 9.047113844317999920, 4.253652595614200393, -6.528144732449299603 ) ) ;
#30323 = CARTESIAN_POINT ( 'NONE',  ( 18.20009441896381119, 0.3284204639250540847, 12.59572022474404562 ) ) ;
#30324 = CYLINDRICAL_SURFACE ( 'NONE', #26067, 0.6999999999999992895 ) ;
#30326 = CIRCLE ( 'NONE', #57110, 10.79999999999999893 ) ;
#30325 = B_SPLINE_CURVE_WITH_KNOTS ( 'NONE', 3,
 ( #60626, #55384, #66205, #18327, #39651, #60973, #55733, #41369, #62004, #62678 ),
 .UNSPECIFIED., .F., .F.,
 ( 4, 2, 2, 2, 4 ),
 ( 0.000000000000000000, 0.2499999999999997780, 0.4999999999999995559, 0.7499999999999997780, 1.000000000000000000 ),
 .UNSPECIFIED. ) ;
#30327 = CARTESIAN_POINT ( 'NONE',  ( 11.76588784977539781, 2.879134238109999799, 7.564049652083489228 ) ) ;
#30328 = CARTESIAN_POINT ( 'NONE',  ( 23.55669233645500071, 10.23544483926000126, 9.677465815984000130 ) ) ;
#30329 = ORIENTED_EDGE ( 'NONE', *, *, #5034, .F. ) ;
#30330 = CARTESIAN_POINT ( 'NONE',  ( 7.678995559621999867, -2.599231861044000169, 7.909347897884000389 ) ) ;
#30331 = FACE_OUTER_BOUND ( 'NONE', #45981, .T. ) ;
#30332 = ADVANCED_FACE ( 'NONE', ( #59763 ), #45053, .T. ) ;
#30333 = CARTESIAN_POINT ( 'NONE',  ( 8.536962618768443534, 5.285878940952796867, -7.027227351473634975 ) ) ;
#30334 = CARTESIAN_POINT ( 'NONE',  ( 10.32055864497999842, 4.682585200569199912, 6.965412239408199646 ) ) ;
#30335 = ORIENTED_EDGE ( 'NONE', *, *, #59901, .F. ) ;
#30336 = EDGE_CURVE ( 'NONE', #1683, #37807, #58707, .T. ) ;
#30337 = CARTESIAN_POINT ( 'NONE',  ( 18.48724299199999876, 3.206939682244000167, 12.14698705996000072 ) ) ;
#30338 = CARTESIAN_POINT ( 'NONE',  ( 10.51925056272499859, 5.174767082365999471, 7.482589369563879877 ) ) ;
#30339 = AXIS2_PLACEMENT_3D ( 'NONE', #6450, #54002, #47742 ) ;
#30340 = CARTESIAN_POINT ( 'NONE',  ( 10.73615471958999912, 3.078044734341000233, -6.088740491863000592 ) ) ;
#30341 = ORIENTED_EDGE ( 'NONE', *, *, #61403, .T. ) ;
#30342 = CARTESIAN_POINT ( 'NONE',  ( 5.055026506350000837, -1.500000000000000000, 0.000000000000000000 ) ) ;
#30343 = CARTESIAN_POINT ( 'NONE',  ( 9.227780634805492710, -4.987352003971340153, -6.146612417831175179 ) ) ;
#30344 = CARTESIAN_POINT ( 'NONE',  ( 11.40425819896749893, 2.744109752373000255, 7.263238376356399684 ) ) ;
#30345 = DIRECTION ( 'NONE',  ( -2.154007395656495261E-21, 3.276905819395100166E-06, -0.9999999999946310725 ) ) ;
#30346 = CARTESIAN_POINT ( 'NONE',  ( 8.162581873609997984, 3.457979189883997329, 6.166988478103001547 ) ) ;
#30347 = VERTEX_POINT ( 'NONE', #43696 ) ;
#30348 = CARTESIAN_POINT ( 'NONE',  ( 11.40162633574000139, -3.633188743968999823, 11.83198634993999931 ) ) ;
#30349 = CARTESIAN_POINT ( 'NONE',  ( 7.268539158768000163, 5.563598295091999546, -6.420781807775999717 ) ) ;
#30350 = CARTESIAN_POINT ( 'NONE',  ( 8.122344632841924650, -4.980189395210384617, 6.061431015808207867 ) ) ;
#30351 = CARTESIAN_POINT ( 'NONE',  ( 11.22567835872029995, -4.993948309075300074, -6.873560442659099046 ) ) ;
#30352 = CARTESIAN_POINT ( 'NONE',  ( 10.48524205624999972, -4.458751122174599679, 6.305876158747000026 ) ) ;
#30353 = ORIENTED_EDGE ( 'NONE', *, *, #3488, .F. ) ;
#30354 = CARTESIAN_POINT ( 'NONE',  ( 10.37168190983000038, -4.576053486415999849, -5.010430378404000074 ) ) ;
#30355 = DIRECTION ( 'NONE',  ( 0.000000000000000000, 0.000000000000000000, -1.000000000000000000 ) ) ;
#30356 = ORIENTED_EDGE ( 'NONE', *, *, #42234, .T. ) ;
#30357 = CARTESIAN_POINT ( 'NONE',  ( 10.02934687351566723, -3.836375382625533348, 6.250000000000000000 ) ) ;
#30358 = ORIENTED_EDGE ( 'NONE', *, *, #41513, .T. ) ;
#30359 = CARTESIAN_POINT ( 'NONE',  ( 10.10891502095999961, -5.332339947063000629, -7.851654145788001138 ) ) ;
#30360 = CARTESIAN_POINT ( 'NONE',  ( 8.546960841229999772, 2.724453559418999582, -8.908010318766001134 ) ) ;
#30361 = CARTESIAN_POINT ( 'NONE',  ( 11.48011496860029901, 4.919769165942200040, -7.028661263734299780 ) ) ;
#30362 = CARTESIAN_POINT ( 'NONE',  ( 12.17766954483535891, -3.284117569315500251, 8.604570063127999546 ) ) ;
#30363 = CARTESIAN_POINT ( 'NONE',  ( 12.22356881520513561, 2.729361768173758751, -12.39519383931446228 ) ) ;
#30364 = CARTESIAN_POINT ( 'NONE',  ( 10.65303300763299887, -3.212834858289399964, 6.674373427955200277 ) ) ;
#30365 = CARTESIAN_POINT ( 'NONE',  ( 9.298698341228998743, 5.159258275969999197, 9.109498396691998678 ) ) ;
#30366 = EDGE_LOOP ( 'NONE', ( #24883, #49375, #58483 ) ) ;
#30367 = CARTESIAN_POINT ( 'NONE',  ( 3.500000000000000000, -3.070497928137199128, 0.6771155813265552492 ) ) ;
#30368 = CARTESIAN_POINT ( 'NONE',  ( 7.903995559621998623, -2.095727472214000020, 8.056487497515000484 ) ) ;
#30369 = B_SPLINE_CURVE_WITH_KNOTS ( 'NONE', 3,
 ( #49717, #50761, #34344, #24183, #44494, #60901, #11963, #65787, #60555, #17912 ),
 .UNSPECIFIED., .F., .F.,
 ( 4, 2, 2, 2, 4 ),
 ( 0.000000000000000000, 0.2500000000000000000, 0.5000000000000000000, 0.7500000000000000000, 1.000000000000000000 ),
 .UNSPECIFIED. ) ;
#30370 = DIRECTION ( 'NONE',  ( 1.000000000000000000, 0.000000000000000000, 1.736057635189999993E-14 ) ) ;
#30371 = ORIENTED_EDGE ( 'NONE', *, *, #58555, .T. ) ;
#30372 = CARTESIAN_POINT ( 'NONE',  ( 12.44743307598047899, -3.012678875451597627, -12.31720924913609139 ) ) ;
#30373 = CARTESIAN_POINT ( 'NONE',  ( 11.10887482311539998, 5.184953745778000389, 7.021250586468399391 ) ) ;
#30374 = CARTESIAN_POINT ( 'NONE',  ( 10.41025564679000048, -4.690690303276999984, -6.142863315966000215 ) ) ;
#30375 = CARTESIAN_POINT ( 'NONE',  ( 6.401834305184006091, 10.52691165332000089, -4.501978947072999837 ) ) ;
#30376 = CARTESIAN_POINT ( 'NONE',  ( 17.77415039705200073, -3.297056071606000227, -11.83473721697999892 ) ) ;
#30377 = CARTESIAN_POINT ( 'NONE',  ( 24.70869262248000098, -8.717234922876000880, 9.201991545054999833 ) ) ;
#30378 = CARTESIAN_POINT ( 'NONE',  ( 12.56988000877540301, -3.209076157321562484, -13.62724777954567124 ) ) ;
#30379 = CARTESIAN_POINT ( 'NONE',  ( 11.73671932425159881, -4.127012898954600217, -8.356835045446798560 ) ) ;
#30380 = CARTESIAN_POINT ( 'NONE',  ( 10.76426088462129904, -3.997280690308189666, -6.221990224628999755 ) ) ;
#30381 = CARTESIAN_POINT ( 'NONE',  ( 17.60324894539392560, -3.198552395131814663, 12.18725844837784855 ) ) ;
#30382 = ORIENTED_EDGE ( 'NONE', *, *, #15946, .T. ) ;
#30383 = ORIENTED_EDGE ( 'NONE', *, *, #16042, .F. ) ;
#30384 = CARTESIAN_POINT ( 'NONE',  ( 12.57118179864146157, 0.6928235585492461546, -13.98285841810701413 ) ) ;
#30385 = SURFACE_STYLE_FILL_AREA ( #56605 ) ;
#30386 = CARTESIAN_POINT ( 'NONE',  ( 12.38752622490241784, -11.20128320855829607, 3.203207420542418138 ) ) ;
#30387 = CARTESIAN_POINT ( 'NONE',  ( 18.14649830791793406, 2.702104747329968859, 13.62846271467367920 ) ) ;
#30388 = CARTESIAN_POINT ( 'NONE',  ( 9.792312867577999569, 4.284154069364999984, -9.000485152170000447 ) ) ;
#30389 = DIRECTION ( 'NONE',  ( -1.000000000000000000, 0.000000000000000000, 0.000000000000000000 ) ) ;
#30390 = CARTESIAN_POINT ( 'NONE',  ( 18.17545025690710148, 2.421661855460688795, 12.46948612151124181 ) ) ;
#30391 = AXIS2_PLACEMENT_3D ( 'NONE', #32458, #53775, #17049 ) ;
#30392 = CARTESIAN_POINT ( 'NONE',  ( 17.79055474012400140, 3.643253463509999790, -12.02383756773999934 ) ) ;
#30393 = CARTESIAN_POINT ( 'NONE',  ( 11.06923869026000062, 5.425682056982999768, 8.012911262916999178 ) ) ;
#30394 = CARTESIAN_POINT ( 'NONE',  ( 9.574925248765625341, -4.744576382809566617, 7.959497855362744012 ) ) ;
#30395 = ADVANCED_FACE ( 'NONE', ( #22357 ), #60117, .F. ) ;
#30396 = ORIENTED_EDGE ( 'NONE', *, *, #36095, .F. ) ;
#30397 = CARTESIAN_POINT ( 'NONE',  ( 9.409314688805999083, 2.634692233435000031, 8.920311306029999443 ) ) ;
#30398 = ADVANCED_FACE ( 'NONE', ( #10834 ), #18388, .T. ) ;
#30399 = CARTESIAN_POINT ( 'NONE',  ( 9.298392757686999133, -3.414780058706900157, -8.139707405630899117 ) ) ;
#30400 = CARTESIAN_POINT ( 'NONE',  ( 10.79500540879000070, 3.503955365545999623, 6.168588659884999714 ) ) ;
#30401 = CARTESIAN_POINT ( 'NONE',  ( 11.38813259637009878, -5.155817667926999803, 6.870201387206400057 ) ) ;
#30402 = CARTESIAN_POINT ( 'NONE',  ( 8.672510841228998402, 4.686731264770999772, -8.717075579553000608 ) ) ;
#30403 = FACE_OUTER_BOUND ( 'NONE', #40278, .T. ) ;
#30404 = CARTESIAN_POINT ( 'NONE',  ( 12.37030581721858269, 0.4491390935506875404, 12.68931154995401123 ) ) ;
#30405 = CARTESIAN_POINT ( 'NONE',  ( 7.711426658771000753, 5.797099724369999763, 8.340484548805999765 ) ) ;
#30406 = CARTESIAN_POINT ( 'NONE',  ( 9.166073843917999397, 4.023333628930999772, 9.122276991855001071 ) ) ;
#30407 = CARTESIAN_POINT ( 'NONE',  ( 9.222206812071494397, -2.649920440492297136, 7.547755730313211231 ) ) ;
#30408 = ORIENTED_EDGE ( 'NONE', *, *, #40190, .F. ) ;
#30409 = CARTESIAN_POINT ( 'NONE',  ( 10.10682028041000002, 4.294368353031000396, -8.968663198664000191 ) ) ;
#30410 = CARTESIAN_POINT ( 'NONE',  ( 7.127572837703999298, -0.3768015417652000321, -1.438462408934000125 ) ) ;
#30411 = CARTESIAN_POINT ( 'NONE',  ( 23.50387503050299998, 0.000000000000000000, 0.000000000000000000 ) ) ;
#30412 = FACE_OUTER_BOUND ( 'NONE', #66209, .T. ) ;
#30413 = ADVANCED_FACE ( 'NONE', ( #15995 ), #10750, .F. ) ;
#30414 = CARTESIAN_POINT ( 'NONE',  ( 10.30226354018233437, 2.907767014557178786, -6.870476274536374994 ) ) ;
#30415 = CARTESIAN_POINT ( 'NONE',  ( 10.69872335273220010, -3.650693637952500126, -8.440710326446700051 ) ) ;
#30416 = ORIENTED_EDGE ( 'NONE', *, *, #20847, .T. ) ;
#30417 = AXIS2_PLACEMENT_3D ( 'NONE', #64356, #65406, #16480 ) ;
#30418 = CARTESIAN_POINT ( 'NONE',  ( 2.302021397264000235, -0.3042438094541999871, -3.579344195347000213 ) ) ;
#30419 = EDGE_CURVE ( 'NONE', #14644, #67945, #28632, .T. ) ;
#30420 = CARTESIAN_POINT ( 'NONE',  ( 11.59999999999999964, 3.182579051151299687, -7.174999999999999822 ) ) ;
#30423 = CARTESIAN_POINT ( 'NONE',  ( 14.03986884071600016, -9.265369649631999494, -8.206962993589000277 ) ) ;
#30422 = CARTESIAN_POINT ( 'NONE',  ( 8.921614158776000281, 3.251172436837000301, -6.320036569851000152 ) ) ;
#30421 = UNCERTAINTY_MEASURE_WITH_UNIT (LENGTH_MEASURE( 1.000000000000000082E-05 ), #9045, 'distance_accuracy_value', 'NONE');
#30424 = CARTESIAN_POINT ( 'NONE',  ( 15.89979320884932612, 5.681736459260974037, 10.98277228430208474 ) ) ;
#30425 = CARTESIAN_POINT ( 'NONE',  ( 11.90221299665285848, -3.091095606691090847, 7.175011619880304004 ) ) ;
#30426 = CARTESIAN_POINT ( 'NONE',  ( 12.27426597077013604, -3.015840035300837663, 13.67132055224443654 ) ) ;
#30427 = CARTESIAN_POINT ( 'NONE',  ( 10.67826222744820086, 3.331419131587999960, 6.949274830123499669 ) ) ;
#30428 = CARTESIAN_POINT ( 'NONE',  ( 11.59999999999999964, -2.792989229543000107, -7.825000000000000178 ) ) ;
#30429 = CARTESIAN_POINT ( 'NONE',  ( 7.924355646793000751, -2.432121990576000314, 6.597519606637999523 ) ) ;
#30430 = EDGE_LOOP ( 'NONE', ( #3012, #13170, #63554, #34489 ) ) ;
#30431 = CARTESIAN_POINT ( 'NONE',  ( 7.828420280408998622, 5.524123123935000379, 6.910361319981999095 ) ) ;
#30433 = CARTESIAN_POINT ( 'NONE',  ( 10.60770805961999841, -2.392337812398999564, -6.587351599745000286 ) ) ;
#30432 = CARTESIAN_POINT ( 'NONE',  ( 5.520207029896999629, -0.8842068839782000200, 1.351115652313999771 ) ) ;
#30434 = CARTESIAN_POINT ( 'NONE',  ( 7.634776897685090269, -5.200043634672757875, 6.239116708909331344 ) ) ;
#30435 = CARTESIAN_POINT ( 'NONE',  ( 18.04536508903462888, -0.3876148459371224764, 13.89272660623140787 ) ) ;
#30436 = CARTESIAN_POINT ( 'NONE',  ( 1.223519645392000088, 0.8784043042010000191, 3.483138632238000021 ) ) ;
#30437 = ORIENTED_EDGE ( 'NONE', *, *, #56041, .F. ) ;
#30438 = CARTESIAN_POINT ( 'NONE',  ( 4.500000000000000000, 0.000000000000000000, 0.000000000000000000 ) ) ;
#30439 = CARTESIAN_POINT ( 'NONE',  ( 11.39979975933730039, -3.180925410802600162, 7.781807394638899922 ) ) ;
#30440 = DIRECTION ( 'NONE',  ( 0.9999999999777403614, 3.933702048292161083E-06, 5.389360667264221932E-06 ) ) ;
#30441 = CARTESIAN_POINT ( 'NONE',  ( 9.667078842372998082, 4.541623431405000133, 5.824038024834000460 ) ) ;
#30442 = CARTESIAN_POINT ( 'NONE',  ( 11.58071932425156980, 3.832730087831799803, 6.371589232479998977 ) ) ;
#30443 = CARTESIAN_POINT ( 'NONE',  ( 8.473304831784332691, -5.100000000000000533, 6.564173320837334735 ) ) ;
#30444 = CARTESIAN_POINT ( 'NONE',  ( 18.10505187282181794, 3.528432543146514000, -12.01774066417131870 ) ) ;
#30445 = CARTESIAN_POINT ( 'NONE',  ( 11.33830977893730108, 3.023401864784708515, -6.673569913327193959 ) ) ;
#30446 = CARTESIAN_POINT ( 'NONE',  ( 8.518741573454621019, 2.828840032196707988, 6.174218200494118847 ) ) ;
#30447 = EDGE_LOOP ( 'NONE', ( #42232, #63783, #5856, #34119, #19161, #56946, #64202, #66637, #29898, #15228, #8036, #13634 ) ) ;
#30448 = CARTESIAN_POINT ( 'NONE',  ( 18.24190944330475617, -2.752675741764516903, 13.72673684790926352 ) ) ;
#30449 = FACE_OUTER_BOUND ( 'NONE', #38925, .T. ) ;
#30450 = VERTEX_POINT ( 'NONE', #53411 ) ;
#30451 = ORIENTED_EDGE ( 'NONE', *, *, #55055, .F. ) ;
#30452 = DIRECTION ( 'NONE',  ( 1.000000000000000000, 0.000000000000000000, 0.000000000000000000 ) ) ;
#30453 = ORIENTED_EDGE ( 'NONE', *, *, #48802, .T. ) ;
#30454 = CARTESIAN_POINT ( 'NONE',  ( 8.999999695565000124, 12.49999969551000056, -3.568585573319000265E-10 ) ) ;
#30455 = CARTESIAN_POINT ( 'NONE',  ( 15.90018573812067260, 7.829696748392686700, 8.945859267998583775 ) ) ;
#30456 = CARTESIAN_POINT ( 'NONE',  ( 10.43579914648999996, 2.587602126999999808, 6.390037244031000263 ) ) ;
#30457 = ADVANCED_FACE ( 'NONE', ( #22965 ), #376, .T. ) ;
#30458 = LINE ( 'NONE', #13009, #55606 ) ;
#30459 = CARTESIAN_POINT ( 'NONE',  ( 9.302887573405627109, -3.409423315843189251, -8.145562893180322561 ) ) ;
#30460 = CARTESIAN_POINT ( 'NONE',  ( 10.14750362918999826, -2.602959084636999876, 6.738575912023000214 ) ) ;
#30461 = CARTESIAN_POINT ( 'NONE',  ( 17.99148514253577602, 0.5743932053697992091, -12.58690132123599525 ) ) ;
#30462 = B_SPLINE_CURVE_WITH_KNOTS ( 'NONE', 3,
 ( #11107, #14975, #9721, #25810 ),
 .UNSPECIFIED., .F., .F.,
 ( 4, 4 ),
 ( 0.000000000000000000, 1.000000000000000000 ),
 .UNSPECIFIED. ) ;
#30463 = CARTESIAN_POINT ( 'NONE',  ( 9.934206403597999113, -5.120430559539999926, -8.883390070891001855 ) ) ;
#30464 = CARTESIAN_POINT ( 'NONE',  ( 11.31825954179440075, -3.333768806796900019, -8.053565341712399572 ) ) ;
#30465 = DIRECTION ( 'NONE',  ( -1.000000000000000000, 0.000000000000000000, 0.000000000000000000 ) ) ;
#30466 = ORIENTED_EDGE ( 'NONE', *, *, #54091, .T. ) ;
#30467 = CARTESIAN_POINT ( 'NONE',  ( 18.50001572531400029, 0.9783175424405120557, -12.52500000000000568 ) ) ;
#30468 = CARTESIAN_POINT ( 'NONE',  ( -0.2999999999999999889, 0.5773502691895999739, -1.000000000000000000 ) ) ;
#30469 = CARTESIAN_POINT ( 'NONE',  ( 10.22726354018266370, -3.370476274536371442, -6.407767014557179230 ) ) ;
#30470 = CARTESIAN_POINT ( 'NONE',  ( 17.79602238657562907, 1.801771354310892859, 12.47051018296934011 ) ) ;
#30471 = CARTESIAN_POINT ( 'NONE',  ( 12.41963733656421098, 3.136527823945737925, 13.64412816271520335 ) ) ;
#30472 = CARTESIAN_POINT ( 'NONE',  ( 11.30000000000000071, 7.371880883511000048E-13, 4.000966224993000022E-14 ) ) ;
#30473 = ORIENTED_EDGE ( 'NONE', *, *, #4804, .F. ) ;
#30474 = CARTESIAN_POINT ( 'NONE',  ( 12.19590851927750386, -0.1412562895450219513, -12.69896251113170749 ) ) ;
#30475 = CARTESIAN_POINT ( 'NONE',  ( 12.54953656384602922, -0.6834693007276645416, 13.98330741474946137 ) ) ;
#30476 = EDGE_CURVE ( 'NONE', #38805, #10241, #2007, .T. ) ;
#30477 = ORIENTED_EDGE ( 'NONE', *, *, #26611, .F. ) ;
#30478 = EDGE_CURVE ( 'NONE', #40213, #8185, #14509, .T. ) ;
#30479 = CARTESIAN_POINT ( 'NONE',  ( 24.30000000000000071, 12.03537377768999939, -3.224868684338999980 ) ) ;
#30480 = CARTESIAN_POINT ( 'NONE',  ( 10.82309687351639660, -5.217465845835395299, -7.172815144550894750 ) ) ;
#30481 = FACE_OUTER_BOUND ( 'NONE', #20081, .T. ) ;
#30482 = COLOUR_RGB ( '', 0.09019608, 0.27058824, 0.51372549) ;
#30483 = EDGE_CURVE ( 'NONE', #42097, #31041, #38648, .T. ) ;
#30484 = CARTESIAN_POINT ( 'NONE',  ( 9.447288403127886980, 2.899999999999999911, 6.305985889523069154 ) ) ;
#30485 = DIRECTION ( 'NONE',  ( 0.7070584287740061535, 0.000000000000000000, -0.7071551302929461880 ) ) ;
#30486 = CARTESIAN_POINT ( 'NONE',  ( 11.18424042080583369, 4.544092497359196514, 8.657883396625685180 ) ) ;
#30487 = CARTESIAN_POINT ( 'NONE',  ( 10.51927318630899855, -3.243547362524661359, -8.526145288591962412 ) ) ;
#30488 = DIRECTION ( 'NONE',  ( 0.000000000000000000, 0.000000000000000000, 1.000000000000000000 ) ) ;
#30489 = CARTESIAN_POINT ( 'NONE',  ( 11.19102897915239936, 4.256858847510399890, -8.470038342183499935 ) ) ;
#30490 = CARTESIAN_POINT ( 'NONE',  ( 6.966665878461012262, -12.09896511371897176, -3.276379751798359052 ) ) ;
#30491 = CARTESIAN_POINT ( 'NONE',  ( 10.40480513895999870, 4.779740423663599636, -7.066537524675499782 ) ) ;
#30492 = CARTESIAN_POINT ( 'NONE',  ( 9.073392757686999488, 4.863450031739999346, -8.443842375698499936 ) ) ;
#30494 = CARTESIAN_POINT ( 'NONE',  ( 12.18137864099478129, 2.541952522782075174, 12.44169427841725017 ) ) ;
#30493 = FACE_OUTER_BOUND ( 'NONE', #39831, .T. ) ;
#30495 = CARTESIAN_POINT ( 'NONE',  ( 23.57017933877721916, -13.34347207735601160, 4.199491041959400484 ) ) ;
#30496 = ORIENTED_EDGE ( 'NONE', *, *, #68640, .F. ) ;
#30497 = EDGE_CURVE ( 'NONE', #65921, #6365, #27015, .T. ) ;
#30498 = CARTESIAN_POINT ( 'NONE',  ( 11.59603632436369125, 3.157359628034400068, 7.696781148700499564 ) ) ;
#30499 = CYLINDRICAL_SURFACE ( 'NONE', #19551, 1.350000000000000089 ) ;
#30501 = B_SPLINE_CURVE_WITH_KNOTS ( 'NONE', 3,
 ( #8088, #12296, #51080, #12640, #49696, #1805, #50047, #44474, #29777, #7739, #66460, #50737, #44812, #35011, #3183, #7045, #66114, #45153, #8431, #55293, #44123, #2835, #29081, #18922, #39556, #23123, #17893, #18581, #28380, #12995, #18235, #56327, #61228, #65420, #34668, #55641, #39210, #24161, #38870, #2156, #40247, #28733, #33970, #60191, #61567, #23473, #33628, #45497, #13682, #34319, #39909, #60880, #50392, #2492, #23816, #13344, #29430, #61909, #24511, #40928, #25189, #30785, #41616, #51418, #45832, #24852, #15397, #41277, #19256 ),
 .UNSPECIFIED., .F., .F.,
 ( 4, 2, 2, 2, 2, 2, 2, 2, 2, 2, 2, 2, 2, 1, 2, 2, 2, 1, 2, 2, 2, 2, 1, 2, 2, 2, 2, 2, 2, 2, 2, 2, 2, 2, 2, 4 ),
 ( 0.000000000000000000, 0.06249999999998720468, 0.1249999999999744094, 0.1562499999999680256, 0.1874999999999616140, 0.2187499999999552025, 0.2343749999999517886, 0.2499999999999483746, 0.2812499999999429900, 0.2968749999999389377, 0.3124999999999349409, 0.3281249999999308886, 0.3437499999999268363, 0.3593749999999228395, 0.3671874999999213407, 0.3749999999999198419, 0.3906249999999188427, 0.3984374999999183986, 0.4023437499999183986, 0.4062499999999184541, 0.4218749999999176215, 0.4296874999999177880, 0.4335937499999183431, 0.4355468749999186207, 0.4374999999999188427, 0.4531249999999202305, 0.4687499999999215627, 0.4843749999999229505, 0.4999999999999242828, 0.5312499999999269473, 0.5468749999999288347, 0.5624999999999306111, 0.5937499999999351630, 0.6249999999999397149, 0.7499999999999591438, 1.000000000000000000 ),
 .UNSPECIFIED. ) ;
#30500 = CARTESIAN_POINT ( 'NONE',  ( 9.703659112603999048, 3.623260508844300176, 6.719118894894999805 ) ) ;
#30502 = DIRECTION ( 'NONE',  ( 1.000000000000000000, 0.000000000000000000, 0.000000000000000000 ) ) ;
#30503 = CARTESIAN_POINT ( 'NONE',  ( 8.599999986286999132, 4.750000013710600655, 7.499999999961952213 ) ) ;
#30504 = CARTESIAN_POINT ( 'NONE',  ( 25.44993786153400350, -9.517611874540000017, 8.103398312166000039 ) ) ;
#30505 = DIRECTION ( 'NONE',  ( 1.000000000000000000, 0.000000000000000000, 0.000000000000000000 ) ) ;
#30506 = CARTESIAN_POINT ( 'NONE',  ( 5.500000000000000000, 0.000000000000000000, 0.000000000000000000 ) ) ;
#30507 = ORIENTED_EDGE ( 'NONE', *, *, #4071, .T. ) ;
#30508 = VECTOR ( 'NONE', #51935, 1000.000000000000227 ) ;
#30509 = CARTESIAN_POINT ( 'NONE',  ( 9.428000818238999159, -5.131870447930000800, -8.096031607030200306 ) ) ;
#30510 = CARTESIAN_POINT ( 'NONE',  ( 11.09999999999999964, 2.649999999999999911, -7.500000000000000000 ) ) ;
#30511 = CARTESIAN_POINT ( 'NONE',  ( 11.02435971519499880, -3.467537960339900138, 8.385788382729799650 ) ) ;
#30512 = CARTESIAN_POINT ( 'NONE',  ( 18.27818099403247132, 2.425134644239746340, -12.36441930324461858 ) ) ;
#30513 = CARTESIAN_POINT ( 'NONE',  ( 2.646806799209334482, -0.9161175952574931447, 3.408904368339100710 ) ) ;
#30514 = CARTESIAN_POINT ( 'NONE',  ( 18.16712151969790412, 2.626596269802297989, 12.42116978061485710 ) ) ;
#30515 = B_SPLINE_CURVE_WITH_KNOTS ( 'NONE', 3,
 ( #42779, #53612, #38216, #64426, #59545, #63747, #16548, #37528, #63403, #32304, #47342, #32639, #6052, #22137, #21111, #20765, #53949, #27391, #43478, #15859, #32981, #54295, #6397 ),
 .UNSPECIFIED., .F., .F.,
 ( 4, 2, 2, 2, 2, 2, 2, 2, 2, 1, 2, 4 ),
 ( 0.000000000000000000, 0.2499999999999990008, 0.3749999999999970579, 0.4374999999999952816, 0.4687499999999953926, 0.4999999999999955591, 0.7499999999999988898, 0.8749999999999990008, 0.9374999999999977796, 0.9687499999999971134, 0.9843749999999986677, 1.000000000000000000 ),
 .UNSPECIFIED. ) ;
#30516 = B_SPLINE_CURVE_WITH_KNOTS ( 'NONE', 3,
 ( #34332, #33638, #12305, #29441, #2168 ),
 .UNSPECIFIED., .F., .F.,
 ( 4, 1, 4 ),
 ( 0.000000000000000000, 0.6268453884324000080, 1.000000000000000000 ),
 .UNSPECIFIED. ) ;
#30517 = CARTESIAN_POINT ( 'NONE',  ( 12.35418469965838995, 2.932966736137118335, -13.57204261866905526 ) ) ;
#30518 = CARTESIAN_POINT ( 'NONE',  ( 11.04862408378999916, -2.758083014511000020, -5.064624117739000120 ) ) ;
#30519 = CARTESIAN_POINT ( 'NONE',  ( 24.69847990089700218, 12.37231928222000121, 2.942482175274999889 ) ) ;
#30520 = CARTESIAN_POINT ( 'NONE',  ( 8.972537864292000620, 2.899999999999999911, -6.571291218949999902 ) ) ;
#30521 = CARTESIAN_POINT ( 'NONE',  ( 12.35439258730998446, 0.5721320424853930664, -13.98830666644471421 ) ) ;
#30522 = CARTESIAN_POINT ( 'NONE',  ( 13.73763077846600034, -8.978479145825000174, -7.363267546620999582 ) ) ;
#30523 = CARTESIAN_POINT ( 'NONE',  ( 11.09999999999000053, 7.516533755232999603, 6.492360339384999790 ) ) ;
#30524 = CARTESIAN_POINT ( 'NONE',  ( 2.435247277619000172, 2.372532593102000043, -2.573147701680999599 ) ) ;
#30525 = CARTESIAN_POINT ( 'NONE',  ( 9.791229719590001324, 4.294368353031000396, -8.968663198664000191 ) ) ;
#30527 = VECTOR ( 'NONE', #3790, 1000.000000000000114 ) ;
#30526 = PLANE ( 'NONE',  #35131 ) ;
#30528 = ORIENTED_EDGE ( 'NONE', *, *, #66350, .T. ) ;
#30529 = CARTESIAN_POINT ( 'NONE',  ( 8.674830025576039105, -2.649890579813208191, 7.499988935010342139 ) ) ;
#30530 = CARTESIAN_POINT ( 'NONE',  ( 18.27898184041757901, 2.472823623527002912, -13.77990254017907112 ) ) ;
#30531 = ORIENTED_EDGE ( 'NONE', *, *, #31322, .T. ) ;
#30532 = CARTESIAN_POINT ( 'NONE',  ( 10.59259632033900012, -4.802737635155300389, 7.827597670336898794 ) ) ;
#30533 = CARTESIAN_POINT ( 'NONE',  ( 11.76588784977539781, 2.879134238109999799, 7.564049652083489228 ) ) ;
#30534 = CARTESIAN_POINT ( 'NONE',  ( 18.50003594170800270, 2.686563649653999963, -11.33603604535000109 ) ) ;
#30535 = ADVANCED_FACE ( 'NONE', ( #45341 ), #11543, .F. ) ;
#30536 = CARTESIAN_POINT ( 'NONE',  ( 9.837290039650055107, 2.697792955639530810, -7.971619481532576934 ) ) ;
#30537 = ADVANCED_FACE ( 'NONE', ( #65953 ), #45683, .F. ) ;
#30538 = CARTESIAN_POINT ( 'NONE',  ( 11.52166954483529793, -3.437903757373499847, -6.632714178206799538 ) ) ;
#30539 = CARTESIAN_POINT ( 'NONE',  ( 11.59999999999999964, -2.820501972398000046, -7.174999999999999822 ) ) ;
#30540 = CARTESIAN_POINT ( 'NONE',  ( 9.075651506909604649, -2.765563590215046830, -7.567790861611047859 ) ) ;
#30541 = ORIENTED_EDGE ( 'NONE', *, *, #20828, .F. ) ;
#30542 = CARTESIAN_POINT ( 'NONE',  ( 9.909870477708999204, 2.749999999999999556, -7.750389189149368363 ) ) ;
#30543 = CARTESIAN_POINT ( 'NONE',  ( 9.933354719590999693, 5.639765292528999829, -8.059103558718000215 ) ) ;
#30544 = ORIENTED_EDGE ( 'NONE', *, *, #45539, .F. ) ;
#30545 = CARTESIAN_POINT ( 'NONE',  ( 10.48414939117999900, 4.098653981087000631, -9.351365234892998757 ) ) ;
#30546 = ORIENTED_EDGE ( 'NONE', *, *, #57050, .T. ) ;
#30547 = CARTESIAN_POINT ( 'NONE',  ( 10.01057120343299900, 3.937990586507050139, 6.222291352336999815 ) ) ;
#30548 = CARTESIAN_POINT ( 'NONE',  ( 17.71825832218067731, -1.896331189961580455, -12.57190091395960252 ) ) ;
#30549 = DIRECTION ( 'NONE',  ( 1.000000000000000000, 0.000000000000000000, 0.000000000000000000 ) ) ;
#30550 = CARTESIAN_POINT ( 'NONE',  ( 4.400040034343773776, -0.7410138808234234542, 1.163549719693206974 ) ) ;
#30551 = CARTESIAN_POINT ( 'NONE',  ( 11.82240614981508742, -3.267563509902000174, 7.017906081141797259 ) ) ;
#30552 = ORIENTED_EDGE ( 'NONE', *, *, #4248, .F. ) ;
#30553 = DIRECTION ( 'NONE',  ( 1.000000000000000000, 0.000000000000000000, 0.000000000000000000 ) ) ;
#30554 = CARTESIAN_POINT ( 'NONE',  ( 10.31153584123000044, 2.716831823259000078, -7.950163994344000784 ) ) ;
#30555 = CARTESIAN_POINT ( 'NONE',  ( 8.091573680993423778, -3.319738643651890531, 8.680038712423783664 ) ) ;
#30556 = CARTESIAN_POINT ( 'NONE',  ( 23.56665657345700282, 3.286260152889999888E-13, -3.641531520771000148E-13 ) ) ;
#30557 = AXIS2_PLACEMENT_3D ( 'NONE', #29637, #61430, #13547 ) ;
#30558 = EDGE_CURVE ( 'NONE', #4322, #12209, #39521, .T. ) ;
#30559 = CARTESIAN_POINT ( 'NONE',  ( 12.79999999975700042, -11.86189249994999884, 3.298671769835999967 ) ) ;
#30560 = DIRECTION ( 'NONE',  ( -1.000000000000000000, 0.000000000000000000, 0.000000000000000000 ) ) ;
#30561 = CARTESIAN_POINT ( 'NONE',  ( 18.10184288975604616, -2.186031417450792880, 12.51954808658139839 ) ) ;
#30562 = ORIENTED_EDGE ( 'NONE', *, *, #32992, .T. ) ;
#30563 = ORIENTED_EDGE ( 'NONE', *, *, #45197, .F. ) ;
#30564 = CARTESIAN_POINT ( 'NONE',  ( 9.825045280412000537, 3.116293075258000478, -6.208411413796000033 ) ) ;
#30565 = CARTESIAN_POINT ( 'NONE',  ( 4.399997082757115763, -2.000000000000000000, 2.821984141243951889E-09 ) ) ;
#30566 = CARTESIAN_POINT ( 'NONE',  ( 1.050973465875000068, 3.500000000000000000, 0.000000000000000000 ) ) ;
#30567 = CARTESIAN_POINT ( 'NONE',  ( 24.45991766033800019, 8.787291314975000489, -8.710735419493000009 ) ) ;
#30568 = CARTESIAN_POINT ( 'NONE',  ( 23.73546195074399989, 9.842300901745000274, -9.786565046940999935 ) ) ;
#30569 = CARTESIAN_POINT ( 'NONE',  ( 17.85728973496400229, -3.190139087762999814, -11.45065787240999988 ) ) ;
#30571 = CARTESIAN_POINT ( 'NONE',  ( 8.634347174277479553, 5.179539635115185447, 6.206398391140019122 ) ) ;
#30570 = CARTESIAN_POINT ( 'NONE',  ( 9.954392757686999715, -3.229293331742300044, 6.657535947657399866 ) ) ;
#30572 = AXIS2_PLACEMENT_3D ( 'NONE', #7218, #66282, #34143 ) ;
#30573 = CARTESIAN_POINT ( 'NONE',  ( 8.366396006187004630, -4.495298813396003013, -6.688382266309997881 ) ) ;
#30574 = ORIENTED_EDGE ( 'NONE', *, *, #44248, .T. ) ;
#30575 = CARTESIAN_POINT ( 'NONE',  ( 9.779346873515665450, 3.836375382625536012, -6.249999999999999112 ) ) ;
#30576 = ADVANCED_FACE ( 'NONE', ( #40099 ), #33818, .F. ) ;
#30577 = CIRCLE ( 'NONE', #12713, 1.449999999999999956 ) ;
#30578 = CARTESIAN_POINT ( 'NONE',  ( 11.09999999999999964, -6.350523631572000838, 5.385484235140999942 ) ) ;
#30579 = CARTESIAN_POINT ( 'NONE',  ( 9.661149330668999724, -3.300107492866999781, -5.762405935562999737 ) ) ;
#30580 = CARTESIAN_POINT ( 'NONE',  ( 17.55505043854147118, -3.248109929747637903, 13.61799478206225444 ) ) ;
#30581 = B_SPLINE_CURVE_WITH_KNOTS ( 'NONE', 3,
 ( #65367, #38462, #17837, #33917 ),
 .UNSPECIFIED., .F., .F.,
 ( 4, 4 ),
 ( 0.000000000000000000, 1.000000000000000000 ),
 .UNSPECIFIED. ) ;
#30582 = LINE ( 'NONE', #29915, #22057 ) ;
#30583 = CARTESIAN_POINT ( 'NONE',  ( 11.13119666232000071, -5.321218240682999756, 5.002382960257000022 ) ) ;
#30584 = CARTESIAN_POINT ( 'NONE',  ( 10.20448674122272337, 2.648429362731234082, 7.853061647120905597 ) ) ;
#30585 = CARTESIAN_POINT ( 'NONE',  ( 13.78329442975000063, 8.859672882948000705, 7.785394853692999995 ) ) ;
#30586 = CARTESIAN_POINT ( 'NONE',  ( 7.960542845103298681, 2.951378269640129393, -6.549292586381456616 ) ) ;
#30587 = B_SPLINE_CURVE_WITH_KNOTS ( 'NONE', 3,
 ( #35945, #42569, #36986, #68780 ),
 .UNSPECIFIED., .F., .F.,
 ( 4, 4 ),
 ( 0.000000000000000000, 1.000000000000000000 ),
 .UNSPECIFIED. ) ;
#30588 = CARTESIAN_POINT ( 'NONE',  ( 6.798969222281000313, -1.006517980596000061, 0.5009083264753000364 ) ) ;
#30589 = DIRECTION ( 'NONE',  ( -1.000000000000000000, 0.000000000000000000, 0.000000000000000000 ) ) ;
#30590 = CARTESIAN_POINT ( 'NONE',  ( 3.348657167312000027, 2.653411138596999841, 1.892272653627999901 ) ) ;
#30591 = ORIENTED_EDGE ( 'NONE', *, *, #17695, .F. ) ;
#30592 = CARTESIAN_POINT ( 'NONE',  ( 12.80505043854144276, 0.7192913403693124152, -12.57945229203838267 ) ) ;
#30593 = CARTESIAN_POINT ( 'NONE',  ( 12.20453436417063386, -2.673271222646852241, -12.40950569886774879 ) ) ;
#30594 = CARTESIAN_POINT ( 'NONE',  ( 24.67921321800200118, -8.727630028894999725, 9.158313644156001132 ) ) ;
#30595 = CARTESIAN_POINT ( 'NONE',  ( 24.67921580188599862, 3.567514645466999923, -12.13750897870000145 ) ) ;
#30596 = CYLINDRICAL_SURFACE ( 'NONE', #27182, 1.250000000000000222 ) ;
#30597 = EDGE_LOOP ( 'NONE', ( #21917, #17373, #46615, #41801 ) ) ;
#30598 = DIRECTION ( 'NONE',  ( -2.317113318597000329E-09, -7.301652274642000223E-12, -1.000000000000000000 ) ) ;
#30599 = APPLICATION_PROTOCOL_DEFINITION ( 'draft international standard', 'automotive_design', 1998, #28926 ) ;
#30600 = CARTESIAN_POINT ( 'NONE',  ( 17.88388243132641975, 0.5319787655177421470, 12.68500714331677770 ) ) ;
#30601 = CARTESIAN_POINT ( 'NONE',  ( 12.99229341877100019, -11.49414526569999850, -1.652619848542000058 ) ) ;
#30602 = CARTESIAN_POINT ( 'NONE',  ( 7.806695108664264637, 3.013278973495211677, 6.528997597326380742 ) ) ;
#30603 = CARTESIAN_POINT ( 'NONE',  ( 11.56322412107030928, 4.054600656575539475, -6.467939235001000320 ) ) ;
#30604 = ORIENTED_EDGE ( 'NONE', *, *, #37813, .T. ) ;
#30605 = CONICAL_SURFACE ( 'NONE', #53012, 1.449999999966000264, 0.7853981633972997312 ) ;
#30606 = CARTESIAN_POINT ( 'NONE',  ( 10.31457635473999979, -5.362146312020000138, 6.677778992223999843 ) ) ;
#30607 = VERTEX_POINT ( 'NONE', #61414 ) ;
#30608 = CARTESIAN_POINT ( 'NONE',  ( 9.299999999999998934, 4.537600397704999899, 9.154563893594000135 ) ) ;
#30609 = CARTESIAN_POINT ( 'NONE',  ( 7.571668146791999732, -2.531197775378000170, 8.216705951490000714 ) ) ;
#30610 = CARTESIAN_POINT ( 'NONE',  ( 17.78802761781599884, -0.6915911779535856008, -13.98290807251246726 ) ) ;
#30611 = EDGE_CURVE ( 'NONE', #24493, #30037, #20488, .T. ) ;
#30612 = ORIENTED_EDGE ( 'NONE', *, *, #2298, .T. ) ;
#30613 = CARTESIAN_POINT ( 'NONE',  ( 23.56664318980499928, 10.37807351222000030, 9.381504534996999212 ) ) ;
#30614 = ADVANCED_FACE ( 'NONE', ( #28221 ), #1648, .T. ) ;
#30615 = CARTESIAN_POINT ( 'NONE',  ( 25.29987517282700082, -11.77655473258999841, 4.190794510628000680 ) ) ;
#30616 = CARTESIAN_POINT ( 'NONE',  ( 6.835779719590999726, 3.450042761745999886, -8.965148246193999526 ) ) ;
#30617 = CARTESIAN_POINT ( 'NONE',  ( 24.30000000000000071, -11.76537389984999926, 3.877215761401999750 ) ) ;
#30618 = EDGE_CURVE ( 'NONE', #46265, #68830, #56165, .T. ) ;
#30619 = CARTESIAN_POINT ( 'NONE',  ( 12.80505043854146940, -3.166036643249212634, 13.55322769257718996 ) ) ;
#30620 = ORIENTED_EDGE ( 'NONE', *, *, #24617, .F. ) ;
#30621 = CARTESIAN_POINT ( 'NONE',  ( 9.967845797207999681, -2.034786297409000078, 7.636877353231999344 ) ) ;
#30622 = EDGE_CURVE ( 'NONE', #47384, #15208, #41130, .T. ) ;
#30623 = CARTESIAN_POINT ( 'NONE',  ( 11.59999999999999609, 4.866008700487510552, 8.272804384030438385 ) ) ;
#30624 = LINE ( 'NONE', #68011, #30508 ) ;
#30625 = VERTEX_POINT ( 'NONE', #62434 ) ;
#30626 = CARTESIAN_POINT ( 'NONE',  ( 10.29094647910999782, -2.903513699412000104, -8.310923036409999298 ) ) ;
#30627 = CONICAL_SURFACE ( 'NONE', #25074, 1.199999999294000252, 0.7853981633972997312 ) ;
#30628 = CARTESIAN_POINT ( 'NONE',  ( 7.954299074928001367, 3.414461172233999697, -6.283593702261001113 ) ) ;
#30629 = EDGE_LOOP ( 'NONE', ( #49646, #30720, #278 ) ) ;
#30630 = CARTESIAN_POINT ( 'NONE',  ( 10.74163761344578738, 5.515432212743636597, 8.372100252378068319 ) ) ;
#30631 = AXIS2_PLACEMENT_3D ( 'NONE', #50904, #24334, #19080 ) ;
#30632 = CARTESIAN_POINT ( 'NONE',  ( 8.599999952505998024, -4.000000000000000000, -8.249999993641800700 ) ) ;
#30633 = CARTESIAN_POINT ( 'NONE',  ( 10.90000000000000036, -2.899999999999999911, 6.414037451299000381 ) ) ;
#30634 = CARTESIAN_POINT ( 'NONE',  ( 3.209306799211167238, -3.058252359239909790, 1.762666431298136382 ) ) ;
#30635 = CARTESIAN_POINT ( 'NONE',  ( 9.404346873515669003, -5.250000000000000888, -7.663624617374465764 ) ) ;
#30636 = CARTESIAN_POINT ( 'NONE',  ( 18.09722825099193599, -2.811571021179180896, 12.37353494292366030 ) ) ;
#30637 = EDGE_LOOP ( 'NONE', ( #45585, #34072, #61996, #68667 ) ) ;
#30638 = CARTESIAN_POINT ( 'NONE',  ( 8.328787166962994704, -5.102611464338999703, 6.655261220345003004 ) ) ;
#30639 = EDGE_LOOP ( 'NONE', ( #52714, #5887 ) ) ;
#30640 = CARTESIAN_POINT ( 'NONE',  ( 9.792569055495000896, 3.463432304708999876, 6.184396499233999478 ) ) ;
#30641 = EDGE_CURVE ( 'NONE', #3842, #58572, #39393, .T. ) ;
#30642 = CYLINDRICAL_SURFACE ( 'NONE', #63502, 1.350000000000000533 ) ;
#30643 = CARTESIAN_POINT ( 'NONE',  ( 10.10682028041000002, 4.294368353031000396, -8.968663198664000191 ) ) ;
#30644 = CARTESIAN_POINT ( 'NONE',  ( 3.641673371380000024, -3.059358981837999814, 1.788244077786999897 ) ) ;
#30645 = CARTESIAN_POINT ( 'NONE',  ( 10.79839246847000034, -5.269358106415999110, -6.148714306659999629 ) ) ;
#30646 = CARTESIAN_POINT ( 'NONE',  ( 15.90000000000000036, 8.611670352361814551, 8.369116320313937152 ) ) ;
#30647 = CARTESIAN_POINT ( 'NONE',  ( 23.61267528292200168, 13.29118196436999888, 4.056509241667999532 ) ) ;
#30648 = ORIENTED_EDGE ( 'NONE', *, *, #24535, .T. ) ;
#30649 = CARTESIAN_POINT ( 'NONE',  ( 11.16995391537419913, -3.056324258617099776, 6.859089544950699668 ) ) ;
#30650 = CARTESIAN_POINT ( 'NONE',  ( 3.134306799210999195, 1.762666431298139713, 3.058252359239908458 ) ) ;
#30651 = CARTESIAN_POINT ( 'NONE',  ( 11.09999999999999964, -2.338960882173506839, -6.969127111924879436 ) ) ;
#30652 = CARTESIAN_POINT ( 'NONE',  ( 11.00000000000000000, 4.000000000000000000, -7.500000000000000000 ) ) ;
#30654 = CARTESIAN_POINT ( 'NONE',  ( 12.56916471290115922, 1.825881566112697696, -13.88043612360007550 ) ) ;
#30653 = CARTESIAN_POINT ( 'NONE',  ( 9.724611353170001138, 2.928305163963000446, 8.718478150869000132 ) ) ;
#30655 = AXIS2_PLACEMENT_3D ( 'NONE', #27079, #37218, #157 ) ;
#30656 = CARTESIAN_POINT ( 'NONE',  ( 11.43302763632549990, 2.964209339073000216, -7.022058766158599141 ) ) ;
#30657 = CARTESIAN_POINT ( 'NONE',  ( 12.80505043854146940, -3.199751711897561801, 12.18694338143115452 ) ) ;
#30658 = EDGE_CURVE ( 'NONE', #42176, #38787, #11027, .T. ) ;
#30659 = CARTESIAN_POINT ( 'NONE',  ( 9.528367640780999182, 4.473477001189199775, -6.614188603779100006 ) ) ;
#30660 = CARTESIAN_POINT ( 'NONE',  ( 18.05096829067922215, 0.5248261352964532778, 12.58906749861124119 ) ) ;
#30661 = PRODUCT_DEFINITION_SHAPE ( 'NONE', 'NONE',  #69202 ) ;
#30662 = CARTESIAN_POINT ( 'NONE',  ( 6.828409023426000424, -0.7941163275365998864, -0.9951805479851000280 ) ) ;
#30663 = FACE_OUTER_BOUND ( 'NONE', #27092, .T. ) ;
#30664 = ADVANCED_FACE ( 'NONE', ( #38273 ), #4856, .T. ) ;
#30665 = CARTESIAN_POINT ( 'NONE',  ( 9.310863317747999801, -3.039136629551499880, 7.499999999926881600 ) ) ;
#30666 = VERTEX_POINT ( 'NONE', #54006 ) ;
#30667 = CARTESIAN_POINT ( 'NONE',  ( 7.191894353207000101, -3.501517589953999643, 9.055975309745999624 ) ) ;
#30668 = CARTESIAN_POINT ( 'NONE',  ( 18.00769469217370400, 3.088460579138320394, 13.65508963078420379 ) ) ;
#30669 = CARTESIAN_POINT ( 'NONE',  ( 9.091433907306445406, 4.945719512329345591, 6.668243572402049679 ) ) ;
#30670 = EDGE_LOOP ( 'NONE', ( #32447, #37712, #25044, #34824, #66487, #14265, #53404, #16009, #67313, #10654 ) ) ;
#30671 = VECTOR ( 'NONE', #58151, 1000.000000000000000 ) ;
#30672 = CARTESIAN_POINT ( 'NONE',  ( 18.35500032369700207, 2.879010252073999521, 12.03969535450000095 ) ) ;
#30673 = AXIS2_PLACEMENT_3D ( 'NONE', #64487, #42500, #5434 ) ;
#30674 = CARTESIAN_POINT ( 'NONE',  ( 10.76857802013509868, 2.825431102905000103, 7.527343341769989316 ) ) ;
#30675 = CARTESIAN_POINT ( 'NONE',  ( 10.41025778040999938, 4.690688562647999937, -6.142866736126999960 ) ) ;
#30676 = ORIENTED_EDGE ( 'NONE', *, *, #64935, .F. ) ;
#30677 = CARTESIAN_POINT ( 'NONE',  ( 5.075859839683335650, -1.460959015002473826, -0.3926218265389207485 ) ) ;
#30678 = CARTESIAN_POINT ( 'NONE',  ( 24.30001694968100168, 3.271769180623000040, -12.21048179117000032 ) ) ;
#30679 = CARTESIAN_POINT ( 'NONE',  ( 10.27610941423800028, 4.844410192686099847, 8.266982106121901097 ) ) ;
#30680 = CARTESIAN_POINT ( 'NONE',  ( 24.53428993882599940, 8.855929947951999281, -9.286429770520999938 ) ) ;
#30681 = CARTESIAN_POINT ( 'NONE',  ( 8.710288521113000115, 3.647046440108700160, -8.284550957747498501 ) ) ;
#30682 = VERTEX_POINT ( 'NONE', #5765 ) ;
#30683 = CARTESIAN_POINT ( 'NONE',  ( 11.44437913529000106, -3.868861692926000462, 11.85573592760000139 ) ) ;
#30684 = DIRECTION ( 'NONE',  ( 0.9999999998140244317, 1.053700670848026541E-05, -1.615309289866040602E-05 ) ) ;
#30685 = VECTOR ( 'NONE', #9027, 1000.000000000000000 ) ;
#30686 = CARTESIAN_POINT ( 'NONE',  ( 8.106698381332673620, -4.688446296872112562, 5.897672128492101429 ) ) ;
#30687 = CARTESIAN_POINT ( 'NONE',  ( 9.423430433046998900, -4.971677342931100085, 8.099647887697699389 ) ) ;
#30688 = ORIENTED_EDGE ( 'NONE', *, *, #3397, .F. ) ;
#30689 = CARTESIAN_POINT ( 'NONE',  ( 10.95570209549000040, -5.337917385706000495, -4.890560488315999876 ) ) ;
#30690 = CYLINDRICAL_SURFACE ( 'NONE', #65189, 1.250000000000000222 ) ;
#30691 = EDGE_LOOP ( 'NONE', ( #10602, #42235, #2258, #14772 ) ) ;
#30692 = CARTESIAN_POINT ( 'NONE',  ( 9.914763540182331525, -5.217465845835395299, 7.172815144550902744 ) ) ;
#30693 = ORIENTED_EDGE ( 'NONE', *, *, #62895, .T. ) ;
#30694 = CYLINDRICAL_SURFACE ( 'NONE', #61000, 1.350000000000000089 ) ;
#30695 = CARTESIAN_POINT ( 'NONE',  ( 2.509306799210165639, 3.058252359239904905, -1.762666431298142600 ) ) ;
#30696 = CARTESIAN_POINT ( 'NONE',  ( 10.59725056272499977, 5.316133253199000208, -7.519505747156228992 ) ) ;
#30697 = CARTESIAN_POINT ( 'NONE',  ( 12.09456039236534330, -2.685288321999000249, 7.436015812896529020 ) ) ;
#30698 = CARTESIAN_POINT ( 'NONE',  ( 12.20301641406251747, 2.331821773330017944, -12.48918929053769844 ) ) ;
#30699 = EDGE_CURVE ( 'NONE', #43332, #53505, #29451, .T. ) ;
#30700 = CARTESIAN_POINT ( 'NONE',  ( 11.39149144726329865, -4.659577337894599935, 8.430724369296298093 ) ) ;
#30701 = CARTESIAN_POINT ( 'NONE',  ( 7.437260841228000352, 2.216873702600000051, 8.370081218683999680 ) ) ;
#30702 = EDGE_CURVE ( 'NONE', #32067, #61556, #32773, .T. ) ;
#30703 = ORIENTED_EDGE ( 'NONE', *, *, #35769, .F. ) ;
#30704 = CARTESIAN_POINT ( 'NONE',  ( 9.552263540183332680, 5.092232985442822546, -8.129523725463625894 ) ) ;
#30705 = CARTESIAN_POINT ( 'NONE',  ( 17.60358162559704454, -0.7192569394297189111, 12.57945425907933945 ) ) ;
#30706 = LINE ( 'NONE', #58300, #1134 ) ;
#30707 = ORIENTED_EDGE ( 'NONE', *, *, #42138, .T. ) ;
#30708 = B_SPLINE_SURFACE_WITH_KNOTS ( 'NONE', 3, 3, ( 
 ( #46506, #40563, #61547, #50720, #30097, #4181, #24144, #3833, #57323, #2814, #9424, #29756, #14688, #19589, #30767, #51401, #45815, #67464, #67809, #8413, #61890, #3497, #45475, #68152, #55961, #19933, #40910, #34992, #36007, #15027, #14006, #52077, #3162, #41254, #66792 ),
 ( #19236, #62906, #25520, #46848, #24833, #9090, #35335, #46160, #24492, #8068, #13663, #20271, #30429, #56649, #62569, #51739, #41597, #29412, #67126, #35673, #56307, #51060, #8755, #62232, #14349, #25171, #5221, #16051, #27241, #36351, #48565, #9772, #37044, #58023, #64626 ),
 ( #321, #37382, #31457, #5560, #25859, #26902, #4523, #5899, #57666, #52426, #63249, #31123, #669, #68493, #21981, #47192, #43322, #20617, #58359, #10125, #41941, #59052, #21637, #42972, #58704, #52775, #48214, #15374, #64279, #36703, #4870, #26211, #47539, #68844, #20962 ),
 ( #53467, #42300, #16396, #26557, #37723, #47884, #63598, #15716, #10461, #31803, #53119, #11154, #32489, #69188, #53802, #21300, #32151, #42630, #63940, #10807, #6938, #48910, #39454, #6242, #12888, #60773, #1354, #43668, #1018, #28273, #17790, #44712, #39108, #7289, #11836 ) ),
 .UNSPECIFIED., .F., .F., .F.,
 ( 4, 4 ),
 ( 4, 1, 1, 1, 1, 1, 1, 1, 1, 1, 1, 1, 1, 1, 1, 1, 1, 1, 1, 1, 1, 1, 1, 1, 1, 1, 1, 1, 1, 1, 1, 1, 4 ),
 ( -0.1039086239011999951, 1.103908623900999864 ),
 ( -0.02000000000000000042, 0.01250000000000000069, 0.04499999999999999833, 0.07749999999999999944, 0.1100000000000000006, 0.1424999999999999878, 0.1749999999999999889, 0.2074999999999999900, 0.2399999999999999911, 0.2725000000000000200, 0.3049999999999999933, 0.3375000000000000222, 0.3699999999999999956, 0.4025000000000000244, 0.4349999999999999978, 0.4675000000000000266, 0.5000000000000000000, 0.5324999999999999734, 0.5649999999999999467, 0.5975000000000000311, 0.6300000000000000044, 0.6624999999999999778, 0.6949999999999999512, 0.7275000000000000355, 0.7600000000000000089, 0.7924999999999999822, 0.8249999999999999556, 0.8575000000000000400, 0.8900000000000000133, 0.9224999999999999867, 0.9549999999999999600, 0.9875000000000000444, 1.020000000000000018 ),
 .UNSPECIFIED. ) ;
#30709 = CARTESIAN_POINT ( 'NONE',  ( 12.39079901834620223, -2.968443430305767627, -12.32999838110541191 ) ) ;
#30710 = CARTESIAN_POINT ( 'NONE',  ( 11.35502763632549872, 2.839566963815999934, 8.035454525731699604 ) ) ;
#30711 = CARTESIAN_POINT ( 'NONE',  ( 10.43325685320999874, -5.596199512734999715, -8.042023143828998855 ) ) ;
#30712 = CARTESIAN_POINT ( 'NONE',  ( 17.60000000000000142, 11.23412379136000006, -3.084957477885999833 ) ) ;
#30713 = CARTESIAN_POINT ( 'NONE',  ( 17.56428618385299956, -12.04952459351999927, 3.198091602616999651 ) ) ;
#30714 = CARTESIAN_POINT ( 'NONE',  ( 13.69992376746900042, 12.26631831379999937, 2.532779022035999805 ) ) ;
#30715 = CARTESIAN_POINT ( 'NONE',  ( 12.60257768741567119, -1.908613650260962080, -13.78119617999061219 ) ) ;
#30716 = CARTESIAN_POINT ( 'NONE',  ( 11.41256651104150066, -3.901000349726440053, -6.501426055769400136 ) ) ;
#30717 = CARTESIAN_POINT ( 'NONE',  ( 10.67500447327519097, 2.650284540010591439, 7.500001951671590561 ) ) ;
#30718 = CARTESIAN_POINT ( 'NONE',  ( 10.84999882987999875, -2.398081733189999864E-14, -12.49999929738252114 ) ) ;
#30719 = EDGE_LOOP ( 'NONE', ( #44813, #33897, #26971, #25623 ) ) ;
#30720 = ORIENTED_EDGE ( 'NONE', *, *, #56712, .F. ) ;
#30721 = LINE ( 'NONE', #57275, #7111 ) ;
#30722 = ADVANCED_FACE ( 'NONE', ( #59249 ), #61375, .T. ) ;
#30723 =( NAMED_UNIT ( * ) SI_UNIT ( $, .STERADIAN. ) SOLID_ANGLE_UNIT ( ) );
#30724 = CARTESIAN_POINT ( 'NONE',  ( 12.09999999999999964, -4.000000000000000000, 7.500000000000000000 ) ) ;
#30725 = CARTESIAN_POINT ( 'NONE',  ( 18.15949994872952900, 2.660112427294489379, 13.63815955491932641 ) ) ;
#30726 = CARTESIAN_POINT ( 'NONE',  ( 9.753031682810998859, 4.922927894835999574, -8.639534507509999628 ) ) ;
#30727 = MANIFOLD_SOLID_BREP ( 'Stock-MAS-678-1', #47056 ) ;
#30728 = CARTESIAN_POINT ( 'NONE',  ( 13.40279821320923581, 11.66091458874561582, 2.117181037223689000 ) ) ;
#30729 = AXIS2_PLACEMENT_3D ( 'NONE', #40350, #4309, #51520 ) ;
#30730 = CARTESIAN_POINT ( 'NONE',  ( 18.12468263438040239, 2.757387671472310675, 12.38786642819432515 ) ) ;
#30731 = CARTESIAN_POINT ( 'NONE',  ( 23.58305315713300132, -13.27270145722000017, 4.268532316603000254 ) ) ;
#30732 = CARTESIAN_POINT ( 'NONE',  ( 11.08992526467999973, 5.210543602612999869, 8.327598319864998544 ) ) ;
#30733 = VERTEX_POINT ( 'NONE', #22798 ) ;
#30734 = CARTESIAN_POINT ( 'NONE',  ( 8.946604883137396769, 4.403857067667214409, -9.229209525869062958 ) ) ;
#30735 = VERTEX_POINT ( 'NONE', #35634 ) ;
#30736 = CARTESIAN_POINT ( 'NONE',  ( 12.37600679962892158, -2.954502784796254833, 12.33399089453511621 ) ) ;
#30737 = CARTESIAN_POINT ( 'NONE',  ( 13.55377458794190382, 8.990344585381031095, 7.716059257659970250 ) ) ;
#30738 = CARTESIAN_POINT ( 'NONE',  ( 11.02445190299000011, 3.404087387974999768, 5.822483872269000216 ) ) ;
#30739 = CARTESIAN_POINT ( 'NONE',  ( 11.22191429142990060, -3.974927396630719922, 8.816028813488999916 ) ) ;
#30740 = CARTESIAN_POINT ( 'NONE',  ( 4.599999999999999645, -1.760845406083394460, 12.47635457398814651 ) ) ;
#30741 = CARTESIAN_POINT ( 'NONE',  ( 10.53521345716899837, 4.924890298941200228, 6.659120737011199331 ) ) ;
#30742 = CARTESIAN_POINT ( 'NONE',  ( 10.91195257254739914, 2.772832764353999835, -7.856899084262298771 ) ) ;
#30743 = CARTESIAN_POINT ( 'NONE',  ( 12.25134400021322456, -0.2899325138666248303, 12.69554708236671914 ) ) ;
#30744 = CARTESIAN_POINT ( 'NONE',  ( 5.687176560462543939, -12.04993902413650453, -3.725892264570328738 ) ) ;
#30745 = CARTESIAN_POINT ( 'NONE',  ( 10.90374609491999891, 3.726846467344000047, 5.900456154266000119 ) ) ;
#30746 = CARTESIAN_POINT ( 'NONE',  ( 9.074999999999999289, -4.417172942406000224, 8.783926296998000538 ) ) ;
#30747 = EDGE_CURVE ( 'NONE', #12746, #34641, #22106, .T. ) ;
#30748 = ORIENTED_EDGE ( 'NONE', *, *, #68903, .T. ) ;
#30749 = CARTESIAN_POINT ( 'NONE',  ( 9.377520280414000098, 4.092867382745001059, -5.937785237406000505 ) ) ;
#30750 = DIRECTION ( 'NONE',  ( 1.000000000000000000, 0.000000000000000000, 0.000000000000000000 ) ) ;
#30751 = CIRCLE ( 'NONE', #25155, 12.52500000000000036 ) ;
#30752 = CARTESIAN_POINT ( 'NONE',  ( 24.45617574031838615, -12.38364418572106018, 3.108063453459867453 ) ) ;
#30753 = CARTESIAN_POINT ( 'NONE',  ( 10.34393020684899867, 2.750000000000000000, 7.500000000000000000 ) ) ;
#30754 = CARTESIAN_POINT ( 'NONE',  ( 12.09999999999999964, -4.817420948848700313, 7.825000000000000178 ) ) ;
#30755 = CARTESIAN_POINT ( 'NONE',  ( 11.43718179236249988, -4.209680326224799707, -6.518682001772900136 ) ) ;
#30756 = ORIENTED_EDGE ( 'NONE', *, *, #27814, .F. ) ;
#30757 = CARTESIAN_POINT ( 'NONE',  ( 1.872883852295999851, 2.591090368091000240, -2.487991068387999771 ) ) ;
#30758 = CARTESIAN_POINT ( 'NONE',  ( 12.80505043854144276, 0.6249999999999994449, 12.67928921589117586 ) ) ;
#30760 = FACE_OUTER_BOUND ( 'NONE', #45417, .T. ) ;
#30759 = CARTESIAN_POINT ( 'NONE',  ( 8.672989158774999652, 4.728328492779000136, -8.692725459657999920 ) ) ;
#30761 = CARTESIAN_POINT ( 'NONE',  ( 5.599999999407000217, -1.300000000000000044, -9.662944685757000940 ) ) ;
#30762 = ORIENTED_EDGE ( 'NONE', *, *, #3851, .T. ) ;
#30763 = LINE ( 'NONE', #4177, #61860 ) ;
#30764 = CARTESIAN_POINT ( 'NONE',  ( 17.93834580300584847, -2.005905130196156350, -13.76587868752633170 ) ) ;
#30765 = CARTESIAN_POINT ( 'NONE',  ( 11.83518044953559922, 4.768048975940600620, 7.099502491684900107 ) ) ;
#30766 = CARTESIAN_POINT ( 'NONE',  ( 11.08757144985999865, -2.712428550139000194, 6.571291218949999902 ) ) ;
#30767 = CARTESIAN_POINT ( 'NONE',  ( 8.143316940379001778, -5.061720701958000390, 5.824087910811999613 ) ) ;
#30768 = ORIENTED_EDGE ( 'NONE', *, *, #58492, .F. ) ;
#30769 = CARTESIAN_POINT ( 'NONE',  ( 8.224926658773000554, 5.629399530851999955, 8.631829656822000985 ) ) ;
#30771 = CARTESIAN_POINT ( 'NONE',  ( 10.57435795695566583, -2.750000000000000000, -7.807440182398264206 ) ) ;
#30770 = CARTESIAN_POINT ( 'NONE',  ( 10.35376078907947495, 4.858294075600578132, -7.665591875800525479 ) ) ;
#30772 = CARTESIAN_POINT ( 'NONE',  ( 7.645452918061504732, -5.358307434801091063, 6.413801445279267988 ) ) ;
#30773 = CARTESIAN_POINT ( 'NONE',  ( 24.30000000000000071, 0.000000000000000000, 0.000000000000000000 ) ) ;
#30774 = CARTESIAN_POINT ( 'NONE',  ( 0.8801993231815000707, 1.717122193005000019, 2.769960469742999809 ) ) ;
#30775 = ORIENTED_EDGE ( 'NONE', *, *, #43758, .F. ) ;
#30776 = CARTESIAN_POINT ( 'NONE',  ( -15.86200481174999943, -13.87069231928999891, -4.225386915259999654 ) ) ;
#30777 = CARTESIAN_POINT ( 'NONE',  ( 12.28179573085659904, -3.026866171144600326, 7.331616337578100051 ) ) ;
#30778 = DIRECTION ( 'NONE',  ( -0.000000000000000000, 1.000000000000000000, 0.000000000000000000 ) ) ;
#30779 = CARTESIAN_POINT ( 'NONE',  ( 10.09181485429000169, 2.440912084162000006, 7.817367409531000177 ) ) ;
#30780 = AXIS2_PLACEMENT_3D ( 'NONE', #16542, #32633, #50431 ) ;
#30781 = CARTESIAN_POINT ( 'NONE',  ( 10.79303032197930001, 4.663532080728800544, 8.427909097977700270 ) ) ;
#30782 = CARTESIAN_POINT ( 'NONE',  ( 8.472124462996665883, -5.100000000000000533, 6.567732269893666874 ) ) ;
#30783 = FACE_OUTER_BOUND ( 'NONE', #33772, .T. ) ;
#30784 = ADVANCED_FACE ( 'NONE', ( #43792 ), #19529, .F. ) ;
#30785 = CARTESIAN_POINT ( 'NONE',  ( 12.20035750765565474, -2.340667166417027989, 12.48730567878010156 ) ) ;
#30786 = EDGE_CURVE ( 'NONE', #54722, #46011, #61809, .T. ) ;
#30787 = CARTESIAN_POINT ( 'NONE',  ( 24.45999011096800047, -3.150047400517000273, -11.96533092960999944 ) ) ;
#30788 = FACE_OUTER_BOUND ( 'NONE', #12593, .T. ) ;
#30789 = CARTESIAN_POINT ( 'NONE',  ( 10.12947109217999930, -5.100000000000000533, 6.152188490330000370 ) ) ;
#30790 = EDGE_LOOP ( 'NONE', ( #28363, #784, #19369, #28846 ) ) ;
#30791 = CARTESIAN_POINT ( 'NONE',  ( 15.75060268747966319, -9.413968701432777308, -8.261605506243164143 ) ) ;
#30792 = CARTESIAN_POINT ( 'NONE',  ( 10.89393020684959978, 2.750000000000000000, -7.500000000000000000 ) ) ;
#30793 = ORIENTED_EDGE ( 'NONE', *, *, #29964, .F. ) ;
#30794 = SURFACE_SIDE_STYLE ('',( #68871 ) ) ;
#30795 = CARTESIAN_POINT ( 'NONE',  ( 11.63825819896753977, 3.148796120250299868, 7.339530235223699073 ) ) ;
#30796 = CARTESIAN_POINT ( 'NONE',  ( 9.662551629919999385, 4.094830335839000135, 9.119946295870999364 ) ) ;
#30797 = CARTESIAN_POINT ( 'NONE',  ( 10.06728116094000036, 4.192860729918999496, -5.985054792427000336 ) ) ;
#30798 = CARTESIAN_POINT ( 'NONE',  ( 9.277558426223626142, -3.641115516887601267, -8.297956262399157623 ) ) ;
#30799 = CARTESIAN_POINT ( 'NONE',  ( 10.18239901426000138, -2.607725299334000102, 7.783410967795999724 ) ) ;
#30800 = CARTESIAN_POINT ( 'NONE',  ( 17.97714073376502242, 0.5849390254007825751, -12.58641711472857594 ) ) ;
#30801 = CARTESIAN_POINT ( 'NONE',  ( 9.010251885924715154, 5.224530136624865762, 8.068208678207518858 ) ) ;
#30802 = CARTESIAN_POINT ( 'NONE',  ( 10.70287750876920008, -4.469200303112399908, -8.228113772635300194 ) ) ;
#30803 = FACE_OUTER_BOUND ( 'NONE', #23546, .T. ) ;
#30804 = ORIENTED_EDGE ( 'NONE', *, *, #2139, .F. ) ;
#30805 = EDGE_CURVE ( 'NONE', #11372, #12398, #17213, .T. ) ;
#30806 = CARTESIAN_POINT ( 'NONE',  ( 11.07074853682000004, -5.433602701969999949, -5.078288957662000058 ) ) ;
#30807 = CARTESIAN_POINT ( 'NONE',  ( 24.90037356005226954, -3.015686408853957889, 11.63997006242029819 ) ) ;
#30808 = DIRECTION ( 'NONE',  ( 0.000000000000000000, -0.9916377111174247139, 0.1290528957048031888 ) ) ;
#30809 = LINE ( 'NONE', #11882, #5750 ) ;
#30810 = B_SPLINE_CURVE_WITH_KNOTS ( 'NONE', 3,
 ( #42705, #52502, #16129, #58775 ),
 .UNSPECIFIED., .F., .F.,
 ( 4, 4 ),
 ( 0.000000000000000000, 1.000000000000000000 ),
 .UNSPECIFIED. ) ;
#30811 = EDGE_CURVE ( 'NONE', #31059, #15974, #30721, .T. ) ;
#30812 = CARTESIAN_POINT ( 'NONE',  ( 17.92061031166184293, 1.858910711595916920, 12.46212218156369111 ) ) ;
#30813 = CARTESIAN_POINT ( 'NONE',  ( 12.35155033006829584, 1.948172666216917648, 13.86379038907994854 ) ) ;
#30814 = CARTESIAN_POINT ( 'NONE',  ( 10.97571094393200042, 2.824289056067999848, 6.306988371318333897 ) ) ;
#30815 = ORIENTED_EDGE ( 'NONE', *, *, #12235, .T. ) ;
#30816 = CARTESIAN_POINT ( 'NONE',  ( 9.227927892482222560, -2.649889402541718120, 7.452433127320587936 ) ) ;
#30817 = DIRECTION ( 'NONE',  ( -0.8987684456439055669, 0.000000000000000000, -0.4384236320214022764 ) ) ;
#30818 = ORIENTED_EDGE ( 'NONE', *, *, #22129, .T. ) ;
#30819 = CARTESIAN_POINT ( 'NONE',  ( 24.46225079000999969, 8.883320982495000351, 9.188387934989000527 ) ) ;
#30820 = CARTESIAN_POINT ( 'NONE',  ( 24.34832160914637456, 12.03537035475460115, -3.224867767164909083 ) ) ;
#30821 = B_SPLINE_CURVE_WITH_KNOTS ( 'NONE', 3,
 ( #48003, #47321, #57799, #32283 ),
 .UNSPECIFIED., .F., .F.,
 ( 4, 4 ),
 ( 0.000000000000000000, 1.000000000000000000 ),
 .UNSPECIFIED. ) ;
#30822 = CARTESIAN_POINT ( 'NONE',  ( 9.476374593785998002, -5.098398394707999159, 6.305533045879999854 ) ) ;
#30823 = CARTESIAN_POINT ( 'NONE',  ( 10.70851354018270207, -3.836375382625528019, -6.250000000000001776 ) ) ;
#30824 = CARTESIAN_POINT ( 'NONE',  ( 12.28594988689359901, -3.606563555963900214, 6.728309553046099012 ) ) ;
#30825 = CONICAL_SURFACE ( 'NONE', #68733, 1.949999999867999767, 0.7853981633972997312 ) ;
#30826 = CIRCLE ( 'NONE', #43097, 1.600000000000000089 ) ;
#30827 = CARTESIAN_POINT ( 'NONE',  ( 24.30000000000000071, -12.03537377768999939, -3.224868684338999980 ) ) ;
#30828 = CARTESIAN_POINT ( 'NONE',  ( 0.3266986677754999957, 3.021985743044000028, 1.081096232840000004 ) ) ;
#30829 = CARTESIAN_POINT ( 'NONE',  ( 10.56498513754060653, -5.349957030113857925, -7.500000808964294663 ) ) ;
#30830 = CARTESIAN_POINT ( 'NONE',  ( 12.11312973616745303, 2.264845417406522898, 12.39478132878350358 ) ) ;
#30831 = DIRECTION ( 'NONE',  ( 0.000000000000000000, -1.000000000000000000, 0.000000000000000000 ) ) ;
#30832 = CARTESIAN_POINT ( 'NONE',  ( 10.72333863405319931, 4.619094858989799768, -8.289729326049599223 ) ) ;
#30833 = CARTESIAN_POINT ( 'NONE',  ( 9.934999999999998721, 4.640430492595999823, -9.117542781427999898 ) ) ;
#30834 = B_SPLINE_CURVE_WITH_KNOTS ( 'NONE', 3,
 ( #22809, #33315, #18270, #65456 ),
 .UNSPECIFIED., .F., .F.,
 ( 4, 4 ),
 ( 0.000000000000000000, 1.000000000000000000 ),
 .UNSPECIFIED. ) ;
#30835 = CARTESIAN_POINT ( 'NONE',  ( 11.12964528040999923, 3.869081149487999749, -9.017143166339000260 ) ) ;
#30836 = CARTESIAN_POINT ( 'NONE',  ( 8.769442991499998286, 3.919472480837189909, -6.223324745230999433 ) ) ;
#30838 = DIRECTION ( 'NONE',  ( 1.000000000000000000, 0.000000000000000000, 0.000000000000000000 ) ) ;
#30837 = CARTESIAN_POINT ( 'NONE',  ( 7.100000000000000533, 4.000000000000000000, -7.500000000000000000 ) ) ;
#30839 = CARTESIAN_POINT ( 'NONE',  ( 8.817462135714999150, 5.100000000000000533, 6.571291218949999902 ) ) ;
#30840 = VERTEX_POINT ( 'NONE', #25128 ) ;
#30841 = CARTESIAN_POINT ( 'NONE',  ( 12.32512882946257626, -0.4004146477438858542, 12.69150435581809688 ) ) ;
#30842 = CARTESIAN_POINT ( 'NONE',  ( 10.34184687351645771, 3.000416447002276943, 8.268183399968647151 ) ) ;
#30843 = CARTESIAN_POINT ( 'NONE',  ( 9.199609130449999839, -2.551382302226000487, 7.536606162076999738 ) ) ;
#30844 = EDGE_CURVE ( 'NONE', #6933, #68711, #59440, .T. ) ;
#30845 = CARTESIAN_POINT ( 'NONE',  ( 10.15958376188599921, 3.268856270222099791, 7.034020612385399218 ) ) ;
#30846 = CARTESIAN_POINT ( 'NONE',  ( 8.796304629759626792, 4.535214477905362251, -8.192154231972200051 ) ) ;
#30847 = FACE_OUTER_BOUND ( 'NONE', #68750, .T. ) ;
#30848 = CARTESIAN_POINT ( 'NONE',  ( 12.61254665343902026, -3.094705746550273862, 13.52917745889216761 ) ) ;
#30849 = CARTESIAN_POINT ( 'NONE',  ( 12.27415370857974253, 2.829964016144990158, 13.59786649615043430 ) ) ;
#30850 = CARTESIAN_POINT ( 'NONE',  ( 8.154557834963361174, 3.119004674881718397, 6.266135323581367267 ) ) ;
#30851 = ORIENTED_EDGE ( 'NONE', *, *, #16746, .F. ) ;
#30852 = CARTESIAN_POINT ( 'NONE',  ( 5.013793765425000437, -0.2272566865862999941, -1.255041691444999996 ) ) ;
#30853 = CARTESIAN_POINT ( 'NONE',  ( 8.845430433046999497, -5.088604610742000212, -6.828193190755800224 ) ) ;
#30854 = CYLINDRICAL_SURFACE ( 'NONE', #5291, 0.5000000000000004441 ) ;
#30855 = CARTESIAN_POINT ( 'NONE',  ( 11.10235971519489873, -3.394698737128500010, 8.506961598696999971 ) ) ;
#30856 = CARTESIAN_POINT ( 'NONE',  ( 17.81516833538380951, 3.068391096118999517, -12.30080513712136003 ) ) ;
#30857 = CARTESIAN_POINT ( 'NONE',  ( 11.04390222146000156, -2.755558049443999735, 5.185384772327999769 ) ) ;
#30858 = AXIS2_PLACEMENT_3D ( 'NONE', #8505, #30865, #29853 ) ;
#30859 = CARTESIAN_POINT ( 'NONE',  ( 17.96892410184997857, 2.968447989616221694, 12.32999203180360581 ) ) ;
#30860 = B_SPLINE_CURVE_WITH_KNOTS ( 'NONE', 3,
 ( #36875, #58191, #10293, #37211 ),
 .UNSPECIFIED., .F., .F.,
 ( 4, 4 ),
 ( 0.000000000000000000, 1.000000000000000000 ),
 .UNSPECIFIED. ) ;
#30861 = CARTESIAN_POINT ( 'NONE',  ( 12.18865263575256641, 2.603587051988978995, -13.65094575294710211 ) ) ;
#30862 = CARTESIAN_POINT ( 'NONE',  ( 10.95934425691999792, -2.844530299042999921, -5.120733195709999741 ) ) ;
#30863 = FACE_OUTER_BOUND ( 'NONE', #17549, .T. ) ;
#30864 = CARTESIAN_POINT ( 'NONE',  ( 9.048601287889788125, 4.000000467705929985, 6.301404677806389465 ) ) ;
#30865 = DIRECTION ( 'NONE',  ( -1.000000000000000000, 0.000000000000000000, 0.000000000000000000 ) ) ;
#30866 = DIRECTION ( 'NONE',  ( 1.000000000000000000, 0.000000000000000000, 0.000000000000000000 ) ) ;
#30867 = EDGE_CURVE ( 'NONE', #56058, #26192, #25469, .T. ) ;
#30868 = DIRECTION ( 'NONE',  ( -1.000000000000000000, 0.000000000000000000, 0.000000000000000000 ) ) ;
#30869 = ADVANCED_FACE ( 'NONE', ( #41551 ), #14979, .T. ) ;
#30870 = CARTESIAN_POINT ( 'NONE',  ( 17.88333207277291592, 1.943312949629576458, 12.56472734206311692 ) ) ;
#30871 = CARTESIAN_POINT ( 'NONE',  ( 9.301695280414000067, 5.619431609641999614, -8.115423117607999615 ) ) ;
#30872 = CARTESIAN_POINT ( 'NONE',  ( 6.742149978683131373, 1.067472389103388153, -1.089157552026253306 ) ) ;
#30873 = ORIENTED_EDGE ( 'NONE', *, *, #50235, .T. ) ;
#30874 = CIRCLE ( 'NONE', #24132, 1.999999999999999556 ) ;
#30875 = EDGE_CURVE ( 'NONE', #35032, #53691, #30263, .T. ) ;
#30876 = CARTESIAN_POINT ( 'NONE',  ( 7.974113208588001100, 4.561154361229000642, -6.272154006859000930 ) ) ;
#30877 = CARTESIAN_POINT ( 'NONE',  ( 18.24299778933909622, 2.286486205740245303, -13.81204233372297985 ) ) ;
#30878 = ORIENTED_EDGE ( 'NONE', *, *, #55793, .F. ) ;
#30879 = CARTESIAN_POINT ( 'NONE',  ( 10.54193802597399987, -4.450760089576400347, 8.240623579255899500 ) ) ;
#30880 = CARTESIAN_POINT ( 'NONE',  ( 11.72433327354039889, 3.016779570871600313, 8.143111181492699302 ) ) ;
#30881 = DIRECTION ( 'NONE',  ( 1.000000000000000000, 0.000000000000000000, 0.000000000000000000 ) ) ;
#30882 = CARTESIAN_POINT ( 'NONE',  ( 8.517351160491482887, -5.205057563154263711, 8.206039936683175995 ) ) ;
#30883 = DIRECTION ( 'NONE',  ( -0.000000000000000000, -0.000000000000000000, 1.000000000000000000 ) ) ;
#30884 = DIRECTION ( 'NONE',  ( 1.000000000000000000, 0.000000000000000000, 0.000000000000000000 ) ) ;
#30885 = CARTESIAN_POINT ( 'NONE',  ( 4.950859839683333874, -0.3926218265389256890, 1.460959015002472050 ) ) ;
#30886 = ORIENTED_EDGE ( 'NONE', *, *, #4951, .T. ) ;
#30887 = CARTESIAN_POINT ( 'NONE',  ( 13.73837349797500096, 9.670565172354999461, 8.019813433522999802 ) ) ;
#30888 = CARTESIAN_POINT ( 'NONE',  ( 8.441604719589999917, 5.473983809665999622, -8.180077404516000072 ) ) ;
#30889 = ORIENTED_EDGE ( 'NONE', *, *, #17841, .F. ) ;
#30890 = CARTESIAN_POINT ( 'NONE',  ( 10.70780830849999887, 5.157484706885999692, -6.267808298721999627 ) ) ;
#30891 =( LENGTH_UNIT ( ) NAMED_UNIT ( * ) SI_UNIT ( .MILLI., .METRE. ) );
#30892 = ORIENTED_EDGE ( 'NONE', *, *, #2910, .T. ) ;
#30893 = CARTESIAN_POINT ( 'NONE',  ( 9.377342523874999003, 2.735516931877000513, 7.693563834190999984 ) ) ;
#30894 = CARTESIAN_POINT ( 'NONE',  ( 17.74512657133773175, -3.174942931788179212, -12.19343219266723466 ) ) ;
#30895 = ADVANCED_FACE ( 'NONE', ( #44019 ), #21577, .F. ) ;
#30896 = DIRECTION ( 'NONE',  ( 0.000000000000000000, 0.8897496663238059211, -0.4564488265695026969 ) ) ;
#30897 = CARTESIAN_POINT ( 'NONE',  ( 10.36409408021999923, -4.600000090830000943, -4.954046131267999087 ) ) ;
#30898 = DIRECTION ( 'NONE',  ( -8.953281780977936028E-11, 0.7455324205424948003, 0.6664693615763958023 ) ) ;
#30899 = ORIENTED_EDGE ( 'NONE', *, *, #46031, .F. ) ;
#30900 = LINE ( 'NONE', #10942, #26977 ) ;
#30901 = CARTESIAN_POINT ( 'NONE',  ( 8.699680597014879169, 3.656951845173556315, -5.776565596854453588 ) ) ;
#30902 = DIRECTION ( 'NONE',  ( -1.000000000000000000, 0.000000000000000000, 0.000000000000000000 ) ) ;
#30903 = DIRECTION ( 'NONE',  ( 1.000000000000000000, 0.000000000000000000, 3.219646771391999928E-14 ) ) ;
#30904 = CIRCLE ( 'NONE', #65474, 2.149999999999999911 ) ;
#30905 = CARTESIAN_POINT ( 'NONE',  ( 17.87597250029675067, 0.6552116771452413113, 13.98466387211990458 ) ) ;
#30906 = CARTESIAN_POINT ( 'NONE',  ( 17.79518154839200150, 3.190852234727000081, 11.45040960482999814 ) ) ;
#30907 = CARTESIAN_POINT ( 'NONE',  ( 10.33022766388000058, -2.650179121646999647, -7.694581537458001108 ) ) ;
#30908 = ORIENTED_EDGE ( 'NONE', *, *, #43836, .T. ) ;
#30909 = ORIENTED_EDGE ( 'NONE', *, *, #16863, .T. ) ;
#30910 = CARTESIAN_POINT ( 'NONE',  ( 9.874770280412001000, 4.038835765825999680, -5.935509327774999733 ) ) ;
#30911 = CIRCLE ( 'NONE', #55471, 13.17499999999999538 ) ;
#30912 = CARTESIAN_POINT ( 'NONE',  ( 11.53144126044203688, 11.54570453903531480, 1.556370816894309783 ) ) ;
#30913 = B_SPLINE_CURVE_WITH_KNOTS ( 'NONE', 3,
 ( #20328, #16114, #379, #37439 ),
 .UNSPECIFIED., .F., .F.,
 ( 4, 4 ),
 ( 0.1836163425310829433, 1.000000000000000000 ),
 .UNSPECIFIED. ) ;
#30914 = LINE ( 'NONE', #4666, #41344 ) ;
#30915 = CARTESIAN_POINT ( 'NONE',  ( 24.17809239055575077, 3.317955234501958728, 12.42377263001247201 ) ) ;
#30916 = CARTESIAN_POINT ( 'NONE',  ( 10.84657802013509986, 2.684088780794000151, -7.469366283838649423 ) ) ;
#30917 = CARTESIAN_POINT ( 'NONE',  ( 10.19391290906799874, 3.451408805716100314, -8.171383386399000415 ) ) ;
#30919 = CARTESIAN_POINT ( 'NONE',  ( 8.701589129073576956, 5.750364994161538235, 7.524138884631350166 ) ) ;
#30918 = CARTESIAN_POINT ( 'NONE',  ( 9.397151519676999243, -3.975306837623020062, 6.358456126310000123 ) ) ;
#30920 = LINE ( 'NONE', #26363, #34163 ) ;
#30921 = ORIENTED_EDGE ( 'NONE', *, *, #67828, .T. ) ;
#30922 = AXIS2_PLACEMENT_3D ( 'NONE', #30504, #29226, #34475 ) ;
#30923 = CARTESIAN_POINT ( 'NONE',  ( 10.13706886426420084, 2.899999999999999911, 6.444141223280826836 ) ) ;
#30924 = CARTESIAN_POINT ( 'NONE',  ( 7.736994134724001881, -2.836597362165000913, 6.822571831264003350 ) ) ;
#30925 = EDGE_CURVE ( 'NONE', #63702, #57137, #9255, .T. ) ;
#30926 = EDGE_CURVE ( 'NONE', #34621, #55729, #15243, .T. ) ;
#30927 = CARTESIAN_POINT ( 'NONE',  ( 9.785684229509998389, 3.098260518542999886, 8.407331414124799451 ) ) ;
#30928 = CARTESIAN_POINT ( 'NONE',  ( 7.951755279714369351, 4.908718838353461678, 6.393521497924140817 ) ) ;
#30929 = CONICAL_SURFACE ( 'NONE', #15305, 2.100041432634999428, 0.7853981633972997312 ) ;
#30930 = DIRECTION ( 'NONE',  ( 1.000000000000000000, 0.000000000000000000, 0.000000000000000000 ) ) ;
#30931 = CARTESIAN_POINT ( 'NONE',  ( 17.96886609968823834, 2.968499926956509327, -12.32999726799525142 ) ) ;
#30932 = CARTESIAN_POINT ( 'NONE',  ( 10.05882936267886940, 4.704418606475568865, 8.703716202581716743 ) ) ;
#30933 = CARTESIAN_POINT ( 'NONE',  ( 13.64649313145500109, 9.010717346174999420, 7.468773375841999851 ) ) ;
#30934 = CARTESIAN_POINT ( 'NONE',  ( -0.2999999999999999889, -1.154700538379000108, 0.000000000000000000 ) ) ;
#30935 = CARTESIAN_POINT ( 'NONE',  ( 11.07101354018312378, -3.231816600031356845, 6.500416447002274722 ) ) ;
#30936 = CARTESIAN_POINT ( 'NONE',  ( 25.26996942120215905, -3.169757571932660944, 11.48332646995987005 ) ) ;
#30937 = CARTESIAN_POINT ( 'NONE',  ( 18.20346453088224692, 2.853274009421435498, 12.27345743254588228 ) ) ;
#30938 = CARTESIAN_POINT ( 'NONE',  ( 2.633427925697999772, -1.603367949813999882, -2.837339924868000463 ) ) ;
#30939 = ORIENTED_EDGE ( 'NONE', *, *, #36751, .F. ) ;
#30940 = CARTESIAN_POINT ( 'NONE',  ( 12.23548902587310039, 0.2575478136180237021, -12.69649014468030757 ) ) ;
#30941 = CARTESIAN_POINT ( 'NONE',  ( 12.19849796477692649, -2.650903665370842432, -12.41512439159400216 ) ) ;
#30942 = CARTESIAN_POINT ( 'NONE',  ( 12.40000000000000213, 11.60847947989999973, 1.809983899806999919 ) ) ;
#30943 = CARTESIAN_POINT ( 'NONE',  ( 3.499564475844618272, 0.6826263220198214299, -3.360566866257050922 ) ) ;
#30944 = CARTESIAN_POINT ( 'NONE',  ( 9.152739834416941278, -2.899999737737819050, -6.597244613339529273 ) ) ;
#30945 = ORIENTED_EDGE ( 'NONE', *, *, #13105, .T. ) ;
#30946 = DIRECTION ( 'NONE',  ( 0.000000000000000000, 1.000000000000000000, 0.000000000000000000 ) ) ;
#30947 = DIRECTION ( 'NONE',  ( 0.000000000000000000, 0.000000000000000000, 1.000000000000000000 ) ) ;
#30948 = EDGE_CURVE ( 'NONE', #21776, #20897, #18255, .T. ) ;
#30949 = CARTESIAN_POINT ( 'NONE',  ( 17.96364285780273207, 0.4729642818460892961, 12.68814481171623321 ) ) ;
#30950 = CARTESIAN_POINT ( 'NONE',  ( 11.10000000011999965, -5.340540540232000311, -6.721892642141000351 ) ) ;
#30951 = CARTESIAN_POINT ( 'NONE',  ( 10.24733997687999931, 4.272363749081500295, 8.748653021963999521 ) ) ;
#30952 = CARTESIAN_POINT ( 'NONE',  ( 11.47500581613029880, 4.988618570924500339, -8.134817373646898275 ) ) ;
#30953 = ORIENTED_EDGE ( 'NONE', *, *, #20481, .F. ) ;
#30954 = AXIS2_PLACEMENT_3D ( 'NONE', #18277, #60922, #17586 ) ;
#30955 = ADVANCED_FACE ( 'NONE', ( #67639 ), #30596, .T. ) ;
#30956 = CARTESIAN_POINT ( 'NONE',  ( 11.20563089100999932, -3.509133048232999652, 6.118191305996999674 ) ) ;
#30957 = ORIENTED_EDGE ( 'NONE', *, *, #68504, .T. ) ;
#30958 = DIRECTION ( 'NONE',  ( 0.000000000000000000, 1.000000000000000000, 0.000000000000000000 ) ) ;
#30959 = CARTESIAN_POINT ( 'NONE',  ( 8.919605646795000453, -5.165500668528999917, 8.645534272955000432 ) ) ;
#30960 = STYLED_ITEM ( 'NONE', ( #20392 ), #46039 ) ;
#30961 = CARTESIAN_POINT ( 'NONE',  ( 9.050000000000000711, 7.679126935408000065, 5.093340497782000043 ) ) ;
#30962 = ORIENTED_EDGE ( 'NONE', *, *, #29465, .T. ) ;
#30963 = DIRECTION ( 'NONE',  ( 0.000000000000000000, 0.2098314828218890149, -0.9777375664342490280 ) ) ;
#30964 = LINE ( 'NONE', #62757, #41652 ) ;
#30965 = CARTESIAN_POINT ( 'NONE',  ( 7.871145280405000833, 4.569394889178999719, -9.136182695123999054 ) ) ;
#30966 = VECTOR ( 'NONE', #54898, 1000.000000000000114 ) ;
#30967 = DIRECTION ( 'NONE',  ( 0.000000000000000000, -0.5000000000000169864, -0.8660254037844288266 ) ) ;
#30968 = CARTESIAN_POINT ( 'NONE',  ( 17.71828964457739986, -3.103661179288114802, 12.29022416951141139 ) ) ;
#30969 = EDGE_LOOP ( 'NONE', ( #17360, #40098, #15572, #62101, #47444 ) ) ;
#30970 = DIRECTION ( 'NONE',  ( 0.000000000000000000, 1.000000000000000000, 0.000000000000000000 ) ) ;
#30971 = B_SPLINE_CURVE_WITH_KNOTS ( 'NONE', 3,
 ( #49838, #21877, #12089, #60672 ),
 .UNSPECIFIED., .F., .F.,
 ( 4, 4 ),
 ( 0.000000000000000000, 1.000000000000000000 ),
 .UNSPECIFIED. ) ;
#30972 = CARTESIAN_POINT ( 'NONE',  ( 12.26374059925572446, -2.812587983977303363, -13.60212386632697346 ) ) ;
#30973 = DIRECTION ( 'NONE',  ( -1.000000000000000000, 2.479407037994000336E-10, -2.337936169761000217E-09 ) ) ;
#30974 = VERTEX_POINT ( 'NONE', #35167 ) ;
#30975 = CARTESIAN_POINT ( 'NONE',  ( 10.76232069631999977, -3.259150589222000072, -8.644998763029001054 ) ) ;
#30976 = AXIS2_PLACEMENT_3D ( 'NONE', #59044, #31794, #60082 ) ;
#30977 = CARTESIAN_POINT ( 'NONE',  ( 8.972537864292000620, 2.899999999999999911, -6.571291218949999902 ) ) ;
#30978 = ORIENTED_EDGE ( 'NONE', *, *, #8362, .T. ) ;
#30979 = CARTESIAN_POINT ( 'NONE',  ( 4.855026506350000659, 1.500000000000000000, 0.000000000000000000 ) ) ;
#30980 = CARTESIAN_POINT ( 'NONE',  ( 17.63676827340842479, 0.6210358159842679360, -13.88132258802015251 ) ) ;
#30981 = CARTESIAN_POINT ( 'NONE',  ( 11.37077408945316925, 2.816736291912564472, -7.913130250469239790 ) ) ;
#30982 = EDGE_CURVE ( 'NONE', #19317, #64156, #57311, .T. ) ;
#30983 = CARTESIAN_POINT ( 'NONE',  ( 8.753040873196827221, 3.779878465243081465, -5.822439910017921605 ) ) ;
#30984 = DIRECTION ( 'NONE',  ( 0.000000000000000000, 0.9999606858717338120, -0.008867170401640298016 ) ) ;
#30985 = DIRECTION ( 'NONE',  ( -1.000000000000000000, 0.000000000000000000, 0.000000000000000000 ) ) ;
#30986 = AXIS2_PLACEMENT_3D ( 'NONE', #41467, #51943, #45687 ) ;
#30987 = CARTESIAN_POINT ( 'NONE',  ( 9.477263540182331525, -4.629523725463626782, -8.592232985442821658 ) ) ;
#30988 = DIRECTION ( 'NONE',  ( 0.000000000000000000, 0.000000000000000000, -1.000000000000000000 ) ) ;
#30989 = ORIENTED_EDGE ( 'NONE', *, *, #52271, .T. ) ;
#30990 = CARTESIAN_POINT ( 'NONE',  ( 10.65413259636999932, -4.783377755405500587, -7.926858177843299380 ) ) ;
#30991 = ORIENTED_EDGE ( 'NONE', *, *, #33706, .F. ) ;
#30992 = CARTESIAN_POINT ( 'NONE',  ( 10.57224177473000104, 4.020426023752999178, 8.920668579831000145 ) ) ;
#30993 = CARTESIAN_POINT ( 'NONE',  ( 9.074999999999999289, 4.417172942406000224, 8.783926296998000538 ) ) ;
#30994 = CARTESIAN_POINT ( 'NONE',  ( 12.48958479105534458, 1.960066648180104565, -13.77326086059893839 ) ) ;
#30995 = CARTESIAN_POINT ( 'NONE',  ( 3.264420700083999982, -1.874241925158999900, -3.007514872430000263 ) ) ;
#30996 = CARTESIAN_POINT ( 'NONE',  ( 8.881891561744774677, -3.585076488109216974, -6.197760796822787910 ) ) ;
#30997 = CARTESIAN_POINT ( 'NONE',  ( 9.236413463905998711, -3.915843685459630574, 6.617590440947399344 ) ) ;
#30998 = CARTESIAN_POINT ( 'NONE',  ( 13.70003001321900449, -11.73562684670656431, -4.491863874615365404 ) ) ;
#30999 = B_SPLINE_CURVE_WITH_KNOTS ( 'NONE', 3,
 ( #14003, #8752, #23453, #51057, #30094, #55958, #18560, #44790, #19586, #34989, #24830, #67123, #51398, #61544 ),
 .UNSPECIFIED., .F., .F.,
 ( 4, 2, 2, 2, 2, 2, 4 ),
 ( 0.000000000000000000, 0.1250000000000024702, 0.2500000000000049405, 0.5000000000000068834, 0.6250000000000041078, 0.7500000000000013323, 1.000000000000000000 ),
 .UNSPECIFIED. ) ;
#31000 = ORIENTED_EDGE ( 'NONE', *, *, #26522, .F. ) ;
#31001 = CARTESIAN_POINT ( 'NONE',  ( 10.65303300763299887, -3.212834858289399964, 6.674373427955200277 ) ) ;
#31002 = CARTESIAN_POINT ( 'NONE',  ( 3.228056799210624384, -2.150913519912213800, 2.798833948393621540 ) ) ;
#31003 = FACE_OUTER_BOUND ( 'NONE', #51356, .T. ) ;
#31004 = LINE ( 'NONE', #40793, #56718 ) ;
#31006 = CARTESIAN_POINT ( 'NONE',  ( 12.08083412505891907, 2.710618184153621435, -13.73644169170462703 ) ) ;
#31005 = CARTESIAN_POINT ( 'NONE',  ( 9.261662452849000360, 2.944259351255000379, 6.507396354981000108 ) ) ;
#31007 = CARTESIAN_POINT ( 'NONE',  ( 11.01872200990539952, 3.052519557825900343, -7.169497859994799605 ) ) ;
#31008 = CONICAL_SURFACE ( 'NONE', #20917, 2.649999808707999893, 0.7853980705567794596 ) ;
#31009 = FACE_OUTER_BOUND ( 'NONE', #3354, .T. ) ;
#31010 =( GEOMETRIC_REPRESENTATION_CONTEXT ( 3 ) GLOBAL_UNCERTAINTY_ASSIGNED_CONTEXT ( ( #26202 ) ) GLOBAL_UNIT_ASSIGNED_CONTEXT ( ( #53159, #38103, #37763 ) ) REPRESENTATION_CONTEXT ( 'NONE', 'WORKASPACE' ) );
#31011 = CARTESIAN_POINT ( 'NONE',  ( 9.095759580228998331, 3.156743194445300382, -7.298441312785299395 ) ) ;
#31012 = EDGE_CURVE ( 'NONE', #6055, #57932, #17440, .T. ) ;
#31013 = ADVANCED_FACE ( 'NONE', ( #24322 ), #53961, .F. ) ;
#31014 = CARTESIAN_POINT ( 'NONE',  ( 17.93858415168864440, 0.6105138165311991827, 12.58520200551375545 ) ) ;
#31015 = CARTESIAN_POINT ( 'NONE',  ( 6.994449685151000295, 1.257374890127000100, -0.2000319440639999891 ) ) ;
#31016 = CARTESIAN_POINT ( 'NONE',  ( 11.30367835872029936, 2.886444435522000251, 8.201822467543799178 ) ) ;
#31017 = AXIS2_PLACEMENT_3D ( 'NONE', #58950, #11057, #64520 ) ;
#31018 = CARTESIAN_POINT ( 'NONE',  ( 0.2554390818521176665, 0.8426791852790889159, -3.173196348029862612 ) ) ;
#31019 = ORIENTED_EDGE ( 'NONE', *, *, #17345, .T. ) ;
#31020 = CARTESIAN_POINT ( 'NONE',  ( 7.293870559621999483, -3.416208448044999901, 6.162501393933999871 ) ) ;
#31021 = EDGE_CURVE ( 'NONE', #41105, #8285, #36109, .T. ) ;
#31022 = DIRECTION ( 'NONE',  ( 0.000000000000000000, 0.9659258262890757507, -0.2588190451024934835 ) ) ;
#31023 = CARTESIAN_POINT ( 'NONE',  ( 5.000030787343000327, -2.099962892530999881, 0.000000000000000000 ) ) ;
#31024 = ORIENTED_EDGE ( 'NONE', *, *, #3302, .F. ) ;
#31025 = VECTOR ( 'NONE', #2149, 1000.000000000000114 ) ;
#31026 = CARTESIAN_POINT ( 'NONE',  ( 0.3210591298330999765, 2.092960143115000005, 2.433246087927000367 ) ) ;
#31027 = CARTESIAN_POINT ( 'NONE',  ( 11.10101463001529964, 4.622233839778099984, 8.496586578655598743 ) ) ;
#31028 = CARTESIAN_POINT ( 'NONE',  ( 10.81187971959000116, 4.614148948243999904, -5.930135044105000475 ) ) ;
#31029 = ORIENTED_EDGE ( 'NONE', *, *, #24805, .T. ) ;
#31030 = CARTESIAN_POINT ( 'NONE',  ( 5.107109839683333874, -1.199500263597270244, -0.9218200799623728070 ) ) ;
#31031 = CONICAL_SURFACE ( 'NONE', #25481, 13.04999999969999891, 0.7853981633972997312 ) ;
#31032 = DIRECTION ( 'NONE',  ( -0.000000000000000000, -0.000000000000000000, 1.000000000000000000 ) ) ;
#31033 = CARTESIAN_POINT ( 'NONE',  ( 10.69041504065829962, 5.024558373595999328, 8.263934892306599167 ) ) ;
#31034 = PLANE ( 'NONE',  #65628 ) ;
#31035 = CARTESIAN_POINT ( 'NONE',  ( 9.341490007895000502, 4.148133901461999784, 9.337478696773001019 ) ) ;
#31036 = VERTEX_POINT ( 'NONE', #22674 ) ;
#31037 = CARTESIAN_POINT ( 'NONE',  ( 11.59999999999999964, 2.500145227336000087, -7.825000000000000178 ) ) ;
#31038 = CARTESIAN_POINT ( 'NONE',  ( 15.52913652543167267, 8.833284221180715434, 7.896593172538426408 ) ) ;
#31039 = CARTESIAN_POINT ( 'NONE',  ( 8.126493406597699476, -5.052135485929927228, 6.114372266853107085 ) ) ;
#31040 = CARTESIAN_POINT ( 'NONE',  ( 10.00398825978600037, -4.167373623506299474, 6.231784538167999266 ) ) ;
#31041 = VERTEX_POINT ( 'NONE', #8583 ) ;
#31042 = CARTESIAN_POINT ( 'NONE',  ( 10.35160840458000031, -4.633672799139000098, -4.861358447487999612 ) ) ;
#31043 = CARTESIAN_POINT ( 'NONE',  ( 11.28887616594230003, -4.386455737425299262, 8.718182393403999697 ) ) ;
#31044 = VERTEX_POINT ( 'NONE', #14523 ) ;
#31045 = CARTESIAN_POINT ( 'NONE',  ( 11.00008140503725329, 5.084125838812211917, -7.367730262387956586 ) ) ;
#31046 = CARTESIAN_POINT ( 'NONE',  ( 24.30000000000000071, 11.77655473258999841, -4.190794510628000680 ) ) ;
#31047 = ORIENTED_EDGE ( 'NONE', *, *, #65040, .T. ) ;
#31048 = CARTESIAN_POINT ( 'NONE',  ( 10.18225119159999892, -4.505165106450999879, -8.732017808253001334 ) ) ;
#31049 = CARTESIAN_POINT ( 'NONE',  ( 8.646410841231000788, 2.261390688294000029, -6.733978371730000134 ) ) ;
#31050 = CARTESIAN_POINT ( 'NONE',  ( 11.01790547754519878, 5.174295865741999734, -7.537269019642879542 ) ) ;
#31051 = CARTESIAN_POINT ( 'NONE',  ( 11.60101463001529964, -3.377766160221900016, 8.496586578655598743 ) ) ;
#31052 = CARTESIAN_POINT ( 'NONE',  ( 24.30001683613300045, -12.21047198529999989, -3.271805531187999883 ) ) ;
#31053 = CARTESIAN_POINT ( 'NONE',  ( 11.29303032197930001, -3.336467919271199900, 8.427909097977700270 ) ) ;
#31054 = CARTESIAN_POINT ( 'NONE',  ( 8.116920280410999666, 5.773189794777000117, 7.141495931231999883 ) ) ;
#31055 = EDGE_LOOP ( 'NONE', ( #53750, #9956, #20473, #35444, #43186, #53225, #56437, #37910, #50164, #17813 ) ) ;
#31056 = DIRECTION ( 'NONE',  ( 0.000000000000000000, -0.2483836997597965168, 0.9686617251102859205 ) ) ;
#31057 = CARTESIAN_POINT ( 'NONE',  ( 9.342519353207999089, -5.057079407184000175, 8.967634647348999621 ) ) ;
#31058 = CARTESIAN_POINT ( 'NONE',  ( 9.979346873516126593, 4.163624617374466652, 6.249999999999999112 ) ) ;
#31059 = VERTEX_POINT ( 'NONE', #2988 ) ;
#31060 = CARTESIAN_POINT ( 'NONE',  ( 12.26287255281689248, -2.811570894161415257, -12.37351047967075779 ) ) ;
#31061 = EDGE_CURVE ( 'NONE', #63987, #46963, #60192, .T. ) ;
#31062 = VECTOR ( 'NONE', #57322, 1000.000000000000000 ) ;
#31063 = CARTESIAN_POINT ( 'NONE',  ( 18.49586274151939236, 2.771911498364446391, 11.31551287271585160 ) ) ;
#31064 = CARTESIAN_POINT ( 'NONE',  ( 18.48724299199999876, -3.206939682244000167, -12.14698705996000072 ) ) ;
#31065 = CARTESIAN_POINT ( 'NONE',  ( 10.87309687351627652, 2.782534154164606921, 7.827184855449101697 ) ) ;
#31066 = CARTESIAN_POINT ( 'NONE',  ( 12.34634080959765079, -2.074995934380768681, -13.75442486551247789 ) ) ;
#31067 = EDGE_CURVE ( 'NONE', #60364, #22975, #54016, .T. ) ;
#31068 = VECTOR ( 'NONE', #44168, 1000.000000000000000 ) ;
#31069 = CARTESIAN_POINT ( 'NONE',  ( 11.28949010443639978, -2.999324937259999935, -7.574834962826040297 ) ) ;
#31070 = CARTESIAN_POINT ( 'NONE',  ( 18.49997192701553317, 2.999031289807200906, 12.16100995559787812 ) ) ;
#31071 = CARTESIAN_POINT ( 'NONE',  ( 18.24702988622819788, -2.264821834935305311, 12.39478563874201633 ) ) ;
#31072 = EDGE_LOOP ( 'NONE', ( #20421, #63091, #30274, #13200, #42873, #57944, #10405, #50487, #51425, #19491, #31311, #27865, #1078, #34729, #54283, #56129, #4957, #49459, #58270, #25979, #51449, #49787, #14533 ) ) ;
#31073 = ORIENTED_EDGE ( 'NONE', *, *, #25089, .F. ) ;
#31074 = CARTESIAN_POINT ( 'NONE',  ( 12.80505043854144098, -0.7302158263239267866, -13.98094363220830871 ) ) ;
#31075 = AXIS2_PLACEMENT_3D ( 'NONE', #38155, #43766, #11938 ) ;
#31076 = CARTESIAN_POINT ( 'NONE',  ( 10.90000658885999840, -1.199999999999999956, 9.776630298829998011 ) ) ;
#31077 = CARTESIAN_POINT ( 'NONE',  ( 4.900006121742000786, 2.000000000000000888, 0.2617993877991453555 ) ) ;
#31078 = CARTESIAN_POINT ( 'NONE',  ( 11.08752642792000032, 2.871528932589999972, -6.302908019754999813 ) ) ;
#31079 = MANIFOLD_SOLID_BREP ( 'Stock-MAS-678-1', #25837 ) ;
#31080 = CARTESIAN_POINT ( 'NONE',  ( 8.616995677562000466, 4.876077402042000131, 5.996974966532000018 ) ) ;
#31081 = CARTESIAN_POINT ( 'NONE',  ( 18.08671436482205763, 2.829189290800525391, 12.36876367364217089 ) ) ;
#31082 = CARTESIAN_POINT ( 'NONE',  ( 24.32786205753600228, -12.60040638205000008, 3.143984624925999949 ) ) ;
#31083 = CARTESIAN_POINT ( 'NONE',  ( 9.696080515601000371, 2.554416243104999928, 7.600685069647000525 ) ) ;
#31084 = CIRCLE ( 'NONE', #34438, 14.00000000000000000 ) ;
#31085 = ORIENTED_EDGE ( 'NONE', *, *, #19091, .T. ) ;
#31086 = CARTESIAN_POINT ( 'NONE',  ( 8.661263445375622538, -4.848494725308105657, -6.449848855944013692 ) ) ;
#31087 = ORIENTED_EDGE ( 'NONE', *, *, #65898, .T. ) ;
#31088 = CARTESIAN_POINT ( 'NONE',  ( 12.23131043852900035, -2.748092942712452746, 12.39032383288960126 ) ) ;
#31089 = CARTESIAN_POINT ( 'NONE',  ( 9.728988259786000015, -4.113440707072600233, -8.359557531806398600 ) ) ;
#31090 = CARTESIAN_POINT ( 'NONE',  ( 10.55813337864000090, 2.466561068647000532, 6.633529813744000414 ) ) ;
#31091 = CARTESIAN_POINT ( 'NONE',  ( 11.34657802013509986, -5.315911219205999849, 7.530633716161349689 ) ) ;
#31092 = B_SPLINE_CURVE_WITH_KNOTS ( 'NONE', 3,
 ( #65087, #65445, #21758, #7066, #1480, #11966, #32612, #64397, #48685, #16518, #65789, #33302, #6717, #32952, #22797, #54966, #64745, #33995 ),
 .UNSPECIFIED., .F., .F.,
 ( 4, 2, 2, 2, 2, 2, 2, 2, 4 ),
 ( 0.000000000000000000, 0.06250000000000212330, 0.1250000000000042466, 0.2500000000000045519, 0.5000000000000019984, 0.7499999999999994449, 0.8749999999999998890, 0.9375000000000000000, 1.000000000000000000 ),
 .UNSPECIFIED. ) ;
#31093 = LINE ( 'NONE', #30740, #39496 ) ;
#31094 = DIRECTION ( 'NONE',  ( 0.000000000000000000, -1.000000000000000000, 0.000000000000000000 ) ) ;
#31095 = CARTESIAN_POINT ( 'NONE',  ( 10.49349279008999858, 3.667611644732699627, -8.734031750754999379 ) ) ;
#31096 = CARTESIAN_POINT ( 'NONE',  ( 12.37753504985973763, -0.4560270868711872594, 12.68898073362800005 ) ) ;
#31097 = CARTESIAN_POINT ( 'NONE',  ( 11.59999999999999964, 3.707964997157290110, -8.536357045506706598 ) ) ;
#31098 = EDGE_CURVE ( 'NONE', #50848, #52040, #30763, .T. ) ;
#31099 = CARTESIAN_POINT ( 'NONE',  ( 9.882259685352000389, 4.932708901218999742, 6.390989635557000170 ) ) ;
#31100 = CARTESIAN_POINT ( 'NONE',  ( 9.218545854265867590, -2.654504660436530994, 7.609872343353834445 ) ) ;
#31101 = VERTEX_POINT ( 'NONE', #3158 ) ;
#31102 = CARTESIAN_POINT ( 'NONE',  ( 9.079170280414000871, 4.815598936798999752, -8.835641302565999666 ) ) ;
#31103 = CARTESIAN_POINT ( 'NONE',  ( 7.360029764120000095, 0.6822332425488999430, 1.321254113936999985 ) ) ;
#31104 = EDGE_CURVE ( 'NONE', #65237, #39410, #16835, .T. ) ;
#31105 = EDGE_CURVE ( 'NONE', #58276, #68518, #54359, .T. ) ;
#31106 = CARTESIAN_POINT ( 'NONE',  ( 17.77733961940312213, 1.915504334253006036, 13.78014422891542345 ) ) ;
#31107 = CARTESIAN_POINT ( 'NONE',  ( 9.261037412837582750, 3.646685539694229039, -8.850715144363563880 ) ) ;
#31108 = CARTESIAN_POINT ( 'NONE',  ( 12.10000000000000142, -3.409519984105202184, 8.459313701734298974 ) ) ;
#31109 = CARTESIAN_POINT ( 'NONE',  ( 11.26072066707849828, -3.023932655881500065, -6.909591111168198907 ) ) ;
#31110 = ORIENTED_EDGE ( 'NONE', *, *, #58868, .T. ) ;
#31111 = CARTESIAN_POINT ( 'NONE',  ( 10.10478570706233370, -2.868293641868291388, -8.113400509224881318 ) ) ;
#31112 = CARTESIAN_POINT ( 'NONE',  ( 7.950760841228999176, 2.095715612964000218, 8.056490963156001328 ) ) ;
#31113 = AXIS2_PLACEMENT_3D ( 'NONE', #62776, #38190, #30988 ) ;
#31116 = UNCERTAINTY_MEASURE_WITH_UNIT (LENGTH_MEASURE( 1.000000000000000082E-05 ), #41969, 'distance_accuracy_value', 'NONE');
#31115 = CARTESIAN_POINT ( 'NONE',  ( 13.64647714749800045, -9.589793698018000967, -7.972185502806999224 ) ) ;
#31114 = CARTESIAN_POINT ( 'NONE',  ( 10.01279489264886458, 2.761698732461363104, 6.264380212190736152 ) ) ;
#31117 = DIRECTION ( 'NONE',  ( 0.000000000000000000, -1.000000000000000000, 0.000000000000000000 ) ) ;
#31118 = VERTEX_POINT ( 'NONE', #36347 ) ;
#31119 = CARTESIAN_POINT ( 'NONE',  ( 9.532678149083000818, 4.663044775770000427, 8.669813205957000335 ) ) ;
#31120 = CARTESIAN_POINT ( 'NONE',  ( 17.98492955360213230, -2.046199355803459241, -13.75924933913552550 ) ) ;
#31121 = CARTESIAN_POINT ( 'NONE',  ( 10.94903032197929882, 4.503839166471300004, 8.204588308639600314 ) ) ;
#31122 = CARTESIAN_POINT ( 'NONE',  ( 24.56711857111956832, -11.92025347580062800, 3.200166735598448664 ) ) ;
#31123 = CARTESIAN_POINT ( 'NONE',  ( 7.769581853207999877, -2.431397064767999439, 7.958394431095000776 ) ) ;
#31124 = ORIENTED_EDGE ( 'NONE', *, *, #58477, .F. ) ;
#31125 = CARTESIAN_POINT ( 'NONE',  ( 8.930989158774000458, 2.019067547072999957, 7.390982789861999969 ) ) ;
#31126 = ADVANCED_FACE ( 'NONE', ( #46843 ), #52073, .T. ) ;
#31128 = CARTESIAN_POINT ( 'NONE',  ( 10.02314899745999988, 5.167567567567999731, -6.822293592207000934 ) ) ;
#31127 = CARTESIAN_POINT ( 'NONE',  ( 11.06623059009866061, 3.312237475846870893, -6.964041498692941090 ) ) ;
#31129 = CARTESIAN_POINT ( 'NONE',  ( 7.645048706201956534, -5.352880121026291071, 6.407055433046042303 ) ) ;
#31130 = VECTOR ( 'NONE', #29787, 1000.000000000000000 ) ;
#31131 = CARTESIAN_POINT ( 'NONE',  ( 18.08681467610534810, -0.3285836819713975343, 13.89477675118381406 ) ) ;
#31132 = CARTESIAN_POINT ( 'NONE',  ( 23.86947959890900250, 3.656851216063000010, 13.22922481556000029 ) ) ;
#31133 = ORIENTED_EDGE ( 'NONE', *, *, #23124, .F. ) ;
#31134 = CARTESIAN_POINT ( 'NONE',  ( 11.79999999684100054, 3.345264396959000130, -11.86064773189999855 ) ) ;
#31135 = CARTESIAN_POINT ( 'NONE',  ( 11.61718313518939993, -4.622449961306399402, 6.712912394634500401 ) ) ;
#31136 = CARTESIAN_POINT ( 'NONE',  ( 9.781673028307999118, 5.464749740720999505, 8.817329433105999925 ) ) ;
#31137 = CARTESIAN_POINT ( 'NONE',  ( 6.953052440528999512, -9.233022020364000326, -5.200634764108000851 ) ) ;
#31138 = CARTESIAN_POINT ( 'NONE',  ( 10.66995391537419913, 4.943675741382899780, 6.859089544950699668 ) ) ;
#31139 = EDGE_LOOP ( 'NONE', ( #61234, #53453, #20928, #12122, #1979, #32427 ) ) ;
#31140 = CIRCLE ( 'NONE', #69041, 1.000000000000000000 ) ;
#31141 = B_SPLINE_CURVE_WITH_KNOTS ( 'NONE', 3,
 ( #48989, #28022, #60178, #5984, #65754, #32571, #32913, #17165, #749, #54226 ),
 .UNSPECIFIED., .F., .F.,
 ( 4, 2, 2, 2, 4 ),
 ( 0.000000000000000000, 0.1249999999280923674, 0.2499999998561847347, 0.3749999997842771160, 0.4999999997123694695 ),
 .UNSPECIFIED. ) ;
#31142 = CARTESIAN_POINT ( 'NONE',  ( 23.96071373372425839, -3.344686053530380399, 12.82063560515832812 ) ) ;
#31143 = CARTESIAN_POINT ( 'NONE',  ( 12.10343314470978804, 2.298052811141196194, -12.38866778002552849 ) ) ;
#31144 = CARTESIAN_POINT ( 'NONE',  ( 11.25158531382730054, 4.272452942476326676, -6.250000000000000000 ) ) ;
#31145 = CARTESIAN_POINT ( 'NONE',  ( 25.37703408795700355, -2.612353912486999885, -11.31741720513000082 ) ) ;
#31146 = AXIS2_PLACEMENT_3D ( 'NONE', #42588, #5176, #53077 ) ;
#31147 = CARTESIAN_POINT ( 'NONE',  ( 17.81256277267588217, -1.835326726223547089, 13.87917840078988263 ) ) ;
#31148 = CARTESIAN_POINT ( 'NONE',  ( 18.12459608109056575, 2.757432806191179253, -13.61548201701641858 ) ) ;
#31149 = ORIENTED_EDGE ( 'NONE', *, *, #54528, .T. ) ;
#31150 = DIRECTION ( 'NONE',  ( -1.000000000000000000, 0.000000000000000000, 0.000000000000000000 ) ) ;
#31151 = CARTESIAN_POINT ( 'NONE',  ( 9.181310023244000362, -3.426978632899654542, -6.377665258770703005 ) ) ;
#31152 = ORIENTED_EDGE ( 'NONE', *, *, #38831, .T. ) ;
#31153 = CARTESIAN_POINT ( 'NONE',  ( 10.98768553379999879, -5.299329486732999861, 4.945210549701000602 ) ) ;
#31154 = CARTESIAN_POINT ( 'NONE',  ( 11.02287616594229824, 3.738072157442200005, 8.325646653015098764 ) ) ;
#31155 = CARTESIAN_POINT ( 'NONE',  ( 9.228133567168001150, 2.875367362387999837, 8.669940206484001877 ) ) ;
#31156 = CARTESIAN_POINT ( 'NONE',  ( 9.961465797930001642, 2.787126709928999801, -8.677707706574000923 ) ) ;
#31157 = CARTESIAN_POINT ( 'NONE',  ( 9.657495633957626779, -4.774169056067385952, -7.907669647568630111 ) ) ;
#31158 = CARTESIAN_POINT ( 'NONE',  ( 11.20563089100999932, -3.509133048232999652, 6.118191305996999674 ) ) ;
#31159 = CARTESIAN_POINT ( 'NONE',  ( 18.20534100106117847, 0.3182341284860654151, -12.59598505207571328 ) ) ;
#31160 = ADVANCED_FACE ( 'NONE', ( #41593 ), #18300, .T. ) ;
#31161 = CARTESIAN_POINT ( 'NONE',  ( 9.044058817429487362, 4.875265736440850262, 8.528255781230162924 ) ) ;
#31162 = CARTESIAN_POINT ( 'NONE',  ( 10.32949413291699869, -3.087070836781100169, -7.083453279150199400 ) ) ;
#31163 = CARTESIAN_POINT ( 'NONE',  ( 5.500000000000000000, -1.315736040608999957, 10.71955403322999878 ) ) ;
#31164 = ORIENTED_EDGE ( 'NONE', *, *, #48377, .F. ) ;
#31165 = CARTESIAN_POINT ( 'NONE',  ( 24.56710006383056211, -3.188707335874072957, 11.92334242227752483 ) ) ;
#31166 = CARTESIAN_POINT ( 'NONE',  ( 24.44496488009700030, 8.810487470433001178, 8.810507756548000557 ) ) ;
#31167 = CARTESIAN_POINT ( 'NONE',  ( 29.60000000000000142, 0.000000000000000000, -9.250000000000000000 ) ) ;
#31168 = CARTESIAN_POINT ( 'NONE',  ( 17.79030838958606964, 1.799800542995206643, 12.47079474911150143 ) ) ;
#31169 = CARTESIAN_POINT ( 'NONE',  ( 12.51441652845167596, 3.187012454917759641, 13.63242365153888791 ) ) ;
#31170 = CARTESIAN_POINT ( 'NONE',  ( 10.74600376124999990, -5.242711034443999552, 8.978690688221998784 ) ) ;
#31171 = VECTOR ( 'NONE', #59291, 1000.000000000000114 ) ;
#31172 = CARTESIAN_POINT ( 'NONE',  ( 12.49508659849326264, -0.5431048944669121248, -12.68437082641160529 ) ) ;
#31173 = CARTESIAN_POINT ( 'NONE',  ( 12.10478902330476991, -0.1895042076700523548, 13.99872220539657164 ) ) ;
#31174 = VERTEX_POINT ( 'NONE', #41250 ) ;
#31175 = CARTESIAN_POINT ( 'NONE',  ( 12.78084734971790581, -1.760846085845585218, 12.47635444213890743 ) ) ;
#31176 = CARTESIAN_POINT ( 'NONE',  ( 10.34091290906799898, -4.722468360609500593, -8.384179803770500428 ) ) ;
#31177 = LINE ( 'NONE', #1071, #58265 ) ;
#31178 = CARTESIAN_POINT ( 'NONE',  ( 10.09697182628999990, -5.253379538902000156, 8.530665717066000298 ) ) ;
#31179 = CARTESIAN_POINT ( 'NONE',  ( 10.80226354018299872, -5.092232985442821658, -6.870476274536374994 ) ) ;
#31180 = CARTESIAN_POINT ( 'NONE',  ( 12.31056516821460001, -3.390321848206700128, 6.884701936848800052 ) ) ;
#31181 = CARTESIAN_POINT ( 'NONE',  ( 12.23732871802943656, 0.4475098806653827199, 12.59205372277267898 ) ) ;
#31182 = FACE_OUTER_BOUND ( 'NONE', #40843, .T. ) ;
#31183 = CARTESIAN_POINT ( 'NONE',  ( 4.598427295411807059, 1.165904589046791173, 0.2775696827697649582 ) ) ;
#31184 = CARTESIAN_POINT ( 'NONE',  ( 12.54683914358772867, 1.807964460291305642, 12.46961431371563478 ) ) ;
#31185 = CARTESIAN_POINT ( 'NONE',  ( 10.71685100253999856, -2.832432432432000269, 6.822293592207000934 ) ) ;
#31186 = CARTESIAN_POINT ( 'NONE',  ( 10.20641772631199906, 4.431553727090300043, -8.388315195900499788 ) ) ;
#31187 = CARTESIAN_POINT ( 'NONE',  ( 12.01640417260608729, 11.69872868927256349, -4.475294149993699122 ) ) ;
#31188 = EDGE_CURVE ( 'NONE', #45386, #63789, #29378, .T. ) ;
#31189 = CARTESIAN_POINT ( 'NONE',  ( 10.22907665877000127, 4.838498214728000235, -5.852435699035000383 ) ) ;
#31190 = CARTESIAN_POINT ( 'NONE',  ( 9.149380199233998923, 5.269225938816000543, -7.340469740450900282 ) ) ;
#31192 = CARTESIAN_POINT ( 'NONE',  ( 12.19254223316779218, 2.624341221351141229, 12.42172529681850435 ) ) ;
#31191 = CARTESIAN_POINT ( 'NONE',  ( 17.55505043854147118, -1.875000000000000000, 12.57545641911172396 ) ) ;
#31193 = B_SPLINE_CURVE_WITH_KNOTS ( 'NONE', 3,
 ( #46022, #19797, #4391, #19105, #25379, #61753 ),
 .UNSPECIFIED., .F., .F.,
 ( 4, 2, 4 ),
 ( 0.000000000000000000, 0.5000000000000000000, 1.000000000000000000 ),
 .UNSPECIFIED. ) ;
#31194 = DIRECTION ( 'NONE',  ( 2.186536431443105034E-10, 0.8764392776392420092, 0.4815124013057229813 ) ) ;
#31195 = ORIENTED_EDGE ( 'NONE', *, *, #2485, .F. ) ;
#31196 = CARTESIAN_POINT ( 'NONE',  ( 12.61465226496487979, -0.5953800884222990586, 12.68120857324682937 ) ) ;
#31197 = CARTESIAN_POINT ( 'NONE',  ( 10.28976354018291239, 3.672815144550904076, 8.717465845835395299 ) ) ;
#31198 = CARTESIAN_POINT ( 'NONE',  ( 10.31668414895000119, -3.819528725844000494, 6.062183754159999438 ) ) ;
#31199 = CARTESIAN_POINT ( 'NONE',  ( 9.450367640780999778, 4.408706755790200660, 8.264635032075899446 ) ) ;
#31200 = CYLINDRICAL_SURFACE ( 'NONE', #33259, 1.999999999999999556 ) ;
#31201 = CARTESIAN_POINT ( 'NONE',  ( 12.24277986057918888, -2.226901448799674998, 13.72760233995392731 ) ) ;
#31202 = CARTESIAN_POINT ( 'NONE',  ( 12.19240574131726618, 2.623658934113291874, 13.64640170894116267 ) ) ;
#31203 = DIRECTION ( 'NONE',  ( 1.000000000000000000, 0.000000000000000000, 0.000000000000000000 ) ) ;
#31204 = ORIENTED_EDGE ( 'NONE', *, *, #64544, .T. ) ;
#31205 = EDGE_CURVE ( 'NONE', #252, #36754, #1872, .T. ) ;
#31206 = CARTESIAN_POINT ( 'NONE',  ( 4.250643903098000109, -0.6845482139417999878, 0.9045979078395999240 ) ) ;
#31207 = CARTESIAN_POINT ( 'NONE',  ( 8.997405316140000053, -4.271593136661399726, -8.750048621292000561 ) ) ;
#31208 = DIRECTION ( 'NONE',  ( 0.000000000000000000, -1.000000000000000000, 0.000000000000000000 ) ) ;
#31209 = CARTESIAN_POINT ( 'NONE',  ( 11.98522412107029922, -3.952868550833580130, 8.390877922225699947 ) ) ;
#31210 = EDGE_CURVE ( 'NONE', #11416, #68324, #26008, .T. ) ;
#31211 = CARTESIAN_POINT ( 'NONE',  ( 17.93748940951487114, 2.994360127459124943, -12.32254798267195994 ) ) ;
#31212 = CARTESIAN_POINT ( 'NONE',  ( 9.823602683899249399, -5.219044746006709978, 7.819247029363189050 ) ) ;
#31213 = CARTESIAN_POINT ( 'NONE',  ( 8.710288521113000115, -4.352953559891299840, -8.284550957747498501 ) ) ;
#31214 = CARTESIAN_POINT ( 'NONE',  ( 7.895830451470996714, 3.177662910779999628, 6.240430379278997464 ) ) ;
#31215 = CARTESIAN_POINT ( 'NONE',  ( 11.04413069183000040, -2.755289458307000228, -5.175229826689999868 ) ) ;
#31216 = CARTESIAN_POINT ( 'NONE',  ( 24.37847037357300195, 12.00848431662999971, 3.275550077227999957 ) ) ;
#31217 = CARTESIAN_POINT ( 'NONE',  ( 9.007644528443009335, -4.705791426005293765, 8.704816259181081151 ) ) ;
#31218 = CARTESIAN_POINT ( 'NONE',  ( 12.10797096423120678, 0.2010519787742809927, -13.99856097495847607 ) ) ;
#31219 = CARTESIAN_POINT ( 'NONE',  ( 11.34393020684979980, -5.250000000000000000, 7.500000000000000000 ) ) ;
#31220 = CARTESIAN_POINT ( 'NONE',  ( 11.10000000031000056, 8.466679424687001188, 6.746294355622000083 ) ) ;
#31221 = CARTESIAN_POINT ( 'NONE',  ( 2.800973465877999669, -3.500000000000000000, 0.000000000000000000 ) ) ;
#31222 = ORIENTED_EDGE ( 'NONE', *, *, #49083, .T. ) ;
#31223 = CARTESIAN_POINT ( 'NONE',  ( 9.202245280414000916, 5.095038542659000136, -6.157541456184000062 ) ) ;
#31224 = CARTESIAN_POINT ( 'NONE',  ( 11.59672200990539892, -4.817867935977999672, 7.785290430335599865 ) ) ;
#31225 = EDGE_LOOP ( 'NONE', ( #43247, #7643, #63200, #60817 ) ) ;
#31226 = DIRECTION ( 'NONE',  ( 1.000000000000000000, 0.000000000000000000, 0.000000000000000000 ) ) ;
#31227 = CARTESIAN_POINT ( 'NONE',  ( 18.10291081608025010, 2.039210736883923403, -13.85070288166277841 ) ) ;
#31228 = ORIENTED_EDGE ( 'NONE', *, *, #27615, .T. ) ;
#31229 = CARTESIAN_POINT ( 'NONE',  ( 11.35034208742529849, 3.369365911179700301, 6.508707709313799050 ) ) ;
#31230 = FACE_OUTER_BOUND ( 'NONE', #30105, .T. ) ;
#31231 = CARTESIAN_POINT ( 'NONE',  ( 9.989493109327902687, 3.453294174495602054, -9.227563350567775657 ) ) ;
#31232 = CARTESIAN_POINT ( 'NONE',  ( 10.37199293566600034, -3.366612813978900220, -8.276990458557699881 ) ) ;
#31233 = CARTESIAN_POINT ( 'NONE',  ( 12.19590749974583943, 0.1412517844600120476, -13.89905214520220333 ) ) ;
#31234 = DIRECTION ( 'NONE',  ( -2.820458616744058146E-07, 2.816894698951058879E-07, -0.9999999999999205080 ) ) ;
#31235 = CARTESIAN_POINT ( 'NONE',  ( 11.09999999999999964, 6.351820664109999903, 5.386194068259000822 ) ) ;
#31236 = ORIENTED_EDGE ( 'NONE', *, *, #17808, .F. ) ;
#31237 = CARTESIAN_POINT ( 'NONE',  ( 13.73854177342199989, 9.465667024606000624, 8.118361260918998568 ) ) ;
#31238 = CARTESIAN_POINT ( 'NONE',  ( 9.228345280414000484, 2.481540185810000132, -7.878707153279001396 ) ) ;
#31239 = ORIENTED_EDGE ( 'NONE', *, *, #46884, .T. ) ;
#31240 = VECTOR ( 'NONE', #50892, 1000.000000000000227 ) ;
#31241 = CARTESIAN_POINT ( 'NONE',  ( 9.961465797930001642, 2.787126709928999801, -8.677707706574000923 ) ) ;
#31242 = VERTEX_POINT ( 'NONE', #36003 ) ;
#31243 = CARTESIAN_POINT ( 'NONE',  ( 8.490822372493999737, 3.632306086542600010, 6.297150255604999636 ) ) ;
#31244 = CARTESIAN_POINT ( 'NONE',  ( 18.02785359611327465, -2.090732611440656807, -12.53755739145392845 ) ) ;
#31245 = CARTESIAN_POINT ( 'NONE',  ( 3.999999173945999686, 0.000000000000000000, 0.000000000000000000 ) ) ;
#31246 = DIRECTION ( 'NONE',  ( 0.000000000000000000, 1.000000000000000000, 0.000000000000000000 ) ) ;
#31247 = CARTESIAN_POINT ( 'NONE',  ( 8.564263637668691587, 2.982766295838745307, 6.174911310893544503 ) ) ;
#31248 = EDGE_LOOP ( 'NONE', ( #40615, #64550, #61465 ) ) ;
#31249 = CARTESIAN_POINT ( 'NONE',  ( 12.20391894010300149, 11.86124369401000145, -3.532130569927999897 ) ) ;
#31250 = CARTESIAN_POINT ( 'NONE',  ( 17.56043522961499903, 11.55259058373999892, -4.939852154758999525 ) ) ;
#31251 = CARTESIAN_POINT ( 'NONE',  ( 8.164556123749317607, -2.650750344902491840, 7.676799495579008870 ) ) ;
#31252 = CARTESIAN_POINT ( 'NONE',  ( 11.09999999999999964, 4.000000000000000000, 7.500000000000000000 ) ) ;
#31253 = CARTESIAN_POINT ( 'NONE',  ( 12.45488131765416284, -11.84188428343376032, 3.380847681380453551 ) ) ;
#31254 = CARTESIAN_POINT ( 'NONE',  ( 18.04310822451204999, 12.08952385220933756, -3.274024637468825993 ) ) ;
#31255 = CARTESIAN_POINT ( 'NONE',  ( 10.10656447933000024, -4.887648864398999926, -6.257283015674000026 ) ) ;
#31256 = EDGE_LOOP ( 'NONE', ( #30945, #57013, #43234, #7510 ) ) ;
#31257 = ORIENTED_EDGE ( 'NONE', *, *, #31932, .F. ) ;
#31258 = CARTESIAN_POINT ( 'NONE',  ( 8.880270280412998929, 4.146787477634999775, -5.941926545671999627 ) ) ;
#31259 = CARTESIAN_POINT ( 'NONE',  ( 11.72006719377404593, 11.52583591983466071, 1.696350940370162652 ) ) ;
#31260 = CARTESIAN_POINT ( 'NONE',  ( 12.30953092759835243, -2.881442378557633077, 13.58513712698411524 ) ) ;
#31261 = CARTESIAN_POINT ( 'NONE',  ( 23.79452334243675438, 3.298030808557463445, 13.14157935970629687 ) ) ;
#31262 = EDGE_CURVE ( 'NONE', #13611, #7244, #3754, .T. ) ;
#31263 = ADVANCED_FACE ( 'NONE', ( #9420 ), #8918, .F. ) ;
#31264 = CARTESIAN_POINT ( 'NONE',  ( 24.67921321731900264, -3.567517257907000250, -12.13750614118000115 ) ) ;
#31265 = CARTESIAN_POINT ( 'NONE',  ( 9.586013376692998023, 3.227076647348800176, -7.107192877568799361 ) ) ;
#31267 = CARTESIAN_POINT ( 'NONE',  ( 8.903314993461870941, 2.546304713195970848, 8.472542641376174188 ) ) ;
#31266 = CARTESIAN_POINT ( 'NONE',  ( 10.25632996542199926, -4.697624103824200148, 6.777391592843399870 ) ) ;
#31268 = DIRECTION ( 'NONE',  ( 0.000000000000000000, 0.000000000000000000, -1.000000000000000000 ) ) ;
#31269 = ORIENTED_EDGE ( 'NONE', *, *, #53449, .T. ) ;
#31270 = CARTESIAN_POINT ( 'NONE',  ( 9.748096873515667227, 4.327184855449106138, -6.282534154164607365 ) ) ;
#31271 = CARTESIAN_POINT ( 'NONE',  ( 7.909525359152002721, -3.174976509417001491, 6.234240719816002141 ) ) ;
#31272 = DIRECTION ( 'NONE',  ( 0.000000000000000000, 0.000000000000000000, 1.000000000000000000 ) ) ;
#31273 = DIRECTION ( 'NONE',  ( 0.000000000000000000, -0.007439385635797960035, -0.9999723273877941798 ) ) ;
#31274 = CARTESIAN_POINT ( 'NONE',  ( 10.43579701286999928, -2.587605342384000195, 6.390039770907999461 ) ) ;
#31275 = CARTESIAN_POINT ( 'NONE',  ( 18.08697361606112253, 2.828309738171238319, -12.36901404291605289 ) ) ;
#31276 = CARTESIAN_POINT ( 'NONE',  ( 15.95266668291200141, -3.685671355860000276, -11.20570641515999988 ) ) ;
#31277 = CARTESIAN_POINT ( 'NONE',  ( 15.88771848669684061, -8.938332686943013528, -8.488529254939264135 ) ) ;
#31278 = AXIS2_PLACEMENT_3D ( 'NONE', #19181, #18849, #34243 ) ;
#31279 = CARTESIAN_POINT ( 'NONE',  ( 7.993989691196518699, 3.116233090823458340, -6.353578959360522305 ) ) ;
#31280 = CARTESIAN_POINT ( 'NONE',  ( 9.864633995697998259, -3.138280386550500012, -7.595641268826199166 ) ) ;
#31281 = CARTESIAN_POINT ( 'NONE',  ( 6.714945356252000508, -0.05887414910050999678, 1.174638368522000098 ) ) ;
#31282 = B_SPLINE_SURFACE_WITH_KNOTS ( 'NONE', 3, 3, ( 
 ( #49691, #12291, #59477, #44468, #60185, #44116, #10900, #27331, #59829, #28030, #5646, #48996, #32246, #11934, #32577, #65055, #59137, #26988, #54233, #49337, #48304, #11577, #53889, #39204, #33619, #65413, #17535, #33273, #5991, #54938, #22767, #6333, #22069, #1798, #410, #21725, #37816, #28375, #6685, #23116, #43419, #54590, #16487, #64714, #27682, #11240, #16827, #1452, #7040, #38864, #17885, #48654, #1108, #65762, #38151, #22420, #17173, #43761, #38505, #18576, #19249, #39551, #45490, #46174, #8082, #67138, #66805 ),
 ( #61560, #40577, #13676, #51074, #55634, #29424, #39903, #18917, #8426, #3509, #60875, #67482, #24506, #28725, #19605, #29076, #66109, #18226, #33965, #24847, #12990, #60526, #35005, #61904, #61222, #51414, #56321, #29768, #40242, #3177, #13338, #45827, #34313, #55288, #14020, #30111, #12635, #7383, #66455, #50041, #2150, #23468, #35347, #56663, #8769, #44805, #7733, #23811, #50386, #2486, #45144, #34662, #55975, #50732, #2826, #24156, #47896, #63614, #4197, #47480, #68856, #20977, #9789, #41956, #20285, #15040, #9104 ),
 ( #41613, #20631, #53135, #40924, #10139, #46520, #30442, #62247, #36718, #51753, #42312, #35688, #15730, #52441, #31815, #63263, #10474, #3847, #25186, #67825, #41268, #19947, #47206, #58039, #62582, #14364, #14703, #5234, #37058, #47555, #36021, #57002, #52789, #58372, #25534, #57336, #62920, #9438, #30781, #52092, #36367, #46862, #57679, #31138, #26572, #68165, #4883, #4536, #25872, #68508, #15391, #26225, #31470, #54507, #32845, #17092, #32165, #43337, #64641, #59064, #53478, #44030, #10821, #17453, #59402, #22342, #49259 ),
 ( #38075, #682, #29246, #11501, #63953, #5572, #11851, #5913, #26913, #16063, #16407, #6606, #64290, #38424, #48228, #39728, #21649, #48922, #1369, #54157, #65334, #16748, #1030, #6257, #27596, #48577, #61045, #334, #27948, #42983, #58718, #37393, #43681, #64978, #22686, #50556, #21992, #13166, #37738, #34495, #11165, #59749, #33189, #55807, #32500, #7908, #21313, #42643, #53815, #27254, #36188, #14184, #35172, #9261, #3338, #51576, #14865, #30951, #41093, #8248, #40079, #23984, #67644, #61388, #51917, #66626, #46689 ) ),
 .UNSPECIFIED., .F., .F., .F.,
 ( 4, 4 ),
 ( 4, 1, 1, 1, 1, 1, 1, 1, 1, 1, 1, 1, 1, 1, 1, 1, 1, 1, 1, 1, 1, 1, 1, 1, 1, 1, 1, 1, 1, 1, 1, 1, 1, 1, 1, 1, 1, 1, 1, 1, 1, 1, 1, 1, 1, 1, 1, 1, 1, 1, 1, 1, 1, 1, 1, 1, 1, 1, 1, 1, 1, 1, 1, 1, 4 ),
 ( -0.02000000000000000042, 1.020000000000000018 ),
 ( 0.008747244164287000176, 0.02453926110774999961, 0.04033127805120999970, 0.05612329499467000327, 0.07191531193812999989, 0.08770732888158999652, 0.1034993458251000087, 0.1192913627684999978, 0.1350833797120000179, 0.1508753966553999792, 0.1666674135988999994, 0.1824594305423999918, 0.1982514474858000086, 0.2140434644293000011, 0.2298354813727000179, 0.2456274983162000103, 0.2614195152596999749, 0.2772115322030999640, 0.2930035491465999842, 0.3087955660900000288, 0.3245875830334999934, 0.3403795999769999581, 0.3561716169204000026, 0.3719636338639000228, 0.3877556508073999875, 0.4035476677507999765, 0.4193396846942999967, 0.4351317016376999858, 0.4509237185811999504, 0.4667157355247000261, 0.4825077524681000152, 0.4982997694115999798, 0.5140917863550000799, 0.5298838032985000446, 0.5456758202420000092, 0.5614678371854000538, 0.5772598541289000185, 0.5930518710723000630, 0.6088438880158000277, 0.6246359049592999924, 0.6404279219027000369, 0.6562199388462000016, 0.6720119557896999662, 0.6878039727331000108, 0.7035959896765999755, 0.7193880066200000201, 0.7351800235634999847, 0.7509720405069999494, 0.7667640574504001050, 0.7825560743939000696, 0.7983480913373000032, 0.8141401082808000789, 0.8299321252243000435, 0.8457241421676999771, 0.8615161591112000528, 0.8773081760545999863, 0.8931001929981000620, 0.9088922099416000266, 0.9246842268849999602, 0.9404762438285000359, 0.9562682607720000005, 0.9720602777153999341, 0.9878522946589000098, 1.003644311601999961, 1.019436328545999970 ),
 .UNSPECIFIED. ) ;
#31283 = ADVANCED_FACE ( 'NONE', ( #24054 ), #54838, .F. ) ;
#31284 = CARTESIAN_POINT ( 'NONE',  ( 17.55505043854144276, -0.6250000000000001110, 12.67928921589117586 ) ) ;
#31285 = CARTESIAN_POINT ( 'NONE',  ( 5.579147251786431561, 12.92151814336059168, -2.574492155646014968 ) ) ;
#31286 = CARTESIAN_POINT ( 'NONE',  ( 2.204290380730999921, 1.127589919772999938, -2.855189883873000323 ) ) ;
#31287 = ORIENTED_EDGE ( 'NONE', *, *, #16863, .F. ) ;
#31288 = CARTESIAN_POINT ( 'NONE',  ( 12.24445512745668374, -0.2765170649790825719, -12.69595318831094666 ) ) ;
#31289 = CARTESIAN_POINT ( 'NONE',  ( 12.32868821303769735, -2.904730879140380750, -12.34800599561816092 ) ) ;
#31290 = DIRECTION ( 'NONE',  ( 1.000000000000000000, 0.000000000000000000, 0.000000000000000000 ) ) ;
#31291 = CARTESIAN_POINT ( 'NONE',  ( 3.499604618624656105, -0.6504880270822478439, -3.309912210867942850 ) ) ;
#31292 = CARTESIAN_POINT ( 'NONE',  ( 4.500000125099000492, 1.829647544581999737E-13, -12.99999867215000116 ) ) ;
#31293 = VERTEX_POINT ( 'NONE', #23015 ) ;
#31294 = DIRECTION ( 'NONE',  ( 0.8480635683783770418, 0.000000000000000000, 0.5298945026977860406 ) ) ;
#31295 = DIRECTION ( 'NONE',  ( 0.000000000000000000, 0.000000000000000000, 1.000000000000000000 ) ) ;
#31296 = CARTESIAN_POINT ( 'NONE',  ( 17.77478288641002635, 0.5854877332479576646, 12.68183053513773473 ) ) ;
#31297 = CARTESIAN_POINT ( 'NONE',  ( 13.19211270977099915, -11.64284154253999937, -1.888701237101999997 ) ) ;
#31298 = CARTESIAN_POINT ( 'NONE',  ( 7.735197674916334698, 3.263818714402415111, -8.649421172292802495 ) ) ;
#31299 = CARTESIAN_POINT ( 'NONE',  ( 12.96900185986900134, 12.22197440418000092, 1.955830866674999946 ) ) ;
#31300 = ORIENTED_EDGE ( 'NONE', *, *, #69048, .F. ) ;
#31301 = CARTESIAN_POINT ( 'NONE',  ( 10.63462194421999918, -5.668721490782999695, 6.527259573254000635 ) ) ;
#31302 = ORIENTED_EDGE ( 'NONE', *, *, #17719, .F. ) ;
#31303 = CARTESIAN_POINT ( 'NONE',  ( 12.06493925477931661, -2.826469659297512482, 7.051164236119339179 ) ) ;
#31304 = CARTESIAN_POINT ( 'NONE',  ( 7.283516392955999841, -4.426925773067000414, 9.293310812901001583 ) ) ;
#31305 = CARTESIAN_POINT ( 'NONE',  ( 7.399999923048000028, 0.000000000000000000, 0.000000000000000000 ) ) ;
#31306 = VERTEX_POINT ( 'NONE', #14936 ) ;
#31307 = CARTESIAN_POINT ( 'NONE',  ( 8.265163602278375876, 3.125207522424720885, -6.192262357212721113 ) ) ;
#31308 = CARTESIAN_POINT ( 'NONE',  ( 8.078904719588999583, 4.421485762723999180, -5.992852494763999616 ) ) ;
#31309 = CARTESIAN_POINT ( 'NONE',  ( 9.510596873516666605, -3.370476274536376771, -8.592232985442825210 ) ) ;
#31310 = CARTESIAN_POINT ( 'NONE',  ( 18.09742839077966892, -2.810734143419357345, 12.37374591515774291 ) ) ;
#31311 = ORIENTED_EDGE ( 'NONE', *, *, #5306, .T. ) ;
#31312 = CARTESIAN_POINT ( 'NONE',  ( 9.442841440870999747, -2.691258483914000355, 6.269525829285999663 ) ) ;
#31313 = CARTESIAN_POINT ( 'NONE',  ( 25.47133129397800033, 11.11904401118000152, -3.299919292445999908 ) ) ;
#31314 = CARTESIAN_POINT ( 'NONE',  ( 12.17504389532245845, 11.54180247361012412, -4.316564347524264988 ) ) ;
#31315 = ORIENTED_EDGE ( 'NONE', *, *, #11260, .T. ) ;
#31316 = DIRECTION ( 'NONE',  ( 1.000000000000000000, 0.000000000000000000, 0.000000000000000000 ) ) ;
#31317 = VERTEX_POINT ( 'NONE', #8999 ) ;
#31318 = CARTESIAN_POINT ( 'NONE',  ( 23.56677800383048194, -10.34876416779365726, 9.413867714140970122 ) ) ;
#31319 = CARTESIAN_POINT ( 'NONE',  ( 23.94495438039136559, 12.80028382019095368, -3.529837795375663667 ) ) ;
#31320 = CARTESIAN_POINT ( 'NONE',  ( 11.46550210169813511, 3.941925478257526372, -8.807012707104282967 ) ) ;
#31321 = CARTESIAN_POINT ( 'NONE',  ( 5.250859839683916341, 0.3926218265389220807, -1.460959015002473382 ) ) ;
#31322 = EDGE_CURVE ( 'NONE', #7217, #11254, #18601, .T. ) ;
#31323 = CARTESIAN_POINT ( 'NONE',  ( 4.599999999999999645, 3.199751711897561801, -12.18694338143115452 ) ) ;
#31324 = CARTESIAN_POINT ( 'NONE',  ( 23.91319602772269093, 12.85058282302694899, 3.562133635490558614 ) ) ;
#31325 = EDGE_CURVE ( 'NONE', #42427, #27101, #41171, .T. ) ;
#31326 = CARTESIAN_POINT ( 'NONE',  ( 12.60230703261658114, 3.091556739796027742, 13.52998185037902701 ) ) ;
#31327 = CARTESIAN_POINT ( 'NONE',  ( 11.01776264201000011, -4.914128622650000722, 8.587713430305999651 ) ) ;
#31328 = ORIENTED_EDGE ( 'NONE', *, *, #49164, .T. ) ;
#31329 = CARTESIAN_POINT ( 'NONE',  ( 10.82035090130999855, -3.241273085157000189, -7.969278253227299658 ) ) ;
#31330 = ORIENTED_EDGE ( 'NONE', *, *, #19592, .F. ) ;
#31331 = CARTESIAN_POINT ( 'NONE',  ( 11.18706938844999854, 3.186790175674999670, 6.232702730851999995 ) ) ;
#31332 = AXIS2_PLACEMENT_3D ( 'NONE', #17072, #315, #21974 ) ;
#31333 = CARTESIAN_POINT ( 'NONE',  ( 11.30671024775549149, -3.379344054882541304, -8.119376818724932221 ) ) ;
#31334 = CARTESIAN_POINT ( 'NONE',  ( 8.821685841230998193, 2.633142096252999664, -7.791134854666999843 ) ) ;
#31335 = CARTESIAN_POINT ( 'NONE',  ( 24.53428991268900106, -12.47024905405999995, -3.026245386525999947 ) ) ;
#31336 = FILL_AREA_STYLE ('',( #10344 ) ) ;
#31337 = CARTESIAN_POINT ( 'NONE',  ( 8.073389927753067852, 5.122947197419580156, -6.729807961493258439 ) ) ;
#31338 = CARTESIAN_POINT ( 'NONE',  ( 18.12842152808600460, 0.2489677814039778780, 13.89700419708307066 ) ) ;
#31339 = ORIENTED_EDGE ( 'NONE', *, *, #6126, .T. ) ;
#31340 = CARTESIAN_POINT ( 'NONE',  ( 24.34832088047999932, 8.810502052204325807, -8.810502052203421641 ) ) ;
#31341 = CARTESIAN_POINT ( 'NONE',  ( 12.02733460557258915, -3.793662715184400014, 6.238754009183999472 ) ) ;
#31342 = CARTESIAN_POINT ( 'NONE',  ( 11.59999999999999964, -2.820501972398000046, -7.174999999999999822 ) ) ;
#31343 = CARTESIAN_POINT ( 'NONE',  ( 15.46531638133300035, 9.264179323101998875, 8.208366262023000459 ) ) ;
#31344 = EDGE_CURVE ( 'NONE', #38028, #31922, #38513, .T. ) ;
#31345 = CARTESIAN_POINT ( 'NONE',  ( 7.239688980126000040, -4.389298280625000714, 9.135255728583000945 ) ) ;
#31347 = DIRECTION ( 'NONE',  ( 1.000000000000000000, 0.000000000000000000, 0.000000000000000000 ) ) ;
#31346 = CARTESIAN_POINT ( 'NONE',  ( 10.81315553411000074, 3.756074350075000012, 6.071610008629000355 ) ) ;
#31348 = CARTESIAN_POINT ( 'NONE',  ( 10.52226222744799955, 3.119510978356100139, -8.225278704382400718 ) ) ;
#31349 = EDGE_CURVE ( 'NONE', #20987, #68613, #10164, .T. ) ;
#31350 = CARTESIAN_POINT ( 'NONE',  ( 25.08547621458700050, -11.33429752798000045, 3.320990893601000415 ) ) ;
#31351 = CARTESIAN_POINT ( 'NONE',  ( 9.501025935145998247, 3.874109063559000088, -6.642177514500700042 ) ) ;
#31352 = CARTESIAN_POINT ( 'NONE',  ( 18.27886405737312003, -0.04734719685816868306, 12.59993264914401045 ) ) ;
#31353 = CARTESIAN_POINT ( 'NONE',  ( 7.035787643465999608, -1.088193288857000063, 1.110433857983999850 ) ) ;
#31354 = CARTESIAN_POINT ( 'NONE',  ( 11.67766954483535891, 4.715882430684499305, 8.604570063127999546 ) ) ;
#31355 = CARTESIAN_POINT ( 'NONE',  ( 12.79999999202000005, 11.41069016990000051, -4.623987642516999230 ) ) ;
#31356 = ORIENTED_EDGE ( 'NONE', *, *, #44680, .F. ) ;
#31357 = CARTESIAN_POINT ( 'NONE',  ( 8.534480646793999981, -3.011617647609999615, 8.801438026873999121 ) ) ;
#31358 = CARTESIAN_POINT ( 'NONE',  ( 8.142589158771000868, 5.074768364528000397, -8.296267706722000312 ) ) ;
#31359 = B_SPLINE_CURVE_WITH_KNOTS ( 'NONE', 3,
 ( #16911, #5399, #153, #64449 ),
 .UNSPECIFIED., .F., .F.,
 ( 4, 4 ),
 ( 0.000000000000000000, 1.000000000000000000 ),
 .UNSPECIFIED. ) ;
#31360 = CARTESIAN_POINT ( 'NONE',  ( 8.158337970077000990E-06, 0.000000000000000000, -2.999989272562999965 ) ) ;
#31361 = CARTESIAN_POINT ( 'NONE',  ( 25.60000000000000142, -11.10814700232000085, -2.976419018679000050 ) ) ;
#31362 = ORIENTED_EDGE ( 'NONE', *, *, #29375, .T. ) ;
#31363 = CARTESIAN_POINT ( 'NONE',  ( 0.2059889680762000130, -0.5148121778627998690, -3.334029978310999898 ) ) ;
#31364 = CONICAL_SURFACE ( 'NONE', #10152, 12.47499939740000130, 0.7853981102588313279 ) ;
#31365 = EDGE_CURVE ( 'NONE', #36843, #1716, #9332, .T. ) ;
#31366 = CARTESIAN_POINT ( 'NONE',  ( 10.68546886766499959, 3.433493735705800187, 8.529286361367999447 ) ) ;
#31367 = CARTESIAN_POINT ( 'NONE',  ( 10.10735778041000010, 4.293584699549000128, -8.994197232567001876 ) ) ;
#31368 = ORIENTED_EDGE ( 'NONE', *, *, #68467, .F. ) ;
#31369 = CARTESIAN_POINT ( 'NONE',  ( 12.71024088650322348, -0.7135009822675040247, -12.57978225961209162 ) ) ;
#31370 = CARTESIAN_POINT ( 'NONE',  ( 9.190027038535603765, -5.045605306419576941, -6.289499010756019359 ) ) ;
#31371 = CARTESIAN_POINT ( 'NONE',  ( 10.32118582084299874, 3.163839350524900063, 8.466515260542900378 ) ) ;
#31372 = DIRECTION ( 'NONE',  ( 1.000000000000000000, 0.000000000000000000, 0.000000000000000000 ) ) ;
#31373 = CARTESIAN_POINT ( 'NONE',  ( 7.330281674562000305, 4.426928431836000044, 9.293321981113999541 ) ) ;
#31374 = ORIENTED_EDGE ( 'NONE', *, *, #9650, .T. ) ;
#31375 = CARTESIAN_POINT ( 'NONE',  ( 11.35564217374000329, -3.878722322503999731, 11.75620894677000017 ) ) ;
#31376 = CARTESIAN_POINT ( 'NONE',  ( 6.920464158770999852, 4.499022151374000522, -9.333214642871000777 ) ) ;
#31377 = CARTESIAN_POINT ( 'NONE',  ( 8.221162047634791747, -5.672745506483112266, 7.976212191220952263 ) ) ;
#31378 = CARTESIAN_POINT ( 'NONE',  ( 9.978659112603999404, -4.555852086785099786, 6.347865960448999090 ) ) ;
#31379 = VERTEX_POINT ( 'NONE', #24743 ) ;
#31380 = CARTESIAN_POINT ( 'NONE',  ( 16.31137892731300099, -3.415016125706999972, -11.89702177947000017 ) ) ;
#31381 = CARTESIAN_POINT ( 'NONE',  ( 11.80432898647400108, 11.49396319796999855, 1.654000935039000142 ) ) ;
#31382 = ORIENTED_EDGE ( 'NONE', *, *, #3165, .F. ) ;
#31383 = CARTESIAN_POINT ( 'NONE',  ( 8.761230081853241813, 4.521411717137521435, 6.718925885376237694 ) ) ;
#31384 = CARTESIAN_POINT ( 'NONE',  ( 7.613512347206999209, 10.68273724490999932, -3.841609246918000320 ) ) ;
#31385 = EDGE_LOOP ( 'NONE', ( #36278, #8778, #64205, #62687 ) ) ;
#31386 = CARTESIAN_POINT ( 'NONE',  ( 18.01189197849805623, 0.4270206790917140394, -13.89118144889037509 ) ) ;
#31387 = CARTESIAN_POINT ( 'NONE',  ( 9.624896294737000702, -5.235394649229000663, -8.110359502241001550 ) ) ;
#31388 = LINE ( 'NONE', #57250, #14850 ) ;
#31389 = CARTESIAN_POINT ( 'NONE',  ( 10.44999293566599974, 4.720032669050099550, -8.383280442119700027 ) ) ;
#31390 = CARTESIAN_POINT ( 'NONE',  ( 11.88678751119029897, -5.166297436425000278, 6.889827023674499173 ) ) ;
#31391 = CARTESIAN_POINT ( 'NONE',  ( 8.709123917668916803, -5.736648055247994371, 7.709653903676097819 ) ) ;
#31392 = CARTESIAN_POINT ( 'NONE',  ( 10.75149413291699929, -2.962184842772000337, 7.973529073237199505 ) ) ;
#31393 = CARTESIAN_POINT ( 'NONE',  ( 8.347267219593000220, 2.741641653469999884, 6.457329666915000210 ) ) ;
#31394 = VERTEX_POINT ( 'NONE', #46069 ) ;
#31395 = CARTESIAN_POINT ( 'NONE',  ( 10.85685100254000091, 2.832432432432000269, -6.822293592207000934 ) ) ;
#31396 = CARTESIAN_POINT ( 'NONE',  ( 8.866808059624998961, -2.550589632307000088, 8.854674225901000284 ) ) ;
#31397 = DIRECTION ( 'NONE',  ( 1.000000000000000000, 0.000000000000000000, 0.000000000000000000 ) ) ;
#31398 = EDGE_LOOP ( 'NONE', ( #63004, #25854, #27949, #28645 ) ) ;
#31399 = CARTESIAN_POINT ( 'NONE',  ( 12.64197434038402790, -3.103437838334064836, -12.29027179270079273 ) ) ;
#31400 = CARTESIAN_POINT ( 'NONE',  ( 10.86919096481999780, 8.268617798044999745, -7.016197574546996663 ) ) ;
#31401 = DIRECTION ( 'NONE',  ( 1.000000000000000000, 0.000000000000000000, 0.000000000000000000 ) ) ;
#31402 = EDGE_CURVE ( 'NONE', #2551, #1379, #35189, .T. ) ;
#31403 = CARTESIAN_POINT ( 'NONE',  ( 10.90000004630000063, 9.856474695503001371, 5.627825000517000298 ) ) ;
#31404 = CARTESIAN_POINT ( 'NONE',  ( 12.63832872341681757, -3.228981699441164199, -13.62254385108541754 ) ) ;
#31405 = EDGE_CURVE ( 'NONE', #60460, #64287, #68062, .T. ) ;
#31406 = CARTESIAN_POINT ( 'NONE',  ( 10.89979975933730039, -3.180925410802600162, -7.218192605361100078 ) ) ;
#31407 = ADVANCED_FACE ( 'NONE', ( #67375 ), #45387, .F. ) ;
#31408 = DIRECTION ( 'NONE',  ( 1.000000000000000000, 0.000000000000000000, 0.000000000000000000 ) ) ;
#31409 = CARTESIAN_POINT ( 'NONE',  ( 18.27533594408738438, -2.564445959844779743, 12.33627802783496286 ) ) ;
#31410 = ORIENTED_EDGE ( 'NONE', *, *, #35618, .F. ) ;
#31411 = ORIENTED_EDGE ( 'NONE', *, *, #64786, .F. ) ;
#31412 = CARTESIAN_POINT ( 'NONE',  ( 0.000000000000000000, 0.000000000000000000, 0.000000000000000000 ) ) ;
#31413 = CARTESIAN_POINT ( 'NONE',  ( 11.80361999289329944, -4.544092497359196514, 8.657883396625690509 ) ) ;
#31414 = CARTESIAN_POINT ( 'NONE',  ( 11.79999999550100220, -3.351258778187000242, 11.15757272551999968 ) ) ;
#31415 = B_SPLINE_CURVE_WITH_KNOTS ( 'NONE', 3,
 ( #5637, #22754, #48294, #44103, #54925, #21378, #42711, #64016, #16137, #58782 ),
 .UNSPECIFIED., .F., .F.,
 ( 4, 2, 2, 2, 4 ),
 ( 0.3934091950370091628, 0.5450568962777566639, 0.6967045975185042206, 0.8483522987592517772, 1.000000000000000000 ),
 .UNSPECIFIED. ) ;
#31416 = CARTESIAN_POINT ( 'NONE',  ( 10.85290485628999946, 3.170386876061999537, -8.782184998573001167 ) ) ;
#31417 = CARTESIAN_POINT ( 'NONE',  ( 10.90635170712999980, -3.089674976714000376, -6.534319251717000121 ) ) ;
#31418 = CARTESIAN_POINT ( 'NONE',  ( 18.16462229618754520, 2.361607881905639417, 12.48272818380096716 ) ) ;
#31419 = CARTESIAN_POINT ( 'NONE',  ( 23.85184979680500206, -13.16354065916999971, 3.535578269679999774 ) ) ;
#31420 = CARTESIAN_POINT ( 'NONE',  ( 10.87521525736000072, 4.831064930369000088, 6.312796576761000367 ) ) ;
#31421 = AXIS2_PLACEMENT_3D ( 'NONE', #7974, #61110, #8314 ) ;
#31422 = EDGE_LOOP ( 'NONE', ( #19119, #2047, #17020, #20667 ) ) ;
#31423 = CARTESIAN_POINT ( 'NONE',  ( 21.49999863197000138, 14.00000000000000000, 0.000000000000000000 ) ) ;
#31424 = ORIENTED_EDGE ( 'NONE', *, *, #30336, .F. ) ;
#31425 = CARTESIAN_POINT ( 'NONE',  ( 9.657553581808000942, 5.333455947841000189, 6.049916795084000043 ) ) ;
#31426 = CARTESIAN_POINT ( 'NONE',  ( 8.715822372493999382, -4.249211653873900651, -8.315254653915399530 ) ) ;
#31427 = CARTESIAN_POINT ( 'NONE',  ( 10.61382428715999993, 3.385080336122999967, 5.849521480782000182 ) ) ;
#31428 = CARTESIAN_POINT ( 'NONE',  ( 12.06833327354034857, -4.746587807672299597, 7.988332985010599963 ) ) ;
#31429 = CARTESIAN_POINT ( 'NONE',  ( 9.816185841232000442, 2.656512020013999997, -7.884832994446999699 ) ) ;
#31430 = CARTESIAN_POINT ( 'NONE',  ( 11.14445592698000098, 10.08445635709999877, -5.720398172012999716 ) ) ;
#31431 = CARTESIAN_POINT ( 'NONE',  ( 24.74447938189800311, 8.626864566307999027, 8.720113821614001282 ) ) ;
#31432 = CARTESIAN_POINT ( 'NONE',  ( 12.26342954938196961, -0.3125562302819448468, 12.69484091569602668 ) ) ;
#31433 = AXIS2_PLACEMENT_3D ( 'NONE', #40935, #13689, #3520 ) ;
#31434 = CARTESIAN_POINT ( 'NONE',  ( 9.251926658770999623, 5.159258275969999197, 9.109498396691998678 ) ) ;
#31435 = CARTESIAN_POINT ( 'NONE',  ( 10.19255830160000009, 2.560287027313000063, 7.664549200117999561 ) ) ;
#31436 = CARTESIAN_POINT ( 'NONE',  ( 9.162712628445618179, -3.042358984555600276, 8.452211083226405464 ) ) ;
#31437 = EDGE_LOOP ( 'NONE', ( #52675, #2997, #18769, #20123 ) ) ;
#31438 = CARTESIAN_POINT ( 'NONE',  ( 8.532195280408998883, 5.331510020787000315, -8.114341808290998159 ) ) ;
#31439 = FACE_OUTER_BOUND ( 'NONE', #35751, .T. ) ;
#31440 = CARTESIAN_POINT ( 'NONE',  ( 17.65854462812407988, 1.883284865257428775, 13.78503182716601394 ) ) ;
#31441 = CARTESIAN_POINT ( 'NONE',  ( 9.354766166764603597, 2.650157509278342705, -7.676821081800753177 ) ) ;
#31442 = CARTESIAN_POINT ( 'NONE',  ( 12.09999999999999964, -3.186139913033901205, 8.315594847681079926 ) ) ;
#31443 = CARTESIAN_POINT ( 'NONE',  ( 10.86687616594229944, -4.344946439135400240, -6.412662853391999818 ) ) ;
#31444 = ORIENTED_EDGE ( 'NONE', *, *, #47101, .F. ) ;
#31445 = CARTESIAN_POINT ( 'NONE',  ( 15.89994436294300151, -8.847904542234999781, -8.580301953175000662 ) ) ;
#31446 = CARTESIAN_POINT ( 'NONE',  ( 8.528448341230999930, 2.472348777564000066, 6.234194744024999402 ) ) ;
#31447 = EDGE_CURVE ( 'NONE', #11176, #55971, #42847, .T. ) ;
#31449 = CARTESIAN_POINT ( 'NONE',  ( 13.59022209853100094, -9.429754002912000388, -8.017367994085999428 ) ) ;
#31448 = CARTESIAN_POINT ( 'NONE',  ( 8.573539158775000502, 5.361622798585000460, -7.185294144754000634 ) ) ;
#31450 = CARTESIAN_POINT ( 'NONE',  ( 18.17918907329226741, -2.539311109799761379, 13.66506621000925037 ) ) ;
#31451 = ORIENTED_EDGE ( 'NONE', *, *, #24621, .T. ) ;
#31452 = CARTESIAN_POINT ( 'NONE',  ( 9.646287586158999616, 2.591467678478000192, 6.760055064032999717 ) ) ;
#31453 = EDGE_CURVE ( 'NONE', #54265, #2358, #43608, .T. ) ;
#31454 = CARTESIAN_POINT ( 'NONE',  ( 18.00692794902808558, -2.068098667605225316, -13.75558205683924484 ) ) ;
#31455 = CARTESIAN_POINT ( 'NONE',  ( 11.09672200990539892, 3.182132064022000328, 7.785290430335599865 ) ) ;
#31456 = CARTESIAN_POINT ( 'NONE',  ( 24.71431109946687243, -11.77711172499810210, 3.190793255218363544 ) ) ;
#31457 = CARTESIAN_POINT ( 'NONE',  ( 7.191894353207000101, -3.501517589953999643, 9.055975309745999624 ) ) ;
#31458 = ORIENTED_EDGE ( 'NONE', *, *, #9736, .T. ) ;
#31459 = CARTESIAN_POINT ( 'NONE',  ( 8.353301658773000682, 2.800103557244999930, 9.079946116129001155 ) ) ;
#31461 = CARTESIAN_POINT ( 'NONE',  ( 10.36503728015293646, 2.650011783304074164, -7.500002219258057323 ) ) ;
#31460 = CARTESIAN_POINT ( 'NONE',  ( 9.317462135714000837, 5.100000000000000533, 6.571291218949999902 ) ) ;
#31462 = CARTESIAN_POINT ( 'NONE',  ( 7.587133471837959497, -4.278447414270965865, 5.782523221580097683 ) ) ;
#31463 = CARTESIAN_POINT ( 'NONE',  ( 18.06139357115090860, -0.3666408745423706539, 13.89349736880855524 ) ) ;
#31464 = CARTESIAN_POINT ( 'NONE',  ( 2.119930008642999741, -2.059315964850999769, -2.525946829712999886 ) ) ;
#31465 = ORIENTED_EDGE ( 'NONE', *, *, #52580, .F. ) ;
#31466 = CARTESIAN_POINT ( 'NONE',  ( 25.29995758267499895, -11.13046986584000031, -3.427500733308000314 ) ) ;
#31467 = CARTESIAN_POINT ( 'NONE',  ( 11.83872066707849946, -3.141388196630700236, 8.019361746728900897 ) ) ;
#31468 = CARTESIAN_POINT ( 'NONE',  ( 0.000000000000000000, 5.100000000000000533, 7.500000000000000000 ) ) ;
#31469 = CARTESIAN_POINT ( 'NONE',  ( 9.743561007103998861, 5.287400066955999733, 8.939966147452000911 ) ) ;
#31470 = CARTESIAN_POINT ( 'NONE',  ( 10.44841638348500013, 2.891666689023999925, 7.769976643522699788 ) ) ;
#31471 = EDGE_LOOP ( 'NONE', ( #46402, #6265, #4822, #7564, #41398 ) ) ;
#31472 = VECTOR ( 'NONE', #11720, 1000.000000000000000 ) ;
#31473 = LINE ( 'NONE', #68510, #22628 ) ;
#31474 = CARTESIAN_POINT ( 'NONE',  ( 12.61568544974630690, 1.785400273382270919, -12.47286636618916589 ) ) ;
#31475 = DIRECTION ( 'NONE',  ( -0.7071070235446059726, -0.7071065388284060171, -2.367528967094019852E-10 ) ) ;
#31476 = CARTESIAN_POINT ( 'NONE',  ( 8.609219020791252674, 4.708310599750610947, 5.912357210627167348 ) ) ;
#31477 = CARTESIAN_POINT ( 'NONE',  ( 17.92014050163765049, -1.886715056483322384, 13.87229028472749981 ) ) ;
#31478 = CARTESIAN_POINT ( 'NONE',  ( 18.13950502221108252, 2.721680755780143013, -13.62394404490971489 ) ) ;
#31479 = ORIENTED_EDGE ( 'NONE', *, *, #52640, .T. ) ;
#31480 = CARTESIAN_POINT ( 'NONE',  ( 9.725191424783275806, 2.649754699899339538, 7.500009801425228773 ) ) ;
#31481 = ORIENTED_EDGE ( 'NONE', *, *, #20828, .T. ) ;
#31482 = CARTESIAN_POINT ( 'NONE',  ( 9.385596873516666605, 2.907767014557175678, 6.870476274536375882 ) ) ;
#31483 = DIRECTION ( 'NONE',  ( 1.000000000000000000, 0.000000000000000000, 0.000000000000000000 ) ) ;
#31484 = CARTESIAN_POINT ( 'NONE',  ( 7.100000000000000533, -11.06886219213000011, -1.536526853569999851 ) ) ;
#31485 = CARTESIAN_POINT ( 'NONE',  ( 11.06133897141000055, 2.503910831767000023, -6.712778933675999760 ) ) ;
#31486 = DIRECTION ( 'NONE',  ( 1.000000000000000000, 0.000000000000000000, 0.000000000000000000 ) ) ;
#31487 = EDGE_CURVE ( 'NONE', #23058, #22260, #16092, .T. ) ;
#31488 = CARTESIAN_POINT ( 'NONE',  ( 9.444317341922999987, -2.927260449021000355, 8.897015448164999896 ) ) ;
#31489 = ADVANCED_FACE ( 'NONE', ( #57933 ), #66299, .T. ) ;
#31490 = CARTESIAN_POINT ( 'NONE',  ( 18.04446571359449791, 0.3888461597108446854, -12.69199065798141568 ) ) ;
#31491 = CARTESIAN_POINT ( 'NONE',  ( 9.040103201076165718, 4.925662930945876816, 8.482493365444813804 ) ) ;
#31492 = CARTESIAN_POINT ( 'NONE',  ( 11.14179841651039915, -4.353306409735099969, -8.439215328713499886 ) ) ;
#31493 = EDGE_CURVE ( 'NONE', #64217, #6549, #17731, .T. ) ;
#31494 = ADVANCED_FACE ( 'NONE', ( #64192 ), #63509, .F. ) ;
#31495 = CARTESIAN_POINT ( 'NONE',  ( 8.662857780412000608, 2.741641653469999884, 6.457329666915000210 ) ) ;
#31496 = ORIENTED_EDGE ( 'NONE', *, *, #50938, .F. ) ;
#31497 = CARTESIAN_POINT ( 'NONE',  ( 11.10000000000000142, 2.290061757222789041, -7.204632786817215084 ) ) ;
#31498 = CARTESIAN_POINT ( 'NONE',  ( 9.231612604287846580, 2.652298733595448432, 7.391242544803094283 ) ) ;
#31499 = CARTESIAN_POINT ( 'NONE',  ( 10.38351354018329253, -5.249999999999998224, -7.336375382625530683 ) ) ;
#31500 = FACE_OUTER_BOUND ( 'NONE', #49239, .T. ) ;
#31501 = CARTESIAN_POINT ( 'NONE',  ( 12.68590879673670102, 1.797325930449587661, 13.88415075348993533 ) ) ;
#31502 = CARTESIAN_POINT ( 'NONE',  ( 10.63462194421999918, -5.668721490782999695, 6.527259573254000635 ) ) ;
#31503 = DIRECTION ( 'NONE',  ( -1.782458877139945186E-07, 1.777825404087945614E-07, -0.9999999999999682476 ) ) ;
#31504 = CARTESIAN_POINT ( 'NONE',  ( 24.30000000000000071, 3.224868684338999980, -12.03537377768999939 ) ) ;
#31505 = ORIENTED_EDGE ( 'NONE', *, *, #48866, .F. ) ;
#31506 = CARTESIAN_POINT ( 'NONE',  ( 12.50285324413425947, -1.826185914346432071, 12.46695919779662454 ) ) ;
#31507 = CARTESIAN_POINT ( 'NONE',  ( 10.46755864497999866, -3.101067942814400347, -8.204026508301600629 ) ) ;
#31508 = CARTESIAN_POINT ( 'NONE',  ( 11.09999233421999953, -1.199999999999999956, -9.776630298829998011 ) ) ;
#31509 = EDGE_CURVE ( 'NONE', #49843, #7211, #6810, .T. ) ;
#31510 = CARTESIAN_POINT ( 'NONE',  ( 10.03491210303999992, -5.615910465798999773, 7.351455544018000943 ) ) ;
#31511 = CARTESIAN_POINT ( 'NONE',  ( 11.49826088462129903, -3.998156935320088756, 8.366195817038299509 ) ) ;
#31512 = AXIS2_PLACEMENT_3D ( 'NONE', #48744, #22505, #58886 ) ;
#31513 = CARTESIAN_POINT ( 'NONE',  ( 12.21591953885794624, 0.4193891200559139998, 12.59302195412780456 ) ) ;
#31514 = CARTESIAN_POINT ( 'NONE',  ( 0.7380201129275000271, 2.302377811826000098, -2.236047032684999714 ) ) ;
#31515 = B_SPLINE_CURVE_WITH_KNOTS ( 'NONE', 3,
 ( #63640, #5943, #4567, #10849, #63977 ),
 .UNSPECIFIED., .F., .F.,
 ( 4, 1, 4 ),
 ( 0.000000000000000000, 0.5000000000000000000, 1.000000000000000000 ),
 .UNSPECIFIED. ) ;
#31516 = CARTESIAN_POINT ( 'NONE',  ( 4.400000000000000355, -0.7080094843779000113, -0.8552562627201000245 ) ) ;
#31517 = CARTESIAN_POINT ( 'NONE',  ( 12.12640605329506016, 2.733942857944761773, 12.29982446443561805 ) ) ;
#31518 = CARTESIAN_POINT ( 'NONE',  ( 9.927916723342999461, -5.290169207169999943, -8.858081286661999343 ) ) ;
#31519 = CARTESIAN_POINT ( 'NONE',  ( 10.67410807141119911, 4.046361247106100123, -8.502397868920999358 ) ) ;
#31520 = CARTESIAN_POINT ( 'NONE',  ( 8.066302634316002695, 3.111242948840002409, -6.203702194951995708 ) ) ;
#31521 = CARTESIAN_POINT ( 'NONE',  ( 11.15264221959000146, 2.317063201199000222, -7.596564358366999947 ) ) ;
#31522 = CARTESIAN_POINT ( 'NONE',  ( 8.577265421554999492, 3.785712956512099936, -8.608472884860999486 ) ) ;
#31524 = CARTESIAN_POINT ( 'NONE',  ( 12.21947784598696352, 2.718529666067204253, 12.39796232694461331 ) ) ;
#31523 = CARTESIAN_POINT ( 'NONE',  ( 15.39999999998900293, 9.471998555523999386, 8.194929586088999685 ) ) ;
#31525 = CARTESIAN_POINT ( 'NONE',  ( 11.13220574173980992, -2.863826994586552654, -6.911917091190554530 ) ) ;
#31526 = ORIENTED_EDGE ( 'NONE', *, *, #35876, .F. ) ;
#31527 = AXIS2_PLACEMENT_3D ( 'NONE', #46221, #51459, #19651 ) ;
#31528 = DIRECTION ( 'NONE',  ( 0.000000000000000000, 1.000000000000000000, 0.000000000000000000 ) ) ;
#31529 = CARTESIAN_POINT ( 'NONE',  ( 15.89979320885400327, 3.824231472901999496, 11.71686814605000038 ) ) ;
#31530 = EDGE_CURVE ( 'NONE', #9263, #23594, #68593, .T. ) ;
#31531 = CIRCLE ( 'NONE', #19250, 1.000000000000000000 ) ;
#31532 = CARTESIAN_POINT ( 'NONE',  ( 9.323728576950999880, -3.947350124452999598, 6.051857392047999440 ) ) ;
#31533 = CARTESIAN_POINT ( 'NONE',  ( 10.32844474310100047, 4.771257858050099721, 7.125715588371799747 ) ) ;
#31534 = FACE_OUTER_BOUND ( 'NONE', #15403, .T. ) ;
#31535 = ADVANCED_FACE ( 'NONE', ( #26465 ), #35157, .T. ) ;
#31536 = CARTESIAN_POINT ( 'NONE',  ( 12.18523880347864718, -2.582858790010648331, 13.65555696386475404 ) ) ;
#31537 = CARTESIAN_POINT ( 'NONE',  ( 12.23172337865302062, 2.748896841597663787, 13.61745941693664186 ) ) ;
#31538 = CARTESIAN_POINT ( 'NONE',  ( 23.52014407070900148, 3.097444545157999940, -13.78484368444999930 ) ) ;
#31539 = ORIENTED_EDGE ( 'NONE', *, *, #58744, .F. ) ;
#31540 = CARTESIAN_POINT ( 'NONE',  ( 5.082213209869999915, 0.8026392371705000084, -0.9912343320891000564 ) ) ;
#31541 = CARTESIAN_POINT ( 'NONE',  ( 8.566809814040999171, -3.217492037304399588, -8.511961036725999463 ) ) ;
#31542 = CARTESIAN_POINT ( 'NONE',  ( 6.999999692251999583, -12.89129024476000041, -1.677687640358999976 ) ) ;
#31543 = CARTESIAN_POINT ( 'NONE',  ( 11.27879632507499963, -3.576455950783300253, 6.714825466131699727 ) ) ;
#31544 = B_SPLINE_CURVE_WITH_KNOTS ( 'NONE', 3,
 ( #66278, #23982, #45319, #65589, #55110, #18402 ),
 .UNSPECIFIED., .F., .F.,
 ( 4, 1, 1, 4 ),
 ( 0.000000000000000000, 0.2305484780870906414, 0.8346924593416191751, 1.000000000000000000 ),
 .UNSPECIFIED. ) ;
#31545 = CARTESIAN_POINT ( 'NONE',  ( 18.14999129509864417, 2.691763112583329676, -12.40484894414121975 ) ) ;
#31546 = CARTESIAN_POINT ( 'NONE',  ( 8.601133948506207716, 4.977182018904446892, 6.107802660072452205 ) ) ;
#31547 = CARTESIAN_POINT ( 'NONE',  ( 8.789886373836322875, -3.999992178805580334, -8.439846342473931173 ) ) ;
#31548 = CARTESIAN_POINT ( 'NONE',  ( 18.00364620834145768, 1.936356668727586827, 13.86561588860068461 ) ) ;
#31549 = CARTESIAN_POINT ( 'NONE',  ( 9.112942518363999156, 5.100000000000000533, 6.192000867487999827 ) ) ;
#31550 = CARTESIAN_POINT ( 'NONE',  ( 24.95409956869000112, 12.04587931301000125, 2.875990604036999798 ) ) ;
#31551 = FACE_OUTER_BOUND ( 'NONE', #30637, .T. ) ;
#31552 = LINE ( 'NONE', #58801, #43126 ) ;
#31553 = CARTESIAN_POINT ( 'NONE',  ( 24.14324603874189279, 9.149633372423830124, -9.124494086798831560 ) ) ;
#31554 = CARTESIAN_POINT ( 'NONE',  ( 12.80505043854146940, -3.125000000000000000, -13.52078605991414761 ) ) ;
#31555 = CARTESIAN_POINT ( 'NONE',  ( 23.83662696556500293, 13.03915312176000008, -3.620547879630999777 ) ) ;
#31556 =( REPRESENTATION_RELATIONSHIP ('NONE','NONE', #10823, #46027 ) REPRESENTATION_RELATIONSHIP_WITH_TRANSFORMATION ( #18451 )SHAPE_REPRESENTATION_RELATIONSHIP( ) );
#31557 = B_SPLINE_CURVE_WITH_KNOTS ( 'NONE', 3,
 ( #28424, #55682, #33667, #2529 ),
 .UNSPECIFIED., .F., .F.,
 ( 4, 4 ),
 ( 0.000000000000000000, 1.000000000000000000 ),
 .UNSPECIFIED. ) ;
#31558 = VERTEX_POINT ( 'NONE', #16568 ) ;
#31559 = CARTESIAN_POINT ( 'NONE',  ( 9.699495280410998177, 5.048004622677000341, -6.120508709481000231 ) ) ;
#31560 = CARTESIAN_POINT ( 'NONE',  ( 10.98133997688000107, -3.815400206859000054, 8.346298710230199092 ) ) ;
#31561 = ORIENTED_EDGE ( 'NONE', *, *, #56097, .F. ) ;
#31562 = AXIS2_PLACEMENT_3D ( 'NONE', #22738, #48976, #54565 ) ;
#31563 = DIRECTION ( 'NONE',  ( 0.000000000000000000, 0.000000000000000000, 1.000000000000000000 ) ) ;
#31564 = CARTESIAN_POINT ( 'NONE',  ( 10.74379975933729980, -2.921317947059999920, -7.128873141726999485 ) ) ;
#31565 = EDGE_LOOP ( 'NONE', ( #1098, #1560, #67688, #15195 ) ) ;
#31566 = CARTESIAN_POINT ( 'NONE',  ( 11.38678751119029897, 2.833702563575000166, 6.889827023674499173 ) ) ;
#31567 = DIRECTION ( 'NONE',  ( 1.000000000000000000, 0.000000000000000000, 0.000000000000000000 ) ) ;
#31568 = CARTESIAN_POINT ( 'NONE',  ( 17.79514046837899954, -3.190852705101999920, 11.45040944101999969 ) ) ;
#31569 = PLANE ( 'NONE',  #9890 ) ;
#31570 = CARTESIAN_POINT ( 'NONE',  ( 9.873096873515667227, -5.217465845835394411, -7.172815144550898303 ) ) ;
#31571 = CARTESIAN_POINT ( 'NONE',  ( 7.067443904950497569, 1.128838519570273258, -0.1795834841119597070 ) ) ;
#31572 = CARTESIAN_POINT ( 'NONE',  ( 13.06873602477000063, 11.64657800763999873, 1.862567138450999860 ) ) ;
#31573 = ORIENTED_EDGE ( 'NONE', *, *, #28372, .T. ) ;
#31574 = CARTESIAN_POINT ( 'NONE',  ( 13.46395943152100116, 9.515552291263999152, 7.774702642439999423 ) ) ;
#31575 = EDGE_CURVE ( 'NONE', #33797, #32376, #55243, .T. ) ;
#31576 = EDGE_CURVE ( 'NONE', #10089, #55299, #52756, .T. ) ;
#31577 = CARTESIAN_POINT ( 'NONE',  ( 8.871410841230998656, 2.721111233225000259, -6.936528696292000085 ) ) ;
#31578 = ORIENTED_EDGE ( 'NONE', *, *, #50711, .F. ) ;
#31579 = AXIS2_PLACEMENT_3D ( 'NONE', #36645, #57968, #31401 ) ;
#31580 = DIRECTION ( 'NONE',  ( 1.000000000000000000, 0.000000000000000000, 7.549516567279000659E-14 ) ) ;
#31581 = ORIENTED_EDGE ( 'NONE', *, *, #30483, .T. ) ;
#31582 = CARTESIAN_POINT ( 'NONE',  ( 9.630633995698000049, 5.271405458160000279, 7.358888170452400068 ) ) ;
#31583 = CARTESIAN_POINT ( 'NONE',  ( 17.63823367518483565, -3.119790641614041959, -12.28531617466518000 ) ) ;
#31584 = CARTESIAN_POINT ( 'NONE',  ( 10.89393020684959978, -5.250000000000000000, -7.500000000000000000 ) ) ;
#31585 = LINE ( 'NONE', #102, #24630 ) ;
#31586 = CARTESIAN_POINT ( 'NONE',  ( 10.16052890781999984, -2.899999999999999911, -6.152188490330000370 ) ) ;
#31587 = VERTEX_POINT ( 'NONE', #54667 ) ;
#31588 = CARTESIAN_POINT ( 'NONE',  ( 12.00339635128600158, 11.70009917314000170, -4.315816162729000816 ) ) ;
#31589 = CARTESIAN_POINT ( 'NONE',  ( 9.769471092180999960, -5.100000000000000533, -6.152188490330000370 ) ) ;
#31590 = ADVANCED_FACE ( 'NONE', ( #44547 ), #3893, .F. ) ;
#31591 = DIRECTION ( 'NONE',  ( -1.000000000000000000, 0.000000000000000000, 0.000000000000000000 ) ) ;
#31592 = CARTESIAN_POINT ( 'NONE',  ( 12.57032717430620927, 3.208883835765880654, -13.62729181966624203 ) ) ;
#31593 = CARTESIAN_POINT ( 'NONE',  ( 25.59994555223600088, 0.6895522877779571846, 11.26073925913301288 ) ) ;
#31594 = CARTESIAN_POINT ( 'NONE',  ( 14.40000000633000177, -11.86188960395448788, 3.298666394459744300 ) ) ;
#31595 = CARTESIAN_POINT ( 'NONE',  ( 9.741009892375998902, -3.588529236307000048, -8.800227248412999970 ) ) ;
#31596 = VERTEX_POINT ( 'NONE', #35601 ) ;
#31597 = ORIENTED_EDGE ( 'NONE', *, *, #36662, .T. ) ;
#31598 = CARTESIAN_POINT ( 'NONE',  ( 10.22180282788866812, -2.874603711589704957, 6.749639981055104876 ) ) ;
#31599 = CARTESIAN_POINT ( 'NONE',  ( 10.14395937989721652, 4.746860684429531574, -8.656482714661228428 ) ) ;
#31600 = CARTESIAN_POINT ( 'NONE',  ( 5.500000000000000000, -0.2500000000000000000, -3.149999999999999911 ) ) ;
#31601 = CARTESIAN_POINT ( 'NONE',  ( 6.063359839683333696, -1.310679582531389498, 0.7554284705563444335 ) ) ;
#31602 = CARTESIAN_POINT ( 'NONE',  ( 11.55811496860034815, 5.045590851977999947, -6.964183526617899744 ) ) ;
#31603 = CARTESIAN_POINT ( 'NONE',  ( 9.231405316140000039, 3.815922504313999930, -8.347244604637999998 ) ) ;
#31605 = CARTESIAN_POINT ( 'NONE',  ( 4.399785476046610633, -0.5075215790221194734, -1.032760291147674314 ) ) ;
#31604 = CARTESIAN_POINT ( 'NONE',  ( 10.83890035061499901, -3.732283713685800031, 6.531924610394499453 ) ) ;
#31606 = CARTESIAN_POINT ( 'NONE',  ( 8.325003570449004187, -2.868532950405002779, 6.316175323229005656 ) ) ;
#31607 = EDGE_LOOP ( 'NONE', ( #53320, #33469, #22862, #64448 ) ) ;
#31608 = VECTOR ( 'NONE', #53711, 1000.000000000000114 ) ;
#31609 = CARTESIAN_POINT ( 'NONE',  ( 2.716664739337339540, 2.750000000000000000, 3.881524028221258434E-10 ) ) ;
#31610 = CARTESIAN_POINT ( 'NONE',  ( 8.076856445596000356, -2.879480170456998778, 6.727212843387002650 ) ) ;
#31611 = CARTESIAN_POINT ( 'NONE',  ( 10.11496314287999887, 5.251703735191999733, 7.763860089407599752 ) ) ;
#31612 = FACE_OUTER_BOUND ( 'NONE', #859, .T. ) ;
#31613 = CARTESIAN_POINT ( 'NONE',  ( 9.256662271119999730, -4.025830307267999508, 9.295859242339000517 ) ) ;
#31614 = ADVANCED_FACE ( 'NONE', ( #3422 ), #10503, .T. ) ;
#31615 = CARTESIAN_POINT ( 'NONE',  ( 18.11183118192862906, 2.784086580334055316, -12.38085211675188013 ) ) ;
#31616 = CARTESIAN_POINT ( 'NONE',  ( 10.77706886429733402, -2.899999999999999911, -6.444141223373583749 ) ) ;
#31617 = CARTESIAN_POINT ( 'NONE',  ( 13.99956681845000084, 8.827069132150999309, 7.822720559936999329 ) ) ;
#31618 = CARTESIAN_POINT ( 'NONE',  ( 7.986960674332891585, 3.285250301221325664, -6.274837602397500547 ) ) ;
#31619 = MECHANICAL_DESIGN_GEOMETRIC_PRESENTATION_REPRESENTATION (  '', ( #22678 ), #2624 ) ;
#31620 = CARTESIAN_POINT ( 'NONE',  ( 9.434038493598999153, -3.372531419565699906, -6.901676404381399621 ) ) ;
#31621 = CARTESIAN_POINT ( 'NONE',  ( 10.94601354018327122, -4.999583552997726166, 6.731816600031359066 ) ) ;
#31622 = CARTESIAN_POINT ( 'NONE',  ( 10.81652245563454784, -3.317579219585634842, 6.971781362826274808 ) ) ;
#31623 = VECTOR ( 'NONE', #4478, 1000.000000000000000 ) ;
#31624 = CARTESIAN_POINT ( 'NONE',  ( 18.00454058111931488, 1.908039605461288035, 12.45487753842856726 ) ) ;
#31625 = DIRECTION ( 'NONE',  ( 0.000000000000000000, 0.007439385635797960035, 0.9999723273877941798 ) ) ;
#31626 = VERTEX_POINT ( 'NONE', #62491 ) ;
#31627 = CARTESIAN_POINT ( 'NONE',  ( 12.21985383964851479, 0.2197131112048736901, -12.69744725510432914 ) ) ;
#31628 = CARTESIAN_POINT ( 'NONE',  ( 12.18137864098527068, -2.541952522640275713, -12.44169427845088194 ) ) ;
#31629 = CARTESIAN_POINT ( 'NONE',  ( 8.710288521113000115, 3.647046440108700160, -8.284550957747498501 ) ) ;
#31630 = LINE ( 'NONE', #52950, #1085 ) ;
#31631 = LINE ( 'NONE', #26386, #3615 ) ;
#31632 = ORIENTED_EDGE ( 'NONE', *, *, #58477, .T. ) ;
#31633 = LINE ( 'NONE', #47715, #56729 ) ;
#31634 = CARTESIAN_POINT ( 'NONE',  ( 10.90346005378009941, -3.213042707518099839, -7.079777642108599167 ) ) ;
#31635 = LINE ( 'NONE', #21817, #9430 ) ;
#31636 = DIRECTION ( 'NONE',  ( -8.147729033647319588E-21, 0.9999999999999638067, 2.692747184958149612E-07 ) ) ;
#31637 = CARTESIAN_POINT ( 'NONE',  ( 10.70440763476387680, 2.684940916868421734, 7.852706794445638572 ) ) ;
#31638 = CARTESIAN_POINT ( 'NONE',  ( 12.96385332268500079, 12.32790784140999918, 1.878650414825000059 ) ) ;
#31639 = ORIENTED_EDGE ( 'NONE', *, *, #20780, .T. ) ;
#31640 = CARTESIAN_POINT ( 'NONE',  ( 10.02202195053999922, -3.298019507654999849, 5.700533868754000366 ) ) ;
#31641 = CARTESIAN_POINT ( 'NONE',  ( 8.755786719645998417, -4.065290607273509771, -8.402920843186199917 ) ) ;
#31642 = ORIENTED_EDGE ( 'NONE', *, *, #27491, .F. ) ;
#31643 = CARTESIAN_POINT ( 'NONE',  ( 13.42968832854115391, 11.50414049279873829, 1.837906235098867302 ) ) ;
#31644 = CARTESIAN_POINT ( 'NONE',  ( 7.994581853207999522, -2.263562268490999951, 8.007440964304000985 ) ) ;
#31645 = CARTESIAN_POINT ( 'NONE',  ( 16.04720874474600123, 8.391565830097999168, 8.158729932893001191 ) ) ;
#31646 = EDGE_LOOP ( 'NONE', ( #37461, #41255, #33171, #31236 ) ) ;
#31647 = CARTESIAN_POINT ( 'NONE',  ( 8.657436137450503111, 2.838366281656380608, -6.183390965021622776 ) ) ;
#31648 = B_SPLINE_CURVE_WITH_KNOTS ( 'NONE', 3,
 ( #10186, #16454, #32549, #53862 ),
 .UNSPECIFIED., .F., .F.,
 ( 4, 4 ),
 ( 0.000000000000000000, 1.000000000000000000 ),
 .UNSPECIFIED. ) ;
#31649 = CARTESIAN_POINT ( 'NONE',  ( 7.432479719588999778, 2.435036720175999925, -7.494591853605999887 ) ) ;
#31650 = CARTESIAN_POINT ( 'NONE',  ( 9.416846873516664829, -4.768183399968644487, -8.499583552997725278 ) ) ;
#31651 = CARTESIAN_POINT ( 'NONE',  ( 7.156825054363874727, 5.205086695061690527, -8.205119277360076069 ) ) ;
#31652 = VERTEX_POINT ( 'NONE', #51663 ) ;
#31653 = CARTESIAN_POINT ( 'NONE',  ( 9.662553763536999796, -4.094830574823999925, 9.119950378356000087 ) ) ;
#31654 = EDGE_CURVE ( 'NONE', #1910, #31995, #59611, .T. ) ;
#31655 = ADVANCED_FACE ( 'NONE', ( #41862 ), #30690, .T. ) ;
#31656 = VECTOR ( 'NONE', #6264, 1000.000000000000000 ) ;
#31657 = CARTESIAN_POINT ( 'NONE',  ( 25.40550542876300000, 11.40415454737000012, -3.013955980041000071 ) ) ;
#31658 = CARTESIAN_POINT ( 'NONE',  ( 5.500000000000000000, -13.87069231928999891, 4.225386915259999654 ) ) ;
#31659 = ORIENTED_EDGE ( 'NONE', *, *, #18280, .T. ) ;
#31660 = VECTOR ( 'NONE', #4846, 1000.000000000000000 ) ;
#31661 = LINE ( 'NONE', #51596, #57120 ) ;
#31662 = EDGE_LOOP ( 'NONE', ( #60783, #37893, #4131, #40832 ) ) ;
#31663 = CARTESIAN_POINT ( 'NONE',  ( 2.250973465874000379, -3.500000000000000000, 0.000000000000000000 ) ) ;
#31664 = CARTESIAN_POINT ( 'NONE',  ( 18.12548987803202394, 0.2560590259361279486, -13.89684012171647787 ) ) ;
#31665 = CARTESIAN_POINT ( 'NONE',  ( 17.56537431432192520, -0.6249999662751110074, -12.67928921590352154 ) ) ;
#31666 = FACE_OUTER_BOUND ( 'NONE', #41184, .T. ) ;
#31667 = FACE_OUTER_BOUND ( 'NONE', #68456, .T. ) ;
#31668 = CARTESIAN_POINT ( 'NONE',  ( 24.11212143908326055, 12.52880557495846503, 3.383090514263496384 ) ) ;
#31669 = CARTESIAN_POINT ( 'NONE',  ( 9.633513540182331525, -2.750000000000000000, -7.663624617374467540 ) ) ;
#31670 = ORIENTED_EDGE ( 'NONE', *, *, #6885, .T. ) ;
#31671 = CARTESIAN_POINT ( 'NONE',  ( 7.612571400991003046, -4.588494467460999537, 6.486759529251004075 ) ) ;
#31672 = VERTEX_POINT ( 'NONE', #36274 ) ;
#31673 = CARTESIAN_POINT ( 'NONE',  ( 11.03856029907000114, 2.974095820320000083, 8.716122353065999917 ) ) ;
#31674 = LINE ( 'NONE', #43190, #41799 ) ;
#31675 = EDGE_CURVE ( 'NONE', #25788, #53930, #56281, .T. ) ;
#31676 = CARTESIAN_POINT ( 'NONE',  ( 10.90000000000000036, -8.091325576830000088, 7.077637346582999811 ) ) ;
#31677 = CARTESIAN_POINT ( 'NONE',  ( 8.639360841228999277, 5.074768364528000397, -8.296267706722000312 ) ) ;
#31678 = CARTESIAN_POINT ( 'NONE',  ( 10.08728840308773300, 2.899999999999999911, -6.305985889617788942 ) ) ;
#31679 = EDGE_CURVE ( 'NONE', #62706, #55241, #7550, .T. ) ;
#31680 = CARTESIAN_POINT ( 'NONE',  ( 25.36445294295100084, 2.635917447299000127, 11.32519224169999994 ) ) ;
#31681 = DIRECTION ( 'NONE',  ( -1.000000000000000000, 0.000000000000000000, 0.000000000000000000 ) ) ;
#31682 = CARTESIAN_POINT ( 'NONE',  ( 18.02496672415909629, 0.4121037244271885669, 13.89177745834280842 ) ) ;
#31683 = VERTEX_POINT ( 'NONE', #20537 ) ;
#31684 = CARTESIAN_POINT ( 'NONE',  ( 11.50001496185000249, 12.52500000000000036, 0.000000000000000000 ) ) ;
#31685 = CARTESIAN_POINT ( 'NONE',  ( 11.06733863405299800, -3.211524470605299886, 6.494205428462000107 ) ) ;
#31686 = CARTESIAN_POINT ( 'NONE',  ( 3.196806799210749617, -0.9161175952574931447, 3.408904368339101598 ) ) ;
#31687 = CARTESIAN_POINT ( 'NONE',  ( 17.94896392901328142, -0.4852513397796477945, -13.88859817538105013 ) ) ;
#31688 = CARTESIAN_POINT ( 'NONE',  ( 9.143918146793000190, -5.791549888895000109, 7.752110689268000954 ) ) ;
#31690 = CARTESIAN_POINT ( 'NONE',  ( 12.45594992591624361, -11.44468663792873642, 4.547234112432998465 ) ) ;
#31689 = DIRECTION ( 'NONE',  ( 1.000000000000000000, 0.000000000000000000, 0.000000000000000000 ) ) ;
#31691 = CARTESIAN_POINT ( 'NONE',  ( 11.01456785386839954, 3.053605396817899997, -8.136888821800198457 ) ) ;
#31692 = CARTESIAN_POINT ( 'NONE',  ( 25.41800046775599853, -11.20523436166000053, 3.227464342313000056 ) ) ;
#31693 = CARTESIAN_POINT ( 'NONE',  ( 10.23557120343299864, 3.957971921952620598, -8.365991721916298474 ) ) ;
#31694 = CARTESIAN_POINT ( 'NONE',  ( 17.91829918956259604, 0.6226057762474783708, 12.58460959628226483 ) ) ;
#31695 = B_SPLINE_SURFACE_WITH_KNOTS ( 'NONE', 3, 3, ( 
 ( #38637, #895, #12419, #1237, #7507, #65544, #64844, #28862, #37944, #16619, #60653, #54719, #17667, #22549, #50170, #11369, #32709, #54020, #43891, #49124, #6122, #49819, #38991, #27461, #65193, #6471, #60311, #12070, #48787, #23252, #38288, #44594, #39333, #27819, #22207 ),
 ( #16955, #59615, #33051, #17312, #33402, #55066, #7167, #12767, #2610, #61683, #18699, #60998, #13119, #66580, #61344, #36405, #40032, #29554, #13462, #50509, #19033, #34785, #25915, #68203, #2950, #56094, #20322, #50856, #36758, #40360, #58079, #8205, #47246, #10182, #41649 ),
 ( #52482, #9479, #35129, #62956, #24283, #45617, #15431, #30822, #52134, #68549, #15080, #52831, #57722, #4929, #4236, #9830, #31510, #31178, #4579, #23941, #26264, #56443, #20671, #25576, #46902, #41999, #66923, #13799, #18357, #66238, #63304, #39679, #34448, #55761, #7863 ),
 ( #45274, #29197, #68901, #47594, #43381, #58413, #6298, #65020, #17137, #64681, #63653, #59444, #10517, #26614, #21691, #59103, #47933, #21017, #374, #1072, #16109, #32207, #723, #53857, #54553, #33234, #37778, #15770, #32886, #48268, #31857, #5956, #37099, #53172, #53521 ) ),
 .UNSPECIFIED., .F., .F., .F.,
 ( 4, 4 ),
 ( 4, 1, 1, 1, 1, 1, 1, 1, 1, 1, 1, 1, 1, 1, 1, 1, 1, 1, 1, 1, 1, 1, 1, 1, 1, 1, 1, 1, 1, 1, 1, 1, 4 ),
 ( -0.1039086239011999951, 1.103908623900999864 ),
 ( -0.01933701211302999920, 0.01208563257065999909, 0.04350827725433999843, 0.07493092193802000645, 0.1063535666217000075, 0.1377762113054000204, 0.1691988559891000055, 0.2006215006727000150, 0.2320441453564000001, 0.2634667900400999851, 0.2948894347238000258, 0.3263120794074999553, 0.3577347240911999959, 0.3891573687748000054, 0.4205800134584999905, 0.4520026581421999756, 0.4834253028259000162, 0.5148479475096000568, 0.5462705921932000663, 0.5776932368768999959, 0.6091158815606000365, 0.6405385262443000771, 0.6719611709280000067, 0.7033838156117000473, 0.7348064602953000568, 0.7662291049789999864, 0.7976517496627000270, 0.8290743943464000676, 0.8604970390300999972, 0.8919196837138000378, 0.9233423283974000473, 0.9547649730810999769, 0.9861876177648000175 ),
 .UNSPECIFIED. ) ;
#31696 = CARTESIAN_POINT ( 'NONE',  ( 6.761992758735999587, -1.270688428506000056, -0.07976375540076000026 ) ) ;
#31697 = CARTESIAN_POINT ( 'NONE',  ( 24.33723497696300342, 8.940350178607999965, 9.046507324144998918 ) ) ;
#31698 = ORIENTED_EDGE ( 'NONE', *, *, #4863, .F. ) ;
#31699 = CARTESIAN_POINT ( 'NONE',  ( 8.662855646795000197, -2.741638482234999952, 6.457327039244000311 ) ) ;
#31700 = CARTESIAN_POINT ( 'NONE',  ( 8.971339158776000744, 4.082930418187999955, -6.104944817728999773 ) ) ;
#31701 = AXIS2_PLACEMENT_3D ( 'NONE', #64169, #43205, #6480 ) ;
#31702 = B_SPLINE_CURVE_WITH_KNOTS ( 'NONE', 3,
 ( #2945, #24278, #41727, #30901, #29890 ),
 .UNSPECIFIED., .F., .F.,
 ( 4, 1, 4 ),
 ( 0.000000000000000000, 0.3074238982151080157, 1.000000000000000000 ),
 .UNSPECIFIED. ) ;
#31703 = DIRECTION ( 'NONE',  ( 1.000000000000000000, 0.000000000000000000, 0.000000000000000000 ) ) ;
#31704 = DIRECTION ( 'NONE',  ( 1.000000000000000000, 0.000000000000000000, 0.000000000000000000 ) ) ;
#31705 = ORIENTED_EDGE ( 'NONE', *, *, #27387, .T. ) ;
#31706 = VECTOR ( 'NONE', #52400, 1000.000000000000000 ) ;
#31707 = CARTESIAN_POINT ( 'NONE',  ( 18.40156003475500057, 3.148349829928000165, 12.06792178657999948 ) ) ;
#31708 = CARTESIAN_POINT ( 'NONE',  ( 10.39969598649000027, 4.888000489779200208, 6.971269690999399415 ) ) ;
#31709 = CARTESIAN_POINT ( 'NONE',  ( 11.25809834123000108, 3.275514549383000240, -8.650774600386998969 ) ) ;
#31710 = EDGE_CURVE ( 'NONE', #44976, #21492, #2601, .T. ) ;
#31711 = VERTEX_POINT ( 'NONE', #63168 ) ;
#31712 = CARTESIAN_POINT ( 'NONE',  ( 23.60000000000000142, -0.9826167936418868099, -13.89473236361234676 ) ) ;
#31713 = CARTESIAN_POINT ( 'NONE',  ( 9.166037027449048580, -5.069767017855149938, -6.374457060939750619 ) ) ;
#31714 = CARTESIAN_POINT ( 'NONE',  ( 11.05964426047339799, 4.687693494822500639, 6.422784126663999338 ) ) ;
#31715 = CARTESIAN_POINT ( 'NONE',  ( 7.100000000000000533, -4.000000000000000000, 8.849999999999999645 ) ) ;
#31716 = CARTESIAN_POINT ( 'NONE',  ( 5.200000000000000178, 0.000000000000000000, 0.000000000000000000 ) ) ;
#31717 = EDGE_LOOP ( 'NONE', ( #43516, #25827, #48402, #56155, #66021, #63506, #60008, #61119 ) ) ;
#31718 = CARTESIAN_POINT ( 'NONE',  ( 17.55505043854144276, -0.6250000000000001110, 12.67928921589117586 ) ) ;
#31719 = CARTESIAN_POINT ( 'NONE',  ( 8.403354719590000244, 5.730434958826999825, -7.416203477251000820 ) ) ;
#31720 = CARTESIAN_POINT ( 'NONE',  ( 8.414009964596925073, -2.427229585700388270, 8.242459441677670640 ) ) ;
#31721 = VECTOR ( 'NONE', #15638, 1000.000000000000000 ) ;
#31722 = CARTESIAN_POINT ( 'NONE',  ( 10.77222057153667656, -3.695719232113590547, -8.319452754344771606 ) ) ;
#31723 = ORIENTED_EDGE ( 'NONE', *, *, #22466, .F. ) ;
#31724 = CARTESIAN_POINT ( 'NONE',  ( 15.95563772304700301, -3.878390400849000219, -11.75631652949000205 ) ) ;
#31725 = CARTESIAN_POINT ( 'NONE',  ( 11.44794916906000104, 11.60968724315999978, 1.479704744065999833 ) ) ;
#31726 = ORIENTED_EDGE ( 'NONE', *, *, #1566, .F. ) ;
#31727 = CARTESIAN_POINT ( 'NONE',  ( 8.798455008774128672, 4.948455060776569603, 7.263673592043552674 ) ) ;
#31728 = CARTESIAN_POINT ( 'NONE',  ( 10.57226862415000035, 9.951161148090999831, -5.461992367169999696 ) ) ;
#31729 = CIRCLE ( 'NONE', #64092, 11.84999999999999964 ) ;
#31730 = FACE_OUTER_BOUND ( 'NONE', #42816, .T. ) ;
#31731 = DIRECTION ( 'NONE',  ( 0.7071067784121117805, -0.5090965378051087731, 0.4907348766070088186 ) ) ;
#31732 = CARTESIAN_POINT ( 'NONE',  ( 9.837291465645295219, -2.697790585206812697, -7.971620370481231177 ) ) ;
#31733 = CARTESIAN_POINT ( 'NONE',  ( 11.23078751119019891, 3.084247107206000038, -7.979095341142500075 ) ) ;
#31734 = VECTOR ( 'NONE', #27067, 1000.000000000000114 ) ;
#31735 = CARTESIAN_POINT ( 'NONE',  ( 12.26077869730539938, -4.595338376575799799, 8.673950353177000139 ) ) ;
#31736 = CARTESIAN_POINT ( 'NONE',  ( 8.616995677562000466, -4.876077402042000131, 5.996974966533000106 ) ) ;
#31737 = CARTESIAN_POINT ( 'NONE',  ( 11.21503032197930061, -3.256621462143499901, 8.539569492647999027 ) ) ;
#31738 = ORIENTED_EDGE ( 'NONE', *, *, #37062, .F. ) ;
#31739 = CARTESIAN_POINT ( 'NONE',  ( 8.502045280412000139, 3.869396554003000421, 5.695652484872999466 ) ) ;
#31740 = EDGE_CURVE ( 'NONE', #16920, #18320, #9342, .T. ) ;
#31741 = ADVANCED_FACE ( 'NONE', ( #58283 ), #8356, .F. ) ;
#31742 = EDGE_LOOP ( 'NONE', ( #14277, #50678, #33406, #4474, #31935 ) ) ;
#31743 = LINE ( 'NONE', #14963, #51884 ) ;
#31744 = EDGE_CURVE ( 'NONE', #15298, #20015, #42219, .T. ) ;
#31745 = CARTESIAN_POINT ( 'NONE',  ( 8.910378124222624763, 5.351542105685659578, 7.263808684111331182 ) ) ;
#31746 = CARTESIAN_POINT ( 'NONE',  ( 11.12373268272000004, 5.763386772010999692, -5.184271159621000713 ) ) ;
#31747 = ORIENTED_EDGE ( 'NONE', *, *, #59509, .T. ) ;
#31748 = CARTESIAN_POINT ( 'NONE',  ( 12.18551697106549447, -2.583096739011645937, -12.43182067874258756 ) ) ;
#31749 = CARTESIAN_POINT ( 'NONE',  ( 17.98179591661069665, 3.334516285427552518, 11.16264808783946805 ) ) ;
#31750 = CARTESIAN_POINT ( 'NONE',  ( 23.60205915885299888, -9.361474752760003071, 7.912850866705011477 ) ) ;
#31751 = CARTESIAN_POINT ( 'NONE',  ( 8.969356963619999235, 2.880642974985999860, -7.499999999914821025 ) ) ;
#31752 = CARTESIAN_POINT ( 'NONE',  ( 12.38995319333359646, -1.919216742092435757, -13.86782799095450258 ) ) ;
#31753 = CARTESIAN_POINT ( 'NONE',  ( 10.65364694612719809, -4.804498860841600383, -7.821061011719899980 ) ) ;
#31754 = CARTESIAN_POINT ( 'NONE',  ( 18.49993212792200126, 2.908182645667999999, 12.18276646858999968 ) ) ;
#31755 = CARTESIAN_POINT ( 'NONE',  ( 18.21784200350680294, -2.188139590168308501, 12.40855205325248534 ) ) ;
#31756 = EDGE_LOOP ( 'NONE', ( #33817, #1213, #18060, #35864, #9030 ) ) ;
#31757 = ORIENTED_EDGE ( 'NONE', *, *, #68210, .F. ) ;
#31758 = AXIS2_PLACEMENT_3D ( 'NONE', #1946, #18372, #50183 ) ;
#31759 = DIRECTION ( 'NONE',  ( 1.000000000000000000, 0.000000000000000000, 0.000000000000000000 ) ) ;
#31760 = CARTESIAN_POINT ( 'NONE',  ( 23.66004879239100234, 3.393653897912999984, 13.50507458845999942 ) ) ;
#31761 = CARTESIAN_POINT ( 'NONE',  ( 11.94571737393083133, -5.011200127299592744, 6.726238946114239781 ) ) ;
#31762 = CARTESIAN_POINT ( 'NONE',  ( 10.16989991304999918, 2.594216849811000092, -6.291257009166999481 ) ) ;
#31763 = EDGE_CURVE ( 'NONE', #37125, #24359, #11754, .T. ) ;
#31764 = CARTESIAN_POINT ( 'NONE',  ( 17.80000000005199823, 3.345268251980999974, -11.86064071431999878 ) ) ;
#31765 = LINE ( 'NONE', #32112, #56263 ) ;
#31766 = CARTESIAN_POINT ( 'NONE',  ( 8.224593659958996383, 3.074059020428998146, -6.140725432342995838 ) ) ;
#31767 = CARTESIAN_POINT ( 'NONE',  ( 18.00302879683550117, -3.053770323303487189, -12.22453350000937888 ) ) ;
#31768 = ORIENTED_EDGE ( 'NONE', *, *, #55444, .F. ) ;
#31769 = CARTESIAN_POINT ( 'NONE',  ( 10.11501430098003773, -5.350017391163235381, -7.499999134156934311 ) ) ;
#31770 = CARTESIAN_POINT ( 'NONE',  ( 12.22356881520516758, -2.729361768173760083, 12.39519383931446228 ) ) ;
#31771 = CARTESIAN_POINT ( 'NONE',  ( 9.349051052051999378, -3.149129950522900234, -7.666517576877299511 ) ) ;
#31772 = CARTESIAN_POINT ( 'NONE',  ( 10.41185190929999926, 2.101586107686999938, 7.856266936613998553 ) ) ;
#31773 = CARTESIAN_POINT ( 'NONE',  ( 10.98791429143000009, -3.983006558652820051, 8.391963954669400039 ) ) ;
#31774 = CARTESIAN_POINT ( 'NONE',  ( 9.368660841232999914, 2.702406276695999754, -6.981052078638000147 ) ) ;
#31775 = MECHANICAL_DESIGN_GEOMETRIC_PRESENTATION_REPRESENTATION (  '', ( #472 ), #1625 ) ;
#31776 = CARTESIAN_POINT ( 'NONE',  ( 11.06165563537000018, 9.156947157375000756, -6.511651601598999584 ) ) ;
#31777 = CARTESIAN_POINT ( 'NONE',  ( 12.55608787177197172, -0.5733651658914331595, 12.68257300503909235 ) ) ;
#31778 = CARTESIAN_POINT ( 'NONE',  ( 5.624287198480453220, -12.11015306275925951, -3.744045437480271410 ) ) ;
#31779 = DIRECTION ( 'NONE',  ( 1.000000000000000000, 0.000000000000000000, 0.000000000000000000 ) ) ;
#31780 = CARTESIAN_POINT ( 'NONE',  ( 9.084331191192241306, -4.271986494075218133, 8.830896599738281338 ) ) ;
#31781 = ORIENTED_EDGE ( 'NONE', *, *, #21380, .F. ) ;
#31782 = CARTESIAN_POINT ( 'NONE',  ( 9.070310841232000598, 5.361622798585000460, -7.185294144754000634 ) ) ;
#31783 = CARTESIAN_POINT ( 'NONE',  ( 6.828954497519999833, -0.8705094924380000210, 0.8473603920708000503 ) ) ;
#31784 = CARTESIAN_POINT ( 'NONE',  ( 17.63806710036368841, 1.880187906035670764, 13.78549581173515115 ) ) ;
#31785 = CARTESIAN_POINT ( 'NONE',  ( 25.46373329105799854, 11.23406619596999967, -3.161081784610999978 ) ) ;
#31786 = CARTESIAN_POINT ( 'NONE',  ( 24.36504260745899941, 8.917410149216999926, -9.042893057505001053 ) ) ;
#31787 = VECTOR ( 'NONE', #46784, 1000.000000000000000 ) ;
#31788 = CARTESIAN_POINT ( 'NONE',  ( 11.13764426047339917, -3.386171819220400003, -8.461511872390000022 ) ) ;
#31789 = ORIENTED_EDGE ( 'NONE', *, *, #36929, .T. ) ;
#31790 = CARTESIAN_POINT ( 'NONE',  ( 5.666085114158424751, -12.07002994274972885, 3.732314430518076875 ) ) ;
#31791 = CARTESIAN_POINT ( 'NONE',  ( 10.51013099342176282, -2.732991197599094590, 6.289013820405174648 ) ) ;
#31794 = DIRECTION ( 'NONE',  ( 1.000000000000000000, 0.000000000000000000, 0.000000000000000000 ) ) ;
#31793 = CARTESIAN_POINT ( 'NONE',  ( 8.664129719593997692, 5.524776413195999325, -7.147585171405999915 ) ) ;
#31792 = PRODUCT_DEFINITION_CONTEXT ( 'detailed design', #20833, 'design' ) ;
#31795 = CARTESIAN_POINT ( 'NONE',  ( 10.79353630809276687, 2.899999999999999911, 6.665341197409489382 ) ) ;
#31796 = ADVANCED_FACE ( 'NONE', ( #43593, #39379 ), #22943, .T. ) ;
#31797 = ORIENTED_EDGE ( 'NONE', *, *, #701, .T. ) ;
#31798 = EDGE_CURVE ( 'NONE', #15587, #38721, #65992, .T. ) ;
#31799 = CARTESIAN_POINT ( 'NONE',  ( 9.701978494675000064, 3.399139198672999740, 6.026757051093999173 ) ) ;
#31800 = CARTESIAN_POINT ( 'NONE',  ( 18.02766551172502574, -2.090896903265579088, -13.75171326662667504 ) ) ;
#31801 = CARTESIAN_POINT ( 'NONE',  ( 11.12133729122639991, 3.134101783108900197, 7.522778681411049995 ) ) ;
#31802 = CARTESIAN_POINT ( 'NONE',  ( 10.42595817177000050, -5.042180160032999403, 8.702227297563000619 ) ) ;
#31803 = CARTESIAN_POINT ( 'NONE',  ( 7.550620559621999739, -4.468370631666999770, 8.882152684713000568 ) ) ;
#31804 = EDGE_LOOP ( 'NONE', ( #1657, #58980, #64089, #54843 ) ) ;
#31805 = CARTESIAN_POINT ( 'NONE',  ( 7.262114158771001193, 4.847807297114000491, 9.065373753110998578 ) ) ;
#31807 = CARTESIAN_POINT ( 'NONE',  ( 10.53198305961999992, -2.323723769066000422, -8.279488812962998878 ) ) ;
#31806 = CARTESIAN_POINT ( 'NONE',  ( 10.42760663304247615, 4.647051049978554005, -6.912280214781111098 ) ) ;
#31808 = CARTESIAN_POINT ( 'NONE',  ( 7.610024113606670859, -4.741952135465052010, 5.926164387956666779 ) ) ;
#31809 = CARTESIAN_POINT ( 'NONE',  ( 18.16417894366952979, -0.1413088920361047773, 13.89905105385967410 ) ) ;
#31810 = CARTESIAN_POINT ( 'NONE',  ( 24.42335568937500057, 3.752333166337999959, 12.53709289204000044 ) ) ;
#31811 = VERTEX_POINT ( 'NONE', #60700 ) ;
#31812 = CARTESIAN_POINT ( 'NONE',  ( 23.73953410686057452, 13.33634109980698845, 3.648241387586184103 ) ) ;
#31813 = CARTESIAN_POINT ( 'NONE',  ( 11.78533594839949927, -3.249987070165300196, 8.359517726022600570 ) ) ;
#31814 = CARTESIAN_POINT ( 'NONE',  ( 10.91307008594999850, 2.096286256021000050, 7.827189715349000210 ) ) ;
#31815 = CARTESIAN_POINT ( 'NONE',  ( 11.38379707368349969, 3.433355370490100533, 8.490052513816499058 ) ) ;
#31816 = PRODUCT_DEFINITION_FORMATION_WITH_SPECIFIED_SOURCE ( 'ANY', '', #56743, .NOT_KNOWN. ) ;
#31817 = ORIENTED_EDGE ( 'NONE', *, *, #20431, .T. ) ;
#31818 = CARTESIAN_POINT ( 'NONE',  ( 16.39999999379500295, -3.351248059343999941, -11.15756683833000018 ) ) ;
#31819 = CARTESIAN_POINT ( 'NONE',  ( 12.58695046962338182, 1.794129438118912345, -12.47161187386927672 ) ) ;
#31820 = CARTESIAN_POINT ( 'NONE',  ( 11.38813259637009878, -5.155817667926999803, 6.870201387206400057 ) ) ;
#31821 = B_SPLINE_CURVE_WITH_KNOTS ( 'NONE', 3,
 ( #19291, #35722, #62287, #40965 ),
 .UNSPECIFIED., .F., .F.,
 ( 4, 4 ),
 ( 0.000000000000000000, 1.000000000000000000 ),
 .UNSPECIFIED. ) ;
#31822 = CARTESIAN_POINT ( 'NONE',  ( 11.07729151584000071, 2.725326910309999739, -5.088622218232000449 ) ) ;
#31823 = CARTESIAN_POINT ( 'NONE',  ( 18.28005242394221241, -2.496404808517243890, 13.77565028140659287 ) ) ;
#31825 = ADVANCED_FACE ( 'NONE', ( #55810 ), #18406, .T. ) ;
#31824 = CARTESIAN_POINT ( 'NONE',  ( 18.15114771542447158, 2.688105180712813347, -13.63176637566754934 ) ) ;
#31826 = ORIENTED_EDGE ( 'NONE', *, *, #39187, .F. ) ;
#31827 = CARTESIAN_POINT ( 'NONE',  ( 7.100000000000000533, 5.349999999999999645, 7.500000000000000000 ) ) ;
#31828 = CARTESIAN_POINT ( 'NONE',  ( 9.610944094206999466, -5.100000000000000533, -6.571291218949999902 ) ) ;
#31829 = ORIENTED_EDGE ( 'NONE', *, *, #33312, .T. ) ;
#31830 = CARTESIAN_POINT ( 'NONE',  ( 9.416846873516664829, 3.231816600031355069, 6.500416447002274722 ) ) ;
#31832 = CARTESIAN_POINT ( 'NONE',  ( 10.64949279009019989, 3.739015461786900030, 6.531063508962500208 ) ) ;
#31831 = VECTOR ( 'NONE', #47347, 1000.000000000000000 ) ;
#31833 = CARTESIAN_POINT ( 'NONE',  ( 10.52462472184161157, -2.899999999999999911, -6.445686799303610215 ) ) ;
#31834 = CARTESIAN_POINT ( 'NONE',  ( 9.753031682810998859, 4.922927894835999574, -8.639534507509999628 ) ) ;
#31835 = FACE_OUTER_BOUND ( 'NONE', #31422, .T. ) ;
#31836 = CARTESIAN_POINT ( 'NONE',  ( 9.242349231304000767, -5.206700957550999931, 8.808818370147001531 ) ) ;
#31837 = CARTESIAN_POINT ( 'NONE',  ( 17.80382244274732173, 0.5734477787136645910, -12.68256797703446281 ) ) ;
#31838 = CARTESIAN_POINT ( 'NONE',  ( 9.005624905851385975, 5.254615185761620566, 7.997778784833124099 ) ) ;
#31839 = CARTESIAN_POINT ( 'NONE',  ( 10.42795525820099911, -4.094749303624469761, -6.501013802764199490 ) ) ;
#31840 = CARTESIAN_POINT ( 'NONE',  ( 7.956795280408998750, 4.524487726177000013, 9.047753146378999745 ) ) ;
#31841 = ORIENTED_EDGE ( 'NONE', *, *, #66706, .F. ) ;
#31842 =( NAMED_UNIT ( * ) PLANE_ANGLE_UNIT ( ) SI_UNIT ( $, .RADIAN. ) );
#31843 = CYLINDRICAL_SURFACE ( 'NONE', #28027, 1.250000000000000222 ) ;
#31844 = CARTESIAN_POINT ( 'NONE',  ( 9.242199581279592735, 2.679961688974304757, 7.218432988884748269 ) ) ;
#31845 = CARTESIAN_POINT ( 'NONE',  ( 10.32101354018304207, -4.768183399968640934, -6.500416447002272946 ) ) ;
#31846 = ADVANCED_FACE ( 'NONE', ( #39731 ), #61049, .F. ) ;
#31847 = CARTESIAN_POINT ( 'NONE',  ( 17.57925147499690155, 1.760911370824148392, 12.47634522799707568 ) ) ;
#31848 = B_SPLINE_CURVE_WITH_KNOTS ( 'NONE', 3,
 ( #39200, #55972, #49686, #45141, #1447, #7380, #39548, #60870, #61219, #66451, #1795, #66105, #60523, #34309, #54935, #23112, #18914, #50038 ),
 .UNSPECIFIED., .F., .F.,
 ( 4, 2, 2, 2, 2, 2, 2, 2, 4 ),
 ( 0.1280414556252505165, 0.2236515624513979450, 0.3192616692775453457, 0.4148717761036927465, 0.5104818829298402028, 0.6060919897559874370, 0.7017020965821346712, 0.7973122034082819054, 0.8929223102344291396 ),
 .UNSPECIFIED. ) ;
#31849 = DIRECTION ( 'NONE',  ( -1.000000000000000000, 0.000000000000000000, 0.000000000000000000 ) ) ;
#31850 = CARTESIAN_POINT ( 'NONE',  ( 11.06995268536000054, 8.134787565625000383, 6.681297597381000486 ) ) ;
#31851 = CARTESIAN_POINT ( 'NONE',  ( -0.2999999999999999889, 1.154700538379000108, 0.000000000000000000 ) ) ;
#31852 = CARTESIAN_POINT ( 'NONE',  ( 0.07500022993665000914, 0.000000000000000000, 0.000000000000000000 ) ) ;
#31853 = EDGE_LOOP ( 'NONE', ( #50125, #21238, #47960, #9326 ) ) ;
#31854 = CARTESIAN_POINT ( 'NONE',  ( 24.66122485234200212, 8.759220508654999904, 9.243943008462998989 ) ) ;
#31855 = CARTESIAN_POINT ( 'NONE',  ( 9.659038493598998798, -3.074215132699300135, -6.617216466537199970 ) ) ;
#31856 = DIRECTION ( 'NONE',  ( 0.000000000000000000, 0.000000000000000000, 1.000000000000000000 ) ) ;
#31857 = CARTESIAN_POINT ( 'NONE',  ( 10.81316193496000011, -3.756072284922999938, 6.071597915422999314 ) ) ;
#31858 = CARTESIAN_POINT ( 'NONE',  ( 12.23671932425159881, -4.127012898954600217, 6.643164954553199664 ) ) ;
#31859 = B_SPLINE_SURFACE_WITH_KNOTS ( 'NONE', 3, 3, ( 
 ( #5930, #27272, #1731, #60120 ),
 ( #12226, #38444, #44047, #22010 ),
 ( #1049, #64658, #43357, #49626 ),
 ( #44400, #348, #11517, #54174 ),
 ( #17110, #65352, #21665, #42999 ),
 ( #6272, #64307, #16425, #22361 ) ),
 .UNSPECIFIED., .F., .F., .F.,
 ( 4, 1, 1, 4 ),
 ( 4, 4 ),
 ( -0.007877447430640999518, 0.000000000000000000, 0.07142857142856999519, 0.1006818857400000045 ),
 ( -0.1835627100093999986, 1.183562709872999941 ),
 .UNSPECIFIED. ) ;
#31860 = CARTESIAN_POINT ( 'NONE',  ( 8.719914745407999490, 3.934662526658240012, 6.596431033727998994 ) ) ;
#31861 = B_SPLINE_CURVE_WITH_KNOTS ( 'NONE', 3,
 ( #64524, #45301, #50537, #20012 ),
 .UNSPECIFIED., .F., .F.,
 ( 4, 4 ),
 ( 0.000000000000000000, 1.000000000000000000 ),
 .UNSPECIFIED. ) ;
#31862 = CARTESIAN_POINT ( 'NONE',  ( 0.4417688295323000114, -3.296907118028000294, 0.7152224222591000435 ) ) ;
#31863 = CARTESIAN_POINT ( 'NONE',  ( 4.544632850966807247, 1.083163139203730418, -0.5129437623365981080 ) ) ;
#31864 = CARTESIAN_POINT ( 'NONE',  ( 12.08418858410074748, 2.401692437127234125, 12.36899414651120566 ) ) ;
#31866 = DIRECTION ( 'NONE',  ( -1.000000000000000000, 0.000000000000000000, 0.000000000000000000 ) ) ;
#31865 = CARTESIAN_POINT ( 'NONE',  ( 9.758342523874999230, 2.871335344632000020, -7.327226901081999699 ) ) ;
#31867 = CARTESIAN_POINT ( 'NONE',  ( 10.30072469555899950, 4.570852684939899824, -6.512367818249299667 ) ) ;
#31868 = CARTESIAN_POINT ( 'NONE',  ( 7.686616257283001907, 3.172402717919002413, -6.371572564913001280 ) ) ;
#31869 = CARTESIAN_POINT ( 'NONE',  ( 10.43325471958999984, 5.596203146559000530, -8.042024377770999877 ) ) ;
#31870 = CARTESIAN_POINT ( 'NONE',  ( 9.453329965421998438, 3.111510091554099855, -8.420309768537698858 ) ) ;
#31872 = CARTESIAN_POINT ( 'NONE',  ( 12.27404183471215937, 2.829784922027013483, 12.36859113741106420 ) ) ;
#31871 = CARTESIAN_POINT ( 'NONE',  ( 17.68432968562860808, -11.86180690035067187, 3.298554102281288980 ) ) ;
#31873 = CARTESIAN_POINT ( 'NONE',  ( 10.10107565221368375, 5.349884357715816385, -7.263395957186810747 ) ) ;
#31874 = EDGE_LOOP ( 'NONE', ( #62058, #37226, #65347, #9419 ) ) ;
#31875 = MANIFOLD_SOLID_BREP ( 'Stock-MAS-678-1', #11304 ) ;
#31876 = CARTESIAN_POINT ( 'NONE',  ( 12.80505043854144276, 0.6249999999999994449, 12.67928921589117586 ) ) ;
#31877 = CARTESIAN_POINT ( 'NONE',  ( 10.22726354018266370, 4.629523725463627670, 8.592232985442818105 ) ) ;
#31878 = AXIS2_PLACEMENT_3D ( 'NONE', #22131, #53942, #11988 ) ;
#31879 = CARTESIAN_POINT ( 'NONE',  ( 10.97865453029000093, -5.273142482194999481, 7.958032781726000593 ) ) ;
#31880 = CARTESIAN_POINT ( 'NONE',  ( 9.855633995697999694, 4.861719613449499988, 7.404358731173799946 ) ) ;
#31881 = EDGE_CURVE ( 'NONE', #252, #19259, #39259, .T. ) ;
#31882 = EDGE_CURVE ( 'NONE', #53057, #61390, #36783, .T. ) ;
#31883 = CARTESIAN_POINT ( 'NONE',  ( 23.61761589919547433, -3.310052744450573847, -13.56819651954416628 ) ) ;
#31884 = CARTESIAN_POINT ( 'NONE',  ( 12.19646863228101452, -2.642680340209514256, 13.64216715890481524 ) ) ;
#31885 = CARTESIAN_POINT ( 'NONE',  ( 12.21224535002822442, 2.300944246528859871, 13.71363154654899041 ) ) ;
#31886 = CARTESIAN_POINT ( 'NONE',  ( 9.518359312500532354, -5.126777126183463373, -6.752018918868714970 ) ) ;
#31887 = VERTEX_POINT ( 'NONE', #54764 ) ;
#31888 = ADVANCED_FACE ( 'NONE', ( #23639 ), #50201, .T. ) ;
#31889 = EDGE_CURVE ( 'NONE', #44668, #9687, #51780, .T. ) ;
#31890 = CARTESIAN_POINT ( 'NONE',  ( 4.969048069769999465, 0.2814927992946000268, -1.098939332150999926 ) ) ;
#31891 = CARTESIAN_POINT ( 'NONE',  ( 9.174709346416998201, -2.844451673749999632, -6.951281079990299538 ) ) ;
#31892 = CARTESIAN_POINT ( 'NONE',  ( 9.710765758303409712, -3.646727114448458984, -8.814525660484084923 ) ) ;
#31893 = CARTESIAN_POINT ( 'NONE',  ( 23.56665676678700194, 2.935519496638999914, -13.67844162499000049 ) ) ;
#31894 = CARTESIAN_POINT ( 'NONE',  ( 18.14163091156140695, 2.284010751868936762, -12.49929939428933601 ) ) ;
#31895 = CARTESIAN_POINT ( 'NONE',  ( 9.793111399473126255, -5.011294126480321687, 8.251846359484561688 ) ) ;
#31896 = CARTESIAN_POINT ( 'NONE',  ( 18.17508965102116036, 2.579233224688229242, 12.43275545429011686 ) ) ;
#31897 = DIRECTION ( 'NONE',  ( 0.7071060218674898312, 0.7071075405047898554, -8.464222916703876687E-10 ) ) ;
#31898 = CARTESIAN_POINT ( 'NONE',  ( 10.26694555961999988, -5.500014128486999887, -6.419508248405999318 ) ) ;
#31899 = CARTESIAN_POINT ( 'NONE',  ( 4.855026506350000659, 1.500000000000000000, 0.000000000000000000 ) ) ;
#31900 = CARTESIAN_POINT ( 'NONE',  ( 24.30000000000000071, 8.810505093353000916, 8.810505093353000916 ) ) ;
#31901 = DIRECTION ( 'NONE',  ( -1.000000000000000000, -0.000000000000000000, -0.000000000000000000 ) ) ;
#31902 = CARTESIAN_POINT ( 'NONE',  ( 7.000000000000000000, 0.6646153846154000400, -2.616923076922999858 ) ) ;
#31903 = FACE_OUTER_BOUND ( 'NONE', #49192, .T. ) ;
#31904 = EDGE_LOOP ( 'NONE', ( #4397, #19770, #3942, #29111, #15994 ) ) ;
#31905 = CARTESIAN_POINT ( 'NONE',  ( 8.605545280412000508, 3.122811675949999977, -6.006064052396999919 ) ) ;
#31906 = CARTESIAN_POINT ( 'NONE',  ( 12.23256516821459883, -3.293702443348299980, 6.787191910456499500 ) ) ;
#31907 = ORIENTED_EDGE ( 'NONE', *, *, #8608, .F. ) ;
#31908 = MECHANICAL_DESIGN_GEOMETRIC_PRESENTATION_REPRESENTATION (  '', ( #32994 ), #21857 ) ;
#31909 = CARTESIAN_POINT ( 'NONE',  ( 11.09999999999999964, 5.299999999999999822, 5.160242730440000258 ) ) ;
#31910 = CARTESIAN_POINT ( 'NONE',  ( 10.62072335273219892, -3.602909566644000083, -8.569396700949999612 ) ) ;
#31911 = ORIENTED_EDGE ( 'NONE', *, *, #61407, .F. ) ;
#31912 = CARTESIAN_POINT ( 'NONE',  ( 11.83003632436370012, 2.756744593645999775, 7.790336465152099876 ) ) ;
#31913 = CARTESIAN_POINT ( 'NONE',  ( 23.89491988614704709, 3.335475672761040844, -12.94525074951522647 ) ) ;
#31914 = AXIS2_PLACEMENT_3D ( 'NONE', #65036, #21707, #54569 ) ;
#31915 = CARTESIAN_POINT ( 'NONE',  ( 9.849204462306733632, -2.899999999999999911, -6.662590550601113826 ) ) ;
#31916 = CARTESIAN_POINT ( 'NONE',  ( 10.65413259636999932, -4.783377755405500587, -7.926858177843299380 ) ) ;
#31917 = CARTESIAN_POINT ( 'NONE',  ( 12.37275480865975830, 0.4515881962949890860, -13.89013012614793041 ) ) ;
#31918 = CARTESIAN_POINT ( 'NONE',  ( 7.000000000000000888, -7.162101251533245616, -3.226271710805416415 ) ) ;
#31919 = CARTESIAN_POINT ( 'NONE',  ( 12.96937411412500119, 11.64648275985999959, 1.863025408066000033 ) ) ;
#31920 = ORIENTED_EDGE ( 'NONE', *, *, #35696, .T. ) ;
#31921 = CARTESIAN_POINT ( 'NONE',  ( 9.269210841233000764, 3.098073081301000009, -8.567513114264999174 ) ) ;
#31922 = VERTEX_POINT ( 'NONE', #63439 ) ;
#31923 = B_SPLINE_CURVE_WITH_KNOTS ( 'NONE', 3,
 ( #48739, #38587, #58879, #22849 ),
 .UNSPECIFIED., .F., .F.,
 ( 4, 4 ),
 ( 0.000000000000000000, 1.000000000000000000 ),
 .UNSPECIFIED. ) ;
#31924 = CARTESIAN_POINT ( 'NONE',  ( 10.71684687351633869, 4.768183399968648040, -6.500416447002277387 ) ) ;
#31925 = FILL_AREA_STYLE_COLOUR ( '', #48816 ) ;
#31926 = ORIENTED_EDGE ( 'NONE', *, *, #57431, .F. ) ;
#31927 = CARTESIAN_POINT ( 'NONE',  ( 9.529317406968999649, 4.237919115995800290, 6.243107450209000042 ) ) ;
#31928 = CARTESIAN_POINT ( 'NONE',  ( 17.98035626696893985, -2.958002308262751789, -12.33297292539930368 ) ) ;
#31929 = AXIS2_PLACEMENT_3D ( 'NONE', #31323, #20478, #14557 ) ;
#31930 = ADVANCED_FACE ( 'NONE', ( #54682 ), #422, .T. ) ;
#31931 = DIRECTION ( 'NONE',  ( -1.000000000000000000, 0.000000000000000000, 0.000000000000000000 ) ) ;
#31932 = EDGE_CURVE ( 'NONE', #53410, #10995, #7163, .T. ) ;
#31933 = PLANE ( 'NONE',  #54767 ) ;
#31934 = CARTESIAN_POINT ( 'NONE',  ( 12.18107303550439902, -0.04113803725886359952, 13.89993798560270832 ) ) ;
#31935 = ORIENTED_EDGE ( 'NONE', *, *, #11821, .F. ) ;
#31936 = CARTESIAN_POINT ( 'NONE',  ( 12.46470380486700158, 12.15408297959000095, -3.184072412108000183 ) ) ;
#31937 = CARTESIAN_POINT ( 'NONE',  ( 18.35475438412399996, 11.75582082520000071, -3.881266971570000113 ) ) ;
#31938 = CARTESIAN_POINT ( 'NONE',  ( 9.682824781140627834, 3.392296711160748490, 6.870532779523098377 ) ) ;
#31939 = CARTESIAN_POINT ( 'NONE',  ( 8.863694533038728451, 4.511314481744639338, 8.385421723231823776 ) ) ;
#31940 = CARTESIAN_POINT ( 'NONE',  ( 8.549914158773001205, 2.141799395716999843, -7.895788736628000848 ) ) ;
#31941 = CARTESIAN_POINT ( 'NONE',  ( 17.79290994143500271, -3.413161104324000217, 11.89755508104000015 ) ) ;
#31942 = CARTESIAN_POINT ( 'NONE',  ( 10.81362580514000094, -3.876947229615999913, -9.022210119840998743 ) ) ;
#31943 = VERTEX_POINT ( 'NONE', #853 ) ;
#31944 = ORIENTED_EDGE ( 'NONE', *, *, #64155, .T. ) ;
#31945 = DIRECTION ( 'NONE',  ( -1.000000000000000000, 0.000000000000000000, 0.000000000000000000 ) ) ;
#31946 = DIRECTION ( 'NONE',  ( -0.000000000000000000, 0.7071067811865475727, 0.7071067811865475727 ) ) ;
#31947 = LINE ( 'NONE', #65111, #21827 ) ;
#31948 = CARTESIAN_POINT ( 'NONE',  ( 12.27416439418442096, -2.829982835910819006, 13.59791655269246924 ) ) ;
#31949 = CARTESIAN_POINT ( 'NONE',  ( 0.2000000000000000389, 0.000000000000000000, 0.000000000000000000 ) ) ;
#31950 = CARTESIAN_POINT ( 'NONE',  ( 11.30367835872029936, 2.886444435522000251, -6.798177532456199934 ) ) ;
#31951 = CARTESIAN_POINT ( 'NONE',  ( 9.206076168957999073, 3.560025096655699883, -8.247081005603298820 ) ) ;
#31953 = CARTESIAN_POINT ( 'NONE',  ( 4.399647091626817996, 1.427585134858555760, -0.03664101042030128152 ) ) ;
#31952 = CARTESIAN_POINT ( 'NONE',  ( 10.12968422950999958, -4.708027397558999461, 8.212418068717900255 ) ) ;
#31954 = B_SPLINE_CURVE_WITH_KNOTS ( 'NONE', 3,
 ( #5461, #14581, #68385, #20505 ),
 .UNSPECIFIED., .F., .F.,
 ( 4, 4 ),
 ( 0.000000000000000000, 1.000000000000000000 ),
 .UNSPECIFIED. ) ;
#31955 = CARTESIAN_POINT ( 'NONE',  ( 4.794609839683333874, 1.500000000000001110, -0.1963495408493590721 ) ) ;
#31956 = ORIENTED_EDGE ( 'NONE', *, *, #39785, .F. ) ;
#31957 = CARTESIAN_POINT ( 'NONE',  ( 11.36749010443639918, -3.136214309321499805, -7.564597762509089662 ) ) ;
#31958 = AXIS2_PLACEMENT_3D ( 'NONE', #42926, #26161, #53072 ) ;
#31959 = CARTESIAN_POINT ( 'NONE',  ( 10.31664229535000032, -3.425746660654999776, -4.565089086486000092 ) ) ;
#31960 = CARTESIAN_POINT ( 'NONE',  ( 10.41891290906799838, 3.190593056227700064, 6.509421987543800192 ) ) ;
#31961 = CARTESIAN_POINT ( 'NONE',  ( 8.200000304434999165, -12.49999969551000056, 3.568585274154000017E-10 ) ) ;
#31962 = ADVANCED_FACE ( 'NONE', ( #22510 ), #30627, .F. ) ;
#31963 = CARTESIAN_POINT ( 'NONE',  ( 9.719606904206999687, -5.967761543230999166, 7.406644089178000101 ) ) ;
#31964 = CARTESIAN_POINT ( 'NONE',  ( 17.83355475039667226, 3.059894173695237640, -12.30333952404643227 ) ) ;
#31965 = FACE_OUTER_BOUND ( 'NONE', #51866, .T. ) ;
#31966 = EDGE_CURVE ( 'NONE', #44325, #61815, #52980, .T. ) ;
#31967 = EDGE_CURVE ( 'NONE', #22650, #35088, #65114, .T. ) ;
#31968 = B_SPLINE_CURVE_WITH_KNOTS ( 'NONE', 3,
 ( #40663, #8168, #41013, #25275 ),
 .UNSPECIFIED., .F., .F.,
 ( 4, 4 ),
 ( 0.000000000000000000, 1.000000000000000000 ),
 .UNSPECIFIED. ) ;
#31969 = CARTESIAN_POINT ( 'NONE',  ( 17.80000000001300009, 3.351264566333000072, 11.15757590352999884 ) ) ;
#31970 = CARTESIAN_POINT ( 'NONE',  ( 5.555026506349999948, -1.500000000000000000, 0.000000000000000000 ) ) ;
#31971 = CARTESIAN_POINT ( 'NONE',  ( 9.155417874594000693, -4.797903641662700558, -7.839201596587598964 ) ) ;
#31972 = VECTOR ( 'NONE', #9507, 1000.000000000000000 ) ;
#31973 = B_SPLINE_CURVE_WITH_KNOTS ( 'NONE', 3,
 ( #44686, #29291, #61435, #34538 ),
 .UNSPECIFIED., .F., .F.,
 ( 4, 4 ),
 ( 0.000000000000000000, 1.000000000000000000 ),
 .UNSPECIFIED. ) ;
#31974 = CARTESIAN_POINT ( 'NONE',  ( 6.103305643943999215, -0.8669997925267000083, 1.185259004083000001 ) ) ;
#31975 = CARTESIAN_POINT ( 'NONE',  ( 11.37068169682077645, -3.126090202221432079, 7.519268307021759412 ) ) ;
#31976 = CARTESIAN_POINT ( 'NONE',  ( 8.761230081853241813, 4.521411717137521435, -8.281074114623761417 ) ) ;
#31977 = VERTEX_POINT ( 'NONE', #64807 ) ;
#31978 = CARTESIAN_POINT ( 'NONE',  ( 12.18532624936142206, -0.08167875237853008952, -12.69965198491187230 ) ) ;
#31979 = CARTESIAN_POINT ( 'NONE',  ( 10.02462472190973486, -2.899999999999999911, -6.445686799157789082 ) ) ;
#31980 = DIRECTION ( 'NONE',  ( -3.667764737047155134E-10, -0.9466472399347399813, 0.3222716294121134584 ) ) ;
#31981 = CARTESIAN_POINT ( 'NONE',  ( 4.699998537092440642, -13.17499999999999893, 0.000000000000000000 ) ) ;
#31982 = CARTESIAN_POINT ( 'NONE',  ( 10.34423739839300715, 2.685214518267480699, -7.853261023685005782 ) ) ;
#31983 = EDGE_LOOP ( 'NONE', ( #38206, #52338, #29972, #59312, #36432, #42166, #63428, #24659, #48050, #55558, #55254 ) ) ;
#31984 = CARTESIAN_POINT ( 'NONE',  ( 25.48370107584300470, -11.09850929439999945, -3.318324248302000345 ) ) ;
#31985 = CARTESIAN_POINT ( 'NONE',  ( 11.60988784977536348, -4.851105903694400645, -7.451365240271489832 ) ) ;
#31986 = CARTESIAN_POINT ( 'NONE',  ( 10.81905590578999998, 2.899999999999999911, -6.571291218949999902 ) ) ;
#31987 = ADVANCED_FACE ( 'NONE', ( #22170 ), #11110, .F. ) ;
#31988 = DIRECTION ( 'NONE',  ( -1.000000000000000000, 0.000000000000000000, 0.000000000000000000 ) ) ;
#31989 = CARTESIAN_POINT ( 'NONE',  ( 5.399999743830999677, 12.99045401563999924, 1.690592933733000125 ) ) ;
#31990 = CARTESIAN_POINT ( 'NONE',  ( 10.77879632507499785, 4.423544049216699747, -8.285174533868300273 ) ) ;
#31991 = ORIENTED_EDGE ( 'NONE', *, *, #29545, .T. ) ;
#31992 = MANIFOLD_SOLID_BREP ( 'Stock-MAS-678-1', #53734 ) ;
#31993 = CARTESIAN_POINT ( 'NONE',  ( 10.83659005484000026, -5.133183563847000030, 8.848364935581999546 ) ) ;
#31994 = CARTESIAN_POINT ( 'NONE',  ( 8.790860954911998704, -3.902433532469449684, -8.421893466755800972 ) ) ;
#31995 = VERTEX_POINT ( 'NONE', #17276 ) ;
#31996 = CARTESIAN_POINT ( 'NONE',  ( 13.70006033574439108, 11.41449502534878491, 2.331043471729913108 ) ) ;
#31997 = CARTESIAN_POINT ( 'NONE',  ( 7.737831853206999178, -5.687202994508999687, 6.847270485579000088 ) ) ;
#31998 = CARTESIAN_POINT ( 'NONE',  ( 15.95481756226799952, 8.457314961363000094, 8.223455601337001042 ) ) ;
#31999 = VERTEX_POINT ( 'NONE', #38959 ) ;
#32000 = LINE ( 'NONE', #37232, #58745 ) ;
#32001 = B_SPLINE_CURVE_WITH_KNOTS ( 'NONE', 3,
 ( #25009, #20795, #9959, #4011 ),
 .UNSPECIFIED., .F., .F.,
 ( 4, 4 ),
 ( 0.8929223102344291396, 1.000000000000000000 ),
 .UNSPECIFIED. ) ;
#32002 = B_SPLINE_CURVE_WITH_KNOTS ( 'NONE', 3,
 ( #49335, #7381, #38149, #22765, #17171, #22067, #43417, #11931 ),
 .UNSPECIFIED., .F., .F.,
 ( 4, 2, 2, 4 ),
 ( 0.000000000000000000, 0.1253882094777247769, 0.2507764189554495537, 0.5015528379108959989 ),
 .UNSPECIFIED. ) ;
#32003 = CARTESIAN_POINT ( 'NONE',  ( 18.18005043824376443, -1.329523415562850021E-10, -12.70000000088146486 ) ) ;
#32004 = CARTESIAN_POINT ( 'NONE',  ( 9.479346873516668381, -3.836375382625532904, -8.749999999999998224 ) ) ;
#32005 = LINE ( 'NONE', #42146, #3865 ) ;
#32006 = EDGE_LOOP ( 'NONE', ( #57069, #37855, #748, #54602 ) ) ;
#32007 = CARTESIAN_POINT ( 'NONE',  ( 10.49785673611999925, -3.776281940467000275, 5.717636230565000588 ) ) ;
#32008 = CARTESIAN_POINT ( 'NONE',  ( 11.60000000000000497, 3.695216987067942327, 8.455673667202294297 ) ) ;
#32009 = CARTESIAN_POINT ( 'NONE',  ( 25.59997239626699894, 8.218962773316999204, -8.043525096612999192 ) ) ;
#32010 = ORIENTED_EDGE ( 'NONE', *, *, #67909, .T. ) ;
#32011 = CIRCLE ( 'NONE', #44297, 13.89999852641999922 ) ;
#32012 = CARTESIAN_POINT ( 'NONE',  ( 11.07299956498199833, 5.207010770456999893, 7.174999999999999822 ) ) ;
#32013 = CARTESIAN_POINT ( 'NONE',  ( 11.25809194037999994, -3.275508415657999883, -8.650784343212000849 ) ) ;
#32014 = ORIENTED_EDGE ( 'NONE', *, *, #28113, .T. ) ;
#32015 = CARTESIAN_POINT ( 'NONE',  ( 23.56860850335619162, -10.31977020530763944, 9.444771763729463032 ) ) ;
#32016 = DIRECTION ( 'NONE',  ( 1.000000000000000000, 0.000000000000000000, 0.000000000000000000 ) ) ;
#32017 = CARTESIAN_POINT ( 'NONE',  ( 5.229588072192999704, 1.415830339355000023, -0.04300091695264000174 ) ) ;
#32018 = AXIS2_PLACEMENT_3D ( 'NONE', #22009, #16761, #16079 ) ;
#32019 = CARTESIAN_POINT ( 'NONE',  ( 7.907275465492005218, 4.844754857023993999, -6.256456030303002791 ) ) ;
#32020 = DIRECTION ( 'NONE',  ( 0.000000000000000000, -1.000000000000000000, 0.000000000000000000 ) ) ;
#32021 = DIRECTION ( 'NONE',  ( 0.000000000000000000, 0.000000000000000000, -1.000000000000000000 ) ) ;
#32022 = CARTESIAN_POINT ( 'NONE',  ( 23.79457312070770669, 13.02989123031758645, 3.714539862624964162 ) ) ;
#32023 = EDGE_CURVE ( 'NONE', #43600, #26545, #40694, .T. ) ;
#32024 = ORIENTED_EDGE ( 'NONE', *, *, #59063, .T. ) ;
#32025 = CARTESIAN_POINT ( 'NONE',  ( 13.17784398560648995, -12.38705052588331412, -1.853828488290533816 ) ) ;
#32026 = ORIENTED_EDGE ( 'NONE', *, *, #59174, .T. ) ;
#32027 = CARTESIAN_POINT ( 'NONE',  ( 10.18908827523999960, 5.907871695079999874, 7.801541097952000570 ) ) ;
#32028 = CARTESIAN_POINT ( 'NONE',  ( 10.64556415877000006, 2.988929467935999895, -5.952329570726999641 ) ) ;
#32029 = CARTESIAN_POINT ( 'NONE',  ( 18.14404865540673129, -11.59829761222289690, 4.728902891304503697 ) ) ;
#32030 = AXIS2_PLACEMENT_3D ( 'NONE', #16993, #11069, #21892 ) ;
#32031 = CARTESIAN_POINT ( 'NONE',  ( 8.921135841230999119, 3.292387953886000140, -6.294868737226000377 ) ) ;
#32032 = CARTESIAN_POINT ( 'NONE',  ( 24.62769666370824950, -12.35739842162390367, -2.995926059522363794 ) ) ;
#32033 = CARTESIAN_POINT ( 'NONE',  ( 18.17981516808187337, -0.01996689158402818742, 13.89998575767904043 ) ) ;
#32034 = CARTESIAN_POINT ( 'NONE',  ( 18.05194946931286282, 0.3792369704146499876, 13.89303997536584667 ) ) ;
#32035 = EDGE_LOOP ( 'NONE', ( #35237, #50228, #50242, #35256 ) ) ;
#32036 = DIRECTION ( 'NONE',  ( -1.000000000000000000, -0.000000000000000000, -0.000000000000000000 ) ) ;
#32037 = CARTESIAN_POINT ( 'NONE',  ( 11.63349010443640097, -2.725546193138000284, 7.404690636538299842 ) ) ;
#32038 = CARTESIAN_POINT ( 'NONE',  ( 16.09992084546400193, 8.991497430826001391, 8.719551690569000257 ) ) ;
#32039 = CARTESIAN_POINT ( 'NONE',  ( 8.758793146794999984, -3.977267280662000193, 9.308921106447000327 ) ) ;
#32041 = DIRECTION ( 'NONE',  ( -1.000000000000000000, 0.000000000000000000, 0.000000000000000000 ) ) ;
#32040 = CARTESIAN_POINT ( 'NONE',  ( 13.99999999347100044, 9.187456302440001110, 8.213201953411001455 ) ) ;
#32042 = CARTESIAN_POINT ( 'NONE',  ( 11.03918313518939875, 3.292400735470800033, -8.394758848575399668 ) ) ;
#32043 = DIRECTION ( 'NONE',  ( 1.000000000000000000, 0.000000000000000000, 0.000000000000000000 ) ) ;
#32044 = CARTESIAN_POINT ( 'NONE',  ( 9.956950584426998319, 4.344127791340399725, -6.704208565179699875 ) ) ;
#32045 = CARTESIAN_POINT ( 'NONE',  ( 18.16373151406918396, -0.1422617729927601882, 12.69893308522357245 ) ) ;
#32046 = CARTESIAN_POINT ( 'NONE',  ( 7.106613235374000581, 1.094478228765999983, 0.2906167377007999875 ) ) ;
#32047 = DIRECTION ( 'NONE',  ( 0.000000000000000000, 0.000000000000000000, -1.000000000000000000 ) ) ;
#32048 = ORIENTED_EDGE ( 'NONE', *, *, #29936, .T. ) ;
#32049 = CARTESIAN_POINT ( 'NONE',  ( 8.791230646795000325, -5.095088356574999366, 6.286978111459999852 ) ) ;
#32050 = CARTESIAN_POINT ( 'NONE',  ( 9.026933059621999433, -4.852736108563000528, 8.683927195503999386 ) ) ;
#32051 = ADVANCED_FACE ( 'NONE', ( #16918 ), #59576, .F. ) ;
#32052 = EDGE_CURVE ( 'NONE', #68446, #11689, #32570, .T. ) ;
#32053 = FACE_OUTER_BOUND ( 'NONE', #44031, .T. ) ;
#32054 = DIRECTION ( 'NONE',  ( -1.000000000000000000, 0.000000000000000000, 0.000000000000000000 ) ) ;
#32055 = B_SPLINE_CURVE_WITH_KNOTS ( 'NONE', 3,
 ( #11228, #22055, #48984, #21713, #28357, #43048, #49320, #1091, #64351, #33601, #23098, #49673, #1782, #32564, #17158, #5977 ),
 .UNSPECIFIED., .F., .F.,
 ( 4, 2, 2, 2, 2, 2, 2, 4 ),
 ( 0.000000000000000000, 0.06250000000000084655, 0.1250000000000016931, 0.2500000000000031641, 0.5000000000000033307, 0.7500000000000034417, 0.8750000000000017764, 1.000000000000000000 ),
 .UNSPECIFIED. ) ;
#32056 = ORIENTED_EDGE ( 'NONE', *, *, #62037, .T. ) ;
#32057 = CARTESIAN_POINT ( 'NONE',  ( 0.8092604209659999270, 2.983562695318000113, -1.348686013867999911 ) ) ;
#32058 = CARTESIAN_POINT ( 'NONE',  ( 10.86190547754509872, 4.891676932241900033, 7.471700551735359852 ) ) ;
#32059 = CARTESIAN_POINT ( 'NONE',  ( 10.50084834123000022, 4.616783736607999344, -6.288082254674000282 ) ) ;
#32060 = ORIENTED_EDGE ( 'NONE', *, *, #744, .T. ) ;
#32061 = CARTESIAN_POINT ( 'NONE',  ( 12.54953071380263019, -0.6732419856523256252, -12.58200148172923605 ) ) ;
#32062 = CARTESIAN_POINT ( 'NONE',  ( 10.99664311227126312, -3.555960431980461411, -8.706333095531745059 ) ) ;
#32063 = CARTESIAN_POINT ( 'NONE',  ( 17.82398025068293990, 3.148553868299631908, -12.20027175159510335 ) ) ;
#32064 = CARTESIAN_POINT ( 'NONE',  ( 7.929178192470822673, -4.758525843572996905, 6.310451091254675404 ) ) ;
#32066 = CARTESIAN_POINT ( 'NONE',  ( 8.849385841230999361, 3.975069902178000270, 9.483774112875002160 ) ) ;
#32065 = AXIS2_PLACEMENT_3D ( 'NONE', #66762, #50002, #40206 ) ;
#32067 = VERTEX_POINT ( 'NONE', #45583 ) ;
#32068 = PLANE ( 'NONE',  #43347 ) ;
#32069 = CARTESIAN_POINT ( 'NONE',  ( 7.399995280410000653, 4.524560801752999240, -6.025559345696000157 ) ) ;
#32070 = EDGE_CURVE ( 'NONE', #5981, #11316, #48414, .T. ) ;
#32071 = CARTESIAN_POINT ( 'NONE',  ( 8.414772878883319152, -2.420192783774375300, 8.227318774112935884 ) ) ;
#32072 = AXIS2_PLACEMENT_3D ( 'NONE', #45305, #12800, #23971 ) ;
#32073 = CARTESIAN_POINT ( 'NONE',  ( 11.64440219406983523, -12.39501813438487154, -1.800675169423894273 ) ) ;
#32074 = ORIENTED_EDGE ( 'NONE', *, *, #52554, .T. ) ;
#32075 = CARTESIAN_POINT ( 'NONE',  ( 9.099999952505998024, -4.000000000000000000, 7.500000000000000000 ) ) ;
#32076 = CARTESIAN_POINT ( 'NONE',  ( 11.60581233665799950, 11.65209074823999913, 1.826497490784000144 ) ) ;
#32077 = VERTEX_POINT ( 'NONE', #45916 ) ;
#32078 = EDGE_CURVE ( 'NONE', #18362, #56639, #26761, .T. ) ;
#32079 = CARTESIAN_POINT ( 'NONE',  ( 12.43681290820071794, 1.853313662622533053, -12.46300903943780725 ) ) ;
#32080 = CARTESIAN_POINT ( 'NONE',  ( 7.720433716083946685, -2.879779226720537100, 6.726083684511015015 ) ) ;
#32081 = DIRECTION ( 'NONE',  ( 0.000000000000000000, 0.000000000000000000, -1.000000000000000000 ) ) ;
#32082 = ORIENTED_EDGE ( 'NONE', *, *, #4121, .F. ) ;
#32083 = CARTESIAN_POINT ( 'NONE',  ( 10.57899597767938360, -2.241951334100745985, -7.748279897758227008 ) ) ;
#32084 = DIRECTION ( 'NONE',  ( -1.000000000000000000, 0.000000000000000000, 0.000000000000000000 ) ) ;
#32085 = CARTESIAN_POINT ( 'NONE',  ( 11.59603632436369125, 3.157359628034400068, -7.303218851299499548 ) ) ;
#32086 = CARTESIAN_POINT ( 'NONE',  ( 12.55417570215094614, 3.072462724870959505, -12.29958987976101703 ) ) ;
#32087 = CARTESIAN_POINT ( 'NONE',  ( 11.46118313518939935, -4.792748567750200195, 6.497569908212999401 ) ) ;
#32088 = ORIENTED_EDGE ( 'NONE', *, *, #39228, .F. ) ;
#32089 = CARTESIAN_POINT ( 'NONE',  ( 9.117517219591000810, 4.954905351382000944, 8.825777580285999235 ) ) ;
#32090 = ORIENTED_EDGE ( 'NONE', *, *, #13105, .F. ) ;
#32091 = CARTESIAN_POINT ( 'NONE',  ( 9.373082992855460205, -5.217431357650287538, -7.172827875665086061 ) ) ;
#32092 = CARTESIAN_POINT ( 'NONE',  ( 15.37415039705200215, -9.132871822554998076, -8.217191491449000296 ) ) ;
#32093 = DIRECTION ( 'NONE',  ( 1.000000000000000000, 0.000000000000000000, 0.000000000000000000 ) ) ;
#32094 = ORIENTED_EDGE ( 'NONE', *, *, #5136, .T. ) ;
#32095 = DIRECTION ( 'NONE',  ( 1.000000000000000000, 0.000000000000000000, 0.000000000000000000 ) ) ;
#32096 = DIRECTION ( 'NONE',  ( -8.896584015454000239E-13, 1.000000000000000000, -2.557804911864000007E-11 ) ) ;
#32097 = CARTESIAN_POINT ( 'NONE',  ( 23.59999468372399889, -2.915558691838999739, 13.58549495651999983 ) ) ;
#32098 = CARTESIAN_POINT ( 'NONE',  ( 23.58110596194431352, -13.37140776802827880, -4.095521627281163646 ) ) ;
#32099 = CARTESIAN_POINT ( 'NONE',  ( 12.57019395242810589, -1.827067495629554728, -13.88026806835660842 ) ) ;
#32100 = CARTESIAN_POINT ( 'NONE',  ( 11.31410538575739899, -3.024036709177600368, -7.266662245194900116 ) ) ;
#32101 = CARTESIAN_POINT ( 'NONE',  ( 11.52531641787287597, 3.660964319297691283, -6.691293037684439504 ) ) ;
#32102 = CARTESIAN_POINT ( 'NONE',  ( 17.97968936757972713, -3.063621360739239297, 12.22187700344946037 ) ) ;
#32103 = ORIENTED_EDGE ( 'NONE', *, *, #2220, .F. ) ;
#32104 = CARTESIAN_POINT ( 'NONE',  ( 11.12372457444999974, -5.764773383430000564, -5.184664793151999795 ) ) ;
#32105 = ORIENTED_EDGE ( 'NONE', *, *, #44390, .F. ) ;
#32106 = DIRECTION ( 'NONE',  ( 0.000000000000000000, 0.000000000000000000, 1.000000000000000000 ) ) ;
#32107 = CARTESIAN_POINT ( 'NONE',  ( 11.69955063476129453, -3.023401864784706294, 8.326430086672804265 ) ) ;
#32108 = CARTESIAN_POINT ( 'NONE',  ( 25.60000000000000142, -10.55163788719000095, -3.754896668835000284 ) ) ;
#32109 = CARTESIAN_POINT ( 'NONE',  ( 10.44486820642000069, 4.964088085664999817, -9.083609801695999408 ) ) ;
#32110 = B_SPLINE_CURVE_WITH_KNOTS ( 'NONE', 3,
 ( #48262, #21011, #42348, #63647 ),
 .UNSPECIFIED., .F., .F.,
 ( 4, 4 ),
 ( 0.1836163425310833319, 1.000000000000000000 ),
 .UNSPECIFIED. ) ;
#32111 = CARTESIAN_POINT ( 'NONE',  ( 12.79999999838119606, -11.94789761932849181, 3.252399792653988708 ) ) ;
#32112 = CARTESIAN_POINT ( 'NONE',  ( 7.000035920415999868, -12.36732175638999998, 2.759089158555000143 ) ) ;
#32113 = PRODUCT_RELATED_PRODUCT_CATEGORY ( 'part', '', ( #29962 ) ) ;
#32114 = CARTESIAN_POINT ( 'NONE',  ( 24.25969244708700145, -12.09494195645999959, 3.326713950767999695 ) ) ;
#32115 = CARTESIAN_POINT ( 'NONE',  ( 8.770072224255999416, 4.093776898754200033, -8.386086300777899183 ) ) ;
#32116 = ORIENTED_EDGE ( 'NONE', *, *, #62502, .T. ) ;
#32117 = AXIS2_PLACEMENT_3D ( 'NONE', #19056, #2974, #24988 ) ;
#32118 = CARTESIAN_POINT ( 'NONE',  ( 11.52531641787287775, -4.339035680702311382, -6.691293037684439504 ) ) ;
#32119 = CARTESIAN_POINT ( 'NONE',  ( 10.77462860031000069, 5.575476001419000127, 8.682676628339999425 ) ) ;
#32120 = CARTESIAN_POINT ( 'NONE',  ( 2.165556799209332528, 0.4581489286485003198, 3.500000000000000444 ) ) ;
#32121 = CARTESIAN_POINT ( 'NONE',  ( 11.56456920625009843, -3.962850971080120299, 8.532838639935999225 ) ) ;
#32122 = CARTESIAN_POINT ( 'NONE',  ( 9.225036466121004253, 2.649952287134117235, 7.500002258928285315 ) ) ;
#32123 = CIRCLE ( 'NONE', #34378, 12.20000000000000284 ) ;
#32124 = CARTESIAN_POINT ( 'NONE',  ( 11.61364291764652812, 3.140345330584100036, -7.393734108507599601 ) ) ;
#32125 = CARTESIAN_POINT ( 'NONE',  ( 12.21300000160833399, -0.2005123242923285698, 12.69787478206144016 ) ) ;
#32126 = CARTESIAN_POINT ( 'NONE',  ( 9.059364158773000497, 4.192919163547999872, 5.525472271700999194 ) ) ;
#32127 = B_SPLINE_CURVE_WITH_KNOTS ( 'NONE', 3,
 ( #4345, #52940, #31618, #36171, #9943, #5036, #63061, #31279, #25678, #62053, #35495, #51898, #62395, #63414, #42109, #41419, #20433, #67977, #3654, #41761, #30586, #15538, #36865, #3996 ),
 .UNSPECIFIED., .F., .F.,
 ( 4, 2, 2, 2, 2, 2, 2, 1, 1, 2, 2, 2, 4 ),
 ( 0.000000000000000000, 0.2499999999999440448, 0.3749999999999168443, 0.4374999999999040767, 0.4999999999998913092, 0.6249999999998667732, 0.6874999999998523403, 0.7187499999998447908, 0.7343749999998396838, 0.7421874999998377964, 0.7499999999998357980, 0.8749999999999178435, 1.000000000000000000 ),
 .UNSPECIFIED. ) ;
#32128 = CARTESIAN_POINT ( 'NONE',  ( 10.93727498060999892, 5.425427353909999972, 7.240585962396000497 ) ) ;
#32129 = CIRCLE ( 'NONE', #41053, 13.17499999999999538 ) ;
#32130 =( NAMED_UNIT ( * ) SI_UNIT ( $, .STERADIAN. ) SOLID_ANGLE_UNIT ( ) );
#32131 = B_SPLINE_SURFACE_WITH_KNOTS ( 'NONE', 3, 3, ( 
 ( #38550, #16189, #37513, #22461, #12333, #65102, #28070, #11978, #49734, #7080, #42762, #49379, #28420, #64070, #1495, #6037, #58837, #53597, #22811 ),
 ( #1843, #10946, #44160, #43108, #11284, #65458, #64409, #32290, #33664, #1152, #803, #11625, #17579, #43806, #48702, #59184, #17225, #59873, #54982 ),
 ( #64757, #38907, #32623, #16534, #53934, #33318, #5693, #54634, #60229, #27375, #22120, #27035, #48348, #454, #21772, #37860, #16875, #38199, #59529 ),
 ( #32965, #54279, #6380, #27731, #49043, #56364, #55680, #65804, #34010, #3220, #39248, #8810, #30150, #8469, #29813, #23855, #34705, #2193, #44510 ) ),
 .UNSPECIFIED., .F., .F., .F.,
 ( 4, 4 ),
 ( 4, 1, 1, 1, 1, 1, 1, 1, 1, 1, 1, 1, 1, 1, 1, 1, 4 ),
 ( -0.02636945251836000231, 1.026369452518000047 ),
 ( -0.01067046919480000092, 0.02400855568828999878, 0.05868758057138000195, 0.09336660545446999471, 0.1280456303375999971, 0.1627246552206000063, 0.1974036801037000188, 0.2320827049868000036, 0.2667617298698999884, 0.3014407547529999731, 0.3361197796361000134, 0.3707988045191999982, 0.4054778294023000385, 0.4401568542853999677, 0.4748358791684000324, 0.5095149040515000172, 0.5441939289345999464 ),
 .UNSPECIFIED. ) ;
#32132 = ORIENTED_EDGE ( 'NONE', *, *, #31487, .T. ) ;
#32133 = CARTESIAN_POINT ( 'NONE',  ( 17.60000000000000142, 48.67241131317999958, -16.56944037379999912 ) ) ;
#32134 = CARTESIAN_POINT ( 'NONE',  ( 7.415504076822000634, -1.167372168626999995, 0.6628743416906999197 ) ) ;
#32135 = ADVANCED_FACE ( 'NONE', ( #36111 ), #33974, .T. ) ;
#32136 = ADVANCED_FACE ( 'NONE', ( #66545 ), #8171, .T. ) ;
#32137 = CARTESIAN_POINT ( 'NONE',  ( 18.00692794902805005, 2.068098667605222207, 13.75558205683924484 ) ) ;
#32138 = CARTESIAN_POINT ( 'NONE',  ( 11.09999999999999964, 2.649999999999999911, -7.500000000000000000 ) ) ;
#32139 = CARTESIAN_POINT ( 'NONE',  ( 10.81764560330029923, -3.650429500487800460, -6.414140625063999401 ) ) ;
#32140 = VERTEX_POINT ( 'NONE', #25624 ) ;
#32141 = CARTESIAN_POINT ( 'NONE',  ( 25.59997327719300131, 11.07537871057999901, 3.096068926251000164 ) ) ;
#32142 = CARTESIAN_POINT ( 'NONE',  ( 9.293536308086499886, -2.899999999999999911, 6.665341197412895546 ) ) ;
#32144 = CARTESIAN_POINT ( 'NONE',  ( 5.000030787343000327, -2.099962892530999881, 0.000000000000000000 ) ) ;
#32143 = CARTESIAN_POINT ( 'NONE',  ( 9.053070280414001303, 2.391443348526999912, -6.856688371964000162 ) ) ;
#32145 = CARTESIAN_POINT ( 'NONE',  ( 25.46373329105799854, 11.23406619596999967, -3.161081784610999978 ) ) ;
#32146 = ORIENTED_EDGE ( 'NONE', *, *, #21381, .F. ) ;
#32147 = CARTESIAN_POINT ( 'NONE',  ( 11.20563302462000088, 3.509134285281999777, 6.118194788334999856 ) ) ;
#32148 = CARTESIAN_POINT ( 'NONE',  ( 18.14139820495729438, -2.283379482803411076, -13.71697381851088160 ) ) ;
#32149 = CARTESIAN_POINT ( 'NONE',  ( 10.64949279009019989, 3.739015461786900030, 6.531063508962500208 ) ) ;
#32150 = CARTESIAN_POINT ( 'NONE',  ( 11.27765354842000001, -3.273798832483999721, 6.368296067120999382 ) ) ;
#32151 = CARTESIAN_POINT ( 'NONE',  ( 7.999933059623999476, -5.198566224659999513, 8.332559954171999905 ) ) ;
#32152 = ORIENTED_EDGE ( 'NONE', *, *, #48885, .T. ) ;
#32153 = CARTESIAN_POINT ( 'NONE',  ( 8.187142219590999304, 4.968147183437999992, 5.971792472497999604 ) ) ;
#32155 = CARTESIAN_POINT ( 'NONE',  ( 10.77401935321000082, -3.826867196099999813, -5.823197386290999589 ) ) ;
#32154 = CARTESIAN_POINT ( 'NONE',  ( 9.975298369746534277, -5.350379160513648813, 7.499985214262776978 ) ) ;
#32156 = CARTESIAN_POINT ( 'NONE',  ( 7.785931005785818648, -4.810406945106828758, 9.044821997675690284 ) ) ;
#32157 = CARTESIAN_POINT ( 'NONE',  ( 9.905786073958001481, -2.698967003257000119, 8.979227319929000473 ) ) ;
#32158 = CARTESIAN_POINT ( 'NONE',  ( 24.32784272479599963, 3.577368779004999944, 12.48430931087000140 ) ) ;
#32159 = ORIENTED_EDGE ( 'NONE', *, *, #10334, .F. ) ;
#32160 = CARTESIAN_POINT ( 'NONE',  ( 24.53429014209899961, 12.47024915613999951, 3.026245713505000268 ) ) ;
#32161 = B_SPLINE_CURVE_WITH_KNOTS ( 'NONE', 3,
 ( #41508, #10033, #30013, #40474 ),
 .UNSPECIFIED., .F., .F.,
 ( 4, 4 ),
 ( 0.000000000000000000, 1.000000000000000000 ),
 .UNSPECIFIED. ) ;
#32162 = CARTESIAN_POINT ( 'NONE',  ( 11.63764426047339917, -3.386171819220400003, 6.538488127609999978 ) ) ;
#32163 = EDGE_CURVE ( 'NONE', #60460, #62750, #27625, .T. ) ;
#32164 = VECTOR ( 'NONE', #61627, 1000.000000000000114 ) ;
#32165 = CARTESIAN_POINT ( 'NONE',  ( 10.34995525820099971, 3.892289273474800471, 8.635644537520001052 ) ) ;
#32166 = VERTEX_POINT ( 'NONE', #5323 ) ;
#32167 = CARTESIAN_POINT ( 'NONE',  ( 8.614404719593999005, 5.030502105212999453, -6.322203460290999999 ) ) ;
#32168 = CIRCLE ( 'NONE', #863, 2.000000000000000444 ) ;
#32169 = CARTESIAN_POINT ( 'NONE',  ( 12.63888201721070637, 1.779588368642098573, -12.47369581775632952 ) ) ;
#32170 = CARTESIAN_POINT ( 'NONE',  ( 11.47635090131019986, -3.000792947412299849, 6.881982988766500497 ) ) ;
#32171 = CARTESIAN_POINT ( 'NONE',  ( 25.08240820202400201, -2.794122706165999670, -11.47835358574999987 ) ) ;
#32172 = AXIS2_PLACEMENT_3D ( 'NONE', #40245, #66458, #2490 ) ;
#32173 = CARTESIAN_POINT ( 'NONE',  ( 18.01231764194518092, 2.926478478987347032, -13.57371117741004340 ) ) ;
#32174 = VERTEX_POINT ( 'NONE', #21740 ) ;
#32175 = CARTESIAN_POINT ( 'NONE',  ( 9.642108463020802489, 3.293853022144934695, 8.705313308395453475 ) ) ;
#32176 = CARTESIAN_POINT ( 'NONE',  ( 5.596693173016832112, -1.310679582531386389, -0.7554284705563492075 ) ) ;
#32177 = ORIENTED_EDGE ( 'NONE', *, *, #20780, .F. ) ;
#32178 = CARTESIAN_POINT ( 'NONE',  ( 12.41985246593411141, -3.089908466900599393, -12.21525705840281972 ) ) ;
#32179 = CARTESIAN_POINT ( 'NONE',  ( 11.43718179236249988, 3.790319673775199849, 8.481317998227099864 ) ) ;
#32180 = CARTESIAN_POINT ( 'NONE',  ( 10.28912155192344535, 2.704284023348198396, -7.938084390888771047 ) ) ;
#32181 = CARTESIAN_POINT ( 'NONE',  ( 10.19715290653000217, 4.982626294267999967, -6.124313696433000054 ) ) ;
#32182 = CARTESIAN_POINT ( 'NONE',  ( 8.086080172061008042, 4.921420473137001927, 6.235316328396007357 ) ) ;
#32183 = CARTESIAN_POINT ( 'NONE',  ( 10.22399006116000031, -5.507891002176999784, 6.589804341508000540 ) ) ;
#32184 = CARTESIAN_POINT ( 'NONE',  ( 17.91054845552246277, 0.5141503178158084442, -12.68598964581897626 ) ) ;
#32185 = CONICAL_SURFACE ( 'NONE', #42207, 1.449999999967999553, 0.7853981633972997312 ) ;
#32186 = CARTESIAN_POINT ( 'NONE',  ( 9.038118784902701819, 4.950731182098148331, 8.458238308662791027 ) ) ;
#32187 = CARTESIAN_POINT ( 'NONE',  ( 10.64949279009019989, -4.260984538213099526, -8.468936491037499792 ) ) ;
#32188 = CARTESIAN_POINT ( 'NONE',  ( 7.828420280408998622, 5.524123123935000379, 6.910361319981999095 ) ) ;
#32189 = ORIENTED_EDGE ( 'NONE', *, *, #19676, .F. ) ;
#32190 = AXIS2_PLACEMENT_3D ( 'NONE', #10267, #10609, #64422 ) ;
#32191 =( NAMED_UNIT ( * ) SI_UNIT ( $, .STERADIAN. ) SOLID_ANGLE_UNIT ( ) );
#32192 = CARTESIAN_POINT ( 'NONE',  ( 24.65657813088902017, -3.152276120826353445, 11.84445435621313969 ) ) ;
#32193 = DIRECTION ( 'NONE',  ( 0.000000000000000000, 1.000000000000000000, 0.000000000000000000 ) ) ;
#32194 = CARTESIAN_POINT ( 'NONE',  ( 9.214598350273000449, -3.399999999999999911, -6.571291218959999902 ) ) ;
#32195 = CARTESIAN_POINT ( 'NONE',  ( 18.25351233825839259, 2.286726172143656477, 12.39076325940497902 ) ) ;
#32196 = EDGE_CURVE ( 'NONE', #50903, #49108, #63354, .T. ) ;
#32197 = LINE ( 'NONE', #16778, #38359 ) ;
#32198 = ADVANCED_FACE ( 'NONE', ( #4288 ), #9884, .T. ) ;
#32199 = CARTESIAN_POINT ( 'NONE',  ( 10.96591775263000024, 9.690018913608000162, 5.974571089057000073 ) ) ;
#32200 = B_SPLINE_CURVE_WITH_KNOTS ( 'NONE', 3,
 ( #41667, #31525, #64008, #16125, #20338, #37451, #47950, #68915, #52848, #62971 ),
 .UNSPECIFIED., .F., .F.,
 ( 4, 2, 2, 2, 4 ),
 ( 0.000000000000000000, 0.2500000000000001665, 0.5000000000000003331, 0.7500000000000001110, 1.000000000000000000 ),
 .UNSPECIFIED. ) ;
#32201 = CARTESIAN_POINT ( 'NONE',  ( 9.245061313321260243, -2.690435683193665550, 7.172319517079158935 ) ) ;
#32202 = CARTESIAN_POINT ( 'NONE',  ( 10.04184687351587613, -3.000416447002275611, -8.268183399968640046 ) ) ;
#32203 = VERTEX_POINT ( 'NONE', #26315 ) ;
#32204 = CARTESIAN_POINT ( 'NONE',  ( 12.22684347114283199, -2.045928570575545891, 12.43279008976418964 ) ) ;
#32205 = CARTESIAN_POINT ( 'NONE',  ( 10.18692546752099837, -5.002009261081000524, -7.430575645513339822 ) ) ;
#32206 = PLANE ( 'NONE',  #41552 ) ;
#32207 = CARTESIAN_POINT ( 'NONE',  ( 10.25462442569999943, -2.860634389522000109, 6.604605425112000994 ) ) ;
#32208 = CARTESIAN_POINT ( 'NONE',  ( 11.59256785386839894, -4.832509746210599921, 6.939751505745099358 ) ) ;
#32209 = CARTESIAN_POINT ( 'NONE',  ( 11.38379707368349969, 3.433355370490100533, -6.509947486183500054 ) ) ;
#32210 = CARTESIAN_POINT ( 'NONE',  ( 8.734200250017998712, 4.093844212487689482, 6.613277660092100163 ) ) ;
#32211 = CARTESIAN_POINT ( 'NONE',  ( 0.2772402514715000543, 2.199938726422999924, 2.557617887446999916 ) ) ;
#32212 = CARTESIAN_POINT ( 'NONE',  ( 7.752942703112657874, -2.713880210350901656, 7.026314146705725072 ) ) ;
#32213 = AXIS2_PLACEMENT_3D ( 'NONE', #47514, #46483, #3812 ) ;
#32214 = CARTESIAN_POINT ( 'NONE',  ( 12.15765997487494587, 2.156065442695494383, 12.41416509552197134 ) ) ;
#32216 = DIRECTION ( 'NONE',  ( 0.000000000000000000, -1.000000000000000000, 0.000000000000000000 ) ) ;
#32215 = CARTESIAN_POINT ( 'NONE',  ( 10.29025461470400060, 2.893436332050999926, -7.781516069110699263 ) ) ;
#32217 = CARTESIAN_POINT ( 'NONE',  ( 11.33456651104149948, 4.112542507956200133, -6.364824110469998963 ) ) ;
#32218 = CARTESIAN_POINT ( 'NONE',  ( 25.46373154986600085, 8.354608910739999672, 8.148450287869000164 ) ) ;
#32219 = EDGE_CURVE ( 'NONE', #23338, #30974, #34320, .T. ) ;
#32220 = CARTESIAN_POINT ( 'NONE',  ( 11.28109528040999976, 2.660125405577999924, -6.904121770750999865 ) ) ;
#32221 = LINE ( 'NONE', #28002, #1461 ) ;
#32223 = CARTESIAN_POINT ( 'NONE',  ( 18.11689826751005938, -0.2739464174237275507, 12.69602652205148985 ) ) ;
#32222 = CARTESIAN_POINT ( 'NONE',  ( 12.79999999914999975, 12.11987927271999865, -3.159802730921999814 ) ) ;
#32224 = FACE_OUTER_BOUND ( 'NONE', #51978, .T. ) ;
#32225 = ORIENTED_EDGE ( 'NONE', *, *, #22195, .F. ) ;
#32226 = VECTOR ( 'NONE', #44456, 1000.000000000000000 ) ;
#32227 = ADVANCED_FACE ( 'NONE', ( #53223 ), #6053, .F. ) ;
#32228 = CARTESIAN_POINT ( 'NONE',  ( 12.39828795399329664, 0.4745523466136125079, 12.68806523617751125 ) ) ;
#32229 = CARTESIAN_POINT ( 'NONE',  ( 15.90003771078200145, 3.695138809391000034, 11.25918926437999978 ) ) ;
#32230 = CARTESIAN_POINT ( 'NONE',  ( 12.57461732485516670, -12.11259905827365913, 3.187575261699951312 ) ) ;
#32231 = CARTESIAN_POINT ( 'NONE',  ( 9.146417874593998576, 3.202096358337300330, 7.160798403412399260 ) ) ;
#32232 = CARTESIAN_POINT ( 'NONE',  ( 12.29449213756047676, -2.138932443162072872, 13.74345175514785033 ) ) ;
#32233 = CARTESIAN_POINT ( 'NONE',  ( 12.18403211231679606, 2.428839562872916691, 13.68824371556415720 ) ) ;
#32234 = CARTESIAN_POINT ( 'NONE',  ( 24.32784070168699841, 3.577437594875000126, -12.48429269957000010 ) ) ;
#32235 = ORIENTED_EDGE ( 'NONE', *, *, #51062, .T. ) ;
#32236 = B_SPLINE_CURVE_WITH_KNOTS ( 'NONE', 3,
 ( #46605, #57418, #4621, #15124, #40656, #10219 ),
 .UNSPECIFIED., .F., .F.,
 ( 4, 2, 4 ),
 ( 0.000000000000000000, 0.5000000000000000000, 1.000000000000000000 ),
 .UNSPECIFIED. ) ;
#32237 = LINE ( 'NONE', #7030, #37101 ) ;
#32238 = AXIS2_PLACEMENT_3D ( 'NONE', #12846, #3372, #19459 ) ;
#32239 = CARTESIAN_POINT ( 'NONE',  ( 11.28627509987130040, -4.272452942476324900, -6.250000000000000000 ) ) ;
#32240 = CARTESIAN_POINT ( 'NONE',  ( 18.06247470497385876, -3.164801830445712394, 11.41978211466257243 ) ) ;
#32241 = LINE ( 'NONE', #26297, #56735 ) ;
#32242 = B_SPLINE_CURVE_WITH_KNOTS ( 'NONE', 3,
 ( #67665, #9630, #4724, #30977 ),
 .UNSPECIFIED., .F., .F.,
 ( 4, 4 ),
 ( 0.000000000000000000, 1.000000000000000000 ),
 .UNSPECIFIED. ) ;
#32243 = ADVANCED_FACE ( 'NONE', ( #83 ), #26665, .F. ) ;
#32244 = CARTESIAN_POINT ( 'NONE',  ( 18.11762593468200322, 2.227530255644427637, -12.51091528569613764 ) ) ;
#32245 = CARTESIAN_POINT ( 'NONE',  ( 9.671146261768624797, -3.287258916643901241, 8.539225147222756718 ) ) ;
#32246 = CARTESIAN_POINT ( 'NONE',  ( 11.58902763632552002, 3.213494089586499847, 7.862914650060299770 ) ) ;
#32247 = CARTESIAN_POINT ( 'NONE',  ( 10.31905590579000176, -2.899999999999999911, -6.571291218949999902 ) ) ;
#32248 = CARTESIAN_POINT ( 'NONE',  ( 10.18308064679000147, -2.953580299898999950, -8.606287508253000595 ) ) ;
#32249 = DIRECTION ( 'NONE',  ( 0.000000000000000000, -0.9905022095861402143, -0.1374968101629056305 ) ) ;
#32250 = CARTESIAN_POINT ( 'NONE',  ( 21.10000109091659937, -1.355183834107999921E-13, -12.52499975980128966 ) ) ;
#32251 = CARTESIAN_POINT ( 'NONE',  ( 24.61098151538899970, 12.21941909980999874, 3.050810341055000041 ) ) ;
#32252 = CYLINDRICAL_SURFACE ( 'NONE', #8619, 0.5000000000000000000 ) ;
#32253 = ORIENTED_EDGE ( 'NONE', *, *, #51776, .F. ) ;
#32254 = CARTESIAN_POINT ( 'NONE',  ( 9.790085841230000696, 5.149303692842000402, -5.987168472229000393 ) ) ;
#32255 = CARTESIAN_POINT ( 'NONE',  ( 10.83364828895399867, -3.239803852721999888, 7.084788038520800413 ) ) ;
#32256 = VERTEX_POINT ( 'NONE', #58464 ) ;
#32257 = CARTESIAN_POINT ( 'NONE',  ( 11.09999999999999964, -4.000000000000000000, 7.500000000000000000 ) ) ;
#32258 = CARTESIAN_POINT ( 'NONE',  ( 10.32533997688000049, -3.756890902898200046, -6.385465081946999355 ) ) ;
#32259 = ORIENTED_EDGE ( 'NONE', *, *, #63286, .F. ) ;
#32260 = CARTESIAN_POINT ( 'NONE',  ( 10.47769598648999967, 5.009476315410999803, 6.898940957443399746 ) ) ;
#32261 = CARTESIAN_POINT ( 'NONE',  ( 7.550000000000000711, 4.000000000000000000, 8.849999999999999645 ) ) ;
#32262 = CARTESIAN_POINT ( 'NONE',  ( 5.000000000000000000, 0.000000000000000000, 0.000000000000000000 ) ) ;
#32263 = CARTESIAN_POINT ( 'NONE',  ( 18.53711938375299795, -2.638714702496000264, 11.30796021345999947 ) ) ;
#32264 = DIRECTION ( 'NONE',  ( 1.000000000000000000, 0.000000000000000000, 0.000000000000000000 ) ) ;
#32265 = CARTESIAN_POINT ( 'NONE',  ( 12.40587428666008840, 0.4809231526954447222, -13.88880064789607616 ) ) ;
#32266 = B_SPLINE_CURVE_WITH_KNOTS ( 'NONE', 1,
 ( #22375, #18526 ),
 .UNSPECIFIED., .F., .F.,
 ( 2, 2 ),
 ( 0.000000000000000000, 1.000000000000000000 ),
 .UNSPECIFIED. ) ;
#32267 = CARTESIAN_POINT ( 'NONE',  ( 17.55505043854147118, -1.875000000000000000, -12.57541666120755863 ) ) ;
#32268 = CONICAL_SURFACE ( 'NONE', #25516, 13.04999934368000147, 0.7853981075146502233 ) ;
#32269 = CARTESIAN_POINT ( 'NONE',  ( 10.48735240295000004, -4.351290250877999810, -6.182246784057000788 ) ) ;
#32270 = CARTESIAN_POINT ( 'NONE',  ( 13.55296092448800138, 11.54193659611999934, 2.433871908353000268 ) ) ;
#32271 = ORIENTED_EDGE ( 'NONE', *, *, #37644, .T. ) ;
#32272 = CARTESIAN_POINT ( 'NONE',  ( 8.496516550600000883, 5.350579948490858051, 7.852800305270208447 ) ) ;
#32273 = ORIENTED_EDGE ( 'NONE', *, *, #60387, .F. ) ;
#32274 = CARTESIAN_POINT ( 'NONE',  ( 0.3446312255616370557, 2.120796480409111506, 2.465608222985203213 ) ) ;
#32275 = ORIENTED_EDGE ( 'NONE', *, *, #22813, .F. ) ;
#32276 = CARTESIAN_POINT ( 'NONE',  ( 11.64459552687324262, -11.53034370678229514, -1.666360532292795904 ) ) ;
#32277 = CARTESIAN_POINT ( 'NONE',  ( 17.87019584817734952, -3.039826384816739502, -12.30925258946623480 ) ) ;
#32278 = CARTESIAN_POINT ( 'NONE',  ( 24.98034467287493854, -8.548010802276017728, 8.348296163080446419 ) ) ;
#32279 = CARTESIAN_POINT ( 'NONE',  ( 10.34184687351645771, 3.000416447002276943, -6.731816600031354625 ) ) ;
#32280 = ADVANCED_FACE ( 'NONE', ( #41700 ), #21400, .F. ) ;
#32281 = EDGE_CURVE ( 'NONE', #44907, #41132, #23414, .T. ) ;
#32282 = B_SPLINE_SURFACE_WITH_KNOTS ( 'NONE', 3, 3, ( 
 ( #68143, #52067, #4172, #25508, #10115, #20260, #41587, #58348, #15017, #9762, #4511, #31112, #10451, #25850, #53109, #68483, #20606, #41932, #63239, #47529, #31446, #68834, #20953, #47872, #69179, #49583, #27924, #64956, #1005, #6232, #54135, #12184, #22317, #27573, #37714 ),
 ( #43311, #44358, #1691, #43659, #54483, #48900, #11145, #22661, #28264, #59042, #42962, #17069, #39098, #48205, #33860, #23009, #38401, #33167, #32818, #60423, #311, #26891, #65658, #59725, #59378, #64269, #60080, #11827, #21627, #6584, #16724, #49234, #1344, #55175, #33514 ),
 ( #54830, #38054, #12529, #44004, #65311, #17780, #16384, #32479, #658, #5890, #17425, #38754, #53793, #27230, #6929, #48555, #21971, #64616, #11479, #2380, #45725, #50278, #39791, #3062, #61115, #67369, #55868, #35238, #8317, #13232, #23703, #29662, #34558, #46064, #29310 ),
 ( #67032, #61795, #34207, #35582, #50622, #7976, #49932, #45382, #50963, #2724, #24047, #28618, #40811, #30004, #62133, #66692, #44703, #13911, #18815, #39443, #13572, #23363, #65998, #40140, #45039, #24737, #51306, #61454, #34894, #56210, #60763, #24395, #8657, #18123, #12879 ) ),
 .UNSPECIFIED., .F., .F., .F.,
 ( 4, 4 ),
 ( 4, 1, 1, 1, 1, 1, 1, 1, 1, 1, 1, 1, 1, 1, 1, 1, 1, 1, 1, 1, 1, 1, 1, 1, 1, 1, 1, 1, 1, 1, 1, 1, 4 ),
 ( -0.1039370721279000015, 1.103937072127999963 ),
 ( -0.02000000000000000042, 0.01250000000000000069, 0.04499999999999999833, 0.07749999999999999944, 0.1100000000000000006, 0.1424999999999999878, 0.1749999999999999889, 0.2074999999999999900, 0.2399999999999999911, 0.2725000000000000200, 0.3049999999999999933, 0.3375000000000000222, 0.3699999999999999956, 0.4025000000000000244, 0.4349999999999999978, 0.4675000000000000266, 0.5000000000000000000, 0.5324999999999999734, 0.5649999999999999467, 0.5975000000000000311, 0.6300000000000000044, 0.6624999999999999778, 0.6949999999999999512, 0.7275000000000000355, 0.7600000000000000089, 0.7924999999999999822, 0.8249999999999999556, 0.8575000000000000400, 0.8900000000000000133, 0.9224999999999999867, 0.9549999999999999600, 0.9875000000000000444, 1.020000000000000018 ),
 .UNSPECIFIED. ) ;
#32283 = CARTESIAN_POINT ( 'NONE',  ( 4.149992563292000725, 2.000000000000000000, 0.000000000000000000 ) ) ;
#32284 = ADVANCED_FACE ( 'NONE', ( #15134 ), #64038, .F. ) ;
#32285 = CARTESIAN_POINT ( 'NONE',  ( 12.33448524795695889, 0.4118363585311526354, 13.89180007025485786 ) ) ;
#32286 = ORIENTED_EDGE ( 'NONE', *, *, #5613, .T. ) ;
#32287 = CARTESIAN_POINT ( 'NONE',  ( 12.34907277967800177, 11.89802509695999966, -3.395950604129000183 ) ) ;
#32288 = CARTESIAN_POINT ( 'NONE',  ( 9.824592608787908077, -5.732646222183269025, -7.158320533632580585 ) ) ;
#32289 = DIRECTION ( 'NONE',  ( 1.000000000000000000, 0.000000000000000000, 0.000000000000000000 ) ) ;
#32290 = CARTESIAN_POINT ( 'NONE',  ( 4.848370016636000202, -0.5474368957134999603, -1.217158087947000089 ) ) ;
#32291 = CARTESIAN_POINT ( 'NONE',  ( 12.18965064077726623, -11.77436608085473857, 3.633175706309820008 ) ) ;
#32292 = CARTESIAN_POINT ( 'NONE',  ( 18.50035835255887307, 11.89543982599948535, -3.922887695644379669 ) ) ;
#32293 = CARTESIAN_POINT ( 'NONE',  ( 10.71983009893999927, -3.571743996388999864, -5.696159701115999674 ) ) ;
#32294 = ORIENTED_EDGE ( 'NONE', *, *, #40342, .F. ) ;
#32295 = ORIENTED_EDGE ( 'NONE', *, *, #41712, .F. ) ;
#32296 = CARTESIAN_POINT ( 'NONE',  ( 10.98417232529000032, 5.106037833414999838, -4.881461580086000396 ) ) ;
#32297 = CARTESIAN_POINT ( 'NONE',  ( 11.80000000000000071, -14.76315775485999993, 50.50083396221000243 ) ) ;
#32298 = CARTESIAN_POINT ( 'NONE',  ( 8.642330585105490570, -3.079257296649804410, -6.512589459674783754 ) ) ;
#32299 = CARTESIAN_POINT ( 'NONE',  ( 8.579946306764748343, -2.950101199909312744, 6.243999687575779944 ) ) ;
#32300 = PLANE ( 'NONE',  #10967 ) ;
#32301 = CARTESIAN_POINT ( 'NONE',  ( 11.13746005378019888, 5.161099018038999731, -6.879992063401499713 ) ) ;
#32302 = CARTESIAN_POINT ( 'NONE',  ( 9.332721904869998752, 4.756019688173900306, -7.924431591189499358 ) ) ;
#32304 = CARTESIAN_POINT ( 'NONE',  ( 8.347900245721101342, 4.939084050600958342, -6.209245198555986001 ) ) ;
#32303 = CARTESIAN_POINT ( 'NONE',  ( 10.86422949779699998, -3.442773960835399993, 6.664331202173499946 ) ) ;
#32305 = CARTESIAN_POINT ( 'NONE',  ( 8.200208800211990834, -2.889590298673998081, 6.692105494707000446 ) ) ;
#32306 = VERTEX_POINT ( 'NONE', #36455 ) ;
#32307 = CARTESIAN_POINT ( 'NONE',  ( 8.221178267935991713, -3.443155653785000769, 6.131664341583003441 ) ) ;
#32308 = CARTESIAN_POINT ( 'NONE',  ( 10.39358376188600097, 2.921249888908000081, 6.812480849273599759 ) ) ;
#32309 = FACE_OUTER_BOUND ( 'NONE', #4769, .T. ) ;
#32310 = CARTESIAN_POINT ( 'NONE',  ( 10.31167756636999933, -2.874479384703000129, 8.900026329558999194 ) ) ;
#32311 = CARTESIAN_POINT ( 'NONE',  ( 18.11618405632788864, 2.775422336685124947, -12.38314678680533021 ) ) ;
#32312 = DIRECTION ( 'NONE',  ( -1.000000000000000000, 0.000000000000000000, 0.000000000000000000 ) ) ;
#32313 = CARTESIAN_POINT ( 'NONE',  ( 6.875001042874380630, 2.534482666265000184, -7.314862106114000007 ) ) ;
#32314 = CARTESIAN_POINT ( 'NONE',  ( 9.560684229509998744, -4.611171355610000688, -6.885038603985500494 ) ) ;
#32315 = CARTESIAN_POINT ( 'NONE',  ( 5.656244644296000601, 0.7464156889442000731, 0.9088697504474000377 ) ) ;
#32316 = ADVANCED_FACE ( 'NONE', ( #27002 ), #24549, .T. ) ;
#32317 = CARTESIAN_POINT ( 'NONE',  ( 6.999999999999999112, 8.396653025789797553, -4.391099154829968931 ) ) ;
#32318 = CARTESIAN_POINT ( 'NONE',  ( 18.27948916824811221, 2.669673601435039956, 12.31540264491035508 ) ) ;
#32319 = ORIENTED_EDGE ( 'NONE', *, *, #29934, .T. ) ;
#32320 = CARTESIAN_POINT ( 'NONE',  ( 12.44044950778751257, 0.5080407711865465581, -12.68632595416894837 ) ) ;
#32321 = CARTESIAN_POINT ( 'NONE',  ( 11.56441235500451015, 3.361299021099800388, -6.914884925939399629 ) ) ;
#32322 = ADVANCED_FACE ( 'NONE', ( #57341 ), #6181, .F. ) ;
#32323 = CARTESIAN_POINT ( 'NONE',  ( 6.826133408972999916, -9.284776586335999227, -5.366079628331000606 ) ) ;
#32324 = CARTESIAN_POINT ( 'NONE',  ( 8.351645692843000290, 5.100874653827000671, 6.601413402487000148 ) ) ;
#32325 = CARTESIAN_POINT ( 'NONE',  ( 5.700000000000000178, 13.04986661130000059, 1.811520473896000016 ) ) ;
#32326 = VERTEX_POINT ( 'NONE', #17019 ) ;
#32327 = CARTESIAN_POINT ( 'NONE',  ( 13.49994651945300284, -12.07042783918999795, -2.492331243371999960 ) ) ;
#32328 = APPLICATION_PROTOCOL_DEFINITION ( 'draft international standard', 'automotive_design', 1998, #40042 ) ;
#32329 = CARTESIAN_POINT ( 'NONE',  ( 11.02812378248509795, -4.416893162838900544, -6.711274001288999536 ) ) ;
#32330 = CARTESIAN_POINT ( 'NONE',  ( 18.14735902879090190, 0.1997594608485829815, 12.69789023918054305 ) ) ;
#32331 = CIRCLE ( 'NONE', #45756, 1.050000000000000044 ) ;
#32332 = CARTESIAN_POINT ( 'NONE',  ( 14.40000001005266661, -12.11987670936007078, 3.159780617438794792 ) ) ;
#32333 = CARTESIAN_POINT ( 'NONE',  ( 11.50029455687000102, -11.65000000000000036, 0.000000000000000000 ) ) ;
#32334 = CARTESIAN_POINT ( 'NONE',  ( 10.82035090130999855, 4.758726914843000699, -7.969278253227299658 ) ) ;
#32335 = VERTEX_POINT ( 'NONE', #59678 ) ;
#32336 = B_SPLINE_CURVE_WITH_KNOTS ( 'NONE', 3,
 ( #32333, #5404, #10992, #15557, #26047, #68679, #53643, #20797, #42811, #26741 ),
 .UNSPECIFIED., .F., .F.,
 ( 4, 2, 2, 2, 4 ),
 ( 0.000000000000000000, 0.2499999999999999445, 0.4999999999999998335, 0.7499999999999997780, 1.000000000000000000 ),
 .UNSPECIFIED. ) ;
#32337 = CARTESIAN_POINT ( 'NONE',  ( 10.94797187187000098, -2.864324950622999744, 8.846246404612999825 ) ) ;
#32338 = CARTESIAN_POINT ( 'NONE',  ( 17.71863970650576192, 3.103558472751648090, -13.52675378075879387 ) ) ;
#32339 = VERTEX_POINT ( 'NONE', #54433 ) ;
#32340 = CARTESIAN_POINT ( 'NONE',  ( 8.115081613917173087, 5.350113345104855256, -7.499995474391613293 ) ) ;
#32341 = CARTESIAN_POINT ( 'NONE',  ( 9.304730646793998972, -5.284133759825000887, 6.489273023403000273 ) ) ;
#32342 = CARTESIAN_POINT ( 'NONE',  ( 15.49162860438300271, 8.811474098792000831, 7.563394002770000846 ) ) ;
#32343 = ORIENTED_EDGE ( 'NONE', *, *, #48470, .T. ) ;
#32344 = CARTESIAN_POINT ( 'NONE',  ( 6.793770280410000417, 5.602143124542999786, -7.927308852422999763 ) ) ;
#32345 = CARTESIAN_POINT ( 'NONE',  ( 11.09999999999999964, -2.649999999999999911, 7.500000000000000000 ) ) ;
#32346 = CARTESIAN_POINT ( 'NONE',  ( 9.451728970891553061, 5.272005692884806471, 7.951869525468983291 ) ) ;
#32347 = ORIENTED_EDGE ( 'NONE', *, *, #49837, .T. ) ;
#32348 = CARTESIAN_POINT ( 'NONE',  ( 9.215289122285998502, -4.861979632688999686, 8.938813901364000003 ) ) ;
#32349 = CARTESIAN_POINT ( 'NONE',  ( 11.59999999999999964, 4.016704963253245886, 8.547709597963843109 ) ) ;
#32350 = CARTESIAN_POINT ( 'NONE',  ( 18.18005044212796051, -2.500000099754955851, 13.67345740034994783 ) ) ;
#32351 = ORIENTED_EDGE ( 'NONE', *, *, #31021, .T. ) ;
#32352 = CARTESIAN_POINT ( 'NONE',  ( 6.232109839683333874, 0.9218200799623741393, -1.199500263597268690 ) ) ;
#32353 = CARTESIAN_POINT ( 'NONE',  ( 7.744301838472999577, -3.130384865731000055, 6.467396727560999814 ) ) ;
#32354 = ORIENTED_EDGE ( 'NONE', *, *, #43008, .F. ) ;
#32355 = CARTESIAN_POINT ( 'NONE',  ( 24.44496351116800170, 3.224881296174999967, 12.03535797436000010 ) ) ;
#32356 = CARTESIAN_POINT ( 'NONE',  ( 18.00922683609310937, -1.919385048924807657, -12.45295227646844793 ) ) ;
#32357 = CARTESIAN_POINT ( 'NONE',  ( 4.829607378956000119, 1.514947213439000073, 0.3616484269658999939 ) ) ;
#32358 = CARTESIAN_POINT ( 'NONE',  ( 11.60000000000000142, 4.813860086966098351, -6.684405152318920074 ) ) ;
#32359 = CARTESIAN_POINT ( 'NONE',  ( 16.00261247405899923, 3.453035413593999792, 11.78892418867000025 ) ) ;
#32360 = CARTESIAN_POINT ( 'NONE',  ( 11.28627509987130040, 3.727547057523676433, 8.749999999999998224 ) ) ;
#32361 = CARTESIAN_POINT ( 'NONE',  ( 7.474999999999999645, 5.349999999999999645, 7.500000000000000000 ) ) ;
#32362 = ADVANCED_FACE ( 'NONE', ( #30788 ), #66952, .F. ) ;
#32363 = EDGE_CURVE ( 'NONE', #13791, #37829, #20058, .T. ) ;
#32364 = EDGE_CURVE ( 'NONE', #33733, #47838, #46296, .T. ) ;
#32365 = ORIENTED_EDGE ( 'NONE', *, *, #14699, .F. ) ;
#32366 = CARTESIAN_POINT ( 'NONE',  ( 13.35060253487350401, -12.37707099949019174, -1.919647290784824545 ) ) ;
#32367 = ORIENTED_EDGE ( 'NONE', *, *, #67014, .T. ) ;
#32368 = CARTESIAN_POINT ( 'NONE',  ( 10.13339736671999880, 5.653645990693000556, 6.501823474484000442 ) ) ;
#32369 = DIRECTION ( 'NONE',  ( 1.000000000000000000, 0.000000000000000000, 0.000000000000000000 ) ) ;
#32370 = CARTESIAN_POINT ( 'NONE',  ( 25.30000327618300204, -2.078227429405999693, 11.31065739696999906 ) ) ;
#32371 = CARTESIAN_POINT ( 'NONE',  ( 12.47325605351258559, 3.030051207268856128, -13.54664584463136556 ) ) ;
#32372 = CARTESIAN_POINT ( 'NONE',  ( 3.760208574517000191, -3.539102845952000198, 0.6295829741491000275 ) ) ;
#32373 = CARTESIAN_POINT ( 'NONE',  ( 25.27036090913500033, 2.549220333827999951, 11.36408438533999998 ) ) ;
#32374 = CARTESIAN_POINT ( 'NONE',  ( 18.17180502197784975, -0.1017048024283995350, 13.89950429703524826 ) ) ;
#32375 = CARTESIAN_POINT ( 'NONE',  ( 13.70003001321900271, -10.86123379505843189, -6.319444516909303644 ) ) ;
#32376 = VERTEX_POINT ( 'NONE', #56851 ) ;
#32377 = CARTESIAN_POINT ( 'NONE',  ( 12.35321263090786559, 0.4320316581265301603, 13.89096707190850211 ) ) ;
#32378 = CARTESIAN_POINT ( 'NONE',  ( 11.41195257254739914, -5.227167235646000165, 7.143100915737699452 ) ) ;
#32379 = PLANE ( 'NONE',  #15689 ) ;
#32380 = CARTESIAN_POINT ( 'NONE',  ( 17.93439120260890363, -0.4967442791062720020, -13.88805191678453177 ) ) ;
#32381 = EDGE_CURVE ( 'NONE', #12913, #43427, #59307, .T. ) ;
#32382 = CARTESIAN_POINT ( 'NONE',  ( 8.913566940379999082, -2.550589632307000088, 8.854674225901000284 ) ) ;
#32383 = VECTOR ( 'NONE', #8861, 1000.000000000000000 ) ;
#32385 = CARTESIAN_POINT ( 'NONE',  ( 12.17504389532412645, -11.54180247360918621, 4.316564347526565371 ) ) ;
#32384 = CARTESIAN_POINT ( 'NONE',  ( 9.075483283097998566, 4.020836891789999257, 8.948690653012000951 ) ) ;
#32386 = CARTESIAN_POINT ( 'NONE',  ( 10.17764828895399809, 5.001141961424000471, -8.046814291299300592 ) ) ;
#32387 = CARTESIAN_POINT ( 'NONE',  ( 24.70770306079000278, -8.718110200638999885, -9.202866107698000064 ) ) ;
#32388 = DIRECTION ( 'NONE',  ( 0.000000000000000000, -1.000000000000000000, 4.054615592038000306E-13 ) ) ;
#32389 = CARTESIAN_POINT ( 'NONE',  ( 18.16600380262988068, -0.1321628250398322602, 12.69908003149455133 ) ) ;
#32390 = CARTESIAN_POINT ( 'NONE',  ( 7.100000000000000533, 13.04986661130000059, -1.811520473896000016 ) ) ;
#32391 = CARTESIAN_POINT ( 'NONE',  ( 23.99069334398700093, 9.436054250658999720, 9.573720703848998426 ) ) ;
#32392 = ORIENTED_EDGE ( 'NONE', *, *, #66517, .F. ) ;
#32393 = CARTESIAN_POINT ( 'NONE',  ( 9.342519353207999089, -5.057079407184000175, 8.967634647348999621 ) ) ;
#32394 = DIRECTION ( 'NONE',  ( 0.000000000000000000, 0.000000000000000000, -1.000000000000000000 ) ) ;
#32395 = B_SPLINE_CURVE_WITH_KNOTS ( 'NONE', 3,
 ( #54943, #65766, #55640, #34666, #7737, #3850 ),
 .UNSPECIFIED., .F., .F.,
 ( 4, 2, 4 ),
 ( 0.3058235430633697294, 0.6529117715316847814, 1.000000000000000000 ),
 .UNSPECIFIED. ) ;
#32396 = CARTESIAN_POINT ( 'NONE',  ( 18.30000000000000071, 48.67241131317999958, -16.56944037379999912 ) ) ;
#32397 = CARTESIAN_POINT ( 'NONE',  ( 10.90000000296000060, 5.100000000009000445, -5.160242730682999657 ) ) ;
#32398 = CARTESIAN_POINT ( 'NONE',  ( 0.2554473843801999822, -2.101315454803999838, -2.652019770012000066 ) ) ;
#32399 = CARTESIAN_POINT ( 'NONE',  ( 10.93990547754509812, 5.032986398992000510, 7.467215766047949899 ) ) ;
#32400 = CARTESIAN_POINT ( 'NONE',  ( 10.38726084123000071, 2.888676266723000374, -6.716337836090000124 ) ) ;
#32401 = ORIENTED_EDGE ( 'NONE', *, *, #34667, .F. ) ;
#32402 = DIRECTION ( 'NONE',  ( -0.4384236320214023319, 0.000000000000000000, 0.8987684456439056779 ) ) ;
#32403 = FACE_OUTER_BOUND ( 'NONE', #12299, .T. ) ;
#32404 = CARTESIAN_POINT ( 'NONE',  ( 18.25219266138121554, 2.678721125794442326, -12.31196912072773308 ) ) ;
#32405 = EDGE_CURVE ( 'NONE', #20142, #35353, #48416, .T. ) ;
#32406 = DIRECTION ( 'NONE',  ( 0.000000000000000000, -1.000000000000000000, 0.000000000000000000 ) ) ;
#32407 = CARTESIAN_POINT ( 'NONE',  ( 13.99999997324030510, -8.827177816329490057, -7.803278505680545152 ) ) ;
#32408 = ORIENTED_EDGE ( 'NONE', *, *, #12818, .F. ) ;
#32409 = CARTESIAN_POINT ( 'NONE',  ( 6.003946504885999680, -1.413039514337999902, -0.3998085520867999954 ) ) ;
#32410 = CARTESIAN_POINT ( 'NONE',  ( 8.295045280407999044, 2.702884610408000210, -6.624425519483001068 ) ) ;
#32411 = CARTESIAN_POINT ( 'NONE',  ( 8.384287192004888922, -2.818189082097684039, 8.777095765030843211 ) ) ;
#32412 = CARTESIAN_POINT ( 'NONE',  ( 9.244113844317999096, -3.676949563211899807, 8.737749087159000894 ) ) ;
#32413 = EDGE_LOOP ( 'NONE', ( #39891, #68148, #61598, #66430 ) ) ;
#32414 = DIRECTION ( 'NONE',  ( 0.000000000000000000, 0.2588190451024932059, -0.9659258262890756397 ) ) ;
#32415 = B_SPLINE_CURVE_WITH_KNOTS ( 'NONE', 3,
 ( #68376, #59271, #64167, #10003, #26091, #69078, #5453, #47417, #47075, #5102, #11374, #20497, #554, #41821, #26789, #52314, #63129, #21525, #68723, #37606, #53005, #42856, #36931, #20843, #58936, #32377, #53692, #5785, #42177, #16625, #27128, #48448, #21865, #58243, #10348, #64504, #7514, #48793, #902, #44256, #11718, #43550, #60660, #64850, #12774, #22215, #18366, #44602, #16961, #33060, #6827, #65552, #54374, #54026, #54726, #39687, #6129, #50177, #38294, #38998, #61006, #1585, #28159, #12076, #59968, #18023, #49473, #59623, #65200, #22902, #43898, #65893, #33409, #17319, #17675, #39339, #28513, #32715, #2280, #60317, #6477, #12426, #44939, #27466, #27826, #28869, #33757, #55072, #38644, #66244, #49131, #1243, #23596 ),
 .UNSPECIFIED., .F., .F.,
 ( 4, 2, 2, 2, 2, 2, 2, 2, 2, 1, 1, 2, 2, 2, 2, 2, 2, 2, 2, 2, 2, 2, 2, 2, 2, 2, 2, 2, 2, 2, 2, 2, 2, 1, 1, 2, 2, 2, 2, 1, 2, 2, 2, 2, 2, 2, 2, 2, 4 ),
 ( 0.000000000000000000, 0.03124999999999007738, 0.06249999999998015476, 0.09374999999997023215, 0.1093749999999640288, 0.1249999999999578115, 0.1562499999999453493, 0.1718749999999391043, 0.1874999999999328593, 0.2031249999999266143, 0.2109374999999235334, 0.2148437499999229505, 0.2187499999999223954, 0.2499999999999291678, 0.2656249999999332756, 0.2734374999999361622, 0.2812499999999390488, 0.2968749999999448219, 0.3124999999999505396, 0.3437499999999608646, 0.3593749999999660272, 0.3749999999999711897, 0.4062499999999815703, 0.4374999999999919509, 0.5000000000000133227, 0.5312500000000240918, 0.5625000000000347500, 0.5937500000000454081, 0.6093750000000502931, 0.6250000000000551781, 0.6562500000000650591, 0.6718750000000692779, 0.6875000000000736078, 0.7031250000000778266, 0.7109375000000800471, 0.7148437500000811573, 0.7187500000000821565, 0.7500000000000738298, 0.7656250000000696110, 0.7734375000000686118, 0.7773437500000668354, 0.7812500000000650591, 0.7968750000000613953, 0.8125000000000577316, 0.8437500000000506262, 0.8593750000000469624, 0.8750000000000432987, 0.9375000000000216493, 1.000000000000000000 ),
 .UNSPECIFIED. ) ;
#32416 = CARTESIAN_POINT ( 'NONE',  ( 11.72772918458500158, 11.64671933177000085, 1.861692232596000141 ) ) ;
#32417 = ORIENTED_EDGE ( 'NONE', *, *, #14825, .T. ) ;
#32418 = LINE ( 'NONE', #43944, #48493 ) ;
#32419 = CARTESIAN_POINT ( 'NONE',  ( 24.44496412535000118, -8.810486166165000910, -8.810507954003998776 ) ) ;
#32420 = CARTESIAN_POINT ( 'NONE',  ( 17.77532102045679352, -0.5849891190461622426, -13.88342664904962831 ) ) ;
#32421 = ORIENTED_EDGE ( 'NONE', *, *, #54484, .F. ) ;
#32422 = CARTESIAN_POINT ( 'NONE',  ( 11.03483424351999886, -8.048618767883999325, 7.048979873803999929 ) ) ;
#32423 = DIRECTION ( 'NONE',  ( -1.000000000000000000, 0.000000000000000000, 0.000000000000000000 ) ) ;
#32424 = CARTESIAN_POINT ( 'NONE',  ( 10.52435971519499880, 4.532462039660099862, -6.614211617270199461 ) ) ;
#32425 = CARTESIAN_POINT ( 'NONE',  ( 5.000000000000000000, -1.199999999999999956, -9.776630298829998011 ) ) ;
#32426 = CARTESIAN_POINT ( 'NONE',  ( 10.55041772631200026, -3.450375740502100275, 6.368647051112000135 ) ) ;
#32427 = ORIENTED_EDGE ( 'NONE', *, *, #42696, .T. ) ;
#32428 = CARTESIAN_POINT ( 'NONE',  ( 7.577017219590000074, 5.480308727866000318, 8.192324747680999053 ) ) ;
#32429 = ORIENTED_EDGE ( 'NONE', *, *, #32690, .T. ) ;
#32430 = CARTESIAN_POINT ( 'NONE',  ( 8.479753663705539068, 5.101882484038004151, -8.673404222138428210 ) ) ;
#32431 = DIRECTION ( 'NONE',  ( 0.8660254037844289376, 0.000000000000000000, 0.5000000000000169864 ) ) ;
#32432 = CARTESIAN_POINT ( 'NONE',  ( 10.96237823296000080, 6.768026792119000490, -5.462786416141000245 ) ) ;
#32433 = VERTEX_POINT ( 'NONE', #53665 ) ;
#32434 = B_SPLINE_SURFACE_WITH_KNOTS ( 'NONE', 3, 3, ( 
 ( #32760, #6170, #17009, #54073 ),
 ( #43598, #65249, #38338, #49177 ),
 ( #64895, #27511, #12124, #6868 ),
 ( #7561, #59667, #50220, #28558 ),
 ( #2322, #43945, #65597, #17365 ),
 ( #60014, #33453, #54768, #39044 ),
 ( #28205, #49519, #22946, #12467 ),
 ( #55118, #25358, #3676, #7915 ),
 ( #56491, #19081, #25018, #14537 ) ),
 .UNSPECIFIED., .F., .F., .F.,
 ( 4, 1, 1, 1, 1, 1, 4 ),
 ( 4, 4 ),
 ( 0.02209653170519000273, 0.1666666666667000196, 0.3333333333333000081, 0.5000000000000000000, 0.6666666666667000474, 0.8333333333333000637, 0.9492823795161999811 ),
 ( -0.1916656884162999952, 1.191851428473000185 ),
 .UNSPECIFIED. ) ;
#32435 = CARTESIAN_POINT ( 'NONE',  ( 12.21176631991879447, -2.303170217796230546, -12.49524360984839433 ) ) ;
#32436 = DIRECTION ( 'NONE',  ( 0.000000000000000000, -1.000000000000000000, 0.000000000000000000 ) ) ;
#32437 = CARTESIAN_POINT ( 'NONE',  ( 7.856851002541000106, 2.832432432432000269, -6.822293592207000934 ) ) ;
#32438 = LINE ( 'NONE', #27191, #681 ) ;
#32439 = CARTESIAN_POINT ( 'NONE',  ( 12.50340631570018068, -1.853896141579339130, -13.87671057111554518 ) ) ;
#32440 = CARTESIAN_POINT ( 'NONE',  ( 10.35410941423799791, -3.257202320419700037, -6.825313060354999628 ) ) ;
#32441 = CARTESIAN_POINT ( 'NONE',  ( 18.43044927002210542, 3.211191212926777450, 12.10643352320258970 ) ) ;
#32444 = EDGE_CURVE ( 'NONE', #56658, #11513, #42828, .T. ) ;
#32443 = CARTESIAN_POINT ( 'NONE',  ( 18.27898910297789925, -2.436826214745341446, 12.36212035235843487 ) ) ;
#32442 = B_SPLINE_CURVE_WITH_KNOTS ( 'NONE', 3,
 ( #64326, #16448, #11205, #53856 ),
 .UNSPECIFIED., .F., .F.,
 ( 4, 4 ),
 ( 0.000000000000000000, 1.000000000000000000 ),
 .UNSPECIFIED. ) ;
#32445 = ORIENTED_EDGE ( 'NONE', *, *, #28582, .T. ) ;
#32446 = CARTESIAN_POINT ( 'NONE',  ( 11.64122412107036908, -3.937930136014310190, -6.326756392227999015 ) ) ;
#32447 = ORIENTED_EDGE ( 'NONE', *, *, #38092, .F. ) ;
#32448 = DIRECTION ( 'NONE',  ( -0.9999999999751629787, -5.691912098208790371E-06, 4.156456142935844641E-06 ) ) ;
#32449 = DIRECTION ( 'NONE',  ( -1.000000000000000000, 0.000000000000000000, 0.000000000000000000 ) ) ;
#32450 = CARTESIAN_POINT ( 'NONE',  ( 15.40000000009400161, 8.833277835210999740, 7.896561221812000930 ) ) ;
#32451 = CARTESIAN_POINT ( 'NONE',  ( 10.33022766388000058, -2.650179121646999647, -7.694581537458001108 ) ) ;
#32452 = DIRECTION ( 'NONE',  ( -1.000000000000000000, 0.000000000000000000, 0.000000000000000000 ) ) ;
#32453 = CARTESIAN_POINT ( 'NONE',  ( 23.66481111098300261, -13.24745896931000111, 3.909204073637000398 ) ) ;
#32454 = CARTESIAN_POINT ( 'NONE',  ( 10.75109581085999899, 2.822145500011000063, 6.655897464539000552 ) ) ;
#32455 = EDGE_LOOP ( 'NONE', ( #16871, #42115, #19237, #6420 ) ) ;
#32456 = CARTESIAN_POINT ( 'NONE',  ( 11.09999999999999964, -5.299316147296000423, 5.124965750789000296 ) ) ;
#32457 = CARTESIAN_POINT ( 'NONE',  ( 11.05639637898999972, 5.030226177531999632, 6.028288223959999748 ) ) ;
#32458 = CARTESIAN_POINT ( 'NONE',  ( 0.000000000000000000, 0.000000000000000000, 0.000000000000000000 ) ) ;
#32459 = ADVANCED_FACE ( 'NONE', ( #58908 ), #23401, .F. ) ;
#32460 = CARTESIAN_POINT ( 'NONE',  ( 10.87199293566600034, -3.366612813978900220, 6.723009541442299231 ) ) ;
#32461 = CARTESIAN_POINT ( 'NONE',  ( 17.79222771582700346, 3.377813322129000095, -11.11021622646999951 ) ) ;
#32462 = CARTESIAN_POINT ( 'NONE',  ( 10.96568151726000018, 9.694042294195000409, -5.969392498067000119 ) ) ;
#32463 = EDGE_CURVE ( 'NONE', #14810, #22779, #16140, .T. ) ;
#32464 = CIRCLE ( 'NONE', #63, 13.89999852641999922 ) ;
#32465 = CARTESIAN_POINT ( 'NONE',  ( 5.500000000000000000, -1.600000000000000089, 0.000000000000000000 ) ) ;
#32466 = CARTESIAN_POINT ( 'NONE',  ( 24.23278707828200140, -9.064214965309000505, -9.161880861702000445 ) ) ;
#32467 = CARTESIAN_POINT ( 'NONE',  ( 10.99933470386000067, 5.081013421858999735, 8.239043921879998678 ) ) ;
#32468 = CIRCLE ( 'NONE', #52568, 13.92493900951000363 ) ;
#32469 = CARTESIAN_POINT ( 'NONE',  ( 11.84006751466700180, -3.254324250158000087, 11.33670592834999979 ) ) ;
#32470 = ORIENTED_EDGE ( 'NONE', *, *, #27406, .T. ) ;
#32471 = CARTESIAN_POINT ( 'NONE',  ( 9.905375278050065901, 5.100000000000000533, -6.445686799065932782 ) ) ;
#32472 = CARTESIAN_POINT ( 'NONE',  ( 7.094492130820000853, 0.2195801626521000083, -1.351071070713000033 ) ) ;
#32473 = CARTESIAN_POINT ( 'NONE',  ( 18.06560877808659882, 2.138932497554040246, 13.74340275081395113 ) ) ;
#32474 = FACE_OUTER_BOUND ( 'NONE', #14881, .T. ) ;
#32475 = CIRCLE ( 'NONE', #62604, 2.000000000000001332 ) ;
#32476 = CARTESIAN_POINT ( 'NONE',  ( 10.49764694612699856, -5.059486515935999407, -7.922821994243300914 ) ) ;
#32477 = ORIENTED_EDGE ( 'NONE', *, *, #31654, .T. ) ;
#32478 = CARTESIAN_POINT ( 'NONE',  ( 17.55505043854144276, -0.6250000000000001110, -13.88107975066922428 ) ) ;
#32479 = CARTESIAN_POINT ( 'NONE',  ( 7.512829719590000010, 5.524123123935000379, 6.910361319981999095 ) ) ;
#32481 = LINE ( 'NONE', #26550, #52168 ) ;
#32480 = CARTESIAN_POINT ( 'NONE',  ( 9.749220280410998640, 5.656948148960999845, -6.994239053114000626 ) ) ;
#32482 = CARTESIAN_POINT ( 'NONE',  ( 2.394284045767109514, 0.2836190127161131169, 3.245552818120243543 ) ) ;
#32483 = VERTEX_POINT ( 'NONE', #20812 ) ;
#32484 = CARTESIAN_POINT ( 'NONE',  ( 9.534905769125000319, 3.030948166328000237, 8.761984216465000586 ) ) ;
#32485 = CARTESIAN_POINT ( 'NONE',  ( 17.72189171626102322, -1.806990214763248392, -13.88289628861100766 ) ) ;
#32486 = CARTESIAN_POINT ( 'NONE',  ( 10.52641638348499953, 3.025038519517300184, 7.737488872214999702 ) ) ;
#32487 = EDGE_CURVE ( 'NONE', #19773, #66241, #45943, .T. ) ;
#32488 = CARTESIAN_POINT ( 'NONE',  ( 9.590594544025000445, -2.445960766574000189, 7.841185849078001091 ) ) ;
#32489 = CARTESIAN_POINT ( 'NONE',  ( 7.743183059623000020, -2.735207418315000361, 6.771977475428999860 ) ) ;
#32490 = ORIENTED_EDGE ( 'NONE', *, *, #64028, .F. ) ;
#32491 = CARTESIAN_POINT ( 'NONE',  ( 24.57937622054542715, 12.41575245047435416, 3.011584258239457412 ) ) ;
#32493 = CARTESIAN_POINT ( 'NONE',  ( 10.13035685320999946, -2.409329538444999752, -8.058042649154000259 ) ) ;
#32492 = CARTESIAN_POINT ( 'NONE',  ( 12.79484580939900162, -11.81466332729999991, 3.323431527667999763 ) ) ;
#32494 = CARTESIAN_POINT ( 'NONE',  ( 7.754005127114919738, -5.344455520341463206, 8.603494402914543926 ) ) ;
#32495 = CARTESIAN_POINT ( 'NONE',  ( 9.471368011205999693, -2.030678448189000118, 7.549764202121000523 ) ) ;
#32496 = CARTESIAN_POINT ( 'NONE',  ( 1.500064665912000050, -2.653487697479000040, 1.892165331686999963 ) ) ;
#32497 = ORIENTED_EDGE ( 'NONE', *, *, #63111, .T. ) ;
#32498 = CARTESIAN_POINT ( 'NONE',  ( 9.498096873515667227, 3.672815144550898303, -8.717465845835393523 ) ) ;
#32499 = CARTESIAN_POINT ( 'NONE',  ( 11.27256919669530077, -3.037654633983899899, 7.215672285280100517 ) ) ;
#32500 = CARTESIAN_POINT ( 'NONE',  ( 10.56733863405299800, 4.788475529394700558, 6.494205428462000107 ) ) ;
#32501 = EDGE_LOOP ( 'NONE', ( #51015, #46161, #2430, #3504, #4531 ) ) ;
#32502 = CARTESIAN_POINT ( 'NONE',  ( 8.465229719592999302, 2.567871051582000241, -6.869011921437000012 ) ) ;
#32503 = VECTOR ( 'NONE', #41662, 1000.000000000000114 ) ;
#32504 = CARTESIAN_POINT ( 'NONE',  ( 12.37951367597793784, 1.897619119404204469, -12.45628731554757351 ) ) ;
#32505 = CARTESIAN_POINT ( 'NONE',  ( 12.18788784977535933, -4.985985832792199979, 7.556342205905759890 ) ) ;
#32506 = ORIENTED_EDGE ( 'NONE', *, *, #64155, .F. ) ;
#32507 = CARTESIAN_POINT ( 'NONE',  ( 9.148130259829166278, 4.680070470244416470, -8.679971105817726240 ) ) ;
#32508 = DIRECTION ( 'NONE',  ( 0.000000000000000000, 0.000000000000000000, -1.000000000000000000 ) ) ;
#32509 = EDGE_LOOP ( 'NONE', ( #52639, #39659, #57166, #12315, #41772 ) ) ;
#32510 = CARTESIAN_POINT ( 'NONE',  ( 23.60205915885299888, 11.88166580726000454, 3.967996863081999948 ) ) ;
#32511 = CARTESIAN_POINT ( 'NONE',  ( 11.09999999999999964, -4.755975669291000300E-06, 1.428076682242000113E-06 ) ) ;
#32513 = ORIENTED_EDGE ( 'NONE', *, *, #51689, .T. ) ;
#32512 = AXIS2_PLACEMENT_3D ( 'NONE', #19977, #41299, #62607 ) ;
#32514 = CARTESIAN_POINT ( 'NONE',  ( 9.552263540183332680, 5.092232985442822546, 6.870476274536374994 ) ) ;
#32515 = CARTESIAN_POINT ( 'NONE',  ( 10.48133997687999930, 4.184599793140999502, 8.346298710230199092 ) ) ;
#32516 = CARTESIAN_POINT ( 'NONE',  ( 9.944319408602000365, 5.443001719280999851, 7.367350382395000175 ) ) ;
#32517 = CARTESIAN_POINT ( 'NONE',  ( 5.500000000000000000, 12.87590651766999983, -2.791353855799999728 ) ) ;
#32518 = CARTESIAN_POINT ( 'NONE',  ( 8.493369886551995762, 5.097498803759001440, 6.607670056088003285 ) ) ;
#32519 = CARTESIAN_POINT ( 'NONE',  ( 11.14993998249000029, -2.627133311863999676, 6.696092388640000337 ) ) ;
#32520 = CARTESIAN_POINT ( 'NONE',  ( 17.91829918956260315, -0.6226057762474851431, -12.58460959628226306 ) ) ;
#32521 = CIRCLE ( 'NONE', #16881, 3.500000000000000000 ) ;
#32522 = FILL_AREA_STYLE_COLOUR ( '', #22961 ) ;
#32523 = CARTESIAN_POINT ( 'NONE',  ( 10.28026357027499849, -3.014700852776899698, -7.690095141806899903 ) ) ;
#32524 = EDGE_CURVE ( 'NONE', #23367, #66228, #58217, .T. ) ;
#32526 = ADVANCED_FACE ( 'NONE', ( #18677 ), #34074, .T. ) ;
#32525 = CARTESIAN_POINT ( 'NONE',  ( 8.020982780409999791, 3.245534453799999941, 8.949623695221001540 ) ) ;
#32527 = ORIENTED_EDGE ( 'NONE', *, *, #20539, .T. ) ;
#32528 = ADVANCED_FACE ( 'NONE', ( #17647 ), #64087, .F. ) ;
#32529 = FILL_AREA_STYLE_COLOUR ( '', #37686 ) ;
#32530 = PLANE ( 'NONE',  #22417 ) ;
#32531 = CARTESIAN_POINT ( 'NONE',  ( 9.243270085646278389, 2.683788241851253531, 7.201163913334668543 ) ) ;
#32532 = CARTESIAN_POINT ( 'NONE',  ( 0.07497316781761000082, 0.000000000000000000, -2.824973347946000413 ) ) ;
#32533 = CARTESIAN_POINT ( 'NONE',  ( 18.27150181675463259, 2.367044107065569669, 12.37568780170008864 ) ) ;
#32534 = CARTESIAN_POINT ( 'NONE',  ( 10.96855433372000022, 5.800069981862000290, 4.929813314009000358 ) ) ;
#32535 = CARTESIAN_POINT ( 'NONE',  ( 10.96261261415000021, 7.423557921018999473, 6.118074476279000251 ) ) ;
#32536 = CARTESIAN_POINT ( 'NONE',  ( 9.853545867770625577, -3.141341610201948686, 7.331958223794097229 ) ) ;
#32537 = DIRECTION ( 'NONE',  ( 0.000000000000000000, 0.000000000000000000, -1.000000000000000000 ) ) ;
#32538 = ORIENTED_EDGE ( 'NONE', *, *, #19837, .F. ) ;
#32539 = CARTESIAN_POINT ( 'NONE',  ( 12.08085380679226262, -2.436412096897888180, 12.36221874022169587 ) ) ;
#32540 = CARTESIAN_POINT ( 'NONE',  ( 9.984292290062997566, -3.131390070940299974, -6.995659746333000584 ) ) ;
#32541 = CARTESIAN_POINT ( 'NONE',  ( 13.99999999379500082, 8.815218614167999789, 7.616697584347000394 ) ) ;
#32542 = EDGE_CURVE ( 'NONE', #43802, #32077, #57406, .T. ) ;
#32543 = PLANE ( 'NONE',  #7497 ) ;
#32544 = B_SPLINE_CURVE_WITH_KNOTS ( 'NONE', 3,
 ( #59201, #57565, #62804, #35903 ),
 .UNSPECIFIED., .F., .F.,
 ( 4, 4 ),
 ( 0.000000000000000000, 1.000000000000000000 ),
 .UNSPECIFIED. ) ;
#32545 = ADVANCED_FACE ( 'NONE', ( #7842 ), #50149, .T. ) ;
#32546 = CARTESIAN_POINT ( 'NONE',  ( 10.60026222744819790, 3.225465054973100099, -8.138001937130599828 ) ) ;
#32547 = CARTESIAN_POINT ( 'NONE',  ( 12.78109913421143062, 0.7192906882580830663, 12.57945229568000123 ) ) ;
#32548 = CARTESIAN_POINT ( 'NONE',  ( 8.534482780410998615, 3.011620138462000273, 8.801434747080000065 ) ) ;
#32549 = CARTESIAN_POINT ( 'NONE',  ( 24.63329111161720419, -10.83443034947476136, -3.855530962446055643 ) ) ;
#32550 = CARTESIAN_POINT ( 'NONE',  ( 12.70218814580025679, 3.116819717849788063, 12.28621950321773326 ) ) ;
#32551 = CARTESIAN_POINT ( 'NONE',  ( 17.89019624313940326, -3.590943193543576495, -11.99920113072214534 ) ) ;
#32552 = CARTESIAN_POINT ( 'NONE',  ( 10.32533997688000049, 4.243109097101799954, -6.385465081946999355 ) ) ;
#32553 = CARTESIAN_POINT ( 'NONE',  ( 8.163776391448005043, 3.396249911995000481, -6.162465440825001473 ) ) ;
#32554 =( BOUNDED_SURFACE ( )  B_SPLINE_SURFACE ( 3, 3, ( 
 ( #15860, #69000, #42096, #5373, #32305, #63050, #21112, #4672, #57821, #20420, #9578 ),
 ( #42780, #31606, #58855, #53614, #10273, #48365, #52928, #5024, #21789, #52578, #26014 ),
 ( #43123, #14838, #47343, #36159, #57471, #52233, #46999, #63404, #20766, #68301, #9930 ),
 ( #58172, #39265, #16549, #22828, #54296, #11642, #44176, #17597, #7439, #17945, #37879 ) ),
 .UNSPECIFIED., .F., .F., .F. ) 
 B_SPLINE_SURFACE_WITH_KNOTS ( ( 4, 4 ),
 ( 4, 1, 1, 1, 1, 1, 1, 1, 4 ),
 ( 0.000000000000000000, 1.000000000000000000 ),
 ( -0.004668278336391999857, 0.000000000000000000, 0.03269534097185999855, 0.06255479614191999937, 0.08986301827556000821, 0.1148786485006000058, 0.1378153831697999931, 0.1587710662428999941, 0.1687086804768000159 ),
 .UNSPECIFIED. ) 
 GEOMETRIC_REPRESENTATION_ITEM ( )  RATIONAL_B_SPLINE_SURFACE ( (
 ( 1.221011660805000121, 1.221011660805000121, 1.221011660805000121, 1.221011660805000121, 1.221011660805000121, 1.221011660805000121, 1.221011660805000121, 1.221011660805000121, 1.221011660805000121, 1.221011660805000121, 1.221011660805000121),
 ( 0.9263294463983999805, 0.9263294463983999805, 0.9263294463983999805, 0.9263294463983999805, 0.9263294463983999805, 0.9263294463983999805, 0.9263294463983999805, 0.9263294463983999805, 0.9263294463983999805, 0.9263294463983999805, 0.9263294463983999805),
 ( 0.9263294463983999805, 0.9263294463983999805, 0.9263294463983999805, 0.9263294463983999805, 0.9263294463983999805, 0.9263294463983999805, 0.9263294463983999805, 0.9263294463983999805, 0.9263294463983999805, 0.9263294463983999805, 0.9263294463983999805),
 ( 1.221011660805000121, 1.221011660805000121, 1.221011660805000121, 1.221011660805000121, 1.221011660805000121, 1.221011660805000121, 1.221011660805000121, 1.221011660805000121, 1.221011660805000121, 1.221011660805000121, 1.221011660805000121) ) ) 
 REPRESENTATION_ITEM ( '' )  SURFACE ( )  );
#32555 = CARTESIAN_POINT ( 'NONE',  ( 10.63743278041000018, 3.721476136598000028, -8.997092462634000753 ) ) ;
#32556 = CARTESIAN_POINT ( 'NONE',  ( 9.612308556530413384, 3.034755127822595266, 8.468084591989956778 ) ) ;
#32558 = CARTESIAN_POINT ( 'NONE',  ( 12.19849796498733951, 2.650903666209170062, 12.41512439138481128 ) ) ;
#32557 = CARTESIAN_POINT ( 'NONE',  ( 7.758693699415004197, 5.085317049932003286, 6.543835681441004581 ) ) ;
#32559 = DIRECTION ( 'NONE',  ( 0.5298945027589778700, -0.5996715052829758585, -0.5996714948181758320 ) ) ;
#32560 = EDGE_LOOP ( 'NONE', ( #7327, #3859, #40788, #36232 ) ) ;
#32561 = CARTESIAN_POINT ( 'NONE',  ( 12.22418410612670314, 0.2308773533104517828, 12.69717962854873150 ) ) ;
#32562 = CARTESIAN_POINT ( 'NONE',  ( 23.84019040512217913, -9.641975614964733765, -9.401257029815200283 ) ) ;
#32563 = CARTESIAN_POINT ( 'NONE',  ( 17.55505043854144276, 0.7192913403693119712, -12.57945229203838267 ) ) ;
#32564 = CARTESIAN_POINT ( 'NONE',  ( 17.74741402327983053, 1.780171064306780071, -12.47366677608254015 ) ) ;
#32565 = CIRCLE ( 'NONE', #2427, 1.800000000000000044 ) ;
#32566 = CARTESIAN_POINT ( 'NONE',  ( 12.13805290469199427, -2.231685852207996312, 13.82098778992224730 ) ) ;
#32567 = CARTESIAN_POINT ( 'NONE',  ( 11.04499918297000072, 2.754540059510000027, 5.176258675770000650 ) ) ;
#32568 = FACE_OUTER_BOUND ( 'NONE', #7705, .T. ) ;
#32569 = ORIENTED_EDGE ( 'NONE', *, *, #11820, .T. ) ;
#32570 = B_SPLINE_CURVE_WITH_KNOTS ( 'NONE', 3,
 ( #61309, #29164, #56410, #19001, #56760, #29520, #51500, #40665, #46613, #57088, #9188, #40328, #50473, #35434, #3597, #3940, #13764, #56060 ),
 .UNSPECIFIED., .F., .F.,
 ( 4, 2, 2, 2, 2, 2, 2, 2, 4 ),
 ( 0.000000000000000000, 0.1250000000000000000, 0.2500000000000000000, 0.3750000000000000000, 0.5000000000000000000, 0.6250000000000000000, 0.7500000000000000000, 0.8750000000000000000, 1.000000000000000000 ),
 .UNSPECIFIED. ) ;
#32571 = CARTESIAN_POINT ( 'NONE',  ( 12.22252627677945291, 11.15475449699942523, -3.361665977246885095 ) ) ;
#32572 = CARTESIAN_POINT ( 'NONE',  ( 9.842730320956407652, 2.713277070382849043, -7.026830998939262329 ) ) ;
#32573 = CARTESIAN_POINT ( 'NONE',  ( 9.617013408676374553, -5.079309631299753214, -8.329427714267961136 ) ) ;
#32574 = CARTESIAN_POINT ( 'NONE',  ( 18.33131097850136371, -3.122881743056324488, 11.22368843778173364 ) ) ;
#32575 = CARTESIAN_POINT ( 'NONE',  ( 17.80628805164905870, 1.927626392034356595, -12.56668820897845329 ) ) ;
#32576 = CARTESIAN_POINT ( 'NONE',  ( 9.650818738817875442, -3.048937241343601112, 8.326721469190600189 ) ) ;
#32577 = CARTESIAN_POINT ( 'NONE',  ( 11.53979707368350027, 3.569730287184500472, 8.251775607861899786 ) ) ;
#32578 = EDGE_CURVE ( 'NONE', #63182, #22430, #50163, .T. ) ;
#32579 = EDGE_CURVE ( 'NONE', #57524, #58532, #64250, .T. ) ;
#32580 = DIRECTION ( 'NONE',  ( 0.000000000000000000, -1.000000000000000000, 0.000000000000000000 ) ) ;
#32581 = CARTESIAN_POINT ( 'NONE',  ( 10.75101814679000078, -2.478465696309000155, -7.438303690845000204 ) ) ;
#32582 = CARTESIAN_POINT ( 'NONE',  ( 11.25962254157670905, 4.169672662336058266, -8.360248390549317676 ) ) ;
#32583 = CARTESIAN_POINT ( 'NONE',  ( 11.50001544675000176, -11.50879548944698527, 5.112724829059166254 ) ) ;
#32584 = CARTESIAN_POINT ( 'NONE',  ( 24.23036450625643923, 9.028689804025722410, -9.024522586024058768 ) ) ;
#32585 = DIRECTION ( 'NONE',  ( -0.8660254037844289376, 0.000000000000000000, -0.5000000000000169864 ) ) ;
#32586 = VERTEX_POINT ( 'NONE', #24608 ) ;
#32587 = CARTESIAN_POINT ( 'NONE',  ( 9.093935841232999806, 2.156584729807999867, -7.959751745006000689 ) ) ;
#32588 = CARTESIAN_POINT ( 'NONE',  ( 12.20794988689359961, -3.544213289744700290, 6.606015074393400077 ) ) ;
#32589 = ORIENTED_EDGE ( 'NONE', *, *, #59901, .T. ) ;
#32590 = CARTESIAN_POINT ( 'NONE',  ( 18.01279121882208045, -2.925678518064911859, 13.57390968381829488 ) ) ;
#32591 = CARTESIAN_POINT ( 'NONE',  ( 11.26072066707849828, -3.023932655881500065, -6.909591111168198907 ) ) ;
#32592 = ORIENTED_EDGE ( 'NONE', *, *, #32578, .T. ) ;
#32593 = CARTESIAN_POINT ( 'NONE',  ( 11.27234208742519783, 3.445253572379500362, 6.627995351445298944 ) ) ;
#32594 = CARTESIAN_POINT ( 'NONE',  ( 5.873758560667790007, -0.9662729582186857513, -0.5911492727768954403 ) ) ;
#32595 = CARTESIAN_POINT ( 'NONE',  ( 9.051550650638001017, 2.899999999999999911, 6.227445478845999638 ) ) ;
#32596 = CARTESIAN_POINT ( 'NONE',  ( 18.40429364930200151, -2.938801558760000265, 11.32979830910000096 ) ) ;
#32597 = B_SPLINE_CURVE_WITH_KNOTS ( 'NONE', 3,
 ( #58877, #31979, #58528, #5045 ),
 .UNSPECIFIED., .F., .F.,
 ( 4, 4 ),
 ( 0.000000000000000000, 1.000000000000000000 ),
 .UNSPECIFIED. ) ;
#32598 = CARTESIAN_POINT ( 'NONE',  ( 3.350000000000000089, 0.000000000000000000, 0.000000000000000000 ) ) ;
#32599 = CARTESIAN_POINT ( 'NONE',  ( 12.31508838510828951, 0.3880332711109533150, -13.89271023030988061 ) ) ;
#32600 = DIRECTION ( 'NONE',  ( 1.000000000000000000, 0.000000000000000000, 0.000000000000000000 ) ) ;
#32601 = CARTESIAN_POINT ( 'NONE',  ( 10.69578225082999978, -5.505007625740000243, -7.759264430206000540 ) ) ;
#32602 = CARTESIAN_POINT ( 'NONE',  ( 11.09999965054999826, 12.24999851416000141, 0.000000000000000000 ) ) ;
#32603 = VERTEX_POINT ( 'NONE', #56773 ) ;
#32604 = ADVANCED_FACE ( 'NONE', ( #51182 ), #45931, .T. ) ;
#32606 = EDGE_CURVE ( 'NONE', #35475, #24715, #58442, .T. ) ;
#32605 = CARTESIAN_POINT ( 'NONE',  ( 9.567560841232999991, 5.349936549139000519, -7.138437102151999447 ) ) ;
#32607 = ORIENTED_EDGE ( 'NONE', *, *, #58862, .F. ) ;
#32608 = CARTESIAN_POINT ( 'NONE',  ( 11.09999999999999964, 5.299999999999999822, -5.160242713806000303 ) ) ;
#32609 = SHAPE_REPRESENTATION_RELATIONSHIP ( 'NONE' , 'NONE' ,  #15732, #61967 ) ;
#32610 = EDGE_CURVE ( 'NONE', #58820, #62111, #61324, .T. ) ;
#32611 = VERTEX_POINT ( 'NONE', #35110 ) ;
#32612 = CARTESIAN_POINT ( 'NONE',  ( 18.00298204921611855, -3.099842930870032376, -13.65268125596126758 ) ) ;
#32613 = CARTESIAN_POINT ( 'NONE',  ( 17.80118387294175974, -3.074517463812005857, -12.29895906470767919 ) ) ;
#32614 = CARTESIAN_POINT ( 'NONE',  ( 10.59991574914826451, -2.968501058370544232, 5.041504506945282849 ) ) ;
#32615 = DIRECTION ( 'NONE',  ( -1.000000000000000000, 0.000000000000000000, -3.164702532202999971E-14 ) ) ;
#32616 = CARTESIAN_POINT ( 'NONE',  ( 10.46085355684000007, -5.403406918566000527, 7.721809917403000156 ) ) ;
#32617 = CARTESIAN_POINT ( 'NONE',  ( 8.433148997460000018, -5.167567567567999731, 6.822293592207000934 ) ) ;
#32618 = CARTESIAN_POINT ( 'NONE',  ( 12.23550883753393848, -0.2581888431706775844, 13.89679013629345228 ) ) ;
#32619 = ORIENTED_EDGE ( 'NONE', *, *, #28539, .F. ) ;
#32620 = CARTESIAN_POINT ( 'NONE',  ( 6.613728317541999857, 5.172411450403999744, -8.246583185469999577 ) ) ;
#32621 = CARTESIAN_POINT ( 'NONE',  ( 18.34010937327100166, 12.07342271643000053, -3.473919584753000223 ) ) ;
#32622 = CARTESIAN_POINT ( 'NONE',  ( 9.226900131858625898, 3.814237572305042345, 6.645000240129933289 ) ) ;
#32623 = CARTESIAN_POINT ( 'NONE',  ( 5.038386820982999836, 0.2713898421607000566, 1.457004540053999930 ) ) ;
#32624 = AXIS2_PLACEMENT_3D ( 'NONE', #31508, #26613, #52830 ) ;
#32625 = EDGE_CURVE ( 'NONE', #51578, #30294, #35908, .T. ) ;
#32626 = CARTESIAN_POINT ( 'NONE',  ( 25.59994555223600088, -0.6895522877783650806, 11.26073925913298801 ) ) ;
#32627 = CARTESIAN_POINT ( 'NONE',  ( 18.38411421680242341, 11.69918008064787074, -4.474081357806680259 ) ) ;
#32628 = CIRCLE ( 'NONE', #25936, 5.000000000000000000 ) ;
#32629 = CARTESIAN_POINT ( 'NONE',  ( 10.13061232742999884, -2.189322372303999842, -7.101642112140999608 ) ) ;
#32630 = ORIENTED_EDGE ( 'NONE', *, *, #37871, .F. ) ;
#32631 = CARTESIAN_POINT ( 'NONE',  ( 10.97197891098000078, 5.142532440135999749, -4.995747455712000296 ) ) ;
#32632 = CARTESIAN_POINT ( 'NONE',  ( 12.80505043854146940, -3.125000000000000000, -25.00000000000000000 ) ) ;
#32633 = DIRECTION ( 'NONE',  ( 0.000000000000000000, -0.3222656952305000266, -0.9466492601157001641 ) ) ;
#32634 = DIRECTION ( 'NONE',  ( 0.000000000000000000, -1.000000000000000000, 0.000000000000000000 ) ) ;
#32635 = DIRECTION ( 'NONE',  ( 0.000000000000000000, 0.000000000000000000, 1.000000000000000000 ) ) ;
#32636 = CARTESIAN_POINT ( 'NONE',  ( 10.52435971519499880, 4.532462039660099862, -6.614211617270199461 ) ) ;
#32637 = CARTESIAN_POINT ( 'NONE',  ( 10.21722949779699974, 4.557226039164599563, -8.335668797826500054 ) ) ;
#32639 = CARTESIAN_POINT ( 'NONE',  ( 8.363921074485642038, 5.017958344788086222, -6.290581482856832274 ) ) ;
#32638 = CARTESIAN_POINT ( 'NONE',  ( 9.671747021775999542, -4.651672637235799712, 6.928134003122899287 ) ) ;
#32640 = CARTESIAN_POINT ( 'NONE',  ( 4.500000000000000000, 0.000000000000000000, 0.000000000000000000 ) ) ;
#32641 = ORIENTED_EDGE ( 'NONE', *, *, #49304, .T. ) ;
#32642 = CARTESIAN_POINT ( 'NONE',  ( 11.13746005378019888, 5.161099018038999731, 8.120007936598501175 ) ) ;
#32643 = CARTESIAN_POINT ( 'NONE',  ( 9.691080333872001518, -5.335644368206000188, 8.701217921043999937 ) ) ;
#32644 = CARTESIAN_POINT ( 'NONE',  ( 9.657025935145998830, 3.834207658792500251, 8.629711178834000407 ) ) ;
#32645 = CARTESIAN_POINT ( 'NONE',  ( 5.634820040245294592, -12.96111452106133122, 2.364727959305737315 ) ) ;
#32646 = CARTESIAN_POINT ( 'NONE',  ( 9.657547180956999711, -5.333447643521000536, 6.049925825719999928 ) ) ;
#32647 = CARTESIAN_POINT ( 'NONE',  ( 9.889653591487839179, -2.705485811107797289, 8.717674038414637394 ) ) ;
#32648 = CARTESIAN_POINT ( 'NONE',  ( 10.81905590578999998, -2.899999999999999911, -6.571291218949999902 ) ) ;
#32649 = B_SPLINE_CURVE_WITH_KNOTS ( 'NONE', 3,
 ( #59238, #5753, #27436, #29444, #55996, #6442, #50750, #27095, #8100, #22522, #49099, #28127, #48410, #48758, #516, #64470, #43164, #16594 ),
 .UNSPECIFIED., .F., .F.,
 ( 4, 2, 2, 2, 2, 2, 2, 2, 4 ),
 ( 0.000000000000000000, 0.1250000000000003331, 0.2500000000000006661, 0.3750000000000009992, 0.5000000000000013323, 0.6250000000000009992, 0.7500000000000006661, 0.8750000000000003331, 1.000000000000000000 ),
 .UNSPECIFIED. ) ;
#32650 = CARTESIAN_POINT ( 'NONE',  ( 9.204063610504999104, -3.588011994494999968, -8.416028484082099581 ) ) ;
#32651 = AXIS2_PLACEMENT_3D ( 'NONE', #28164, #1248, #28873 ) ;
#32652 = CARTESIAN_POINT ( 'NONE',  ( 5.123560349866000507, 0.1309856596131999951, 1.229810997071999923 ) ) ;
#32653 = CARTESIAN_POINT ( 'NONE',  ( 11.24760529021567734, -3.959614718189205185, 6.626811228128840270 ) ) ;
#32654 = FACE_OUTER_BOUND ( 'NONE', #52030, .T. ) ;
#32655 = ORIENTED_EDGE ( 'NONE', *, *, #39900, .F. ) ;
#32656 = EDGE_CURVE ( 'NONE', #66492, #64300, #15111, .T. ) ;
#32657 = ADVANCED_FACE ( 'NONE', ( #13323 ), #11641, .T. ) ;
#32658 = CARTESIAN_POINT ( 'NONE',  ( 11.81825954179440075, -3.333768806796900019, 6.946434658287599540 ) ) ;
#32659 = CARTESIAN_POINT ( 'NONE',  ( 11.51518179236248862, 3.819003318705799899, -6.652923384986699773 ) ) ;
#32660 = CARTESIAN_POINT ( 'NONE',  ( 10.99999975383417627, -5.062986770486452848, -7.366608021396839234 ) ) ;
#32661 = DIRECTION ( 'NONE',  ( 0.7071067811865475727, -0.7071067811865475727, 0.000000000000000000 ) ) ;
#32662 = CARTESIAN_POINT ( 'NONE',  ( 1.009306799208383065, 3.058252359239904905, -1.762666431298142600 ) ) ;
#32663 = ORIENTED_EDGE ( 'NONE', *, *, #11007, .F. ) ;
#32664 = CARTESIAN_POINT ( 'NONE',  ( 25.19548857725200008, -11.71503324258999967, -2.904521392034999927 ) ) ;
#32665 = CONTEXT_DEPENDENT_SHAPE_REPRESENTATION ( #67270, #30661 ) ;
#32666 = CARTESIAN_POINT ( 'NONE',  ( 11.31389666366019853, -4.045876550911099656, -8.532487796751999198 ) ) ;
#32667 = CARTESIAN_POINT ( 'NONE',  ( 18.17906593022460626, 0.04061720351850793553, 12.69993396819095643 ) ) ;
#32668 = FACE_OUTER_BOUND ( 'NONE', #34130, .T. ) ;
#32669 = DIRECTION ( 'NONE',  ( 0.000000000000000000, 0.000000000000000000, -1.000000000000000000 ) ) ;
#32671 = AXIS2_PLACEMENT_3D ( 'NONE', #53068, #10408, #16684 ) ;
#32670 = CARTESIAN_POINT ( 'NONE',  ( 10.32169598648999909, 4.766524664146899681, -7.956401575444799867 ) ) ;
#32672 = ORIENTED_EDGE ( 'NONE', *, *, #51778, .F. ) ;
#32673 = CARTESIAN_POINT ( 'NONE',  ( 10.91307648679999964, -2.096298111716999646, 7.827187677719999570 ) ) ;
#32674 = CARTESIAN_POINT ( 'NONE',  ( 17.65850582825305892, 3.116720375661584441, -13.52313201004804277 ) ) ;
#32675 = EDGE_LOOP ( 'NONE', ( #34552, #39213, #15385, #11142, #56916 ) ) ;
#32676 = DIRECTION ( 'NONE',  ( 1.000000000000000000, 0.000000000000000000, 0.000000000000000000 ) ) ;
#32677 = CARTESIAN_POINT ( 'NONE',  ( 8.738433059624998833, -5.414909314743000301, 8.890670256079998168 ) ) ;
#32678 = CARTESIAN_POINT ( 'NONE',  ( 8.126014158770999529, 5.189036231907000030, -8.048606212067999977 ) ) ;
#32679 = ORIENTED_EDGE ( 'NONE', *, *, #15057, .F. ) ;
#32680 = CARTESIAN_POINT ( 'NONE',  ( 23.61437304120291358, -13.25092132859138339, 4.104831388036656037 ) ) ;
#32681 = CARTESIAN_POINT ( 'NONE',  ( 6.926370280408000291, 3.391196421714000042, -9.121921547671998809 ) ) ;
#32682 = CARTESIAN_POINT ( 'NONE',  ( 8.645206806413895606, 4.733533093241248935, -8.663332967138325458 ) ) ;
#32683 = CARTESIAN_POINT ( 'NONE',  ( 9.458877515925783186, 5.224829427659542169, 8.067569713668623521 ) ) ;
#32684 = ORIENTED_EDGE ( 'NONE', *, *, #52080, .T. ) ;
#32685 = CARTESIAN_POINT ( 'NONE',  ( 10.28315099603999982, -2.387772357283999725, 7.684266429524000408 ) ) ;
#32686 = CARTESIAN_POINT ( 'NONE',  ( 24.67558927346200193, 12.15674323158999925, -3.025799392731000292 ) ) ;
#32687 = ORIENTED_EDGE ( 'NONE', *, *, #66377, .F. ) ;
#32688 = FACE_OUTER_BOUND ( 'NONE', #5139, .T. ) ;
#32689 = CARTESIAN_POINT ( 'NONE',  ( 10.72801694037999987, -3.751276547904999870, -8.836912395451999913 ) ) ;
#32690 = EDGE_CURVE ( 'NONE', #24715, #57059, #42599, .T. ) ;
#32691 = EDGE_LOOP ( 'NONE', ( #52784, #39737, #22572, #6159 ) ) ;
#32692 = CARTESIAN_POINT ( 'NONE',  ( 8.722809814040999754, 4.614409247670200109, 6.705428891605899722 ) ) ;
#32693 = CARTESIAN_POINT ( 'NONE',  ( 18.07980642414615247, 0.3396162601617248034, -13.89441893193946775 ) ) ;
#32694 = CARTESIAN_POINT ( 'NONE',  ( 4.887490849967999651, -0.5294863075682000320, 1.313799488281000016 ) ) ;
#32695 = CARTESIAN_POINT ( 'NONE',  ( 8.021095686590996365, 4.867149410870005077, -6.207068544376001640 ) ) ;
#32696 = CARTESIAN_POINT ( 'NONE',  ( 16.44809435262699893, 3.299700711820999555, 11.83394467541999973 ) ) ;
#32697 = CARTESIAN_POINT ( 'NONE',  ( 5.449999267937000624, 6.217248937900999058E-14, 3.708144902247999495E-14 ) ) ;
#32698 = B_SPLINE_SURFACE_WITH_KNOTS ( 'NONE', 3, 3, ( 
 ( #52049, #67783, #9397, #13385 ),
 ( #4152, #29120, #2530, #14662 ),
 ( #25492, #41569, #55683, #68464 ),
 ( #44851, #25145, #56018, #20244 ),
 ( #41230, #4493, #7429, #39597 ),
 ( #28777, #50089, #18619, #66500 ),
 ( #66158, #60919, #13035, #7781 ),
 ( #34707, #59027, #10435, #37698 ),
 ( #5875, #43294, #31776, #42603 ),
 ( #36675, #57995, #42946, #32805 ),
 ( #27214, #32462, #992, #21953 ),
 ( #11130, #48884, #54119, #22302 ),
 ( #15348, #63218, #10095, #58678 ),
 ( #6217, #52746, #20936, #31430 ) ),
 .UNSPECIFIED., .F., .F., .F.,
 ( 4, 1, 1, 1, 1, 1, 1, 1, 1, 1, 1, 4 ),
 ( 4, 4 ),
 ( -0.01123015465801999874, 0.000000000000000000, 0.1111111111111000027, 0.2222222222222000054, 0.3333333333333000081, 0.4444444444444000109, 0.5555555555555999891, 0.6666666666667000474, 0.7777777777777999946, 0.8888888888888999418, 1.000000000000000000, 1.008787911365999879 ),
 ( -0.2206650672665999846, 1.220665067267000081 ),
 .UNSPECIFIED. ) ;
#32699 = CARTESIAN_POINT ( 'NONE',  ( 9.326707230296040763, -3.961060040642459423, 9.239254357279243379 ) ) ;
#32700 = B_SPLINE_CURVE_WITH_KNOTS ( 'NONE', 3,
 ( #25465, #11703, #59253, #27112, #32360, #37587, #16263, #43535, #5770, #46798 ),
 .UNSPECIFIED., .F., .F.,
 ( 4, 2, 2, 2, 4 ),
 ( 0.000000000000000000, 0.2500000000000002220, 0.5000000000000004441, 0.7500000000000002220, 1.000000000000000000 ),
 .UNSPECIFIED. ) ;
#32701 = ORIENTED_EDGE ( 'NONE', *, *, #38169, .T. ) ;
#32702 = CARTESIAN_POINT ( 'NONE',  ( 10.30047009227000032, 4.027768540959000276, 9.431354536774000152 ) ) ;
#32703 = CARTESIAN_POINT ( 'NONE',  ( 9.964039158770999549, 3.485905350467000119, -9.275749134703000109 ) ) ;
#32704 = CARTESIAN_POINT ( 'NONE',  ( 18.04463993611876660, -11.57310880395660746, 4.789662202686257864 ) ) ;
#32705 = CARTESIAN_POINT ( 'NONE',  ( 12.75683046442381929, 1.789027279908999679, -13.88522190323555172 ) ) ;
#32706 = VECTOR ( 'NONE', #48812, 1000.000000000000000 ) ;
#32707 = CYLINDRICAL_SURFACE ( 'NONE', #10311, 1.350000000000000533 ) ;
#32708 = B_SPLINE_CURVE_WITH_KNOTS ( 'NONE', 3,
 ( #52584, #26019, #62720, #20772, #4339 ),
 .UNSPECIFIED., .F., .F.,
 ( 4, 1, 4 ),
 ( 0.000000000000000000, 0.5000000000000000000, 1.000000000000000000 ),
 .UNSPECIFIED. ) ;
#32709 = CARTESIAN_POINT ( 'NONE',  ( 10.21608469020999976, -5.961703525007000515, 7.319668113368000384 ) ) ;
#32710 = EDGE_CURVE ( 'NONE', #57302, #14855, #23452, .T. ) ;
#32711 = CARTESIAN_POINT ( 'NONE',  ( 18.09667340657836121, -0.3125520594525368900, 13.89528657259775102 ) ) ;
#32712 = FACE_OUTER_BOUND ( 'NONE', #68884, .T. ) ;
#32713 = ORIENTED_EDGE ( 'NONE', *, *, #24053, .F. ) ;
#32714 = EDGE_LOOP ( 'NONE', ( #9920, #8524, #21854, #23638 ) ) ;
#32715 = CARTESIAN_POINT ( 'NONE',  ( 12.40639171141861929, -0.4813567170522365934, 13.88878047999798682 ) ) ;
#32716 = CARTESIAN_POINT ( 'NONE',  ( 12.40965214754211843, -0.4840331165010965941, -13.88865521357928934 ) ) ;
#32717 = CARTESIAN_POINT ( 'NONE',  ( 9.634027193201999850, -3.042970193091000031, 8.588108172435999776 ) ) ;
#32718 = CARTESIAN_POINT ( 'NONE',  ( 17.78593649205363647, -0.5808626952866734472, -13.88365973251372765 ) ) ;
#32719 = CARTESIAN_POINT ( 'NONE',  ( 8.721004440379999778, -5.983034890242000081, 7.440798487724999966 ) ) ;
#32720 = DIRECTION ( 'NONE',  ( 0.2392860387991979920, 0.9709491189736919603, 1.627359028554984806E-14 ) ) ;
#32722 = CARTESIAN_POINT ( 'NONE',  ( 9.819055905797000605, -2.899999999999999911, -6.571291218949999902 ) ) ;
#32721 = CARTESIAN_POINT ( 'NONE',  ( 10.53897570133299944, -3.061513547538400104, 6.630731591496600075 ) ) ;
#32723 = CONICAL_SURFACE ( 'NONE', #28232, 12.44999944941000081, 0.7853981146832407223 ) ;
#32724 = CARTESIAN_POINT ( 'NONE',  ( 10.96533729122639933, 2.859653469230999612, -7.470001566214039990 ) ) ;
#32725 = CARTESIAN_POINT ( 'NONE',  ( 12.09999999999999964, -2.935681553670999921, 6.844464917182299324 ) ) ;
#32726 = CARTESIAN_POINT ( 'NONE',  ( 10.90000000000000036, 0.2999999999999999889, 4.902439024389999567 ) ) ;
#32727 = CARTESIAN_POINT ( 'NONE',  ( 18.16408092502819116, 0.1418569258565852420, 12.69895512164409368 ) ) ;
#32728 = CARTESIAN_POINT ( 'NONE',  ( 8.472124462996665883, 5.100000000000000533, 6.567732269893666874 ) ) ;
#32729 = CARTESIAN_POINT ( 'NONE',  ( 18.47825479160223239, -3.085175724103950579, 12.13916519603823119 ) ) ;
#32730 = VERTEX_POINT ( 'NONE', #17870 ) ;
#32731 = CARTESIAN_POINT ( 'NONE',  ( 7.481081853206999810, -2.374041291348000016, 8.293390875797999939 ) ) ;
#32732 = CARTESIAN_POINT ( 'NONE',  ( 8.374639158773000247, 2.721111233225000259, -6.936528696292000085 ) ) ;
#32733 = CARTESIAN_POINT ( 'NONE',  ( 10.90000000296000060, -5.100000000009000445, 5.160242730682999657 ) ) ;
#32734 = CARTESIAN_POINT ( 'NONE',  ( 9.118435835444707038, -5.100000000000000533, 6.178531823617834817 ) ) ;
#32735 = CARTESIAN_POINT ( 'NONE',  ( 0.6173104132283999679, -3.219656052487999798, -1.007448552055000057 ) ) ;
#32736 = CARTESIAN_POINT ( 'NONE',  ( 9.593930206849998754, 5.250000000000000000, -7.500000000000000000 ) ) ;
#32737 = CARTESIAN_POINT ( 'NONE',  ( 2.457020142123000461, 2.375218314457999913, -2.913196738027000077 ) ) ;
#32738 = ORIENTED_EDGE ( 'NONE', *, *, #11302, .F. ) ;
#32739 = EDGE_CURVE ( 'NONE', #6003, #4443, #47394, .T. ) ;
#32740 = EDGE_CURVE ( 'NONE', #18501, #54794, #122, .T. ) ;
#32741 = CARTESIAN_POINT ( 'NONE',  ( 9.154341692891295068, 5.250000716804955836, -7.336371291557481022 ) ) ;
#32742 = DIRECTION ( 'NONE',  ( 0.000000000000000000, -1.000000000000000000, 0.000000000000000000 ) ) ;
#32743 = CARTESIAN_POINT ( 'NONE',  ( 18.20615948710261733, 2.797893282243137492, -12.28544817418252855 ) ) ;
#32744 = CARTESIAN_POINT ( 'NONE',  ( 7.890669427268998781, -4.660296165433000404, 6.322498843348999920 ) ) ;
#32745 = CARTESIAN_POINT ( 'NONE',  ( 8.924954719592001595, 4.158911560497999815, 5.873540104660999184 ) ) ;
#32746 = EDGE_LOOP ( 'NONE', ( #65773, #32846, #52878, #48937 ) ) ;
#32747 = CARTESIAN_POINT ( 'NONE',  ( 6.709746979523999677, 1.411445953971000034, -0.4053984660343999957 ) ) ;
#32748 = ADVANCED_FACE ( 'NONE', ( #28708 ), #29012, .F. ) ;
#32749 = EDGE_CURVE ( 'NONE', #52849, #46692, #17243, .T. ) ;
#32750 = AXIS2_PLACEMENT_3D ( 'NONE', #48933, #24003, #56504 ) ;
#32751 = CARTESIAN_POINT ( 'NONE',  ( 7.648620280409000216, 3.500992739020000410, -8.983283880004998778 ) ) ;
#32752 = CARTESIAN_POINT ( 'NONE',  ( 8.359995882382332155, -3.256579615318050624, 9.091912762848693319 ) ) ;
#32753 = CARTESIAN_POINT ( 'NONE',  ( 9.548063610505000298, -3.475294527116599586, 6.333351572150998976 ) ) ;
#32754 = ORIENTED_EDGE ( 'NONE', *, *, #42441, .T. ) ;
#32755 = CARTESIAN_POINT ( 'NONE',  ( 10.06493315628555862, -5.349942305088194239, -7.500003965376651038 ) ) ;
#32756 = B_SPLINE_CURVE_WITH_KNOTS ( 'NONE', 3,
 ( #13180, #17372, #34509, #38700, #2330, #7923, #56154, #55820 ),
 .UNSPECIFIED., .F., .F.,
 ( 4, 2, 2, 4 ),
 ( 0.000000000000000000, 0.2500000000000002776, 0.5000000000000005551, 1.000000000000000000 ),
 .UNSPECIFIED. ) ;
#32757 = CARTESIAN_POINT ( 'NONE',  ( 6.271693173016666734, 0.7554284705563509839, -1.310679582531385945 ) ) ;
#32758 = ORIENTED_EDGE ( 'NONE', *, *, #60920, .T. ) ;
#32759 = CARTESIAN_POINT ( 'NONE',  ( 25.10989042599555177, 2.855873493246296579, -11.47557929325230930 ) ) ;
#32760 = CARTESIAN_POINT ( 'NONE',  ( 16.42348875342600323, 3.378076265369000186, 11.11016813414000204 ) ) ;
#32761 = CARTESIAN_POINT ( 'NONE',  ( 17.88507584039978582, -0.5311540453515659621, -13.88634387573209494 ) ) ;
#32762 = ORIENTED_EDGE ( 'NONE', *, *, #54091, .F. ) ;
#32763 = DIRECTION ( 'NONE',  ( 0.000000000000000000, 0.000000000000000000, 1.000000000000000000 ) ) ;
#32764 = CARTESIAN_POINT ( 'NONE',  ( 7.000000000000000000, 8.307879248642999315, 4.307879248643000203 ) ) ;
#32765 = CARTESIAN_POINT ( 'NONE',  ( 10.44635971519499940, 4.459622816450200311, -6.735384833238199143 ) ) ;
#32766 = CARTESIAN_POINT ( 'NONE',  ( 8.987238607305510385, -2.413693965082394310, 6.702889251169676932 ) ) ;
#32767 = CARTESIAN_POINT ( 'NONE',  ( 24.60000000000000142, 0.000000000000000000, 0.000000000000000000 ) ) ;
#32768 = ORIENTED_EDGE ( 'NONE', *, *, #33229, .T. ) ;
#32769 = CARTESIAN_POINT ( 'NONE',  ( 9.143920280410000601, 5.791553967443999973, 7.752111263209999770 ) ) ;
#32770 = EDGE_CURVE ( 'NONE', #54361, #38721, #53502, .T. ) ;
#32771 = ORIENTED_EDGE ( 'NONE', *, *, #39665, .T. ) ;
#32772 = CARTESIAN_POINT ( 'NONE',  ( 10.05226354018333446, -2.907767014557177898, 6.870476274536374994 ) ) ;
#32773 = CIRCLE ( 'NONE', #35033, 2.749999999999999556 ) ;
#32774 = CARTESIAN_POINT ( 'NONE',  ( 8.350387243830999395, 4.599999999999999645, -6.632262360512000576 ) ) ;
#32775 = CARTESIAN_POINT ( 'NONE',  ( 10.96237843380999877, 5.422598724373000501, -4.905487645836000610 ) ) ;
#32776 = ORIENTED_EDGE ( 'NONE', *, *, #8990, .F. ) ;
#32777 = CARTESIAN_POINT ( 'NONE',  ( 12.46308409927492455, -1.976751580904480443, -12.55819113744975546 ) ) ;
#32778 = VECTOR ( 'NONE', #12933, 1000.000000000000000 ) ;
#32779 = CARTESIAN_POINT ( 'NONE',  ( 10.69809687351599869, 4.327184855449106138, -6.282534154164607365 ) ) ;
#32780 = DIRECTION ( 'NONE',  ( 1.000000000000000000, 0.000000000000000000, 0.000000000000000000 ) ) ;
#32781 = CARTESIAN_POINT ( 'NONE',  ( 6.999999691988000095, 0.000000000000000000, 0.000000000000000000 ) ) ;
#32782 = CARTESIAN_POINT ( 'NONE',  ( 12.25828482332356728, -2.997587547359419791, -13.67532635696712440 ) ) ;
#32783 = CARTESIAN_POINT ( 'NONE',  ( 11.65456516821461008, -3.197083038490000195, -8.310318115935698913 ) ) ;
#32784 = CARTESIAN_POINT ( 'NONE',  ( 12.15658143854451545, -2.853298863235071092, 12.27345178217744603 ) ) ;
#32785 = CARTESIAN_POINT ( 'NONE',  ( 17.91266776300918551, -3.012678901972745571, 12.31722829471395464 ) ) ;
#32786 = ORIENTED_EDGE ( 'NONE', *, *, #64769, .T. ) ;
#32787 = CARTESIAN_POINT ( 'NONE',  ( 10.80502344389999791, -5.125258734743999511, -6.817099149379099110 ) ) ;
#32788 = ORIENTED_EDGE ( 'NONE', *, *, #52896, .T. ) ;
#32789 = CARTESIAN_POINT ( 'NONE',  ( 11.61689913334100055, -12.44392429648999965, -1.730928413625999918 ) ) ;
#32790 = CARTESIAN_POINT ( 'NONE',  ( 9.535554719593998030, 3.927090956378999742, -9.230892435423001530 ) ) ;
#32791 = CARTESIAN_POINT ( 'NONE',  ( 10.95552360838999917, 4.744046441415999738, -9.198140387677000263 ) ) ;
#32792 = CARTESIAN_POINT ( 'NONE',  ( 5.100000001045000175, 0.000000000000000000, -1.699999998954999869 ) ) ;
#32793 = EDGE_CURVE ( 'NONE', #60220, #43301, #36651, .T. ) ;
#32794 = CARTESIAN_POINT ( 'NONE',  ( 24.14469595025496318, -12.92580541902093216, -3.214657694676578803 ) ) ;
#32795 = CARTESIAN_POINT ( 'NONE',  ( 24.45266148221099911, 12.43950837972999857, 3.093335738978999938 ) ) ;
#32796 = CARTESIAN_POINT ( 'NONE',  ( 16.86666666323366925, 3.595157417865990634, 11.99793599502776154 ) ) ;
#32797 = ORIENTED_EDGE ( 'NONE', *, *, #9654, .T. ) ;
#32798 = EDGE_CURVE ( 'NONE', #3842, #20189, #40008, .T. ) ;
#32799 = CARTESIAN_POINT ( 'NONE',  ( 10.87835931249053267, -5.126777126165768195, 6.752018918838227357 ) ) ;
#32800 = CARTESIAN_POINT ( 'NONE',  ( 9.600491906670001185, 5.206545077004999911, 8.585111878242999595 ) ) ;
#32801 = LINE ( 'NONE', #43985, #39319 ) ;
#32802 = CARTESIAN_POINT ( 'NONE',  ( 12.02677869730533011, -4.403502086956500250, 8.295667533166499297 ) ) ;
#32803 = CARTESIAN_POINT ( 'NONE',  ( 18.16715644869600155, 3.024463723863999753, -11.49930835314999911 ) ) ;
#32804 = VECTOR ( 'NONE', #14908, 1000.000000000000000 ) ;
#32805 = CARTESIAN_POINT ( 'NONE',  ( 11.13611325966000010, 9.539967198755999078, -6.380887600928000225 ) ) ;
#32806 = CARTESIAN_POINT ( 'NONE',  ( 10.16210844129514790, 5.577934564358349334, 6.690706121504116588 ) ) ;
#32807 = CARTESIAN_POINT ( 'NONE',  ( 23.99190355937800234, -9.434386195893999627, -9.573065527095000249 ) ) ;
#32808 = FACE_OUTER_BOUND ( 'NONE', #56071, .T. ) ;
#32809 = CARTESIAN_POINT ( 'NONE',  ( 11.72781722417300188, -3.253150999210000283, 11.33706231867000014 ) ) ;
#32810 = ORIENTED_EDGE ( 'NONE', *, *, #42921, .F. ) ;
#32811 = CARTESIAN_POINT ( 'NONE',  ( 9.617285841233000454, 5.306366356490000769, -7.996450761531000317 ) ) ;
#32812 = CARTESIAN_POINT ( 'NONE',  ( 7.260660218006000477, 0.07416480754746999915, 1.248399527803000009 ) ) ;
#32813 = CARTESIAN_POINT ( 'NONE',  ( 18.13009756288981222, 2.254948952832145359, 13.72233930590318884 ) ) ;
#32814 = CARTESIAN_POINT ( 'NONE',  ( 24.35146665670700017, 8.929414329884000523, -9.054894786836999998 ) ) ;
#32815 = CARTESIAN_POINT ( 'NONE',  ( 10.29657053952199952, -4.502253688815499366, -6.324815923923999605 ) ) ;
#32816 = VERTEX_POINT ( 'NONE', #6672 ) ;
#32817 = FACE_OUTER_BOUND ( 'NONE', #63117, .T. ) ;
#32818 = CARTESIAN_POINT ( 'NONE',  ( 8.309482780410998970, 2.905861847853000057, 8.940690431604000565 ) ) ;
#32819 = AXIS2_PLACEMENT_3D ( 'NONE', #29370, #27982, #60480 ) ;
#32821 = CARTESIAN_POINT ( 'NONE',  ( 11.51961669203094196, 5.030276287827526005, 7.824983907773938263 ) ) ;
#32820 = CARTESIAN_POINT ( 'NONE',  ( 9.260829719593999698, 4.861259245430999520, -8.806664389576001284 ) ) ;
#32822 = CARTESIAN_POINT ( 'NONE',  ( 3.274540278792131165, 3.257195673479903686, -0.06878223238550713881 ) ) ;
#32823 = ORIENTED_EDGE ( 'NONE', *, *, #45146, .T. ) ;
#32824 = CARTESIAN_POINT ( 'NONE',  ( 9.757669403192000601, 4.489270656625000022, 5.986034819543999852 ) ) ;
#32825 = CARTESIAN_POINT ( 'NONE',  ( 17.87892170566136230, -1.864264957476227780, -13.87532524069350259 ) ) ;
#32826 = CARTESIAN_POINT ( 'NONE',  ( 11.36333594839950045, 4.659759757475400832, 8.256087240512899328 ) ) ;
#32827 = CARTESIAN_POINT ( 'NONE',  ( 11.24052627608000066, -2.774025043188999895, 6.782107572692000375 ) ) ;
#32828 = CARTESIAN_POINT ( 'NONE',  ( 7.432076984665996200, 3.524670056070998037, 6.650527748631001046 ) ) ;
#32830 = VERTEX_POINT ( 'NONE', #19415 ) ;
#32829 = AXIS2_PLACEMENT_3D ( 'NONE', #28808, #16566, #1186 ) ;
#32831 = CARTESIAN_POINT ( 'NONE',  ( 24.25374608244500152, 12.19813778996000053, -3.308085337617999944 ) ) ;
#32832 = EDGE_CURVE ( 'NONE', #4446, #25728, #29985, .T. ) ;
#32833 = EDGE_CURVE ( 'NONE', #2928, #8734, #31674, .T. ) ;
#32834 = B_SPLINE_CURVE_WITH_KNOTS ( 'NONE', 3,
 ( #13519, #34150, #55469, #1987 ),
 .UNSPECIFIED., .F., .F.,
 ( 4, 4 ),
 ( 0.000000000000000000, 1.000000000000000000 ),
 .UNSPECIFIED. ) ;
#32835 = B_SPLINE_CURVE_WITH_KNOTS ( 'NONE', 3,
 ( #23912, #65167, #12741, #13439, #61321, #65864, #43863, #60977, #7143, #38613, #44572, #7839, #34071, #59933, #22874, #45249, #50482, #1905 ),
 .UNSPECIFIED., .F., .F.,
 ( 4, 2, 2, 2, 2, 2, 2, 2, 4 ),
 ( 0.000000000000000000, 0.1250000000000000000, 0.2500000000000000000, 0.3750000000000000000, 0.5000000000000000000, 0.6250000000000000000, 0.7500000000000000000, 0.8750000000000000000, 1.000000000000000000 ),
 .UNSPECIFIED. ) ;
#32837 = CARTESIAN_POINT ( 'NONE',  ( 11.26847231345999845, -2.565616654150999931, -7.116622328138999976 ) ) ;
#32836 = CARTESIAN_POINT ( 'NONE',  ( 12.68129448069100107, -12.04903608036000051, 3.200077553391999619 ) ) ;
#32838 = CARTESIAN_POINT ( 'NONE',  ( 7.806951053071116142, -4.387620322963519115, 9.195870376599991403 ) ) ;
#32839 = CARTESIAN_POINT ( 'NONE',  ( 9.815199780373001559, -2.813634733202999616, 8.848854270764999086 ) ) ;
#32840 = CARTESIAN_POINT ( 'NONE',  ( 23.51521485843800008, 2.989497430995999849, 13.81461181470000099 ) ) ;
#32841 = ORIENTED_EDGE ( 'NONE', *, *, #42613, .F. ) ;
#32842 = CARTESIAN_POINT ( 'NONE',  ( 5.646693173016667622, -1.310679582531386611, -0.7554284705563495406 ) ) ;
#32843 = CARTESIAN_POINT ( 'NONE',  ( 12.15456516821461008, -3.197083038490000195, 6.689681884064299311 ) ) ;
#32844 = CARTESIAN_POINT ( 'NONE',  ( 8.325004567511003373, 2.868524053507002236, 6.316175840085996640 ) ) ;
#32845 = CARTESIAN_POINT ( 'NONE',  ( 10.39918582084299992, 3.253651555277099927, 8.362701637490498996 ) ) ;
#32846 = ORIENTED_EDGE ( 'NONE', *, *, #39147, .F. ) ;
#32847 = B_SPLINE_SURFACE_WITH_KNOTS ( 'NONE', 3, 3, ( 
 ( #52615, #25703, #52968, #63787 ),
 ( #4021, #31645, #31998, #41445 ),
 ( #68339, #53311, #62754, #41102 ),
 ( #20804, #4710, #57865, #62417 ),
 ( #14538, #35855, #26054, #14873 ),
 ( #36195, #9616, #20457, #41785 ),
 ( #16923, #22865, #27091, #38254 ),
 ( #32342, #53651, #65512, #16589 ),
 ( #64466, #53991, #5747, #48406 ),
 ( #512, #49436, #22516, #27431 ) ),
 .UNSPECIFIED., .F., .F., .F.,
 ( 4, 1, 1, 1, 1, 1, 1, 4 ),
 ( 4, 4 ),
 ( 0.04183311431307000505, 0.1428571428570999946, 0.2857142857143000203, 0.4285714285713999594, 0.5714285714286000406, 0.7142857142856999797, 0.8571428571429000609, 0.9292981235707000742 ),
 ( -0.1917799910644999994, 1.191756862851000021 ),
 .UNSPECIFIED. ) ;
#32848 = CARTESIAN_POINT ( 'NONE',  ( 9.211104719594999324, 5.462898983065000102, -8.055936939571999744 ) ) ;
#32849 = CARTESIAN_POINT ( 'NONE',  ( 12.18817755169812678, 2.859236737589999411, -12.27131451573979071 ) ) ;
#32850 = CARTESIAN_POINT ( 'NONE',  ( 11.59590547754519996, -2.684394667508000154, 7.458246194669389872 ) ) ;
#32851 = ADVANCED_FACE ( 'NONE', ( #58929 ), #65242, .T. ) ;
#32852 = CARTESIAN_POINT ( 'NONE',  ( 9.210653099680683908, 3.646553657477270782, -8.850805462952818559 ) ) ;
#32853 = CARTESIAN_POINT ( 'NONE',  ( 11.09999999999999964, -6.354980837003999738, -5.388690576903999663 ) ) ;
#32854 = ORIENTED_EDGE ( 'NONE', *, *, #17695, .T. ) ;
#32855 = CARTESIAN_POINT ( 'NONE',  ( 9.621289888149652469, 3.647081445668302724, 8.849739427182289120 ) ) ;
#32856 = CARTESIAN_POINT ( 'NONE',  ( 11.00000000000000000, -5.200000000000000178, -5.864181267619000160 ) ) ;
#32857 = VERTEX_POINT ( 'NONE', #5092 ) ;
#32858 = CARTESIAN_POINT ( 'NONE',  ( 12.44013165738125615, -3.102068138921904694, -12.21217476962502069 ) ) ;
#32859 = CARTESIAN_POINT ( 'NONE',  ( 11.19102897915239936, 4.256858847510399890, 6.529961657816500065 ) ) ;
#32860 = CARTESIAN_POINT ( 'NONE',  ( 9.385781899350000401, 4.980865465981000106, 6.433345686594999613 ) ) ;
#32861 = CARTESIAN_POINT ( 'NONE',  ( 10.44486820642000069, 4.964088085664999817, -9.083609801695999408 ) ) ;
#32862 = CARTESIAN_POINT ( 'NONE',  ( 8.187982051047001164, 4.942702676859997979, 6.196150354213001421 ) ) ;
#32863 = CARTESIAN_POINT ( 'NONE',  ( 12.79999998712400178, 11.53033693765999779, -4.891431908114999949 ) ) ;
#32864 = DIRECTION ( 'NONE',  ( -0.000000000000000000, 1.000000000000000000, 0.000000000000000000 ) ) ;
#32865 = CARTESIAN_POINT ( 'NONE',  ( 17.93858415168864440, -0.6105138165312175014, -12.58520200551375368 ) ) ;
#32866 = CARTESIAN_POINT ( 'NONE',  ( 12.19239630165612276, 2.623612345200928342, -12.42193400453944285 ) ) ;
#32867 = CARTESIAN_POINT ( 'NONE',  ( 10.62072335273219892, -3.602909566644000083, -8.569396700949999612 ) ) ;
#32868 = CARTESIAN_POINT ( 'NONE',  ( 7.609454719589999527, 3.276311362504999991, 5.841989464160999290 ) ) ;
#32869 = ORIENTED_EDGE ( 'NONE', *, *, #28372, .F. ) ;
#32870 = VECTOR ( 'NONE', #11012, 1000.000000000000000 ) ;
#32871 = CARTESIAN_POINT ( 'NONE',  ( 23.89320776801300283, -11.54071136931999852, 2.936967729253997295 ) ) ;
#32872 = CARTESIAN_POINT ( 'NONE',  ( 7.225632159681131483, 2.625029116607175972, 7.496691097032143425 ) ) ;
#32873 = CARTESIAN_POINT ( 'NONE',  ( 11.55259020248000112, 12.34178403982000205, 1.785089783152000065 ) ) ;
#32874 = VECTOR ( 'NONE', #21483, 1000.000000000000227 ) ;
#32875 = CARTESIAN_POINT ( 'NONE',  ( 18.20792762907817419, 2.166426970554221842, 12.41237440719187290 ) ) ;
#32876 = CARTESIAN_POINT ( 'NONE',  ( 11.07243245105999918, 6.084025226422999921, 5.191545849810999869 ) ) ;
#32877 = CARTESIAN_POINT ( 'NONE',  ( 11.12952936848999919, 8.831357469829999474, 6.732325948479999767 ) ) ;
#32878 = ADVANCED_FACE ( 'NONE', ( #16270 ), #26182, .F. ) ;
#32879 = CARTESIAN_POINT ( 'NONE',  ( 10.25881222268762549, -3.837269700090108593, 6.640319176431033199 ) ) ;
#32880 = DIRECTION ( 'NONE',  ( 0.000000000000000000, -1.000000000000000000, 0.000000000000000000 ) ) ;
#32881 = ORIENTED_EDGE ( 'NONE', *, *, #43371, .T. ) ;
#32882 = CARTESIAN_POINT ( 'NONE',  ( 12.11828080172250921, -2.711598415135501483, 12.30476978351483197 ) ) ;
#32883 = CARTESIAN_POINT ( 'NONE',  ( 9.832317406968998696, -3.813190776280700245, -8.486886322867700727 ) ) ;
#32884 = CARTESIAN_POINT ( 'NONE',  ( 10.34947814066000049, 4.457562099971999814, 6.154877938302999674 ) ) ;
#32885 = APPLICATION_CONTEXT ( 'automotive_design' ) ;
#32886 = CARTESIAN_POINT ( 'NONE',  ( 10.68904248846000016, -2.568964727443000307, 7.728094434513999467 ) ) ;
#32887 = B_SPLINE_CURVE_WITH_KNOTS ( 'NONE', 3,
 ( #55019, #65142, #28812, #13067 ),
 .UNSPECIFIED., .F., .F.,
 ( 4, 4 ),
 ( 0.000000000000000000, 1.000000000000000000 ),
 .UNSPECIFIED. ) ;
#32888 = CARTESIAN_POINT ( 'NONE',  ( 11.01456785386839954, 3.053605396817899997, -8.136888821800198457 ) ) ;
#32889 = CARTESIAN_POINT ( 'NONE',  ( 12.15464131684817950, -0.3178346465811148769, 12.59599179195193663 ) ) ;
#32890 = CARTESIAN_POINT ( 'NONE',  ( 7.854823341228001077, 4.561643343497000735, 6.153061759127000485 ) ) ;
#32891 = CARTESIAN_POINT ( 'NONE',  ( 9.533434135307000901, 2.564753581125000181, 6.150586364588000343 ) ) ;
#32892 = CARTESIAN_POINT ( 'NONE',  ( 12.18852176789201813, 2.603049415106243103, 12.42696357550859787 ) ) ;
#32893 = CARTESIAN_POINT ( 'NONE',  ( 7.598073341229000022, 3.554857159507999853, 8.889479859586000288 ) ) ;
#32894 = CARTESIAN_POINT ( 'NONE',  ( 10.17764828895399809, 5.001141961424000471, -8.046814291299300592 ) ) ;
#32895 = CARTESIAN_POINT ( 'NONE',  ( 18.05078025084782567, -0.5250004125410587807, 12.58906021966015842 ) ) ;
#32896 = CARTESIAN_POINT ( 'NONE',  ( 10.46298584122999920, 3.993164721578000176, -6.140176455708999725 ) ) ;
#32897 = CARTESIAN_POINT ( 'NONE',  ( 11.21253483539785556, 3.661009989788314822, 6.691360637068768824 ) ) ;
#32899 = CARTESIAN_POINT ( 'NONE',  ( 25.21376063843823445, 11.24064175245759678, 3.343247825242493754 ) ) ;
#32898 = CARTESIAN_POINT ( 'NONE',  ( 9.724226531639931892, 2.899999999999999911, -6.304440313831950249 ) ) ;
#32900 = CARTESIAN_POINT ( 'NONE',  ( 8.941941226754561711, 5.237474851784025276, 6.943363493799808772 ) ) ;
#32901 = ORIENTED_EDGE ( 'NONE', *, *, #18399, .T. ) ;
#32902 = CIRCLE ( 'NONE', #8352, 11.26964301940000013 ) ;
#32903 = CARTESIAN_POINT ( 'NONE',  ( 12.47664625033035968, 0.5322368321508662570, 12.68499235032564521 ) ) ;
#32904 = CARTESIAN_POINT ( 'NONE',  ( 23.96071917867679346, -9.430644054855381597, -9.306896137895602550 ) ) ;
#32905 = CARTESIAN_POINT ( 'NONE',  ( 3.500000000000000000, 1.113524292603000010, -3.231029921506000324 ) ) ;
#32906 = CARTESIAN_POINT ( 'NONE',  ( 8.766480666858997850, 4.289077172771600388, 6.682599852064000423 ) ) ;
#32907 = CARTESIAN_POINT ( 'NONE',  ( 12.17655141950255882, -2.882034090924107339, 13.70014555608275941 ) ) ;
#32908 = CARTESIAN_POINT ( 'NONE',  ( 11.12988950403999944, 2.715405747272999548, 4.847983218306000097 ) ) ;
#32909 = CARTESIAN_POINT ( 'NONE',  ( 23.86816321758700354, 3.656111997911000167, -13.23100399352999901 ) ) ;
#32910 = EDGE_LOOP ( 'NONE', ( #66817, #56956, #58856, #43971, #63568, #26497, #1768, #11679, #22529, #65831, #48203, #47389 ) ) ;
#32911 = ADVANCED_FACE ( 'NONE', ( #5776 ), #22814, .T. ) ;
#32912 = EDGE_CURVE ( 'NONE', #7311, #63350, #31702, .T. ) ;
#32913 = CARTESIAN_POINT ( 'NONE',  ( 12.17041389168972643, 11.12724491010661332, -3.450620876805502668 ) ) ;
#32914 = CARTESIAN_POINT ( 'NONE',  ( 18.29999330150736014, -11.02846243710336616, 3.754394858745019103 ) ) ;
#32915 = CARTESIAN_POINT ( 'NONE',  ( 18.49586274151939591, -2.771911498359158621, -11.31551287271714656 ) ) ;
#32916 = DIRECTION ( 'NONE',  ( 1.000000000000000000, 0.000000000000000000, 0.000000000000000000 ) ) ;
#32917 = FACE_OUTER_BOUND ( 'NONE', #24041, .T. ) ;
#32918 = CARTESIAN_POINT ( 'NONE',  ( 17.93883077754965072, 2.006280984399065659, -12.55302554764001499 ) ) ;
#32919 = CARTESIAN_POINT ( 'NONE',  ( 10.96207813434000045, 5.399835028078000754, 7.743264559064000352 ) ) ;
#32920 = CONICAL_SURFACE ( 'NONE', #2780, 1.449999999965999375, 0.7853981633972997312 ) ;
#32921 = CARTESIAN_POINT ( 'NONE',  ( 8.328909422836733967, 2.650170743412998409, -7.263558743223875958 ) ) ;
#32922 = DIRECTION ( 'NONE',  ( 0.8843050093870327144, 0.1786786010978065053, -0.4313682972620159761 ) ) ;
#32923 = CARTESIAN_POINT ( 'NONE',  ( 10.84974435320999930, -5.265000209383999596, -6.385811305909999902 ) ) ;
#32924 = CARTESIAN_POINT ( 'NONE',  ( 12.70934146434746559, 1.792598170639653876, 13.88476440024012604 ) ) ;
#32925 = CARTESIAN_POINT ( 'NONE',  ( 6.305026506349999948, 1.500000000000000000, 0.000000000000000000 ) ) ;
#32926 = CARTESIAN_POINT ( 'NONE',  ( 24.36958145701300182, 12.05823614978999991, 3.270605474396000023 ) ) ;
#32927 = DIRECTION ( 'NONE',  ( 0.9999999999938153916, -3.516990153967782703E-06, -1.152484550329262306E-11 ) ) ;
#32928 = EDGE_CURVE ( 'NONE', #32611, #57225, #40860, .T. ) ;
#32929 = VECTOR ( 'NONE', #54434, 1000.000000000000000 ) ;
#32930 = ORIENTED_EDGE ( 'NONE', *, *, #801, .F. ) ;
#32931 = CARTESIAN_POINT ( 'NONE',  ( 7.452411699453480587, 2.247457503992560390, 7.471653287871163229 ) ) ;
#32932 = CARTESIAN_POINT ( 'NONE',  ( 11.05103166480599874, -5.000984463463999496, 7.429424106427209296 ) ) ;
#32933 = ORIENTED_EDGE ( 'NONE', *, *, #26214, .F. ) ;
#32934 = CARTESIAN_POINT ( 'NONE',  ( 18.16447345601865848, -2.360953327207878871, 13.70196990072541077 ) ) ;
#32935 = CARTESIAN_POINT ( 'NONE',  ( 11.40425819896749893, -5.255890247626999745, -7.736761623643599428 ) ) ;
#32936 = EDGE_LOOP ( 'NONE', ( #42583, #57689, #49245, #37734 ) ) ;
#32937 = ADVANCED_FACE ( 'NONE', ( #56788 ), #19721, .T. ) ;
#32938 = CARTESIAN_POINT ( 'NONE',  ( 10.52435971519499880, 4.532462039660099862, 8.385788382729799650 ) ) ;
#32939 = CARTESIAN_POINT ( 'NONE',  ( 5.582903883426274305, 1.131774569182460111, 0.04058116965622569905 ) ) ;
#32940 = CARTESIAN_POINT ( 'NONE',  ( 23.76527109147985328, 3.280149080713666176, -13.20035194756249020 ) ) ;
#32941 = CARTESIAN_POINT ( 'NONE',  ( 17.76930066282600151, -3.251864118589000263, 11.33740735155000046 ) ) ;
#32942 = CARTESIAN_POINT ( 'NONE',  ( 24.34833292274466743, -12.15210578639278793, 3.256146931800457001 ) ) ;
#32943 = CARTESIAN_POINT ( 'NONE',  ( 11.10000000115999974, 8.827960611545998759, -6.689729118101999994 ) ) ;
#32944 = CARTESIAN_POINT ( 'NONE',  ( 17.55505043854147118, -1.760910691117812954, -12.47634535983622861 ) ) ;
#32945 = CARTESIAN_POINT ( 'NONE',  ( 10.18512684885999953, -5.526147823900999789, -7.556025229989000280 ) ) ;
#32946 = CARTESIAN_POINT ( 'NONE',  ( 11.06622274902552405, 4.530851388969875160, -8.944471867876563564 ) ) ;
#32947 = VERTEX_POINT ( 'NONE', #41044 ) ;
#32948 = CARTESIAN_POINT ( 'NONE',  ( 8.970860841232001448, 4.131080973160000447, -6.108642999115999395 ) ) ;
#32949 = ORIENTED_EDGE ( 'NONE', *, *, #50073, .T. ) ;
#32950 = CARTESIAN_POINT ( 'NONE',  ( 15.96663488596630742, 8.445622082970144717, 8.216900471613380219 ) ) ;
#32951 = EDGE_LOOP ( 'NONE', ( #66242, #67703, #17066, #67799 ) ) ;
#32952 = CARTESIAN_POINT ( 'NONE',  ( 17.79094441639333013, -1.825864066368119598, -13.88043842654159299 ) ) ;
#32953 = SURFACE_STYLE_FILL_AREA ( #59517 ) ;
#32954 = PRODUCT_DEFINITION_FORMATION_WITH_SPECIFIED_SOURCE ( 'ANY', '', #29962, .NOT_KNOWN. ) ;
#32955 = CARTESIAN_POINT ( 'NONE',  ( 7.974113208588001100, 4.561154361229000642, -6.272154006859000930 ) ) ;
#32956 = FACE_OUTER_BOUND ( 'NONE', #53881, .T. ) ;
#32957 = CARTESIAN_POINT ( 'NONE',  ( 12.51718303290431678, 3.054853725429544919, 13.53993614671056811 ) ) ;
#32958 = CARTESIAN_POINT ( 'NONE',  ( 4.900006121741999010, 2.000000000000000000, 0.000000000000000000 ) ) ;
#32959 = LINE ( 'NONE', #27723, #20286 ) ;
#32960 = CARTESIAN_POINT ( 'NONE',  ( 12.66238154463050769, 0.6088408278571617593, 13.88204686096232621 ) ) ;
#32961 = ORIENTED_EDGE ( 'NONE', *, *, #53515, .T. ) ;
#32962 = CARTESIAN_POINT ( 'NONE',  ( 7.190590560818999499, 2.534482666265000184, -7.314862106114000007 ) ) ;
#32963 = DIRECTION ( 'NONE',  ( 1.000000000000000000, -3.631529569662070274E-15, 1.174496025128702085E-14 ) ) ;
#32964 = CARTESIAN_POINT ( 'NONE',  ( 9.809470517051625649, 4.641899585206984646, 6.905443702049931964 ) ) ;
#32965 = CARTESIAN_POINT ( 'NONE',  ( 5.013225847549999337, -0.7131102322965999774, 1.331318456966000152 ) ) ;
#32966 = CARTESIAN_POINT ( 'NONE',  ( 9.128895280414001334, 3.880154689736000417, -9.060377011187000562 ) ) ;
#32967 = AXIS2_PLACEMENT_3D ( 'NONE', #65562, #17686, #32388 ) ;
#32968 = DIRECTION ( 'NONE',  ( 0.000000000000000000, 1.000000000000000000, 0.000000000000000000 ) ) ;
#32969 = CARTESIAN_POINT ( 'NONE',  ( 10.28773706650000008, -5.077599250153999932, -5.991350640809000261 ) ) ;
#32970 = ADVANCED_FACE ( 'NONE', ( #45613 ), #45207, .F. ) ;
#32971 = ORIENTED_EDGE ( 'NONE', *, *, #11180, .F. ) ;
#32972 = CARTESIAN_POINT ( 'NONE',  ( 23.60000000000000142, -2.258942858049999725, 12.29419282279000036 ) ) ;
#32973 = LINE ( 'NONE', #36844, #29295 ) ;
#32974 = PRESENTATION_STYLE_ASSIGNMENT (( #55335 ) ) ;
#32975 = CARTESIAN_POINT ( 'NONE',  ( 29.60000000000000142, 2.052090884164000168E-07, -7.720759220056000238 ) ) ;
#32976 = CARTESIAN_POINT ( 'NONE',  ( 5.399999743830999677, 0.000000000000000000, 0.000000000000000000 ) ) ;
#32977 = CARTESIAN_POINT ( 'NONE',  ( 5.875859839683334584, 1.460959015002472494, 0.3926218265389233020 ) ) ;
#32978 = CARTESIAN_POINT ( 'NONE',  ( 11.35034208742529849, 3.369365911179700301, -8.491292290686200062 ) ) ;
#32979 = CARTESIAN_POINT ( 'NONE',  ( 9.963938025973998691, 3.477805217445600228, -6.642005297568199573 ) ) ;
#32981 = CARTESIAN_POINT ( 'NONE',  ( 8.455089073534951538, 5.099985254049173022, -6.566459068862928738 ) ) ;
#32980 = CARTESIAN_POINT ( 'NONE',  ( 10.76090035061499961, -3.768906505327899836, 6.664354444139199529 ) ) ;
#32982 = CARTESIAN_POINT ( 'NONE',  ( 6.999998782146999332, 11.95749337870000062, -3.642574926947999892 ) ) ;
#32983 = EDGE_LOOP ( 'NONE', ( #64355, #41635, #3535, #68318 ) ) ;
#32984 = CARTESIAN_POINT ( 'NONE',  ( 11.06456920625009843, 4.037149028919880145, 8.532838639935999225 ) ) ;
#32985 = CARTESIAN_POINT ( 'NONE',  ( 9.347248564704999652, -4.028326926800000152, 9.469437404464001062 ) ) ;
#32986 = CARTESIAN_POINT ( 'NONE',  ( 10.11295058442699890, 4.453199839589800035, 8.548019252390998801 ) ) ;
#32987 = CARTESIAN_POINT ( 'NONE',  ( 5.534341697420971151, -12.89488364876162763, 2.703816489143735513 ) ) ;
#32988 = CARTESIAN_POINT ( 'NONE',  ( 11.06924082387999952, -5.425685649895999774, 8.012912555523998392 ) ) ;
#32989 = CARTESIAN_POINT ( 'NONE',  ( 24.37816251333097028, 12.29708173412044481, 3.190021852498594601 ) ) ;
#32990 = DIRECTION ( 'NONE',  ( 0.000000000000000000, 0.9466492601157001641, -0.3222656952305000266 ) ) ;
#32991 = CIRCLE ( 'NONE', #46372, 11.50000000000000178 ) ;
#32992 = EDGE_CURVE ( 'NONE', #67585, #65548, #23983, .T. ) ;
#32993 = EDGE_CURVE ( 'NONE', #37807, #36315, #5803, .T. ) ;
#32994 = STYLED_ITEM ( 'NONE', ( #55575 ), #7037 ) ;
#32995 = CARTESIAN_POINT ( 'NONE',  ( 9.609329965421999020, -4.697624103824200148, -8.222608407156599242 ) ) ;
#32996 = EDGE_CURVE ( 'NONE', #19638, #57425, #10254, .T. ) ;
#32997 = CARTESIAN_POINT ( 'NONE',  ( 6.657863159730999847, -1.329569516000000062, 0.3446834961110000206 ) ) ;
#32998 = B_SPLINE_SURFACE_WITH_KNOTS ( 'NONE', 3, 3, ( 
 ( #49447, #39312, #65520, #50486, #34428, #66559, #13443, #1556, #60633, #2588, #18678, #22878, #60981, #17648, #23918, #23230, #55740, #55391, #60290, #13093, #29533, #33728, #7843, #7487, #55045, #19017, #50836, #61664, #45253, #28840, #13779, #7147, #3953, #19708, #68615 ),
 ( #51513, #24609, #20388, #30543, #15147, #51854, #19358, #25291, #20047, #63368, #41028, #41716, #46625, #8871, #62011, #4643, #63016, #58140, #36466, #41375, #25636, #40681, #67931, #62684, #67584, #14123, #52545, #35449, #25981, #47310, #14468, #56774, #30209, #14806, #30888 ),
 ( #57787, #36124, #46966, #3613, #57439, #9544, #62351, #24947, #20734, #46280, #42063, #15495, #35787, #57102, #9200, #52201, #4302, #9900, #68268, #31238, #36821, #29874, #51183, #3279, #45932, #67241, #68968, #787, #64050, #63716, #4992, #53581, #27710, #47654, #27358 ),
 ( #21412, #43786, #42408, #64392, #49025, #65082, #17204, #16172, #22445, #10240, #21079, #53918, #38178, #59508, #32605, #22100, #42746, #37158, #53235, #16855, #31921, #43444, #6019, #37495, #5335, #38532, #32948, #58821, #31577, #11606, #54260, #48332, #11267, #10929, #5675 ) ),
 .UNSPECIFIED., .F., .F., .F.,
 ( 4, 4 ),
 ( 4, 1, 1, 1, 1, 1, 1, 1, 1, 1, 1, 1, 1, 1, 1, 1, 1, 1, 1, 1, 1, 1, 1, 1, 1, 1, 1, 1, 1, 1, 1, 1, 4 ),
 ( -0.1039370721279000015, 1.103937072127999963 ),
 ( -0.02000000000000000042, 0.01250000000000000069, 0.04499999999999999833, 0.07749999999999999944, 0.1100000000000000006, 0.1424999999999999878, 0.1749999999999999889, 0.2074999999999999900, 0.2399999999999999911, 0.2725000000000000200, 0.3049999999999999933, 0.3375000000000000222, 0.3699999999999999956, 0.4025000000000000244, 0.4349999999999999978, 0.4675000000000000266, 0.5000000000000000000, 0.5324999999999999734, 0.5649999999999999467, 0.5975000000000000311, 0.6300000000000000044, 0.6624999999999999778, 0.6949999999999999512, 0.7275000000000000355, 0.7600000000000000089, 0.7924999999999999822, 0.8249999999999999556, 0.8575000000000000400, 0.8900000000000000133, 0.9224999999999999867, 0.9549999999999999600, 0.9875000000000000444, 1.020000000000000018 ),
 .UNSPECIFIED. ) ;
#32999 = CARTESIAN_POINT ( 'NONE',  ( 7.000000000000001776, 10.08082116580678367, -4.449062842274066121 ) ) ;
#33000 = CARTESIAN_POINT ( 'NONE',  ( 25.49994615399576148, 8.603880941064447896, 7.325437794649206857 ) ) ;
#33001 = CARTESIAN_POINT ( 'NONE',  ( 12.28594988689359901, -3.606563555963900214, 6.728309553046099012 ) ) ;
#33002 = CARTESIAN_POINT ( 'NONE',  ( 23.59999192078999997, 10.30759737717999869, 9.317725909430999209 ) ) ;
#33003 = CARTESIAN_POINT ( 'NONE',  ( 9.266851002542999538, 2.832432432432000269, 6.822293592207000934 ) ) ;
#33004 = CARTESIAN_POINT ( 'NONE',  ( 25.48370471471800158, -8.423010586709999359, 7.952419693825000024 ) ) ;
#33005 = CARTESIAN_POINT ( 'NONE',  ( 12.70687399448022425, 1.760978113263438560, 12.47633584387834027 ) ) ;
#33006 = EDGE_LOOP ( 'NONE', ( #31164, #5847, #53406, #66956 ) ) ;
#33007 = CARTESIAN_POINT ( 'NONE',  ( 25.40244255529000128, -11.40891536676000051, -3.011592991499000060 ) ) ;
#33008 = CARTESIAN_POINT ( 'NONE',  ( 10.69057802013490033, -5.033226574983999946, -7.475947032624040034 ) ) ;
#33009 = CARTESIAN_POINT ( 'NONE',  ( 5.500000000000000000, 0.000000000000000000, 0.000000000000000000 ) ) ;
#33010 = CARTESIAN_POINT ( 'NONE',  ( 25.60000000000000142, -2.023988666086999899, -11.01546541709000060 ) ) ;
#33011 = CARTESIAN_POINT ( 'NONE',  ( 6.999999999999998224, 10.44690841785601698, 4.123972661126250827 ) ) ;
#33012 = CARTESIAN_POINT ( 'NONE',  ( 24.30000000000000071, -3.224868684338999980, 12.03537377768999939 ) ) ;
#33013 = VERTEX_POINT ( 'NONE', #63385 ) ;
#33014 = AXIS2_PLACEMENT_3D ( 'NONE', #2217, #55006, #1869 ) ;
#33015 = CARTESIAN_POINT ( 'NONE',  ( 23.60205915885299888, 9.223492163368996799, 8.025915643339997629 ) ) ;
#33016 = CARTESIAN_POINT ( 'NONE',  ( 17.81506173200506637, 3.068442049787682979, -13.53632421860061186 ) ) ;
#33017 = ORIENTED_EDGE ( 'NONE', *, *, #45232, .F. ) ;
#33018 = ADVANCED_FACE ( 'NONE', ( #16185 ), #3324, .F. ) ;
#33019 = CARTESIAN_POINT ( 'NONE',  ( 13.35262485425079326, 11.51206127779273203, 1.787622147829904362 ) ) ;
#33020 = LINE ( 'NONE', #28122, #48035 ) ;
#33021 = AXIS2_PLACEMENT_3D ( 'NONE', #45040, #28620, #49933 ) ;
#33022 = CARTESIAN_POINT ( 'NONE',  ( 9.509454719593000149, 3.116293075258000478, -6.208411413796000033 ) ) ;
#33023 = ORIENTED_EDGE ( 'NONE', *, *, #2827, .T. ) ;
#33024 = CARTESIAN_POINT ( 'NONE',  ( -0.000000000000000000, 2.824745580908275766, -0.7586348975822421181 ) ) ;
#33025 = CARTESIAN_POINT ( 'NONE',  ( 10.72191429142990060, -3.974927396630719922, -6.183971186511000084 ) ) ;
#33026 = CARTESIAN_POINT ( 'NONE',  ( 8.458985841228999547, 4.642843096736999797, -9.160097874508000615 ) ) ;
#33027 = CARTESIAN_POINT ( 'NONE',  ( 10.45746213570999927, -5.100000000000000533, -6.571291218949999902 ) ) ;
#33028 = CARTESIAN_POINT ( 'NONE',  ( 9.432982363827456140, 5.350302034667164364, 7.637571449422903669 ) ) ;
#33029 = ORIENTED_EDGE ( 'NONE', *, *, #45255, .T. ) ;
#33030 = CARTESIAN_POINT ( 'NONE',  ( 9.075489683949001574, -4.020837068201999820, 8.948702918089999514 ) ) ;
#33031 = CARTESIAN_POINT ( 'NONE',  ( 18.15949994905106735, -2.660112426196167057, -13.63815955517138789 ) ) ;
#33032 = FACE_OUTER_BOUND ( 'NONE', #32006, .T. ) ;
#33033 = ORIENTED_EDGE ( 'NONE', *, *, #62093, .F. ) ;
#33034 = CARTESIAN_POINT ( 'NONE',  ( 9.002599499754321499, 5.050337702473633783, -7.998361244042363261 ) ) ;
#33035 = CARTESIAN_POINT ( 'NONE',  ( 10.23580444037999904, -3.621838308198000345, -8.806219190581000333 ) ) ;
#33036 = ORIENTED_EDGE ( 'NONE', *, *, #29545, .F. ) ;
#33037 = CARTESIAN_POINT ( 'NONE',  ( 9.330709346416998784, 4.907312911337299965, 7.930842873041400232 ) ) ;
#33038 = DIRECTION ( 'NONE',  ( 1.000000000000000000, 0.000000000000000000, 0.000000000000000000 ) ) ;
#33039 = CARTESIAN_POINT ( 'NONE',  ( 4.555929601177000521, -1.554405035535000090, 0.09838377833599000477 ) ) ;
#33040 = CARTESIAN_POINT ( 'NONE',  ( 11.59999999999999964, 3.182579051151299687, -7.174999999999999822 ) ) ;
#33041 = CARTESIAN_POINT ( 'NONE',  ( 8.472537864290000442, 2.899999999999999911, -6.571291218949999902 ) ) ;
#33042 = CARTESIAN_POINT ( 'NONE',  ( 10.67008267378785646, 2.650318246679984391, 7.583525964882096737 ) ) ;
#33043 = CARTESIAN_POINT ( 'NONE',  ( 9.104759580228998672, 3.156743194445300382, 7.701558687214699717 ) ) ;
#33044 = CARTESIAN_POINT ( 'NONE',  ( 12.80505043854144276, 0.6600719421079697113, 13.91436771118226012 ) ) ;
#33045 = ORIENTED_EDGE ( 'NONE', *, *, #57129, .F. ) ;
#33046 = DIRECTION ( 'NONE',  ( -1.000000000000000000, 0.000000000000000000, 0.000000000000000000 ) ) ;
#33047 = CARTESIAN_POINT ( 'NONE',  ( 4.434171084391500095, 0.8317986529663452533, 1.289119990005314520 ) ) ;
#33048 = DIRECTION ( 'NONE',  ( -1.000000000000000000, 0.000000000000000000, 0.000000000000000000 ) ) ;
#33049 = CARTESIAN_POINT ( 'NONE',  ( 12.76358235960661780, 3.123961849445188843, -13.52113151862113938 ) ) ;
#33050 = CARTESIAN_POINT ( 'NONE',  ( 10.19095058442699830, -3.492264136285500253, -6.325866838823999139 ) ) ;
#33051 = CARTESIAN_POINT ( 'NONE',  ( 9.256662271119999730, -4.025830307267999508, 9.295859242339000517 ) ) ;
#33052 = CARTESIAN_POINT ( 'NONE',  ( 18.16600461949966672, 0.1321590433901028427, 13.89915950722681970 ) ) ;
#33053 = VECTOR ( 'NONE', #3296, 1000.000000000000000 ) ;
#33054 = CARTESIAN_POINT ( 'NONE',  ( 24.67558972156300001, -3.457952286748999793, 12.04094770214000043 ) ) ;
#33055 = EDGE_CURVE ( 'NONE', #63838, #37303, #59527, .T. ) ;
#33056 = EDGE_CURVE ( 'NONE', #10018, #23381, #57452, .T. ) ;
#33057 = ORIENTED_EDGE ( 'NONE', *, *, #51224, .T. ) ;
#33058 = ORIENTED_EDGE ( 'NONE', *, *, #36137, .T. ) ;
#33059 = CARTESIAN_POINT ( 'NONE',  ( 10.96876099447000108, 2.333339469804000199, 6.524055942683999021 ) ) ;
#33060 = CARTESIAN_POINT ( 'NONE',  ( 12.18504202262453262, -0.08143095622523290056, 13.89969831568979153 ) ) ;
#33061 = CARTESIAN_POINT ( 'NONE',  ( 12.32512809858833869, -0.4004137792110806782, -13.89223825656353739 ) ) ;
#33062 = CARTESIAN_POINT ( 'NONE',  ( 10.25462442569999943, -2.860634389522000109, 6.604605425112000994 ) ) ;
#33063 = PLANE ( 'NONE',  #35058 ) ;
#33064 = CARTESIAN_POINT ( 'NONE',  ( 7.871558059623000148, -4.780993534312999671, 6.267212032957000467 ) ) ;
#33065 = LINE ( 'NONE', #28520, #42684 ) ;
#33067 = CARTESIAN_POINT ( 'NONE',  ( 23.50387503050299998, -0.02050624307146717284, 13.79998476426676923 ) ) ;
#33066 = CARTESIAN_POINT ( 'NONE',  ( 10.84292546752099895, -5.276153033933000280, 7.588418444866789514 ) ) ;
#33068 = CARTESIAN_POINT ( 'NONE',  ( 10.22272469555899832, 4.639546521693399761, -6.393520617113999549 ) ) ;
#33069 = AXIS2_PLACEMENT_3D ( 'NONE', #13966, #30060, #67765 ) ;
#33070 = B_SPLINE_CURVE_WITH_KNOTS ( 'NONE', 3,
 ( #68430, #63183, #20553, #52710, #959, #28217, #6183, #27181, #1299, #64564, #43613, #6881, #22960, #33119, #261, #32091, #15991, #59680 ),
 .UNSPECIFIED., .F., .F.,
 ( 4, 2, 2, 2, 2, 2, 2, 2, 4 ),
 ( 0.1494581667962512628, 0.2557758959467200111, 0.3620936250971887316, 0.4684113542476574521, 0.5747290833981262281, 0.6810468125485945601, 0.7873645416990631141, 0.8936822708495314460, 1.000000000000000000 ),
 .UNSPECIFIED. ) ;
#33071 = CARTESIAN_POINT ( 'NONE',  ( 24.43232361759900328, -8.806075257782000065, -8.751960807121999864 ) ) ;
#33072 = AXIS2_PLACEMENT_3D ( 'NONE', #41886, #48166, #68789 ) ;
#33073 = CARTESIAN_POINT ( 'NONE',  ( 17.77436674347223189, 11.41733448236052517, -4.609296047865278467 ) ) ;
#33074 = CARTESIAN_POINT ( 'NONE',  ( 17.86760901219547648, -0.5416145769730059678, 12.68445494689096087 ) ) ;
#33075 = CARTESIAN_POINT ( 'NONE',  ( 11.09999999999999964, -5.299999999999999822, 6.469505845987999493 ) ) ;
#33076 = CARTESIAN_POINT ( 'NONE',  ( 18.01268549162643495, -2.926083040860917084, -12.34202569327525012 ) ) ;
#33077 = ORIENTED_EDGE ( 'NONE', *, *, #44565, .T. ) ;
#33079 = CARTESIAN_POINT ( 'NONE',  ( 9.344351860772725615, 2.684670005318823716, -7.853455765640516617 ) ) ;
#33078 = CARTESIAN_POINT ( 'NONE',  ( 7.839808059622000336, -3.084082018960999871, 9.259837032825000591 ) ) ;
#33080 = CARTESIAN_POINT ( 'NONE',  ( 9.898395280408998076, 3.987760651117999711, -9.123263301387000368 ) ) ;
#33081 = EDGE_CURVE ( 'NONE', #8185, #29320, #47560, .T. ) ;
#33082 = CARTESIAN_POINT ( 'NONE',  ( 17.60000000024299993, 11.86189249994999884, -3.298671769835999967 ) ) ;
#33083 = CARTESIAN_POINT ( 'NONE',  ( 24.35365242081699932, 8.885108761826009172, -7.331500822316997734 ) ) ;
#33084 = EDGE_CURVE ( 'NONE', #29332, #68416, #30834, .T. ) ;
#33085 = CARTESIAN_POINT ( 'NONE',  ( 0.3788438179258999949, 2.727922606149000284, -2.252402744047000471 ) ) ;
#33086 = CARTESIAN_POINT ( 'NONE',  ( 11.02812378248509795, 3.583106837161099900, 8.288725998710999576 ) ) ;
#33087 = CARTESIAN_POINT ( 'NONE',  ( 10.16008584122999991, 4.812959680871000678, -8.526582921144999716 ) ) ;
#33088 = EDGE_LOOP ( 'NONE', ( #45466, #11852, #40862, #47501, #27691 ) ) ;
#33089 = CARTESIAN_POINT ( 'NONE',  ( 12.14465108362472634, -0.2970375428997896194, -12.59650273238872487 ) ) ;
#33090 = CARTESIAN_POINT ( 'NONE',  ( 9.933148997456999751, 5.167567567567999731, 6.822293592207000934 ) ) ;
#33091 = CARTESIAN_POINT ( 'NONE',  ( 18.26113864896146666, 2.644667523736219827, -12.31932909903656537 ) ) ;
#33092 = CARTESIAN_POINT ( 'NONE',  ( 5.648274849241552431, 12.08704511044957464, 3.737576519652656248 ) ) ;
#33093 = CARTESIAN_POINT ( 'NONE',  ( 7.769579719591000355, 2.431401017850999935, 7.958393275880999873 ) ) ;
#33094 = ORIENTED_EDGE ( 'NONE', *, *, #40728, .F. ) ;
#33095 = CARTESIAN_POINT ( 'NONE',  ( 6.306432422588000186, 0.8716839254852999375, 1.181818379215999970 ) ) ;
#33096 = CARTESIAN_POINT ( 'NONE',  ( 7.408854719586000392, 5.732054911314000023, -7.535918460973999977 ) ) ;
#33098 = CARTESIAN_POINT ( 'NONE',  ( 10.02201554968999986, 3.298015135926000152, 5.700522662207000657 ) ) ;
#33097 = CARTESIAN_POINT ( 'NONE',  ( 8.347296311784370815, -3.523203782693021591, 9.195961815643585169 ) ) ;
#33099 = CARTESIAN_POINT ( 'NONE',  ( 11.59456039236534330, 5.314711678001000195, -7.563984187103470092 ) ) ;
#33100 = ORIENTED_EDGE ( 'NONE', *, *, #51566, .T. ) ;
#33101 = CARTESIAN_POINT ( 'NONE',  ( 16.44809435262699893, -3.299700711820999555, -11.83394467541999973 ) ) ;
#33102 = AXIS2_PLACEMENT_3D ( 'NONE', #28921, #43252, #11425 ) ;
#33103 = CARTESIAN_POINT ( 'NONE',  ( 8.232750256034279346, 4.666560802815586051, 6.122829837893929650 ) ) ;
#33104 = EDGE_LOOP ( 'NONE', ( #31269, #29998, #30015, #25360 ) ) ;
#33105 = EDGE_CURVE ( 'NONE', #41119, #5164, #39590, .T. ) ;
#33106 = CARTESIAN_POINT ( 'NONE',  ( 17.55505043854143565, 2.500000000000000000, -25.00000000000000000 ) ) ;
#33107 = CARTESIAN_POINT ( 'NONE',  ( 11.23052404082913291, 2.954319127720149041, 7.824990945864982450 ) ) ;
#33108 = VECTOR ( 'NONE', #53654, 1000.000000000000000 ) ;
#33109 = CARTESIAN_POINT ( 'NONE',  ( 17.74345116425200075, 0.7055305429986109544, -13.98221279804358019 ) ) ;
#33110 = ORIENTED_EDGE ( 'NONE', *, *, #30811, .F. ) ;
#33111 = CARTESIAN_POINT ( 'NONE',  ( 21.47500033997000202, -1.509903313490000218E-14, 4.329869796037999436E-14 ) ) ;
#33112 = CARTESIAN_POINT ( 'NONE',  ( 8.788005865575000186, -3.396241925389000382, -6.276539452210999848 ) ) ;
#33113 = CARTESIAN_POINT ( 'NONE',  ( 10.82035090130999855, 4.758726914843000699, -7.969278253227299658 ) ) ;
#33114 = DIRECTION ( 'NONE',  ( -1.000000000000000000, 0.000000000000000000, 0.000000000000000000 ) ) ;
#33115 = CARTESIAN_POINT ( 'NONE',  ( 11.43656785386840014, -5.060279460151999587, 6.786470850652599474 ) ) ;
#33116 = ORIENTED_EDGE ( 'NONE', *, *, #58492, .T. ) ;
#33117 = FACE_OUTER_BOUND ( 'NONE', #58985, .T. ) ;
#33118 = CARTESIAN_POINT ( 'NONE',  ( 17.99906018690873211, -1.940665501735332032, 13.86484298168863738 ) ) ;
#33119 = CARTESIAN_POINT ( 'NONE',  ( 9.341834235717470847, -4.999591705763744898, -6.731799792051353037 ) ) ;
#33120 = CARTESIAN_POINT ( 'NONE',  ( 15.36900185986900169, -9.263677555280001030, -8.208910455558001473 ) ) ;
#33121 = LINE ( 'NONE', #53409, #49137 ) ;
#33122 = ORIENTED_EDGE ( 'NONE', *, *, #51165, .F. ) ;
#33123 = CARTESIAN_POINT ( 'NONE',  ( 12.43764207941355338, -1.993980486415520614, -12.55516735266245121 ) ) ;
#33124 = CARTESIAN_POINT ( 'NONE',  ( 0.4266613450451046674, -1.726519499994412454, -2.993820366163598923 ) ) ;
#33125 = CARTESIAN_POINT ( 'NONE',  ( 7.292197165043062590, 5.528435618896470949, -6.445051596221718526 ) ) ;
#33126 = DIRECTION ( 'NONE',  ( 0.000000000000000000, 1.000000000000000000, 0.000000000000000000 ) ) ;
#33127 = CARTESIAN_POINT ( 'NONE',  ( 12.08136008893002966, -2.567386246332875377, -13.76259835127842202 ) ) ;
#33128 = B_SPLINE_CURVE_WITH_KNOTS ( 'NONE', 3,
 ( #63125, #30646, #51956, #13884 ),
 .UNSPECIFIED., .F., .F.,
 ( 4, 4 ),
 ( 0.000000000000000000, 1.000000000000000000 ),
 .UNSPECIFIED. ) ;
#33129 = B_SPLINE_CURVE_WITH_KNOTS ( 'NONE', 3,
 ( #41391, #46982, #10597, #57117, #42077, #25997, #9218, #20752, #20405, #15511, #21425, #31939, #63388, #36143, #68631, #68285 ),
 .UNSPECIFIED., .F., .F.,
 ( 4, 2, 2, 2, 2, 2, 2, 4 ),
 ( 0.000000000000000000, 0.1250000000000002498, 0.2500000000000004996, 0.3750000000000007772, 0.5000000000000009992, 0.6250000000000004441, 0.7499999999999998890, 1.000000000000000000 ),
 .UNSPECIFIED. ) ;
#33130 = CARTESIAN_POINT ( 'NONE',  ( 11.35918179236250047, -4.238363971154499588, -6.384440618559000136 ) ) ;
#33131 = DIRECTION ( 'NONE',  ( 1.000000000000000000, 0.000000000000000000, 0.000000000000000000 ) ) ;
#33132 = CARTESIAN_POINT ( 'NONE',  ( 17.59659125555225145, -3.123958135111998491, 12.28406395290800823 ) ) ;
#33133 = ORIENTED_EDGE ( 'NONE', *, *, #35909, .F. ) ;
#33134 = CARTESIAN_POINT ( 'NONE',  ( 11.01790547754519878, -2.825704134258000266, -7.537269019642879542 ) ) ;
#33135 = ORIENTED_EDGE ( 'NONE', *, *, #57177, .T. ) ;
#33136 = CARTESIAN_POINT ( 'NONE',  ( 11.80577368593200305, -12.32791529894999982, -1.878576500660000148 ) ) ;
#33137 = CARTESIAN_POINT ( 'NONE',  ( 9.096889158776001238, 2.235961884443999459, -6.794506518623999902 ) ) ;
#33138 = CARTESIAN_POINT ( 'NONE',  ( 10.27571527605999968, 5.689443924112000062, -7.562019866568999049 ) ) ;
#33139 = CARTESIAN_POINT ( 'NONE',  ( 10.66852499011999988, -4.435470817312999969, -5.866470266317000082 ) ) ;
#33140 = CARTESIAN_POINT ( 'NONE',  ( 0.000000000000000000, 5.100000000000000533, -7.500000000000000000 ) ) ;
#33141 = CARTESIAN_POINT ( 'NONE',  ( 7.572352458090005456, 3.472372354340000911, -6.527657354165006254 ) ) ;
#33142 = EDGE_CURVE ( 'NONE', #33910, #55299, #43343, .T. ) ;
#33144 = EDGE_CURVE ( 'NONE', #10227, #68412, #55849, .T. ) ;
#33143 = CARTESIAN_POINT ( 'NONE',  ( 5.000000000000000000, 0.000000000000000000, 0.000000000000000000 ) ) ;
#33145 = EDGE_LOOP ( 'NONE', ( #67731, #19167, #43626, #31581 ) ) ;
#33146 = CARTESIAN_POINT ( 'NONE',  ( 1.862398069789666710, -2.519008840803133698, -2.453290717214521521 ) ) ;
#33147 = EDGE_CURVE ( 'NONE', #55276, #58820, #60818, .T. ) ;
#33148 = CARTESIAN_POINT ( 'NONE',  ( 10.24961997674000003, 4.184221916050000267, 9.286882020979000174 ) ) ;
#33149 = CARTESIAN_POINT ( 'NONE',  ( 25.29995737991200144, -8.533537546129998930, 7.925519566782000425 ) ) ;
#33150 = CARTESIAN_POINT ( 'NONE',  ( 10.37581074856900187, 2.827416853083249748, -8.000243450341619322 ) ) ;
#33151 = CARTESIAN_POINT ( 'NONE',  ( 17.86871151025999893, 3.252328409732000214, -11.33729656921000029 ) ) ;
#33152 = CARTESIAN_POINT ( 'NONE',  ( 10.35826357027499789, 4.850513154668600002, -7.664090691848299386 ) ) ;
#33153 = AXIS2_PLACEMENT_3D ( 'NONE', #41482, #36933, #62113 ) ;
#33154 = CARTESIAN_POINT ( 'NONE',  ( 23.56665676678100141, 1.475264355121999897E-12, 7.429612480791998923E-13 ) ) ;
#33155 = CARTESIAN_POINT ( 'NONE',  ( 23.51508444987500113, -10.47082793957999947, -9.494578343657000374 ) ) ;
#33156 = CARTESIAN_POINT ( 'NONE',  ( 23.91165634958499808, -9.488820091758000785, 9.248970464519000956 ) ) ;
#33157 = VECTOR ( 'NONE', #33438, 1000.000000000000114 ) ;
#33158 = ORIENTED_EDGE ( 'NONE', *, *, #25281, .T. ) ;
#33159 = CARTESIAN_POINT ( 'NONE',  ( 9.766460841231999979, 3.135494838036999798, -8.598037907310999373 ) ) ;
#33160 = CARTESIAN_POINT ( 'NONE',  ( 7.194116527854999887, 1.351798952403999943, -0.2150535807229000118 ) ) ;
#33161 = CARTESIAN_POINT ( 'NONE',  ( 18.03429950922807734, 2.098690172523155262, 13.75037901049766731 ) ) ;
#33162 = CARTESIAN_POINT ( 'NONE',  ( 24.46729256464000457, 8.826997888453998797, -8.952499471243999807 ) ) ;
#33163 = CARTESIAN_POINT ( 'NONE',  ( 10.22687885159599830, -2.867290578374000365, -7.364871923548499844 ) ) ;
#33164 = VERTEX_POINT ( 'NONE', #23159 ) ;
#33165 = AXIS2_PLACEMENT_3D ( 'NONE', #7894, #22928, #65578 ) ;
#33166 = CARTESIAN_POINT ( 'NONE',  ( 10.67956456102511886, -4.176706786694480478, -8.849774126559321274 ) ) ;
#33167 = CARTESIAN_POINT ( 'NONE',  ( 8.245295280410999794, 4.283000592898000392, 9.286795422009001655 ) ) ;
#33169 = CARTESIAN_POINT ( 'NONE',  ( 21.10000109091659937, 0.000000000000000000, 0.000000000000000000 ) ) ;
#33168 = CARTESIAN_POINT ( 'NONE',  ( 9.410004719593999312, 2.495531372253999791, -7.930944806125000746 ) ) ;
#33170 = CARTESIAN_POINT ( 'NONE',  ( 2.215865467774827735, 2.262839795465755977, -2.144213487925047623 ) ) ;
#33171 = ORIENTED_EDGE ( 'NONE', *, *, #8880, .F. ) ;
#33172 = CARTESIAN_POINT ( 'NONE',  ( 9.854942824136999846, 2.800308224477999985, 9.013816726157999781 ) ) ;
#33173 = CARTESIAN_POINT ( 'NONE',  ( 17.80546914520764545, -3.072731260628055683, -13.53510445278181962 ) ) ;
#33174 = CARTESIAN_POINT ( 'NONE',  ( 10.72333863405319931, 4.619094858989799768, 6.710270673950399889 ) ) ;
#33175 = CARTESIAN_POINT ( 'NONE',  ( 9.757667269575000191, -4.489271889653999814, 5.986031004145000445 ) ) ;
#33176 = CARTESIAN_POINT ( 'NONE',  ( 7.885003087483005046, 2.917683036408002195, 6.444041402419006914 ) ) ;
#33177 = ORIENTED_EDGE ( 'NONE', *, *, #6375, .T. ) ;
#33178 = CARTESIAN_POINT ( 'NONE',  ( 24.46580263708699832, 12.16839033447999974, -3.168637030101999930 ) ) ;
#33180 = CARTESIAN_POINT ( 'NONE',  ( 10.73615685320999980, -3.078046833211999900, -6.088743704655001032 ) ) ;
#33179 = CARTESIAN_POINT ( 'NONE',  ( 12.13642952379600004, -11.66478987891999886, 3.865847705614000152 ) ) ;
#33181 = CARTESIAN_POINT ( 'NONE',  ( 7.738470611522092923, -5.540180350881191096, 8.309424268451294893 ) ) ;
#33182 = CARTESIAN_POINT ( 'NONE',  ( 9.347248564704999652, -4.028326926800000152, 9.469437404464001062 ) ) ;
#33183 = CARTESIAN_POINT ( 'NONE',  ( 10.98768472639999949, 5.139099012905000485, 4.945212061661000469 ) ) ;
#33184 = ORIENTED_EDGE ( 'NONE', *, *, #17947, .T. ) ;
#33185 = CARTESIAN_POINT ( 'NONE',  ( 24.05220196936242161, -9.284530115100020353, 9.220592073794886545 ) ) ;
#33186 = CARTESIAN_POINT ( 'NONE',  ( 11.66225954179439839, -3.122605388210700106, 6.770980925167799036 ) ) ;
#33187 = EDGE_CURVE ( 'NONE', #42061, #67307, #9444, .T. ) ;
#33188 = CARTESIAN_POINT ( 'NONE',  ( 17.55505043854143565, 1.787797342887044394, 13.88538010501570952 ) ) ;
#33189 = CARTESIAN_POINT ( 'NONE',  ( 10.61656919669529842, 5.225637333137999718, 7.137881914002699446 ) ) ;
#33190 = ORIENTED_EDGE ( 'NONE', *, *, #62895, .F. ) ;
#33191 = CARTESIAN_POINT ( 'NONE',  ( 8.225464158772000545, 3.844886277615000125, -8.888911790991000927 ) ) ;
#33192 = EDGE_CURVE ( 'NONE', #48333, #66718, #3855, .T. ) ;
#33193 = CARTESIAN_POINT ( 'NONE',  ( 24.38583233132600014, 12.22835294837999953, -3.200653174729999773 ) ) ;
#33194 = CARTESIAN_POINT ( 'NONE',  ( 12.51946955736927691, 3.141640009352831608, -12.20205326030422377 ) ) ;
#33195 = CARTESIAN_POINT ( 'NONE',  ( 11.97500581613029880, -3.011381429075500105, 6.865182626353099948 ) ) ;
#33196 = ORIENTED_EDGE ( 'NONE', *, *, #39934, .F. ) ;
#33197 = CARTESIAN_POINT ( 'NONE',  ( 23.57777265339244721, 2.928868628335262514, 13.64745830326427800 ) ) ;
#33198 = CIRCLE ( 'NONE', #19771, 5.760713961201000544 ) ;
#33199 = CARTESIAN_POINT ( 'NONE',  ( 10.49809687351654297, 3.672815144550898303, -8.717465845835393523 ) ) ;
#33200 = ORIENTED_EDGE ( 'NONE', *, *, #51955, .T. ) ;
#33201 = FACE_OUTER_BOUND ( 'NONE', #51888, .T. ) ;
#33202 = DIRECTION ( 'NONE',  ( 0.7071067811865475727, 0.7071067811865475727, 0.000000000000000000 ) ) ;
#33203 = ORIENTED_EDGE ( 'NONE', *, *, #56274, .F. ) ;
#33204 = CARTESIAN_POINT ( 'NONE',  ( 12.78084604758903886, -3.199697762315045768, -12.18695750762853258 ) ) ;
#33205 = CARTESIAN_POINT ( 'NONE',  ( 10.50595525820100029, 3.918212119278319694, 8.362327856951900173 ) ) ;
#33206 =( GEOMETRIC_REPRESENTATION_CONTEXT ( 3 ) GLOBAL_UNCERTAINTY_ASSIGNED_CONTEXT ( ( #7108 ) ) GLOBAL_UNIT_ASSIGNED_CONTEXT ( ( #28402, #34345, #2514 ) ) REPRESENTATION_CONTEXT ( 'NONE', 'WORKASPACE' ) );
#33207 = CARTESIAN_POINT ( 'NONE',  ( 10.75915805961999894, -5.387268372866000021, -6.278119777966000292 ) ) ;
#33208 = CARTESIAN_POINT ( 'NONE',  ( 10.59393020684899867, 5.250000000000000000, 7.500000000000000000 ) ) ;
#33209 = CARTESIAN_POINT ( 'NONE',  ( 18.33872945691700096, -11.68442479034000137, 4.616443127689999315 ) ) ;
#33210 = CARTESIAN_POINT ( 'NONE',  ( 10.85738557828999973, -2.754556666341999804, 8.976367391363998749 ) ) ;
#33211 = CARTESIAN_POINT ( 'NONE',  ( 13.60261247405900242, 9.239907047945001395, 8.094831983377998696 ) ) ;
#33212 = CARTESIAN_POINT ( 'NONE',  ( 17.88568294903051736, -0.5304820368560130284, -12.68508456201359991 ) ) ;
#33213 = CARTESIAN_POINT ( 'NONE',  ( 12.20163823172845596, 2.663908709213365533, -12.41191052582379939 ) ) ;
#33214 = CARTESIAN_POINT ( 'NONE',  ( 11.52733460557258915, -3.793662715184400014, -8.761245990815998752 ) ) ;
#33215 = CARTESIAN_POINT ( 'NONE',  ( 8.122954719591000128, 3.566637212418000136, 5.743604853744000316 ) ) ;
#33216 = ORIENTED_EDGE ( 'NONE', *, *, #36802, .F. ) ;
#33217 = VECTOR ( 'NONE', #52265, 1000.000000000000114 ) ;
#33218 = CARTESIAN_POINT ( 'NONE',  ( 11.79999999684100054, 12.15995044155999949, 2.000340912084999978 ) ) ;
#33219 = CYLINDRICAL_SURFACE ( 'NONE', #58416, 1.350000000000000533 ) ;
#33220 = CARTESIAN_POINT ( 'NONE',  ( 11.56599877858000092, 12.45298756855999933, 1.663864064400000009 ) ) ;
#33221 = CARTESIAN_POINT ( 'NONE',  ( 18.17187109576073567, 2.859211385468999556, 12.27132042014887148 ) ) ;
#33222 = CARTESIAN_POINT ( 'NONE',  ( 4.599999999999999645, -3.199698446519375850, -12.18695736643652694 ) ) ;
#33224 = EDGE_CURVE ( 'NONE', #55934, #50471, #49041, .T. ) ;
#33223 = CARTESIAN_POINT ( 'NONE',  ( 9.318724127987000116, 2.755029797911999978, 8.795125756257000660 ) ) ;
#33225 = CIRCLE ( 'NONE', #12004, 1.250000000000000000 ) ;
#33226 = CARTESIAN_POINT ( 'NONE',  ( 9.878875014952626543, -3.131883468830893857, 7.609114422657746069 ) ) ;
#33227 = EDGE_CURVE ( 'NONE', #958, #16538, #19192, .T. ) ;
#33228 = CARTESIAN_POINT ( 'NONE',  ( 8.762289945692000259, 3.761977284103799946, 6.588711079851200303 ) ) ;
#33229 = EDGE_CURVE ( 'NONE', #66034, #1019, #9153, .T. ) ;
#33230 = EDGE_LOOP ( 'NONE', ( #15576, #17565, #12126, #63810, #45156 ) ) ;
#33231 = CARTESIAN_POINT ( 'NONE',  ( 12.50301483199535468, -3.134404823497601633, 12.20391382861247109 ) ) ;
#33232 = CARTESIAN_POINT ( 'NONE',  ( 8.998468108405997867, -2.901397043998999781, -7.811136554427399403 ) ) ;
#33233 = CARTESIAN_POINT ( 'NONE',  ( 24.26733149983100191, -3.229785797570000394, -12.20153234936999986 ) ) ;
#33234 = CARTESIAN_POINT ( 'NONE',  ( 10.50286331871000023, -5.158900740613000302, 8.369962360110999811 ) ) ;
#33235 = CARTESIAN_POINT ( 'NONE',  ( 10.42795525820099911, 3.905250696375530239, -6.501013802764199490 ) ) ;
#33236 = CARTESIAN_POINT ( 'NONE',  ( 12.70960625021945312, -0.7131288892044757022, 12.57980326738671906 ) ) ;
#33237 = CARTESIAN_POINT ( 'NONE',  ( 8.598670280411999656, 2.376526778640999815, 7.686980884243000745 ) ) ;
#33238 = CARTESIAN_POINT ( 'NONE',  ( 10.21609109105999913, 5.961715741921000067, 7.319666990313999477 ) ) ;
#33239 = CARTESIAN_POINT ( 'NONE',  ( 12.64197434038399237, 3.103437838334064391, 12.29027179270079806 ) ) ;
#33240 = ORIENTED_EDGE ( 'NONE', *, *, #30235, .T. ) ;
#33241 = CARTESIAN_POINT ( 'NONE',  ( 7.919010841228001141, 5.361039412362000434, 6.973453640356000349 ) ) ;
#33242 = CARTESIAN_POINT ( 'NONE',  ( 10.57149279008999798, 3.703313553258400059, -8.601484120896000007 ) ) ;
#33243 = CARTESIAN_POINT ( 'NONE',  ( 18.18297319953441971, -0.3597466176220683876, 12.59486741915706709 ) ) ;
#33244 = TOROIDAL_SURFACE ( 'NONE', #8687, 6.000000000000000000, 1.000000000000000000 ) ;
#33245 = ADVANCED_FACE ( 'NONE', ( #36060, #50774 ), #66843, .F. ) ;
#33246 = CYLINDRICAL_SURFACE ( 'NONE', #31562, 5.000000000000000000 ) ;
#33248 = CARTESIAN_POINT ( 'NONE',  ( 24.89163422318532426, 11.59758331541865672, 3.206058750856457529 ) ) ;
#33247 = CARTESIAN_POINT ( 'NONE',  ( 24.59999999957999961, -2.749830041232999947E-09, 4.999999999859999988 ) ) ;
#33249 = CARTESIAN_POINT ( 'NONE',  ( 11.85159063708299954, -3.174974693948799942, -7.731961446576300467 ) ) ;
#33250 = CARTESIAN_POINT ( 'NONE',  ( 11.00000000000000000, 5.079754677601000523, 7.174999999999999822 ) ) ;
#33251 = ORIENTED_EDGE ( 'NONE', *, *, #9291, .T. ) ;
#33252 = AXIS2_PLACEMENT_3D ( 'NONE', #61292, #39277, #34731 ) ;
#33253 = CARTESIAN_POINT ( 'NONE',  ( 1.496201594832999859, -1.181558911493999942, 3.215390670984000554 ) ) ;
#33254 = CARTESIAN_POINT ( 'NONE',  ( 23.76527261957394188, -9.791761873676088967, -9.440867193121368572 ) ) ;
#33255 = STYLED_ITEM ( 'NONE', ( #55923 ), #42763 ) ;
#33256 = VECTOR ( 'NONE', #28452, 1000.000000000000000 ) ;
#33257 = CARTESIAN_POINT ( 'NONE',  ( 12.08335418496243463, -11.66230666314274345, 4.568774126648690093 ) ) ;
#33258 = CARTESIAN_POINT ( 'NONE',  ( 24.53429015151300163, -3.614318902553999902, -12.31267542782000035 ) ) ;
#33260 = CARTESIAN_POINT ( 'NONE',  ( 12.63821499911166413, -1.807008444693748439, 13.88289391573714049 ) ) ;
#33259 = AXIS2_PLACEMENT_3D ( 'NONE', #52505, #4604, #25939 ) ;
#33261 = CARTESIAN_POINT ( 'NONE',  ( 7.947784805528978147, 5.286778829772822874, 7.027374276529180896 ) ) ;
#33262 = CARTESIAN_POINT ( 'NONE',  ( 8.702564146836854420, -2.714984396920495868, 7.027277620402951896 ) ) ;
#33263 = CARTESIAN_POINT ( 'NONE',  ( 13.18628609634500215, -12.21854424350999935, -1.979874043355999813 ) ) ;
#33264 = ORIENTED_EDGE ( 'NONE', *, *, #59035, .F. ) ;
#33265 = CARTESIAN_POINT ( 'NONE',  ( 5.500000000000000000, -6.661338147750999827E-14, 12.79999953825637427 ) ) ;
#33266 = CARTESIAN_POINT ( 'NONE',  ( 8.610875063856999745, 4.757997781751000410, 5.934102420827000124 ) ) ;
#33267 = AXIS2_PLACEMENT_3D ( 'NONE', #25955, #52179, #47287 ) ;
#33268 = DIRECTION ( 'NONE',  ( 1.000000000000000000, 0.000000000000000000, 0.000000000000000000 ) ) ;
#33269 = CARTESIAN_POINT ( 'NONE',  ( 10.90000000000000036, -2.899999999999999911, -6.571291218949999902 ) ) ;
#33270 = CARTESIAN_POINT ( 'NONE',  ( 2.000973465872999846, 3.500000000000000000, 0.000000000000000000 ) ) ;
#33271 = DIRECTION ( 'NONE',  ( -0.000000000000000000, 0.06400262754466103099, 0.9979497300302152540 ) ) ;
#33272 = CARTESIAN_POINT ( 'NONE',  ( 9.852250488097013204, -5.092274670905198697, 8.129544561320937390 ) ) ;
#33273 = CARTESIAN_POINT ( 'NONE',  ( 11.21979841651039855, 3.695024856201900132, 6.689266534545799558 ) ) ;
#33274 = AXIS2_PLACEMENT_3D ( 'NONE', #61900, #45823, #67819 ) ;
#33275 = CARTESIAN_POINT ( 'NONE',  ( 11.49999035076000276, -3.886252136122000156, 11.90689009355000039 ) ) ;
#33276 = CARTESIAN_POINT ( 'NONE',  ( 11.20536814679000059, -2.688541832249000230, -8.273932507170000505 ) ) ;
#33277 = EDGE_CURVE ( 'NONE', #40612, #58532, #61262, .T. ) ;
#33278 = CARTESIAN_POINT ( 'NONE',  ( 11.27531844363630320, 4.339035105373933554, -8.308695084076104465 ) ) ;
#33279 = CARTESIAN_POINT ( 'NONE',  ( 10.98768472639999949, -0.3876847264043000174, -4.945212061661000469 ) ) ;
#33280 = CARTESIAN_POINT ( 'NONE',  ( 9.214598350275000627, -4.599999999999999645, -6.571291218958999814 ) ) ;
#33281 = ORIENTED_EDGE ( 'NONE', *, *, #57711, .F. ) ;
#33282 = CARTESIAN_POINT ( 'NONE',  ( 7.489726418404281993, 2.461536839440352065, 6.668271594188382778 ) ) ;
#33283 = VERTEX_POINT ( 'NONE', #61945 ) ;
#33284 = CARTESIAN_POINT ( 'NONE',  ( 18.14722095428672333, -2.700912180127440276, 13.62881044890620608 ) ) ;
#33285 = CARTESIAN_POINT ( 'NONE',  ( 10.96118313518939935, -4.792748567750200195, -8.502430091786999711 ) ) ;
#33287 = VERTEX_POINT ( 'NONE', #2868 ) ;
#33286 = B_SPLINE_CURVE_WITH_KNOTS ( 'NONE', 3,
 ( #36868, #20093, #58184, #35832 ),
 .UNSPECIFIED., .F., .F.,
 ( 4, 4 ),
 ( 0.000000000000000000, 1.000000000000000000 ),
 .UNSPECIFIED. ) ;
#33288 = CARTESIAN_POINT ( 'NONE',  ( 11.06456920625009843, 4.037149028919880145, 8.532838639935999225 ) ) ;
#33289 = CARTESIAN_POINT ( 'NONE',  ( 9.643930206848999376, -2.750000000000000000, -7.500000000000000000 ) ) ;
#33290 = CARTESIAN_POINT ( 'NONE',  ( 10.35685100253999913, -2.832432432432000269, -6.822293592207000934 ) ) ;
#33291 = CARTESIAN_POINT ( 'NONE',  ( 10.52638970730999901, 2.451081172664000274, 6.282749363171999946 ) ) ;
#33292 = CARTESIAN_POINT ( 'NONE',  ( 8.599999952505998024, 4.000000000000000000, -7.500000000000000000 ) ) ;
#33293 = LINE ( 'NONE', #36219, #67393 ) ;
#33294 = FACE_BOUND ( 'NONE', #1216, .T. ) ;
#33295 = CARTESIAN_POINT ( 'NONE',  ( 9.922182479546000522, -3.489927462211000364, -9.111803974470001677 ) ) ;
#33296 = CARTESIAN_POINT ( 'NONE',  ( 10.00991387826809920, -4.592587181568636545, -8.996716702657641562 ) ) ;
#33297 = ORIENTED_EDGE ( 'NONE', *, *, #63905, .F. ) ;
#33298 = PRESENTATION_STYLE_ASSIGNMENT (( #54961 ) ) ;
#33299 = VERTEX_POINT ( 'NONE', #24196 ) ;
#33300 = CARTESIAN_POINT ( 'NONE',  ( 8.883506238772763908, 4.136150106583480479, -6.466493704552775945 ) ) ;
#33301 = ORIENTED_EDGE ( 'NONE', *, *, #39936, .T. ) ;
#33302 = CARTESIAN_POINT ( 'NONE',  ( 18.00364620838984919, -1.936356668767989397, -13.86561588859484395 ) ) ;
#33303 = CARTESIAN_POINT ( 'NONE',  ( 11.08518686003000120, -5.334253229556999543, 4.956526821568000507 ) ) ;
#33304 = CARTESIAN_POINT ( 'NONE',  ( 10.31021345716899873, 4.636538040886300394, 6.921280946186199934 ) ) ;
#33305 = CARTESIAN_POINT ( 'NONE',  ( 10.21627973160999936, 4.114789684104299461, -6.225948307210999566 ) ) ;
#33306 = CARTESIAN_POINT ( 'NONE',  ( 12.24262961005303296, 2.226644062380152445, 13.72761226533214440 ) ) ;
#33307 = CARTESIAN_POINT ( 'NONE',  ( 10.62792628238999981, -3.100579357212000176, 8.599905962393000536 ) ) ;
#33308 = CIRCLE ( 'NONE', #36648, 11.79499999999999993 ) ;
#33309 = CARTESIAN_POINT ( 'NONE',  ( 23.60205915885299888, -9.223492163368996799, -8.025915643339997629 ) ) ;
#33310 = EDGE_CURVE ( 'NONE', #873, #38701, #44225, .T. ) ;
#33311 = CARTESIAN_POINT ( 'NONE',  ( 11.64975833414749928, -4.796537143354000499, 7.174999999999999822 ) ) ;
#33312 = EDGE_CURVE ( 'NONE', #56519, #41499, #67522, .T. ) ;
#33313 = ORIENTED_EDGE ( 'NONE', *, *, #60477, .F. ) ;
#33314 = CARTESIAN_POINT ( 'NONE',  ( 6.976090560819000252, 5.172411450403999744, -8.246583185469999577 ) ) ;
#33315 = CARTESIAN_POINT ( 'NONE',  ( 9.342711596876126734, 5.100000000000000533, -6.305985889523087806 ) ) ;
#33316 = DIRECTION ( 'NONE',  ( 0.000000000000000000, -1.000000000000000000, 0.000000000000000000 ) ) ;
#33317 = AXIS2_PLACEMENT_3D ( 'NONE', #40595, #50060, #33983 ) ;
#33318 = CARTESIAN_POINT ( 'NONE',  ( 4.877003487648000402, 1.187560281918999872, -0.8868741825288999348 ) ) ;
#33319 = CARTESIAN_POINT ( 'NONE',  ( 9.626145280412998773, 3.934138271021000222, -9.063586117809000697 ) ) ;
#33320 = CARTESIAN_POINT ( 'NONE',  ( 9.864763540183249191, 2.782534154164605589, -7.827184855449096368 ) ) ;
#33321 = CARTESIAN_POINT ( 'NONE',  ( 10.70780617489000086, -5.157482071823000780, -6.267811103859000532 ) ) ;
#33322 = AXIS2_PLACEMENT_3D ( 'NONE', #94, #16514, #37842 ) ;
#33323 = CARTESIAN_POINT ( 'NONE',  ( 6.976556957425999350, -9.209923018478999523, -5.193750594735999648 ) ) ;
#33324 = DIRECTION ( 'NONE',  ( 0.000000000000000000, 1.000000000000000000, 0.000000000000000000 ) ) ;
#33325 = CARTESIAN_POINT ( 'NONE',  ( 4.555026506349999948, -1.500000000000000000, 0.000000000000000000 ) ) ;
#33326 = CARTESIAN_POINT ( 'NONE',  ( 8.617943828495366887, -2.919020491875332635, -6.688170526709825481 ) ) ;
#33327 = CARTESIAN_POINT ( 'NONE',  ( 8.642077642326000841, -2.899999999999999911, 6.463854830420999953 ) ) ;
#33328 = CARTESIAN_POINT ( 'NONE',  ( 1.053056799209125094, 2.798833948393625537, 2.150913519912209360 ) ) ;
#33329 = CARTESIAN_POINT ( 'NONE',  ( 10.81013259637009938, 2.968328969579000276, -8.062151801142800167 ) ) ;
#33330 = EDGE_CURVE ( 'NONE', #49843, #18862, #34703, .T. ) ;
#33331 = CARTESIAN_POINT ( 'NONE',  ( 8.798797255587999189, 5.003512473869000665, -7.457514444071209780 ) ) ;
#33333 = CARTESIAN_POINT ( 'NONE',  ( 10.33240787032999997, -3.158183717747000241, 4.868352313451000057 ) ) ;
#33332 = CARTESIAN_POINT ( 'NONE',  ( 10.82844474310100047, -3.228742141949900279, 7.125715588371799747 ) ) ;
#33334 = CARTESIAN_POINT ( 'NONE',  ( 11.31059687351629961, -4.629523725463621453, 8.592232985442823434 ) ) ;
#33335 = ORIENTED_EDGE ( 'NONE', *, *, #62725, .F. ) ;
#33336 = B_SPLINE_CURVE_WITH_KNOTS ( 'NONE', 3,
 ( #66903, #34075, #56423, #8184 ),
 .UNSPECIFIED., .F., .F.,
 ( 4, 4 ),
 ( 0.000000000000000000, 1.000000000000000000 ),
 .UNSPECIFIED. ) ;
#33337 = ADVANCED_FACE ( 'NONE', ( #46216 ), #13378, .T. ) ;
#33338 = CARTESIAN_POINT ( 'NONE',  ( 10.52435971519499880, 4.532462039660099862, 8.385788382729799650 ) ) ;
#33339 = CARTESIAN_POINT ( 'NONE',  ( 11.20904026220999938, -5.937811873294999820, 7.147336919140999001 ) ) ;
#33340 = CARTESIAN_POINT ( 'NONE',  ( 9.783671671056998420, 2.873958896683999953, 7.310881302803900361 ) ) ;
#33341 = CARTESIAN_POINT ( 'NONE',  ( 9.758812222687625493, 4.162730299909893183, -8.359680823568968577 ) ) ;
#33342 = CARTESIAN_POINT ( 'NONE',  ( 10.13050497920000126, -3.092053006542000215, 8.629388195475000245 ) ) ;
#33343 = LINE ( 'NONE', #59554, #41948 ) ;
#33344 = CARTESIAN_POINT ( 'NONE',  ( 11.80852891948700290, 3.296364302329999774, -11.83491796280999964 ) ) ;
#33345 = VERTEX_POINT ( 'NONE', #8808 ) ;
#33346 = CARTESIAN_POINT ( 'NONE',  ( 9.634659112603999986, -4.436443689698799986, -8.404632083253700259 ) ) ;
#33347 = DIRECTION ( 'NONE',  ( 1.000000000000000000, 0.000000000000000000, 0.000000000000000000 ) ) ;
#33348 = CARTESIAN_POINT ( 'NONE',  ( 6.641058386525000579, -1.256780975885000151, 0.6254553495446000255 ) ) ;
#33349 = CARTESIAN_POINT ( 'NONE',  ( 10.56927318630899926, -3.243547362524661359, 6.473854711408034923 ) ) ;
#33350 = AXIS2_PLACEMENT_3D ( 'NONE', #56701, #8801, #30141 ) ;
#33351 = CARTESIAN_POINT ( 'NONE',  ( 24.60999195316300003, -3.467950226999999774, 12.10892777233999951 ) ) ;
#33352 = CARTESIAN_POINT ( 'NONE',  ( 12.06441235500451015, -4.638700978900200056, 8.085115074060599483 ) ) ;
#33353 = CARTESIAN_POINT ( 'NONE',  ( 10.75210807141120029, 4.040019166404060336, -8.365272822098500427 ) ) ;
#33354 = CARTESIAN_POINT ( 'NONE',  ( 15.40000000009400161, 8.833277835210999740, 7.896561221812000930 ) ) ;
#33356 = CARTESIAN_POINT ( 'NONE',  ( 5.449999267937000624, 6.217248937900999058E-14, -13.04999927352996281 ) ) ;
#33355 = AXIS2_PLACEMENT_3D ( 'NONE', #67701, #57218, #20509 ) ;
#33357 = CARTESIAN_POINT ( 'NONE',  ( 12.08078742596348576, 2.670354628897900540, 12.31525682382392084 ) ) ;
#33358 = ORIENTED_EDGE ( 'NONE', *, *, #63903, .F. ) ;
#33359 = CARTESIAN_POINT ( 'NONE',  ( 7.590045049562995416, -4.176984001086847087, 8.849581831964579592 ) ) ;
#33360 = CARTESIAN_POINT ( 'NONE',  ( 12.13047358906990958, -0.2678304234474128687, -13.99744223245316199 ) ) ;
#33361 = CARTESIAN_POINT ( 'NONE',  ( 13.99965637475000158, -8.819038952442999957, -7.693330608063000398 ) ) ;
#33362 = DIRECTION ( 'NONE',  ( 1.000000000000000000, 0.000000000000000000, 0.000000000000000000 ) ) ;
#33363 = FACE_OUTER_BOUND ( 'NONE', #69183, .T. ) ;
#33364 = CARTESIAN_POINT ( 'NONE',  ( 7.000000000000002665, 8.394866283432396159, 4.394866297543325473 ) ) ;
#33365 = CARTESIAN_POINT ( 'NONE',  ( 5.657901059019435408, 12.07783836333738847, -3.734765664958211051 ) ) ;
#33366 = ORIENTED_EDGE ( 'NONE', *, *, #63903, .T. ) ;
#33367 = SURFACE_STYLE_USAGE ( .BOTH. , #65507 ) ;
#33368 = CARTESIAN_POINT ( 'NONE',  ( 17.57587346436483600, 1.875000586273749992, -13.78631940097169739 ) ) ;
#33369 = ORIENTED_EDGE ( 'NONE', *, *, #33081, .F. ) ;
#33370 = CARTESIAN_POINT ( 'NONE',  ( 5.099999999740999712, 0.000000000000000000, 0.000000000000000000 ) ) ;
#33371 = CARTESIAN_POINT ( 'NONE',  ( 24.81044895848265952, 8.607468258889918289, -8.518276782355464150 ) ) ;
#33372 = CARTESIAN_POINT ( 'NONE',  ( 8.175739158770999992, 4.686731264770999772, -8.717075579553000608 ) ) ;
#33373 = CYLINDRICAL_SURFACE ( 'NONE', #11883, 0.5000000000000002220 ) ;
#33374 = CARTESIAN_POINT ( 'NONE',  ( 11.46989666366029859, -4.058428102321880004, -8.814970315645998866 ) ) ;
#33375 = CARTESIAN_POINT ( 'NONE',  ( 7.016960841228000234, 3.332350081667999842, -9.278694849147001378 ) ) ;
#33376 = CARTESIAN_POINT ( 'NONE',  ( 15.95370777310256294, -3.574818104395616647, -11.79277689209176749 ) ) ;
#33377 = FACE_OUTER_BOUND ( 'NONE', #20972, .T. ) ;
#33378 = EDGE_LOOP ( 'NONE', ( #60851, #18492, #43770, #38743 ) ) ;
#33379 = CARTESIAN_POINT ( 'NONE',  ( 10.59999999999999964, 3.399999999999999911, -4.756097560976000338 ) ) ;
#33380 = CARTESIAN_POINT ( 'NONE',  ( 18.17920330502697013, -2.539026862082569558, -13.66507545610718921 ) ) ;
#33381 = CARTESIAN_POINT ( 'NONE',  ( 11.23627509987185746, 3.727547057523675988, -6.249999999999998224 ) ) ;
#33382 = ORIENTED_EDGE ( 'NONE', *, *, #868, .T. ) ;
#33383 = AXIS2_PLACEMENT_3D ( 'NONE', #58317, #68109, #14646 ) ;
#33384 = CARTESIAN_POINT ( 'NONE',  ( 6.065443173016666911, -1.500000000000000222, -0.1963495408493622363 ) ) ;
#33385 = CARTESIAN_POINT ( 'NONE',  ( 10.80374194038000013, -2.766944173105999827, -8.073385940268000383 ) ) ;
#33386 = EDGE_LOOP ( 'NONE', ( #68273, #47863, #66668 ) ) ;
#33387 = CARTESIAN_POINT ( 'NONE',  ( 8.849455549952999434, 4.781695603001899997, 8.130709350565298976 ) ) ;
#33388 = CARTESIAN_POINT ( 'NONE',  ( 18.18389880332057018, -2.839229093938480997, -12.27596119698807975 ) ) ;
#33389 = CARTESIAN_POINT ( 'NONE',  ( 8.138783675073003820, 5.105454305967005446, -6.386197971998996969 ) ) ;
#33390 = CARTESIAN_POINT ( 'NONE',  ( 4.500000000000000000, 0.000000000000000000, 0.000000000000000000 ) ) ;
#33391 = CARTESIAN_POINT ( 'NONE',  ( 30.60000000000000142, 0.000000000000000000, -8.250000000000000000 ) ) ;
#33392 = CARTESIAN_POINT ( 'NONE',  ( 9.332721904869998752, 4.756019688173900306, 7.075568408810499754 ) ) ;
#33393 = EDGE_CURVE ( 'NONE', #31379, #14147, #10021, .T. ) ;
#33394 = FACE_OUTER_BOUND ( 'NONE', #68179, .T. ) ;
#33395 = EDGE_CURVE ( 'NONE', #38268, #35889, #29242, .T. ) ;
#33396 = ORIENTED_EDGE ( 'NONE', *, *, #30476, .F. ) ;
#33397 = DIRECTION ( 'NONE',  ( -1.000000000000000000, 0.000000000000000000, 0.000000000000000000 ) ) ;
#33398 = CARTESIAN_POINT ( 'NONE',  ( 10.84974221959000218, 5.265003089217000998, -6.385808769407000263 ) ) ;
#33399 = CARTESIAN_POINT ( 'NONE',  ( 25.29986325275000070, 2.078227429405999693, 11.31065739696999906 ) ) ;
#33400 = CARTESIAN_POINT ( 'NONE',  ( 12.18013031904082233, 2.522561724994068388, -13.66866813226131327 ) ) ;
#33401 = CARTESIAN_POINT ( 'NONE',  ( 9.937659112603999034, -4.555852086785099786, -8.652134039551000910 ) ) ;
#33402 = CARTESIAN_POINT ( 'NONE',  ( 9.380781717619999682, -2.204246399534000034, 7.545378188773000261 ) ) ;
#33403 = CARTESIAN_POINT ( 'NONE',  ( 17.69685691690359164, 0.6090406077983143707, 13.88203505342131550 ) ) ;
#33404 = CARTESIAN_POINT ( 'NONE',  ( 8.599999952505998024, 4.000000000000000000, 7.500000000000000000 ) ) ;
#33405 = ORIENTED_EDGE ( 'NONE', *, *, #21482, .F. ) ;
#33406 = ORIENTED_EDGE ( 'NONE', *, *, #48052, .T. ) ;
#33407 = VECTOR ( 'NONE', #49928, 1000.000000000000000 ) ;
#33408 = CARTESIAN_POINT ( 'NONE',  ( 10.03280471959000231, 3.987760651117999711, -9.123263301387000368 ) ) ;
#33409 = CARTESIAN_POINT ( 'NONE',  ( 12.38151006044884639, -0.4597209098220048640, 13.88976952607801074 ) ) ;
#33410 = CARTESIAN_POINT ( 'NONE',  ( 10.79657053952199952, -4.502253688815499366, 8.675184076076000395 ) ) ;
#33411 = CARTESIAN_POINT ( 'NONE',  ( 7.329854050017977407, -3.645852630943380746, 6.184363563554137855 ) ) ;
#33412 = DIRECTION ( 'NONE',  ( 0.000000000000000000, 0.000000000000000000, -1.000000000000000000 ) ) ;
#33413 = CARTESIAN_POINT ( 'NONE',  ( 7.058516392956000196, -4.314043295739000250, 8.819145559946001356 ) ) ;
#33414 = FACE_OUTER_BOUND ( 'NONE', #54045, .T. ) ;
#33416 = CARTESIAN_POINT ( 'NONE',  ( 11.07242469412000041, -6.088279333841999374, 5.193826216086000258 ) ) ;
#33415 = CARTESIAN_POINT ( 'NONE',  ( 10.05772190487000017, -2.884547197234000215, 6.873781641694999500 ) ) ;
#33417 = CARTESIAN_POINT ( 'NONE',  ( 10.98579841651039857, 3.550031058388499972, -8.696179055230999211 ) ) ;
#33418 = EDGE_CURVE ( 'NONE', #68619, #46698, #18333, .T. ) ;
#33419 = CARTESIAN_POINT ( 'NONE',  ( -15.86200481174999943, -2.399999999999999911, 6.571291218949999902 ) ) ;
#33420 = DIRECTION ( 'NONE',  ( 0.000000000000000000, 0.9999808993455937545, 0.006180691221632959691 ) ) ;
#33421 = CARTESIAN_POINT ( 'NONE',  ( 18.17602447836047475, -0.07155418421575514276, 12.69973420405192144 ) ) ;
#33422 = B_SPLINE_SURFACE_WITH_KNOTS ( 'NONE', 3, 3, ( 
 ( #8053, #34636, #66776, #45119, #39876, #39176, #30083, #19221, #67112, #29742, #55260, #34286, #39523, #60847, #12962, #55608, #40547, #44780, #28699, #13649, #2123, #12608, #51385, #51045, #7709, #23442, #34977, #13992, #24818, #60499, #35317, #56294, #18892, #8738, #2459 ),
 ( #2801, #3482, #33939, #29395, #8397, #66079, #3146, #24477, #40217, #23783, #66426, #61193, #13314, #50704, #61875, #42530, #5468, #69095, #31357, #42874, #31699, #16640, #32049, #26107, #59287, #67450, #54046, #21883, #15953, #53365, #53021, #11392, #19575, #63496, #64522 ),
 ( #37283, #11059, #64182, #32731, #37967, #48118, #6144, #46144, #5117, #26453, #48464, #40895, #62216, #10704, #58603, #58260, #58952, #26805, #10364, #68741, #27144, #15273, #47786, #222, #47432, #53708, #20858, #43216, #21539, #16296, #37619, #63839, #32393, #5801, #572 ),
 ( #36597, #57923, #10019, #52671, #4765, #42196, #15616, #36946, #21199, #28886, #33078, #22920, #22573, #38312, #59640, #2295, #43916, #65912, #1258, #59983, #11736, #54392, #65220, #6495, #55438, #28531, #33426, #17335, #49844, #12095, #66260, #49492, #18381, #38664, #7531 ) ),
 .UNSPECIFIED., .F., .F., .F.,
 ( 4, 4 ),
 ( 4, 1, 1, 1, 1, 1, 1, 1, 1, 1, 1, 1, 1, 1, 1, 1, 1, 1, 1, 1, 1, 1, 1, 1, 1, 1, 1, 1, 1, 1, 1, 1, 4 ),
 ( -0.1039086239011999951, 1.103908623900999864 ),
 ( -0.02000000000000000042, 0.01250000000000000069, 0.04499999999999999833, 0.07749999999999999944, 0.1100000000000000006, 0.1424999999999999878, 0.1749999999999999889, 0.2074999999999999900, 0.2399999999999999911, 0.2725000000000000200, 0.3049999999999999933, 0.3375000000000000222, 0.3699999999999999956, 0.4025000000000000244, 0.4349999999999999978, 0.4675000000000000266, 0.5000000000000000000, 0.5324999999999999734, 0.5649999999999999467, 0.5975000000000000311, 0.6300000000000000044, 0.6624999999999999778, 0.6949999999999999512, 0.7275000000000000355, 0.7600000000000000089, 0.7924999999999999822, 0.8249999999999999556, 0.8575000000000000400, 0.8900000000000000133, 0.9224999999999999867, 0.9549999999999999600, 0.9875000000000000444, 1.020000000000000018 ),
 .UNSPECIFIED. ) ;
#33423 = CARTESIAN_POINT ( 'NONE',  ( 6.911134836320000474, -12.43100038668999829, -2.821124938267000282 ) ) ;
#33424 = CARTESIAN_POINT ( 'NONE',  ( 4.149992563291999836, -1.747525841223986465, 1.007210908820208140 ) ) ;
#33425 = ORIENTED_EDGE ( 'NONE', *, *, #22122, .F. ) ;
#33427 = CARTESIAN_POINT ( 'NONE',  ( 9.313108942797164502, 2.920708135355637225, -8.329534079918376577 ) ) ;
#33426 = CARTESIAN_POINT ( 'NONE',  ( 8.866808059624998961, -2.550589632307000088, 8.854674225901000284 ) ) ;
#33428 = CARTESIAN_POINT ( 'NONE',  ( 8.863029719594999634, 2.990001567622999623, -8.695425648791999862 ) ) ;
#33429 = DIRECTION ( 'NONE',  ( 0.000000000000000000, 1.000000000000000000, 0.000000000000000000 ) ) ;
#33430 = CARTESIAN_POINT ( 'NONE',  ( 6.999999691988000095, -12.11716380430000051, 3.069905306952000146 ) ) ;
#33431 = CARTESIAN_POINT ( 'NONE',  ( 0.5105665232603000536, 3.646234950436999966, -0.6383912046097000026 ) ) ;
#33432 = B_SPLINE_SURFACE_WITH_KNOTS ( 'NONE', 3, 3, ( 
 ( #27378, #16192, #43466, #58840 ),
 ( #59186, #9916, #53937, #21100 ),
 ( #48350, #15513, #47330, #52564 ),
 ( #6040, #64413, #42425, #64073 ),
 ( #25999, #48704, #27038, #37515 ),
 ( #68633, #52915, #20754, #22123 ),
 ( #53600, #37176, #457, #4660 ),
 ( #42082, #36838, #58157, #10259 ),
 ( #63733, #15845, #31941, #5358 ),
 ( #26697, #50088, #2197, #22816 ) ),
 .UNSPECIFIED., .F., .F., .F.,
 ( 4, 1, 1, 1, 1, 1, 1, 4 ),
 ( 4, 4 ),
 ( 0.04111222701783000255, 0.1428571428570999946, 0.2857142857143000203, 0.4285714285713999594, 0.5714285714286000406, 0.7142857142856999797, 0.8571428571429000609, 0.9278613184711000939 ),
 ( -0.1900620218102000158, 1.190128522698000069 ),
 .UNSPECIFIED. ) ;
#33433 = LINE ( 'NONE', #54749, #65541 ) ;
#33434 = CARTESIAN_POINT ( 'NONE',  ( 3.024430197351000160, 1.374756561418999823, -3.318718615493999824 ) ) ;
#33435 = ORIENTED_EDGE ( 'NONE', *, *, #64292, .F. ) ;
#33436 = CARTESIAN_POINT ( 'NONE',  ( 12.15201606283210900, 0.3124912280145352161, -12.59612551846059780 ) ) ;
#33437 = DIRECTION ( 'NONE',  ( 0.000000000000000000, 0.000000000000000000, -1.000000000000000000 ) ) ;
#33438 = DIRECTION ( 'NONE',  ( -0.5000000000000150990, 0.08222066253632250021, -0.8621135439442261239 ) ) ;
#33439 = CARTESIAN_POINT ( 'NONE',  ( 7.165489158771000788, 2.688365364125000045, 8.140015608605001063 ) ) ;
#33440 = ORIENTED_EDGE ( 'NONE', *, *, #57129, .T. ) ;
#33441 = CARTESIAN_POINT ( 'NONE',  ( 5.780416005063000462, 1.497237214918999859, -0.6046620561147000306 ) ) ;
#33442 = B_SPLINE_CURVE_WITH_KNOTS ( 'NONE', 3,
 ( #19229, #2808, #40556, #39884 ),
 .UNSPECIFIED., .F., .F.,
 ( 4, 4 ),
 ( 0.000000000000000000, 1.000000000000000000 ),
 .UNSPECIFIED. ) ;
#33443 = CARTESIAN_POINT ( 'NONE',  ( 10.93466815658861613, 9.405386378085696109, 6.163902746065222260 ) ) ;
#33445 = CARTESIAN_POINT ( 'NONE',  ( 11.00588826681000043, 3.012760565655999923, 5.961496895743000124 ) ) ;
#33444 = CARTESIAN_POINT ( 'NONE',  ( 8.606573840185609114, -4.691422996753022545, 5.902471595303201646 ) ) ;
#33446 = CARTESIAN_POINT ( 'NONE',  ( 11.17901463001529905, 4.697110652903200290, -6.383488688482000128 ) ) ;
#33447 = EDGE_LOOP ( 'NONE', ( #49588, #20542, #13029, #48684, #65198 ) ) ;
#33448 = CARTESIAN_POINT ( 'NONE',  ( 8.616332388160998335, -5.167567399848000065, -6.822293593032000558 ) ) ;
#33449 = B_SPLINE_CURVE_WITH_KNOTS ( 'NONE', 3,
 ( #54303, #37197, #64433, #58515, #65128, #59552, #22144, #827, #37884 ),
 .UNSPECIFIED., .F., .F.,
 ( 4, 1, 2, 2, 4 ),
 ( 0.000000000000000000, 0.2500000000000002220, 0.3750000000000004441, 0.5000000000000006661, 1.000000000000000000 ),
 .UNSPECIFIED. ) ;
#33450 = CARTESIAN_POINT ( 'NONE',  ( 8.241912900173000267, 4.599999999999999645, 6.117539782833000928 ) ) ;
#33451 = ORIENTED_EDGE ( 'NONE', *, *, #28863, .T. ) ;
#33452 = DIRECTION ( 'NONE',  ( 0.000000000000000000, -0.9999606858717338120, 0.008867170401640298016 ) ) ;
#33453 = CARTESIAN_POINT ( 'NONE',  ( 16.07488484168399978, 3.504106430365000246, 11.16639795596000084 ) ) ;
#33454 = CARTESIAN_POINT ( 'NONE',  ( 18.17177275037307638, -0.1018973686818569341, -13.89950237059084870 ) ) ;
#33455 = ADVANCED_FACE ( 'NONE', ( #30147 ), #29811, .F. ) ;
#33456 = EDGE_CURVE ( 'NONE', #11483, #24435, #51454, .T. ) ;
#33457 = ORIENTED_EDGE ( 'NONE', *, *, #66716, .F. ) ;
#33458 = CARTESIAN_POINT ( 'NONE',  ( 10.59529221449796665, -2.228646686619264905, -7.375818029046365076 ) ) ;
#33459 = CARTESIAN_POINT ( 'NONE',  ( 24.53428988874600236, -8.855929874993998752, -9.286429786912000495 ) ) ;
#33460 = CARTESIAN_POINT ( 'NONE',  ( 10.52946886766499901, 3.569835351907400423, -6.718432993015899690 ) ) ;
#33461 = CARTESIAN_POINT ( 'NONE',  ( 9.643927823787143083, -2.750011555256801188, 7.500000155056757656 ) ) ;
#33462 = CARTESIAN_POINT ( 'NONE',  ( 24.54223752884104925, 3.611770689525808375, 12.30300795115269175 ) ) ;
#33463 = VERTEX_POINT ( 'NONE', #19989 ) ;
#33464 = LINE ( 'NONE', #17730, #38760 ) ;
#33465 = CARTESIAN_POINT ( 'NONE',  ( 12.31588542589000390, -2.889160216960383387, -13.58313038422638286 ) ) ;
#33466 = CARTESIAN_POINT ( 'NONE',  ( 9.885596873516664829, -5.092232985442824322, 6.870476274536375882 ) ) ;
#33467 = CARTESIAN_POINT ( 'NONE',  ( 15.95168611684299975, -8.949867560646000086, -8.553740745252000011 ) ) ;
#33468 = B_SPLINE_CURVE_WITH_KNOTS ( 'NONE', 3,
 ( #42914, #12136, #54782, #609 ),
 .UNSPECIFIED., .F., .F.,
 ( 4, 4 ),
 ( 0.000000000000000000, 1.000000000000000000 ),
 .UNSPECIFIED. ) ;
#33469 = ORIENTED_EDGE ( 'NONE', *, *, #22954, .T. ) ;
#33470 = CARTESIAN_POINT ( 'NONE',  ( 12.18021258978589039, -2.482515821435917314, -12.45562150274660596 ) ) ;
#33471 = CARTESIAN_POINT ( 'NONE',  ( 10.79184687351629535, 3.000416447002276943, -6.731816600031355513 ) ) ;
#33472 = CARTESIAN_POINT ( 'NONE',  ( 7.640272165042063079, 2.497528546856052412, -6.408390592194270319 ) ) ;
#33473 = DIRECTION ( 'NONE',  ( 0.000000000000000000, -0.7614089499631908620, 0.6482718649732929217 ) ) ;
#33474 = CARTESIAN_POINT ( 'NONE',  ( 11.49978667957999967, -12.52500000000000213, -0.5112815185527788131 ) ) ;
#33475 = B_SPLINE_CURVE_WITH_KNOTS ( 'NONE', 3,
 ( #7183, #22907, #65207, #38650, #12083, #17680 ),
 .UNSPECIFIED., .F., .F.,
 ( 4, 2, 4 ),
 ( 0.000000000000000000, 0.5000000000000000000, 1.000000000000000000 ),
 .UNSPECIFIED. ) ;
#33476 = CARTESIAN_POINT ( 'NONE',  ( 11.67918044953561996, -2.988516238873000219, -8.027436060358800418 ) ) ;
#33477 = CARTESIAN_POINT ( 'NONE',  ( 5.877943173017373901, 0.9218200799623692543, 1.199500263597272687 ) ) ;
#33478 = CARTESIAN_POINT ( 'NONE',  ( 17.89002091993515720, -1.842089822799543253, 12.46461944294985358 ) ) ;
#33479 = ORIENTED_EDGE ( 'NONE', *, *, #7796, .T. ) ;
#33480 = CARTESIAN_POINT ( 'NONE',  ( 11.22056920625029974, -3.952687217764870198, -6.184582852561999466 ) ) ;
#33481 = EDGE_CURVE ( 'NONE', #6782, #43577, #27487, .T. ) ;
#33482 = ORIENTED_EDGE ( 'NONE', *, *, #51651, .T. ) ;
#33483 = AXIS2_PLACEMENT_3D ( 'NONE', #21468, #68322, #64110 ) ;
#33484 = CARTESIAN_POINT ( 'NONE',  ( 3.999971066382000284, -2.149963194831999935, 0.000000000000000000 ) ) ;
#33485 = CARTESIAN_POINT ( 'NONE',  ( 8.725348536223782148, -2.649439212887072959, 7.500023728975150128 ) ) ;
#33486 = EDGE_CURVE ( 'NONE', #38790, #47849, #18955, .T. ) ;
#33487 = CARTESIAN_POINT ( 'NONE',  ( 2.796577467967999997, 2.816309704165000039, -1.867789267639999862 ) ) ;
#33488 = CARTESIAN_POINT ( 'NONE',  ( 10.22440803363000050, -5.317414323721999736, -8.272454209812998727 ) ) ;
#33489 = CARTESIAN_POINT ( 'NONE',  ( 6.629591280611910165, -1.445352440277137163, -0.4631782753073599990 ) ) ;
#33490 = CARTESIAN_POINT ( 'NONE',  ( 5.200000002601999682, 0.2500000026021999555, 3.150000007068999963 ) ) ;
#33491 = CARTESIAN_POINT ( 'NONE',  ( 11.57299956498156845, 5.207010770456999893, 7.174999999999999822 ) ) ;
#33492 = VERTEX_POINT ( 'NONE', #14741 ) ;
#33493 = CARTESIAN_POINT ( 'NONE',  ( 4.600000127571206576, -3.073097332162000125E-13, -5.595524044110998485E-14 ) ) ;
#33494 = CARTESIAN_POINT ( 'NONE',  ( 12.25718044953559982, -3.110233631466100324, 7.036033215662999218 ) ) ;
#33495 = CARTESIAN_POINT ( 'NONE',  ( 9.815201913989998417, 2.813632032385000148, 8.848857341496000117 ) ) ;
#33496 = CARTESIAN_POINT ( 'NONE',  ( 11.09999999999999964, -2.700000000000000178, -6.461133846875999787 ) ) ;
#33497 = CARTESIAN_POINT ( 'NONE',  ( 12.80505043854144276, -0.7192913403693169672, -12.57945229203838267 ) ) ;
#33498 = CARTESIAN_POINT ( 'NONE',  ( 18.44721083353000068, 2.702837639295000205, -11.38762126772000016 ) ) ;
#33499 = CARTESIAN_POINT ( 'NONE',  ( 11.38795122972049967, 4.398282450130399646, -6.578956058177199751 ) ) ;
#33500 = EDGE_CURVE ( 'NONE', #29486, #5467, #15843, .T. ) ;
#33501 = CARTESIAN_POINT ( 'NONE',  ( 10.34160003447459708, 3.644395320192564736, 9.238506757596626429 ) ) ;
#33502 = CARTESIAN_POINT ( 'NONE',  ( 9.555709346417000205, 5.031430618794000331, -7.010219103474399915 ) ) ;
#33503 = CARTESIAN_POINT ( 'NONE',  ( 23.74330720574500120, -9.836545709669998416, -9.383277561883000217 ) ) ;
#33504 = CARTESIAN_POINT ( 'NONE',  ( 24.15332041333400070, -9.223082443678000786, 9.474599958732000005 ) ) ;
#33505 = CARTESIAN_POINT ( 'NONE',  ( 11.50029455687000102, 11.65000000000000036, 0.000000000000000000 ) ) ;
#33506 = VERTEX_POINT ( 'NONE', #57376 ) ;
#33507 = CARTESIAN_POINT ( 'NONE',  ( 7.308879440377999970, -4.847802017252000439, 9.065364004483999594 ) ) ;
#33508 = CARTESIAN_POINT ( 'NONE',  ( 9.397139116365000433, -4.993413662858000812, -9.088148847710000311 ) ) ;
#33509 = CARTESIAN_POINT ( 'NONE',  ( 18.06966903239548827, 2.854820418091308820, 13.59172178685414423 ) ) ;
#33510 = CARTESIAN_POINT ( 'NONE',  ( 24.60000000000000142, 0.000000000000000000, -5.000000000000000000 ) ) ;
#33511 = CARTESIAN_POINT ( 'NONE',  ( 11.10887482311539998, -2.815046254222000055, -7.978749413531599721 ) ) ;
#33512 = ORIENTED_EDGE ( 'NONE', *, *, #20264, .T. ) ;
#33513 = DIRECTION ( 'NONE',  ( -1.000000000000000000, 0.000000000000000000, 0.000000000000000000 ) ) ;
#33514 = CARTESIAN_POINT ( 'NONE',  ( 9.272295280408998863, 3.705846972803000128, 9.096435887808000942 ) ) ;
#33516 = CARTESIAN_POINT ( 'NONE',  ( 11.42834208742529967, 3.293478249981899975, 6.389420067180999752 ) ) ;
#33515 = CARTESIAN_POINT ( 'NONE',  ( 8.356920280409999791, 4.851303550474000303, -9.008742670124000540 ) ) ;
#33517 = CARTESIAN_POINT ( 'NONE',  ( 2.855370644018131010, 1.774957683866571490, 2.731955323636169553 ) ) ;
#33518 = ORIENTED_EDGE ( 'NONE', *, *, #28946, .T. ) ;
#33519 = CARTESIAN_POINT ( 'NONE',  ( 9.743561007103998861, 5.287400066955999733, 8.939966147452000911 ) ) ;
#33520 = CARTESIAN_POINT ( 'NONE',  ( 18.24298441323066555, -2.287290078788475345, -13.81189461436434307 ) ) ;
#33521 = CARTESIAN_POINT ( 'NONE',  ( 10.79718447801629999, 5.003225587801999552, 7.522119512433738997 ) ) ;
#33522 = CARTESIAN_POINT ( 'NONE',  ( 9.834153701540001791, -5.173926576843999925, 8.813045240277000758 ) ) ;
#33523 = CARTESIAN_POINT ( 'NONE',  ( 8.057199896074001444, 2.877672799700000450, 6.732802633655004421 ) ) ;
#33524 = VERTEX_POINT ( 'NONE', #9478 ) ;
#33525 = CARTESIAN_POINT ( 'NONE',  ( 24.60999195316300003, 12.22061417693999985, -3.051130890528999995 ) ) ;
#33527 = CARTESIAN_POINT ( 'NONE',  ( 10.59956814679000026, -4.438148200474000937, -8.958389257466000899 ) ) ;
#33526 = CARTESIAN_POINT ( 'NONE',  ( 12.13190478341600098, -11.96733320521999921, 3.503025077341000326 ) ) ;
#33528 = CARTESIAN_POINT ( 'NONE',  ( 7.677856441088493078, -5.680960098108038814, 7.021194307766620568 ) ) ;
#33529 = CARTESIAN_POINT ( 'NONE',  ( 9.380781717619999682, -2.204246399534000034, 7.545378188773000261 ) ) ;
#33530 = CARTESIAN_POINT ( 'NONE',  ( 23.54917040509700144, 2.965869371470000182, 13.72136993952999973 ) ) ;
#33531 = CARTESIAN_POINT ( 'NONE',  ( 10.13264655415100002, -3.447209681134600245, 6.500921769151600138 ) ) ;
#33532 = EDGE_LOOP ( 'NONE', ( #9799, #32810, #52532, #26827 ) ) ;
#33533 = CARTESIAN_POINT ( 'NONE',  ( 23.84134149042290574, -9.640897496743738415, 9.399424730200435008 ) ) ;
#33534 = CARTESIAN_POINT ( 'NONE',  ( 11.85502763632550050, -5.160433036184000066, 8.035454525731699604 ) ) ;
#33535 = ORIENTED_EDGE ( 'NONE', *, *, #33310, .T. ) ;
#33536 = CARTESIAN_POINT ( 'NONE',  ( 17.60000000000000142, 10.78295181803999903, -4.410266442048000002 ) ) ;
#33537 = ORIENTED_EDGE ( 'NONE', *, *, #56098, .T. ) ;
#33538 = EDGE_CURVE ( 'NONE', #63477, #7350, #63382, .T. ) ;
#33539 = EDGE_CURVE ( 'NONE', #52478, #65259, #68202, .T. ) ;
#33540 = CARTESIAN_POINT ( 'NONE',  ( 9.848670280409999478, 5.002683760508999988, -8.912673867568997821 ) ) ;
#33541 = CARTESIAN_POINT ( 'NONE',  ( 23.85322625602900004, 13.16205774920000060, -3.533916265924000211 ) ) ;
#33542 = EDGE_CURVE ( 'NONE', #15832, #29686, #54932, .T. ) ;
#33543 = CARTESIAN_POINT ( 'NONE',  ( 12.63802361681258191, 3.180808137691514936, -12.19190235712761883 ) ) ;
#33544 = CARTESIAN_POINT ( 'NONE',  ( 11.31524174883999834, -4.028418853626810403, 6.466884287543999577 ) ) ;
#33545 = CARTESIAN_POINT ( 'NONE',  ( 7.000000000000000000, -9.186881099820000784, 5.186879182879000183 ) ) ;
#33546 = ORIENTED_EDGE ( 'NONE', *, *, #15417, .T. ) ;
#33547 = FACE_OUTER_BOUND ( 'NONE', #68969, .T. ) ;
#33548 = CARTESIAN_POINT ( 'NONE',  ( 16.39999999347100257, 3.345256695718999751, 11.86066175541999890 ) ) ;
#33549 = VERTEX_POINT ( 'NONE', #42681 ) ;
#33550 = CARTESIAN_POINT ( 'NONE',  ( 10.14163331274965962, -2.604736771093051129, -6.440282737489662956 ) ) ;
#33551 = CARTESIAN_POINT ( 'NONE',  ( 10.89149144726329865, 3.340422662105400065, 8.430724369296298093 ) ) ;
#33552 = CARTESIAN_POINT ( 'NONE',  ( 24.35365242081700288, 3.193712117489998281, -11.49150331539999215 ) ) ;
#33553 = CARTESIAN_POINT ( 'NONE',  ( 11.03408597791999846, 2.992846905312999795, -9.056576857348998644 ) ) ;
#33554 = CARTESIAN_POINT ( 'NONE',  ( 17.83726331522299802, -11.40363207186999972, 4.542070182500999920 ) ) ;
#33555 = CARTESIAN_POINT ( 'NONE',  ( 12.79999998875598344, 11.49049412642037460, -4.802266170000438983 ) ) ;
#33556 = CARTESIAN_POINT ( 'NONE',  ( 12.55449126378684532, -3.072671109762266095, -13.53512077903586786 ) ) ;
#33557 = CARTESIAN_POINT ( 'NONE',  ( 18.11112283403659262, -0.2853680816562768063, -12.69568625917504257 ) ) ;
#33558 = CARTESIAN_POINT ( 'NONE',  ( 12.19275557192769632, 2.625384353351010613, -12.42149591643997475 ) ) ;
#33559 = CARTESIAN_POINT ( 'NONE',  ( 11.35918179236250047, -4.238363971154499588, -6.384440618559000136 ) ) ;
#33560 = CARTESIAN_POINT ( 'NONE',  ( 9.385308886257000438, 4.135077451221000011, 9.175524215473998879 ) ) ;
#33561 = VERTEX_POINT ( 'NONE', #37777 ) ;
#33562 = B_SPLINE_CURVE_WITH_KNOTS ( 'NONE', 3,
 ( #49141, #22911, #43909, #11384, #43561, #55082, #64175, #911, #64861, #42866, #6836, #28169, #49485, #1596, #6138, #32725 ),
 .UNSPECIFIED., .F., .F.,
 ( 4, 2, 2, 2, 2, 2, 2, 4 ),
 ( 0.000000000000000000, 0.06250000000000043021, 0.1250000000000008604, 0.2500000000000007216, 0.3750000000000006106, 0.5000000000000005551, 0.7500000000000002220, 1.000000000000000000 ),
 .UNSPECIFIED. ) ;
#33563 =( LENGTH_UNIT ( ) NAMED_UNIT ( * ) SI_UNIT ( .MILLI., .METRE. ) );
#33564 = CARTESIAN_POINT ( 'NONE',  ( 23.89320776801300283, -10.87822567731000234, 3.284864823438000236 ) ) ;
#33565 = CARTESIAN_POINT ( 'NONE',  ( 10.31021345716899873, 4.636538040886300394, 6.921280946186199934 ) ) ;
#33566 = CARTESIAN_POINT ( 'NONE',  ( 7.856038276909000473, 2.869044596334999753, -6.744487387516000076 ) ) ;
#33567 = CARTESIAN_POINT ( 'NONE',  ( 24.13718786373500080, -3.227326363975000056, 12.37799336445999998 ) ) ;
#33568 = AXIS2_PLACEMENT_3D ( 'NONE', #2941, #46975, #47664 ) ;
#33569 = CARTESIAN_POINT ( 'NONE',  ( 17.79060029153382416, 3.161091907734801865, 12.19703033907565981 ) ) ;
#33570 = DIRECTION ( 'NONE',  ( 1.000000000000000000, 0.000000000000000000, 0.000000000000000000 ) ) ;
#33571 = CARTESIAN_POINT ( 'NONE',  ( 11.00000000000000000, 2.941427501403999667, -7.825000000000000178 ) ) ;
#33572 = CARTESIAN_POINT ( 'NONE',  ( 10.43464903646999886, -8.245890014837998550, -6.615317941358999754 ) ) ;
#33573 = CARTESIAN_POINT ( 'NONE',  ( 8.811649685568998080, 4.101356036306899711, 6.542299367266399379 ) ) ;
#33574 = EDGE_LOOP ( 'NONE', ( #6769, #51674, #9533, #23945 ) ) ;
#33575 = CARTESIAN_POINT ( 'NONE',  ( 12.11461379017079665, -2.700589376673579789, 12.30719081517757907 ) ) ;
#33576 = CARTESIAN_POINT ( 'NONE',  ( 9.682355082327998019, -4.511005581663400044, -6.478918346312998899 ) ) ;
#33577 = CARTESIAN_POINT ( 'NONE',  ( 24.54688887196200042, -3.662825465818000392, -12.34578425079000041 ) ) ;
#33578 = FACE_OUTER_BOUND ( 'NONE', #13255, .T. ) ;
#33579 = B_SPLINE_CURVE_WITH_KNOTS ( 'NONE', 3,
 ( #24301, #23271, #28881, #55779 ),
 .UNSPECIFIED., .F., .F.,
 ( 4, 4 ),
 ( 0.000000000000000000, 1.000000000000000000 ),
 .UNSPECIFIED. ) ;
#33580 = B_SPLINE_SURFACE_WITH_KNOTS ( 'NONE', 3, 3, ( 
 ( #32775, #43615, #58996, #53062 ),
 ( #6185, #16340, #38356, #11780 ),
 ( #37666, #21924, #54436, #48161 ),
 ( #42571, #27184, #17024, #31746 ),
 ( #16680, #15993, #43262, #64910 ),
 ( #47826, #27527, #11434, #69136 ),
 ( #11098, #5163, #962, #5507 ),
 ( #54088, #42916, #26847, #26496 ),
 ( #32432, #37324, #22273, #59682 ) ),
 .UNSPECIFIED., .F., .F., .F.,
 ( 4, 1, 1, 1, 1, 1, 4 ),
 ( 4, 4 ),
 ( -0.01864526228370000024, 0.000000000000000000, 0.2500000000000000000, 0.5000000000000000000, 0.7500000000000000000, 1.000000000000000000, 1.019255357118999950 ),
 ( -0.2206650646280000072, 1.220665064628000174 ),
 .UNSPECIFIED. ) ;
#33581 = CARTESIAN_POINT ( 'NONE',  ( 11.53148876160955005, 3.209326035813000022, -8.322268080792200706 ) ) ;
#33582 = ORIENTED_EDGE ( 'NONE', *, *, #43714, .T. ) ;
#33583 = EDGE_CURVE ( 'NONE', #62256, #52670, #4938, .T. ) ;
#33584 = CARTESIAN_POINT ( 'NONE',  ( 12.25170120909046645, -0.4648927885597778920, 12.59142395508372836 ) ) ;
#33585 = CARTESIAN_POINT ( 'NONE',  ( 9.395323341230000125, 5.146726419831999522, 6.597424767138000412 ) ) ;
#33586 = DIRECTION ( 'NONE',  ( 0.000000000000000000, 0.000000000000000000, -1.000000000000000000 ) ) ;
#33587 = CARTESIAN_POINT ( 'NONE',  ( 12.33364337825305768, 2.910866508044257284, 12.34629936699908370 ) ) ;
#33588 = EDGE_LOOP ( 'NONE', ( #26220, #64721, #56650 ) ) ;
#33589 = CARTESIAN_POINT ( 'NONE',  ( 8.748814158775001459, 5.251032986819000214, -6.070151079272999795 ) ) ;
#33590 = CARTESIAN_POINT ( 'NONE',  ( 11.52733460557258915, 4.206337284815599986, -8.761245990815998752 ) ) ;
#33591 = FACE_OUTER_BOUND ( 'NONE', #67276, .T. ) ;
#33593 = CARTESIAN_POINT ( 'NONE',  ( 17.59542495535444218, -0.6250000000000002220, 12.67928922306855277 ) ) ;
#33592 = CARTESIAN_POINT ( 'NONE',  ( 8.500383147356993518, 5.097359707274998541, 6.605634423517003029 ) ) ;
#33594 = CARTESIAN_POINT ( 'NONE',  ( 9.528772138681999238, -4.322628849750500102, 8.304747519296199698 ) ) ;
#33595 = CARTESIAN_POINT ( 'NONE',  ( 11.34287482311539996, -3.196874704906699893, -7.824481664695199790 ) ) ;
#33596 = CARTESIAN_POINT ( 'NONE',  ( 11.29996849689000271, 12.23272706294999956, 1.505586356912999912 ) ) ;
#33597 = ORIENTED_EDGE ( 'NONE', *, *, #66632, .F. ) ;
#33598 = CARTESIAN_POINT ( 'NONE',  ( 1.353155746511000235, 3.398721108301999916, 0.4283847067656000318 ) ) ;
#33599 = CARTESIAN_POINT ( 'NONE',  ( 23.98814404780929621, -9.385780080724808627, -9.282153661438828252 ) ) ;
#33600 = CARTESIAN_POINT ( 'NONE',  ( 9.462753061708918167, -5.112753122729035482, 7.646523492023318269 ) ) ;
#33601 = CARTESIAN_POINT ( 'NONE',  ( 18.28104795956111062, 2.296528561426856019, -12.39041189979782409 ) ) ;
#33602 = B_SPLINE_CURVE_WITH_KNOTS ( 'NONE', 3,
 ( #19669, #62315, #50803, #3915, #40639, #61974, #39619, #55703, #13058, #34728, #66519, #14430, #13739, #7801, #45216, #35072, #8146, #50448, #18642, #40306, #62981, #4955, #30849, #52856, #67895, #63327, #14770, #4264, #31537, #47958, #15792, #53546, #37123, #5636, #26291, #20013, #15457, #36087, #25601, #47617, #56, #15108, #21042, #31202, #37459, #20697, #58781, #36430, #21377, #10889, #68928, #42710, #64015, #57747, #42374, #16136, #32233, #63677, #41337, #62647, #58439, #26979, #31885, #57402, #9857, #20351, #41675, #52507, #4607 ),
 .UNSPECIFIED., .F., .F.,
 ( 4, 2, 2, 2, 2, 2, 2, 2, 2, 2, 2, 2, 2, 1, 2, 2, 2, 1, 2, 2, 2, 2, 1, 2, 2, 2, 2, 2, 2, 2, 2, 2, 2, 2, 2, 4 ),
 ( 0.000000000000000000, 0.06250000000002821354, 0.1250000000000564271, 0.1562500000000705269, 0.1875000000000846545, 0.2187500000000987543, 0.2343750000001060263, 0.2500000000001132983, 0.2812500000001282863, 0.2968750000001355582, 0.3125000000001428302, 0.3281250000001501022, 0.3437500000001573741, 0.3593750000001646461, 0.3671875000001683098, 0.3750000000001719735, 0.3906250000001779688, 0.3984375000001809108, 0.4023437500001826872, 0.4062500000001844636, 0.4218750000001930678, 0.4296875000001972866, 0.4335937500001988965, 0.4355468750001977307, 0.4375000000001965650, 0.4531250000001914580, 0.4687500000001863509, 0.4843750000001812439, 0.5000000000001760814, 0.5312500000001659783, 0.5468750000001606493, 0.5625000000001552092, 0.5937500000001438849, 0.6250000000001325606, 0.7500000000000878186, 1.000000000000000000 ),
 .UNSPECIFIED. ) ;
#33603 = CARTESIAN_POINT ( 'NONE',  ( 24.44916829770000177, -12.41483723393999838, 3.103225306172999964 ) ) ;
#33604 = CARTESIAN_POINT ( 'NONE',  ( 12.10347303272475372, -2.332585440199567817, 13.80433171579881879 ) ) ;
#33605 = CARTESIAN_POINT ( 'NONE',  ( 10.95213788363000162, 2.845858105723999998, 5.181730564763999958 ) ) ;
#33606 = CARTESIAN_POINT ( 'NONE',  ( 24.13681546429500102, 3.227485322444999749, -12.37873180773000215 ) ) ;
#33607 = CARTESIAN_POINT ( 'NONE',  ( 13.46281931570200108, -12.03411875281000043, -2.480748420245000307 ) ) ;
#33608 = EDGE_LOOP ( 'NONE', ( #44481, #44925, #47721, #15375 ) ) ;
#33609 = CONICAL_SURFACE ( 'NONE', #51462, 10.64999999998000035, 0.7853981633972997312 ) ;
#33610 = CARTESIAN_POINT ( 'NONE',  ( 17.55505043854144631, -0.7192913403693119712, -12.57945229203838267 ) ) ;
#33611 = CARTESIAN_POINT ( 'NONE',  ( 9.550814556648244746, 5.350066006687046460, -7.263181378929296272 ) ) ;
#33612 = CARTESIAN_POINT ( 'NONE',  ( 17.74638838757924120, -10.78680295286659074, 4.401676307955865397 ) ) ;
#33613 = CARTESIAN_POINT ( 'NONE',  ( 18.41451919223733213, -3.018310540773369688, -11.25254019301576669 ) ) ;
#33614 = CARTESIAN_POINT ( 'NONE',  ( 10.81746213571000048, -5.100000000000000533, 6.571291218949999902 ) ) ;
#33615 = FACE_OUTER_BOUND ( 'NONE', #50512, .T. ) ;
#33616 = AXIS2_PLACEMENT_3D ( 'NONE', #9817, #64315, #58741 ) ;
#33617 = CARTESIAN_POINT ( 'NONE',  ( 17.75825915738905536, 1.908867900852240673, -12.56984843829418530 ) ) ;
#33618 = CARTESIAN_POINT ( 'NONE',  ( 9.625496329943999285, 3.134638325776999856, 8.626949804392001653 ) ) ;
#33619 = CARTESIAN_POINT ( 'NONE',  ( 11.29364426047339975, 4.466097552695299733, 6.769896129503799820 ) ) ;
#33620 = EDGE_CURVE ( 'NONE', #28572, #30733, #49330, .T. ) ;
#33621 = EDGE_CURVE ( 'NONE', #58219, #14861, #49380, .T. ) ;
#33622 = CARTESIAN_POINT ( 'NONE',  ( 10.90000000164000049, -2.899999999992999733, 5.160242739040000082 ) ) ;
#33623 = CARTESIAN_POINT ( 'NONE',  ( 10.48598064679000075, -5.506038521567000465, -7.274786670944999756 ) ) ;
#33624 = CARTESIAN_POINT ( 'NONE',  ( 18.20249159964110675, 0.3803681712634291445, -13.99548972733973073 ) ) ;
#33625 = EDGE_CURVE ( 'NONE', #51298, #4821, #63303, .T. ) ;
#33626 = EDGE_CURVE ( 'NONE', #18530, #17232, #869, .T. ) ;
#33627 = DIRECTION ( 'NONE',  ( 1.000000000000000000, 0.000000000000000000, 0.000000000000000000 ) ) ;
#33628 = CARTESIAN_POINT ( 'NONE',  ( 12.19004578041274911, -2.611920287615140168, 12.42482035882550484 ) ) ;
#33629 = ORIENTED_EDGE ( 'NONE', *, *, #68166, .T. ) ;
#33630 = CARTESIAN_POINT ( 'NONE',  ( 8.845310841232000953, 5.851083642416999631, -7.072167224702999633 ) ) ;
#33631 = ORIENTED_EDGE ( 'NONE', *, *, #40923, .T. ) ;
#33632 = B_SPLINE_CURVE_WITH_KNOTS ( 'NONE', 3,
 ( #60358, #66284, #33800, #7220, #6867, #28557, #60702, #7913, #28914, #12819, #49868, #7560, #1982, #23304, #44644, #39381, #34145, #50219, #18408, #56490, #57863, #20114, #20802, #68684, #4019, #51248 ),
 .UNSPECIFIED., .F., .F.,
 ( 4, 2, 2, 2, 2, 2, 2, 2, 2, 2, 2, 2, 4 ),
 ( 0.000000000000000000, 0.08792262688039514940, 0.1758452537607902988, 0.2198065672009883176, 0.2417872239210860641, 0.2527775522811350761, 0.2637678806411841159, 0.3516905075215719378, 0.4396131344019597598, 0.4835744478421525883, 0.5055551045622493911, 0.5275357612823460274, 0.7033810150431129005 ),
 .UNSPECIFIED. ) ;
#33633 = CARTESIAN_POINT ( 'NONE',  ( 18.17485192111307057, -2.583003800953512563, 13.65552556266986350 ) ) ;
#33634 = FACE_OUTER_BOUND ( 'NONE', #15567, .T. ) ;
#33635 = ORIENTED_EDGE ( 'NONE', *, *, #58227, .F. ) ;
#33636 = CARTESIAN_POINT ( 'NONE',  ( 10.89324174884020024, 3.967693531726030010, 6.325557131097000685 ) ) ;
#33637 = CYLINDRICAL_SURFACE ( 'NONE', #42748, 0.4999999999999998335 ) ;
#33638 = CARTESIAN_POINT ( 'NONE',  ( 7.774523880555999966, -9.023795782617998640, 5.558109039331999846 ) ) ;
#33639 = CARTESIAN_POINT ( 'NONE',  ( 9.305881816721999655, 4.945299866898000829, 9.077891794505999812 ) ) ;
#33640 = FACE_OUTER_BOUND ( 'NONE', #66149, .T. ) ;
#33641 = CARTESIAN_POINT ( 'NONE',  ( 11.09999993992000000, 9.806598331764000420, -6.066326716004000197 ) ) ;
#33642 = CARTESIAN_POINT ( 'NONE',  ( 11.35620373058000077, 3.594096350588000366, -11.23428177897000069 ) ) ;
#33643 = CARTESIAN_POINT ( 'NONE',  ( 10.49937632700000023, -2.985311165300999825, -6.358653174814000053 ) ) ;
#33644 = CARTESIAN_POINT ( 'NONE',  ( 11.63825819896753977, -4.851203879749700576, -7.660469764776300039 ) ) ;
#33645 = CARTESIAN_POINT ( 'NONE',  ( 10.36409408021999923, -3.399999909169000301, -4.954046131279000065 ) ) ;
#33646 = ORIENTED_EDGE ( 'NONE', *, *, #41271, .F. ) ;
#33647 = ADVANCED_FACE ( 'NONE', ( #63990 ), #2478, .F. ) ;
#33648 = CARTESIAN_POINT ( 'NONE',  ( 8.923129650240841926, 3.341122914829671497, -6.641242496392400163 ) ) ;
#33649 = VERTEX_POINT ( 'NONE', #32541 ) ;
#33650 = CARTESIAN_POINT ( 'NONE',  ( 10.81218444402201584, 3.003105123708600388, -4.859602167815589624 ) ) ;
#33651 =( NAMED_UNIT ( * ) PLANE_ANGLE_UNIT ( ) SI_UNIT ( $, .RADIAN. ) );
#33652 = CARTESIAN_POINT ( 'NONE',  ( 10.62546583196254879, -2.957832985152635263, 5.049157649731592201 ) ) ;
#33653 = CARTESIAN_POINT ( 'NONE',  ( 10.06430484851600049, 5.163382381259999931, -8.031907719862799055 ) ) ;
#33654 = CARTESIAN_POINT ( 'NONE',  ( 12.41408225146703970, 2.012274740545226592, 13.76483611190083600 ) ) ;
#33655 = CARTESIAN_POINT ( 'NONE',  ( 9.444317341922999987, -2.927260449021000355, 8.897015448164999896 ) ) ;
#33656 = VERTEX_POINT ( 'NONE', #4577 ) ;
#33657 = CARTESIAN_POINT ( 'NONE',  ( 7.878292898358790097, 3.256492674266815435, -6.335713178755712605 ) ) ;
#33658 = CARTESIAN_POINT ( 'NONE',  ( 12.11457335221578369, 0.2229649748661308717, 13.99822903660538564 ) ) ;
#33659 = ORIENTED_EDGE ( 'NONE', *, *, #43881, .F. ) ;
#33660 = CARTESIAN_POINT ( 'NONE',  ( 12.78268972790800184, 11.49710380946999955, -4.820178426657999005 ) ) ;
#33661 = DIRECTION ( 'NONE',  ( 0.000000000000000000, -0.5000000000000169864, 0.8660254037844288266 ) ) ;
#33662 = B_SPLINE_CURVE_WITH_KNOTS ( 'NONE', 3,
 ( #2343, #28578, #2001, #65616 ),
 .UNSPECIFIED., .F., .F.,
 ( 4, 4 ),
 ( 0.000000000000000000, 1.000000000000000000 ),
 .UNSPECIFIED. ) ;
#33663 = CARTESIAN_POINT ( 'NONE',  ( 8.821633776942626071, 4.724939341952408611, 7.010106850326409678 ) ) ;
#33664 = CARTESIAN_POINT ( 'NONE',  ( 4.794575572191000390, -1.188595002225999897, -0.6069625248515000404 ) ) ;
#33665 = CARTESIAN_POINT ( 'NONE',  ( 9.874770280412001000, 4.038835765825999680, -5.935509327774999733 ) ) ;
#33666 = EDGE_CURVE ( 'NONE', #31242, #9579, #38381, .T. ) ;
#33667 = CARTESIAN_POINT ( 'NONE',  ( 8.378939856114634210, -5.131721215521674040, 6.760536705178638250 ) ) ;
#33668 = CARTESIAN_POINT ( 'NONE',  ( 10.07930721860999945, -2.718124813223000036, -6.397797539448999871 ) ) ;
#33669 = CARTESIAN_POINT ( 'NONE',  ( 8.064958992852089281, 5.350069970865218849, -7.500002487662858819 ) ) ;
#33670 = AXIS2_PLACEMENT_3D ( 'NONE', #12760, #33046, #64839 ) ;
#33671 = FACE_OUTER_BOUND ( 'NONE', #21911, .T. ) ;
#33672 = ADVANCED_FACE ( 'NONE', ( #36404 ), #25575, .T. ) ;
#33673 = CARTESIAN_POINT ( 'NONE',  ( 9.216140818749000374, -4.008306780893000187, -8.877926425468999128 ) ) ;
#33674 = FACE_OUTER_BOUND ( 'NONE', #59199, .T. ) ;
#33675 = DIRECTION ( 'NONE',  ( -1.000000000000000000, 0.000000000000000000, 0.000000000000000000 ) ) ;
#33676 = CARTESIAN_POINT ( 'NONE',  ( 10.60235971519489873, 4.605301262871499546, -6.493038401303000029 ) ) ;
#33677 = CARTESIAN_POINT ( 'NONE',  ( 9.735975701333000387, 4.736880367605900588, -8.182531775206799196 ) ) ;
#33679 = CARTESIAN_POINT ( 'NONE',  ( 4.650000881942629505, 3.375077994860000042E-14, 13.94999927503010362 ) ) ;
#33678 = CARTESIAN_POINT ( 'NONE',  ( 9.823721904869998411, -3.243980311826100138, 7.075568408810499754 ) ) ;
#33680 = CARTESIAN_POINT ( 'NONE',  ( 11.32101354018296568, -4.768183399968640934, 8.499583552997727054 ) ) ;
#33681 = ORIENTED_EDGE ( 'NONE', *, *, #10811, .T. ) ;
#33682 = CARTESIAN_POINT ( 'NONE',  ( 10.89324174884020024, 3.967693531726030010, 6.325557131097000685 ) ) ;
#33683 = AXIS2_PLACEMENT_3D ( 'NONE', #34848, #50920, #3019 ) ;
#33684 = CARTESIAN_POINT ( 'NONE',  ( 10.65050275296000137, -5.200029647236999786, 5.937716681140000397 ) ) ;
#33685 = CARTESIAN_POINT ( 'NONE',  ( 9.859659112603999631, 3.503852111758100296, 6.471616938597000157 ) ) ;
#33686 = CARTESIAN_POINT ( 'NONE',  ( 9.708153928322625248, 3.619812067603167538, -8.288028809740389136 ) ) ;
#33687 = CARTESIAN_POINT ( 'NONE',  ( 9.972852379787999766, -5.044471434015000533, 6.258101649750000384 ) ) ;
#33688 = CARTESIAN_POINT ( 'NONE',  ( 23.57773632097178407, -13.28348942634863583, 4.287207044979979287 ) ) ;
#33690 = UNCERTAINTY_MEASURE_WITH_UNIT (LENGTH_MEASURE( 1.000000000000000082E-05 ), #59323, 'distance_accuracy_value', 'NONE');
#33689 = CARTESIAN_POINT ( 'NONE',  ( 10.47726354018323214, 3.370476274536374106, 6.407767014557177454 ) ) ;
#33691 = VERTEX_POINT ( 'NONE', #10860 ) ;
#33692 = CARTESIAN_POINT ( 'NONE',  ( 9.153405316139998860, -4.213249376011100722, -8.481512610189300361 ) ) ;
#33693 = CARTESIAN_POINT ( 'NONE',  ( 9.708513540183332680, -3.836375382625528019, -6.250000000000001776 ) ) ;
#33694 = CARTESIAN_POINT ( 'NONE',  ( 5.055026506350000837, -1.500000000000000000, 0.000000000000000000 ) ) ;
#33695 = CARTESIAN_POINT ( 'NONE',  ( 6.999998971696786754, 12.01547034654740109, 3.452253082527627637 ) ) ;
#33696 = CARTESIAN_POINT ( 'NONE',  ( 5.700000000000000178, 13.04986661130000059, -1.811520473896000016 ) ) ;
#33697 = CARTESIAN_POINT ( 'NONE',  ( 12.21210404293059959, -4.381818659177399766, 6.722495590581700320 ) ) ;
#33698 = CARTESIAN_POINT ( 'NONE',  ( 11.73256516821459883, 4.706297556651700020, -8.212808089543500500 ) ) ;
#33699 = CARTESIAN_POINT ( 'NONE',  ( 4.599999651764373532, 13.27499965161999818, -2.617296141720999949E-09 ) ) ;
#33700 = CARTESIAN_POINT ( 'NONE',  ( 25.40241821196899963, -8.312581368709999197, 8.374650789474999968 ) ) ;
#33701 = CARTESIAN_POINT ( 'NONE',  ( 5.619513206070969602, 12.94695275831319492, 2.446394316580341233 ) ) ;
#33702 = ORIENTED_EDGE ( 'NONE', *, *, #27078, .T. ) ;
#33703 = CARTESIAN_POINT ( 'NONE',  ( 9.136057238048000073, -5.084840204920000772, -6.477689566282000655 ) ) ;
#33704 = ADVANCED_FACE ( 'NONE', ( #21015 ), #32206, .T. ) ;
#33705 = CARTESIAN_POINT ( 'NONE',  ( 12.78440349184324987, 0.6249994334955760733, -13.88107975403457495 ) ) ;
#33706 = EDGE_CURVE ( 'NONE', #13653, #45966, #46899, .T. ) ;
#33707 = CARTESIAN_POINT ( 'NONE',  ( 11.00000000000000000, -5.058572498595999889, -7.825000000000000178 ) ) ;
#33708 = CARTESIAN_POINT ( 'NONE',  ( 25.26979265321100243, -8.566783789541000615, -7.890681328063000599 ) ) ;
#33709 = CARTESIAN_POINT ( 'NONE',  ( 13.18179592085193974, -11.52326738618029012, -1.714065324703454740 ) ) ;
#33710 = CARTESIAN_POINT ( 'NONE',  ( 10.57960558317114774, 4.353252721116626311, 8.851706718789662531 ) ) ;
#33711 = CARTESIAN_POINT ( 'NONE',  ( 5.602426839032992767, 12.13128594426812690, -3.749700506050852145 ) ) ;
#33712 = VERTEX_POINT ( 'NONE', #59102 ) ;
#33713 = VECTOR ( 'NONE', #29869, 1000.000000000000000 ) ;
#33714 = B_SPLINE_CURVE_WITH_KNOTS ( 'NONE', 3,
 ( #53852, #16102, #53514, #27 ),
 .UNSPECIFIED., .F., .F.,
 ( 4, 4 ),
 ( 0.000000000000000000, 1.000000000000000000 ),
 .UNSPECIFIED. ) ;
#33715 = CARTESIAN_POINT ( 'NONE',  ( 3.500000000000000000, 0.000000000000000000, 0.000000000000000000 ) ) ;
#33716 = CARTESIAN_POINT ( 'NONE',  ( 18.05294241905982133, 2.122066809870763127, -13.74638883949611845 ) ) ;
#33717 = EDGE_LOOP ( 'NONE', ( #35593, #27001, #58935, #36998, #43669 ) ) ;
#33718 = DIRECTION ( 'NONE',  ( 0.000000000000000000, 0.000000000000000000, -1.000000000000000000 ) ) ;
#33719 = CARTESIAN_POINT ( 'NONE',  ( 24.72673738265526922, 8.645762772944534547, -8.593181399093179351 ) ) ;
#33720 = CARTESIAN_POINT ( 'NONE',  ( 8.772439158776000667, 3.098073081301000009, -8.567513114264999174 ) ) ;
#33721 = CARTESIAN_POINT ( 'NONE',  ( 9.365000000002998704, -2.649999999999999911, -7.500000000000000000 ) ) ;
#33722 = CARTESIAN_POINT ( 'NONE',  ( 11.22056920625029974, -3.952687217764870198, -6.184582852561999466 ) ) ;
#33723 = DIRECTION ( 'NONE',  ( 0.000000000000000000, -1.000000000000000000, 0.000000000000000000 ) ) ;
#33724 = CARTESIAN_POINT ( 'NONE',  ( 10.39393020684999946, 2.750000000000000000, -7.500000000000000000 ) ) ;
#33725 = ORIENTED_EDGE ( 'NONE', *, *, #30100, .T. ) ;
#33726 = CARTESIAN_POINT ( 'NONE',  ( 8.368787704064557076, 3.808649829341963056, -6.044288580653415899 ) ) ;
#33727 = CARTESIAN_POINT ( 'NONE',  ( 18.10300909149178494, -2.800751615193656008, -13.60500513792289468 ) ) ;
#33728 = CARTESIAN_POINT ( 'NONE',  ( 8.947714158774999760, 3.854507394315999758, -9.394302886912999639 ) ) ;
#33729 = VERTEX_POINT ( 'NONE', #21690 ) ;
#33730 = EDGE_CURVE ( 'NONE', #26679, #852, #32442, .T. ) ;
#33731 = CARTESIAN_POINT ( 'NONE',  ( 9.701722306758000514, 4.253749110891999585, -8.839930742927998963 ) ) ;
#33732 = CARTESIAN_POINT ( 'NONE',  ( 11.00000000000000000, 2.941427501403999667, 7.174999999999999822 ) ) ;
#33733 = VERTEX_POINT ( 'NONE', #43024 ) ;
#33734 = CARTESIAN_POINT ( 'NONE',  ( 9.558671671056998775, 3.009461603020800347, 7.333638993632098924 ) ) ;
#33735 = CARTESIAN_POINT ( 'NONE',  ( 18.19141764354318269, -2.135256814392523683, -12.41776106013548464 ) ) ;
#33736 = CONICAL_SURFACE ( 'NONE', #37074, 2.325000277643999969, 0.7853982725543797727 ) ;
#33737 = CARTESIAN_POINT ( 'NONE',  ( 9.508513540182335078, 3.836375382625529795, 6.250000000000000888 ) ) ;
#33738 = CARTESIAN_POINT ( 'NONE',  ( 15.86053068095500151, 3.820355458042000052, 11.67812044351000011 ) ) ;
#33739 = CARTESIAN_POINT ( 'NONE',  ( 11.29998658800000122, 3.824194713071000340, -11.71675648045999907 ) ) ;
#33740 = B_SPLINE_CURVE_WITH_KNOTS ( 'NONE', 3,
 ( #46089, #18841, #2071, #40838 ),
 .UNSPECIFIED., .F., .F.,
 ( 4, 4 ),
 ( 0.000000000000000000, 0.1253528645472067604 ),
 .UNSPECIFIED. ) ;
#33741 = B_SPLINE_CURVE_WITH_KNOTS ( 'NONE', 3,
 ( #45799, #56635, #50360, #45462 ),
 .UNSPECIFIED., .F., .F.,
 ( 4, 4 ),
 ( 0.000000000000000000, 1.000000000000000000 ),
 .UNSPECIFIED. ) ;
#33742 = CARTESIAN_POINT ( 'NONE',  ( 10.01459632033899894, 3.070047649444500149, 7.879514065647800436 ) ) ;
#33743 = CARTESIAN_POINT ( 'NONE',  ( 9.353559602067283762, -3.378361522263298777, 9.124549040636324548 ) ) ;
#33744 = ORIENTED_EDGE ( 'NONE', *, *, #32052, .F. ) ;
#33745 = CARTESIAN_POINT ( 'NONE',  ( 10.69030645188999884, 5.903031974240000146, 7.830710565751001440 ) ) ;
#33746 = CARTESIAN_POINT ( 'NONE',  ( 10.22094528040999961, 2.563078870232999851, -8.004103956955001209 ) ) ;
#33747 = CARTESIAN_POINT ( 'NONE',  ( 17.55505043854147118, -3.125000000000000000, -13.52078605991414761 ) ) ;
#33748 = CARTESIAN_POINT ( 'NONE',  ( 12.54527475442094442, 3.068547466015816294, -13.53629565290702352 ) ) ;
#33749 = LINE ( 'NONE', #17666, #24796 ) ;
#33750 = CARTESIAN_POINT ( 'NONE',  ( 24.84741859043700174, 3.386183434052000063, 11.85236409072000008 ) ) ;
#33751 = CARTESIAN_POINT ( 'NONE',  ( 18.17115727977514084, -0.3856318793704094361, 13.99470184309725695 ) ) ;
#33752 = CARTESIAN_POINT ( 'NONE',  ( 17.93439120251456487, 0.4967442791785504075, 13.88805191678101458 ) ) ;
#33753 = ORIENTED_EDGE ( 'NONE', *, *, #13383, .T. ) ;
#33754 = ORIENTED_EDGE ( 'NONE', *, *, #18095, .T. ) ;
#33755 = CARTESIAN_POINT ( 'NONE',  ( 9.594139158774000364, 2.212639797530000063, -6.855876382544999537 ) ) ;
#33756 = EDGE_CURVE ( 'NONE', #37026, #13153, #22469, .T. ) ;
#33757 = CARTESIAN_POINT ( 'NONE',  ( 12.54858531443457892, -0.5700392133465188582, 13.88426419246647292 ) ) ;
#33758 = CARTESIAN_POINT ( 'NONE',  ( 12.72336452621133773, -0.6199804606865816359, -13.88138355690254855 ) ) ;
#33759 = CARTESIAN_POINT ( 'NONE',  ( 10.37874387220000116, -4.882732524430000609, 6.350796477317000921 ) ) ;
#33760 = CARTESIAN_POINT ( 'NONE',  ( 23.56665676678700194, 2.935519496638999914, -13.67844162499000049 ) ) ;
#33761 = CARTESIAN_POINT ( 'NONE',  ( 7.935745559623000212, -5.430412429559000387, 7.210798766422999329 ) ) ;
#33762 = DIRECTION ( 'NONE',  ( -1.000000000000000000, 0.000000000000000000, 0.000000000000000000 ) ) ;
#33764 = FACE_OUTER_BOUND ( 'NONE', #58629, .T. ) ;
#33763 = CARTESIAN_POINT ( 'NONE',  ( 9.829759580229000093, -5.244164909883999748, 7.797385380423699885 ) ) ;
#33765 = CARTESIAN_POINT ( 'NONE',  ( 10.88733729122639993, 2.722429312291999803, -7.466391690027689876 ) ) ;
#33766 = AXIS2_PLACEMENT_3D ( 'NONE', #36559, #15581, #8366 ) ;
#33767 = CARTESIAN_POINT ( 'NONE',  ( 5.700000000399000122, -0.2999999996014000025, -3.150000003758000044 ) ) ;
#33768 = CARTESIAN_POINT ( 'NONE',  ( 23.56960665000709909, 10.30499699461899610, -9.460494264439814671 ) ) ;
#33769 = CARTESIAN_POINT ( 'NONE',  ( 18.05145864173986325, 0.3802890292809061323, 12.69234946364260708 ) ) ;
#33770 = CARTESIAN_POINT ( 'NONE',  ( 6.537665658289999904, -1.082219296144999898, 1.053440284172000085 ) ) ;
#33771 = CARTESIAN_POINT ( 'NONE',  ( 17.88923853192078184, -3.028508370110811310, -12.31258559103177674 ) ) ;
#33772 = EDGE_LOOP ( 'NONE', ( #9286, #58360, #65424, #48904, #43663 ) ) ;
#33774 = CARTESIAN_POINT ( 'NONE',  ( 11.09999999999999964, 5.299999999999999822, -5.160242713806000303 ) ) ;
#33773 = CARTESIAN_POINT ( 'NONE',  ( 11.09999999999999964, -6.593648099371000271, -5.598803483715999896 ) ) ;
#33775 = CARTESIAN_POINT ( 'NONE',  ( 9.061929719594999710, 4.092867382745001059, -5.937785237406000505 ) ) ;
#33776 = CARTESIAN_POINT ( 'NONE',  ( 25.60000000000000142, 0.000000000000000000, 0.000000000000000000 ) ) ;
#33777 = LINE ( 'NONE', #40307, #32164 ) ;
#33778 = CARTESIAN_POINT ( 'NONE',  ( 10.32118582084299874, 3.163839350524900063, 8.466515260542900378 ) ) ;
#33779 = CIRCLE ( 'NONE', #8124, 11.49999999999999467 ) ;
#33780 = LINE ( 'NONE', #51227, #44550 ) ;
#33781 = LINE ( 'NONE', #61032, #40995 ) ;
#33782 = AXIS2_PLACEMENT_3D ( 'NONE', #47078, #68379, #47771 ) ;
#33783 = CARTESIAN_POINT ( 'NONE',  ( 2.685883213202000075, 3.284924929773000102, -0.9716413097203999705 ) ) ;
#33784 = ORIENTED_EDGE ( 'NONE', *, *, #47858, .T. ) ;
#33785 = CARTESIAN_POINT ( 'NONE',  ( 12.13986395842896648, -0.2863297863804592502, -12.59675086341328232 ) ) ;
#33786 = LINE ( 'NONE', #8580, #17497 ) ;
#33787 = CARTESIAN_POINT ( 'NONE',  ( 23.95413516103606000, -12.78631318506285020, -3.518586055979009863 ) ) ;
#33788 = CARTESIAN_POINT ( 'NONE',  ( 7.833767219591000419, 2.583668273793999770, 6.684750595573999199 ) ) ;
#33789 = EDGE_LOOP ( 'NONE', ( #28923, #68395, #36203, #63855 ) ) ;
#33790 = CARTESIAN_POINT ( 'NONE',  ( 6.839116717017999392, 1.514695785805999950, 0.5594970275663000425 ) ) ;
#33791 = EDGE_CURVE ( 'NONE', #41535, #22650, #31177, .T. ) ;
#33792 = EDGE_CURVE ( 'NONE', #27164, #10252, #43723, .T. ) ;
#33793 = CARTESIAN_POINT ( 'NONE',  ( 7.987835841226000433, 4.422660346525999486, -6.167928437610999737 ) ) ;
#33795 = CARTESIAN_POINT ( 'NONE',  ( 10.80457650502821387, 2.650115154242055127, -7.676668932391350175 ) ) ;
#33794 = CARTESIAN_POINT ( 'NONE',  ( 8.557873356888400451, -3.635451402876086924, 5.799052727755670489 ) ) ;
#33796 = CARTESIAN_POINT ( 'NONE',  ( 11.34523293495530005, 2.684794526488000432, -7.447129085684729866 ) ) ;
#33797 = VERTEX_POINT ( 'NONE', #39164 ) ;
#33798 = CARTESIAN_POINT ( 'NONE',  ( 10.12670810574000058, -3.117521507207000386, 8.613544937223998943 ) ) ;
#33799 = ORIENTED_EDGE ( 'NONE', *, *, #33481, .F. ) ;
#33800 = CARTESIAN_POINT ( 'NONE',  ( 9.511909979525512426, -4.618059472559051137, 8.703333823275881898 ) ) ;
#33801 = CARTESIAN_POINT ( 'NONE',  ( 25.39408680342049252, -2.774728762786359493, -11.32588899302948882 ) ) ;
#33802 = CARTESIAN_POINT ( 'NONE',  ( 18.18003636789866917, -0.02080959496299032013, -13.89999914846831075 ) ) ;
#33803 = ORIENTED_EDGE ( 'NONE', *, *, #45969, .F. ) ;
#33804 = CARTESIAN_POINT ( 'NONE',  ( 10.94095842555437059, 9.300938419463392393, -6.243091547608035086 ) ) ;
#33805 = LINE ( 'NONE', #50224, #328 ) ;
#33806 = B_SPLINE_CURVE_WITH_KNOTS ( 'NONE', 3,
 ( #20221, #16348, #57618, #5171, #5854, #53757 ),
 .UNSPECIFIED., .F., .F.,
 ( 4, 2, 4 ),
 ( 0.000000000000000000, 0.5000000000000000000, 1.000000000000000000 ),
 .UNSPECIFIED. ) ;
#33807 = LINE ( 'NONE', #65942, #68313 ) ;
#33808 = FACE_OUTER_BOUND ( 'NONE', #3000, .T. ) ;
#33809 = CARTESIAN_POINT ( 'NONE',  ( 25.34480302439135713, 8.474813402932349859, 7.997915580558633941 ) ) ;
#33810 = ORIENTED_EDGE ( 'NONE', *, *, #30315, .T. ) ;
#33811 = CARTESIAN_POINT ( 'NONE',  ( 5.200000000000000178, -1.600000000000000089, 0.000000000000000000 ) ) ;
#33812 = CARTESIAN_POINT ( 'NONE',  ( 23.55064466279999991, -13.34882249087999995, -4.337886341278000657 ) ) ;
#33813 = ADVANCED_FACE ( 'NONE', ( #18187 ), #65228, .F. ) ;
#33814 = CARTESIAN_POINT ( 'NONE',  ( 16.10004050617000004, 7.492404338401442487, 10.08789649943575029 ) ) ;
#33815 = VECTOR ( 'NONE', #64343, 1000.000000000000114 ) ;
#33816 = CARTESIAN_POINT ( 'NONE',  ( 8.849999778957998942, 4.000000000000000000, -7.500000000000000000 ) ) ;
#33817 = ORIENTED_EDGE ( 'NONE', *, *, #62888, .F. ) ;
#33818 = CYLINDRICAL_SURFACE ( 'NONE', #48378, 2.750000000000000000 ) ;
#33819 = ADVANCED_FACE ( 'NONE', ( #54551 ), #27642, .F. ) ;
#33820 = CARTESIAN_POINT ( 'NONE',  ( 8.837278925393345475, -3.116678102649797832, -6.987098574663185069 ) ) ;
#33821 = CARTESIAN_POINT ( 'NONE',  ( 7.938622165042806600, 4.610389606898620762, -9.253982923057691323 ) ) ;
#33822 = CARTESIAN_POINT ( 'NONE',  ( 5.000030787343001215, -1.057581170753187694, 1.834918991542629163 ) ) ;
#33823 = LINE ( 'NONE', #39405, #36563 ) ;
#33824 = CARTESIAN_POINT ( 'NONE',  ( 6.999998782146999332, -11.95749337870000062, -3.642574926947999892 ) ) ;
#33825 = CARTESIAN_POINT ( 'NONE',  ( 17.61541550669256395, -1.763241988052376641, 12.47601615708916789 ) ) ;
#33826 = ORIENTED_EDGE ( 'NONE', *, *, #31967, .F. ) ;
#33827 = CARTESIAN_POINT ( 'NONE',  ( 11.68277869730536977, -4.531392946702499813, -6.452143920160000157 ) ) ;
#33828 = ORIENTED_EDGE ( 'NONE', *, *, #36018, .T. ) ;
#33829 = AXIS2_PLACEMENT_3D ( 'NONE', #35183, #62079, #14198 ) ;
#33830 = CARTESIAN_POINT ( 'NONE',  ( 11.48381255716000027, -12.35454260995000020, -1.695649549036999826 ) ) ;
#33831 = CARTESIAN_POINT ( 'NONE',  ( 9.983079719591000156, 5.002683760508999988, -8.912673867568997821 ) ) ;
#33832 = CARTESIAN_POINT ( 'NONE',  ( 3.208990468877999991, 2.744503479086000119, -1.674591564687999856 ) ) ;
#33833 = CARTESIAN_POINT ( 'NONE',  ( 9.701728707608999969, -4.253751259212999791, -8.839942087209999855 ) ) ;
#33834 = CARTESIAN_POINT ( 'NONE',  ( 24.45625562564337585, 3.500080689026665581, 12.27866752497065761 ) ) ;
#33835 = CARTESIAN_POINT ( 'NONE',  ( 8.220124669774001802, 3.381964873247001790, -6.130490311850000928 ) ) ;
#33836 = LINE ( 'NONE', #34182, #30028 ) ;
#33837 = VERTEX_POINT ( 'NONE', #38819 ) ;
#33838 = CARTESIAN_POINT ( 'NONE',  ( 18.26242637978999994, 2.744390477411999818, 11.56740641610000075 ) ) ;
#33839 = CARTESIAN_POINT ( 'NONE',  ( 12.15871932425157098, -4.147141405561299621, 6.507377093516500288 ) ) ;
#33840 = CARTESIAN_POINT ( 'NONE',  ( 9.571961069101000419, 4.084683332033999470, 8.946609345378000455 ) ) ;
#33841 = DIRECTION ( 'NONE',  ( -1.000000000000000000, 0.000000000000000000, 0.000000000000000000 ) ) ;
#33842 = DIRECTION ( 'NONE',  ( 1.000000000000000000, 0.000000000000000000, 0.000000000000000000 ) ) ;
#33843 = DIRECTION ( 'NONE',  ( 0.000000000000000000, -0.8648648648648717963, 0.5020047465136829867 ) ) ;
#33844 = CARTESIAN_POINT ( 'NONE',  ( 11.14179841651039915, 3.646693590264900031, -8.439215328713499886 ) ) ;
#33845 = CARTESIAN_POINT ( 'NONE',  ( 7.100000000000060041, 5.084948259510642110, -8.362010274963123990 ) ) ;
#33846 = ADVANCED_FACE ( 'NONE', ( #12251 ), #23687, .T. ) ;
#33847 = ADVANCED_FACE ( 'NONE', ( #12596 ), #34597, .F. ) ;
#33848 = CARTESIAN_POINT ( 'NONE',  ( 9.859659112603999631, 3.503852111758100296, -8.528383061402999843 ) ) ;
#33849 = CARTESIAN_POINT ( 'NONE',  ( 23.61707917866500139, -10.26292876439000068, 9.294242752039000521 ) ) ;
#33850 = CARTESIAN_POINT ( 'NONE',  ( 11.02452225494999993, 2.775477745048999800, -6.571291218949999902 ) ) ;
#33851 = EDGE_LOOP ( 'NONE', ( #13598, #47186, #34099, #44600 ) ) ;
#33852 = CARTESIAN_POINT ( 'NONE',  ( 7.950754440378000609, -2.095727472214000020, 8.056487497515000484 ) ) ;
#33853 = CARTESIAN_POINT ( 'NONE',  ( 9.883740731405000091, -5.634417356902000407, -7.003562403358999156 ) ) ;
#33854 = CARTESIAN_POINT ( 'NONE',  ( 18.22207129059743380, 2.231684076289587981, 13.82098807703153476 ) ) ;
#33855 = CARTESIAN_POINT ( 'NONE',  ( 23.56971388309658266, 3.042564011621391895, 13.65415468161493706 ) ) ;
#33856 = CARTESIAN_POINT ( 'NONE',  ( 10.78887616594230003, -4.386455737425299262, -6.281817606595999415 ) ) ;
#33857 = VERTEX_POINT ( 'NONE', #49129 ) ;
#33858 = CONICAL_SURFACE ( 'NONE', #20471, 11.75015521449999945, 0.7854113701714536822 ) ;
#33859 = CARTESIAN_POINT ( 'NONE',  ( 25.20466149916200038, 2.650184388215000020, -11.40090097795000013 ) ) ;
#33860 = CARTESIAN_POINT ( 'NONE',  ( 8.052732780410000402, 4.968147183437999992, 5.971792472497999604 ) ) ;
#33862 = CARTESIAN_POINT ( 'NONE',  ( 11.01279632507519857, 4.624908853805600906, 6.341531314375999706 ) ) ;
#33861 = FACE_OUTER_BOUND ( 'NONE', #24500, .T. ) ;
#33863 = CARTESIAN_POINT ( 'NONE',  ( 10.45625165877000029, 3.661871102473000406, -9.317475234260999883 ) ) ;
#33864 = VERTEX_POINT ( 'NONE', #1242 ) ;
#33865 = CARTESIAN_POINT ( 'NONE',  ( 9.632179190069999564, 5.638172764974000550, 6.476627236431999890 ) ) ;
#33866 = CARTESIAN_POINT ( 'NONE',  ( 18.00769469217373597, -3.088460579138319062, -13.65508963078420201 ) ) ;
#33867 = CARTESIAN_POINT ( 'NONE',  ( 10.69456919669529960, 5.093991349577000172, 7.176777099639999768 ) ) ;
#33868 = CARTESIAN_POINT ( 'NONE',  ( 11.11504459742000073, -3.456612073675000119, 5.970342812640000218 ) ) ;
#33869 = CARTESIAN_POINT ( 'NONE',  ( 8.332048273611004419, 2.867478057767001154, 6.314276212112998721 ) ) ;
#33870 = ORIENTED_EDGE ( 'NONE', *, *, #61002, .T. ) ;
#33871 = CARTESIAN_POINT ( 'NONE',  ( 8.983146706526143888, -2.899999999999999911, 6.231099004638222638 ) ) ;
#33872 = ADVANCED_FACE ( 'NONE', ( #22554 ), #13950, .T. ) ;
#33873 = EDGE_CURVE ( 'NONE', #42176, #32174, #15719, .T. ) ;
#33874 = CARTESIAN_POINT ( 'NONE',  ( 10.38725444037999956, -2.888666857901000196, -6.716331201355000502 ) ) ;
#33875 = CARTESIAN_POINT ( 'NONE',  ( 7.929910832275415267, -2.314979100831407788, 7.934222329365288040 ) ) ;
#33876 = CARTESIAN_POINT ( 'NONE',  ( 9.538434317036999843, -5.620900626097999897, 7.423100105894999245 ) ) ;
#33877 = CARTESIAN_POINT ( 'NONE',  ( 23.58699566483300103, 3.020915523320000240, 13.60570109925000004 ) ) ;
#33878 = CARTESIAN_POINT ( 'NONE',  ( 10.00600081823899856, -5.010295986746999830, 6.967988282883199602 ) ) ;
#33879 = ORIENTED_EDGE ( 'NONE', *, *, #55235, .T. ) ;
#33880 = CARTESIAN_POINT ( 'NONE',  ( 24.73253179669367086, -11.75903539564235523, -3.190943823743348950 ) ) ;
#33881 = ADVANCED_FACE ( 'NONE', ( #6044 ), #68992, .T. ) ;
#33882 = CARTESIAN_POINT ( 'NONE',  ( 10.72687885159599830, -2.867290578374000365, 7.635128076451499268 ) ) ;
#33883 = ORIENTED_EDGE ( 'NONE', *, *, #65959, .T. ) ;
#33884 = LINE ( 'NONE', #50304, #9401 ) ;
#33885 = AXIS2_PLACEMENT_3D ( 'NONE', #25212, #41300, #44583 ) ;
#33886 = ORIENTED_EDGE ( 'NONE', *, *, #64761, .F. ) ;
#33887 = CARTESIAN_POINT ( 'NONE',  ( 9.193385841233000733, 2.981992329588000423, -5.895876591910999664 ) ) ;
#33888 = CARTESIAN_POINT ( 'NONE',  ( 23.51706673858500096, 13.43779730422000007, -4.375994916149999803 ) ) ;
#33889 = CARTESIAN_POINT ( 'NONE',  ( 9.115118560745049336, 5.349923934101355805, -7.499992884230159973 ) ) ;
#33890 = CARTESIAN_POINT ( 'NONE',  ( 12.61495819220210635, 3.174994159617164691, -12.19341885412869608 ) ) ;
#33891 = CARTESIAN_POINT ( 'NONE',  ( 11.48656920625009903, -3.967932847735990531, 8.391549386185598536 ) ) ;
#33892 = CARTESIAN_POINT ( 'NONE',  ( 9.791846873516664829, 3.000416447002276943, 8.268183399968645375 ) ) ;
#33894 = ORIENTED_EDGE ( 'NONE', *, *, #13156, .F. ) ;
#33893 = B_SPLINE_CURVE_WITH_KNOTS ( 'NONE', 3,
 ( #11750, #16653, #48823, #15966, #54408, #48478, #47802, #585, #64195, #59653, #21894, #58618, #43231, #27498, #10717, #64536, #5482, #11405, #33092, #20872, #42210, #26817, #63512, #42888 ),
 .UNSPECIFIED., .F., .F.,
 ( 4, 2, 1, 1, 1, 2, 2, 1, 2, 2, 2, 2, 2, 4 ),
 ( 0.000000000000000000, 0.2499999999999175104, 0.3749999999998697708, 0.4374999999998425704, 0.4687499999998201994, 0.4843749999998034350, 0.4999999999997866706, 0.5624999999998281375, 0.5937499999998393507, 0.6249999999998505640, 0.6874999999998731015, 0.7499999999998955280, 0.8749999999999477085, 1.000000000000000000 ),
 .UNSPECIFIED. ) ;
#33895 = CARTESIAN_POINT ( 'NONE',  ( 9.496378438922302934, 5.350075508921114498, 7.852928877054549339 ) ) ;
#33896 = CARTESIAN_POINT ( 'NONE',  ( 24.30001694670299983, 8.938702829764999080, 8.938676122491999720 ) ) ;
#33897 = ORIENTED_EDGE ( 'NONE', *, *, #48928, .F. ) ;
#33898 = CARTESIAN_POINT ( 'NONE',  ( 12.10796728133595579, -2.678710578830987288, -12.31197141455839272 ) ) ;
#33899 = ADVANCED_FACE ( 'NONE', ( #64765 ), #61949, .F. ) ;
#33900 = CARTESIAN_POINT ( 'NONE',  ( 11.43302763632549990, 2.964209339073000216, 7.977941233841399971 ) ) ;
#33901 = CARTESIAN_POINT ( 'NONE',  ( 10.18576633586645031, 4.069734382926330163, -8.865705745737809451 ) ) ;
#33902 = CARTESIAN_POINT ( 'NONE',  ( 10.68055531501999944, 2.768167480619000198, -6.114404645958000373 ) ) ;
#33903 = CARTESIAN_POINT ( 'NONE',  ( 18.22523891024100351, -11.70723067604000001, 3.729442327036999849 ) ) ;
#33904 = LINE ( 'NONE', #17112, #19648 ) ;
#33905 = CARTESIAN_POINT ( 'NONE',  ( 12.42259655075935143, -2.994741173188553596, -13.55594337657172410 ) ) ;
#33906 = CARTESIAN_POINT ( 'NONE',  ( 18.09636316215239660, 0.3125877143166576055, -12.69482668528969604 ) ) ;
#33907 = CARTESIAN_POINT ( 'NONE',  ( 7.399999923048000028, -0.9999997023190999590, 0.000000000000000000 ) ) ;
#33908 = CARTESIAN_POINT ( 'NONE',  ( 11.08841369783139896, -4.057552111898620417, -8.639288317626999003 ) ) ;
#33909 = DIRECTION ( 'NONE',  ( 0.000000000000000000, -1.000000000000000000, 0.000000000000000000 ) ) ;
#33910 = VERTEX_POINT ( 'NONE', #16882 ) ;
#33911 = AXIS2_PLACEMENT_3D ( 'NONE', #33140, #6205, #64244 ) ;
#33912 = CARTESIAN_POINT ( 'NONE',  ( 17.55505043854147118, -3.248147246781390329, -13.61798588129781074 ) ) ;
#33913 = CARTESIAN_POINT ( 'NONE',  ( 10.60113158428419311, -5.349785647438510594, -7.263300972600942984 ) ) ;
#33914 = CARTESIAN_POINT ( 'NONE',  ( 11.18484176840999922, 2.599663474744000169, 7.740674686800000259 ) ) ;
#33915 = CARTESIAN_POINT ( 'NONE',  ( 24.32839855075200219, -3.577297860116000372, 12.48354892467999910 ) ) ;
#33916 = CARTESIAN_POINT ( 'NONE',  ( 18.09076461395649105, 2.178034604381229311, 12.52076370778328851 ) ) ;
#33917 = CARTESIAN_POINT ( 'NONE',  ( 13.50003721581400029, -9.159934378815998812, -7.517910889891000537 ) ) ;
#33918 = CARTESIAN_POINT ( 'NONE',  ( 9.566963020987998334, 5.215925787220999865, 6.177726425586999248 ) ) ;
#33919 = CARTESIAN_POINT ( 'NONE',  ( 10.08150819241162566, -4.779998216922380472, 7.896402636871828307 ) ) ;
#33920 = CARTESIAN_POINT ( 'NONE',  ( 2.328734235851999568, 1.852089340889000013, 2.627990287460999941 ) ) ;
#33921 = ORIENTED_EDGE ( 'NONE', *, *, #35969, .F. ) ;
#33922 = CARTESIAN_POINT ( 'NONE',  ( 12.49755103297840542, -3.131894283645457300, 12.20455838002552795 ) ) ;
#33923 = CARTESIAN_POINT ( 'NONE',  ( 9.021784697134998865, -3.454948069423500190, -6.656340890368899643 ) ) ;
#33924 = CARTESIAN_POINT ( 'NONE',  ( 24.43231275843400141, -3.176386277817000003, -12.00227839950999886 ) ) ;
#33925 = CARTESIAN_POINT ( 'NONE',  ( 9.343930206849998754, 2.750000000000000000, 7.500000000000000000 ) ) ;
#33926 = AXIS2_PLACEMENT_3D ( 'NONE', #46156, #20267, #51056 ) ;
#33927 = CARTESIAN_POINT ( 'NONE',  ( 11.42887348028849992, 2.875789035466000065, -8.107837221875000111 ) ) ;
#33928 = CARTESIAN_POINT ( 'NONE',  ( 12.09857507241189900, -0.1632583333441840756, 12.59896334813831764 ) ) ;
#33929 = AXIS2_PLACEMENT_3D ( 'NONE', #58241, #21182, #57902 ) ;
#33930 = ADVANCED_FACE ( 'NONE', ( #22128 ), #21426, .T. ) ;
#33931 = EDGE_CURVE ( 'NONE', #50218, #16743, #44087, .T. ) ;
#33932 = CARTESIAN_POINT ( 'NONE',  ( 7.635857780409000206, 2.466388272391000225, 6.935562100014999842 ) ) ;
#33933 = LINE ( 'NONE', #22391, #45038 ) ;
#33934 = CARTESIAN_POINT ( 'NONE',  ( 12.30608813017793857, 2.123066299447892824, 12.53144042021393645 ) ) ;
#33935 = ORIENTED_EDGE ( 'NONE', *, *, #46455, .F. ) ;
#33936 = CARTESIAN_POINT ( 'NONE',  ( 25.52466926685099935, 8.322335989133000211, 8.137640611811999491 ) ) ;
#33937 = CARTESIAN_POINT ( 'NONE',  ( 10.51810807141099779, 4.059045408506610109, -8.776647962565998995 ) ) ;
#33938 = CARTESIAN_POINT ( 'NONE',  ( 5.500000000000000000, -0.2500000000000000000, 9.776630298829998011 ) ) ;
#33940 = CARTESIAN_POINT ( 'NONE',  ( 17.86524243499061271, -0.5426972542814749723, 12.68439075057083443 ) ) ;
#33939 = CARTESIAN_POINT ( 'NONE',  ( 7.507480646791999668, -3.501517589953999643, 9.055975309745999624 ) ) ;
#33941 = CARTESIAN_POINT ( 'NONE',  ( 10.21064655415099942, -3.513729974241599940, 6.621146336197599958 ) ) ;
#33942 = CARTESIAN_POINT ( 'NONE',  ( 10.82595391537419971, -3.283439621430300104, -7.986661909549199301 ) ) ;
#33943 = VERTEX_POINT ( 'NONE', #16540 ) ;
#33944 = CARTESIAN_POINT ( 'NONE',  ( 1.067064049866000008, -3.242811033061999915, 1.104080751309999942 ) ) ;
#33945 = CARTESIAN_POINT ( 'NONE',  ( 23.59999467231800097, -10.30760443253999981, -9.317695455237998914 ) ) ;
#33946 = DIRECTION ( 'NONE',  ( -1.000000000000000000, 0.000000000000000000, 0.000000000000000000 ) ) ;
#33947 = CARTESIAN_POINT ( 'NONE',  ( 18.06384107467706102, -2.863137910839477662, 13.58970737937971229 ) ) ;
#33948 = CARTESIAN_POINT ( 'NONE',  ( 24.60170725970500172, -12.45697516994999887, 2.983025822335999777 ) ) ;
#33949 = CARTESIAN_POINT ( 'NONE',  ( 12.33301873031884810, -1.963679441452091723, 13.86160245617593034 ) ) ;
#33950 = CARTESIAN_POINT ( 'NONE',  ( 10.90728308714999883, 2.969488398748000080, 4.935980545376000173 ) ) ;
#33951 = CARTESIAN_POINT ( 'NONE',  ( 17.55505043854147118, -1.875000000000000000, 12.57545641911172396 ) ) ;
#33952 = CARTESIAN_POINT ( 'NONE',  ( 17.55505043854143565, 3.248109929747637903, -13.61799478206225444 ) ) ;
#33953 = EDGE_LOOP ( 'NONE', ( #4405, #41919, #55214 ) ) ;
#33954 = CARTESIAN_POINT ( 'NONE',  ( 10.02790872788999899, 7.656519725853999425, -5.745353671516999938 ) ) ;
#33955 = DIRECTION ( 'NONE',  ( -1.000000000000000000, 0.000000000000000000, 0.000000000000000000 ) ) ;
#33956 = CARTESIAN_POINT ( 'NONE',  ( 7.433267076835290865, -2.295947205248204170, 7.848471278922707128 ) ) ;
#33957 = CIRCLE ( 'NONE', #3792, 1.700000201121000032 ) ;
#33958 = CARTESIAN_POINT ( 'NONE',  ( 17.98179591661178023, -3.334516285427086668, -11.16264808783960305 ) ) ;
#33959 = CARTESIAN_POINT ( 'NONE',  ( 1.800476376745000051, -3.604362431180999859, -1.066289260138999939 ) ) ;
#33960 = VERTEX_POINT ( 'NONE', #37868 ) ;
#33961 = CARTESIAN_POINT ( 'NONE',  ( 12.79999999914999975, 12.11987927271999865, -3.159802730921999814 ) ) ;
#33962 = EDGE_CURVE ( 'NONE', #36930, #50903, #5016, .T. ) ;
#33963 = DIRECTION ( 'NONE',  ( -1.000000000000000000, 0.000000000000000000, 0.000000000000000000 ) ) ;
#33964 = CARTESIAN_POINT ( 'NONE',  ( 10.90638722582999875, 5.227488226180000197, 6.784465725675999259 ) ) ;
#33965 = CARTESIAN_POINT ( 'NONE',  ( 11.36333594839950045, 4.659759757475400832, 8.256087240512899328 ) ) ;
#33966 = CARTESIAN_POINT ( 'NONE',  ( 18.50001572531399674, -0.9783175319534245240, 12.52500000122871526 ) ) ;
#33967 = CARTESIAN_POINT ( 'NONE',  ( 10.72801694037999987, -3.751276547904999870, -8.836912395451999913 ) ) ;
#33968 = CARTESIAN_POINT ( 'NONE',  ( 11.29998901737826955, 3.699024971382844029, -11.75540534549141825 ) ) ;
#33969 = CARTESIAN_POINT ( 'NONE',  ( 12.10941530413763445, -10.98038939419360815, 3.892884065153699336 ) ) ;
#33970 = CARTESIAN_POINT ( 'NONE',  ( 12.19275557201275362, -2.625384353767556078, 12.42149591633707573 ) ) ;
#33971 = B_SPLINE_CURVE_WITH_KNOTS ( 'NONE', 3,
 ( #54325, #27776, #32332, #43151 ),
 .UNSPECIFIED., .F., .F.,
 ( 4, 4 ),
 ( 0.000000000000000000, 1.000000000000000000 ),
 .UNSPECIFIED. ) ;
#33972 = EDGE_LOOP ( 'NONE', ( #59247, #6182, #15544, #36879 ) ) ;
#33973 = CARTESIAN_POINT ( 'NONE',  ( 7.377259056795572256, 2.936797553513828873, 8.875456578139957031 ) ) ;
#33974 = TOROIDAL_SURFACE ( 'NONE', #49635, 13.79999999999999893, 0.2000000000000000111 ) ;
#33975 = ORIENTED_EDGE ( 'NONE', *, *, #53515, .F. ) ;
#33976 = CARTESIAN_POINT ( 'NONE',  ( 18.18010564875750390, -2.481546250174181623, 13.67737493447378938 ) ) ;
#33977 = CARTESIAN_POINT ( 'NONE',  ( 10.83810672858429847, -5.021298157087000114, -6.731711997412900494 ) ) ;
#33978 = EDGE_LOOP ( 'NONE', ( #24447, #58510, #31757, #59965 ) ) ;
#33979 = CARTESIAN_POINT ( 'NONE',  ( 24.99828677809757238, -2.941260336786404306, -11.56306762256811105 ) ) ;
#33980 = CARTESIAN_POINT ( 'NONE',  ( 5.728331222046617377, -0.3264931479727770647, 1.084430188123998828 ) ) ;
#33981 = ADVANCED_FACE ( 'NONE', ( #27382 ), #53940, .T. ) ;
#33983 = DIRECTION ( 'NONE',  ( 0.000000000000000000, 0.9439966912222074180, 0.3299549165591025846 ) ) ;
#33982 = CIRCLE ( 'NONE', #21678, 0.9499999999999999556 ) ;
#33984 = PLANE ( 'NONE',  #27559 ) ;
#33985 = FACE_OUTER_BOUND ( 'NONE', #18048, .T. ) ;
#33986 = DIRECTION ( 'NONE',  ( -1.000000000000000000, 4.460717509654651142E-14, 1.610814656264179684E-14 ) ) ;
#33987 = CARTESIAN_POINT ( 'NONE',  ( 11.80600022547799988, 3.313997181012000137, -11.22408540768999963 ) ) ;
#33988 = CARTESIAN_POINT ( 'NONE',  ( 9.856713838269000050, -4.814118338972999567, -8.929571672388000536 ) ) ;
#33989 = AXIS2_PLACEMENT_3D ( 'NONE', #9869, #26300, #66 ) ;
#33990 = CARTESIAN_POINT ( 'NONE',  ( 11.07503769033409746, 4.268003910470056894, -9.025037683628568175 ) ) ;
#33991 = DIRECTION ( 'NONE',  ( 1.000000000000000000, 0.000000000000000000, 0.000000000000000000 ) ) ;
#33992 = ORIENTED_EDGE ( 'NONE', *, *, #57349, .T. ) ;
#33993 = DIRECTION ( 'NONE',  ( 1.000000000000000000, 0.000000000000000000, 0.000000000000000000 ) ) ;
#33994 =( LENGTH_UNIT ( ) NAMED_UNIT ( * ) SI_UNIT ( .MILLI., .METRE. ) );
#33995 = CARTESIAN_POINT ( 'NONE',  ( 17.55505043854147118, -1.787797342887044172, -13.88538010501570774 ) ) ;
#33996 = CARTESIAN_POINT ( 'NONE',  ( 10.53432647553000123, -4.980255174632999271, 5.071214337227999636 ) ) ;
#33997 = CARTESIAN_POINT ( 'NONE',  ( 5.000015393671500163, -2.571712834666313134E-16, -2.099962892531002545 ) ) ;
#33998 = CARTESIAN_POINT ( 'NONE',  ( 10.34292546752099895, 2.723846966067000164, -7.411581555133209598 ) ) ;
#33999 = CARTESIAN_POINT ( 'NONE',  ( 12.55438499206305458, 1.927376109800345905, 13.77831414012769251 ) ) ;
#34000 = B_SPLINE_SURFACE_WITH_KNOTS ( 'NONE', 3, 3, ( 
 ( #27926, #49236, #22663, #7627 ),
 ( #28973, #18468, #29664, #13234 ),
 ( #28621, #34560, #39794, #50281 ),
 ( #17782, #28266, #44705, #7282 ) ),
 .UNSPECIFIED., .F., .F., .F.,
 ( 4, 4 ),
 ( 4, 4 ),
 ( -0.01349945606786999951, 0.08053609420915000539 ),
 ( -0.0005287450254680999126, 0.02696599629895000266 ),
 .UNSPECIFIED. ) ;
#34001 = CARTESIAN_POINT ( 'NONE',  ( 10.61382642076999971, -3.385081736013999976, 5.849525238167000651 ) ) ;
#34003 = ORIENTED_EDGE ( 'NONE', *, *, #31405, .T. ) ;
#34002 = B_SPLINE_CURVE_WITH_KNOTS ( 'NONE', 3,
 ( #21340, #16436, #27285, #42670, #43012, #37421 ),
 .UNSPECIFIED., .F., .F.,
 ( 4, 1, 1, 4 ),
 ( 0.000000000000000000, 0.1550125217837789171, 0.7488612475957610037, 1.000000000000000000 ),
 .UNSPECIFIED. ) ;
#34004 = CARTESIAN_POINT ( 'NONE',  ( 7.849093588702794833, 2.941815248762500890, -6.601834848426078040 ) ) ;
#34005 = CARTESIAN_POINT ( 'NONE',  ( 12.08612513405892841, 0.09509187666555039831, 13.99968209810982600 ) ) ;
#34006 = VERTEX_POINT ( 'NONE', #11632 ) ;
#34007 = CYLINDRICAL_SURFACE ( 'NONE', #37624, 3.500000000000000000 ) ;
#34008 = CARTESIAN_POINT ( 'NONE',  ( 5.500000000000000000, -1.300000000000000044, 9.662944685757000940 ) ) ;
#34009 = CARTESIAN_POINT ( 'NONE',  ( 24.33638798420900073, -3.364639815177999704, -12.26716122899000005 ) ) ;
#34010 = CARTESIAN_POINT ( 'NONE',  ( 4.636664736434999767, -1.451451435390000100, -0.7411915970320999136 ) ) ;
#34011 = AXIS2_PLACEMENT_3D ( 'NONE', #62382, #8561, #36157 ) ;
#34012 = B_SPLINE_SURFACE_WITH_KNOTS ( 'NONE', 3, 3, ( 
 ( #38655, #37961, #6487, #60328 ),
 ( #21533, #22224, #48803, #16289 ),
 ( #65211, #38304, #27479, #43210 ),
 ( #21875, #7188, #54737, #58944 ),
 ( #59281, #48456, #565, #32387 ),
 ( #33071, #53700, #22567, #12435 ) ),
 .UNSPECIFIED., .F., .F., .F.,
 ( 4, 1, 1, 4 ),
 ( 4, 4 ),
 ( 0.1811037619699999990, 0.3333333333333000081, 0.6666666666667000474, 0.8725156331704999602 ),
 ( -0.1256563615239000009, 1.125656361510000147 ),
 .UNSPECIFIED. ) ;
#34013 = CARTESIAN_POINT ( 'NONE',  ( 9.327795280414001411, 3.161445734422999809, -6.178649910536000434 ) ) ;
#34014 = CYLINDRICAL_SURFACE ( 'NONE', #50340, 1.350000000000000089 ) ;
#34015 = CARTESIAN_POINT ( 'NONE',  ( 9.593930206849998754, 5.250000000000000000, 7.500000000000000000 ) ) ;
#34016 = EDGE_CURVE ( 'NONE', #32335, #42555, #32973, .T. ) ;
#34017 = ADVANCED_FACE ( 'NONE', ( #47680 ), #44167, .F. ) ;
#34018 = DIRECTION ( 'NONE',  ( 0.000000000000000000, 1.000000000000000000, 0.000000000000000000 ) ) ;
#34019 = CARTESIAN_POINT ( 'NONE',  ( 18.30017264560542145, 0.9191760154459583942, -11.85014035451979630 ) ) ;
#34020 = DIRECTION ( 'NONE',  ( 0.000000000000000000, -0.9659258262890756397, 0.2588190451024934280 ) ) ;
#34021 = CARTESIAN_POINT ( 'NONE',  ( 9.837330429757999539, -5.176458967229000230, -8.738385553646999426 ) ) ;
#34022 = EDGE_CURVE ( 'NONE', #38686, #46374, #6912, .T. ) ;
#34023 = EDGE_CURVE ( 'NONE', #37068, #11162, #47500, .T. ) ;
#34024 = CARTESIAN_POINT ( 'NONE',  ( 11.58902763632552002, 3.213494089586499847, -7.137085349939700230 ) ) ;
#34025 = CARTESIAN_POINT ( 'NONE',  ( 1.178056799208624827, -2.150913519912214245, 2.798833948393621984 ) ) ;
#34026 = CARTESIAN_POINT ( 'NONE',  ( 11.60477869730532774, 3.532552483170099844, -6.578238193496799724 ) ) ;
#34027 = CARTESIAN_POINT ( 'NONE',  ( 8.697480666858998788, 4.334888990546500231, -8.446938520915798776 ) ) ;
#34029 = CARTESIAN_POINT ( 'NONE',  ( 10.41599335357999934, -3.102203969901999869, 5.040281075867000027 ) ) ;
#34028 = CARTESIAN_POINT ( 'NONE',  ( 10.38096314287999888, -3.151633609938700342, 7.678836273503299559 ) ) ;
#34030 = CARTESIAN_POINT ( 'NONE',  ( 11.22726354018300121, -3.370476274536371442, 8.592232985442818105 ) ) ;
#34031 = ORIENTED_EDGE ( 'NONE', *, *, #9596, .F. ) ;
#34032 = B_SPLINE_CURVE_WITH_KNOTS ( 'NONE', 3,
 ( #30233, #30565, #41402, #24289 ),
 .UNSPECIFIED., .F., .F.,
 ( 4, 4 ),
 ( 0.000000000000000000, 1.000000000000000000 ),
 .UNSPECIFIED. ) ;
#34033 = CARTESIAN_POINT ( 'NONE',  ( 11.43345123989529810, 4.540230239159599890, 6.456682674800999777 ) ) ;
#34034 = AXIS2_PLACEMENT_3D ( 'NONE', #32767, #54081, #6177 ) ;
#34035 = CARTESIAN_POINT ( 'NONE',  ( 10.46933016578999975, -4.988498232033999891, 6.213103211926000569 ) ) ;
#34036 = CARTESIAN_POINT ( 'NONE',  ( 9.705671671056999017, 3.009461603020800347, 7.333638993632098924 ) ) ;
#34037 = CARTESIAN_POINT ( 'NONE',  ( 9.404204162135625822, 4.790364090350968773, -7.124690962532754135 ) ) ;
#34038 = CARTESIAN_POINT ( 'NONE',  ( 9.476374593785998002, -5.098398394707999159, 6.305533045879999854 ) ) ;
#34039 = CARTESIAN_POINT ( 'NONE',  ( 24.30001696810800027, 12.21047201856000086, 3.271805692349999628 ) ) ;
#34040 = CARTESIAN_POINT ( 'NONE',  ( 10.46684687351657672, 3.231816600031355069, 6.500416447002276499 ) ) ;
#34041 = EDGE_LOOP ( 'NONE', ( #59663, #52286, #29250, #18054 ) ) ;
#34042 = B_SPLINE_CURVE_WITH_KNOTS ( 'NONE', 3,
 ( #44690, #5876, #17054, #59712 ),
 .UNSPECIFIED., .F., .F.,
 ( 4, 4 ),
 ( 0.000000000000000000, 1.000000000000000000 ),
 .UNSPECIFIED. ) ;
#34043 = CARTESIAN_POINT ( 'NONE',  ( 10.03992546752099990, -5.002009261081000524, -7.430575645513339822 ) ) ;
#34044 = CARTESIAN_POINT ( 'NONE',  ( 8.731616107288068918, 4.000002263255225898, 6.618420992905501343 ) ) ;
#34045 = CARTESIAN_POINT ( 'NONE',  ( 6.427664783001999282, 0.8895447933473999980, 1.347595971237000256 ) ) ;
#34046 = CARTESIAN_POINT ( 'NONE',  ( 10.55333291544900121, -3.468906853242414989, 6.341063066638221279 ) ) ;
#34047 = CARTESIAN_POINT ( 'NONE',  ( 24.39664882158933423, -3.240506423573137784, 12.09373461503223091 ) ) ;
#34048 = CARTESIAN_POINT ( 'NONE',  ( 11.28949010443639978, 5.000675062740000065, -7.574834962826040297 ) ) ;
#34049 = DIRECTION ( 'NONE',  ( -1.000000000000000000, 0.000000000000000000, 0.000000000000000000 ) ) ;
#34050 = CARTESIAN_POINT ( 'NONE',  ( 9.260142521132999960, -3.283392111224999965, -8.676955243274001361 ) ) ;
#34051 = CARTESIAN_POINT ( 'NONE',  ( 25.52344634951100133, 11.21071681617999971, 3.136836603414999924 ) ) ;
#34052 = VERTEX_POINT ( 'NONE', #34709 ) ;
#34053 = CARTESIAN_POINT ( 'NONE',  ( 10.02052890782000105, -2.899999999999999911, 6.152188490330000370 ) ) ;
#34054 = CARTESIAN_POINT ( 'NONE',  ( 12.08006676141314983, 0.02431279293012172937, -13.99999914078080110 ) ) ;
#34055 = DIRECTION ( 'NONE',  ( 0.000000000000000000, 1.000000000000000000, 0.000000000000000000 ) ) ;
#34056 = CARTESIAN_POINT ( 'NONE',  ( 24.46218697145600274, -8.785835042869001299, -8.709278711906000225 ) ) ;
#34057 = CARTESIAN_POINT ( 'NONE',  ( 4.900006121741999010, 0.5234957687185600728, -1.947945353336631102 ) ) ;
#34058 = DIRECTION ( 'NONE',  ( -1.000000000000000000, 0.000000000000000000, 0.000000000000000000 ) ) ;
#34059 = CARTESIAN_POINT ( 'NONE',  ( 13.46005557146100173, 12.04952288628000012, 2.412084176363999966 ) ) ;
#34060 = ORIENTED_EDGE ( 'NONE', *, *, #17050, .T. ) ;
#34061 = CARTESIAN_POINT ( 'NONE',  ( 18.17249645628715626, 2.401006805677767808, -13.69397427989633620 ) ) ;
#34062 = ORIENTED_EDGE ( 'NONE', *, *, #66295, .F. ) ;
#34063 = CARTESIAN_POINT ( 'NONE',  ( 11.46021572556888657, -5.045751188959975764, -7.175002613693187925 ) ) ;
#34064 = CARTESIAN_POINT ( 'NONE',  ( 8.930995559624999913, -2.019079883662000086, 7.390983468784999566 ) ) ;
#34065 = ADVANCED_FACE ( 'NONE', ( #7783 ), #39254, .T. ) ;
#34066 = CARTESIAN_POINT ( 'NONE',  ( 8.356920280409999791, 4.851303550474000303, -9.008742670124000540 ) ) ;
#34067 = CARTESIAN_POINT ( 'NONE',  ( 13.55370778485685435, -9.344737785247383854, -8.032732227356667920 ) ) ;
#34068 = CARTESIAN_POINT ( 'NONE',  ( 10.52314899745999988, -5.167567567567999731, -6.822293592207000934 ) ) ;
#34069 = FACE_OUTER_BOUND ( 'NONE', #21524, .T. ) ;
#34070 = ADVANCED_FACE ( 'NONE', ( #17587 ), #13387, .F. ) ;
#34071 = CARTESIAN_POINT ( 'NONE',  ( 10.21684687351566723, -3.231816600031351516, 8.499583552997721725 ) ) ;
#34072 = ORIENTED_EDGE ( 'NONE', *, *, #68903, .F. ) ;
#34073 = CARTESIAN_POINT ( 'NONE',  ( 11.06924082387999952, -5.425685649895999774, 8.012912555523998392 ) ) ;
#34074 = CYLINDRICAL_SURFACE ( 'NONE', #50739, 1.000000000000000444 ) ;
#34075 = CARTESIAN_POINT ( 'NONE',  ( 25.59994555223700274, -10.09686240769118903, 5.033199831113347678 ) ) ;
#34076 = VERTEX_POINT ( 'NONE', #18279 ) ;
#34077 = CARTESIAN_POINT ( 'NONE',  ( 10.84087666499999969, 2.636288985756999992, -7.512643730465999425 ) ) ;
#34078 = B_SPLINE_CURVE_WITH_KNOTS ( 'NONE', 3,
 ( #54689, #1209, #43860, #13087 ),
 .UNSPECIFIED., .F., .F.,
 ( 4, 4 ),
 ( 0.000000000000000000, 1.000000000000000000 ),
 .UNSPECIFIED. ) ;
#34079 = CARTESIAN_POINT ( 'NONE',  ( 9.957462135714001406, -5.100000000000000533, -6.571291218949999902 ) ) ;
#34080 = VERTEX_POINT ( 'NONE', #12338 ) ;
#34081 = CARTESIAN_POINT ( 'NONE',  ( 9.735975701333000387, 4.736880367605900588, 6.817468224793199916 ) ) ;
#34082 = CARTESIAN_POINT ( 'NONE',  ( 18.08778676580602607, -1.991706414748710463, -12.44159931028328181 ) ) ;
#34083 = CARTESIAN_POINT ( 'NONE',  ( 10.85685100254000091, 2.832432432432000269, -6.822293592207000934 ) ) ;
#34084 = DIRECTION ( 'NONE',  ( 1.000000000000000000, 0.000000000000000000, 0.000000000000000000 ) ) ;
#34085 = FACE_BOUND ( 'NONE', #46385, .T. ) ;
#34086 = CARTESIAN_POINT ( 'NONE',  ( 9.963938025973998691, 3.477805217445600228, 8.357994702431799539 ) ) ;
#34087 = CARTESIAN_POINT ( 'NONE',  ( 6.748939170459999914, -9.313044101531000152, -5.427197938553000256 ) ) ;
#34088 = VERTEX_POINT ( 'NONE', #50429 ) ;
#34089 = CARTESIAN_POINT ( 'NONE',  ( 9.428197172113266689, 5.125396288426561142, 6.749639981083131346 ) ) ;
#34090 = CARTESIAN_POINT ( 'NONE',  ( 10.44812028041000040, 5.235600787608000850, -6.609970743661000903 ) ) ;
#34091 = CARTESIAN_POINT ( 'NONE',  ( 10.89034309416000035, -5.058758371668000464, -5.035645192038000317 ) ) ;
#34092 = CARTESIAN_POINT ( 'NONE',  ( 12.28091743413948578, 2.013400871504815282, -13.85446832019263397 ) ) ;
#34093 = CARTESIAN_POINT ( 'NONE',  ( 11.33351354018309998, -5.249999999999999112, 7.663624617374471093 ) ) ;
#34094 = CARTESIAN_POINT ( 'NONE',  ( 25.19548756823600399, 3.342128045641000078, 11.59777824541000157 ) ) ;
#34095 = CARTESIAN_POINT ( 'NONE',  ( 17.91891929415153228, 0.5082612142235592989, 13.88749228919890122 ) ) ;
#34096 = CARTESIAN_POINT ( 'NONE',  ( 24.63779836814899937, -3.092549035221999976, 11.81391394322000110 ) ) ;
#34097 = EDGE_CURVE ( 'NONE', #32203, #68795, #42649, .T. ) ;
#34098 = ORIENTED_EDGE ( 'NONE', *, *, #4184, .T. ) ;
#34099 = ORIENTED_EDGE ( 'NONE', *, *, #9007, .F. ) ;
#34100 = CARTESIAN_POINT ( 'NONE',  ( 9.246064158776000852, 5.200883864107000321, -6.027780766890000308 ) ) ;
#34101 = CARTESIAN_POINT ( 'NONE',  ( 9.129428851719998406, 5.099284414202999827, 6.151604790022999758 ) ) ;
#34102 = EDGE_CURVE ( 'NONE', #12282, #12604, #63252, .T. ) ;
#34103 = CIRCLE ( 'NONE', #41922, 1.825000327749000117 ) ;
#34104 = ADVANCED_FACE ( 'NONE', ( #33671 ), #54989, .F. ) ;
#34105 = CARTESIAN_POINT ( 'NONE',  ( 12.19034750719213278, -2.613044105505787584, 13.64883414299444198 ) ) ;
#34106 = FACE_OUTER_BOUND ( 'NONE', #32983, .T. ) ;
#34107 = CARTESIAN_POINT ( 'NONE',  ( 8.962745559623000347, -5.445226602819000838, 7.703375344019999460 ) ) ;
#34108 = CYLINDRICAL_SURFACE ( 'NONE', #49411, 1.250000000000000222 ) ;
#34110 = CARTESIAN_POINT ( 'NONE',  ( 5.399998535875000449, 6.217248937900999058E-14, 3.708144902247999495E-14 ) ) ;
#34109 = CARTESIAN_POINT ( 'NONE',  ( 10.94424205625099944, -4.458751122174599679, 6.305876158747000026 ) ) ;
#34111 = CARTESIAN_POINT ( 'NONE',  ( 11.03502897915239878, 4.327133900127000388, -8.735435061820998826 ) ) ;
#34112 = ORIENTED_EDGE ( 'NONE', *, *, #18790, .F. ) ;
#34113 = CARTESIAN_POINT ( 'NONE',  ( 7.564999999998999414, 5.349999999999999645, -7.500000000000000000 ) ) ;
#34114 = CARTESIAN_POINT ( 'NONE',  ( 8.126014158770999529, 5.189036231907000030, -8.048606212067999977 ) ) ;
#34115 = CARTESIAN_POINT ( 'NONE',  ( 9.361802827890667089, 2.874603711572071951, -6.749639981085484131 ) ) ;
#34116 = CARTESIAN_POINT ( 'NONE',  ( 11.09999999999999964, 5.538898460221000519, 7.685179721164000277 ) ) ;
#34117 = CARTESIAN_POINT ( 'NONE',  ( 12.46489138696793475, -0.5244033890137438370, 12.68542455843550343 ) ) ;
#34118 = CARTESIAN_POINT ( 'NONE',  ( 18.09718405123029328, -2.811158313956393151, -12.37360767970495701 ) ) ;
#34119 = ORIENTED_EDGE ( 'NONE', *, *, #4267, .T. ) ;
#34121 = CARTESIAN_POINT ( 'NONE',  ( 12.35578833716350822, -1.907710147612963203, -12.45493153468922287 ) ) ;
#34120 = CARTESIAN_POINT ( 'NONE',  ( 10.88867070183947483, 5.215510510159838020, 6.904563811839100396 ) ) ;
#34122 = CARTESIAN_POINT ( 'NONE',  ( 9.111654719595000174, 4.989193221215000307, -6.287302145481000082 ) ) ;
#34123 = CARTESIAN_POINT ( 'NONE',  ( 8.580795537699431819, 5.100000000000000533, -6.662590550605527184 ) ) ;
#34124 = EDGE_CURVE ( 'NONE', #1057, #65964, #28427, .T. ) ;
#34125 = CARTESIAN_POINT ( 'NONE',  ( 10.61656919669529842, 5.225637333137999718, 7.137881914002699446 ) ) ;
#34126 = CARTESIAN_POINT ( 'NONE',  ( 13.56683625432858342, -9.108504156368539384, -7.475700167246311700 ) ) ;
#34127 = AXIS2_PLACEMENT_3D ( 'NONE', #26274, #68908, #41321 ) ;
#34128 = CARTESIAN_POINT ( 'NONE',  ( 8.203568157088000135, 3.399999998409999780, 6.139678131101000247 ) ) ;
#34129 = CARTESIAN_POINT ( 'NONE',  ( 3.262839944555000038, -0.8785454485268000546, 3.483102888041999634 ) ) ;
#34130 = EDGE_LOOP ( 'NONE', ( #2481, #1726, #18444, #15356 ) ) ;
#34131 = CARTESIAN_POINT ( 'NONE',  ( 12.23732871802942590, -0.4475098806653898253, -12.59205372277267720 ) ) ;
#34132 = B_SPLINE_CURVE_WITH_KNOTS ( 'NONE', 3,
 ( #14584, #61101, #24383, #45714 ),
 .UNSPECIFIED., .F., .F.,
 ( 4, 4 ),
 ( 0.000000000000000000, 1.000000000000000000 ),
 .UNSPECIFIED. ) ;
#34133 = DIRECTION ( 'NONE',  ( 0.000000000000000000, 1.000000000000000000, 0.000000000000000000 ) ) ;
#34134 = CARTESIAN_POINT ( 'NONE',  ( 20.10000000000000142, 0.000000000000000000, 0.000000000000000000 ) ) ;
#34135 = CARTESIAN_POINT ( 'NONE',  ( 8.539829719592999524, 5.633477595780999714, 7.451234169193000412 ) ) ;
#34136 = ORIENTED_EDGE ( 'NONE', *, *, #36263, .F. ) ;
#34137 = CARTESIAN_POINT ( 'NONE',  ( 5.773748128158000092, 0.07142731211511998968, 1.320368930804000085 ) ) ;
#34138 = CARTESIAN_POINT ( 'NONE',  ( 10.95521427414540128, 9.021152868672782432, 6.404909939993181034 ) ) ;
#34140 = CARTESIAN_POINT ( 'NONE',  ( 10.73165287102628085, 3.320185038362386098, -8.679412628036420330 ) ) ;
#34139 = DIRECTION ( 'NONE',  ( -1.000000000000000000, 0.000000000000000000, 0.000000000000000000 ) ) ;
#34141 = CARTESIAN_POINT ( 'NONE',  ( 10.57529832096847677, -4.746004694577873551, -7.044405226132214537 ) ) ;
#34142 = ORIENTED_EDGE ( 'NONE', *, *, #9887, .T. ) ;
#34143 = DIRECTION ( 'NONE',  ( 0.000000000000000000, 1.000000000000000000, 0.000000000000000000 ) ) ;
#34144 = ORIENTED_EDGE ( 'NONE', *, *, #19336, .F. ) ;
#34145 = CARTESIAN_POINT ( 'NONE',  ( 9.464432710331807996, -5.182476493413302521, 8.153247799998663226 ) ) ;
#34146 = CARTESIAN_POINT ( 'NONE',  ( 10.31746213571000048, -5.100000000000000533, 6.571291218949999902 ) ) ;
#34147 = CARTESIAN_POINT ( 'NONE',  ( 18.27397574302396777, 0.09509187666554888563, -13.99968209810982067 ) ) ;
#34148 = VERTEX_POINT ( 'NONE', #13037 ) ;
#34149 = CARTESIAN_POINT ( 'NONE',  ( 10.92633922843239169, 9.535098715412203774, -6.046881589190145512 ) ) ;
#34150 = CARTESIAN_POINT ( 'NONE',  ( 8.270987821524766304, 2.867662864822190016, 6.761597825165790887 ) ) ;
#34151 = CARTESIAN_POINT ( 'NONE',  ( 10.90000154029999990, 0.000000000000000000, 0.000000000000000000 ) ) ;
#34152 = ADVANCED_FACE ( 'NONE', ( #2532 ), #1501, .F. ) ;
#34153 = CARTESIAN_POINT ( 'NONE',  ( 9.629282595918656540, -2.750056606219161370, 7.269976573734650671 ) ) ;
#34154 = CARTESIAN_POINT ( 'NONE',  ( 18.18005043817898425, -2.519674554510558107, 12.44700836740716277 ) ) ;
#34155 = VERTEX_POINT ( 'NONE', #23860 ) ;
#34156 = LINE ( 'NONE', #50229, #34339 ) ;
#34157 = CARTESIAN_POINT ( 'NONE',  ( 23.64816398247700135, -13.35748263717000128, -3.865423979300999680 ) ) ;
#34158 = DIRECTION ( 'NONE',  ( 0.000000000000000000, -1.000000000000000000, 0.000000000000000000 ) ) ;
#34159 = CARTESIAN_POINT ( 'NONE',  ( 12.56936319536957214, -3.210092459286436828, 13.62701963584217957 ) ) ;
#34160 = B_SPLINE_CURVE_WITH_KNOTS ( 'NONE', 3,
 ( #43400, #60507, #37799, #59122 ),
 .UNSPECIFIED., .F., .F.,
 ( 4, 4 ),
 ( 0.000000000000000000, 1.000000000000000000 ),
 .UNSPECIFIED. ) ;
#34161 = EDGE_LOOP ( 'NONE', ( #31382, #50743, #23386, #44707, #26664, #10980, #8806 ) ) ;
#34162 = CARTESIAN_POINT ( 'NONE',  ( 10.68864842108893498, -2.651255354521660834, 7.268672825006785132 ) ) ;
#34163 = VECTOR ( 'NONE', #26711, 999.9999999999998863 ) ;
#34164 = CARTESIAN_POINT ( 'NONE',  ( 0.1744510438295829302, -0.5461907802877905560, -3.174431049355146861 ) ) ;
#34165 = CARTESIAN_POINT ( 'NONE',  ( 8.038072165043022466, 2.528277501517397940, -8.632724327209173154 ) ) ;
#34166 = CARTESIAN_POINT ( 'NONE',  ( 24.54174074851610143, 12.46120270712776090, -3.023779783529694676 ) ) ;
#34167 = CARTESIAN_POINT ( 'NONE',  ( 12.75695018768104028, -1.789009927756594953, -13.88522413357867258 ) ) ;
#34168 = CARTESIAN_POINT ( 'NONE',  ( 5.857109839684125241, 1.199500263597268246, 0.9218200799623752495 ) ) ;
#34169 = CARTESIAN_POINT ( 'NONE',  ( 17.82442946238797887, -1.812220263014551858, 12.46899672597967523 ) ) ;
#34170 = ORIENTED_EDGE ( 'NONE', *, *, #9073, .F. ) ;
#34171 = CARTESIAN_POINT ( 'NONE',  ( 10.89324174884020024, -4.032306468273969990, -8.674442868902998427 ) ) ;
#34172 = ORIENTED_EDGE ( 'NONE', *, *, #24948, .T. ) ;
#34173 = B_SPLINE_CURVE_WITH_KNOTS ( 'NONE', 3,
 ( #32617, #52905, #5003, #26688 ),
 .UNSPECIFIED., .F., .F.,
 ( 4, 4 ),
 ( 0.000000000000000000, 0.1253969396550571880 ),
 .UNSPECIFIED. ) ;
#34174 = CARTESIAN_POINT ( 'NONE',  ( 0.1499942179679999710, -1.384928887584818469, 2.402872127494066756 ) ) ;
#34175 = AXIS2_PLACEMENT_3D ( 'NONE', #24989, #62392, #14507 ) ;
#34176 = CARTESIAN_POINT ( 'NONE',  ( 9.236820887142258130, -4.253281749927232624, 6.641515014115457305 ) ) ;
#34177 = CARTESIAN_POINT ( 'NONE',  ( 2.370651199330000125, 0.2798869272278999842, 3.202845242003000248 ) ) ;
#34178 = CARTESIAN_POINT ( 'NONE',  ( 10.34225158793000077, -3.348983461003999906, -8.881464249475000017 ) ) ;
#34179 = AXIS2_PLACEMENT_3D ( 'NONE', #69063, #35874, #5433 ) ;
#34180 = DIRECTION ( 'NONE',  ( 0.000000000000000000, 1.000000000000000000, 0.000000000000000000 ) ) ;
#34181 = CARTESIAN_POINT ( 'NONE',  ( 24.21983515806600096, 12.94789048768999962, 3.132737188682000351 ) ) ;
#34182 = CARTESIAN_POINT ( 'NONE',  ( 11.09999999999999964, -2.649999999999999911, 7.500000000000000000 ) ) ;
#34183 = VERTEX_POINT ( 'NONE', #56021 ) ;
#34184 = CARTESIAN_POINT ( 'NONE',  ( 10.16000000000000014, -4.496968146123999865, -8.755198255949000696 ) ) ;
#34185 = ADVANCED_FACE ( 'NONE', ( #27738 ), #65810, .F. ) ;
#34186 = CARTESIAN_POINT ( 'NONE',  ( 12.28179573085659904, -3.026866171144600326, 7.331616337578100051 ) ) ;
#34187 = CARTESIAN_POINT ( 'NONE',  ( 10.46932803217000085, 4.988495740890000363, 6.213106455073000411 ) ) ;
#34188 = EDGE_CURVE ( 'NONE', #40775, #61047, #4061, .T. ) ;
#34189 = CARTESIAN_POINT ( 'NONE',  ( 10.72963504510672195, -4.176677120266497845, -8.849854844400173448 ) ) ;
#34190 = CARTESIAN_POINT ( 'NONE',  ( 18.36682228790375859, -2.717338739979838547, 11.46589211741050285 ) ) ;
#34191 = CARTESIAN_POINT ( 'NONE',  ( 11.04752711762115780, -2.837609288610280167, -7.824990536777686856 ) ) ;
#34192 = CARTESIAN_POINT ( 'NONE',  ( 11.68333460557258796, 4.162011815820000571, -8.490304555719900392 ) ) ;
#34193 = CARTESIAN_POINT ( 'NONE',  ( 25.55305567154783475, -2.866385917523393001, -11.19763132080514367 ) ) ;
#34194 = CARTESIAN_POINT ( 'NONE',  ( 9.251759580228998914, 2.889471124893000287, -7.234556850645999404 ) ) ;
#34195 = CARTESIAN_POINT ( 'NONE',  ( 23.51695514933100029, -10.50652978964999917, 9.451976498271999816 ) ) ;
#34196 = CARTESIAN_POINT ( 'NONE',  ( 0.9319208874357501893, 2.278816592008448882, -2.686138227945438217 ) ) ;
#34197 = CARTESIAN_POINT ( 'NONE',  ( 11.25809834123000108, 3.275514549383000240, -8.650774600386998969 ) ) ;
#34198 = ORIENTED_EDGE ( 'NONE', *, *, #65365, .T. ) ;
#34199 = CARTESIAN_POINT ( 'NONE',  ( 9.041941940379999210, -2.707994276285999646, 5.994456121676999594 ) ) ;
#34200 = CARTESIAN_POINT ( 'NONE',  ( 17.57920283571456110, 1.787797991197233038, 13.88537998700429554 ) ) ;
#34201 = EDGE_CURVE ( 'NONE', #9091, #20205, #54977, .T. ) ;
#34202 = CARTESIAN_POINT ( 'NONE',  ( 24.35365242081700288, -2.582848009804000533, 11.10541636511000085 ) ) ;
#34203 = CARTESIAN_POINT ( 'NONE',  ( 11.18272066707849888, -2.906477115133000222, -6.838543969064300398 ) ) ;
#34204 = ORIENTED_EDGE ( 'NONE', *, *, #10811, .F. ) ;
#34205 = B_SPLINE_CURVE_WITH_KNOTS ( 'NONE', 3,
 ( #32350, #49802, #40341, #2931, #56074, #44576, #8528, #61325, #24259, #12745, #1909, #44228, #40010, #50150, #34765, #2255, #38972, #23569 ),
 .UNSPECIFIED., .F., .F.,
 ( 4, 2, 2, 2, 2, 2, 2, 2, 4 ),
 ( 0.5009155270902391210, 0.5633010862039588007, 0.5944938657608188626, 0.6256866453176790355, 0.6568794248745390973, 0.6880722044313991592, 0.7504577635451192830, 0.8752288817725597525, 1.000000000000000000 ),
 .UNSPECIFIED. ) ;
#34206 = EDGE_CURVE ( 'NONE', #42155, #32256, #16984, .T. ) ;
#34207 = CARTESIAN_POINT ( 'NONE',  ( 7.101301658771000724, 3.554857159507999853, 8.889479859586000288 ) ) ;
#34208 = VECTOR ( 'NONE', #68770, 1000.000000000000000 ) ;
#34210 = CARTESIAN_POINT ( 'NONE',  ( 0.7179470766575658525, -1.805094916197470312, 3.044603405180807965 ) ) ;
#34209 = CARTESIAN_POINT ( 'NONE',  ( 8.795585841232000490, 5.251032986819000214, -6.070151079272999795 ) ) ;
#34211 = CARTESIAN_POINT ( 'NONE',  ( 21.10000000000000142, 0.000000000000000000, 0.000000000000000000 ) ) ;
#34212 = EDGE_LOOP ( 'NONE', ( #50932, #60843, #9724, #65173, #48918 ) ) ;
#34213 = CARTESIAN_POINT ( 'NONE',  ( 10.00122429346999908, 2.274087081648999753, 7.851326250696001097 ) ) ;
#34214 = FACE_OUTER_BOUND ( 'NONE', #53461, .T. ) ;
#34215 = CARTESIAN_POINT ( 'NONE',  ( 10.34995525820099971, 3.892289273474800471, 8.635644537520001052 ) ) ;
#34216 = CARTESIAN_POINT ( 'NONE',  ( 9.388626433405999450, -4.079401915682999480, 9.259353168384000909 ) ) ;
#34217 = DIRECTION ( 'NONE',  ( 0.000000000000000000, -1.000000000000000000, 0.000000000000000000 ) ) ;
#34218 = ORIENTED_EDGE ( 'NONE', *, *, #56516, .F. ) ;
#34219 = DIRECTION ( 'NONE',  ( 1.000000000000000000, 0.000000000000000000, 0.000000000000000000 ) ) ;
#34220 = CARTESIAN_POINT ( 'NONE',  ( 1.459306799207500172, 3.058252359239905793, -1.762666431298143488 ) ) ;
#34221 = CARTESIAN_POINT ( 'NONE',  ( 7.998638406009124679, -2.569044558284087731, 6.497043829224429246 ) ) ;
#34222 = CARTESIAN_POINT ( 'NONE',  ( 9.662553763536999796, -4.094830574823999925, 9.119950378356000087 ) ) ;
#34224 = CARTESIAN_POINT ( 'NONE',  ( 11.63611496860034933, -2.828587461987000395, -6.899705789500199415 ) ) ;
#34223 = CIRCLE ( 'NONE', #63184, 1.000000000000000000 ) ;
#34225 = CARTESIAN_POINT ( 'NONE',  ( 9.602747021775998704, -4.754947163618299832, 6.837506920432799618 ) ) ;
#34226 = ORIENTED_EDGE ( 'NONE', *, *, #9246, .F. ) ;
#34227 = CARTESIAN_POINT ( 'NONE',  ( 24.57709178557182383, -11.91258736157513098, -3.191969742968967516 ) ) ;
#34228 = CARTESIAN_POINT ( 'NONE',  ( 12.10118044953561878, -2.866798846279000390, 6.909094663619399945 ) ) ;
#34229 = ORIENTED_EDGE ( 'NONE', *, *, #28179, .T. ) ;
#34230 = CARTESIAN_POINT ( 'NONE',  ( 9.314928906318884927, 2.650140463285438397, -7.499996151983930659 ) ) ;
#34231 = ORIENTED_EDGE ( 'NONE', *, *, #41790, .F. ) ;
#34232 = CARTESIAN_POINT ( 'NONE',  ( 9.619730517102000888, -2.477793449086000077, -8.275032865112999403 ) ) ;
#34233 = CARTESIAN_POINT ( 'NONE',  ( 8.655270280412999284, 4.162493982103000256, -5.775210092227999858 ) ) ;
#34234 = CARTESIAN_POINT ( 'NONE',  ( 10.68035971519489813, 4.678140486081599825, -6.371865185335000348 ) ) ;
#34235 = FACE_OUTER_BOUND ( 'NONE', #68779, .T. ) ;
#34236 = CARTESIAN_POINT ( 'NONE',  ( 12.25790434794250494, 2.952613167459276156, -12.24916959777017134 ) ) ;
#34237 = CARTESIAN_POINT ( 'NONE',  ( 10.95257053952200010, -4.394359323863099576, 8.422730500489899796 ) ) ;
#34238 = CARTESIAN_POINT ( 'NONE',  ( 11.61123293495519881, -4.891405920092699589, 7.535834283667469435 ) ) ;
#34239 = ORIENTED_EDGE ( 'NONE', *, *, #35465, .T. ) ;
#34240 = DIRECTION ( 'NONE',  ( 0.000000000000000000, -1.000000000000000000, 0.000000000000000000 ) ) ;
#34241 = ORIENTED_EDGE ( 'NONE', *, *, #27708, .F. ) ;
#34242 = CARTESIAN_POINT ( 'NONE',  ( 8.572269353210000276, -2.606998386752999775, 6.345764833140000505 ) ) ;
#34243 = DIRECTION ( 'NONE',  ( 0.000000000000000000, 0.000000000000000000, -1.000000000000000000 ) ) ;
#34244 = VERTEX_POINT ( 'NONE', #9148 ) ;
#34245 = CARTESIAN_POINT ( 'NONE',  ( 12.14231515301104736, -2.188169521966901065, -12.40854677421460295 ) ) ;
#34246 = CARTESIAN_POINT ( 'NONE',  ( 10.86687616594229944, 3.655053560864600204, 8.587337146608000182 ) ) ;
#34247 = PRODUCT_RELATED_PRODUCT_CATEGORY ( 'part', '', ( #50578 ) ) ;
#34248 = CARTESIAN_POINT ( 'NONE',  ( 10.91060805961999947, -4.702347118766000200, -9.210032991522000501 ) ) ;
#34249 = CARTESIAN_POINT ( 'NONE',  ( 6.308905548400004726, 8.386554649686992491, -3.907920053779999847 ) ) ;
#34250 = CARTESIAN_POINT ( 'NONE',  ( 17.90248731685900196, -11.51619295222000083, 4.775850843141999924 ) ) ;
#34251 = CARTESIAN_POINT ( 'NONE',  ( 8.058915628308609413, -4.678948124125613894, 8.679023822940409971 ) ) ;
#34252 = CARTESIAN_POINT ( 'NONE',  ( 12.46419745175926153, -3.023973028971910004, -13.54820305185628904 ) ) ;
#34253 = CARTESIAN_POINT ( 'NONE',  ( 18.13658048666561484, -0.2292434675627126606, -12.69722039463305840 ) ) ;
#34254 = CARTESIAN_POINT ( 'NONE',  ( 11.16225954179439839, -3.122605388210700106, -8.229019074832200076 ) ) ;
#34255 = CARTESIAN_POINT ( 'NONE',  ( 8.610051658774001027, 5.329437560656000272, 6.027391099688998999 ) ) ;
#34256 = VERTEX_POINT ( 'NONE', #35052 ) ;
#34257 = AXIS2_PLACEMENT_3D ( 'NONE', #65165, #12043, #59586 ) ;
#34258 = DIRECTION ( 'NONE',  ( -1.000000000000000000, 0.000000000000000000, 0.000000000000000000 ) ) ;
#34259 = CARTESIAN_POINT ( 'NONE',  ( 18.30003129332100187, -2.732683818840999646, -11.53064095373000164 ) ) ;
#34260 = CARTESIAN_POINT ( 'NONE',  ( 23.74082840454099852, -3.323468775169000189, 13.27900164760999857 ) ) ;
#34261 = VECTOR ( 'NONE', #46959, 1000.000000000000000 ) ;
#34262 = CARTESIAN_POINT ( 'NONE',  ( 18.13782450322838358, 2.273941707540254598, 12.50136077393157308 ) ) ;
#34263 = CARTESIAN_POINT ( 'NONE',  ( 11.01812914314999858, 5.553047824615000572, 4.991737071610000243 ) ) ;
#34264 = CARTESIAN_POINT ( 'NONE',  ( 10.02991192131000098, 2.506457833269999824, 6.215406506815000398 ) ) ;
#34265 = VECTOR ( 'NONE', #4354, 1000.000000000000000 ) ;
#34266 = CARTESIAN_POINT ( 'NONE',  ( 9.397621218489627282, -3.181327125463422334, 7.808718305523518310 ) ) ;
#34267 = B_SPLINE_CURVE_WITH_KNOTS ( 'NONE', 3,
 ( #32355, #53671, #21165, #48422 ),
 .UNSPECIFIED., .F., .F.,
 ( 4, 4 ),
 ( 0.000000000000000000, 1.000000000000000000 ),
 .UNSPECIFIED. ) ;
#34268 = CARTESIAN_POINT ( 'NONE',  ( 8.720712484379999907, 3.780467314030099946, 6.659501631675699862 ) ) ;
#34269 = EDGE_CURVE ( 'NONE', #37026, #53667, #35006, .T. ) ;
#34270 = EDGE_LOOP ( 'NONE', ( #68866, #63580, #17881, #25544 ) ) ;
#34271 = CARTESIAN_POINT ( 'NONE',  ( 12.29460735697735174, -2.139198256859472291, 12.52837235904283730 ) ) ;
#34272 = EDGE_CURVE ( 'NONE', #3478, #4443, #52139, .T. ) ;
#34273 = CARTESIAN_POINT ( 'NONE',  ( 8.793822372493998785, -4.288705740401799638, -8.444453017408701356 ) ) ;
#34274 = CARTESIAN_POINT ( 'NONE',  ( 9.848259964010999568, 4.436917881843999822, 6.148031614254000132 ) ) ;
#34275 = CARTESIAN_POINT ( 'NONE',  ( 9.181310023244000362, 4.573021367100345458, 8.622334741229296995 ) ) ;
#34276 = CIRCLE ( 'NONE', #4099, 1.500000000000000000 ) ;
#34277 = CARTESIAN_POINT ( 'NONE',  ( 10.49764694612699856, 2.940513484064000149, -7.922821994243300914 ) ) ;
#34278 = CARTESIAN_POINT ( 'NONE',  ( 12.51625386035102316, -0.6598665579121884006, 12.58271022457860688 ) ) ;
#34279 = CARTESIAN_POINT ( 'NONE',  ( 7.545267219589999463, 2.302289264429000504, 6.875166305059000393 ) ) ;
#34280 = CARTESIAN_POINT ( 'NONE',  ( 9.256664404737000140, 4.025830366070999311, 9.295863330698999505 ) ) ;
#34281 = CARTESIAN_POINT ( 'NONE',  ( 12.35269809054579149, 2.068595867586759063, 12.54166796000260398 ) ) ;
#34282 = ORIENTED_EDGE ( 'NONE', *, *, #52792, .T. ) ;
#34283 = CARTESIAN_POINT ( 'NONE',  ( 9.585279719593998493, 2.928319778732999978, -8.861178115809998701 ) ) ;
#34284 = CARTESIAN_POINT ( 'NONE',  ( 11.03502897915239878, 4.327133900127000388, -8.735435061820998826 ) ) ;
#34285 = CARTESIAN_POINT ( 'NONE',  ( 10.68437022634959099, -5.721797460400984470, 7.171884794389442597 ) ) ;
#34287 = CARTESIAN_POINT ( 'NONE',  ( 25.05003967968370304, 11.42808677591299649, 3.253271619634388045 ) ) ;
#34286 = CARTESIAN_POINT ( 'NONE',  ( 8.175754440378000254, -2.599231861044000169, 7.909347897884000389 ) ) ;
#34288 = CARTESIAN_POINT ( 'NONE',  ( 10.66657120343299958, -4.048688523195909994, 6.496769302834999316 ) ) ;
#34289 = CARTESIAN_POINT ( 'NONE',  ( 11.56441235500451015, -4.638700978900200056, -6.914884925939399629 ) ) ;
#34290 = ORIENTED_EDGE ( 'NONE', *, *, #68985, .T. ) ;
#34291 = CARTESIAN_POINT ( 'NONE',  ( 1.644020781218000105, 0.6682336154344999946, -3.189788463028000454 ) ) ;
#34292 = EDGE_CURVE ( 'NONE', #26174, #8994, #69080, .T. ) ;
#34293 = CARTESIAN_POINT ( 'NONE',  ( 17.91802421017324320, -0.5088992770524164433, -12.68627498207444226 ) ) ;
#34294 = CARTESIAN_POINT ( 'NONE',  ( 9.423129650240840149, -4.658877085170328058, 8.358757503607595396 ) ) ;
#34295 = CARTESIAN_POINT ( 'NONE',  ( 17.55505043854147118, -3.125000000000000000, 13.52084414783465860 ) ) ;
#34296 = CARTESIAN_POINT ( 'NONE',  ( 24.36453968330800279, -12.29068757565999981, 3.201420012455000297 ) ) ;
#34297 = CARTESIAN_POINT ( 'NONE',  ( 4.900006121741999898, -0.2617993877991499074, -2.000000000000000444 ) ) ;
#34298 = CARTESIAN_POINT ( 'NONE',  ( 10.90000000000000036, -8.263403946409999534, 6.953859016290999229 ) ) ;
#34299 = CARTESIAN_POINT ( 'NONE',  ( 9.398030179116712901, -5.281061815207925392, 7.060613688865339910 ) ) ;
#34300 = FACE_OUTER_BOUND ( 'NONE', #56988, .T. ) ;
#34301 = ORIENTED_EDGE ( 'NONE', *, *, #30497, .F. ) ;
#34302 = CARTESIAN_POINT ( 'NONE',  ( 17.55505043854144276, -0.6250000000000001110, -12.67928921589118474 ) ) ;
#34303 = CARTESIAN_POINT ( 'NONE',  ( 11.13731690804999985, 5.336290732615000643, 5.187964585069000378 ) ) ;
#34304 = CARTESIAN_POINT ( 'NONE',  ( 7.433210666546943735, -2.296204528772303188, 7.849734464718515881 ) ) ;
#34305 = CIRCLE ( 'NONE', #33153, 11.85002173638999778 ) ;
#34306 = CARTESIAN_POINT ( 'NONE',  ( 10.55880524124688158, -4.703942329536042521, 8.703471051125557523 ) ) ;
#34307 = CARTESIAN_POINT ( 'NONE',  ( 1.752794427304000147, -3.577811800725999802, 1.152232014823999950 ) ) ;
#34308 = VERTEX_POINT ( 'NONE', #45542 ) ;
#34309 = CARTESIAN_POINT ( 'NONE',  ( 10.81294898260098947, 2.920599542024987727, -8.329474447052378494 ) ) ;
#34310 = FACE_OUTER_BOUND ( 'NONE', #16173, .T. ) ;
#34311 = LINE ( 'NONE', #38863, #31025 ) ;
#34312 =( GEOMETRIC_REPRESENTATION_CONTEXT ( 3 ) GLOBAL_UNCERTAINTY_ASSIGNED_CONTEXT ( ( #65829 ) ) GLOBAL_UNIT_ASSIGNED_CONTEXT ( ( #52898, #27714, #59168 ) ) REPRESENTATION_CONTEXT ( 'NONE', 'WORKASPACE' ) );
#34313 = CARTESIAN_POINT ( 'NONE',  ( 11.01872200990539952, 3.052519557825900343, 7.830502140005199507 ) ) ;
#34314 = CARTESIAN_POINT ( 'NONE',  ( 11.14975833414749928, -4.796537143354000499, -7.825000000000000178 ) ) ;
#34315 = CARTESIAN_POINT ( 'NONE',  ( 11.37167944038000122, -2.803484087760999888, -6.967877228197000505 ) ) ;
#34316 = AXIS2_PLACEMENT_3D ( 'NONE', #45364, #2705, #22643 ) ;
#34317 = CARTESIAN_POINT ( 'NONE',  ( 17.55505043854147118, -3.199751711897561801, 12.18694338143115452 ) ) ;
#34318 = CARTESIAN_POINT ( 'NONE',  ( 0.4529763571839853786, 3.676114825633475335E-06, -3.452897576335808072 ) ) ;
#34319 = CARTESIAN_POINT ( 'NONE',  ( 12.18432844470339127, -2.573800461448675136, 12.43409912879217849 ) ) ;
#34320 = B_SPLINE_CURVE_WITH_KNOTS ( 'NONE', 3,
 ( #42397, #47297, #42734, #20377, #4981, #30876 ),
 .UNSPECIFIED., .F., .F.,
 ( 4, 2, 4 ),
 ( 0.000000000000000000, 0.5000000000000005551, 1.000000000000000000 ),
 .UNSPECIFIED. ) ;
#34321 = VERTEX_POINT ( 'NONE', #4241 ) ;
#34322 = CARTESIAN_POINT ( 'NONE',  ( 8.401779134048657838, 2.565904574551121975, 8.507432892281750370 ) ) ;
#34323 = ORIENTED_EDGE ( 'NONE', *, *, #56798, .F. ) ;
#34324 = AXIS2_PLACEMENT_3D ( 'NONE', #19583, #63242, #14343 ) ;
#34325 = B_SPLINE_CURVE_WITH_KNOTS ( 'NONE', 3,
 ( #58874, #41422, #36175, #47014 ),
 .UNSPECIFIED., .F., .F.,
 ( 4, 4 ),
 ( 0.000000000000000000, 1.000000000000000000 ),
 .UNSPECIFIED. ) ;
#34326 = CARTESIAN_POINT ( 'NONE',  ( 18.23401891600715885, -2.774919967966536838, 13.72225625730859377 ) ) ;
#34327 = CARTESIAN_POINT ( 'NONE',  ( 10.14887885159599890, -2.730985436695000157, -7.348611220446799486 ) ) ;
#34328 = ORIENTED_EDGE ( 'NONE', *, *, #65959, .F. ) ;
#34329 = CARTESIAN_POINT ( 'NONE',  ( 8.949577224479325466, -5.282137943145613690, 7.064064936788390980 ) ) ;
#34330 = CARTESIAN_POINT ( 'NONE',  ( 25.12927302627635484, -2.819697932548927533, -11.46537540841081615 ) ) ;
#34331 = CARTESIAN_POINT ( 'NONE',  ( 9.823096873516664829, 2.782534154164606921, -7.172815144550894750 ) ) ;
#34332 = CARTESIAN_POINT ( 'NONE',  ( 6.953073139469000630, -9.233001678504999532, 5.200628701625999994 ) ) ;
#34333 = EDGE_CURVE ( 'NONE', #29419, #61078, #9899, .T. ) ;
#34334 = CARTESIAN_POINT ( 'NONE',  ( 10.34021053755999908, 4.202028620710000162, 9.459600235481000041 ) ) ;
#34335 = ADVANCED_FACE ( 'NONE', ( #2877 ), #46566, .T. ) ;
#34336 = FACE_OUTER_BOUND ( 'NONE', #12440, .T. ) ;
#34337 = CARTESIAN_POINT ( 'NONE',  ( 10.89393020684999946, -5.250000000000000000, 7.500000000000000000 ) ) ;
#34338 = CARTESIAN_POINT ( 'NONE',  ( 11.44446797630000034, 3.649424658612000272, -11.12042579671999931 ) ) ;
#34339 = VECTOR ( 'NONE', #28214, 1000.000000000000114 ) ;
#34340 = CARTESIAN_POINT ( 'NONE',  ( 10.55068143582000140, -2.412180768165999911, -6.919582641217999708 ) ) ;
#34341 = CARTESIAN_POINT ( 'NONE',  ( 4.000000000000000000, -2.136325177875821435, -0.2822470469891263378 ) ) ;
#34342 = FACE_OUTER_BOUND ( 'NONE', #60495, .T. ) ;
#34343 = VERTEX_POINT ( 'NONE', #62624 ) ;
#34344 = CARTESIAN_POINT ( 'NONE',  ( 10.05333291544899943, 4.531093146757585011, 6.341063066638221279 ) ) ;
#34345 =( NAMED_UNIT ( * ) PLANE_ANGLE_UNIT ( ) SI_UNIT ( $, .RADIAN. ) );
#34346 = DIRECTION ( 'NONE',  ( 1.000000000000000000, 0.000000000000000000, 0.000000000000000000 ) ) ;
#34347 = CARTESIAN_POINT ( 'NONE',  ( 11.09689463776999929, -5.238465444143000305, 5.055407489333999749 ) ) ;
#34348 = CARTESIAN_POINT ( 'NONE',  ( 5.000030787343001215, 0.2748844998327731326, -2.099962892531005654 ) ) ;
#34349 = CARTESIAN_POINT ( 'NONE',  ( 10.56244474310100045, 5.137935629024000583, -8.052229793103100164 ) ) ;
#34350 = CARTESIAN_POINT ( 'NONE',  ( 12.75679378108275586, 3.246933784478220009, 13.61827548339043581 ) ) ;
#34351 = CARTESIAN_POINT ( 'NONE',  ( 10.50244460374000077, -2.268915328469999881, 7.824865002012999504 ) ) ;
#34352 = EDGE_LOOP ( 'NONE', ( #32351, #38020, #165, #62614, #2660, #41088, #25765, #51245, #2841 ) ) ;
#34353 = CARTESIAN_POINT ( 'NONE',  ( 10.81746213571000048, -5.100000000000000533, 6.571291218949999902 ) ) ;
#34354 = CARTESIAN_POINT ( 'NONE',  ( 12.08146951720330975, 0.04720351400547449089, 13.99992551180917388 ) ) ;
#34355 = VERTEX_POINT ( 'NONE', #57047 ) ;
#34356 = CARTESIAN_POINT ( 'NONE',  ( 23.85395881716046773, 13.23045290494460247, -3.489568871745106549 ) ) ;
#34357 = ADVANCED_FACE ( 'NONE', ( #8474 ), #56716, .T. ) ;
#34358 = CARTESIAN_POINT ( 'NONE',  ( 10.60000000000016485, 4.647604842474216902, -4.756097560975663718 ) ) ;
#34359 = CARTESIAN_POINT ( 'NONE',  ( 24.63625149985600160, -3.694707171958000025, -12.29749030356000006 ) ) ;
#34360 = CARTESIAN_POINT ( 'NONE',  ( 10.97843137008999825, -5.235400103863000254, 6.782920672145000829 ) ) ;
#34361 = EDGE_CURVE ( 'NONE', #8973, #14855, #50845, .T. ) ;
#34362 = STYLED_ITEM ( 'NONE', ( #44059 ), #6030 ) ;
#34363 = CARTESIAN_POINT ( 'NONE',  ( 10.04184687351587613, 4.999583552997725278, -8.268183399968640046 ) ) ;
#34364 = CARTESIAN_POINT ( 'NONE',  ( 9.356463691919302050, 5.100000000000000533, 6.665341197421592589 ) ) ;
#34365 = CARTESIAN_POINT ( 'NONE',  ( 8.231612003192127602, 3.320411601377035726, -8.679267246414919867 ) ) ;
#34366 = CARTESIAN_POINT ( 'NONE',  ( 5.500000000000000000, -1.199999999999999956, -9.776630298829998011 ) ) ;
#34367 = AXIS2_PLACEMENT_3D ( 'NONE', #23961, #66602, #7529 ) ;
#34368 = DIRECTION ( 'NONE',  ( -1.000000000000000000, 0.000000000000000000, 0.000000000000000000 ) ) ;
#34369 = CARTESIAN_POINT ( 'NONE',  ( 9.101385834542000453, -4.783349162191000481, -6.231236652334000148 ) ) ;
#34370 = CARTESIAN_POINT ( 'NONE',  ( 10.92441504065829960, 4.694414232677499577, -6.982228367137699898 ) ) ;
#34371 = CARTESIAN_POINT ( 'NONE',  ( 12.80505043854144276, -0.7192913403693027563, 12.57945229203838267 ) ) ;
#34372 = CARTESIAN_POINT ( 'NONE',  ( 10.96888392554999925, 5.599999999999999645, 6.571291218949999902 ) ) ;
#34373 = CARTESIAN_POINT ( 'NONE',  ( 9.835279731608999043, 4.102460098134500299, -6.362794488108000301 ) ) ;
#34375 = CARTESIAN_POINT ( 'NONE',  ( 10.27678977068999977, -3.259542233426000024, 4.694017977725000179 ) ) ;
#34374 = CARTESIAN_POINT ( 'NONE',  ( 9.570430433046999141, -4.737822807309499673, 7.955330044604899342 ) ) ;
#34376 = CARTESIAN_POINT ( 'NONE',  ( 23.58690406892612756, -13.37933363478873794, 4.060878750407953319 ) ) ;
#34377 = ORIENTED_EDGE ( 'NONE', *, *, #21684, .T. ) ;
#34378 = AXIS2_PLACEMENT_3D ( 'NONE', #60602, #29149, #50457 ) ;
#34379 = EDGE_CURVE ( 'NONE', #4046, #32306, #22579, .T. ) ;
#34380 = CARTESIAN_POINT ( 'NONE',  ( 11.68788784977535933, 3.014014167207800465, 7.556342205905759890 ) ) ;
#34381 = CARTESIAN_POINT ( 'NONE',  ( 9.104016254283999743, -5.045864843302999780, 8.527867871227000407 ) ) ;
#34382 = CARTESIAN_POINT ( 'NONE',  ( 10.38955864497999926, 4.790758628877400227, 6.880692865553299953 ) ) ;
#34383 = CARTESIAN_POINT ( 'NONE',  ( 10.03743284169262573, 3.545113930219122800, -6.752597208702827203 ) ) ;
#34384 = CIRCLE ( 'NONE', #54427, 12.35000000006999876 ) ;
#34385 = CARTESIAN_POINT ( 'NONE',  ( 9.696086916451999826, -2.554404004330999900, 7.600685922079000179 ) ) ;
#34386 = CYLINDRICAL_SURFACE ( 'NONE', #10696, 1.350000000000000533 ) ;
#34387 = UNCERTAINTY_MEASURE_WITH_UNIT (LENGTH_MEASURE( 1.000000000000000082E-05 ), #25560, 'distance_accuracy_value', 'NONE');
#34388 = ORIENTED_EDGE ( 'NONE', *, *, #36387, .T. ) ;
#34389 = CARTESIAN_POINT ( 'NONE',  ( 8.619480666858999385, -3.619299191678599925, -8.576476893896000320 ) ) ;
#34390 = DIRECTION ( 'NONE',  ( -1.000000000000000000, 0.000000000000000000, 0.000000000000000000 ) ) ;
#34391 = CARTESIAN_POINT ( 'NONE',  ( 6.478079102618999663, -0.08083205921694999740, 1.612735633780000066 ) ) ;
#34392 = PRODUCT_DEFINITION_SHAPE ( 'NONE', 'NONE',  #29121 ) ;
#34393 = CARTESIAN_POINT ( 'NONE',  ( 18.21613312502037019, 2.776914653343697026, -12.29020858420810924 ) ) ;
#34394 = CARTESIAN_POINT ( 'NONE',  ( 7.000000000000000000, 9.904500808576843340, -4.554970072511064672 ) ) ;
#34395 = CARTESIAN_POINT ( 'NONE',  ( 7.000002934099999408, -1.865174681369999698E-13, 1.040631535496999952E-13 ) ) ;
#34396 = CARTESIAN_POINT ( 'NONE',  ( 10.29262282008599882, 4.451581486939200083, -8.228386593078399258 ) ) ;
#34397 = CARTESIAN_POINT ( 'NONE',  ( 14.93333333083533532, 8.833279250037010755, 7.896561129384958910 ) ) ;
#34398 = CARTESIAN_POINT ( 'NONE',  ( 9.746744136172999617, -5.062748727288000516, -8.618689820632001286 ) ) ;
#34399 = CARTESIAN_POINT ( 'NONE',  ( 24.98214587845099999, 11.60529653845999931, 3.133087885915999848 ) ) ;
#34400 = VERTEX_POINT ( 'NONE', #8128 ) ;
#34401 = CARTESIAN_POINT ( 'NONE',  ( 17.55505043854143565, 1.787816316115923954, -13.88537766212463254 ) ) ;
#34402 = CONICAL_SURFACE ( 'NONE', #41073, 1.349999999648999971, 0.7853981633972997312 ) ;
#34403 = CARTESIAN_POINT ( 'NONE',  ( 12.60420804235854675, 0.5919407257947373324, -13.88303015925713879 ) ) ;
#34404 = CYLINDRICAL_SURFACE ( 'NONE', #44392, 1.250000000000000222 ) ;
#34405 = DIRECTION ( 'NONE',  ( 0.000000000000000000, 0.7198977633594745296, -0.6940801180771755119 ) ) ;
#34406 = B_SPLINE_CURVE_WITH_KNOTS ( 'NONE', 3,
 ( #39206, #18918, #60530, #67140, #49692, #44470 ),
 .UNSPECIFIED., .F., .F.,
 ( 4, 1, 1, 4 ),
 ( 0.000000000000000000, 0.3333333333333000081, 0.6666666666667000474, 1.000000000000000000 ),
 .UNSPECIFIED. ) ;
#34407 = CARTESIAN_POINT ( 'NONE',  ( 4.900006121741999898, 1.229093439949828781, -1.599333684796360844 ) ) ;
#34408 = CARTESIAN_POINT ( 'NONE',  ( 18.30000000002852900, -11.04996330604345722, 3.691231741008185629 ) ) ;
#34409 = DIRECTION ( 'NONE',  ( 1.000000000000000000, 0.000000000000000000, 0.000000000000000000 ) ) ;
#34410 = ORIENTED_EDGE ( 'NONE', *, *, #66570, .F. ) ;
#34411 = CARTESIAN_POINT ( 'NONE',  ( 17.81510163565844707, 1.931577867956977945, -13.77771208381435031 ) ) ;
#34412 = ORIENTED_EDGE ( 'NONE', *, *, #37952, .F. ) ;
#34413 = DIRECTION ( 'NONE',  ( 0.000000000000000000, -1.000000000000000000, 0.000000000000000000 ) ) ;
#34414 = CARTESIAN_POINT ( 'NONE',  ( 25.29995422340600086, 2.596935224161999844, 11.35301931920000129 ) ) ;
#34415 = VECTOR ( 'NONE', #61889, 1000.000000000000000 ) ;
#34416 = CARTESIAN_POINT ( 'NONE',  ( 9.798945280410000791, 5.639765292528999829, -8.059103558718000215 ) ) ;
#34417 = ADVANCED_FACE ( 'NONE', ( #50783 ), #25921, .F. ) ;
#34418 = CARTESIAN_POINT ( 'NONE',  ( 11.09999999999999964, -2.660544054589125462, -8.447007675617404843 ) ) ;
#34419 = ADVANCED_FACE ( 'NONE', ( #63997 ), #48625, .T. ) ;
#34420 = CARTESIAN_POINT ( 'NONE',  ( 12.80505043854146940, -3.248109929747638347, 13.61799478206225444 ) ) ;
#34421 = CARTESIAN_POINT ( 'NONE',  ( 17.78594645484335857, 0.5808586469753534987, -12.68211397078068003 ) ) ;
#34422 = MECHANICAL_DESIGN_GEOMETRIC_PRESENTATION_REPRESENTATION (  '', ( #28835 ), #24372 ) ;
#34423 = EDGE_CURVE ( 'NONE', #34720, #19975, #19131, .T. ) ;
#34424 = CARTESIAN_POINT ( 'NONE',  ( 4.857109839683332986, 1.199500263597268246, 0.9218200799623752495 ) ) ;
#34425 = ORIENTED_EDGE ( 'NONE', *, *, #40584, .F. ) ;
#34426 = CARTESIAN_POINT ( 'NONE',  ( 10.25462442569999943, -2.860634389522000109, 6.604605425112000994 ) ) ;
#34427 = CARTESIAN_POINT ( 'NONE',  ( 18.03215848267582189, -2.904634633620106765, -13.57923905310026313 ) ) ;
#34428 = CARTESIAN_POINT ( 'NONE',  ( 9.793039158772000263, 5.817107086401000160, -6.945352709928000579 ) ) ;
#34429 = ORIENTED_EDGE ( 'NONE', *, *, #870, .T. ) ;
#34430 = CARTESIAN_POINT ( 'NONE',  ( 10.05525296965999971, 5.223856410664000194, -6.898317050646999959 ) ) ;
#34431 = ORIENTED_EDGE ( 'NONE', *, *, #21606, .F. ) ;
#34432 = CARTESIAN_POINT ( 'NONE',  ( 9.934583761885999564, 2.921249888908000081, 6.812480849273599759 ) ) ;
#34433 = CARTESIAN_POINT ( 'NONE',  ( 18.21786174063356967, -2.187645605293250917, -12.40865382983254506 ) ) ;
#34434 = B_SPLINE_CURVE_WITH_KNOTS ( 'NONE', 3,
 ( #24030, #38383, #34190, #54465 ),
 .UNSPECIFIED., .F., .F.,
 ( 4, 4 ),
 ( 0.000000000000000000, 1.000000000000000000 ),
 .UNSPECIFIED. ) ;
#34435 = DIRECTION ( 'NONE',  ( 0.000000000000000000, 0.000000000000000000, 1.000000000000000000 ) ) ;
#34436 = CARTESIAN_POINT ( 'NONE',  ( 9.023148997459999876, 5.167567567567999731, -6.822293592207000934 ) ) ;
#34437 = CARTESIAN_POINT ( 'NONE',  ( 23.60205915885299888, 2.504446818062000535, 12.27382285989999566 ) ) ;
#34438 = AXIS2_PLACEMENT_3D ( 'NONE', #45058, #7644, #2398 ) ;
#34439 = CARTESIAN_POINT ( 'NONE',  ( 9.687329965421998423, 3.397808798486600335, 6.876242273533999416 ) ) ;
#34440 = CARTESIAN_POINT ( 'NONE',  ( 9.379272429982512094, -2.901493056294750073, 8.849497897647601974 ) ) ;
#34441 = ORIENTED_EDGE ( 'NONE', *, *, #43404, .T. ) ;
#34442 = DIRECTION ( 'NONE',  ( 0.7071067779452319124, 0.5091007393949228410, -0.4907305184431219325 ) ) ;
#34443 = CARTESIAN_POINT ( 'NONE',  ( 10.69829221958999987, 2.534027248431999890, -6.667786804432999759 ) ) ;
#34444 = CARTESIAN_POINT ( 'NONE',  ( 11.04423059897000137, -5.244779299905999892, -5.172774331138000115 ) ) ;
#34445 = CARTESIAN_POINT ( 'NONE',  ( 12.11351653522380545, 2.298558756434998518, -13.81002389223456106 ) ) ;
#34446 = CIRCLE ( 'NONE', #43367, 2.574999650349000024 ) ;
#34447 = CARTESIAN_POINT ( 'NONE',  ( 10.16562143724499911, -3.150324864944999970, -6.543738240676099771 ) ) ;
#34448 = CARTESIAN_POINT ( 'NONE',  ( 11.02786767503999954, -5.596230239120999705, 7.209501483790000442 ) ) ;
#34449 = CARTESIAN_POINT ( 'NONE',  ( 17.57569738523962144, 0.6249994334955766284, 13.88107975403459626 ) ) ;
#34450 = CARTESIAN_POINT ( 'NONE',  ( 25.46372797112000086, -8.354608193938998895, 8.148457429720000533 ) ) ;
#34451 = ORIENTED_EDGE ( 'NONE', *, *, #27354, .F. ) ;
#34452 = ORIENTED_EDGE ( 'NONE', *, *, #17119, .T. ) ;
#34453 = CARTESIAN_POINT ( 'NONE',  ( 9.038304719595000591, 3.867331042029999999, -9.227339949050001877 ) ) ;
#34454 = FACE_OUTER_BOUND ( 'NONE', #64821, .T. ) ;
#34455 = CARTESIAN_POINT ( 'NONE',  ( 12.18008982747132229, -2.511713771506315140, 13.67097129485760476 ) ) ;
#34456 = CARTESIAN_POINT ( 'NONE',  ( 10.98768472639999949, 2.860900986606000007, -4.945212061661000469 ) ) ;
#34457 = B_SPLINE_CURVE_WITH_KNOTS ( 'NONE', 3,
 ( #62259, #14380, #47568, #57347, #25889, #51767, #20644, #35700, #4899 ),
 .UNSPECIFIED., .F., .F.,
 ( 4, 1, 2, 2, 4 ),
 ( 0.000000000000000000, 0.2500000000000000555, 0.3750000000000000000, 0.5000000000000000000, 1.000000000000000000 ),
 .UNSPECIFIED. ) ;
#34458 = CARTESIAN_POINT ( 'NONE',  ( 7.422245559621999611, -5.361050935357000391, 6.973449182446000094 ) ) ;
#34459 = CARTESIAN_POINT ( 'NONE',  ( 6.899999691988000450, 0.000000000000000000, 0.000000000000000000 ) ) ;
#34461 = CARTESIAN_POINT ( 'NONE',  ( 11.12486982654999856, -5.426806274205000058, 5.164827877695000069 ) ) ;
#34460 = CARTESIAN_POINT ( 'NONE',  ( 10.98444474310100105, -2.984290294633999974, 7.007085334055199510 ) ) ;
#34462 = DIRECTION ( 'NONE',  ( 0.7071067811865475727, -0.7071067811865475727, 0.000000000000000000 ) ) ;
#34463 = ORIENTED_EDGE ( 'NONE', *, *, #33456, .T. ) ;
#34464 = CARTESIAN_POINT ( 'NONE',  ( 24.67921310950000091, -12.29514723793999842, -2.979192343402000009 ) ) ;
#34465 = EDGE_CURVE ( 'NONE', #7462, #47308, #23280, .T. ) ;
#34466 = AXIS2_PLACEMENT_3D ( 'NONE', #28239, #50253, #23679 ) ;
#34467 = CARTESIAN_POINT ( 'NONE',  ( 17.85930819889520293, 0.5460377805369025506, 12.68419612078310621 ) ) ;
#34468 = CARTESIAN_POINT ( 'NONE',  ( 12.66329582877813387, -0.6090237436603173071, 12.68033599931052713 ) ) ;
#34469 = EDGE_CURVE ( 'NONE', #12694, #45049, #3215, .T. ) ;
#34470 = CARTESIAN_POINT ( 'NONE',  ( 18.11819331234647024, -2.771443073964306336, -12.38417569150683128 ) ) ;
#34471 = EDGE_LOOP ( 'NONE', ( #2775, #30762, #38084, #40489 ) ) ;
#34473 = CARTESIAN_POINT ( 'NONE',  ( 12.80505043854146940, -1.760910691117821614, -12.47634535983622683 ) ) ;
#34472 = CARTESIAN_POINT ( 'NONE',  ( 10.90000000000000036, 5.283926297003000094, 7.082827057608000132 ) ) ;
#34474 = CARTESIAN_POINT ( 'NONE',  ( 8.912754719595000097, 2.481540185810000132, -7.878707153279001396 ) ) ;
#34475 = DIRECTION ( 'NONE',  ( 0.000000000000000000, 0.000000000000000000, -1.000000000000000000 ) ) ;
#34476 = CARTESIAN_POINT ( 'NONE',  ( 8.057193283769001013, -5.122325659685000865, 6.732791538586998747 ) ) ;
#34477 = VECTOR ( 'NONE', #23826, 1000.000000000000000 ) ;
#34478 = CARTESIAN_POINT ( 'NONE',  ( 17.60000001947600268, -11.86186880240999919, 3.298627760718999991 ) ) ;
#34479 = CARTESIAN_POINT ( 'NONE',  ( 8.590472024761121261, -4.653241489316459756, 5.916299078424147595 ) ) ;
#34480 = CARTESIAN_POINT ( 'NONE',  ( 2.876611010965999693, -1.756444158189999882, 2.941041065258999776 ) ) ;
#34481 = ORIENTED_EDGE ( 'NONE', *, *, #42574, .T. ) ;
#34482 = CIRCLE ( 'NONE', #46743, 1.625000000000000000 ) ;
#34483 = B_SPLINE_CURVE_WITH_KNOTS ( 'NONE', 3,
 ( #62345, #8865, #14801, #15143 ),
 .UNSPECIFIED., .F., .F.,
 ( 4, 4 ),
 ( 0.000000000000000000, 1.000000000000000000 ),
 .UNSPECIFIED. ) ;
#34484 = CARTESIAN_POINT ( 'NONE',  ( 12.18940205905204621, -0.3800566752825980110, -12.59427093624936767 ) ) ;
#34485 = CARTESIAN_POINT ( 'NONE',  ( 7.807587516710824183, -3.023362854828683499, 6.518709396491844110 ) ) ;
#34486 = DIRECTION ( 'NONE',  ( 0.7071067486699967874, -0.7071068137030968037, 9.022793105466955192E-11 ) ) ;
#34487 = CARTESIAN_POINT ( 'NONE',  ( 9.069718325438000051, 4.108964550738000376, 8.851615252874999840 ) ) ;
#34488 = CARTESIAN_POINT ( 'NONE',  ( 1.775000508673000077, 0.000000000000000000, 0.000000000000000000 ) ) ;
#34489 = ORIENTED_EDGE ( 'NONE', *, *, #34102, .T. ) ;
#34490 = CARTESIAN_POINT ( 'NONE',  ( 6.378719963561000128, -1.260983081135999884, 0.3979920142897999669 ) ) ;
#34491 = CARTESIAN_POINT ( 'NONE',  ( 8.435360841226998474, 3.517942668285999996, -6.188254172171000711 ) ) ;
#34493 = CARTESIAN_POINT ( 'NONE',  ( 11.00000000000000000, 4.991767524623399233, -7.174999999999999822 ) ) ;
#34492 = CARTESIAN_POINT ( 'NONE',  ( 9.516209514376292589, -2.899999999999999911, -6.465979581418092259 ) ) ;
#34494 = AXIS2_PLACEMENT_3D ( 'NONE', #47067, #9301, #25387 ) ;
#34495 = CARTESIAN_POINT ( 'NONE',  ( 10.69041504065829962, 5.024558373595999328, 8.263934892306599167 ) ) ;
#34496 = CARTESIAN_POINT ( 'NONE',  ( 10.42760663304247615, -3.352948950021445995, -6.912280214781111098 ) ) ;
#34497 = VERTEX_POINT ( 'NONE', #22039 ) ;
#34498 = ORIENTED_EDGE ( 'NONE', *, *, #23750, .F. ) ;
#34499 = CARTESIAN_POINT ( 'NONE',  ( 0.04997405931213007302, 2.849971983161022848, 1.472630648340316603E-09 ) ) ;
#34500 = CARTESIAN_POINT ( 'NONE',  ( 8.881816940380000247, -4.977917894183000236, 6.416767031887000705 ) ) ;
#34501 = CARTESIAN_POINT ( 'NONE',  ( 17.85480509960784445, 0.6653129401483860450, -13.98418548573916098 ) ) ;
#34502 = ORIENTED_EDGE ( 'NONE', *, *, #49188, .T. ) ;
#34503 = CARTESIAN_POINT ( 'NONE',  ( 10.96186279128636620, 8.868890186250860452, -6.466688578834012269 ) ) ;
#34504 = ADVANCED_FACE ( 'NONE', ( #10868 ), #33858, .F. ) ;
#34505 = DIRECTION ( 'NONE',  ( 1.000000000000000000, 0.000000000000000000, 0.000000000000000000 ) ) ;
#34506 = CARTESIAN_POINT ( 'NONE',  ( 7.590514158769000375, 5.397384434738000003, -7.480682713844000631 ) ) ;
#34507 = CARTESIAN_POINT ( 'NONE',  ( 5.600000001140999828, 0.000000000000000000, -1.349999998858999906 ) ) ;
#34508 = EDGE_CURVE ( 'NONE', #26111, #66341, #56587, .T. ) ;
#34509 = CARTESIAN_POINT ( 'NONE',  ( 18.28771814374038129, -2.987295517884131169, 11.95930540589378133 ) ) ;
#34510 = EDGE_LOOP ( 'NONE', ( #32253, #38779, #49007, #37749 ) ) ;
#34511 = CARTESIAN_POINT ( 'NONE',  ( 12.80505043854146940, -1.875000000000000444, -12.57541666120756396 ) ) ;
#34512 = EDGE_CURVE ( 'NONE', #28231, #28381, #31648, .T. ) ;
#34513 = CARTESIAN_POINT ( 'NONE',  ( 12.80505043854146940, -3.125000000000000000, -13.52078605991414761 ) ) ;
#34514 = DIRECTION ( 'NONE',  ( 1.000000000000000000, 0.000000000000000000, 0.000000000000000000 ) ) ;
#34515 = DIRECTION ( 'NONE',  ( 1.000000000000000000, 0.000000000000000000, 0.000000000000000000 ) ) ;
#34516 = CARTESIAN_POINT ( 'NONE',  ( 9.629471092178999214, -5.100000000000000533, 6.152188490330000370 ) ) ;
#34517 = EDGE_LOOP ( 'NONE', ( #60104, #67230, #56288, #55367 ) ) ;
#34518 = DIRECTION ( 'NONE',  ( 0.000000000000000000, 0.000000000000000000, -1.000000000000000000 ) ) ;
#34519 = CARTESIAN_POINT ( 'NONE',  ( 10.88210843320517007, 2.862311695598936723, -8.098394516494941797 ) ) ;
#34520 = CARTESIAN_POINT ( 'NONE',  ( 6.993847165045809611, 3.347364397022671856, -9.238695015924625054 ) ) ;
#34521 = CARTESIAN_POINT ( 'NONE',  ( 24.66708179677300450, 12.30983497458833931, -2.983163088688387976 ) ) ;
#34522 = DIRECTION ( 'NONE',  ( 0.000000000000000000, 0.1807154286440006141, 0.9835354258236025382 ) ) ;
#34523 = CARTESIAN_POINT ( 'NONE',  ( 12.30864111941013128, -0.3802875570022061225, -13.89301034115781874 ) ) ;
#34524 = CARTESIAN_POINT ( 'NONE',  ( 18.16360624365139742, -2.642789843301108554, 12.41718366361783232 ) ) ;
#34525 = ORIENTED_EDGE ( 'NONE', *, *, #40499, .F. ) ;
#34526 = CARTESIAN_POINT ( 'NONE',  ( 10.60746886766490071, -4.498335456194499926, -6.594573315824700188 ) ) ;
#34527 = ORIENTED_EDGE ( 'NONE', *, *, #42613, .T. ) ;
#34528 = ADVANCED_FACE ( 'NONE', ( #27301 ), #57295, .T. ) ;
#34529 = CARTESIAN_POINT ( 'NONE',  ( 18.17481653528710339, 2.416771143787688203, 13.69072451370120369 ) ) ;
#34530 = CARTESIAN_POINT ( 'NONE',  ( 9.079170280414000871, 4.815598936798999752, -8.835641302565999666 ) ) ;
#34531 = CARTESIAN_POINT ( 'NONE',  ( 2.628909614058000166, -3.044403958803000076, -1.466915694452000096 ) ) ;
#34532 = CARTESIAN_POINT ( 'NONE',  ( 10.78636854442000192, -5.666037955714999796, -7.787004779180999314 ) ) ;
#34533 = CARTESIAN_POINT ( 'NONE',  ( 24.53429010005800137, -12.47024913742999885, 3.026245653581999928 ) ) ;
#34534 = DIRECTION ( 'NONE',  ( 0.000000000000000000, 1.000000000000000000, 0.000000000000000000 ) ) ;
#34535 = EDGE_LOOP ( 'NONE', ( #17317, #65692, #3762 ) ) ;
#34536 = CARTESIAN_POINT ( 'NONE',  ( 12.10533460557258323, -3.815825449682300086, 6.374224726731999802 ) ) ;
#34537 = CARTESIAN_POINT ( 'NONE',  ( 10.11094409420000062, 5.100000000000000533, -6.571291218949999902 ) ) ;
#34538 = CARTESIAN_POINT ( 'NONE',  ( 25.29987333571600061, -10.83443035398000021, -3.855530949778000149 ) ) ;
#34539 = CARTESIAN_POINT ( 'NONE',  ( 23.66004879239100234, 9.998911746292000302, 9.691526727427998367 ) ) ;
#34541 = CARTESIAN_POINT ( 'NONE',  ( 9.167131993064588258, 2.992074715526335194, 8.398797324404764453 ) ) ;
#34540 = CARTESIAN_POINT ( 'NONE',  ( 11.25041981190000051, 5.730782764036999488, 8.122675980938000251 ) ) ;
#34542 = CARTESIAN_POINT ( 'NONE',  ( 10.57980110216399972, 3.260758259645400337, -7.048535450274799885 ) ) ;
#34543 = CARTESIAN_POINT ( 'NONE',  ( 10.95930679442663269, 2.825993392401128901, -6.684172063606795611 ) ) ;
#34544 = EDGE_CURVE ( 'NONE', #55747, #10029, #33933, .T. ) ;
#34545 = CARTESIAN_POINT ( 'NONE',  ( 9.655013376692998861, 3.104586782631499897, -7.044942343771899651 ) ) ;
#34546 = FACE_OUTER_BOUND ( 'NONE', #41950, .T. ) ;
#34547 = CARTESIAN_POINT ( 'NONE',  ( 7.305862029444999628, -1.022267936763999963, 0.4061956009805000600 ) ) ;
#34548 = B_SPLINE_CURVE_WITH_KNOTS ( 'NONE', 3,
 ( #42247, #26504, #63552, #58311, #58656, #5515, #37676, #6547, #49542, #65960 ),
 .UNSPECIFIED., .F., .F.,
 ( 4, 2, 2, 2, 4 ),
 ( 0.5000000021935380179, 0.6250000016451535689, 0.7500000010967690089, 0.8750000005483844490, 1.000000000000000000 ),
 .UNSPECIFIED. ) ;
#34549 = CARTESIAN_POINT ( 'NONE',  ( 7.000000000000000000, -7.526486366024999874, 3.526486366024999874 ) ) ;
#34550 = EDGE_CURVE ( 'NONE', #718, #10646, #43728, .T. ) ;
#34551 = CARTESIAN_POINT ( 'NONE',  ( 11.22023584123000006, 3.883089684441999978, -8.854806321849000739 ) ) ;
#34552 = ORIENTED_EDGE ( 'NONE', *, *, #52393, .T. ) ;
#34553 = CARTESIAN_POINT ( 'NONE',  ( 8.373668146795001377, -2.202816532622999812, 7.706987678916999762 ) ) ;
#34554 = CARTESIAN_POINT ( 'NONE',  ( 18.15197774836038036, 2.932501865601730984, 13.68943155935733991 ) ) ;
#34555 = CARTESIAN_POINT ( 'NONE',  ( 15.90018573812399971, -8.493548356068000516, -8.263529029821000904 ) ) ;
#34556 = CARTESIAN_POINT ( 'NONE',  ( 9.991279731608999626, 4.077800926195140008, 8.363513150096299142 ) ) ;
#34557 = EDGE_LOOP ( 'NONE', ( #21937, #3433, #48155, #12094 ) ) ;
#34558 = CARTESIAN_POINT ( 'NONE',  ( 9.117517219591000810, 4.954905351382000944, 8.825777580285999235 ) ) ;
#34560 = CARTESIAN_POINT ( 'NONE',  ( 9.226967411678998587, -4.064442376558529801, 6.608809560686199625 ) ) ;
#34559 = CARTESIAN_POINT ( 'NONE',  ( 10.34588779216199939, -3.198058499272899979, -7.789199634454999632 ) ) ;
#34561 = CARTESIAN_POINT ( 'NONE',  ( 10.03976415876999972, 2.255572964181999929, -8.111983882175000105 ) ) ;
#34562 = ORIENTED_EDGE ( 'NONE', *, *, #10810, .T. ) ;
#34563 = CARTESIAN_POINT ( 'NONE',  ( 10.24477918374999952, 5.265206995764999398, 8.959504263949002123 ) ) ;
#34564 = CARTESIAN_POINT ( 'NONE',  ( 5.000030787343000327, -2.099962892530999881, 0.000000000000000000 ) ) ;
#34565 = CARTESIAN_POINT ( 'NONE',  ( 11.13764426047339917, 4.613828180779599997, 6.538488127609999978 ) ) ;
#34566 = CARTESIAN_POINT ( 'NONE',  ( 9.854949224988001077, -2.800315695760000168, 9.013807298610000629 ) ) ;
#34567 = PLANE ( 'NONE',  #60019 ) ;
#34568 = ORIENTED_EDGE ( 'NONE', *, *, #57044, .T. ) ;
#34569 = DIRECTION ( 'NONE',  ( 0.000000000000000000, 1.000000000000000000, 0.000000000000000000 ) ) ;
#34570 = CARTESIAN_POINT ( 'NONE',  ( 11.03091694037999915, -5.020463882420000523, -6.601194361798000010 ) ) ;
#34571 = CARTESIAN_POINT ( 'NONE',  ( 7.899652377730045139, -2.585612559568443380, 8.512102292667707459 ) ) ;
#34572 = CARTESIAN_POINT ( 'NONE',  ( 9.034116535116000435, -4.695350938297000454, 8.660677768253002284 ) ) ;
#34573 = CARTESIAN_POINT ( 'NONE',  ( 10.44999293566599974, -3.279967330949900450, -8.383280442119700027 ) ) ;
#34574 = CARTESIAN_POINT ( 'NONE',  ( 9.146822372494000319, -4.288705740401799638, 6.555546982591299532 ) ) ;
#34575 = VERTEX_POINT ( 'NONE', #55252 ) ;
#34576 = CARTESIAN_POINT ( 'NONE',  ( 24.81041655173479299, -11.68081165545370403, -3.195144698386812809 ) ) ;
#34577 = CARTESIAN_POINT ( 'NONE',  ( 11.87964291764649971, -5.268358781405000357, 7.656787697937099679 ) ) ;
#34578 = EDGE_LOOP ( 'NONE', ( #5555, #28656, #10475, #11489 ) ) ;
#34579 = CARTESIAN_POINT ( 'NONE',  ( 10.14393020684900115, -2.750000000000000000, 7.500000000000000000 ) ) ;
#34580 = ORIENTED_EDGE ( 'NONE', *, *, #9311, .F. ) ;
#34581 = CARTESIAN_POINT ( 'NONE',  ( 9.886323620223000930, -4.261100936929000049, -5.979198511086000423 ) ) ;
#34582 = CARTESIAN_POINT ( 'NONE',  ( 9.093935841232999806, 2.156584729807999867, -7.959751745006000689 ) ) ;
#34583 = CARTESIAN_POINT ( 'NONE',  ( 10.84657802013509986, 2.684088780794000151, -7.469366283838649423 ) ) ;
#34584 = CYLINDRICAL_SURFACE ( 'NONE', #65646, 0.5000000000000004441 ) ;
#34585 = CARTESIAN_POINT ( 'NONE',  ( 12.20034797952038552, 2.341680320747017596, -12.48707311375845030 ) ) ;
#34586 = EDGE_CURVE ( 'NONE', #22584, #68990, #6655, .T. ) ;
#34587 = CARTESIAN_POINT ( 'NONE',  ( 11.64179841651039915, -4.353306409735099969, 6.560784671286499226 ) ) ;
#34588 = CARTESIAN_POINT ( 'NONE',  ( 11.10746886766490071, -4.498335456194499926, 8.405426684175299812 ) ) ;
#34589 = EDGE_CURVE ( 'NONE', #31306, #26914, #54099, .T. ) ;
#34590 = ORIENTED_EDGE ( 'NONE', *, *, #30618, .F. ) ;
#34591 = AXIS2_PLACEMENT_3D ( 'NONE', #65415, #49339, #54940 ) ;
#34592 = CARTESIAN_POINT ( 'NONE',  ( 7.718334321649531482, 2.593359702620003038, 7.633860556273081244 ) ) ;
#34593 = ORIENTED_EDGE ( 'NONE', *, *, #13366, .F. ) ;
#34594 = CARTESIAN_POINT ( 'NONE',  ( 8.149355646792999508, -2.583664704444999849, 6.684748541034000624 ) ) ;
#34595 = CARTESIAN_POINT ( 'NONE',  ( 17.55505043854144276, 0.7302158263239086899, 13.98094363220831049 ) ) ;
#34596 = VERTEX_POINT ( 'NONE', #44431 ) ;
#34597 = B_SPLINE_SURFACE_WITH_KNOTS ( 'NONE', 3, 3, ( 
 ( #2112, #48620, #12946, #23429, #44767, #66068, #60833, #34274, #11541, #721, #48962, #43380, #64680, #16787, #38117, #59442, #32884, #54195, #6297, #2446, #40533, #55593, #24804, #14322, #30400, #29380, #29037, #62201, #24463, #45788, #2788, #19559, #23770, #51032, #7695 ),
 ( #3132, #13979, #51708, #3804, #61858, #8725, #34962, #67099, #39860, #18878, #13300, #30068, #56279, #46128, #61181, #45105, #50346, #62538, #25142, #50692, #51371, #46473, #67779, #3469, #66414, #67435, #35304, #34624, #18533, #14659, #35647, #55937, #19209, #40881, #8039 ),
 ( #56620, #66761, #40204, #61522, #24114, #56959, #29728, #9061, #45448, #19901, #41227, #13637, #8386, #47853, #36672, #47160, #4838, #20583, #27825, #20931, #52046, #9392, #10092, #31090, #31427, #52743, #9742, #52398, #4490, #26179, #25830, #15683, #68460, #57992, #41909 ),
 ( #11717, #63214, #62875, #68122, #35975, #15344, #47506, #63571, #36320, #58329, #68811, #54373, #64849, #16960, #42267, #65199, #38293, #4149, #37017, #5189, #41566, #10431, #31772, #59622, #53089, #26526, #20241, #14995, #57637, #901, #22213, #43549, #33059, #6476, #30738 ) ),
 .UNSPECIFIED., .F., .F., .F.,
 ( 4, 4 ),
 ( 4, 1, 1, 1, 1, 1, 1, 1, 1, 1, 1, 1, 1, 1, 1, 1, 1, 1, 1, 1, 1, 1, 1, 1, 1, 1, 1, 1, 1, 1, 1, 1, 4 ),
 ( -0.1039370721279000015, 1.103937072127999963 ),
 ( -0.01735257130020999988, 0.01084535706264999969, 0.03904328542550000031, 0.06724121378835999641, 0.09543914215121999944, 0.1236370705141000004, 0.1518349988768999959, 0.1800329272397999947, 0.2082308556026999935, 0.2364287839655000167, 0.2646267123283999601, 0.2928246406912000110, 0.3210225690540999821, 0.3492204974169000331, 0.3774184257798000042, 0.4056163541427000307, 0.4338142825054999707, 0.4620122108683999973, 0.4902101392311999928, 0.5184080675940999638, 0.5466059959569999904, 0.5748039243197999859, 0.6030018526827000125, 0.6311997810455000080, 0.6593977094084000345, 0.6875956377712000300, 0.7157935661340999456, 0.7439914944969999722, 0.7721894228597999676, 0.8003873512226999942, 0.8285852795854999897, 0.8567832079484000163, 0.8849811363112999318 ),
 .UNSPECIFIED. ) ;
#34598 = CARTESIAN_POINT ( 'NONE',  ( 12.13061620557594722, -2.744764576889035634, -12.29741386912397161 ) ) ;
#34599 = CARTESIAN_POINT ( 'NONE',  ( 10.45257053952200010, 3.605640676136899980, 8.422730500489899796 ) ) ;
#34600 = CARTESIAN_POINT ( 'NONE',  ( 11.19050685320999960, -2.516759970060999940, -6.840363309917000478 ) ) ;
#34601 = CARTESIAN_POINT ( 'NONE',  ( 6.357109839683332986, 1.199500263597268246, 0.9218200799623752495 ) ) ;
#34602 = DIRECTION ( 'NONE',  ( 0.000000000000000000, 0.2483835927444960623, -0.9686617525510834437 ) ) ;
#34603 = CARTESIAN_POINT ( 'NONE',  ( 9.838567964380441566, 5.764523275123773161, -7.468534388609791463 ) ) ;
#34604 = CARTESIAN_POINT ( 'NONE',  ( 12.60230703261661667, -3.091556739796029074, -13.52998185037902346 ) ) ;
#34605 = CARTESIAN_POINT ( 'NONE',  ( 18.17607568152034148, -0.07112609253419316380, -12.69973757146476778 ) ) ;
#34606 = CARTESIAN_POINT ( 'NONE',  ( 11.09672200990539892, -4.817867935977999672, -7.214709569664399247 ) ) ;
#34607 = CARTESIAN_POINT ( 'NONE',  ( 10.25000000000000000, 0.000000000000000000, 0.000000000000000000 ) ) ;
#34608 = CARTESIAN_POINT ( 'NONE',  ( 8.315517219592001297, 5.485785046334999748, 8.532070739720001740 ) ) ;
#34609 = ORIENTED_EDGE ( 'NONE', *, *, #62589, .T. ) ;
#34610 = ADVANCED_FACE ( 'NONE', ( #17502 ), #62511, .F. ) ;
#34611 = SURFACE_STYLE_FILL_AREA ( #54539 ) ;
#34612 = CYLINDRICAL_SURFACE ( 'NONE', #39201, 0.4999999999999998335 ) ;
#34613 = CARTESIAN_POINT ( 'NONE',  ( 8.027701659444428373, 5.080332885338247451, 8.330387188615796745 ) ) ;
#34614 = FACE_OUTER_BOUND ( 'NONE', #59347, .T. ) ;
#34615 = EDGE_CURVE ( 'NONE', #68689, #58024, #5878, .T. ) ;
#34616 = CARTESIAN_POINT ( 'NONE',  ( 17.88942345255911093, 3.118753088769705251, 12.20792418036210591 ) ) ;
#34617 = CARTESIAN_POINT ( 'NONE',  ( 18.26004861284300063, 2.925574202914999589, -11.93524904697000011 ) ) ;
#34618 = CARTESIAN_POINT ( 'NONE',  ( 11.20904666305999875, 5.937823941418000295, 7.147334722859000067 ) ) ;
#34619 = CARTESIAN_POINT ( 'NONE',  ( 9.346962924124627037, -3.158163127838481188, 7.261582451272839300 ) ) ;
#34620 = CARTESIAN_POINT ( 'NONE',  ( 8.797364180957998769, 3.929432544163579788, 6.524104241236299728 ) ) ;
#34621 = VERTEX_POINT ( 'NONE', #21278 ) ;
#34622 = CARTESIAN_POINT ( 'NONE',  ( 12.20034797952042105, -2.341680320747018484, 12.48707311375845208 ) ) ;
#34623 = CARTESIAN_POINT ( 'NONE',  ( 9.804975701332999449, -3.363922674822000136, -8.089163458558500608 ) ) ;
#34624 = CARTESIAN_POINT ( 'NONE',  ( 10.87148757351999961, 5.567567343464999929, 7.772413227960999649 ) ) ;
#34625 = CARTESIAN_POINT ( 'NONE',  ( 9.303275160948496492, 2.900329483618105719, 8.115397037630309285 ) ) ;
#34626 = CARTESIAN_POINT ( 'NONE',  ( 10.17764828895399809, 5.001141961424000471, -8.046814291299300592 ) ) ;
#34627 = CARTESIAN_POINT ( 'NONE',  ( 12.22381919988786869, 0.2299973361971391905, 12.69720198919503495 ) ) ;
#34628 = CARTESIAN_POINT ( 'NONE',  ( 8.700642219592999993, 5.212261578733999201, 6.157186134061999994 ) ) ;
#34629 = CARTESIAN_POINT ( 'NONE',  ( 10.99433665574000152, 3.697618584609999814, 5.729302299903000772 ) ) ;
#34630 = CARTESIAN_POINT ( 'NONE',  ( 12.48926758269842807, 1.960545016317334355, 12.56101064709213411 ) ) ;
#34631 = EDGE_CURVE ( 'NONE', #24517, #63941, #47513, .T. ) ;
#34632 = ORIENTED_EDGE ( 'NONE', *, *, #39622, .F. ) ;
#34633 = CARTESIAN_POINT ( 'NONE',  ( 9.743314158772999889, 5.149303692842000402, -5.987168472229000393 ) ) ;
#34634 = CARTESIAN_POINT ( 'NONE',  ( 10.49349279008999858, 3.667611644732699627, -8.734031750754999379 ) ) ;
#34635 = CARTESIAN_POINT ( 'NONE',  ( 10.81249950090998269, -4.268769985470544093, 9.219235902382948211 ) ) ;
#34637 = CARTESIAN_POINT ( 'NONE',  ( 24.66908053516780086, 11.82197461467616684, 3.190505267773458886 ) ) ;
#34636 = CARTESIAN_POINT ( 'NONE',  ( 7.555275273711000494, -4.314043295739000250, 8.819145559946001356 ) ) ;
#34638 = CARTESIAN_POINT ( 'NONE',  ( 10.41327973160900022, -3.909869487835140323, 8.500359330993999762 ) ) ;
#34639 = CIRCLE ( 'NONE', #45802, 1.000000000000000222 ) ;
#34640 = CARTESIAN_POINT ( 'NONE',  ( 11.11718313518939816, -4.622449961306399402, -8.287087605365499599 ) ) ;
#34641 = VERTEX_POINT ( 'NONE', #53783 ) ;
#34642 = B_SPLINE_CURVE_WITH_KNOTS ( 'NONE', 3,
 ( #47813, #54421, #17008, #21227, #64551, #32079, #5144, #5831, #38691, #26480, #1287, #42556, #59317, #60013, #12123, #43244 ),
 .UNSPECIFIED., .F., .F.,
 ( 4, 2, 2, 2, 2, 2, 2, 4 ),
 ( 0.000000000000000000, 0.06250000000000105471, 0.1250000000000021094, 0.2500000000000022204, 0.5000000000000011102, 0.7500000000000000000, 0.8750000000000000000, 1.000000000000000000 ),
 .UNSPECIFIED. ) ;
#34643 = CARTESIAN_POINT ( 'NONE',  ( 0.8286543026616000063, 3.368557921162000479, -0.6219103594335000373 ) ) ;
#34644 = CARTESIAN_POINT ( 'NONE',  ( 18.12548766259744326, -0.2560639956372497972, -12.69654133872746726 ) ) ;
#34645 = CYLINDRICAL_SURFACE ( 'NONE', #28538, 0.5000000000000002220 ) ;
#34646 = FACE_OUTER_BOUND ( 'NONE', #23397, .T. ) ;
#34647 = CARTESIAN_POINT ( 'NONE',  ( 7.000000000000000000, -1.065814103639999922E-14, 1.505462421391999793E-13 ) ) ;
#34648 = CARTESIAN_POINT ( 'NONE',  ( 4.900006121741999010, -2.000000000000000000, 0.000000000000000000 ) ) ;
#34649 = FACE_OUTER_BOUND ( 'NONE', #58895, .T. ) ;
#34650 = DIRECTION ( 'NONE',  ( 0.000000000000000000, -1.000000000000000000, 0.000000000000000000 ) ) ;
#34651 = CARTESIAN_POINT ( 'NONE',  ( 13.51587707751000167, -12.16770442808000041, -2.286102833273000012 ) ) ;
#34652 = ORIENTED_EDGE ( 'NONE', *, *, #13506, .T. ) ;
#34653 = CARTESIAN_POINT ( 'NONE',  ( 8.983795280412000039, 3.979464555644999901, 9.134076336209998814 ) ) ;
#34654 = CARTESIAN_POINT ( 'NONE',  ( 11.12983972095000063, 5.283814160399000315, 4.845726857105999485 ) ) ;
#34655 = CARTESIAN_POINT ( 'NONE',  ( 17.94172469452077223, 2.002341272942101291, -13.76666224251748893 ) ) ;
#34656 = CARTESIAN_POINT ( 'NONE',  ( 9.050000000000000711, 7.679126935408000065, -5.093340497782000043 ) ) ;
#34657 = CARTESIAN_POINT ( 'NONE',  ( 0.8325173737407000063, 2.980225901380999964, 1.319047437492999908 ) ) ;
#34658 = ORIENTED_EDGE ( 'NONE', *, *, #46844, .F. ) ;
#34659 = CARTESIAN_POINT ( 'NONE',  ( 1.834306799206333549, -1.762666431298145708, -3.058252359239904461 ) ) ;
#34660 = DIRECTION ( 'NONE',  ( -0.8660254037844289376, 0.000000000000000000, 0.5000000000000169864 ) ) ;
#34661 = CARTESIAN_POINT ( 'NONE',  ( 11.24053267693000002, 2.774035422596999645, 6.782113650547000105 ) ) ;
#34662 = CARTESIAN_POINT ( 'NONE',  ( 10.55103166480599874, 2.999015536536000504, 7.429424106427209296 ) ) ;
#34663 = CARTESIAN_POINT ( 'NONE',  ( 7.000000000000000000, 0.2708497377871000311, 3.000000000000000000 ) ) ;
#34664 = CARTESIAN_POINT ( 'NONE',  ( 10.27366694038000006, -3.065543393453000309, -8.487918777453998587 ) ) ;
#34665 = CARTESIAN_POINT ( 'NONE',  ( 12.80505043854143388, 1.760845406083386688, -12.47635457398814829 ) ) ;
#34666 = CARTESIAN_POINT ( 'NONE',  ( 9.678552719866329923, 4.965075498814901955, -8.480910291410426183 ) ) ;
#34667 = EDGE_CURVE ( 'NONE', #58783, #34762, #56666, .T. ) ;
#34668 = CARTESIAN_POINT ( 'NONE',  ( 12.21062133715901332, -2.693099985139989272, 12.40450382423467346 ) ) ;
#34669 = EDGE_CURVE ( 'NONE', #56202, #62522, #2608, .T. ) ;
#34670 = CARTESIAN_POINT ( 'NONE',  ( 8.472609142682756556, 2.304035199181565297, 7.029818754297329164 ) ) ;
#34671 = ORIENTED_EDGE ( 'NONE', *, *, #21002, .F. ) ;
#34672 = CARTESIAN_POINT ( 'NONE',  ( 17.91291100103723011, -1.987489628841895062, 13.76889314140747622 ) ) ;
#34673 = CARTESIAN_POINT ( 'NONE',  ( 7.800894426331000275, 3.218815461055000160, 6.398977422524000147 ) ) ;
#34674 = ORIENTED_EDGE ( 'NONE', *, *, #6090, .T. ) ;
#34675 = ORIENTED_EDGE ( 'NONE', *, *, #8133, .T. ) ;
#34676 = CARTESIAN_POINT ( 'NONE',  ( 24.44496356232399847, -3.224881240379999792, -12.03535804424000055 ) ) ;
#34677 = CARTESIAN_POINT ( 'NONE',  ( 9.698096873516668381, 4.327184855449106138, -6.282534154164607365 ) ) ;
#34678 = CIRCLE ( 'NONE', #52514, 13.89999856298999958 ) ;
#34679 = CARTESIAN_POINT ( 'NONE',  ( 9.721802827886667941, -2.874603711572091935, 6.749639981085449492 ) ) ;
#34680 = CARTESIAN_POINT ( 'NONE',  ( 11.25041981190000051, 5.730782764036999488, 8.122675980938000251 ) ) ;
#34681 = CARTESIAN_POINT ( 'NONE',  ( 10.72303311070000120, 3.890114357827999747, -8.859327677199999584 ) ) ;
#34682 = LINE ( 'NONE', #32345, #1861 ) ;
#34683 = CARTESIAN_POINT ( 'NONE',  ( 10.53733998880999856, -2.992814141720000265, 8.731692578598000409 ) ) ;
#34684 = CARTESIAN_POINT ( 'NONE',  ( 11.26444844843000048, 3.604811106221999850, -11.32703155999000089 ) ) ;
#34685 = LINE ( 'NONE', #51435, #12948 ) ;
#34686 = CARTESIAN_POINT ( 'NONE',  ( 11.58487348028854846, -4.882707455860599843, -7.977261354519500358 ) ) ;
#34687 = CARTESIAN_POINT ( 'NONE',  ( 10.70846056750539788, -2.938500698085303675, -5.066367099627377080 ) ) ;
#34688 = ORIENTED_EDGE ( 'NONE', *, *, #4563, .F. ) ;
#34689 = EDGE_CURVE ( 'NONE', #25967, #63987, #67468, .T. ) ;
#34690 = AXIS2_PLACEMENT_3D ( 'NONE', #27741, #28430, #1160 ) ;
#34691 = CARTESIAN_POINT ( 'NONE',  ( 0.5914240926529371611, -2.218416840111444355, -2.378158849281455822 ) ) ;
#34692 = DIRECTION ( 'NONE',  ( -0.7071067735209209948, -0.6115516217690190048, -0.3549713013083110047 ) ) ;
#34693 = ADVANCED_FACE ( 'NONE', ( #5540 ), #29434, .T. ) ;
#34694 = DIRECTION ( 'NONE',  ( 0.000000000000000000, -0.9928377162714321358, 0.1194707878476041485 ) ) ;
#34695 = CARTESIAN_POINT ( 'NONE',  ( 12.80505043854144276, -0.6951438842159390896, 13.94765567169528531 ) ) ;
#34696 = CARTESIAN_POINT ( 'NONE',  ( 12.33271654538601325, 2.090191715682863993, 13.75184336857263467 ) ) ;
#34697 = CARTESIAN_POINT ( 'NONE',  ( 10.00122642709000154, -2.274091010763000131, 7.851325450887000734 ) ) ;
#34698 = EDGE_LOOP ( 'NONE', ( #44751, #14910, #60098, #49039 ) ) ;
#34699 = CARTESIAN_POINT ( 'NONE',  ( 12.26182617413804365, 0.3097617570999572911, -12.69493148512597180 ) ) ;
#34700 = CARTESIAN_POINT ( 'NONE',  ( 12.61664971283087233, 0.7055305429986050703, 13.98221279804358019 ) ) ;
#34701 = VERTEX_POINT ( 'NONE', #42274 ) ;
#34702 = FACE_OUTER_BOUND ( 'NONE', #67477, .T. ) ;
#34703 = LINE ( 'NONE', #51793, #60519 ) ;
#34704 = FACE_OUTER_BOUND ( 'NONE', #66146, .T. ) ;
#34705 = CARTESIAN_POINT ( 'NONE',  ( 4.206309180874000297, -0.3613166205557999944, -1.589066327271000167 ) ) ;
#34706 = CARTESIAN_POINT ( 'NONE',  ( 8.781845775272032029, 3.294641396360323604, -8.705015079476726925 ) ) ;
#34707 = CARTESIAN_POINT ( 'NONE',  ( 10.93634361804999955, 8.767998367038000396, -6.465339435565999437 ) ) ;
#34708 = CARTESIAN_POINT ( 'NONE',  ( 0.1783234188636000084, -1.176389486124999939, 3.509795687408999942 ) ) ;
#34709 = CARTESIAN_POINT ( 'NONE',  ( 16.39999999347100257, 3.345256695718999751, 11.86066175541999890 ) ) ;
#34710 = CARTESIAN_POINT ( 'NONE',  ( 12.41985246593407766, 3.089908466900595396, 12.21525705840282150 ) ) ;
#34711 = CARTESIAN_POINT ( 'NONE',  ( 9.573320215454998561, -2.624754973437999794, -6.486841649805000110 ) ) ;
#34712 = CARTESIAN_POINT ( 'NONE',  ( 11.77359063708300013, 4.955772084214699724, -7.768721787835699999 ) ) ;
#34713 = CARTESIAN_POINT ( 'NONE',  ( 20.10000000000000142, -12.35000000006999876, 0.000000000000000000 ) ) ;
#34714 = B_SPLINE_CURVE_WITH_KNOTS ( 'NONE', 3,
 ( #27416, #22502, #54321, #44203 ),
 .UNSPECIFIED., .F., .F.,
 ( 4, 4 ),
 ( 0.000000000000000000, 1.000000000000000000 ),
 .UNSPECIFIED. ) ;
#34715 = CARTESIAN_POINT ( 'NONE',  ( 10.87273915876999908, 5.407616985330000681, -8.698399706473999515 ) ) ;
#34716 = CARTESIAN_POINT ( 'NONE',  ( 9.556659112603998807, 3.503852111758100296, -8.528383061402999843 ) ) ;
#34718 = CARTESIAN_POINT ( 'NONE',  ( 10.28638091290000034, -3.298456390694000095, 5.006422727232999748 ) ) ;
#34717 = CARTESIAN_POINT ( 'NONE',  ( 15.83887202961200025, -8.726161303169000405, -7.661206663860999910 ) ) ;
#34719 = DIRECTION ( 'NONE',  ( 0.000000000000000000, 0.000000000000000000, -1.000000000000000000 ) ) ;
#34720 = VERTEX_POINT ( 'NONE', #297 ) ;
#34721 = AXIS2_PLACEMENT_3D ( 'NONE', #44411, #1058, #54540 ) ;
#34722 = FACE_OUTER_BOUND ( 'NONE', #68839, .T. ) ;
#34723 = CARTESIAN_POINT ( 'NONE',  ( 10.55991645936999923, -5.094263939633999705, 6.075409946530999861 ) ) ;
#34724 = CARTESIAN_POINT ( 'NONE',  ( 9.756329965421999262, 3.302375896175799852, 6.777391592843399870 ) ) ;
#34725 = CARTESIAN_POINT ( 'NONE',  ( 10.87309687351627652, -5.217465845835394411, -7.172815144550898303 ) ) ;
#34726 = CIRCLE ( 'NONE', #53719, 13.17499999999999893 ) ;
#34727 = CARTESIAN_POINT ( 'NONE',  ( 10.37874387220000116, -4.882732524430000609, 6.350796477317000921 ) ) ;
#34728 = CARTESIAN_POINT ( 'NONE',  ( 12.43967993051476562, 3.007449918965190871, 13.55258931251708887 ) ) ;
#34729 = ORIENTED_EDGE ( 'NONE', *, *, #63373, .F. ) ;
#34730 = CARTESIAN_POINT ( 'NONE',  ( 10.01258376188599897, -4.962881317320600338, -8.113672563022399586 ) ) ;
#34731 = DIRECTION ( 'NONE',  ( 0.000000000000000000, 0.000000000000000000, 1.000000000000000000 ) ) ;
#34732 = CARTESIAN_POINT ( 'NONE',  ( 18.05438665931229636, 1.958444820271048270, -12.44686948166836338 ) ) ;
#34733 = CARTESIAN_POINT ( 'NONE',  ( 8.839582747487000347, -3.464784534403999139, -6.238107624440003107 ) ) ;
#34734 = CARTESIAN_POINT ( 'NONE',  ( 8.599999999999999645, -4.000000000000000000, -7.500000000000000000 ) ) ;
#34735 = CARTESIAN_POINT ( 'NONE',  ( 11.24025954179439957, 4.771812902496799680, -8.141292208271599051 ) ) ;
#34736 = CARTESIAN_POINT ( 'NONE',  ( 12.20625471193361911, 2.679103183902759699, -13.63384013640462911 ) ) ;
#34737 = CARTESIAN_POINT ( 'NONE',  ( 9.957251191599000961, -4.686746084135999801, -9.174865097765998456 ) ) ;
#34738 = CARTESIAN_POINT ( 'NONE',  ( 0.8530567992085708040, -2.798833948393629534, -2.150913519912204031 ) ) ;
#34739 = ORIENTED_EDGE ( 'NONE', *, *, #42251, .F. ) ;
#34740 = CARTESIAN_POINT ( 'NONE',  ( 17.92262925329511347, 1.881361389459298650, -13.87306285015964669 ) ) ;
#34741 = CARTESIAN_POINT ( 'NONE',  ( 12.10431174240585683, -0.1888260363403144737, -13.99874504378992590 ) ) ;
#34742 = CARTESIAN_POINT ( 'NONE',  ( 13.92975648157900004, -8.821327856274999490, -7.690719526968000430 ) ) ;
#34743 = EDGE_CURVE ( 'NONE', #36489, #9530, #68463, .T. ) ;
#34744 = CARTESIAN_POINT ( 'NONE',  ( 18.16413073598037187, -2.358269131811904007, -13.70246680370806835 ) ) ;
#34745 = EDGE_CURVE ( 'NONE', #4821, #21830, #51621, .T. ) ;
#34746 = CARTESIAN_POINT ( 'NONE',  ( 2.281685767831499234, -3.258006849854496512, -1.322661048612402412 ) ) ;
#34747 = CARTESIAN_POINT ( 'NONE',  ( 18.22958618736246095, -11.12724485990815282, 3.450621024319162622 ) ) ;
#34748 = CARTESIAN_POINT ( 'NONE',  ( 43.76123417800000226, 11.06886219213000011, -1.536526853569999851 ) ) ;
#34749 = ORIENTED_EDGE ( 'NONE', *, *, #39534, .T. ) ;
#34750 = EDGE_CURVE ( 'NONE', #30037, #59040, #19375, .T. ) ;
#34751 = CARTESIAN_POINT ( 'NONE',  ( 3.999999999999999112, 0.5626148410807583211, 2.094138670346520570 ) ) ;
#34752 = CARTESIAN_POINT ( 'NONE',  ( 17.93785022694513742, 2.005837716635007428, -13.76593133495255650 ) ) ;
#34753 = ORIENTED_EDGE ( 'NONE', *, *, #2019, .T. ) ;
#34754 = DIRECTION ( 'NONE',  ( 1.000000000000000000, 0.000000000000000000, 0.000000000000000000 ) ) ;
#34755 = CARTESIAN_POINT ( 'NONE',  ( 24.57709181747383909, 3.191966789821324646, 11.91258812936151479 ) ) ;
#34756 = CARTESIAN_POINT ( 'NONE',  ( 8.903895280414001689, 3.867331042029999999, -9.227339949050001877 ) ) ;
#34757 = CARTESIAN_POINT ( 'NONE',  ( 11.09999999999999964, -3.166318547749471080, -8.857024312923449827 ) ) ;
#34758 = CARTESIAN_POINT ( 'NONE',  ( 11.51656039236534923, -2.826501801118000312, -7.557111631074219460 ) ) ;
#34759 = CARTESIAN_POINT ( 'NONE',  ( 18.03350839574970266, 0.4021454017141842252, -12.69143011153355971 ) ) ;
#34760 = CONICAL_SURFACE ( 'NONE', #60401, 2.049966935984999683, 0.7853819979415218588 ) ;
#34761 = DIRECTION ( 'NONE',  ( -1.000000000000000000, 0.000000000000000000, 0.000000000000000000 ) ) ;
#34762 = VERTEX_POINT ( 'NONE', #60069 ) ;
#34763 = LINE ( 'NONE', #55738, #25380 ) ;
#34764 = CARTESIAN_POINT ( 'NONE',  ( 11.59999999999999964, -4.000000000000000000, -7.500000000000000000 ) ) ;
#34765 = CARTESIAN_POINT ( 'NONE',  ( 17.87143624847783130, -1.954798354107785796, 13.77413458886801934 ) ) ;
#34766 = ORIENTED_EDGE ( 'NONE', *, *, #55190, .T. ) ;
#34767 = CARTESIAN_POINT ( 'NONE',  ( 10.09453415443000068, 5.362844031509000686, -7.550030311027999375 ) ) ;
#34768 = CARTESIAN_POINT ( 'NONE',  ( 5.500000000000000000, 0.5415384615384001288, 2.132307692307999769 ) ) ;
#34769 = B_SPLINE_CURVE_WITH_KNOTS ( 'NONE', 3,
 ( #747, #26980, #399, #64354 ),
 .UNSPECIFIED., .F., .F.,
 ( 4, 4 ),
 ( 0.000000000000000000, 1.000000000000000000 ),
 .UNSPECIFIED. ) ;
#34770 = ORIENTED_EDGE ( 'NONE', *, *, #55884, .T. ) ;
#34771 = CARTESIAN_POINT ( 'NONE',  ( 9.632646554151000018, 4.552790318865400643, 6.500921769151600138 ) ) ;
#34772 = CARTESIAN_POINT ( 'NONE',  ( 18.10215020711902767, -2.952580169587739167, -12.24917755118609008 ) ) ;
#34773 = ADVANCED_FACE ( 'NONE', ( #18113 ), #10434, .T. ) ;
#34774 = CARTESIAN_POINT ( 'NONE',  ( 9.571013540182331525, 4.768183399968643599, 6.500416447002274722 ) ) ;
#34775 = CARTESIAN_POINT ( 'NONE',  ( 9.023148997459999876, 5.167567567567999731, -6.822293592207000934 ) ) ;
#34776 = AXIS2_PLACEMENT_3D ( 'NONE', #50071, #8456, #2858 ) ;
#34777 = CYLINDRICAL_SURFACE ( 'NONE', #16775, 0.5000000000000002220 ) ;
#34778 = CARTESIAN_POINT ( 'NONE',  ( 9.363635060566240398, -3.176852285862109770, 9.044600143522814051 ) ) ;
#34779 = VERTEX_POINT ( 'NONE', #64943 ) ;
#34780 = CARTESIAN_POINT ( 'NONE',  ( 11.60000000000000320, 3.125502297258556883, 7.130791426018634915 ) ) ;
#34781 = CARTESIAN_POINT ( 'NONE',  ( 11.35906500789999996, 2.719101288111000159, -7.157645240044000268 ) ) ;
#34782 = CARTESIAN_POINT ( 'NONE',  ( 8.736820887142258130, 3.746718250072767820, 6.641515014115457305 ) ) ;
#34783 = CARTESIAN_POINT ( 'NONE',  ( 12.30643338748584092, 1.987817336848021421, -13.85816184334709611 ) ) ;
#34784 = CARTESIAN_POINT ( 'NONE',  ( 9.431076168958000494, -4.649151400100800302, -8.602264418015000302 ) ) ;
#34785 = CARTESIAN_POINT ( 'NONE',  ( 10.43579701286999928, -2.587605342384000195, 6.390039770907999461 ) ) ;
#34786 = CARTESIAN_POINT ( 'NONE',  ( 18.18884185737634951, 0.3547769576528340130, 13.99550803169339730 ) ) ;
#34787 = CARTESIAN_POINT ( 'NONE',  ( 18.15916593610296559, -2.338515402807624710, 12.48776758576643964 ) ) ;
#34788 = ORIENTED_EDGE ( 'NONE', *, *, #61488, .F. ) ;
#34789 = ORIENTED_EDGE ( 'NONE', *, *, #1099, .F. ) ;
#34790 = CARTESIAN_POINT ( 'NONE',  ( 9.096889158776001238, 2.235961884443999459, -6.794506518623999902 ) ) ;
#34791 = DIRECTION ( 'NONE',  ( 1.000000000000000000, 0.000000000000000000, 0.000000000000000000 ) ) ;
#34792 = CARTESIAN_POINT ( 'NONE',  ( 12.18578014162844170, -2.585505937787686559, 13.65496065471434051 ) ) ;
#34793 = DIRECTION ( 'NONE',  ( -0.7071067811865475727, 0.7071067811865475727, 0.000000000000000000 ) ) ;
#34794 = CARTESIAN_POINT ( 'NONE',  ( 23.68315217816700269, 9.987916080909998939, -9.401273449222999901 ) ) ;
#34795 = CARTESIAN_POINT ( 'NONE',  ( 17.76427412810700091, -3.313981393620000215, -11.22406656470000108 ) ) ;
#34797 = CARTESIAN_POINT ( 'NONE',  ( 11.02039621389999979, -6.423930830464999353, 5.275616672426000520 ) ) ;
#34796 = CARTESIAN_POINT ( 'NONE',  ( 10.18235508232799980, -4.511005581663400044, 8.521081653687000212 ) ) ;
#34798 = CARTESIAN_POINT ( 'NONE',  ( 8.393929141338995592, -5.090180864267003003, -6.637945330154001233 ) ) ;
#34799 = ORIENTED_EDGE ( 'NONE', *, *, #17354, .F. ) ;
#34800 = DIRECTION ( 'NONE',  ( -0.8660254037844289376, -1.431232957501532063E-11, -0.5000000000000169864 ) ) ;
#34801 = CARTESIAN_POINT ( 'NONE',  ( 9.349204462308000174, 2.899999999999999911, -6.662590550603827211 ) ) ;
#34802 = ADVANCED_FACE ( 'NONE', ( #59715 ), #41314, .F. ) ;
#34803 = ADVANCED_FACE ( 'NONE', ( #59368 ), #43940, .F. ) ;
#34804 = CARTESIAN_POINT ( 'NONE',  ( 17.98256582722315144, 0.4560270868711856496, 12.68898073362800005 ) ) ;
#34805 = CARTESIAN_POINT ( 'NONE',  ( 12.23478064047700009, -0.2559538865579775724, 12.69653251248904979 ) ) ;
#34806 = CARTESIAN_POINT ( 'NONE',  ( 12.09999999999999964, -2.935681553670999921, 6.844464917182299324 ) ) ;
#34807 = ORIENTED_EDGE ( 'NONE', *, *, #67689, .F. ) ;
#34809 = CARTESIAN_POINT ( 'NONE',  ( 8.957462135714999718, 5.100000000000000533, -6.571291218949999902 ) ) ;
#34808 = CARTESIAN_POINT ( 'NONE',  ( 10.96882000591000050, -5.145193212282999973, 5.031654701678999864 ) ) ;
#34810 = CARTESIAN_POINT ( 'NONE',  ( 9.996404771875296191, 5.349457780298017440, 7.853068642099864327 ) ) ;
#34811 =( BOUNDED_SURFACE ( )  B_SPLINE_SURFACE ( 3, 3, ( 
 ( #6621, #54520, #27960, #32510 ),
 ( #49269, #11860, #65693, #28297 ),
 ( #60458, #49618, #60114, #26923 ),
 ( #44040, #65345, #21659, #64987 ) ),
 .UNSPECIFIED., .F., .F., .T. ) 
 B_SPLINE_SURFACE_WITH_KNOTS ( ( 4, 4 ),
 ( 4, 4 ),
 ( 0.000000000000000000, 1.000000000000000000 ),
 ( 0.000000000000000000, 1.000000000000000000 ),
 .UNSPECIFIED. ) 
 GEOMETRIC_REPRESENTATION_ITEM ( )  RATIONAL_B_SPLINE_SURFACE ( (
 ( 1.512182578520000042, 1.160176301760999840, 1.160176301760999840, 1.512182578520000042),
 ( 1.111288591041000196, 0.8526025270081000196, 0.8526025270081000196, 1.111288591041000196),
 ( 1.111288591041000196, 0.8526025270081000196, 0.8526025270081000196, 1.111288591041000196),
 ( 1.512182578520000042, 1.160176301760999840, 1.160176301760999840, 1.512182578520000042) ) ) 
 REPRESENTATION_ITEM ( '' )  SURFACE ( )  );
#34812 = DIRECTION ( 'NONE',  ( 1.000000000000000000, 0.000000000000000000, 0.000000000000000000 ) ) ;
#34813 = CARTESIAN_POINT ( 'NONE',  ( 10.07503300763299947, 4.881889043637199777, 6.575021251017499679 ) ) ;
#34814 = PRESENTATION_STYLE_ASSIGNMENT (( #23621 ) ) ;
#34815 = CARTESIAN_POINT ( 'NONE',  ( 9.337344653340027278, 3.744151942263672872, 9.232870615261292713 ) ) ;
#34816 = CARTESIAN_POINT ( 'NONE',  ( 3.315295232058000252, -3.344614842881000527, -1.715167582504999899 ) ) ;
#34817 = VERTEX_POINT ( 'NONE', #7614 ) ;
#34818 = CARTESIAN_POINT ( 'NONE',  ( 12.79307474260548538, 0.7192913015564709189, -12.57945229205062176 ) ) ;
#34820 = AXIS2_PLACEMENT_3D ( 'NONE', #38544, #59867, #11972 ) ;
#34819 = CARTESIAN_POINT ( 'NONE',  ( 11.96253286130404980, -3.661005694687299528, 8.308656198582323071 ) ) ;
#34821 = CARTESIAN_POINT ( 'NONE',  ( 11.08757144985999865, -2.712428550139000194, 6.571291218949999902 ) ) ;
#34822 = CARTESIAN_POINT ( 'NONE',  ( 24.53003472522700434, 3.319296498592000155, -12.04487452434999994 ) ) ;
#34823 = DIRECTION ( 'NONE',  ( 0.000000000000000000, -0.8646938284590766077, 0.5022992962614868384 ) ) ;
#34824 = ORIENTED_EDGE ( 'NONE', *, *, #30315, .F. ) ;
#34825 = CARTESIAN_POINT ( 'NONE',  ( 6.277891324327000255, 0.002616650692276999927, 1.322296913527999829 ) ) ;
#34826 = CARTESIAN_POINT ( 'NONE',  ( 7.142510841228999929, 5.086541985415000688, -8.378805615758999181 ) ) ;
#34827 = DIRECTION ( 'NONE',  ( -0.000000000000000000, -0.000000000000000000, 1.000000000000000000 ) ) ;
#34828 = CARTESIAN_POINT ( 'NONE',  ( 7.000000000000000000, 7.526486366024999874, 3.526486366024999874 ) ) ;
#34829 = CARTESIAN_POINT ( 'NONE',  ( 11.64122412107036908, 4.062069863985690255, -6.326756392227999015 ) ) ;
#34830 = EDGE_LOOP ( 'NONE', ( #30335, #50589, #45333, #60731 ) ) ;
#34831 = EDGE_CURVE ( 'NONE', #30840, #47368, #7419, .T. ) ;
#34832 = CARTESIAN_POINT ( 'NONE',  ( 9.479212726990999371, -4.071727350623000063, 9.089303488377000306 ) ) ;
#34833 = ORIENTED_EDGE ( 'NONE', *, *, #12499, .F. ) ;
#34834 = CARTESIAN_POINT ( 'NONE',  ( 16.39999999347100257, -3.345256695718999751, -11.86066175541999890 ) ) ;
#34835 = CARTESIAN_POINT ( 'NONE',  ( 8.175754440378000254, -2.599231861044000169, 7.909347897884000389 ) ) ;
#34836 = VECTOR ( 'NONE', #46291, 1000.000000000000000 ) ;
#34837 = CARTESIAN_POINT ( 'NONE',  ( 18.24183043734545961, 0.2342631834278595948, -13.99804438501501203 ) ) ;
#34838 = ORIENTED_EDGE ( 'NONE', *, *, #3103, .F. ) ;
#34839 = CARTESIAN_POINT ( 'NONE',  ( 10.98851211193927035, 7.849834481462382385, -6.454919206791046804 ) ) ;
#34840 = CARTESIAN_POINT ( 'NONE',  ( 23.85396356904521298, -9.637273725658499046, -9.713123508487292668 ) ) ;
#34841 = DIRECTION ( 'NONE',  ( 0.000000000000000000, -1.000000000000000000, 0.000000000000000000 ) ) ;
#34842 = CARTESIAN_POINT ( 'NONE',  ( 9.354346873516664829, -5.250000000000000000, -7.663624617374463099 ) ) ;
#34843 = DIRECTION ( 'NONE',  ( 0.000000000000000000, 1.000000000000000000, 0.000000000000000000 ) ) ;
#34844 = ORIENTED_EDGE ( 'NONE', *, *, #60659, .F. ) ;
#34845 = CARTESIAN_POINT ( 'NONE',  ( 2.011390132539708997, 3.499999999999998224, 0.4581489286485194157 ) ) ;
#34846 = CARTESIAN_POINT ( 'NONE',  ( 23.91242816463300258, -12.75285422775000121, -3.592234604002999987 ) ) ;
#34847 = CARTESIAN_POINT ( 'NONE',  ( 5.563359839683501562, -1.310679582531389498, 0.7554284705563444335 ) ) ;
#34848 = CARTESIAN_POINT ( 'NONE',  ( 4.000000000000000000, 0.000000000000000000, 0.000000000000000000 ) ) ;
#34849 = ORIENTED_EDGE ( 'NONE', *, *, #29570, .T. ) ;
#34850 = CARTESIAN_POINT ( 'NONE',  ( 10.47094409420000005, -5.100000000000000533, 6.571291218949999902 ) ) ;
#34851 = ADVANCED_FACE ( 'NONE', ( #32808 ), #24038, .T. ) ;
#34852 = CARTESIAN_POINT ( 'NONE',  ( 11.05391045180431675, 5.129049487418005704, -8.114538794791121390 ) ) ;
#34853 = CARTESIAN_POINT ( 'NONE',  ( 3.499999999999999556, 0.6014456285219068610, 3.255366668256093554 ) ) ;
#34854 = CARTESIAN_POINT ( 'NONE',  ( 9.909870477708999204, -5.250000000000000888, -7.750389189149368363 ) ) ;
#34855 = CARTESIAN_POINT ( 'NONE',  ( 6.799999045260999964, -9.295457794069999835, 5.399713664196000629 ) ) ;
#34856 = CARTESIAN_POINT ( 'NONE',  ( 12.39285819377765918, 0.4699225802676940122, -13.88930950616751225 ) ) ;
#34857 = CARTESIAN_POINT ( 'NONE',  ( 17.99286279921838982, -2.053846844283184758, 12.54442212638278775 ) ) ;
#34858 = ORIENTED_EDGE ( 'NONE', *, *, #2778, .F. ) ;
#34859 = CARTESIAN_POINT ( 'NONE',  ( 11.23589666366019912, -4.039600775206940497, -8.391246537305399045 ) ) ;
#34860 = ORIENTED_EDGE ( 'NONE', *, *, #42775, .F. ) ;
#34861 = CARTESIAN_POINT ( 'NONE',  ( 0.1499942179680000542, 2.199046806507070961, 1.689975037551098680 ) ) ;
#34862 = CARTESIAN_POINT ( 'NONE',  ( 9.187479719595000205, 2.391443348526999912, -6.856688371964000162 ) ) ;
#34863 = CARTESIAN_POINT ( 'NONE',  ( 3.125156541922999853, -0.09820418113198998988, -3.213551318459999973 ) ) ;
#34864 = CARTESIAN_POINT ( 'NONE',  ( 10.58996262057999971, -2.876743158681999812, -6.236533224899999617 ) ) ;
#34865 = CARTESIAN_POINT ( 'NONE',  ( 25.30000327618300204, -8.756202924575998026, -7.455126447192999883 ) ) ;
#34866 = CARTESIAN_POINT ( 'NONE',  ( 9.652022804587478078, -2.759070395092175332, -6.267057333003529074 ) ) ;
#34867 = B_SPLINE_CURVE_WITH_KNOTS ( 'NONE', 3,
 ( #57994, #10433, #4840, #47508 ),
 .UNSPECIFIED., .F., .F.,
 ( 4, 4 ),
 ( 0.000000000000000000, 1.000000000000000000 ),
 .UNSPECIFIED. ) ;
#34868 = B_SPLINE_CURVE_WITH_KNOTS ( 'NONE', 3,
 ( #52121, #57363, #18002, #62276, #28850, #1919 ),
 .UNSPECIFIED., .F., .F.,
 ( 4, 1, 1, 4 ),
 ( 0.000000000000000000, 0.2305484670070869491, 0.8346924774606477859, 1.000000000000000000 ),
 .UNSPECIFIED. ) ;
#34869 = EDGE_LOOP ( 'NONE', ( #24529, #65822, #62433, #68636, #2916, #21752, #42492, #30453, #62412, #1133, #9541, #28837, #60869, #21993, #39716, #38271, #10771 ) ) ;
#34870 = CARTESIAN_POINT ( 'NONE',  ( 11.36687616594229944, -4.344946439135400240, 8.587337146608000182 ) ) ;
#34871 = CARTESIAN_POINT ( 'NONE',  ( 9.075483283097998566, 4.020836891789999257, 8.948690653012000951 ) ) ;
#34872 = CARTESIAN_POINT ( 'NONE',  ( 24.44496412535000118, -8.810486166165000910, -8.810507954003998776 ) ) ;
#34873 = DIRECTION ( 'NONE',  ( 0.7071067811865474617, 0.7071067811865474617, -5.048527528662336139E-09 ) ) ;
#34875 = FACE_OUTER_BOUND ( 'NONE', #40564, .T. ) ;
#34874 = CARTESIAN_POINT ( 'NONE',  ( 9.538432183420001209, 5.620896541217999420, 7.423100299691999915 ) ) ;
#34876 = CARTESIAN_POINT ( 'NONE',  ( 11.67918044953561996, 5.011483761127000669, -8.027436060358800418 ) ) ;
#34877 = CARTESIAN_POINT ( 'NONE',  ( 10.97513183233909473, 2.816994567542234318, -6.653220807580209950 ) ) ;
#34878 = AXIS2_PLACEMENT_3D ( 'NONE', #43019, #64322, #16444 ) ;
#34879 = CARTESIAN_POINT ( 'NONE',  ( 9.832317406968998696, 4.186809223719299311, -8.486886322867700727 ) ) ;
#34880 = EDGE_CURVE ( 'NONE', #30625, #6314, #8307, .T. ) ;
#34881 = ADVANCED_FACE ( 'NONE', ( #29995 ), #12222, .F. ) ;
#34882 = CARTESIAN_POINT ( 'NONE',  ( 18.20001934199751759, -0.3287229608534071867, 12.59571550161850695 ) ) ;
#34883 = DIRECTION ( 'NONE',  ( -1.000000000000000000, 0.000000000000000000, 2.886579864060000134E-14 ) ) ;
#34884 = CARTESIAN_POINT ( 'NONE',  ( 0.9228735163577627132, 1.956520987066745931, -2.929226735302376206 ) ) ;
#34885 = DIRECTION ( 'NONE',  ( 0.000000000000000000, -0.9624505444715651947, 0.2714570858282905341 ) ) ;
#34886 = ORIENTED_EDGE ( 'NONE', *, *, #14369, .T. ) ;
#34887 = CARTESIAN_POINT ( 'NONE',  ( 7.731793146792000471, -4.580607464247000493, 9.213361409141999303 ) ) ;
#34888 = ADVANCED_FACE ( 'NONE', ( #61444 ), #13563, .F. ) ;
#34889 = ADVANCED_FACE ( 'NONE', ( #23694 ), #30324, .F. ) ;
#34890 = CARTESIAN_POINT ( 'NONE',  ( 17.72189171626099125, 1.806990214763249059, 13.88289628861100589 ) ) ;
#34891 = CARTESIAN_POINT ( 'NONE',  ( 10.34588779216199939, 4.801941500727100021, 7.210800365544999480 ) ) ;
#34892 = ORIENTED_EDGE ( 'NONE', *, *, #24564, .F. ) ;
#34893 = B_SPLINE_CURVE_WITH_KNOTS ( 'NONE', 3,
 ( #55421, #45281, #24637, #56449 ),
 .UNSPECIFIED., .F., .F.,
 ( 4, 4 ),
 ( 0.8746828543526545818, 1.000000000000000000 ),
 .UNSPECIFIED. ) ;
#34894 = CARTESIAN_POINT ( 'NONE',  ( 8.770176658772999900, 3.049618631524000367, 6.392542946894000266 ) ) ;
#34896 = CARTESIAN_POINT ( 'NONE',  ( 11.83003632436370012, 2.756744593645999775, 7.790336465152099876 ) ) ;
#34895 = CARTESIAN_POINT ( 'NONE',  ( 10.90453766415000025, -2.900310535872000273, -5.130381900875999435 ) ) ;
#34897 = CARTESIAN_POINT ( 'NONE',  ( 10.41838915877000105, 4.531912033713999755, -9.270484952459998595 ) ) ;
#34898 = ORIENTED_EDGE ( 'NONE', *, *, #44475, .F. ) ;
#34899 = CARTESIAN_POINT ( 'NONE',  ( 1.509306799207333460, 3.058252359239904905, -1.762666431298142600 ) ) ;
#34900 = CARTESIAN_POINT ( 'NONE',  ( 18.18935690068784794, -2.871730747427968300, -13.70230915895854018 ) ) ;
#34901 = CARTESIAN_POINT ( 'NONE',  ( 11.03918313518939875, 3.292400735470800033, 6.605241151424599444 ) ) ;
#34902 = CARTESIAN_POINT ( 'NONE',  ( 9.889844610056000462, -4.052276314598000084, 9.260527932809999641 ) ) ;
#34903 = CARTESIAN_POINT ( 'NONE',  ( 10.10000011340999926, -1.714184350020999865E-13, 8.687683754368000722E-14 ) ) ;
#34904 = VERTEX_POINT ( 'NONE', #7964 ) ;
#34905 = CARTESIAN_POINT ( 'NONE',  ( 11.64585080655600002, -3.555558855182999967, 11.95257446901999998 ) ) ;
#34906 = EDGE_CURVE ( 'NONE', #37994, #31995, #14067, .T. ) ;
#34907 = CARTESIAN_POINT ( 'NONE',  ( 10.06949314679000018, -4.910373174915999783, -8.649593977693999847 ) ) ;
#34908 = B_SPLINE_CURVE_WITH_KNOTS ( 'NONE', 3,
 ( #24968, #23339, #44682, #65974, #18102, #34184 ),
 .UNSPECIFIED., .F., .F.,
 ( 4, 2, 4 ),
 ( 0.3058164706682733325, 0.6529082353341366662, 1.000000000000000000 ),
 .UNSPECIFIED. ) ;
#34909 = CARTESIAN_POINT ( 'NONE',  ( 8.053293077950769430, -3.529150488797779595, 5.824254571415059978 ) ) ;
#34910 = CARTESIAN_POINT ( 'NONE',  ( 10.84168850528999961, -2.681008214828000114, 6.554752254946000889 ) ) ;
#34911 = CARTESIAN_POINT ( 'NONE',  ( 11.48011496860029901, -3.080230834057799960, -7.028661263734299780 ) ) ;
#34912 = CARTESIAN_POINT ( 'NONE',  ( 10.68988779216199880, -2.943881405003000218, 7.119137915499500480 ) ) ;
#34913 = EDGE_LOOP ( 'NONE', ( #30909, #5759, #30921, #34739, #19598, #14988, #58575, #46243, #21739, #46198, #38143, #61891 ) ) ;
#34915 = CARTESIAN_POINT ( 'NONE',  ( 10.32891567890999873, -4.769919575850000371, -4.571345007831999929 ) ) ;
#34914 = CIRCLE ( 'NONE', #39349, 12.59999999999999964 ) ;
#34916 = CARTESIAN_POINT ( 'NONE',  ( 11.07149279008999976, -4.296686446741600385, 6.398515879103999993 ) ) ;
#34917 = ORIENTED_EDGE ( 'NONE', *, *, #50752, .F. ) ;
#34918 = CARTESIAN_POINT ( 'NONE',  ( 1.775000508673000077, 0.000000000000000000, 0.000000000000000000 ) ) ;
#34919 = ORIENTED_EDGE ( 'NONE', *, *, #51796, .T. ) ;
#34920 = CARTESIAN_POINT ( 'NONE',  ( 9.754318513071000396, -2.462132291381999849, -7.373611177161000008 ) ) ;
#34921 = CARTESIAN_POINT ( 'NONE',  ( 8.754720280412998434, 5.687930027805999877, -7.109876198051000351 ) ) ;
#34922 = CARTESIAN_POINT ( 'NONE',  ( 11.38678751119029897, 2.833702563575000166, -8.110172976325500827 ) ) ;
#34923 = CARTESIAN_POINT ( 'NONE',  ( 10.90000000000000036, 2.899999999999999911, 6.414037451299000381 ) ) ;
#34924 = CARTESIAN_POINT ( 'NONE',  ( 12.37600679962888961, 2.954502784796254389, -12.33399089453511444 ) ) ;
#34925 = CARTESIAN_POINT ( 'NONE',  ( 11.37103032197929942, -3.416314376401300201, 8.316248703309600643 ) ) ;
#34926 = CARTESIAN_POINT ( 'NONE',  ( 7.501448341228000416, 2.138190256467000339, 6.814770510101999967 ) ) ;
#34927 = B_SPLINE_CURVE_WITH_KNOTS ( 'NONE', 3,
 ( #16345, #20216, #26853, #14972 ),
 .UNSPECIFIED., .F., .F.,
 ( 4, 4 ),
 ( 0.8746030603449276297, 1.000000000000000000 ),
 .UNSPECIFIED. ) ;
#34928 = ORIENTED_EDGE ( 'NONE', *, *, #58697, .F. ) ;
#34929 = CARTESIAN_POINT ( 'NONE',  ( 9.677263540183332680, 4.629523725463628558, 8.592232985442819881 ) ) ;
#34930 = CIRCLE ( 'NONE', #27083, 1.300000000000000044 ) ;
#34931 = CARTESIAN_POINT ( 'NONE',  ( 8.058769353207999586, -2.432121990576000314, 6.597519606637999523 ) ) ;
#34932 = CARTESIAN_POINT ( 'NONE',  ( 24.63332939992940140, -2.078227417246087505, 11.31065739920066804 ) ) ;
#34933 = EDGE_LOOP ( 'NONE', ( #68375, #12248, #41453, #43215, #46347, #36149, #10040, #56557 ) ) ;
#34934 = CARTESIAN_POINT ( 'NONE',  ( 12.22840029456390099, -2.917071392396663576, -12.25769309035714905 ) ) ;
#34935 = CARTESIAN_POINT ( 'NONE',  ( 11.62994988689359843, 4.518136976474400157, 6.483720595741000459 ) ) ;
#34936 = ADVANCED_FACE ( 'NONE', ( #62464 ), #40587, .T. ) ;
#34937 = CARTESIAN_POINT ( 'NONE',  ( 10.67529314679000052, -3.066674550532999977, -8.703235919197002346 ) ) ;
#34938 = CARTESIAN_POINT ( 'NONE',  ( 10.77101354018289925, 3.231816600031359066, 8.499583552997725278 ) ) ;
#34939 = CARTESIAN_POINT ( 'NONE',  ( 17.87616489729400371, -3.527537751923000009, -11.96092219328000006 ) ) ;
#34940 = CARTESIAN_POINT ( 'NONE',  ( 9.921464875192169686, 4.920967364567339963, -9.006643819163958398 ) ) ;
#34941 = CARTESIAN_POINT ( 'NONE',  ( 12.66131753640905266, -3.108595072584062091, -13.52531149670802968 ) ) ;
#34942 = CARTESIAN_POINT ( 'NONE',  ( 5.069075434514000555, -1.549422555689000003, -0.1585698209677000037 ) ) ;
#34943 = EDGE_CURVE ( 'NONE', #21223, #36042, #39076, .T. ) ;
#34944 = CARTESIAN_POINT ( 'NONE',  ( 11.44133594839949986, -3.430493414882899827, -6.847343244997600387 ) ) ;
#34945 = CARTESIAN_POINT ( 'NONE',  ( 11.15810538575740019, -2.757018958839999812, -7.202822423614300362 ) ) ;
#34946 = CARTESIAN_POINT ( 'NONE',  ( 17.70945903195350724, -3.183352579998545373, 12.19123751323113325 ) ) ;
#34947 = ORIENTED_EDGE ( 'NONE', *, *, #41232, .F. ) ;
#34948 = ORIENTED_EDGE ( 'NONE', *, *, #37253, .T. ) ;
#34949 =( NAMED_UNIT ( * ) PLANE_ANGLE_UNIT ( ) SI_UNIT ( $, .RADIAN. ) );
#34950 = CARTESIAN_POINT ( 'NONE',  ( 25.29987654162099986, 8.533547811387000692, 7.925584028117998336 ) ) ;
#34951 = CARTESIAN_POINT ( 'NONE',  ( 18.18005043832643963, 2.519786135693555806, 13.66921024419250763 ) ) ;
#34952 = CARTESIAN_POINT ( 'NONE',  ( 23.82002623614400250, -3.247612122070000051, 13.03939220338999938 ) ) ;
#34953 = CARTESIAN_POINT ( 'NONE',  ( 13.26247400726061976, 11.68416116973912366, 1.976808445614457677 ) ) ;
#34954 = CARTESIAN_POINT ( 'NONE',  ( 17.63760627221310173, 1.880133632725761172, 12.57457483776006768 ) ) ;
#34955 = DIRECTION ( 'NONE',  ( 0.000000000000000000, -0.9999606858717338120, 0.008867170401640296282 ) ) ;
#34956 = B_SPLINE_CURVE_WITH_KNOTS ( 'NONE', 3,
 ( #61370, #67975, #67624, #19750 ),
 .UNSPECIFIED., .F., .F.,
 ( 4, 4 ),
 ( 0.000000000000000000, 1.000000000000000000 ),
 .UNSPECIFIED. ) ;
#34957 = CARTESIAN_POINT ( 'NONE',  ( 11.15982925107999968, 5.578232410510000072, 8.067793621926998782 ) ) ;
#34958 = CARTESIAN_POINT ( 'NONE',  ( 10.26088874563355091, -3.646602187523998673, -8.814783671671618137 ) ) ;
#34959 = ORIENTED_EDGE ( 'NONE', *, *, #16906, .T. ) ;
#34960 = CARTESIAN_POINT ( 'NONE',  ( 12.20301641406255477, -2.331821773330018832, 12.48918929053770199 ) ) ;
#34961 = CARTESIAN_POINT ( 'NONE',  ( 9.427051052051998781, -3.014287398677499841, -7.692906630067099627 ) ) ;
#34962 = CARTESIAN_POINT ( 'NONE',  ( 9.701978494675000064, 3.399139198672999740, 6.026757051093999173 ) ) ;
#34963 = CARTESIAN_POINT ( 'NONE',  ( 8.158337970077000990E-06, 0.000000000000000000, 0.000000000000000000 ) ) ;
#34964 = B_SPLINE_SURFACE_WITH_KNOTS ( 'NONE', 3, 3, ( 
 ( #55913, #27965, #1730, #23049, #60463, #39486, #34248, #65699, #64993, #38443, #33207, #6627, #54872, #66389, #59766, #2086, #7318, #11867, #18164, #17822, #60809, #39136, #50322, #7668, #29015, #2420, #12225, #49275, #6974, #18512, #54525, #39834, #61156, #44046, #13273 ),
 ( #34600, #65351, #61834, #25118, #24092, #50665, #68096, #8702, #10666, #56252, #62173, #51006, #67072, #25458, #2766, #9033, #40508, #18853, #30045, #29705, #9365, #30711, #13953, #14969, #45425, #61496, #36292, #46790, #35279, #66734, #19185, #40180, #46104, #52021, #8359 ),
 ( #14296, #13614, #35624, #24777, #67749, #24438, #3106, #20213, #35951, #62514, #41539, #51348, #56937, #4122, #19874, #57612, #62851, #34937, #45764, #56595, #3440, #67410, #19534, #40853, #30374, #51682, #3780, #46450, #41204, #14633, #57265, #17293, #21841, #11016, #6105 ),
 ( #65176, #1218, #38975, #65524, #32013, #38620, #17652, #53327, #59941, #64479, #5427, #42832, #12052, #48077, #60293, #26767, #33385, #54701, #32689, #11695, #181, #16256, #37579, #37927, #59596, #21498, #54003, #38270, #64141, #58913, #22191, #33035, #16937, #59246, #54347 ) ),
 .UNSPECIFIED., .F., .F., .F.,
 ( 4, 4 ),
 ( 4, 1, 1, 1, 1, 1, 1, 1, 1, 1, 1, 1, 1, 1, 1, 1, 1, 1, 1, 1, 1, 1, 1, 1, 1, 1, 1, 1, 1, 1, 1, 1, 4 ),
 ( -0.1039086239011999951, 1.103908623900999864 ),
 ( 0.2233333333344000027, 0.2480800653604999795, 0.2728267973865999840, 0.2975735294126999886, 0.3223202614387999931, 0.3470669934649999733, 0.3718137254910999778, 0.3965604575171999824, 0.4213071895433000424, 0.4460539215694000470, 0.4708006535954999960, 0.4955473856216000006, 0.5202941176476999496, 0.5450408496738000652, 0.5697875816999000698, 0.5945343137260000743, 0.6192810457521999989, 0.6440277777783000035, 0.6687745098044000081, 0.6935212418305000126, 0.7182679738566000172, 0.7430147058827000217, 0.7677614379088000263, 0.7925081699349000308, 0.8172549019609999243, 0.8420016339870999289, 0.8667483660132000445, 0.8914950980394000801, 0.9162418300655000847, 0.9409885620915999782, 0.9657352941176999828, 0.9904820261437999873, 1.015228758169999912 ),
 .UNSPECIFIED. ) ;
#34965 = CARTESIAN_POINT ( 'NONE',  ( 10.32533997688000049, 4.243109097101799954, -6.385465081946999355 ) ) ;
#34966 = CARTESIAN_POINT ( 'NONE',  ( 12.20412026884455692, 0.1720826094844745413, 12.69843621396828226 ) ) ;
#34967 = AXIS2_PLACEMENT_3D ( 'NONE', #60239, #12342, #65467 ) ;
#34968 = CARTESIAN_POINT ( 'NONE',  ( 7.454676658771000497, 2.138190256467000339, 6.814770510101999967 ) ) ;
#34969 = CARTESIAN_POINT ( 'NONE',  ( 10.80815748598999981, 2.937526572573000205, 8.948458885032000154 ) ) ;
#34970 = CARTESIAN_POINT ( 'NONE',  ( 12.18180637322645055, 2.452078064253477407, 12.46259978693892556 ) ) ;
#34971 = ORIENTED_EDGE ( 'NONE', *, *, #62182, .T. ) ;
#34972 = CARTESIAN_POINT ( 'NONE',  ( 9.833904719592002408, 5.048004622677000341, -6.120508709481000231 ) ) ;
#34973 = CARTESIAN_POINT ( 'NONE',  ( 11.25656651104150008, 4.126085365637900182, -6.228222165170999247 ) ) ;
#34974 = EDGE_CURVE ( 'NONE', #2862, #48127, #34132, .T. ) ;
#34975 = ADVANCED_FACE ( 'NONE', ( #13221 ), #54636, .F. ) ;
#34976 = CARTESIAN_POINT ( 'NONE',  ( 10.89729545638381403, -2.607631909929567282, 8.596128993616638070 ) ) ;
#34978 = CARTESIAN_POINT ( 'NONE',  ( 24.73255498974337385, 11.75901231425727289, 3.190944228439685837 ) ) ;
#34977 = CARTESIAN_POINT ( 'NONE',  ( 9.138566940380000503, -2.933824946949000090, 8.496487880080000110 ) ) ;
#34979 = CARTESIAN_POINT ( 'NONE',  ( 9.233265421555000074, -4.162714371335800578, 6.658304367510099908 ) ) ;
#34980 = CARTESIAN_POINT ( 'NONE',  ( 11.33872066707849768, -3.141388196630700236, -6.980638253271099103 ) ) ;
#34981 = EDGE_LOOP ( 'NONE', ( #66450, #18692, #3594, #59487, #20632, #25888, #54224, #31817 ) ) ;
#34982 = AXIS2_PLACEMENT_3D ( 'NONE', #61236, #18590, #46188 ) ;
#34983 = CARTESIAN_POINT ( 'NONE',  ( 2.106520261437999864, 1.927138280259999892, 3.227152792068999965 ) ) ;
#34984 = CARTESIAN_POINT ( 'NONE',  ( 12.45488131765549511, 11.84188428343392552, -3.380847681379787417 ) ) ;
#34985 = AXIS2_PLACEMENT_3D ( 'NONE', #10330, #27807, #65531 ) ;
#34986 = CARTESIAN_POINT ( 'NONE',  ( 12.57536348658395831, -11.53887048480306632, 4.871543742293778401 ) ) ;
#34987 = DIRECTION ( 'NONE',  ( 0.8480635683784220058, 0.000000000000000000, -0.5298945026977139872 ) ) ;
#34988 = CARTESIAN_POINT ( 'NONE',  ( 9.903950872528001881, 5.205009505618999555, 6.747225973806000532 ) ) ;
#34989 = CARTESIAN_POINT ( 'NONE',  ( 15.75262483093262844, 8.754898706353550608, 7.686019545158286448 ) ) ;
#34990 = LINE ( 'NONE', #29410, #15189 ) ;
#34991 = DIRECTION ( 'NONE',  ( -0.000000000000000000, -0.000000000000000000, 1.000000000000000000 ) ) ;
#34992 = CARTESIAN_POINT ( 'NONE',  ( 8.977754440379998258, -2.019079883662000086, 7.390983468784999566 ) ) ;
#34993 = ORIENTED_EDGE ( 'NONE', *, *, #53040, .T. ) ;
#34994 = CARTESIAN_POINT ( 'NONE',  ( 8.919607780412000864, 5.165497731316000873, 8.645531386060000045 ) ) ;
#34995 = EDGE_CURVE ( 'NONE', #32140, #40775, #40801, .T. ) ;
#34996 = CARTESIAN_POINT ( 'NONE',  ( 5.500000000000000000, 0.000000000000000000, 0.000000000000000000 ) ) ;
#34997 = CARTESIAN_POINT ( 'NONE',  ( 7.428154886651814337, -2.321820467422959666, 7.962693524187518079 ) ) ;
#34998 = CARTESIAN_POINT ( 'NONE',  ( 17.88386803574400830, -0.5319881936462144134, 13.88630234897559035 ) ) ;
#34999 = CARTESIAN_POINT ( 'NONE',  ( 1.266428256771000127, 2.565043520226999885, 2.270544068615000022 ) ) ;
#35000 = ORIENTED_EDGE ( 'NONE', *, *, #7177, .T. ) ;
#35001 = FACE_OUTER_BOUND ( 'NONE', #61930, .T. ) ;
#35002 = CARTESIAN_POINT ( 'NONE',  ( 13.50003721581400029, -9.159934378815998812, -7.517910889891000537 ) ) ;
#35003 = CARTESIAN_POINT ( 'NONE',  ( 11.09999999999999964, -2.274006712557999688, -7.281956340829000673 ) ) ;
#35004 = CARTESIAN_POINT ( 'NONE',  ( 9.590596677641999079, 2.445964682955000136, 7.841184989245001624 ) ) ;
#35005 = CARTESIAN_POINT ( 'NONE',  ( 11.26487482311540056, 4.930401445321599851, 7.124095752359899336 ) ) ;
#35006 = B_SPLINE_CURVE_WITH_KNOTS ( 'NONE', 3,
 ( #45876, #24553, #67186, #3897, #41318 ),
 .UNSPECIFIED., .F., .F.,
 ( 4, 1, 4 ),
 ( 0.000000000000000000, 0.5000000000000000000, 1.000000000000000000 ),
 .UNSPECIFIED. ) ;
#35007 = DIRECTION ( 'NONE',  ( 1.000000000000000000, 0.000000000000000000, 0.000000000000000000 ) ) ;
#35008 = CARTESIAN_POINT ( 'NONE',  ( 10.99305444037999990, -4.495427106425000652, -6.233607450113000326 ) ) ;
#35009 = CARTESIAN_POINT ( 'NONE',  ( 4.625859839682417984, -1.460959015002473382, -0.3926218265389205819 ) ) ;
#35010 = CARTESIAN_POINT ( 'NONE',  ( 18.49562053141631779, 2.998066116905866441, -12.16097201970168307 ) ) ;
#35011 = CARTESIAN_POINT ( 'NONE',  ( 12.37651575366414924, -2.955073904877951296, 12.33383124654599072 ) ) ;
#35012 = AXIS2_PLACEMENT_3D ( 'NONE', #64475, #58909, #38617 ) ;
#35013 = CARTESIAN_POINT ( 'NONE',  ( 7.632009264042212138, 5.138780499484131070, 6.167916169763508094 ) ) ;
#35014 = EDGE_LOOP ( 'NONE', ( #22590, #14941, #57587, #27197 ) ) ;
#35015 = AXIS2_PLACEMENT_3D ( 'NONE', #57644, #53443, #58335 ) ;
#35016 = CARTESIAN_POINT ( 'NONE',  ( 17.94601859325910098, -2.012274714637017681, 13.76488447091686496 ) ) ;
#35017 = DIRECTION ( 'NONE',  ( 0.000000000000000000, 1.000000000000000000, 0.000000000000000000 ) ) ;
#35018 = ORIENTED_EDGE ( 'NONE', *, *, #21482, .T. ) ;
#35019 = ORIENTED_EDGE ( 'NONE', *, *, #31447, .F. ) ;
#35020 = CARTESIAN_POINT ( 'NONE',  ( 18.50003594167399967, 2.686563651857999613, 11.33603604486000016 ) ) ;
#35021 = CARTESIAN_POINT ( 'NONE',  ( 44.24148000000000280, 2.258942858049999725, 12.29419282279000036 ) ) ;
#35022 = DIRECTION ( 'NONE',  ( 0.000000000000000000, 0.9421243786071877846, 0.3352635608502959608 ) ) ;
#35023 = CARTESIAN_POINT ( 'NONE',  ( 9.877261637240000169, 2.207988120125000009, 7.624813826992999921 ) ) ;
#35024 = CARTESIAN_POINT ( 'NONE',  ( 11.00000000000000000, -2.799999999999999822, 5.865766984179000332 ) ) ;
#35025 = FACE_OUTER_BOUND ( 'NONE', #50989, .T. ) ;
#35026 = CARTESIAN_POINT ( 'NONE',  ( 10.40516264833000015, -5.216401621862000404, 6.765753642936999768 ) ) ;
#35027 = CARTESIAN_POINT ( 'NONE',  ( 18.26845433917840822, -0.1286734328892429335, -12.59934825840596773 ) ) ;
#35028 = EDGE_CURVE ( 'NONE', #10153, #35633, #65122, .T. ) ;
#35029 = CARTESIAN_POINT ( 'NONE',  ( 10.64126772939999910, -2.258710642251000156, -6.863482599505999815 ) ) ;
#35030 = CARTESIAN_POINT ( 'NONE',  ( 11.53564291764652872, -4.995889373412399692, -7.376893506359599506 ) ) ;
#35031 = DIRECTION ( 'NONE',  ( 1.000000000000000000, 0.000000000000000000, 0.000000000000000000 ) ) ;
#35032 = VERTEX_POINT ( 'NONE', #32390 ) ;
#35033 = AXIS2_PLACEMENT_3D ( 'NONE', #64482, #33038, #54350 ) ;
#35034 = CARTESIAN_POINT ( 'NONE',  ( 10.96866170142999941, -6.476647493854999382, -5.207916108537000710 ) ) ;
#35035 = DIRECTION ( 'NONE',  ( 0.000000000000000000, 1.000000000000000000, 0.000000000000000000 ) ) ;
#35036 = B_SPLINE_CURVE_WITH_KNOTS ( 'NONE', 3,
 ( #59380, #32821, #54486, #6586 ),
 .UNSPECIFIED., .F., .F.,
 ( 4, 4 ),
 ( 0.000000000000000000, 1.000000000000000000 ),
 .UNSPECIFIED. ) ;
#35037 = CARTESIAN_POINT ( 'NONE',  ( 8.929547492598356229, 4.733899445644309978, 6.695580748437408580 ) ) ;
#35038 = CARTESIAN_POINT ( 'NONE',  ( 9.101797255588000013, 5.278067516796999925, -7.445890648716809501 ) ) ;
#35039 = CARTESIAN_POINT ( 'NONE',  ( 12.25828482332352820, 2.997587547359421123, 13.67532635696712440 ) ) ;
#35040 = CARTESIAN_POINT ( 'NONE',  ( 9.500008250440000523, -2.279684233303000074, 7.877691491255999878 ) ) ;
#35041 = ORIENTED_EDGE ( 'NONE', *, *, #3463, .F. ) ;
#35042 = CARTESIAN_POINT ( 'NONE',  ( 12.18394763206765852, 0.08111188053566398271, -12.69973954613554135 ) ) ;
#35043 = CARTESIAN_POINT ( 'NONE',  ( 12.68599131528412371, 0.7206971133477456659, 13.98143832535762954 ) ) ;
#35044 = EDGE_LOOP ( 'NONE', ( #31085, #809, #35373 ) ) ;
#35045 = DIRECTION ( 'NONE',  ( -1.000000000000000000, 0.000000000000000000, 0.000000000000000000 ) ) ;
#35046 = CARTESIAN_POINT ( 'NONE',  ( 12.80505043854144276, -0.6564304467897670303, 12.64601024127357931 ) ) ;
#35047 = B_SPLINE_CURVE_WITH_KNOTS ( 'NONE', 3,
 ( #6131, #22904, #54728, #59626 ),
 .UNSPECIFIED., .F., .F.,
 ( 4, 4 ),
 ( 0.000000000000000000, 1.000000000000000000 ),
 .UNSPECIFIED. ) ;
#35048 = CARTESIAN_POINT ( 'NONE',  ( 23.52033604279600354, -3.098099968686999883, -13.78446056569000078 ) ) ;
#35049 = CARTESIAN_POINT ( 'NONE',  ( 4.599999999999999645, 0.7192913403693023122, 12.57945229203838267 ) ) ;
#35050 = CARTESIAN_POINT ( 'NONE',  ( 8.933148997457999840, -5.167567567567999731, 6.822293592207000934 ) ) ;
#35051 = CARTESIAN_POINT ( 'NONE',  ( 0.4334425577436000210, -2.413104819777999843, -2.586865767356999690 ) ) ;
#35052 = CARTESIAN_POINT ( 'NONE',  ( 9.020964430773000586, 2.907392932634000005, 6.146188468825999784 ) ) ;
#35053 = CARTESIAN_POINT ( 'NONE',  ( 12.44013165738121884, 3.102068138921894036, 12.21217476962502246 ) ) ;
#35054 = CARTESIAN_POINT ( 'NONE',  ( 9.776078604427999252, -4.565692099013000771, -8.879633571423999783 ) ) ;
#35055 = CARTESIAN_POINT ( 'NONE',  ( 11.17056785386839834, 3.281375110759499947, -7.983608166707499620 ) ) ;
#35056 = DIRECTION ( 'NONE',  ( 0.000000000000000000, -1.000000000000000000, 0.000000000000000000 ) ) ;
#35057 = EDGE_CURVE ( 'NONE', #45349, #65308, #49514, .T. ) ;
#35058 = AXIS2_PLACEMENT_3D ( 'NONE', #54377, #64855, #36934 ) ;
#35059 = EDGE_CURVE ( 'NONE', #13225, #29696, #64060, .T. ) ;
#35060 = CARTESIAN_POINT ( 'NONE',  ( 11.19434208742519843, 3.521141233577200325, -8.252717006421999457 ) ) ;
#35061 = CARTESIAN_POINT ( 'NONE',  ( 9.126063610504999701, 4.468346739194200445, -8.541338455964998744 ) ) ;
#35063 = CARTESIAN_POINT ( 'NONE',  ( 12.18124154974186801, 2.460017072603256860, 12.46078795775544812 ) ) ;
#35062 = CARTESIAN_POINT ( 'NONE',  ( 16.13712493497300215, -8.294738329384999886, -8.125890082391000746 ) ) ;
#35064 = CARTESIAN_POINT ( 'NONE',  ( 11.09999999999999964, 4.000000000000000000, -7.500000000000000000 ) ) ;
#35065 = EDGE_LOOP ( 'NONE', ( #61628, #49534, #50768, #49308, #35041, #46068, #28542, #50700, #29522, #49432 ) ) ;
#35066 = VECTOR ( 'NONE', #8631, 1000.000000000000114 ) ;
#35067 = CARTESIAN_POINT ( 'NONE',  ( 11.36056039236529891, 4.891071240644300211, 7.456633480985620288 ) ) ;
#35068 = CARTESIAN_POINT ( 'NONE',  ( 10.03491210303999992, -5.615910465798999773, 7.351455544018000943 ) ) ;
#35069 = CARTESIAN_POINT ( 'NONE',  ( 9.302417874593999159, 2.949199072237000063, 7.053287723251499663 ) ) ;
#35070 = CARTESIAN_POINT ( 'NONE',  ( 8.821633776942626071, 4.724939341952408611, -7.989893149673591211 ) ) ;
#35071 = CARTESIAN_POINT ( 'NONE',  ( 23.56666365135700403, 11.16210620489000327, -3.571147223011999827 ) ) ;
#35072 = CARTESIAN_POINT ( 'NONE',  ( 12.34838569214080550, 2.927120983257067710, 13.57349088381402247 ) ) ;
#35073 = CARTESIAN_POINT ( 'NONE',  ( 24.35365242081699932, 8.948887819865001703, -8.923422014301001681 ) ) ;
#35074 = ORIENTED_EDGE ( 'NONE', *, *, #489, .T. ) ;
#35075 = EDGE_CURVE ( 'NONE', #44229, #7255, #26574, .T. ) ;
#35076 = AXIS2_PLACEMENT_3D ( 'NONE', #12816, #50217, #28555 ) ;
#35077 = CARTESIAN_POINT ( 'NONE',  ( 8.670138961223999630, -3.053949131563199693, -8.139313957553699908 ) ) ;
#35078 = DIRECTION ( 'NONE',  ( -1.000000000000000000, 0.000000000000000000, 0.000000000000000000 ) ) ;
#35079 = EDGE_CURVE ( 'NONE', #26809, #45133, #21602, .T. ) ;
#35080 = CARTESIAN_POINT ( 'NONE',  ( 17.94181191902910655, 1.871597878487315292, -12.46022310877026662 ) ) ;
#35081 = CARTESIAN_POINT ( 'NONE',  ( 2.542640132542666631, 3.058252359239899132, 1.762666431298154146 ) ) ;
#35082 = AXIS2_PLACEMENT_3D ( 'NONE', #6783, #12734, #23906 ) ;
#35083 = DIRECTION ( 'NONE',  ( 0.7071067811865475727, 0.7071067811865475727, 0.000000000000000000 ) ) ;
#35084 = B_SPLINE_CURVE_WITH_KNOTS ( 'NONE', 3,
 ( #20179, #46415, #15627, #51985, #41506, #67716, #41172, #9333, #62479, #36958, #25772, #58272, #14599, #47104, #63156, #10375 ),
 .UNSPECIFIED., .F., .F.,
 ( 4, 2, 2, 2, 2, 2, 2, 4 ),
 ( 0.000000000000000000, 0.06250000000000126288, 0.1250000000000025258, 0.2500000000000006106, 0.4999999999999993339, 0.7499999999999980016, 0.8749999999999990008, 1.000000000000000000 ),
 .UNSPECIFIED. ) ;
#35085 = CARTESIAN_POINT ( 'NONE',  ( 12.19113298428035996, 2.617185168768731529, -13.64790684748345839 ) ) ;
#35086 = CARTESIAN_POINT ( 'NONE',  ( 9.348145925901000908, -2.626678530444999993, -7.387134320497999340 ) ) ;
#35087 = DIRECTION ( 'NONE',  ( 0.000000000000000000, -0.000000000000000000, 1.000000000000000000 ) ) ;
#35088 = VERTEX_POINT ( 'NONE', #43564 ) ;
#35089 = DIRECTION ( 'NONE',  ( 0.7071067796723968790, 0.6140599801297969007, -0.3506142366537984834 ) ) ;
#35090 = CIRCLE ( 'NONE', #44016, 12.42499880353999941 ) ;
#35091 = CARTESIAN_POINT ( 'NONE',  ( 12.08965255773059155, 0.1190513140356027066, -13.99949878896183719 ) ) ;
#35092 = CARTESIAN_POINT ( 'NONE',  ( 23.65249378741842534, 13.39790967320782045, 3.829259155508669021 ) ) ;
#35093 = FACE_OUTER_BOUND ( 'NONE', #35174, .T. ) ;
#35094 = CARTESIAN_POINT ( 'NONE',  ( 21.05000072320139992, -1.355183834107999921E-13, -12.47499939739999064 ) ) ;
#35095 = CARTESIAN_POINT ( 'NONE',  ( 23.60000000000000142, -12.92130526834925242, -5.202888421357703130 ) ) ;
#35096 = CARTESIAN_POINT ( 'NONE',  ( 1.700000000000000178, 1.500000000000000000, 0.000000000000000000 ) ) ;
#35097 = EDGE_LOOP ( 'NONE', ( #32823, #39390, #6895, #62286, #65770 ) ) ;
#35098 = CARTESIAN_POINT ( 'NONE',  ( 4.000000000000000000, 2.136325177875821435, 0.2822470469891264488 ) ) ;
#35099 = CARTESIAN_POINT ( 'NONE',  ( 17.87817017025372834, 1.864246049947063666, -13.87532391830906420 ) ) ;
#35100 = ORIENTED_EDGE ( 'NONE', *, *, #21219, .F. ) ;
#35101 = CARTESIAN_POINT ( 'NONE',  ( 9.883380199233998908, -3.139757597894699881, 7.608124715612800237 ) ) ;
#35102 = CARTESIAN_POINT ( 'NONE',  ( 6.899999691988000450, -12.20988339176000004, -3.111064831550000243 ) ) ;
#35103 = CARTESIAN_POINT ( 'NONE',  ( 8.664129719593997692, 5.524776413195999325, -7.147585171405999915 ) ) ;
#35104 = CARTESIAN_POINT ( 'NONE',  ( 11.09999999999999964, -3.512324525112999751, -8.971282648301999174 ) ) ;
#35105 = CARTESIAN_POINT ( 'NONE',  ( 10.77368717260499942, -4.539928529895099985, -8.381256426168800289 ) ) ;
#35106 = CARTESIAN_POINT ( 'NONE',  ( 18.02496081238558645, 0.4121104636170003777, -12.69099970358804086 ) ) ;
#35107 = CARTESIAN_POINT ( 'NONE',  ( 12.09999999999999964, -5.499854772664000357, 7.174999999999999822 ) ) ;
#35108 = VERTEX_POINT ( 'NONE', #7192 ) ;
#35109 = CARTESIAN_POINT ( 'NONE',  ( 8.883148997460001084, 5.167567567567999731, 6.822293592207000934 ) ) ;
#35110 = CARTESIAN_POINT ( 'NONE',  ( 7.325000000000000178, 4.000000000000000000, 9.239711431703000244 ) ) ;
#35111 = CARTESIAN_POINT ( 'NONE',  ( 6.899999691988000450, 0.000000000000000000, 0.000000000000000000 ) ) ;
#35112 = ORIENTED_EDGE ( 'NONE', *, *, #6293, .T. ) ;
#35113 = AXIS2_PLACEMENT_3D ( 'NONE', #38564, #49749, #2209 ) ;
#35114 = CARTESIAN_POINT ( 'NONE',  ( 10.68375192593000023, 4.547306763790999184, -8.749120576764999768 ) ) ;
#35115 = DIRECTION ( 'NONE',  ( 0.000000000000000000, -1.000000000000000000, 0.000000000000000000 ) ) ;
#35116 = ORIENTED_EDGE ( 'NONE', *, *, #58305, .T. ) ;
#35117 = CARTESIAN_POINT ( 'NONE',  ( 8.847442991499999465, 3.928121959910110483, 8.639547276484998761 ) ) ;
#35118 = CARTESIAN_POINT ( 'NONE',  ( 18.10356236467040958, -2.200227019994205779, -12.51636715934673383 ) ) ;
#35119 = PRODUCT_DEFINITION ( 'UNKNOWN', '', #566, #63240 ) ;
#35120 = CARTESIAN_POINT ( 'NONE',  ( 21.00000000000000000, 0.000000000000000000, 0.000000000000000000 ) ) ;
#35121 = CARTESIAN_POINT ( 'NONE',  ( 24.41555930013399944, -12.00270549100999951, -3.255728780632000330 ) ) ;
#35122 = CARTESIAN_POINT ( 'NONE',  ( 9.501882463939899992, -2.610834736344150642, 6.433711780408752468 ) ) ;
#35123 = ORIENTED_EDGE ( 'NONE', *, *, #62427, .T. ) ;
#35124 = DIRECTION ( 'NONE',  ( 0.000000000000000000, 0.9553735099700839672, 0.2954005017724949389 ) ) ;
#35125 = CARTESIAN_POINT ( 'NONE',  ( 9.838376522720714945, -5.764887630754955694, -7.468471882345152579 ) ) ;
#35126 = CARTESIAN_POINT ( 'NONE',  ( 10.95934799724999920, -5.155594434375000645, -5.120697376301999171 ) ) ;
#35127 = CARTESIAN_POINT ( 'NONE',  ( 12.13805290469195874, 2.231685852207990095, -13.82098778992225441 ) ) ;
#35128 = CARTESIAN_POINT ( 'NONE',  ( 9.960975701332998256, -3.162316589966200020, -8.275900091855099561 ) ) ;
#35129 = CARTESIAN_POINT ( 'NONE',  ( 9.166075977534999808, -4.023333687735000552, 9.122281080215000060 ) ) ;
#35130 = DIRECTION ( 'NONE',  ( 1.000000000000000000, 0.000000000000000000, 0.000000000000000000 ) ) ;
#35131 = AXIS2_PLACEMENT_3D ( 'NONE', #19339, #23901, #19692 ) ;
#35132 = CARTESIAN_POINT ( 'NONE',  ( 7.840808840898988663, 5.014465085856414817, 6.545777694986461448 ) ) ;
#35133 = ORIENTED_EDGE ( 'NONE', *, *, #11866, .F. ) ;
#35134 = ORIENTED_EDGE ( 'NONE', *, *, #63072, .F. ) ;
#35135 = CARTESIAN_POINT ( 'NONE',  ( 9.965360841230999966, 4.034680274230000308, -6.102912434217000026 ) ) ;
#35136 = CARTESIAN_POINT ( 'NONE',  ( 7.000000000000000000, 0.3230303992915000144, 3.000000000000000000 ) ) ;
#35137 = CARTESIAN_POINT ( 'NONE',  ( 12.18233509006626214, -2.554099910185274602, 13.66183974825599279 ) ) ;
#35138 = CARTESIAN_POINT ( 'NONE',  ( 25.47110272103000028, 8.417196128994998361, -7.979950812399000171 ) ) ;
#35139 = EDGE_CURVE ( 'NONE', #25073, #33524, #46635, .T. ) ;
#35140 = EDGE_CURVE ( 'NONE', #63126, #16649, #16637, .T. ) ;
#35141 = CARTESIAN_POINT ( 'NONE',  ( 23.52062617334100025, 10.38635790624000066, -9.577244370524999439 ) ) ;
#35142 = CARTESIAN_POINT ( 'NONE',  ( 17.79518154839200150, -3.190852234727000081, -11.45040960482999814 ) ) ;
#35144 = CARTESIAN_POINT ( 'NONE',  ( 8.709994373423086245, 5.736668034480788769, 7.709616018064762599 ) ) ;
#35143 = CARTESIAN_POINT ( 'NONE',  ( 10.53696314287999947, -2.882742046518000034, 7.735518817439499983 ) ) ;
#35145 = CARTESIAN_POINT ( 'NONE',  ( 8.853612782865001307, -4.539814389745004952, -6.225821853175999010 ) ) ;
#35146 = ORIENTED_EDGE ( 'NONE', *, *, #33486, .F. ) ;
#35147 = CARTESIAN_POINT ( 'NONE',  ( 7.419155789456778116, 3.646555675397749940, -6.184975449998299624 ) ) ;
#35148 = CARTESIAN_POINT ( 'NONE',  ( 8.199995110659001440, -2.894508759333000114, 6.645190873281999089 ) ) ;
#35149 = CARTESIAN_POINT ( 'NONE',  ( 9.976909913808000852, -4.233164088428999605, -6.141918726850000176 ) ) ;
#35150 = CARTESIAN_POINT ( 'NONE',  ( 18.09667132770092834, 0.3125562302819395732, 12.69484091569602668 ) ) ;
#35151 = CARTESIAN_POINT ( 'NONE',  ( 18.17924748726904838, -2.534358940396702842, -12.44349985638940304 ) ) ;
#35152 = CARTESIAN_POINT ( 'NONE',  ( 3.899999503719000060, 0.000000000000000000, 0.000000000000000000 ) ) ;
#35153 = CARTESIAN_POINT ( 'NONE',  ( 9.193385841233000733, 2.981992329588000423, -5.895876591910999664 ) ) ;
#35154 = CARTESIAN_POINT ( 'NONE',  ( 10.91195257254739914, 2.772832764353999835, 7.143100915737699452 ) ) ;
#35155 = AXIS2_PLACEMENT_3D ( 'NONE', #41178, #25091, #36617 ) ;
#35156 = B_SPLINE_CURVE_WITH_KNOTS ( 'NONE', 3,
 ( #10540, #42372, #37121, #26289, #68229, #9855, #15106, #31883, #25599, #46925 ),
 .UNSPECIFIED., .F., .F.,
 ( 4, 2, 2, 2, 4 ),
 ( 0.000000000000000000, 0.2500000000000029976, 0.3750000000000044964, 0.5000000000000059952, 1.000000000000000000 ),
 .UNSPECIFIED. ) ;
#35157 = B_SPLINE_SURFACE_WITH_KNOTS ( 'NONE', 1, 3, ( 
 ( #36608, #21211, #10030, #31369, #47797, #42541, #53377, #21891, #43228, #32061, #582, #69105, #58615, #52681, #10714, #4777, #64532, #59298, #11402, #26117, #43578, #27495, #13154, #2306, #49157, #49854, #65581, #59996, #44283, #34131, #1966, #12451, #11747, #22240, #34484, #55448, #64878, #17706, #44630, #33089, #33785, #7207, #28898, #43926, #39029, #38320, #54405, #59650, #60344, #6505, #38675, #23289, #27850, #48820, #22585, #23626, #50205, #1615, #65232, #17347, #12107, #65922, #39367, #6154, #60686, #22931, #18049, #7543, #1269, #929, #6851, #33436, #54752, #16992, #49503, #44966, #28188, #12803, #66270, #55101, #18392, #39717, #28543, #61035, #24660, #40391, #46678, #40735, #2645, #55795, #45651, #56822, #61379, #51231, #29586, #2984, #50889, #30259, #67635, #24317, #8922, #56475, #61714, #20099, #14174, #3328, #13833, #8239, #35501, #62400, #34818, #30592 ),
 ( #35163, #51563, #3660, #25000, #19410, #29234, #66957, #46333, #67982, #29925, #45308, #19758, #45982, #41082, #14519, #19064, #41425, #56131, #35836, #57154, #9250, #8578, #51906, #62734, #67294, #62060, #4003, #25340, #14856, #23974, #7897, #50545, #66615, #18736, #40067, #13499, #9598, #68668, #31288, #43140, #58876, #26382, #37544, #58527, #48045, #5044, #37210, #15545, #10292, #42116, #52596, #31978, #10633, #63422, #4691, #10981, #36874, #147, #36178, #26034, #15878, #63767, #64107, #47708, #58190, #57490, #15196, #31627, #64443, #27069, #30940, #48386, #52256, #53290, #16222, #69018, #21133, #57844, #4352, #20785, #5391, #47363, #52947, #42458, #9951, #26729, #21465, #42801, #32320, #25684, #53633, #47017, #68319, #5728, #493, #21808, #20440, #41767, #63070, #36521, #65140, #6764, #838, #49074, #43495, #38942, #17261, #55017, #22153, #53968, #37894, #24502 ) ),
 .UNSPECIFIED., .F., .F., .F.,
 ( 2, 2 ),
 ( 4, 2, 2, 2, 2, 2, 2, 2, 2, 2, 2, 2, 2, 2, 2, 2, 2, 2, 2, 2, 2, 2, 2, 2, 2, 2, 2, 2, 2, 2, 2, 2, 2, 2, 2, 2, 2, 2, 2, 2, 2, 2, 2, 2, 2, 2, 2, 2, 2, 2, 2, 2, 2, 2, 2, 4 ),
 ( 0.000000000000000000, 1.000000000000000000 ),
 ( 0.000000000000000000, 7.083325941644376151E-05, 0.0001416665188328875230, 0.0002124997782493312981, 0.0002479164079575531992, 0.0002833330376657750460, 0.0003187496673739968929, 0.0003541662970822187940, 0.0004249995564986625961, 0.0004604161862068844972, 0.0004781245010609954478, 0.0004958328159151063983, 0.0005312494456233282994, 0.0005666660753315500921, 0.0006374993347479937858, 0.0006729159644562156869, 0.0007083325941644375880, 0.0007437492238726594890, 0.0007791658535808813901, 0.0008145824832891032912, 0.0008499991129973251923, 0.0008854157427055470934, 0.0009208323724137689945, 0.0009562490021219908955, 0.0009916656318302127966, 0.001027082261538434698, 0.001062498891246656599, 0.001133332150663100184, 0.001168748780371322085, 0.001204165410079543769, 0.001239582039787765671, 0.001274998669495987572, 0.001345831928912431374, 0.001381248558620653275, 0.001416665188328875176, 0.001452081818037097077, 0.001469790132891207919, 0.001487498447745318978, 0.001558331707161762780, 0.001629164966578206582, 0.001664581596286428484, 0.001699998225994650385, 0.001735414855702872286, 0.001770831485411094187, 0.001841664744827537989, 0.001877081374535759890, 0.001912498004243981791, 0.001947914633952203692, 0.001983331263660425593, 0.002018747893368647711, 0.002054164523076869395, 0.002124997782493313198, 0.002160414412201534882, 0.002195831041909756566, 0.002231247671617978684, 0.002266664301326200368 ),
 .UNSPECIFIED. ) ;
#35158 = EDGE_CURVE ( 'NONE', #32256, #24046, #62878, .T. ) ;
#35159 = CARTESIAN_POINT ( 'NONE',  ( 0.2153359931920000025, 3.215315751876999695, 1.126573897625000029E-09 ) ) ;
#35160 = PRODUCT_DEFINITION_FORMATION_WITH_SPECIFIED_SOURCE ( 'ANY', '', #61183, .NOT_KNOWN. ) ;
#35161 = CARTESIAN_POINT ( 'NONE',  ( 21.35000154058000277, 0.000000000000000000, 0.000000000000000000 ) ) ;
#35162 = VERTEX_POINT ( 'NONE', #12438 ) ;
#35163 = CARTESIAN_POINT ( 'NONE',  ( 12.80505043854144276, -0.6250000000000006661, -12.67928921589118652 ) ) ;
#35164 = CARTESIAN_POINT ( 'NONE',  ( 7.808061958594711527, -3.029385392905544538, 6.512745199459435419 ) ) ;
#35165 = FACE_OUTER_BOUND ( 'NONE', #48707, .T. ) ;
#35166 = CARTESIAN_POINT ( 'NONE',  ( 10.64393020684969926, 5.250000000000000000, 7.500000000000000000 ) ) ;
#35167 = CARTESIAN_POINT ( 'NONE',  ( 7.974113208588001100, 4.561154361229000642, -6.272154006859000930 ) ) ;
#35168 = ORIENTED_EDGE ( 'NONE', *, *, #65075, .T. ) ;
#35169 = CARTESIAN_POINT ( 'NONE',  ( 6.451007504533999182, 0.02828639361845000297, -1.175746811673999970 ) ) ;
#35170 = CARTESIAN_POINT ( 'NONE',  ( 17.81164675503526951, 0.5699806461722944917, 12.68277882560270875 ) ) ;
#35171 = CARTESIAN_POINT ( 'NONE',  ( 13.46242637979000101, -11.63956415132000011, -2.420148064723000481 ) ) ;
#35172 = CARTESIAN_POINT ( 'NONE',  ( 10.37041638348499895, 2.758294858530000226, 7.802464414828100381 ) ) ;
#35173 = CARTESIAN_POINT ( 'NONE',  ( 11.52166954483529793, 4.562096242626500597, -6.632714178206799538 ) ) ;
#35174 = EDGE_LOOP ( 'NONE', ( #14545, #9058, #39068, #9617, #46787 ) ) ;
#35175 = CARTESIAN_POINT ( 'NONE',  ( 10.34947173981000113, -4.457565973839000328, 6.154866550070000386 ) ) ;
#35176 = EDGE_LOOP ( 'NONE', ( #2954, #27143, #40111, #66696 ) ) ;
#35177 = FACE_OUTER_BOUND ( 'NONE', #35044, .T. ) ;
#35178 = CARTESIAN_POINT ( 'NONE',  ( 8.432504440379000599, -5.430412429559000387, 7.210798766422999329 ) ) ;
#35179 = CONICAL_SURFACE ( 'NONE', #47495, 13.04999927352999833, 0.7853981075146502233 ) ;
#35180 = CARTESIAN_POINT ( 'NONE',  ( 18.27977752388258281, 0.02332822437944338106, -13.99998565365491388 ) ) ;
#35181 = EDGE_LOOP ( 'NONE', ( #41714, #39575, #7123, #14465 ) ) ;
#35182 = CARTESIAN_POINT ( 'NONE',  ( 10.95867266763608328, 8.944080322854695453, -6.438115898787937219 ) ) ;
#35183 = CARTESIAN_POINT ( 'NONE',  ( 5.700000000000000178, -13.94845324556000143, 4.312847325879000770 ) ) ;
#35184 = CARTESIAN_POINT ( 'NONE',  ( 10.29184687351666838, -4.999583552997724389, 8.268183399968647151 ) ) ;
#35185 = CARTESIAN_POINT ( 'NONE',  ( 15.90003771078200145, 3.695138809391000034, 11.25918926437999978 ) ) ;
#35186 = CARTESIAN_POINT ( 'NONE',  ( 18.13004437690753434, -2.745098799756841679, 12.39110308487445344 ) ) ;
#35187 = ORIENTED_EDGE ( 'NONE', *, *, #11302, .T. ) ;
#35188 = CARTESIAN_POINT ( 'NONE',  ( 10.96080136920999948, -2.054580854576999904, 7.810082699133999995 ) ) ;
#35189 = B_SPLINE_CURVE_WITH_KNOTS ( 'NONE', 3,
 ( #3745, #46759, #24400, #20178 ),
 .UNSPECIFIED., .F., .F.,
 ( 4, 4 ),
 ( 0.000000000000000000, 1.000000000000000000 ),
 .UNSPECIFIED. ) ;
#35190 = B_SPLINE_CURVE_WITH_KNOTS ( 'NONE', 3,
 ( #49114, #58920, #21506, #68102, #22199, #48428, #26774, #33042, #30717 ),
 .UNSPECIFIED., .F., .F.,
 ( 4, 1, 1, 1, 1, 1, 4 ),
 ( 0.1253746098019370980, 0.1627898251898792226, 0.3296782782853378002, 0.4965667313813880712, 0.6634551844774385643, 0.8303436375728971974, 0.8746155046758248286 ),
 .UNSPECIFIED. ) ;
#35191 = CARTESIAN_POINT ( 'NONE',  ( 11.60000000000000320, 4.804380105966679082, 8.322973907256262294 ) ) ;
#35192 = FACE_OUTER_BOUND ( 'NONE', #28370, .T. ) ;
#35193 = CARTESIAN_POINT ( 'NONE',  ( 11.01684168656612961, 5.218333533724945461, 6.608889323344318889 ) ) ;
#35194 = CARTESIAN_POINT ( 'NONE',  ( 12.70933660604967130, -3.243304671741783274, 13.61914346456210012 ) ) ;
#35195 = B_SPLINE_CURVE_WITH_KNOTS ( 'NONE', 3,
 ( #65113, #17238, #11990, #54993 ),
 .UNSPECIFIED., .F., .F.,
 ( 4, 4 ),
 ( 0.000000000000000000, 1.000000000000000000 ),
 .UNSPECIFIED. ) ;
#35196 = VERTEX_POINT ( 'NONE', #6491 ) ;
#35197 = CARTESIAN_POINT ( 'NONE',  ( 23.71152188531511129, 13.14507144390817572, -3.853799391295626542 ) ) ;
#35198 = CARTESIAN_POINT ( 'NONE',  ( 10.92360823440131590, -2.830160228212987850, -6.777088824845431958 ) ) ;
#35199 = B_SPLINE_CURVE_WITH_KNOTS ( 'NONE', 3,
 ( #35388, #51455, #46217, #66027 ),
 .UNSPECIFIED., .F., .F.,
 ( 4, 4 ),
 ( 0.000000000000000000, 1.000000000000000000 ),
 .UNSPECIFIED. ) ;
#35200 = ADVANCED_FACE ( 'NONE', ( #44269 ), #27141, .T. ) ;
#35201 = CARTESIAN_POINT ( 'NONE',  ( 24.14647681242191624, -3.326418506915634676, -12.48018534518304357 ) ) ;
#35202 = CARTESIAN_POINT ( 'NONE',  ( 3.136390132544209397, -0.4581489286485235790, 3.499999999999998224 ) ) ;
#35203 = EDGE_CURVE ( 'NONE', #29696, #606, #53314, .T. ) ;
#35204 = CARTESIAN_POINT ( 'NONE',  ( 12.66238154463050769, -0.6088408278571626475, -13.88204686096231733 ) ) ;
#35205 = CARTESIAN_POINT ( 'NONE',  ( 18.06416738895852347, -2.863102795628076347, 12.35955380825001093 ) ) ;
#35206 = ORIENTED_EDGE ( 'NONE', *, *, #58578, .T. ) ;
#35207 = CARTESIAN_POINT ( 'NONE',  ( 10.98146005378009882, -3.088328798999600000, -7.013182449205100255 ) ) ;
#35208 = ORIENTED_EDGE ( 'NONE', *, *, #15396, .T. ) ;
#35209 = CARTESIAN_POINT ( 'NONE',  ( 9.980433037259000884, 4.047223446241999589, 9.090360698422999874 ) ) ;
#35210 = CARTESIAN_POINT ( 'NONE',  ( 18.05677685604840832, 2.118334401049060567, 13.74715678132749019 ) ) ;
#35211 = CARTESIAN_POINT ( 'NONE',  ( 8.889129719593999113, 5.687930027805999877, -7.109876198051000351 ) ) ;
#35212 = CARTESIAN_POINT ( 'NONE',  ( 2.971001955742000433, 3.162850693241999966, 1.598219008581000189 ) ) ;
#35213 = CARTESIAN_POINT ( 'NONE',  ( 9.882901294779998125, -4.314558311729999929, -9.161035779983999205 ) ) ;
#35214 = LINE ( 'NONE', #20151, #5986 ) ;
#35215 = CARTESIAN_POINT ( 'NONE',  ( 23.64695494181500379, 13.35841243503999820, 3.868091839254999886 ) ) ;
#35216 = ORIENTED_EDGE ( 'NONE', *, *, #3401, .F. ) ;
#35217 = CARTESIAN_POINT ( 'NONE',  ( 11.26841504065830080, -3.085489673376300424, 8.181880472491098288 ) ) ;
#35218 = CARTESIAN_POINT ( 'NONE',  ( 9.323722176100000425, 3.947350570199999797, 6.051869652381999920 ) ) ;
#35219 = CARTESIAN_POINT ( 'NONE',  ( 15.55534550153200080, 9.119897322331999234, 8.232476562723000768 ) ) ;
#35220 = EDGE_CURVE ( 'NONE', #19244, #23058, #61794, .T. ) ;
#35221 = CARTESIAN_POINT ( 'NONE',  ( 23.85399089423582453, 9.637233468683378490, 9.713115584480068065 ) ) ;
#35223 = CARTESIAN_POINT ( 'NONE',  ( -15.86200481174999943, -2.399999999999999911, 6.571291218949999902 ) ) ;
#35222 = CARTESIAN_POINT ( 'NONE',  ( 9.815201913989998417, 2.813632032385000148, 8.848857341496000117 ) ) ;
#35224 = CARTESIAN_POINT ( 'NONE',  ( 11.53148876160955005, 3.209326035813000022, -8.322268080792200706 ) ) ;
#35225 = ADVANCED_FACE ( 'NONE', ( #9499 ), #1512, .T. ) ;
#35226 = CARTESIAN_POINT ( 'NONE',  ( 10.96040066253607037, 2.825454854422092765, -6.681915423809532406 ) ) ;
#35227 = CARTESIAN_POINT ( 'NONE',  ( 9.579025935145997650, 3.854158361175799907, -6.506233167833100239 ) ) ;
#35228 = CARTESIAN_POINT ( 'NONE',  ( 17.55505043854144276, -0.7192913403693027563, 12.57945229203838267 ) ) ;
#35229 = CARTESIAN_POINT ( 'NONE',  ( 11.37299956498129916, -5.207010770456999893, -7.174999999999999822 ) ) ;
#35230 = CARTESIAN_POINT ( 'NONE',  ( 8.087104536824956114, 4.663776001496819923, -6.206918359655642092 ) ) ;
#35231 = DIRECTION ( 'NONE',  ( 0.000000000000000000, 0.000000000000000000, -1.000000000000000000 ) ) ;
#35232 = ORIENTED_EDGE ( 'NONE', *, *, #47132, .T. ) ;
#35233 = CARTESIAN_POINT ( 'NONE',  ( 8.668206853210000062, -3.979464503892999439, 9.134080454305001595 ) ) ;
#35234 = CARTESIAN_POINT ( 'NONE',  ( 18.16514092158336879, 2.912582788079544294, 13.69368340938387973 ) ) ;
#35235 = CARTESIAN_POINT ( 'NONE',  ( 7.744301838472999577, -3.130384865731000055, 6.467396727560999814 ) ) ;
#35236 = CARTESIAN_POINT ( 'NONE',  ( 8.331682176603999679, 5.101289360622999425, 6.607176324693000424 ) ) ;
#35237 = ORIENTED_EDGE ( 'NONE', *, *, #22162, .F. ) ;
#35238 = CARTESIAN_POINT ( 'NONE',  ( 8.796579719592999780, 2.368264398678999516, 7.410200237937000445 ) ) ;
#35239 = EDGE_CURVE ( 'NONE', #11817, #11372, #37242, .T. ) ;
#35241 = CARTESIAN_POINT ( 'NONE',  ( 11.23078751119019891, 3.084247107206000038, 7.020904658857499925 ) ) ;
#35240 = CARTESIAN_POINT ( 'NONE',  ( 9.003442991499998271, -4.054579081944059915, -6.634708680083400090 ) ) ;
#35242 = CARTESIAN_POINT ( 'NONE',  ( 11.05392028041000074, 5.159483628325999938, -8.487146968478000986 ) ) ;
#35243 = EDGE_LOOP ( 'NONE', ( #69067, #47100, #48867, #36842, #44564, #58607, #47995, #19416 ) ) ;
#35244 = CARTESIAN_POINT ( 'NONE',  ( 5.065443173016666911, -1.500000000000000222, -0.1963495408493622363 ) ) ;
#35245 = CARTESIAN_POINT ( 'NONE',  ( 9.437500199782947519, -5.100000000000000533, -6.523154174498921876 ) ) ;
#35246 = CARTESIAN_POINT ( 'NONE',  ( 10.84226088462129844, 4.002427228022017225, 8.640738455926999961 ) ) ;
#35247 = CARTESIAN_POINT ( 'NONE',  ( 7.936333720142999759, -5.123034382927999175, 6.721303993095999907 ) ) ;
#35248 = CARTESIAN_POINT ( 'NONE',  ( 25.59997774154300032, -2.856411620672000051, -11.13959722905999961 ) ) ;
#35249 = ORIENTED_EDGE ( 'NONE', *, *, #13156, .T. ) ;
#35250 = DIRECTION ( 'NONE',  ( -1.000000000000000000, 0.000000000000000000, 0.000000000000000000 ) ) ;
#35251 = CARTESIAN_POINT ( 'NONE',  ( 11.25809194037999994, -3.275508415657999883, -8.650784343212000849 ) ) ;
#35252 = CARTESIAN_POINT ( 'NONE',  ( 8.071816895048858242, -3.937760767473150292, 5.761230312822644528 ) ) ;
#35253 = AXIS2_PLACEMENT_3D ( 'NONE', #7675, #61502, #45770 ) ;
#35254 = CARTESIAN_POINT ( 'NONE',  ( 11.51656039236534923, -2.826501801118000312, -7.557111631074219460 ) ) ;
#35255 = CARTESIAN_POINT ( 'NONE',  ( 9.499417874594000111, -5.050800927762999493, 7.053287723251499663 ) ) ;
#35256 = ORIENTED_EDGE ( 'NONE', *, *, #43191, .F. ) ;
#35257 = DIRECTION ( 'NONE',  ( -0.000000000000000000, 0.8660254037844288266, 0.5000000000000169864 ) ) ;
#35258 = CARTESIAN_POINT ( 'NONE',  ( 11.19041504065829962, -2.975441626403999784, 8.263934892306599167 ) ) ;
#35259 = ORIENTED_EDGE ( 'NONE', *, *, #30199, .T. ) ;
#35260 = CARTESIAN_POINT ( 'NONE',  ( 10.98768472569999943, 6.720753179915999631, -5.471698458723999181 ) ) ;
#35261 = AXIS2_PLACEMENT_3D ( 'NONE', #41409, #34462, #3982 ) ;
#35262 = VERTEX_POINT ( 'NONE', #55780 ) ;
#35263 = CARTESIAN_POINT ( 'NONE',  ( 9.399722005181999407, -5.700621988293000264, -7.339579610785999186 ) ) ;
#35264 = DIRECTION ( 'NONE',  ( 1.000000000000000000, 0.000000000000000000, 0.000000000000000000 ) ) ;
#35265 = CARTESIAN_POINT ( 'NONE',  ( 14.93333333083533532, -8.833279250037012531, -7.896561129384960687 ) ) ;
#35266 = FACE_OUTER_BOUND ( 'NONE', #25352, .T. ) ;
#35267 = CARTESIAN_POINT ( 'NONE',  ( 12.30770095535949338, 2.879049501765980512, -12.35516346652264552 ) ) ;
#35268 = CARTESIAN_POINT ( 'NONE',  ( 10.94841638348500013, -5.108333310975999630, 7.769976643522699788 ) ) ;
#35269 = CARTESIAN_POINT ( 'NONE',  ( 7.629823341228000544, 4.763536573491999881, 5.668879554882000349 ) ) ;
#35270 = ORIENTED_EDGE ( 'NONE', *, *, #45724, .T. ) ;
#35272 = CARTESIAN_POINT ( 'NONE',  ( 9.475279990687596410, 5.350441389720215213, 7.499985493516660107 ) ) ;
#35271 = B_SPLINE_CURVE_WITH_KNOTS ( 'NONE', 3,
 ( #62327, #68941, #25612, #51831, #35762, #41688 ),
 .UNSPECIFIED., .F., .F.,
 ( 4, 1, 1, 4 ),
 ( 0.000000000000000000, 0.3333333333333000081, 0.6666666666667000474, 1.000000000000000000 ),
 .UNSPECIFIED. ) ;
#35273 = CARTESIAN_POINT ( 'NONE',  ( 7.635855646791999796, -2.466384407480000096, 6.935560677555000275 ) ) ;
#35274 = CARTESIAN_POINT ( 'NONE',  ( 18.20249159964072661, -0.3803681712697531969, 13.99548972733949803 ) ) ;
#35275 = ORIENTED_EDGE ( 'NONE', *, *, #45255, .F. ) ;
#35276 = CARTESIAN_POINT ( 'NONE',  ( 12.24851426484566908, -2.019008278824865332, -12.43718985311489966 ) ) ;
#35278 = CARTESIAN_POINT ( 'NONE',  ( 10.32533997688000049, 4.243109097101799954, 8.614534918052999757 ) ) ;
#35277 = AXIS2_PLACEMENT_3D ( 'NONE', #12972, #60508, #55268 ) ;
#35279 = CARTESIAN_POINT ( 'NONE',  ( 10.16821935321000048, -2.330398934821000356, -7.267462182607999921 ) ) ;
#35280 = CARTESIAN_POINT ( 'NONE',  ( 6.377943173016666911, 0.9218200799623692543, 1.199500263597272687 ) ) ;
#35281 = CARTESIAN_POINT ( 'NONE',  ( 18.01722669115800102, -3.499390932422000056, -11.96939125376999868 ) ) ;
#35282 = ADVANCED_FACE ( 'NONE', ( #20341 ), #68568, .T. ) ;
#35283 = CARTESIAN_POINT ( 'NONE',  ( 24.60320129381999976, -8.810542265102998982, 9.295223627185000836 ) ) ;
#35284 = CARTESIAN_POINT ( 'NONE',  ( 12.49029065891183343, -1.959656569402036475, -13.77327738386123279 ) ) ;
#35285 = EDGE_CURVE ( 'NONE', #46698, #53716, #2426, .T. ) ;
#35286 = LINE ( 'NONE', #3445, #41929 ) ;
#35287 = CARTESIAN_POINT ( 'NONE',  ( 10.39503166480599994, -5.274847857784000560, -7.589885038193400213 ) ) ;
#35288 = ADVANCED_FACE ( 'NONE', ( #16128 ), #21371, .F. ) ;
#35289 = CARTESIAN_POINT ( 'NONE',  ( 6.999999691988000095, 12.89129024452999950, 1.677687644161999891 ) ) ;
#35290 = VERTEX_POINT ( 'NONE', #48288 ) ;
#35291 = ORIENTED_EDGE ( 'NONE', *, *, #11260, .F. ) ;
#35292 = DIRECTION ( 'NONE',  ( -1.000000000000000000, 0.000000000000000000, 0.000000000000000000 ) ) ;
#35293 = CARTESIAN_POINT ( 'NONE',  ( 18.05135021982939492, 2.880031268700117941, 13.58542674995964994 ) ) ;
#35294 = CARTESIAN_POINT ( 'NONE',  ( 10.97074841058999972, 2.648521302318000092, -6.788870928221999890 ) ) ;
#35295 = B_SPLINE_CURVE_WITH_KNOTS ( 'NONE', 3,
 ( #1411, #13638, #12947, #18188 ),
 .UNSPECIFIED., .F., .F.,
 ( 4, 4 ),
 ( 0.8163836489557148024, 1.000000000000000000 ),
 .UNSPECIFIED. ) ;
#35296 = CARTESIAN_POINT ( 'NONE',  ( 24.52301136554485694, -8.782808807263306150, -8.926452893334182903 ) ) ;
#35297 = DIRECTION ( 'NONE',  ( 1.000000000000000000, 0.000000000000000000, 0.000000000000000000 ) ) ;
#35298 = CARTESIAN_POINT ( 'NONE',  ( 23.58444451512600182, -13.25737176886000057, 4.306335449404000038 ) ) ;
#35299 = CARTESIAN_POINT ( 'NONE',  ( 9.786671076420999427, 2.381202181614999525, 7.612749448318000489 ) ) ;
#35300 = CARTESIAN_POINT ( 'NONE',  ( 10.19837725605996326, -4.679950664087114909, -8.679651447173698742 ) ) ;
#35301 = ORIENTED_EDGE ( 'NONE', *, *, #14194, .F. ) ;
#35302 = CARTESIAN_POINT ( 'NONE',  ( 12.23374516775632159, -2.245741837849043687, 12.50722324768529781 ) ) ;
#35303 = CARTESIAN_POINT ( 'NONE',  ( 9.275076168957998135, -4.509700402263200125, -8.365475476407400635 ) ) ;
#35304 = CARTESIAN_POINT ( 'NONE',  ( 10.81579666500999970, 5.374569445151000657, 6.698728322222000209 ) ) ;
#35305 = CARTESIAN_POINT ( 'NONE',  ( 11.10235971519489873, -3.394698737128500010, 8.506961598696999971 ) ) ;
#35306 = CARTESIAN_POINT ( 'NONE',  ( 9.775320280412000074, 2.527713920559999661, -6.969421869128999525 ) ) ;
#35307 = CARTESIAN_POINT ( 'NONE',  ( 11.20733594839949809, 4.840266102192999575, -6.537051788466999191 ) ) ;
#35308 = CARTESIAN_POINT ( 'NONE',  ( 12.42881362571445436, 0.4990964484179714611, 12.68679736436866712 ) ) ;
#35309 = AXIS2_PLACEMENT_3D ( 'NONE', #4107, #69123, #21231 ) ;
#35310 = CARTESIAN_POINT ( 'NONE',  ( 7.930392219590000735, 3.164805384346000228, 9.104735843897000080 ) ) ;
#35311 = CARTESIAN_POINT ( 'NONE',  ( 10.37373942323999998, 2.215265813302000009, 7.703982730183001060 ) ) ;
#35312 = CARTESIAN_POINT ( 'NONE',  ( 12.78420607872184966, 1.875260891907201133, 12.57537395219491216 ) ) ;
#35313 = ORIENTED_EDGE ( 'NONE', *, *, #62693, .T. ) ;
#35314 = CARTESIAN_POINT ( 'NONE',  ( 8.880270280412998929, 4.146787477634999775, -5.941926545671999627 ) ) ;
#35315 = CARTESIAN_POINT ( 'NONE',  ( 7.393237896465000958, 0.08818371649832000558, 1.484376669706999996 ) ) ;
#35316 = CARTESIAN_POINT ( 'NONE',  ( 10.81004357109428327, -4.321142019900527487, 9.210264094307881066 ) ) ;
#35318 = CARTESIAN_POINT ( 'NONE',  ( 3.323606204996916613, -2.160720528238035953, -2.790977566173463931 ) ) ;
#35317 = CARTESIAN_POINT ( 'NONE',  ( 9.395316940379000670, -5.146736128384000075, 6.597417125647000447 ) ) ;
#35319 = CARTESIAN_POINT ( 'NONE',  ( 12.09999999999999787, -3.983295036746753670, 8.547709597963841333 ) ) ;
#35320 = CARTESIAN_POINT ( 'NONE',  ( 10.29262282008599882, -3.548418513060800361, -8.228386593078399258 ) ) ;
#35321 = ORIENTED_EDGE ( 'NONE', *, *, #23039, .F. ) ;
#35322 = CIRCLE ( 'NONE', #48731, 0.9999999999999993339 ) ;
#35323 = CARTESIAN_POINT ( 'NONE',  ( 1.396064357887999874, 3.196468001211000054, -1.639036658905000055 ) ) ;
#35324 = CARTESIAN_POINT ( 'NONE',  ( 17.69809845378366120, -0.6087666915580426386, -12.68035271361765304 ) ) ;
#35325 = EDGE_CURVE ( 'NONE', #2511, #10719, #55113, .T. ) ;
#35327 = CARTESIAN_POINT ( 'NONE',  ( 15.95563472374800185, -3.716697538693999991, -11.19594450203000058 ) ) ;
#35326 = CARTESIAN_POINT ( 'NONE',  ( 8.424364158774000799, 3.292387953886000140, -6.294868737226000377 ) ) ;
#35329 = B_SPLINE_CURVE_WITH_KNOTS ( 'NONE', 3,
 ( #56948, #50681, #45775, #18865, #30386, #24103, #45435, #39497, #3119, #45093 ),
 .UNSPECIFIED., .F., .F.,
 ( 4, 2, 2, 2, 4 ),
 ( 0.000000000000000000, 0.1249999999280926311, 0.2499999998561852621, 0.3749999997842778932, 0.4999999997123705242 ),
 .UNSPECIFIED. ) ;
#35328 = CARTESIAN_POINT ( 'NONE',  ( 6.999999999999999112, -7.162151381622562596, 3.226150686063063322 ) ) ;
#35330 = CARTESIAN_POINT ( 'NONE',  ( 10.34947814066000049, 4.457562099971999814, 6.154877938302999674 ) ) ;
#35331 = ADVANCED_FACE ( 'NONE', ( #54216 ), #2195, .F. ) ;
#35332 = CARTESIAN_POINT ( 'NONE',  ( 12.35242198444192674, -3.088429417998432847, 13.65509667848947473 ) ) ;
#35333 = CARTESIAN_POINT ( 'NONE',  ( 0.2000000000000000389, -2.149999999999999911, -1.475903017541000135E-12 ) ) ;
#35334 = FACE_OUTER_BOUND ( 'NONE', #21081, .T. ) ;
#35335 = CARTESIAN_POINT ( 'NONE',  ( 7.539230646792000279, -4.696237245142999228, 5.830277424166999900 ) ) ;
#35336 = ORIENTED_EDGE ( 'NONE', *, *, #1656, .T. ) ;
#35337 = CARTESIAN_POINT ( 'NONE',  ( 7.802017219589999719, 5.638704226117999596, 8.266404648244000342 ) ) ;
#35338 = CARTESIAN_POINT ( 'NONE',  ( 10.95203274928999804, 5.154111710649999623, 5.182718807703999175 ) ) ;
#35339 = CARTESIAN_POINT ( 'NONE',  ( 7.450492827224381109, -2.261080942162393637, 7.469285780581691903 ) ) ;
#35340 = CARTESIAN_POINT ( 'NONE',  ( 10.67320712187270004, -2.921171224854953063, 8.329102901498991685 ) ) ;
#35341 = CARTESIAN_POINT ( 'NONE',  ( 2.124703346705999696, 1.685541059001999908, -2.982097634516000184 ) ) ;
#35342 = VERTEX_POINT ( 'NONE', #15705 ) ;
#35343 = CARTESIAN_POINT ( 'NONE',  ( 1.095639153602063987, -2.129181563504743746, -2.524889412081005258 ) ) ;
#35344 = CARTESIAN_POINT ( 'NONE',  ( 11.49410672858429905, -4.801902424331299990, 8.103244025831999764 ) ) ;
#35345 = CARTESIAN_POINT ( 'NONE',  ( 10.94841903626084090, -4.366312240206965178, -9.227246227427363223 ) ) ;
#35346 = CARTESIAN_POINT ( 'NONE',  ( 9.722769750889000306, 5.493785011855999656, 6.566826815556000341 ) ) ;
#35347 = CARTESIAN_POINT ( 'NONE',  ( 10.77256919669529900, 4.962345366016100101, 7.215672285280100517 ) ) ;
#35348 = CARTESIAN_POINT ( 'NONE',  ( 10.69015444038000062, -4.391267940138999570, -8.802346922965000431 ) ) ;
#35349 = DIRECTION ( 'NONE',  ( -1.000000000000000000, 0.000000000000000000, 0.000000000000000000 ) ) ;
#35350 = CARTESIAN_POINT ( 'NONE',  ( 11.29998636608000062, 3.695122995756999984, -11.25914041192000070 ) ) ;
#35351 = CARTESIAN_POINT ( 'NONE',  ( 10.97581817698185525, -5.215421929002181933, 6.751285922363551073 ) ) ;
#35352 = CARTESIAN_POINT ( 'NONE',  ( 8.039315972864844895, 3.244806080982685526, 5.913190043580576649 ) ) ;
#35353 = VERTEX_POINT ( 'NONE', #58691 ) ;
#35354 = CIRCLE ( 'NONE', #48766, 5.760713961201000544 ) ;
#35355 = CARTESIAN_POINT ( 'NONE',  ( 17.55505043854147118, -3.248109929747638347, 13.61799478206225444 ) ) ;
#35356 = CARTESIAN_POINT ( 'NONE',  ( 21.49999863197000138, 1.172395514003999961E-13, 13.99999975536035279 ) ) ;
#35357 = ORIENTED_EDGE ( 'NONE', *, *, #24503, .F. ) ;
#35358 = ORIENTED_EDGE ( 'NONE', *, *, #68558, .T. ) ;
#35359 = CARTESIAN_POINT ( 'NONE',  ( 10.94501463001509833, 4.472480213525599879, 8.256737112932800216 ) ) ;
#35360 = DIRECTION ( 'NONE',  ( 0.000000000000000000, -1.000000000000000000, 0.000000000000000000 ) ) ;
#35361 = CARTESIAN_POINT ( 'NONE',  ( 10.92441504065829960, 4.694414232677499577, 8.017771632862299214 ) ) ;
#35362 = CARTESIAN_POINT ( 'NONE',  ( 10.96580581817999978, 4.930645553951000792, 6.170542400361000546 ) ) ;
#35363 = FACE_OUTER_BOUND ( 'NONE', #10667, .T. ) ;
#35364 = PLANE ( 'NONE',  #24212 ) ;
#35365 = CARTESIAN_POINT ( 'NONE',  ( 10.68361719090999884, -2.603550124652000086, 7.762065570229999878 ) ) ;
#35366 = EDGE_CURVE ( 'NONE', #57425, #53074, #51564, .T. ) ;
#35367 = CARTESIAN_POINT ( 'NONE',  ( 18.27863132999453200, -0.04649795050485940051, -12.59991969135870526 ) ) ;
#35368 = CARTESIAN_POINT ( 'NONE',  ( 11.79999999550100220, 3.351258778187000242, -11.15757272551999968 ) ) ;
#35369 = CARTESIAN_POINT ( 'NONE',  ( 11.34287482311539996, -3.196874704906699893, -7.824481664695199790 ) ) ;
#35370 = EDGE_CURVE ( 'NONE', #56839, #65623, #43285, .T. ) ;
#35371 = EDGE_CURVE ( 'NONE', #6018, #15621, #68277, .T. ) ;
#35372 = CARTESIAN_POINT ( 'NONE',  ( 8.255239991808057454, 5.012978268976954865, -8.578693711955805767 ) ) ;
#35373 = ORIENTED_EDGE ( 'NONE', *, *, #20787, .T. ) ;
#35374 = AXIS2_PLACEMENT_3D ( 'NONE', #38321, #27852, #32742 ) ;
#35375 = CARTESIAN_POINT ( 'NONE',  ( 18.49985170088394426, -7.837663500889314729E-14, -12.52499999999998792 ) ) ;
#35376 = CARTESIAN_POINT ( 'NONE',  ( 10.66922466689405269, 3.154184221645670139, -4.789865691167801920 ) ) ;
#35377 = CARTESIAN_POINT ( 'NONE',  ( 10.67437910952998870, 7.450072830998997198, 5.983005019645002420 ) ) ;
#35378 = CARTESIAN_POINT ( 'NONE',  ( 9.304430433046999127, 2.911395389258000233, -6.828193190755800224 ) ) ;
#35379 = CARTESIAN_POINT ( 'NONE',  ( 12.18713711904774399, 2.135907760014737811, 13.83611243771405697 ) ) ;
#35380 = CARTESIAN_POINT ( 'NONE',  ( 13.69997185827400088, 10.10519270881758480, 5.872265061164083200 ) ) ;
#35381 = ORIENTED_EDGE ( 'NONE', *, *, #53847, .T. ) ;
#35382 = CARTESIAN_POINT ( 'NONE',  ( 12.54851516836652969, 0.5702235046495642834, -12.68276536598757787 ) ) ;
#35383 = CARTESIAN_POINT ( 'NONE',  ( 12.09168665071629967, -0.1308528744652237841, 13.99939340647621044 ) ) ;
#35384 = EDGE_LOOP ( 'NONE', ( #62488, #19457, #48573, #68002 ) ) ;
#35385 = PLANE ( 'NONE',  #7489 ) ;
#35386 = DIRECTION ( 'NONE',  ( 5.840561064144232596E-06, 0.2588571483570100695, 0.9659156157296374667 ) ) ;
#35387 = ADVANCED_FACE ( 'NONE', ( #5889 ), #42782, .F. ) ;
#35388 = CARTESIAN_POINT ( 'NONE',  ( 13.99999999347100044, 9.187456302440001110, 8.213201953411001455 ) ) ;
#35389 = DIRECTION ( 'NONE',  ( 0.000000000000000000, -0.7270098363383266094, -0.6866270442294852838 ) ) ;
#35390 = FACE_OUTER_BOUND ( 'NONE', #61326, .T. ) ;
#35391 = CARTESIAN_POINT ( 'NONE',  ( 0.4662484304700000304, 2.655425791298000160, -2.578923811134000044 ) ) ;
#35392 = CARTESIAN_POINT ( 'NONE',  ( 8.174990947233153449, 2.650692654198087972, 7.500004443805798005 ) ) ;
#35393 = CARTESIAN_POINT ( 'NONE',  ( 12.54729787553182341, 3.152819052640265518, 12.19917003430776248 ) ) ;
#35394 = CARTESIAN_POINT ( 'NONE',  ( 9.282558421712998609, -4.950980172046000050, -5.959730545597000884 ) ) ;
#35395 = CARTESIAN_POINT ( 'NONE',  ( 11.51518179236248862, 3.819003318705799899, -6.652923384986699773 ) ) ;
#35396 = FACE_OUTER_BOUND ( 'NONE', #1395, .T. ) ;
#35397 = CARTESIAN_POINT ( 'NONE',  ( 11.02812378248509795, 3.583106837161099900, -6.711274001288999536 ) ) ;
#35398 = CARTESIAN_POINT ( 'NONE',  ( 9.506000818238998562, 2.989704013253000614, -8.032011717116800398 ) ) ;
#35400 = CARTESIAN_POINT ( 'NONE',  ( 12.18009741656777045, 2.512104454645549545, 12.44873738064200808 ) ) ;
#35399 = CARTESIAN_POINT ( 'NONE',  ( 15.62410434383600055, -8.799879896029001003, -7.715564795277000343 ) ) ;
#35401 = DIRECTION ( 'NONE',  ( 1.000000000000000000, 5.773164121932000354E-14, 0.000000000000000000 ) ) ;
#35402 = ORIENTED_EDGE ( 'NONE', *, *, #55846, .T. ) ;
#35403 = TOROIDAL_SURFACE ( 'NONE', #26459, 6.000000000000000000, 1.000000000000000000 ) ;
#35404 = CARTESIAN_POINT ( 'NONE',  ( 5.500000000000000000, -11.06886219213000011, -1.536526853569999851 ) ) ;
#35405 = VECTOR ( 'NONE', #44914, 1000.000000000000000 ) ;
#35406 = CARTESIAN_POINT ( 'NONE',  ( 9.538434317036999843, -5.620900626097999897, 7.423100105894999245 ) ) ;
#35407 = CARTESIAN_POINT ( 'NONE',  ( 10.06027973160899869, 4.090130512164860122, 8.500359330993999762 ) ) ;
#35408 = CARTESIAN_POINT ( 'NONE',  ( 23.58444974876299938, -2.899236306833000043, 13.63438999212000091 ) ) ;
#35409 = CARTESIAN_POINT ( 'NONE',  ( 23.56666365135700403, 11.61524011578000604, -3.333188920255001353 ) ) ;
#35410 = EDGE_CURVE ( 'NONE', #60390, #5246, #3693, .T. ) ;
#35411 = FACE_OUTER_BOUND ( 'NONE', #54570, .T. ) ;
#35412 = CARTESIAN_POINT ( 'NONE',  ( 10.17284693385893490, -4.293232846717661033, -8.835933254752704968 ) ) ;
#35413 = ORIENTED_EDGE ( 'NONE', *, *, #49352, .T. ) ;
#35414 = CARTESIAN_POINT ( 'NONE',  ( 9.885938025973999288, -4.593629475532499562, -6.524634174392399899 ) ) ;
#35415 = CONICAL_SURFACE ( 'NONE', #37643, 13.04999934368000147, 0.7853981075146502233 ) ;
#35416 = CARTESIAN_POINT ( 'NONE',  ( 8.576923877145999242, 3.399999999999999911, 5.924121105096999962 ) ) ;
#35417 = CARTESIAN_POINT ( 'NONE',  ( 12.06322412107030928, -3.945399343424460525, 8.532060764998998792 ) ) ;
#35418 = CARTESIAN_POINT ( 'NONE',  ( 17.68813047654957771, 3.110753822336481011, -12.28807462416255092 ) ) ;
#35419 = CARTESIAN_POINT ( 'NONE',  ( 2.698890132542666631, -2.798833948393640192, 2.150913519912191152 ) ) ;
#35420 = CARTESIAN_POINT ( 'NONE',  ( 10.98768472639999949, 0.3876847264043000174, 4.945212061661000469 ) ) ;
#35422 = AXIS2_PLACEMENT_3D ( 'NONE', #49882, #65946, #65607 ) ;
#35421 = CARTESIAN_POINT ( 'NONE',  ( 23.60000000000000142, 0.000000000000000000, 0.000000000000000000 ) ) ;
#35423 = CARTESIAN_POINT ( 'NONE',  ( 9.436149330669000079, -3.485164486501000081, -6.221839249167999242 ) ) ;
#35424 = DIRECTION ( 'NONE',  ( 0.000000000000000000, 0.000000000000000000, -1.000000000000000000 ) ) ;
#35425 = EDGE_LOOP ( 'NONE', ( #64848, #31826, #17864, #57324, #66004, #60638, #10243, #47016 ) ) ;
#35426 = CARTESIAN_POINT ( 'NONE',  ( 6.294818531611999781E-06, -2.999993704296999741, -7.007531981267999457E-10 ) ) ;
#35427 = CARTESIAN_POINT ( 'NONE',  ( 12.57207325926688668, 0.6915911779535816040, -13.98290807251246548 ) ) ;
#35428 = CARTESIAN_POINT ( 'NONE',  ( 13.50542051561400214, -9.036698429651000453, -7.720610530813999617 ) ) ;
#35429 = CARTESIAN_POINT ( 'NONE',  ( 11.10000000001999965, 7.806347126537000136, 6.642166469876999990 ) ) ;
#35430 = CARTESIAN_POINT ( 'NONE',  ( 2.884306799211333594, -1.762666431298145930, -3.058252359239904905 ) ) ;
#35431 = CARTESIAN_POINT ( 'NONE',  ( 9.219964158774999419, 3.941185585667000169, -8.896279800194999865 ) ) ;
#35432 = CARTESIAN_POINT ( 'NONE',  ( 12.31056516821460001, -3.390321848206700128, 6.884701936848800052 ) ) ;
#35433 = ORIENTED_EDGE ( 'NONE', *, *, #11422, .F. ) ;
#35434 = CARTESIAN_POINT ( 'NONE',  ( 9.167129859538265535, -5.079276359681585973, -8.329393289878948892 ) ) ;
#35435 = CARTESIAN_POINT ( 'NONE',  ( 18.27122651615330895, 2.402315819361971805, -13.79236889726217363 ) ) ;
#35436 = ORIENTED_EDGE ( 'NONE', *, *, #50107, .F. ) ;
#35437 = CARTESIAN_POINT ( 'NONE',  ( 10.61792546752099931, -4.864937374655599278, 7.559927309296559983 ) ) ;
#35438 = FACE_OUTER_BOUND ( 'NONE', #24742, .T. ) ;
#35439 = CARTESIAN_POINT ( 'NONE',  ( 8.365779719592000063, 2.949305648881000330, -8.659807625323999503 ) ) ;
#35440 = CARTESIAN_POINT ( 'NONE',  ( 9.958268565653391136, 4.155869445530794515, -9.269508239148089856 ) ) ;
#35441 = CARTESIAN_POINT ( 'NONE',  ( 10.48280513895999988, -3.096689368913399854, -6.997844089834400094 ) ) ;
#35442 = CARTESIAN_POINT ( 'NONE',  ( 11.59999999999999609, -3.011522968892933250, -6.852161599766354527 ) ) ;
#35443 = CARTESIAN_POINT ( 'NONE',  ( 5.044609839683332986, -1.500000000000000444, 0.1963495408493560745 ) ) ;
#35444 = ORIENTED_EDGE ( 'NONE', *, *, #31104, .T. ) ;
#35445 = CARTESIAN_POINT ( 'NONE',  ( 8.654403730149667240, -2.899999999999999911, 6.499666959930667787 ) ) ;
#35446 = EDGE_CURVE ( 'NONE', #66620, #7152, #9327, .T. ) ;
#35447 = CARTESIAN_POINT ( 'NONE',  ( 10.73976354018233437, -4.327184855449098144, 8.717465845835395299 ) ) ;
#35449 = CARTESIAN_POINT ( 'NONE',  ( 8.739954719592999410, 3.122811675949999977, -6.006064052396999919 ) ) ;
#35448 = B_SPLINE_CURVE_WITH_KNOTS ( 'NONE', 3,
 ( #36368, #41614, #20633, #31818 ),
 .UNSPECIFIED., .F., .F.,
 ( 4, 4 ),
 ( 0.000000000000000000, 1.000000000000000000 ),
 .UNSPECIFIED. ) ;
#35450 = ORIENTED_EDGE ( 'NONE', *, *, #5393, .F. ) ;
#35451 = VECTOR ( 'NONE', #51822, 1000.000000000000114 ) ;
#35452 = CARTESIAN_POINT ( 'NONE',  ( 10.35427764559999986, 4.879113829302000660, -8.944031201701999834 ) ) ;
#35453 = FILL_AREA_STYLE ('',( #14126 ) ) ;
#35454 = ORIENTED_EDGE ( 'NONE', *, *, #44943, .T. ) ;
#35455 = CARTESIAN_POINT ( 'NONE',  ( 9.050076168957998490, 3.420574098817999786, 6.516130052788599691 ) ) ;
#35456 = CARTESIAN_POINT ( 'NONE',  ( 17.84060712062129639, -3.141591522576406614, -12.20206574396288346 ) ) ;
#35457 = STYLED_ITEM ( 'NONE', ( #8110 ), #30277 ) ;
#35458 = CARTESIAN_POINT ( 'NONE',  ( 11.31919037786000182, -11.76444917719000038, -1.692529869092999961 ) ) ;
#35459 = VECTOR ( 'NONE', #63205, 1000.000000000000000 ) ;
#35460 = CARTESIAN_POINT ( 'NONE',  ( 24.26733149983100191, -12.18172987844000055, -3.303689625207000269 ) ) ;
#35461 = CARTESIAN_POINT ( 'NONE',  ( 9.089766096192999356, -8.660638521191998507, -6.051256224376999171 ) ) ;
#35462 = ORIENTED_EDGE ( 'NONE', *, *, #20177, .T. ) ;
#35463 = CARTESIAN_POINT ( 'NONE',  ( 11.52285868696541549, 4.059810388505518119, 6.228129494253469289 ) ) ;
#35464 = CARTESIAN_POINT ( 'NONE',  ( 7.100000000000000533, 4.000000000000000000, 8.849999999999999645 ) ) ;
#35465 = EDGE_CURVE ( 'NONE', #28630, #18146, #49978, .T. ) ;
#35466 = CARTESIAN_POINT ( 'NONE',  ( 8.122851870745966707, -2.921728982776596872, 8.328193042681078850 ) ) ;
#35467 = CIRCLE ( 'NONE', #14253, 11.84999999999999964 ) ;
#35468 = CARTESIAN_POINT ( 'NONE',  ( 12.10347303272471997, 2.332585440199563376, -13.80433171579881879 ) ) ;
#35469 = EDGE_CURVE ( 'NONE', #59964, #64650, #43989, .T. ) ;
#35470 = CARTESIAN_POINT ( 'NONE',  ( 5.500000000000000000, 0.000000000000000000, 0.000000000000000000 ) ) ;
#35471 = CARTESIAN_POINT ( 'NONE',  ( 10.20271159698171815, 5.100000000000000533, 6.305985889763628727 ) ) ;
#35472 = CARTESIAN_POINT ( 'NONE',  ( 18.05707515698670207, -2.118723117022102365, 12.53248177916035289 ) ) ;
#35473 = B_SPLINE_CURVE_WITH_KNOTS ( 'NONE', 3,
 ( #53050, #3181, #24509, #69121, #21566, #63867 ),
 .UNSPECIFIED., .F., .F.,
 ( 4, 2, 4 ),
 ( 0.000000000000000000, 0.5000000000000000000, 1.000000000000000000 ),
 .UNSPECIFIED. ) ;
#35474 = VERTEX_POINT ( 'NONE', #32478 ) ;
#35475 = VERTEX_POINT ( 'NONE', #36690 ) ;
#35476 = AXIS2_PLACEMENT_3D ( 'NONE', #34903, #8329, #19503 ) ;
#35477 = CARTESIAN_POINT ( 'NONE',  ( 9.716735841232001292, 3.941185585667000169, -8.896279800194999865 ) ) ;
#35478 = CARTESIAN_POINT ( 'NONE',  ( 10.58718478751670666, 5.286440948694374420, -7.026985308887427450 ) ) ;
#35479 = CARTESIAN_POINT ( 'NONE',  ( 12.19818565438123414, -2.649653951396504503, 13.64057837019845998 ) ) ;
#35480 = CARTESIAN_POINT ( 'NONE',  ( 25.18904416930200085, 8.466527073521000091, -8.230891403741001255 ) ) ;
#35481 = CARTESIAN_POINT ( 'NONE',  ( 7.830819424294336528, 3.674999207176894878, 6.165344395466317629 ) ) ;
#35482 = CARTESIAN_POINT ( 'NONE',  ( 18.53712493497300073, -2.638811780578999677, -11.30793729956000071 ) ) ;
#35484 = CARTESIAN_POINT ( 'NONE',  ( 9.020964430773000586, 2.907392932634000005, 6.146188468825999784 ) ) ;
#35483 = CARTESIAN_POINT ( 'NONE',  ( 9.726430433046999724, -4.971677342931100085, 8.099647887697699389 ) ) ;
#35485 = CARTESIAN_POINT ( 'NONE',  ( 12.09999999999999964, -4.817420948848700313, 7.825000000000000178 ) ) ;
#35486 = VERTEX_POINT ( 'NONE', #15364 ) ;
#35487 = CARTESIAN_POINT ( 'NONE',  ( 12.43971800579959464, 0.6379138416539124057, 13.98550699733573133 ) ) ;
#35488 = CARTESIAN_POINT ( 'NONE',  ( 10.60811446581000084, -2.866936631589000140, -4.836298645267000929 ) ) ;
#35489 = CARTESIAN_POINT ( 'NONE',  ( 9.930325322607000516, -5.020908168068000776, -6.342951604057000203 ) ) ;
#35490 = DIRECTION ( 'NONE',  ( 1.000000000000000000, 0.000000000000000000, 0.000000000000000000 ) ) ;
#35491 = DIRECTION ( 'NONE',  ( 0.000000000000000000, 0.2714570858282905341, -0.9624505444715651947 ) ) ;
#35492 = CARTESIAN_POINT ( 'NONE',  ( 5.700000000000000178, 13.04986661130000059, 1.811520473896000016 ) ) ;
#35493 = FACE_OUTER_BOUND ( 'NONE', #30288, .T. ) ;
#35494 = VECTOR ( 'NONE', #55829, 1000.000000000000000 ) ;
#35495 = CARTESIAN_POINT ( 'NONE',  ( 7.986889964180154955, 3.051162356207695492, -6.411554890354049796 ) ) ;
#35496 = FACE_OUTER_BOUND ( 'NONE', #423, .T. ) ;
#35497 = AXIS2_PLACEMENT_3D ( 'NONE', #13740, #29838, #45895 ) ;
#35498 = DIRECTION ( 'NONE',  ( 0.000000000000000000, -0.3380467785883188858, -0.9411293085894520960 ) ) ;
#35499 = CARTESIAN_POINT ( 'NONE',  ( 3.115020758170000015, 1.311005030890000089, -3.164819811060000099 ) ) ;
#35500 = ORIENTED_EDGE ( 'NONE', *, *, #43191, .T. ) ;
#35501 = CARTESIAN_POINT ( 'NONE',  ( 12.75722706473760226, 0.7178228174669301076, -12.57953618971562193 ) ) ;
#35502 = CARTESIAN_POINT ( 'NONE',  ( 12.24474413009778750, -2.777098231000808326, -12.38267840003653752 ) ) ;
#35503 = CARTESIAN_POINT ( 'NONE',  ( 11.79999999550100220, -3.351258778187000242, 11.15757272551999968 ) ) ;
#35505 = CARTESIAN_POINT ( 'NONE',  ( 7.871551658771999804, 4.780986922229000236, 6.267222470044999660 ) ) ;
#35504 = AXIS2_PLACEMENT_3D ( 'NONE', #67351, #62116, #40123 ) ;
#35506 = DIRECTION ( 'NONE',  ( -1.000000000000000000, 0.000000000000000000, 0.000000000000000000 ) ) ;
#35507 = ORIENTED_EDGE ( 'NONE', *, *, #63340, .T. ) ;
#35508 = CARTESIAN_POINT ( 'NONE',  ( 6.227477004709999875, 0.7848946462383999956, 1.064150538460000073 ) ) ;
#35509 = SHAPE_DEFINITION_REPRESENTATION ( #51151, #12958 ) ;
#35510 = CARTESIAN_POINT ( 'NONE',  ( 10.95645069460308108, 8.994232988617600455, 6.417022446611309938 ) ) ;
#35511 = CARTESIAN_POINT ( 'NONE',  ( 11.09999999999999964, 2.685305999535000154, 6.664030027596000494 ) ) ;
#35512 = CARTESIAN_POINT ( 'NONE',  ( 7.832456446343600831, 2.667230532683134481, -7.203453600678752622 ) ) ;
#35513 = CIRCLE ( 'NONE', #28843, 0.7499999936418002555 ) ;
#35514 = CARTESIAN_POINT ( 'NONE',  ( 11.59966954483535773, 4.638989336656000440, -6.514072057539499916 ) ) ;
#35515 = EDGE_LOOP ( 'NONE', ( #19437, #53422, #52270 ) ) ;
#35516 = CARTESIAN_POINT ( 'NONE',  ( 10.85068991645999859, -4.478102922274999287, 6.162028334171000488 ) ) ;
#35517 = VERTEX_POINT ( 'NONE', #32141 ) ;
#35518 = PLANE ( 'NONE',  #54074 ) ;
#35519 = CARTESIAN_POINT ( 'NONE',  ( 7.983191940377000861, -5.321924421352999701, 8.118250081378000971 ) ) ;
#35520 = CARTESIAN_POINT ( 'NONE',  ( 17.93787990420809209, -0.6205713442106968181, -13.98624562867392385 ) ) ;
#35521 = VERTEX_POINT ( 'NONE', #53792 ) ;
#35522 = CARTESIAN_POINT ( 'NONE',  ( 8.525869573596782658, 2.785289313170467462, -8.768765148542382093 ) ) ;
#35523 = CARTESIAN_POINT ( 'NONE',  ( 10.98688827724942207, -5.367975154760490142, -6.994477628653238632 ) ) ;
#35524 = AXIS2_PLACEMENT_3D ( 'NONE', #16484, #37129, #58448 ) ;
#35525 = CARTESIAN_POINT ( 'NONE',  ( 8.128629719589000047, 5.223492654083000453, -6.524203877525000195 ) ) ;
#35526 = CARTESIAN_POINT ( 'NONE',  ( 9.179055905797000037, -2.899999999999999911, 6.571291218949999902 ) ) ;
#35527 = CARTESIAN_POINT ( 'NONE',  ( 8.199995110659001440, -2.894508759333000114, 6.645190873281999089 ) ) ;
#35528 = ORIENTED_EDGE ( 'NONE', *, *, #12235, .F. ) ;
#35529 = CARTESIAN_POINT ( 'NONE',  ( 8.679055905797000037, -2.899999999999999911, 6.571291218949999902 ) ) ;
#35530 = ADVANCED_FACE ( 'NONE', ( #63929 ), #25849, .T. ) ;
#35531 = EDGE_CURVE ( 'NONE', #64134, #36266, #7365, .T. ) ;
#35532 = CARTESIAN_POINT ( 'NONE',  ( 12.24918480870326043, -2.785872542151285547, -13.60860763679505325 ) ) ;
#35533 = CARTESIAN_POINT ( 'NONE',  ( 8.099999999999999645, 0.000000000000000000, 0.000000000000000000 ) ) ;
#35534 = CARTESIAN_POINT ( 'NONE',  ( 10.91944543538999923, -3.268376408192000149, -6.413937436229999456 ) ) ;
#35535 = B_SPLINE_CURVE_WITH_KNOTS ( 'NONE', 3,
 ( #5035, #63413, #42108, #15537, #62726, #31277, #15869, #20776 ),
 .UNSPECIFIED., .F., .F.,
 ( 4, 2, 2, 4 ),
 ( 0.000000000000000000, 0.4999999999999937828, 0.7499999999999968914, 1.000000000000000000 ),
 .UNSPECIFIED. ) ;
#35536 = DIRECTION ( 'NONE',  ( 1.000000000000000000, 0.000000000000000000, 0.000000000000000000 ) ) ;
#35537 = ORIENTED_EDGE ( 'NONE', *, *, #19255, .F. ) ;
#35538 = PRODUCT ( '510 Pin Insulator', '510 Pin Insulator', '', ( #14181 ) ) ;
#35539 = CARTESIAN_POINT ( 'NONE',  ( 23.91426378890381343, 12.84858547818794250, -3.562216227305645244 ) ) ;
#35540 = CARTESIAN_POINT ( 'NONE',  ( 5.240443173017209411, 0.1963495408493638184, -1.499999999999999778 ) ) ;
#35541 = CARTESIAN_POINT ( 'NONE',  ( 24.15455626517813670, -3.324392337986376678, -12.46571004933703719 ) ) ;
#35542 = CARTESIAN_POINT ( 'NONE',  ( 12.80505043854144276, 0.6564304467897672524, 12.64601024127357931 ) ) ;
#35543 = B_SPLINE_CURVE_WITH_KNOTS ( 'NONE', 3,
 ( #56806, #40047, #24296, #24645 ),
 .UNSPECIFIED., .F., .F.,
 ( 4, 4 ),
 ( 0.8745245747709967654, 1.000000000000000000 ),
 .UNSPECIFIED. ) ;
#35544 = CARTESIAN_POINT ( 'NONE',  ( 12.20411985647183428, 0.1720826668005528137, -13.89857125525884207 ) ) ;
#35545 = CARTESIAN_POINT ( 'NONE',  ( 18.14000279917957315, -2.720357798290598428, 12.39752072230842650 ) ) ;
#35546 = ORIENTED_EDGE ( 'NONE', *, *, #60451, .F. ) ;
#35547 = CARTESIAN_POINT ( 'NONE',  ( 10.39969598649000027, -3.111999510220800236, -8.028730309000598808 ) ) ;
#35548 = ORIENTED_EDGE ( 'NONE', *, *, #45280, .T. ) ;
#35549 = CARTESIAN_POINT ( 'NONE',  ( 10.96207813434000045, 5.399835028078000754, 7.743264559064000352 ) ) ;
#35550 = FACE_OUTER_BOUND ( 'NONE', #62099, .T. ) ;
#35551 = CARTESIAN_POINT ( 'NONE',  ( 9.576420280414000175, 4.861259245430999520, -8.806664389576001284 ) ) ;
#35552 = CARTESIAN_POINT ( 'NONE',  ( 2.467998394013000141, 3.220898723588000223, 1.477727276234999998 ) ) ;
#35553 = EDGE_CURVE ( 'NONE', #57489, #47653, #24956, .T. ) ;
#35554 = CARTESIAN_POINT ( 'NONE',  ( 10.20917469696999902, -3.334764780022000163, -5.769478358936999562 ) ) ;
#35555 = CARTESIAN_POINT ( 'NONE',  ( 9.469356963619999235, -5.119357025014000584, 7.500000000085178087 ) ) ;
#35556 = CARTESIAN_POINT ( 'NONE',  ( 23.51695493258000269, 13.43892003569000160, 4.372923714577000354 ) ) ;
#35557 = VERTEX_POINT ( 'NONE', #53454 ) ;
#35558 = AXIS2_PLACEMENT_3D ( 'NONE', #55514, #3392, #2715 ) ;
#35559 = CARTESIAN_POINT ( 'NONE',  ( 12.12994988689360021, -3.481863023525599843, 6.483720595741000459 ) ) ;
#35560 = CARTESIAN_POINT ( 'NONE',  ( 10.48131298037437453, 3.643872424580264724, -9.239416608973755274 ) ) ;
#35561 = CARTESIAN_POINT ( 'NONE',  ( 16.13494720760600032, 9.102952917978999636, 8.658486291235998777 ) ) ;
#35562 = CARTESIAN_POINT ( 'NONE',  ( 7.758191940376999440, -5.797088532631000213, 8.340479314546998424 ) ) ;
#35564 = CARTESIAN_POINT ( 'NONE',  ( 11.09999999999999964, 2.700683852703999577, 5.124965750789000296 ) ) ;
#35563 = CARTESIAN_POINT ( 'NONE',  ( 10.89874804681000064, 2.834828962328999502, 9.088465460431999432 ) ) ;
#35565 = VECTOR ( 'NONE', #27349, 999.9999999999998863 ) ;
#35566 = CARTESIAN_POINT ( 'NONE',  ( 10.47718582084299932, 3.343463760027599818, -6.741111985563299491 ) ) ;
#35567 = DIRECTION ( 'NONE',  ( -0.7071066712931889375, 0.7071068910798888885, -1.670485323815974547E-10 ) ) ;
#35569 = CIRCLE ( 'NONE', #9912, 12.35000000006999876 ) ;
#35568 = CARTESIAN_POINT ( 'NONE',  ( 10.33890035061499901, 4.267716286314199969, -8.468075389605498771 ) ) ;
#35570 = CARTESIAN_POINT ( 'NONE',  ( 17.68572386047929967, 0.7076089047904873253, 12.58011506138060831 ) ) ;
#35571 = DIRECTION ( 'NONE',  ( 0.000000000000000000, 0.9659258262890757507, -0.2588190451024934835 ) ) ;
#35572 = CARTESIAN_POINT ( 'NONE',  ( 11.55300581613033906, 5.107584469683000172, 6.788791567531699656 ) ) ;
#35573 = CARTESIAN_POINT ( 'NONE',  ( 23.61990774387100345, 10.21722221107000017, 9.338757681905001107 ) ) ;
#35574 = EDGE_LOOP ( 'NONE', ( #41461, #47707, #43176, #638, #20723, #68133, #13079, #26227, #13456, #1533, #54962, #30793, #62705, #39077, #23287, #31632, #29863 ) ) ;
#35575 = CARTESIAN_POINT ( 'NONE',  ( 7.358058059621999547, -4.561648098548999997, 6.153050355516999304 ) ) ;
#35576 = B_SPLINE_CURVE_WITH_KNOTS ( 'NONE', 3,
 ( #17539, #28731, #50044, #2154, #23471, #60878, #66112 ),
 .UNSPECIFIED., .F., .F.,
 ( 4, 1, 1, 1, 4 ),
 ( 0.000000000000000000, 0.2500000039165359289, 0.5000000015352937810, 0.7499999991540515776, 1.000000000000000000 ),
 .UNSPECIFIED. ) ;
#35577 = CARTESIAN_POINT ( 'NONE',  ( 7.077542425583873253, -1.465994342824544899E-06, -1.322443989608400816 ) ) ;
#35578 = FACE_OUTER_BOUND ( 'NONE', #7148, .T. ) ;
#35579 = CARTESIAN_POINT ( 'NONE',  ( 10.11792546752099931, 3.135062625344399834, 7.559927309296559983 ) ) ;
#35580 = ORIENTED_EDGE ( 'NONE', *, *, #50407, .F. ) ;
#35581 = AXIS2_PLACEMENT_3D ( 'NONE', #69070, #58580, #30305 ) ;
#35582 = CARTESIAN_POINT ( 'NONE',  ( 7.165489158771000788, 2.688365364125000045, 8.140015608605001063 ) ) ;
#35583 = CARTESIAN_POINT ( 'NONE',  ( 11.51656039236534923, 5.173498198882000132, 7.442888368925779652 ) ) ;
#35584 = CARTESIAN_POINT ( 'NONE',  ( 10.67529528041000120, 3.066676902634999813, -8.703232886886000941 ) ) ;
#35585 = ADVANCED_FACE ( 'NONE', ( #32817 ), #28422, .F. ) ;
#35586 = ORIENTED_EDGE ( 'NONE', *, *, #39003, .F. ) ;
#35587 = ADVANCED_FACE ( 'NONE', ( #23008 ), #8251, .T. ) ;
#35588 = CARTESIAN_POINT ( 'NONE',  ( 11.50000000000000000, -3.008232475376599879, 7.825000000000000178 ) ) ;
#35589 = CARTESIAN_POINT ( 'NONE',  ( 8.609967445932182883, 4.707159105297979096, 5.915074581558411815 ) ) ;
#35590 = CARTESIAN_POINT ( 'NONE',  ( 11.42887348028849992, 2.875789035466000065, 6.892162778124999889 ) ) ;
#35591 = CARTESIAN_POINT ( 'NONE',  ( 11.09999999999999964, 4.000000000000000000, 7.500000000000000000 ) ) ;
#35592 = CARTESIAN_POINT ( 'NONE',  ( 25.60000000000000142, 11.77655473258999841, 4.190794510628000680 ) ) ;
#35593 = ORIENTED_EDGE ( 'NONE', *, *, #46572, .T. ) ;
#35594 = CARTESIAN_POINT ( 'NONE',  ( 11.57299956498156845, 5.207010770456999893, 7.174999999999999822 ) ) ;
#35595 = CARTESIAN_POINT ( 'NONE',  ( 7.218814158767999700, 4.636818559850000909, -5.710024136463999866 ) ) ;
#35596 = CARTESIAN_POINT ( 'NONE',  ( 8.242389367084641094, -5.499373901227779804, 8.386263970964396464 ) ) ;
#35597 = CARTESIAN_POINT ( 'NONE',  ( 10.51414141025500015, -3.384226587288500010, -8.596754040696000132 ) ) ;
#35598 = CARTESIAN_POINT ( 'NONE',  ( 10.45991290906800053, -4.809406943772300380, 6.509421987543800192 ) ) ;
#35599 = VERTEX_POINT ( 'NONE', #39442 ) ;
#35600 = CARTESIAN_POINT ( 'NONE',  ( 10.33327595171000013, -4.639045857913999704, -4.712793788258000660 ) ) ;
#35601 = CARTESIAN_POINT ( 'NONE',  ( 7.100000000000000533, -13.04986661130000059, 1.811520473896000016 ) ) ;
#35602 = ORIENTED_EDGE ( 'NONE', *, *, #45024, .F. ) ;
#35603 = CARTESIAN_POINT ( 'NONE',  ( 25.60000000000000142, 0.000000000000000000, 0.000000000000000000 ) ) ;
#35604 = AXIS2_PLACEMENT_3D ( 'NONE', #11599, #23136, #38172 ) ;
#35605 = ORIENTED_EDGE ( 'NONE', *, *, #57123, .T. ) ;
#35606 = CARTESIAN_POINT ( 'NONE',  ( 9.837156140204001531, -5.811247906278000031, -7.978055797018001272 ) ) ;
#35607 = CYLINDRICAL_SURFACE ( 'NONE', #46098, 1.250000000000000222 ) ;
#35608 = VECTOR ( 'NONE', #19406, 1000.000000000000114 ) ;
#35609 = CARTESIAN_POINT ( 'NONE',  ( 11.22567835872029995, 3.006051690924700370, -6.873560442659099046 ) ) ;
#35610 = CARTESIAN_POINT ( 'NONE',  ( 11.18035971519489813, -3.321859513918399731, 8.628134814664999652 ) ) ;
#35611 = CARTESIAN_POINT ( 'NONE',  ( 12.18751053307000198, 2.401600969044472400, -12.47399295505824135 ) ) ;
#35612 = CARTESIAN_POINT ( 'NONE',  ( 10.99764694612700033, -5.059486515935999407, 7.077178005756699974 ) ) ;
#35613 = CARTESIAN_POINT ( 'NONE',  ( 10.82169598649000086, -3.233475335853099875, 7.043598424555200133 ) ) ;
#35614 = EDGE_CURVE ( 'NONE', #20205, #9159, #18278, .T. ) ;
#35615 = EDGE_CURVE ( 'NONE', #10441, #43157, #11563, .T. ) ;
#35616 = ORIENTED_EDGE ( 'NONE', *, *, #51055, .T. ) ;
#35617 = CARTESIAN_POINT ( 'NONE',  ( 9.461621083092172313, 5.351423275947217562, 7.263649724570491628 ) ) ;
#35618 = EDGE_CURVE ( 'NONE', #53044, #59076, #24098, .T. ) ;
#35619 = CARTESIAN_POINT ( 'NONE',  ( 7.571668146791999732, -2.531197775378000170, 8.216705951490000714 ) ) ;
#35620 = LINE ( 'NONE', #20209, #68088 ) ;
#35621 = EDGE_LOOP ( 'NONE', ( #59321, #32538, #46148, #47740 ) ) ;
#35622 = CARTESIAN_POINT ( 'NONE',  ( 12.49051143973452227, -3.040180064579590891, -12.30914836342242680 ) ) ;
#35623 = CARTESIAN_POINT ( 'NONE',  ( 10.98579841651039857, 3.550031058388499972, 6.303820944768999901 ) ) ;
#35624 = CARTESIAN_POINT ( 'NONE',  ( 11.24323064679000161, -2.479730344050999680, -7.587230764681999418 ) ) ;
#35625 = CARTESIAN_POINT ( 'NONE',  ( 10.84393020684979980, 2.750000000000000000, 7.500000000000000000 ) ) ;
#35626 = CARTESIAN_POINT ( 'NONE',  ( 2.435247277619000172, 2.372532593102000043, -2.573147701680999599 ) ) ;
#35627 = CARTESIAN_POINT ( 'NONE',  ( 7.399258644420781295, -3.999959970822239530, 9.109379115530307658 ) ) ;
#35628 = CARTESIAN_POINT ( 'NONE',  ( 12.54749102628331947, -3.200935012631489496, -13.62916378024774566 ) ) ;
#35629 = CARTESIAN_POINT ( 'NONE',  ( 11.61364291764652812, -4.859654669415900408, -7.393734108507599601 ) ) ;
#35630 = CARTESIAN_POINT ( 'NONE',  ( 10.09964828895399869, -2.878385131502000149, -8.112615456209400833 ) ) ;
#35631 = CARTESIAN_POINT ( 'NONE',  ( 11.59999999999999964, -2.792989229543000107, -7.825000000000000178 ) ) ;
#35632 = EDGE_LOOP ( 'NONE', ( #5835, #26712, #13285, #7284, #52003, #46869 ) ) ;
#35633 = VERTEX_POINT ( 'NONE', #17917 ) ;
#35634 = CARTESIAN_POINT ( 'NONE',  ( 8.082873386424997975, 5.111739203374999541, -6.679001318365999751 ) ) ;
#35635 = LINE ( 'NONE', #56264, #26925 ) ;
#35636 = CARTESIAN_POINT ( 'NONE',  ( 18.17607324740734143, 2.571217238393650906, 13.65805047069406974 ) ) ;
#35637 = CARTESIAN_POINT ( 'NONE',  ( 10.22440590001000160, 5.317411003666999925, -8.272452263128000638 ) ) ;
#35638 = ADVANCED_FACE ( 'NONE', ( #13369 ), #8112, .T. ) ;
#35639 = CARTESIAN_POINT ( 'NONE',  ( 10.64393020684899938, -2.750000000000000000, 7.500000000000000000 ) ) ;
#35640 = CARTESIAN_POINT ( 'NONE',  ( 17.80118387294172422, 3.074517463812005857, 12.29895906470767919 ) ) ;
#35641 = CARTESIAN_POINT ( 'NONE',  ( 23.64082968872000023, -13.18734614699999952, 4.071470701135999626 ) ) ;
#35642 = CARTESIAN_POINT ( 'NONE',  ( 10.28314886242000092, 2.387776420306999992, 7.684265965147999644 ) ) ;
#35643 = CARTESIAN_POINT ( 'NONE',  ( 10.31298165360644425, -2.920330592985297624, -8.329669302950559739 ) ) ;
#35644 = ORIENTED_EDGE ( 'NONE', *, *, #29251, .F. ) ;
#35645 = CARTESIAN_POINT ( 'NONE',  ( 12.37479069268424148, -2.046560891103778701, 12.54575476380192534 ) ) ;
#35646 = CARTESIAN_POINT ( 'NONE',  ( 8.994442991499997930, -4.054579081944059915, -6.634708680083400090 ) ) ;
#35647 = CARTESIAN_POINT ( 'NONE',  ( 11.03856029907000114, 2.974095820320000083, 8.716122353065999917 ) ) ;
#35648 = CARTESIAN_POINT ( 'NONE',  ( 11.60101463001529964, -3.377766160221900016, 8.496586578655598743 ) ) ;
#35649 = CARTESIAN_POINT ( 'NONE',  ( 10.06481084123000080, 5.336630274082000192, -7.092011739486999922 ) ) ;
#35650 = CARTESIAN_POINT ( 'NONE',  ( 10.07503300763299947, 4.881889043637199777, -8.424978748982498544 ) ) ;
#35651 = CARTESIAN_POINT ( 'NONE',  ( 12.61399029061283450, 0.5951698179256255106, 12.68122092285040559 ) ) ;
#35652 = CARTESIAN_POINT ( 'NONE',  ( 8.764829719592999169, 5.808262417891000062, 7.446016144116000213 ) ) ;
#35653 = CARTESIAN_POINT ( 'NONE',  ( 10.00138108374000012, 3.855364958793999985, 5.709478909302000638 ) ) ;
#35654 = CARTESIAN_POINT ( 'NONE',  ( 11.48394322905000031, -3.487217528443999903, 11.17162453992000160 ) ) ;
#35655 = ORIENTED_EDGE ( 'NONE', *, *, #57971, .T. ) ;
#35656 = CARTESIAN_POINT ( 'NONE',  ( 9.137754719594999742, 2.319062457810000311, -7.919229449146000022 ) ) ;
#35657 = CARTESIAN_POINT ( 'NONE',  ( 7.260405367085000172, 1.468527740333999798, -0.2336236082946000214 ) ) ;
#35658 = CARTESIAN_POINT ( 'NONE',  ( 10.94563198394039283, -2.254998712725911236, 7.605124749578603627 ) ) ;
#35659 = DIRECTION ( 'NONE',  ( -1.000000000000000000, 0.000000000000000000, -1.275169027325000072E-14 ) ) ;
#35660 = CARTESIAN_POINT ( 'NONE',  ( 12.09999999999999787, -3.636382150325344842, 8.530211724564091824 ) ) ;
#35661 = CARTESIAN_POINT ( 'NONE',  ( 10.87103032197929942, -3.416314376401300201, -6.683751296690399357 ) ) ;
#35662 = VERTEX_POINT ( 'NONE', #19283 ) ;
#35663 = CARTESIAN_POINT ( 'NONE',  ( 1.486654918706999950, 3.344697682836000219, -1.715043639744999959 ) ) ;
#35664 = CARTESIAN_POINT ( 'NONE',  ( 11.46021572556888657, 2.954248811040025124, 7.824997386306807634 ) ) ;
#35666 = CARTESIAN_POINT ( 'NONE',  ( 13.73854177342199989, -9.465667024606000624, -8.118361260918998568 ) ) ;
#35665 = CARTESIAN_POINT ( 'NONE',  ( 9.931248637830082160, 2.301670995521332141, 7.915216903584279429 ) ) ;
#35667 = CARTESIAN_POINT ( 'NONE',  ( 6.999999691988000095, 12.89129024452999950, -1.677687644161999891 ) ) ;
#35668 = EDGE_CURVE ( 'NONE', #606, #54866, #27213, .T. ) ;
#35669 = ADVANCED_FACE ( 'NONE', ( #23495 ), #12667, .T. ) ;
#35670 = DIRECTION ( 'NONE',  ( 0.000000000000000000, 0.000000000000000000, -1.000000000000000000 ) ) ;
#35671 = CARTESIAN_POINT ( 'NONE',  ( 11.09999999999999964, 2.700000000000000178, 5.160242713806000303 ) ) ;
#35672 = CARTESIAN_POINT ( 'NONE',  ( 25.10992574103807229, -11.36603783439706916, 3.264548188536176010 ) ) ;
#35673 = CARTESIAN_POINT ( 'NONE',  ( 8.373668146795001377, -2.202816532622999812, 7.706987678916999762 ) ) ;
#35674 = ORIENTED_EDGE ( 'NONE', *, *, #33224, .T. ) ;
#35675 = EDGE_CURVE ( 'NONE', #17831, #67057, #55314, .T. ) ;
#35676 = CARTESIAN_POINT ( 'NONE',  ( 8.817635841231000526, 3.894644548817000285, 6.044465307984999924 ) ) ;
#35678 = CARTESIAN_POINT ( 'NONE',  ( 5.000000004069000248, 0.6153845687985000090, 2.423076939105999639 ) ) ;
#35677 = CARTESIAN_POINT ( 'NONE',  ( 6.024350226066000680, -0.9533226957039999672, 1.303269410926999994 ) ) ;
#35679 = AXIS2_PLACEMENT_3D ( 'NONE', #60265, #32661, #43498 ) ;
#35680 = CARTESIAN_POINT ( 'NONE',  ( 7.454383804049630413, -2.263917759343326619, 7.386920749780896855 ) ) ;
#35681 = DIRECTION ( 'NONE',  ( 0.000000000000000000, -1.000000000000000000, 0.000000000000000000 ) ) ;
#35682 = CARTESIAN_POINT ( 'NONE',  ( 1.128155746510000057, 3.563994061069000185, 0.4492161910706000127 ) ) ;
#35683 = EDGE_LOOP ( 'NONE', ( #20458, #26002, #34241, #42220 ) ) ;
#35684 = CARTESIAN_POINT ( 'NONE',  ( 1.667822546892261393, 0.6772077056339234069, -3.232625950882237031 ) ) ;
#35685 = CARTESIAN_POINT ( 'NONE',  ( 10.80903300763299946, -3.402282662142699809, 6.873077781830399857 ) ) ;
#35686 = PLANE ( 'NONE',  #9590 ) ;
#35687 = CARTESIAN_POINT ( 'NONE',  ( 9.423523952092001110, 4.993991073313000406, 8.578107851305000864 ) ) ;
#35688 = CARTESIAN_POINT ( 'NONE',  ( 11.45764291764649911, 2.867875922590999771, 7.639947095788999221 ) ) ;
#35689 = CARTESIAN_POINT ( 'NONE',  ( 8.474485200571999499, -5.100000000000000533, 6.560614371780999043 ) ) ;
#35690 = CARTESIAN_POINT ( 'NONE',  ( 18.49995202021990082, 2.953582884394188479, -12.17185907300008907 ) ) ;
#35691 = CARTESIAN_POINT ( 'NONE',  ( 10.99937785741359519, -5.205492584227198627, 6.645915226615812799 ) ) ;
#35692 = CARTESIAN_POINT ( 'NONE',  ( 7.717636619252205676, 5.722644694260130116, 7.867024080253358420 ) ) ;
#35693 = VERTEX_POINT ( 'NONE', #50764 ) ;
#35694 = CARTESIAN_POINT ( 'NONE',  ( 18.20032535889736280, -2.850937372247259738, 13.70665064220730578 ) ) ;
#35696 = EDGE_CURVE ( 'NONE', #35912, #15625, #38385, .T. ) ;
#35695 = CARTESIAN_POINT ( 'NONE',  ( 18.18005044212796051, -2.500000099754955851, 13.67345740034994783 ) ) ;
#35697 = VERTEX_POINT ( 'NONE', #50074 ) ;
#35698 = CARTESIAN_POINT ( 'NONE',  ( 8.933148997457999840, -5.167567567567999731, 6.822293592207000934 ) ) ;
#35699 = CARTESIAN_POINT ( 'NONE',  ( 9.099999931440999390, -2.753634353389999845, -7.404749409716440134 ) ) ;
#35700 = CARTESIAN_POINT ( 'NONE',  ( 8.491228313223627922, 4.376000986002790860, 5.973597461995679758 ) ) ;
#35701 = CARTESIAN_POINT ( 'NONE',  ( 11.34287482311539996, 4.803125295093300551, 7.175518335304800210 ) ) ;
#35702 = CARTESIAN_POINT ( 'NONE',  ( 10.24961997674000003, 4.184221916050000267, 9.286882020979000174 ) ) ;
#35703 = CARTESIAN_POINT ( 'NONE',  ( 7.000000000000000000, -0.2897247358851999799, -3.000000000000000000 ) ) ;
#35704 = CARTESIAN_POINT ( 'NONE',  ( 8.948279512853625661, -3.525202972512352595, -6.765085003841553757 ) ) ;
#35705 = CARTESIAN_POINT ( 'NONE',  ( 10.90638082498000117, -5.227498618488000126, 6.784459667733999666 ) ) ;
#35706 = CARTESIAN_POINT ( 'NONE',  ( 18.27538032657187017, 0.08234928811777227076, -12.59973629603894274 ) ) ;
#35707 = CARTESIAN_POINT ( 'NONE',  ( 9.973487588364999823, -4.344961837988999598, -9.321582626371998970 ) ) ;
#35708 = CARTESIAN_POINT ( 'NONE',  ( 10.55518582084299872, -4.566724035220099509, -6.844925608615599621 ) ) ;
#35709 = CARTESIAN_POINT ( 'NONE',  ( 10.90227388941000086, -5.099948884123999271, -5.143660596970000221 ) ) ;
#35710 = ORIENTED_EDGE ( 'NONE', *, *, #3707, .F. ) ;
#35711 = CARTESIAN_POINT ( 'NONE',  ( 9.522188178962254668, -4.591134893453497234, 6.476088678109181984 ) ) ;
#35712 = CARTESIAN_POINT ( 'NONE',  ( 9.018359312501498692, 5.126777126186109257, -6.752018918873272213 ) ) ;
#35713 = CARTESIAN_POINT ( 'NONE',  ( 10.39393020684999946, -5.250000000000000000, -7.500000000000000000 ) ) ;
#35714 = ADVANCED_FACE ( 'NONE', ( #44498 ), #24991, .F. ) ;
#35715 = CARTESIAN_POINT ( 'NONE',  ( 8.206872618705004285, 10.60779917172999376, 4.026525179214997863 ) ) ;
#35716 = CARTESIAN_POINT ( 'NONE',  ( 12.13953890720636863, 2.807801093580546858, 13.71555245415304292 ) ) ;
#35717 = CARTESIAN_POINT ( 'NONE',  ( 9.298040139821001304, -4.087076480742000584, 9.429402848390999736 ) ) ;
#35718 = ORIENTED_EDGE ( 'NONE', *, *, #22490, .T. ) ;
#35719 = CARTESIAN_POINT ( 'NONE',  ( 12.41699802696285992, 0.4899468513230743061, -12.68727699267097719 ) ) ;
#35720 = CARTESIAN_POINT ( 'NONE',  ( 12.75735126819566290, -0.7290235424212101467, 13.98100605002522734 ) ) ;
#35721 = ORIENTED_EDGE ( 'NONE', *, *, #61088, .T. ) ;
#35722 = CARTESIAN_POINT ( 'NONE',  ( 25.39994675557665005, 2.060146035114244878, -11.21225038255773043 ) ) ;
#35723 = DIRECTION ( 'NONE',  ( 0.000000000000000000, 1.000000000000000000, -3.576848554708999905E-13 ) ) ;
#35724 = AXIS2_PLACEMENT_3D ( 'NONE', #264, #58647, #10748 ) ;
#35725 = CARTESIAN_POINT ( 'NONE',  ( 1.849999551004999798, 1.625000000000000000, 0.000000000000000000 ) ) ;
#35726 = CARTESIAN_POINT ( 'NONE',  ( 11.32595391537419971, -3.283439621430300104, 7.013338090450799811 ) ) ;
#35727 = B_SPLINE_SURFACE_WITH_KNOTS ( 'NONE', 3, 3, ( 
 ( #15178, #33249, #49314, #44091, #18203, #23786, #45122, #5376, #54912, #49666, #55611, #12965, #39879, #34289, #2126, #50018, #23446, #1427, #17863, #2462, #28702, #31957, #33595, #60163, #26713, #11910, #7357, #1775, #38837, #54568, #60502, #6665, #18550, #66083, #130, #61196, #22742, #38484, #59807, #43739, #12267, #44442, #65035, #33942, #50363, #7712, #29052, #7015, #66429, #65740, #17152, #12611, #44783, #28350, #48027, #39526, #21447, #60850, #65389, #55263, #28005, #39179, #53274, #17511, #23093, #35320, #46834 ),
 ( #61537, #62219, #67115, #29398, #8400, #29745, #46492, #50707, #8741, #13317, #8056, #56638, #30086, #40898, #9411, #30755, #19578, #68140, #14338, #34980, #19918, #20257, #41243, #51048, #61879, #51726, #18895, #2804, #34640, #24130, #62555, #67798, #3149, #3485, #3821, #45465, #14677, #9078, #35661, #40221, #66779, #56297, #13652, #4168, #56976, #30415, #40550, #25159, #24480, #45803, #19224, #13995, #51389, #24821, #46147, #35993, #52062, #57309, #25505, #67453, #41583, #55951, #25847, #42618, #53452, #58344, #36339 ),
 ( #15703, #52761, #5205, #5547, #15362, #53790, #63586, #69176, #21287, #62893, #26887, #26544, #41927, #63926, #47523, #9759, #58011, #10112, #48202, #31109, #10447, #15013, #57653, #37032, #31788, #16037, #59039, #11141, #37369, #27227, #58689, #36688, #307, #48551, #21623, #31443, #42284, #32139, #68478, #52414, #4507, #47176, #42959, #64266, #4854, #53105, #16381, #20602, #37711, #10793, #32476, #63235, #26198, #68829, #20950, #5886, #654, #21967, #47869, #39095, #23360, #33163, #2378, #28260, #59722, #49579, #43306 ),
 ( #11824, #6229, #54132, #7276, #49231, #54480, #60077, #12181, #17065, #6581, #27569, #48897, #17777, #1002, #12525, #64613, #28615, #54827, #60420, #34203, #50276, #44699, #33511, #27921, #64951, #22314, #43656, #18120, #1340, #38397, #22656, #6926, #44354, #2040, #65655, #33856, #55172, #1688, #44000, #23005, #65307, #59375, #17422, #38750, #49929, #11476, #65995, #16720, #38050, #39439, #60759, #12876, #55521, #7623, #28969, #32815, #13908, #2721, #67366, #3738, #19490, #45380, #56207, #51304, #55866, #39789, #45036 ) ),
 .UNSPECIFIED., .F., .F., .F.,
 ( 4, 4 ),
 ( 4, 1, 1, 1, 1, 1, 1, 1, 1, 1, 1, 1, 1, 1, 1, 1, 1, 1, 1, 1, 1, 1, 1, 1, 1, 1, 1, 1, 1, 1, 1, 1, 1, 1, 1, 1, 1, 1, 1, 1, 1, 1, 1, 1, 1, 1, 1, 1, 1, 1, 1, 1, 1, 1, 1, 1, 1, 1, 1, 1, 1, 1, 1, 1, 4 ),
 ( -0.02000000000000000042, 1.020000000000000018 ),
 ( 0.008747244164287000176, 0.02453926110774999961, 0.04033127805120999970, 0.05612329499467000327, 0.07191531193812999989, 0.08770732888158999652, 0.1034993458251000087, 0.1192913627684999978, 0.1350833797120000179, 0.1508753966553999792, 0.1666674135988999994, 0.1824594305423999918, 0.1982514474858000086, 0.2140434644293000011, 0.2298354813727000179, 0.2456274983162000103, 0.2614195152596999749, 0.2772115322030999640, 0.2930035491465999842, 0.3087955660900000288, 0.3245875830334999934, 0.3403795999769999581, 0.3561716169204000026, 0.3719636338639000228, 0.3877556508073999875, 0.4035476677507999765, 0.4193396846942999967, 0.4351317016376999858, 0.4509237185811999504, 0.4667157355247000261, 0.4825077524681000152, 0.4982997694115999798, 0.5140917863550000799, 0.5298838032985000446, 0.5456758202420000092, 0.5614678371854000538, 0.5772598541289000185, 0.5930518710723000630, 0.6088438880158000277, 0.6246359049592999924, 0.6404279219027000369, 0.6562199388462000016, 0.6720119557896999662, 0.6878039727331000108, 0.7035959896765999755, 0.7193880066200000201, 0.7351800235634999847, 0.7509720405069999494, 0.7667640574504001050, 0.7825560743939000696, 0.7983480913373000032, 0.8141401082808000789, 0.8299321252243000435, 0.8457241421676999771, 0.8615161591112000528, 0.8773081760545999863, 0.8931001929981000620, 0.9088922099416000266, 0.9246842268849999602, 0.9404762438285000359, 0.9562682607720000005, 0.9720602777153999341, 0.9878522946589000098, 1.003644311601999961, 1.019436328545999970 ),
 .UNSPECIFIED. ) ;
#35728 = CARTESIAN_POINT ( 'NONE',  ( 23.59999999999999787, 12.52456229676467103, -6.096442089472905224 ) ) ;
#35729 = CARTESIAN_POINT ( 'NONE',  ( 0.06325325710666998558, 2.727922606149000284, -2.252402744047000471 ) ) ;
#35730 = CARTESIAN_POINT ( 'NONE',  ( 7.997739111735369555, 4.828320830117592166, 8.578514095141908768 ) ) ;
#35731 = CARTESIAN_POINT ( 'NONE',  ( 19.99999987597299977, 0.000000000000000000, 5.040412531797999279E-14 ) ) ;
#35732 = B_SPLINE_CURVE_WITH_KNOTS ( 'NONE', 3,
 ( #62584, #35690, #35010, #61565, #24510, #56326, #41615, #9106, #14706, #29776, #30444, #51756, #36023, #57338 ),
 .UNSPECIFIED., .F., .F.,
 ( 4, 2, 2, 2, 2, 2, 4 ),
 ( 0.000000000000000000, 0.1250000000000010270, 0.2500000000000020539, 0.5000000000000017764, 0.6250000000000012212, 0.7500000000000006661, 1.000000000000000000 ),
 .UNSPECIFIED. ) ;
#35733 = DIRECTION ( 'NONE',  ( -0.7071067811865475727, 0.7071067811865475727, 0.000000000000000000 ) ) ;
#35734 = CARTESIAN_POINT ( 'NONE',  ( 11.65871932425156920, 3.852858594438699935, -8.492622906483498824 ) ) ;
#35735 = CARTESIAN_POINT ( 'NONE',  ( 1.240556799208374805, -3.500000000000003109, 0.4581489286484972667 ) ) ;
#35736 = CARTESIAN_POINT ( 'NONE',  ( 10.69568717260499824, 3.533932086969799879, -8.260703168378098482 ) ) ;
#35737 = CARTESIAN_POINT ( 'NONE',  ( 8.999417874593998334, 2.949199072237000063, -7.946712276748498560 ) ) ;
#35739 = DIRECTION ( 'NONE',  ( -1.000000000000000000, 0.000000000000000000, 0.000000000000000000 ) ) ;
#35738 = CARTESIAN_POINT ( 'NONE',  ( 8.599999986286999132, 3.249999986289399789, 7.500000000038047787 ) ) ;
#35740 = CARTESIAN_POINT ( 'NONE',  ( 23.57173046905473868, -13.34896468215902843, 4.180125146958469706 ) ) ;
#35741 = ORIENTED_EDGE ( 'NONE', *, *, #2357, .T. ) ;
#35742 = CARTESIAN_POINT ( 'NONE',  ( 10.61257802013489737, 3.108115747127599970, 7.520762592984879369 ) ) ;
#35743 = CARTESIAN_POINT ( 'NONE',  ( 9.285767973100965023, 5.375727035179655111, -6.377217275772713023 ) ) ;
#35744 = CARTESIAN_POINT ( 'NONE',  ( 10.00760887879199856, 3.803658216258800184, 8.344486736701099971 ) ) ;
#35745 = CARTESIAN_POINT ( 'NONE',  ( 23.58303186465700207, -2.940599899367999814, 13.62861925944999975 ) ) ;
#35746 = ADVANCED_FACE ( 'NONE', ( #31500 ), #67856, .T. ) ;
#35747 = EDGE_CURVE ( 'NONE', #64753, #18982, #25215, .T. ) ;
#35748 = CARTESIAN_POINT ( 'NONE',  ( 23.89320776801300283, 12.21745654473000542, -3.256241354580001524 ) ) ;
#35749 = CARTESIAN_POINT ( 'NONE',  ( 21.47500033997000202, -1.509903313490000218E-14, 4.329869796037999436E-14 ) ) ;
#35750 = CARTESIAN_POINT ( 'NONE',  ( 44.24148000000000280, 11.77655473258999841, 4.190794510628000680 ) ) ;
#35751 = EDGE_LOOP ( 'NONE', ( #60900, #7373, #46783, #38496 ) ) ;
#35752 = EDGE_CURVE ( 'NONE', #43226, #27541, #47583, .T. ) ;
#35753 = ADVANCED_FACE ( 'NONE', ( #37088 ), #17819, .T. ) ;
#35754 = CARTESIAN_POINT ( 'NONE',  ( 10.01057120343299900, -4.062009413492949861, -8.777708647662999297 ) ) ;
#35755 = DIRECTION ( 'NONE',  ( 0.000000000000000000, 0.9867381147929490393, 0.1623203401144079905 ) ) ;
#35756 = CARTESIAN_POINT ( 'NONE',  ( 11.81900581613029999, -3.249313226592100534, 7.017964743997199939 ) ) ;
#35757 = B_SPLINE_CURVE_WITH_KNOTS ( 'NONE', 3,
 ( #35159, #63065, #62397, #14852, #24995, #14171, #41079, #36174, #67979, #57840 ),
 .UNSPECIFIED., .F., .F.,
 ( 4, 2, 2, 2, 4 ),
 ( 0.000000000000000000, 0.1886333293263050825, 0.3772666586526101651, 0.5658999879789150533, 0.7545333173052201081 ),
 .UNSPECIFIED. ) ;
#35758 = CARTESIAN_POINT ( 'NONE',  ( 17.65791272883255303, 3.116819718221111035, -12.28623542600055174 ) ) ;
#35759 = CARTESIAN_POINT ( 'NONE',  ( 9.048302809847001527, -2.866747332746000243, -6.341063895044004362 ) ) ;
#35760 = DIRECTION ( 'NONE',  ( 0.000000000000000000, 0.5000000000000169864, -0.8660254037844288266 ) ) ;
#35761 = CARTESIAN_POINT ( 'NONE',  ( 12.19221373227584237, 2.622703613139459655, -13.64666900996694388 ) ) ;
#35762 = CARTESIAN_POINT ( 'NONE',  ( 11.51811411617009817, -5.026960591456000493, 7.174999999999999822 ) ) ;
#35763 = CARTESIAN_POINT ( 'NONE',  ( 24.67333021737300314, 12.15929973297999922, 3.026485043723000423 ) ) ;
#35764 = CARTESIAN_POINT ( 'NONE',  ( 9.548601287889788125, -3.999999532294070459, 6.301404677806389465 ) ) ;
#35765 = CARTESIAN_POINT ( 'NONE',  ( 12.36383866360284145, 0.5795518042670567693, -13.98800095993140857 ) ) ;
#35766 = FACE_OUTER_BOUND ( 'NONE', #15651, .T. ) ;
#35767 = CARTESIAN_POINT ( 'NONE',  ( 8.266851002545999805, -2.832432432432000269, 6.822293592207000934 ) ) ;
#35768 = DIRECTION ( 'NONE',  ( 0.000000000000000000, 0.000000000000000000, -1.000000000000000000 ) ) ;
#35769 = EDGE_CURVE ( 'NONE', #7194, #15848, #51760, .T. ) ;
#35770 = B_SPLINE_CURVE_WITH_KNOTS ( 'NONE', 3,
 ( #46124, #40200, #18528, #61174 ),
 .UNSPECIFIED., .F., .F.,
 ( 4, 4 ),
 ( 0.8745969165622392572, 1.000000000000000000 ),
 .UNSPECIFIED. ) ;
#35771 = CARTESIAN_POINT ( 'NONE',  ( 18.01256889503379099, -11.20125638878304208, 3.203298770433383513 ) ) ;
#35772 = CARTESIAN_POINT ( 'NONE',  ( 12.26133460557259980, -3.860150918677800025, 6.645166161828299778 ) ) ;
#35773 = ORIENTED_EDGE ( 'NONE', *, *, #17138, .T. ) ;
#35774 = CARTESIAN_POINT ( 'NONE',  ( 8.507804550190643411, -4.678883388517643738, 8.679043930492003511 ) ) ;
#35775 = CARTESIAN_POINT ( 'NONE',  ( 18.27043923978326490, 2.638421884002155160, -13.74915584829237680 ) ) ;
#35776 = EDGE_LOOP ( 'NONE', ( #2762, #33457, #66364, #35321 ) ) ;
#35777 = CARTESIAN_POINT ( 'NONE',  ( 9.782063610505000284, -3.644370728184199937, 6.709281487801199262 ) ) ;
#35778 = CARTESIAN_POINT ( 'NONE',  ( 2.571806799210416550, 3.408904368339104263, 0.9161175952574878156 ) ) ;
#35779 = CARTESIAN_POINT ( 'NONE',  ( 18.33131097849702229, 3.122881743061651783, -11.22368843778023439 ) ) ;
#35780 = CARTESIAN_POINT ( 'NONE',  ( 13.50006915090078152, 9.429349056561928677, 7.934633652400466808 ) ) ;
#35781 = CARTESIAN_POINT ( 'NONE',  ( 10.97635090131019986, -3.000792947412299849, -8.118017011233499503 ) ) ;
#35782 = CARTESIAN_POINT ( 'NONE',  ( 11.59999999999999964, -3.304217902137881691, -6.595854147058992645 ) ) ;
#35783 = DIRECTION ( 'NONE',  ( 0.000000000000000000, 0.000000000000000000, -1.000000000000000000 ) ) ;
#35784 = ORIENTED_EDGE ( 'NONE', *, *, #3934, .T. ) ;
#35785 = CARTESIAN_POINT ( 'NONE',  ( 10.05333291544899943, 4.531093146757585011, -8.658936933361781385 ) ) ;
#35786 = B_SPLINE_CURVE_WITH_KNOTS ( 'NONE', 3,
 ( #39837, #2423, #35627, #29708 ),
 .UNSPECIFIED., .F., .F.,
 ( 4, 4 ),
 ( 0.000000000000000000, 1.000000000000000000 ),
 .UNSPECIFIED. ) ;
#35787 = CARTESIAN_POINT ( 'NONE',  ( 9.576420280414000175, 4.861259245430999520, -8.806664389576001284 ) ) ;
#35788 = ORIENTED_EDGE ( 'NONE', *, *, #6686, .F. ) ;
#35789 = CARTESIAN_POINT ( 'NONE',  ( 10.51140238467000110, 2.326714339996000191, -7.741210149842999932 ) ) ;
#35790 =( NAMED_UNIT ( * ) SI_UNIT ( $, .STERADIAN. ) SOLID_ANGLE_UNIT ( ) );
#35791 = ORIENTED_EDGE ( 'NONE', *, *, #25309, .T. ) ;
#35792 = CARTESIAN_POINT ( 'NONE',  ( 9.784621437244998887, 4.758411336345700349, 8.353549467159899322 ) ) ;
#35793 = CARTESIAN_POINT ( 'NONE',  ( 17.55505043854147118, -3.199698446519380735, -12.18695736643652339 ) ) ;
#35794 = EDGE_CURVE ( 'NONE', #46842, #10663, #27434, .T. ) ;
#35795 = CARTESIAN_POINT ( 'NONE',  ( 16.13125657743222519, 3.735736757533928198, 11.95504925863862411 ) ) ;
#35796 = ADVANCED_FACE ( 'NONE', ( #22293 ), #40633, .F. ) ;
#35797 = CARTESIAN_POINT ( 'NONE',  ( 4.400045583829395923, -0.1517171157701598105, 1.464984729050318846 ) ) ;
#35798 = CARTESIAN_POINT ( 'NONE',  ( 25.59997036749100374, 2.856417224717999748, 11.13959153667999935 ) ) ;
#35799 = ORIENTED_EDGE ( 'NONE', *, *, #27979, .T. ) ;
#35800 = DIRECTION ( 'NONE',  ( 0.000000000000000000, 1.000000000000000000, 2.114232622412000242E-14 ) ) ;
#35801 = CARTESIAN_POINT ( 'NONE',  ( 10.80374834123000127, 2.766954612461999918, -8.073381085840999560 ) ) ;
#35802 = CARTESIAN_POINT ( 'NONE',  ( 3.999999173945999686, 0.000000000000000000, 0.000000000000000000 ) ) ;
#35803 = CARTESIAN_POINT ( 'NONE',  ( 18.30000000000000071, -2.818741034879777008, 11.83575128182368452 ) ) ;
#35804 = CIRCLE ( 'NONE', #29134, 1.449999999999999956 ) ;
#35805 = CARTESIAN_POINT ( 'NONE',  ( 18.27538073532129914, 0.08359636179364303421, 13.99975542440154186 ) ) ;
#35806 = CARTESIAN_POINT ( 'NONE',  ( 8.716851002545999094, -2.832432432432000269, 6.822293592207000934 ) ) ;
#35807 = LINE ( 'NONE', #13121, #33053 ) ;
#35808 = ORIENTED_EDGE ( 'NONE', *, *, #100, .T. ) ;
#35809 = ORIENTED_EDGE ( 'NONE', *, *, #17755, .T. ) ;
#35810 = CARTESIAN_POINT ( 'NONE',  ( 9.468110841233000841, 4.082930418187999955, -6.104944817728999773 ) ) ;
#35811 = CARTESIAN_POINT ( 'NONE',  ( 9.201178352479098876, 5.768932051408849127, 7.515051652316785180 ) ) ;
#35812 = CARTESIAN_POINT ( 'NONE',  ( 10.10000000000000142, 11.84999999999999964, 0.000000000000000000 ) ) ;
#35813 = FACE_OUTER_BOUND ( 'NONE', #19709, .T. ) ;
#35814 = CARTESIAN_POINT ( 'NONE',  ( 24.33654939907400205, 8.941170855541997753, -9.047257172721998586 ) ) ;
#35816 = AXIS2_PLACEMENT_3D ( 'NONE', #35161, #41080, #51902 ) ;
#35815 = LINE ( 'NONE', #51883, #29329 ) ;
#35818 = CARTESIAN_POINT ( 'NONE',  ( 2.285684048949442104, 2.196238783330880739, -2.381962904619033594 ) ) ;
#35817 = CARTESIAN_POINT ( 'NONE',  ( 10.38498825978699891, -4.149395984695000372, 6.368003848175999515 ) ) ;
#35819 = PLANE ( 'NONE',  #35261 ) ;
#35820 = ORIENTED_EDGE ( 'NONE', *, *, #9052, .T. ) ;
#35821 = CARTESIAN_POINT ( 'NONE',  ( 9.893930206848997599, 2.750000000000000000, -7.500000000000000000 ) ) ;
#35822 = CARTESIAN_POINT ( 'NONE',  ( 10.36995232148000134, -3.372430527473000428, -5.009914361523000181 ) ) ;
#35823 = CARTESIAN_POINT ( 'NONE',  ( 9.707733921870000060, -2.624754973437999794, -6.486841649805000110 ) ) ;
#35824 = CARTESIAN_POINT ( 'NONE',  ( 17.55505043854143565, 1.787816316115923954, -13.88537766212463254 ) ) ;
#35825 = CARTESIAN_POINT ( 'NONE',  ( 25.39994675514505218, -2.060146016733654939, 11.21225038637377303 ) ) ;
#35826 = CARTESIAN_POINT ( 'NONE',  ( 11.12299956498149811, -2.792989229543000107, -7.825000000000000178 ) ) ;
#35827 = CYLINDRICAL_SURFACE ( 'NONE', #67782, 1.000000000000000222 ) ;
#35828 = EDGE_CURVE ( 'NONE', #79, #21742, #26112, .T. ) ;
#35829 = EDGE_CURVE ( 'NONE', #35353, #51133, #1317, .T. ) ;
#35830 = DIRECTION ( 'NONE',  ( -1.000000000000000000, 0.000000000000000000, 0.000000000000000000 ) ) ;
#35831 = CARTESIAN_POINT ( 'NONE',  ( 7.913666363270997373, -4.616745235331003450, 6.306613118563004328 ) ) ;
#35832 = CARTESIAN_POINT ( 'NONE',  ( 17.60000000798000386, 11.41069016990000051, -4.623987642516999230 ) ) ;
#35833 = CARTESIAN_POINT ( 'NONE',  ( 0.2417516622353175770, 2.832911453320530626, 1.631798746758986285 ) ) ;
#35834 = CARTESIAN_POINT ( 'NONE',  ( 2.919519622344000087, 0.1980832466146000004, 3.253006245077000091 ) ) ;
#35835 = ORIENTED_EDGE ( 'NONE', *, *, #33277, .T. ) ;
#35836 = CARTESIAN_POINT ( 'NONE',  ( 12.44117949531283784, -0.5082598251325813887, -12.68630931495243530 ) ) ;
#35837 = CARTESIAN_POINT ( 'NONE',  ( 12.18236035867607292, -2.554391060938209446, -12.43872824569138480 ) ) ;
#35838 = CARTESIAN_POINT ( 'NONE',  ( 12.80505043854146940, -1.787816316115923287, 13.88537766212463076 ) ) ;
#35839 = CARTESIAN_POINT ( 'NONE',  ( 8.577614158774000686, 3.981661882377999895, 8.959227447876999761 ) ) ;
#35840 = DIRECTION ( 'NONE',  ( -1.000000000000000000, 0.000000000000000000, 0.000000000000000000 ) ) ;
#35841 = ORIENTED_EDGE ( 'NONE', *, *, #63645, .T. ) ;
#35842 = DIRECTION ( 'NONE',  ( -1.000000000000000000, 0.000000000000000000, 0.000000000000000000 ) ) ;
#35843 = SHAPE_DEFINITION_REPRESENTATION ( #62322, #22871 ) ;
#35844 = CARTESIAN_POINT ( 'NONE',  ( 17.71610594224511814, 0.6042361945079729457, 12.68064620453998792 ) ) ;
#35845 = EDGE_CURVE ( 'NONE', #43188, #47743, #31765, .T. ) ;
#35846 = CARTESIAN_POINT ( 'NONE',  ( 12.96937411412500119, -11.64648275985999959, -1.863025408066000033 ) ) ;
#35847 = CARTESIAN_POINT ( 'NONE',  ( 7.810846861326904644, 3.150764258446524746, 6.417811892696772880 ) ) ;
#35848 = CARTESIAN_POINT ( 'NONE',  ( 10.43614141025499897, 4.549633050978300730, -8.478951440767898973 ) ) ;
#35849 = VERTEX_POINT ( 'NONE', #27204 ) ;
#35850 = CARTESIAN_POINT ( 'NONE',  ( 10.51654446536000087, -4.930670681812999945, 8.573593359022000371 ) ) ;
#35851 = ORIENTED_EDGE ( 'NONE', *, *, #36133, .F. ) ;
#35852 = CIRCLE ( 'NONE', #62636, 1.000000000000000444 ) ;
#35853 = CARTESIAN_POINT ( 'NONE',  ( 9.374309343116463467, 4.497301283948258899, 9.030649165034382975 ) ) ;
#35854 = CARTESIAN_POINT ( 'NONE',  ( 8.368316940379001423, -4.780993534312999671, 6.267212032957000467 ) ) ;
#35855 = CARTESIAN_POINT ( 'NONE',  ( 15.91386961183700244, 8.663061527162000175, 7.870519177131000355 ) ) ;
#35856 = ORIENTED_EDGE ( 'NONE', *, *, #57288, .F. ) ;
#35857 = CARTESIAN_POINT ( 'NONE',  ( 16.39999999439439549, 3.511866690759578802, 11.95216930658972032 ) ) ;
#35858 = DIRECTION ( 'NONE',  ( -1.000000000000000000, 0.000000000000000000, 0.000000000000000000 ) ) ;
#35859 = VECTOR ( 'NONE', #19393, 1000.000000000000114 ) ;
#35860 = CARTESIAN_POINT ( 'NONE',  ( 7.780554719587999379, 4.514357753279999663, -8.978030925517998639 ) ) ;
#35861 = B_SPLINE_CURVE_WITH_KNOTS ( 'NONE', 3,
 ( #23682, #25056, #56876, #40791, #68378, #36234, #41145, #26094, #9656, #10005, #35560, #20845, #15258, #25747, #46387, #8975, #62454, #30314, #10350, #47077, #20499, #57552 ),
 .UNSPECIFIED., .F., .F.,
 ( 4, 2, 2, 2, 2, 2, 2, 2, 2, 2, 4 ),
 ( 0.000000000000000000, 0.1249999999999992506, 0.2499999999999985012, 0.3124999999999983902, 0.3749999999999982792, 0.4999999999999984457, 0.6249999999999985567, 0.7499999999999986677, 0.8124999999999990008, 0.8749999999999993339, 1.000000000000000000 ),
 .UNSPECIFIED. ) ;
#35862 = CARTESIAN_POINT ( 'NONE',  ( 10.12435795695566476, 5.250000000000000000, 7.192559817601734906 ) ) ;
#35863 = CARTESIAN_POINT ( 'NONE',  ( 17.81528574998987580, -3.068593513700731190, 12.30074760041515880 ) ) ;
#35864 = ORIENTED_EDGE ( 'NONE', *, *, #27795, .T. ) ;
#35865 = DIRECTION ( 'NONE',  ( 0.000000000000000000, 0.000000000000000000, -1.000000000000000000 ) ) ;
#35866 = CARTESIAN_POINT ( 'NONE',  ( 12.18133850337606461, -2.541372565769276282, -13.66455005695259572 ) ) ;
#35867 = FACE_OUTER_BOUND ( 'NONE', #31756, .T. ) ;
#35868 = EDGE_LOOP ( 'NONE', ( #59982, #1985, #68637, #16935 ) ) ;
#35869 = CARTESIAN_POINT ( 'NONE',  ( 10.09454055528000005, -5.362855569781999954, -7.550030734599999960 ) ) ;
#35870 = CARTESIAN_POINT ( 'NONE',  ( 10.76947109217999810, -5.100000000000000533, -6.152188490330000370 ) ) ;
#35871 = ORIENTED_EDGE ( 'NONE', *, *, #32690, .F. ) ;
#35872 = CARTESIAN_POINT ( 'NONE',  ( 10.73362722026812932, 5.594669424171384797, 8.214019094825715683 ) ) ;
#35873 = CARTESIAN_POINT ( 'NONE',  ( 5.209193173017084177, -0.3926218265389190276, -1.460959015002473826 ) ) ;
#35874 = DIRECTION ( 'NONE',  ( -1.000000000000000000, 0.000000000000000000, 0.000000000000000000 ) ) ;
#35875 = CARTESIAN_POINT ( 'NONE',  ( 9.349999778958000718, -4.000000000000000000, 6.500000166194499940 ) ) ;
#35876 = EDGE_CURVE ( 'NONE', #6623, #46086, #17402, .T. ) ;
#35877 = CARTESIAN_POINT ( 'NONE',  ( 12.24428838907443229, -0.2761834754990900032, -13.89631168292871344 ) ) ;
#35878 = CARTESIAN_POINT ( 'NONE',  ( 17.83452421831951895, -1.940868773865736197, 12.56443418441918780 ) ) ;
#35879 = VERTEX_POINT ( 'NONE', #17043 ) ;
#35880 = CARTESIAN_POINT ( 'NONE',  ( 8.186778834302003816, -5.111320685747004156, 6.695945149192998436 ) ) ;
#35881 = ORIENTED_EDGE ( 'NONE', *, *, #20937, .F. ) ;
#35882 = CARTESIAN_POINT ( 'NONE',  ( 10.68362359175999998, 2.603561947343000060, 7.762063351517999976 ) ) ;
#35883 = DIRECTION ( 'NONE',  ( 0.000000000000000000, -0.9539392014169415512, -0.3000000000000128120 ) ) ;
#35884 = CARTESIAN_POINT ( 'NONE',  ( 9.427245280414000561, 4.989193221215000307, -6.287302145481000082 ) ) ;
#35885 = CARTESIAN_POINT ( 'NONE',  ( 3.180586773128999845, -3.540884173372999655, 0.1416607846616000088 ) ) ;
#35886 = CARTESIAN_POINT ( 'NONE',  ( 16.86666666157666583, -3.216308280197300196, -11.40341444503674850 ) ) ;
#35887 = CARTESIAN_POINT ( 'NONE',  ( 21.72233714749290101, 0.000000000000000000, 5.000000000000000000 ) ) ;
#35888 = DIRECTION ( 'NONE',  ( -1.000000000000000000, 0.000000000000000000, 0.000000000000000000 ) ) ;
#35889 = VERTEX_POINT ( 'NONE', #48525 ) ;
#35890 = CARTESIAN_POINT ( 'NONE',  ( 11.12072335273220069, -3.602909566644000083, 6.430603299050000388 ) ) ;
#35891 = CARTESIAN_POINT ( 'NONE',  ( 3.092640132544500098, 3.058252359239899132, 1.762666431298155034 ) ) ;
#35892 = CARTESIAN_POINT ( 'NONE',  ( 15.39165415090800337, 9.395515400280999074, 8.199438574490999443 ) ) ;
#35893 = LINE ( 'NONE', #46736, #9737 ) ;
#35894 = B_SPLINE_CURVE_WITH_KNOTS ( 'NONE', 3,
 ( #58188, #65756, #60520, #12629 ),
 .UNSPECIFIED., .F., .F.,
 ( 4, 4 ),
 ( 0.000000000000000000, 1.000000000000000000 ),
 .UNSPECIFIED. ) ;
#35896 = CARTESIAN_POINT ( 'NONE',  ( 12.43708913302417152, 1.881554942472513314, -13.87303690248482013 ) ) ;
#35895 = CARTESIAN_POINT ( 'NONE',  ( 11.20904666305999875, 5.937823941418000295, 7.147334722859000067 ) ) ;
#35897 = CARTESIAN_POINT ( 'NONE',  ( 11.45764291764649911, 2.867875922590999771, -7.360052904210999891 ) ) ;
#35898 = CARTESIAN_POINT ( 'NONE',  ( 25.26979939644500206, -11.11691833729999779, 3.473712811964000391 ) ) ;
#35899 = CARTESIAN_POINT ( 'NONE',  ( 10.40644474310099810, 4.893483781708200198, -7.933599538786499039 ) ) ;
#35900 = CARTESIAN_POINT ( 'NONE',  ( 18.27397540914052243, 0.09367178904473957846, 12.59965724591066483 ) ) ;
#35901 = CARTESIAN_POINT ( 'NONE',  ( 9.129428851719998406, -5.099284414202999827, 6.151604790022999758 ) ) ;
#35902 = CIRCLE ( 'NONE', #23629, 0.5999999999999999778 ) ;
#35903 = CARTESIAN_POINT ( 'NONE',  ( 24.53429014662800256, -8.855930250654999725, 9.286429702500999639 ) ) ;
#35904 = CARTESIAN_POINT ( 'NONE',  ( 23.83545958851000179, 9.657130125948000909, 9.482575700297999788 ) ) ;
#35905 = VERTEX_POINT ( 'NONE', #21597 ) ;
#35906 = CARTESIAN_POINT ( 'NONE',  ( 8.951355646795001064, -2.821866379289000193, 6.127148604720000336 ) ) ;
#35907 = EDGE_CURVE ( 'NONE', #7406, #5174, #29926, .T. ) ;
#35909 = EDGE_CURVE ( 'NONE', #21396, #47463, #61846, .T. ) ;
#35908 = B_SPLINE_CURVE_WITH_KNOTS ( 'NONE', 3,
 ( #19707, #41027, #62350, #8183 ),
 .UNSPECIFIED., .F., .F.,
 ( 4, 4 ),
 ( 0.000000000000000000, 1.000000000000000000 ),
 .UNSPECIFIED. ) ;
#35910 = CARTESIAN_POINT ( 'NONE',  ( 6.900019030169000089, 12.43894676821000012, -2.828897736577999922 ) ) ;
#35911 = CARTESIAN_POINT ( 'NONE',  ( 5.000030787343001215, -0.2748844998327745759, -2.099962892531005210 ) ) ;
#35912 = VERTEX_POINT ( 'NONE', #11454 ) ;
#35913 = CARTESIAN_POINT ( 'NONE',  ( 0.4033234188635999584, -1.019984463426999888, 3.043156295769000153 ) ) ;
#35914 = CARTESIAN_POINT ( 'NONE',  ( 10.81013259637009938, 2.968328969579000276, 6.937848198857199833 ) ) ;
#35915 = AXIS2_PLACEMENT_3D ( 'NONE', #17564, #66137, #55662 ) ;
#35917 = B_SPLINE_CURVE_WITH_KNOTS ( 'NONE', 3,
 ( #22254, #29856, #13424, #64891, #51162, #43592, #24589, #45911, #34744, #24240, #45578, #66884, #19335, #57766 ),
 .UNSPECIFIED., .F., .F.,
 ( 4, 2, 2, 2, 2, 2, 4 ),
 ( 0.000000000000000000, 0.2494049090184954909, 0.3741073635277432641, 0.4052829771550562343, 0.4364585907823692046, 0.4676342044096822304, 0.4988098180369952006 ),
 .UNSPECIFIED. ) ;
#35916 = CARTESIAN_POINT ( 'NONE',  ( 11.01605778040999972, 5.482856203356999636, -7.846408531951999166 ) ) ;
#35918 = ORIENTED_EDGE ( 'NONE', *, *, #42467, .T. ) ;
#35919 = CARTESIAN_POINT ( 'NONE',  ( 1.550973465874000201, 3.500000000000000000, 0.000000000000000000 ) ) ;
#35920 = CARTESIAN_POINT ( 'NONE',  ( 25.37956555325600405, -8.342521218007666661, 8.311507340610738481 ) ) ;
#35921 = CARTESIAN_POINT ( 'NONE',  ( 11.35502763632549872, 2.839566963815999934, 8.035454525731699604 ) ) ;
#35922 = CARTESIAN_POINT ( 'NONE',  ( 7.000000092426000187, -9.186879080274000131, 5.186879143973999184 ) ) ;
#35923 = CARTESIAN_POINT ( 'NONE',  ( 14.93333333119166717, 9.187454790032710150, 8.213178404203523186 ) ) ;
#35924 = EDGE_LOOP ( 'NONE', ( #32354, #43468, #54693, #26926 ) ) ;
#35925 = CARTESIAN_POINT ( 'NONE',  ( 7.839304865445928527, -5.021524044172331891, 6.546612932266471674 ) ) ;
#35926 = CARTESIAN_POINT ( 'NONE',  ( 8.113864158768999246, 2.425297598239999797, -6.437049665397999831 ) ) ;
#35927 = EDGE_CURVE ( 'NONE', #26293, #51926, #50714, .T. ) ;
#35928 = CARTESIAN_POINT ( 'NONE',  ( 8.128419906718608701, -5.085263205253937713, 6.140446736834060282 ) ) ;
#35929 = CARTESIAN_POINT ( 'NONE',  ( 10.38392546752099932, -5.276153033933000280, 7.588418444866789514 ) ) ;
#35930 = ORIENTED_EDGE ( 'NONE', *, *, #12840, .F. ) ;
#35931 = CARTESIAN_POINT ( 'NONE',  ( 10.31724051754000016, -4.562409174416999669, -4.565398975579999963 ) ) ;
#35932 = CARTESIAN_POINT ( 'NONE',  ( 25.60000000000000142, -11.77655473258999841, 4.190794510628000680 ) ) ;
#35933 = ORIENTED_EDGE ( 'NONE', *, *, #56908, .T. ) ;
#35934 = ADVANCED_FACE ( 'NONE', ( #981 ), #26866, .T. ) ;
#35935 = CARTESIAN_POINT ( 'NONE',  ( 9.904346873515667227, -5.250000000000000888, 7.336375382625536901 ) ) ;
#35936 = ORIENTED_EDGE ( 'NONE', *, *, #51146, .F. ) ;
#35937 = CARTESIAN_POINT ( 'NONE',  ( 9.490308298768001194, -5.536248950452999473, -7.355084988757000453 ) ) ;
#35938 = CARTESIAN_POINT ( 'NONE',  ( 2.373890132542958220, -2.150913519912200922, -2.798833948393631754 ) ) ;
#35939 = CARTESIAN_POINT ( 'NONE',  ( 10.77368717260499942, 3.460071470104900015, -8.381256426168800289 ) ) ;
#35940 = CARTESIAN_POINT ( 'NONE',  ( 11.55435090131019926, -2.880552878538999995, 6.807613609764599616 ) ) ;
#35941 = CARTESIAN_POINT ( 'NONE',  ( 12.20120475779644842, 2.662482513922677096, -12.41227208748767197 ) ) ;
#35942 = CARTESIAN_POINT ( 'NONE',  ( 11.61302897915239818, -3.708003626182200030, 6.397263297997000109 ) ) ;
#35943 = CARTESIAN_POINT ( 'NONE',  ( 9.341490007895000502, 4.148133901461999784, 9.337478696773001019 ) ) ;
#35944 = ORIENTED_EDGE ( 'NONE', *, *, #48613, .T. ) ;
#35945 = CARTESIAN_POINT ( 'NONE',  ( 7.766851002543999627, 2.832432432432000269, 6.822293592207000934 ) ) ;
#35946 = CARTESIAN_POINT ( 'NONE',  ( 11.58457173739308743, -3.062774903199518839, -8.361882233189922076 ) ) ;
#35947 = CARTESIAN_POINT ( 'NONE',  ( 11.09999999999999964, 5.350000000000000533, -7.500000000000000000 ) ) ;
#35948 = ORIENTED_EDGE ( 'NONE', *, *, #29089, .F. ) ;
#35949 = CARTESIAN_POINT ( 'NONE',  ( 12.61719528873172891, -3.096122730228594744, -12.29247817764211348 ) ) ;
#35950 = CARTESIAN_POINT ( 'NONE',  ( 10.20226357027499908, 5.120085139777000194, 7.283900408233900059 ) ) ;
#35951 = CARTESIAN_POINT ( 'NONE',  ( 11.01605564679000082, -5.482859940357000639, -7.846409404949000077 ) ) ;
#35952 = LINE ( 'NONE', #30712, #28817 ) ;
#35953 = CARTESIAN_POINT ( 'NONE',  ( 18.04816728597000264, -3.610133590554000182, -12.03375048192000207 ) ) ;
#35954 = CARTESIAN_POINT ( 'NONE',  ( 7.954299074928001367, 3.414461172233999697, -6.283593702261001113 ) ) ;
#35955 = CARTESIAN_POINT ( 'NONE',  ( 12.64211699103826270, -1.896258653787261217, -13.78307619201600254 ) ) ;
#35956 = CARTESIAN_POINT ( 'NONE',  ( 11.60948876160955479, -4.695527826393099957, -8.223320049540498999 ) ) ;
#35957 = CARTESIAN_POINT ( 'NONE',  ( 10.07503300763299947, -3.118110956362800223, -8.424978748982498544 ) ) ;
#35958 = DIRECTION ( 'NONE',  ( 0.000000000000000000, 1.000000000000000000, 0.000000000000000000 ) ) ;
#35959 = ORIENTED_EDGE ( 'NONE', *, *, #14195, .F. ) ;
#35960 = EDGE_LOOP ( 'NONE', ( #18363, #44617, #49824, #39337, #53397, #29008 ) ) ;
#35961 = CARTESIAN_POINT ( 'NONE',  ( 12.07990818253658105, -0.1906559480948835372, -14.00000681886699461 ) ) ;
#35962 = DIRECTION ( 'NONE',  ( 0.000000000000000000, 0.7198977633594747516, 0.6940801180771756229 ) ) ;
#35963 = CARTESIAN_POINT ( 'NONE',  ( 18.09719409067036011, 2.811143122875886302, 13.60247644588032223 ) ) ;
#35964 = CARTESIAN_POINT ( 'NONE',  ( 9.766125411066999717, 4.735428155407000794, -8.791393655830999521 ) ) ;
#35965 = CARTESIAN_POINT ( 'NONE',  ( 10.64393020684969926, 5.250000000000000000, -7.500000000000000000 ) ) ;
#35966 = CARTESIAN_POINT ( 'NONE',  ( 17.71888513161119505, 3.103492732303466450, 12.29025695670425300 ) ) ;
#35967 = CIRCLE ( 'NONE', #43810, 0.6999999999999992895 ) ;
#35968 = CARTESIAN_POINT ( 'NONE',  ( 17.77423364829699892, 3.297060500158999652, -11.83473586442999981 ) ) ;
#35969 = EDGE_CURVE ( 'NONE', #20236, #16591, #11441, .T. ) ;
#35970 = CARTESIAN_POINT ( 'NONE',  ( 9.910790522921001156, 3.869345236050000025, 5.882548872612999524 ) ) ;
#35971 = CARTESIAN_POINT ( 'NONE',  ( 11.39975833414730033, -3.203462856645999945, -7.174999999999999822 ) ) ;
#35972 = ORIENTED_EDGE ( 'NONE', *, *, #6064, .T. ) ;
#35973 = CARTESIAN_POINT ( 'NONE',  ( 12.24870215512123650, -2.784965704346237469, 12.38061966815949511 ) ) ;
#35974 = CARTESIAN_POINT ( 'NONE',  ( 9.475696787962998968, -3.851113559088000127, -6.645868410478299459 ) ) ;
#35975 = CARTESIAN_POINT ( 'NONE',  ( 9.409415556003999370, 2.113395950889999764, 7.914199712930999553 ) ) ;
#35976 = CARTESIAN_POINT ( 'NONE',  ( 11.39324174884020024, -4.032306468273969990, 6.325557131097000685 ) ) ;
#35977 = CARTESIAN_POINT ( 'NONE',  ( 9.269210841233000764, 3.098073081301000009, -8.567513114264999174 ) ) ;
#35978 = DIRECTION ( 'NONE',  ( -1.000000000000000000, 0.000000000000000000, 0.000000000000000000 ) ) ;
#35979 = CARTESIAN_POINT ( 'NONE',  ( 25.08547572896300082, 8.543211284141001727, 8.155294727984999881 ) ) ;
#35980 = CARTESIAN_POINT ( 'NONE',  ( 12.40062372901866894, 0.4766234715920624199, 12.68796191786312910 ) ) ;
#35981 = CARTESIAN_POINT ( 'NONE',  ( 5.536227981748580440, -12.19240621326411578, -3.776122996998608983 ) ) ;
#35982 = CARTESIAN_POINT ( 'NONE',  ( 10.62197831623999988, 5.779783227492000464, 7.256572995198999898 ) ) ;
#35983 = CARTESIAN_POINT ( 'NONE',  ( 10.97807333593999957, -5.235090452703000885, -6.783100406990000053 ) ) ;
#35984 = ORIENTED_EDGE ( 'NONE', *, *, #68496, .T. ) ;
#35985 = CARTESIAN_POINT ( 'NONE',  ( 8.889129719593999113, 5.687930027805999877, -7.109876198051000351 ) ) ;
#35986 = B_SPLINE_CURVE_WITH_KNOTS ( 'NONE', 3,
 ( #44744, #18514, #6976, #49277 ),
 .UNSPECIFIED., .F., .F.,
 ( 4, 4 ),
 ( 0.000000000000000000, 1.000000000000000000 ),
 .UNSPECIFIED. ) ;
#35987 = CARTESIAN_POINT ( 'NONE',  ( 0.000000000000000000, 2.319305672483364056, 1.781768641235244921 ) ) ;
#35988 = ADVANCED_FACE ( 'NONE', ( #42936 ), #16358, .T. ) ;
#35989 = EDGE_CURVE ( 'NONE', #48764, #47657, #15664, .T. ) ;
#35990 = CARTESIAN_POINT ( 'NONE',  ( 17.96975113184317152, 2.032288328865630156, 13.76155421333986695 ) ) ;
#35991 = CARTESIAN_POINT ( 'NONE',  ( 10.64393020684969926, -2.750000000000000000, -7.500000000000000000 ) ) ;
#35992 = CARTESIAN_POINT ( 'NONE',  ( 12.10000000000000142, -2.912667852269568147, 8.017651347927678529 ) ) ;
#35993 = CARTESIAN_POINT ( 'NONE',  ( 10.45257053952200010, -4.394359323863099576, -6.577269499510100204 ) ) ;
#35994 = VERTEX_POINT ( 'NONE', #18786 ) ;
#35995 = VECTOR ( 'NONE', #32720, 1000.000000000000114 ) ;
#35996 = EDGE_CURVE ( 'NONE', #26398, #5569, #39768, .T. ) ;
#35997 = CARTESIAN_POINT ( 'NONE',  ( 2.058838311996999959, 3.411444769430000079, 1.578107062294999974 ) ) ;
#35998 = CARTESIAN_POINT ( 'NONE',  ( 11.43328525708585452, -3.653536053513362525, 11.13242455109463869 ) ) ;
#36001 = DIRECTION ( 'NONE',  ( 1.000000000000000000, 0.000000000000000000, 0.000000000000000000 ) ) ;
#36000 = CARTESIAN_POINT ( 'NONE',  ( 9.518314158773000244, 4.845406482350000488, -6.387189183984999907 ) ) ;
#35999 = PRODUCT_DEFINITION_CONTEXT ( 'detailed design', #56566, 'design' ) ;
#36002 = LINE ( 'NONE', #14344, #61469 ) ;
#36003 = CARTESIAN_POINT ( 'NONE',  ( 13.99999999379500082, -8.815218614167999789, -7.616697584347000394 ) ) ;
#36004 = CARTESIAN_POINT ( 'NONE',  ( 17.96200919170520649, -2.025537500457071705, -13.76266550596354321 ) ) ;
#36005 = CARTESIAN_POINT ( 'NONE',  ( 10.55518582084299872, 3.433275964779900047, 8.155074391384399490 ) ) ;
#36006 = DIRECTION ( 'NONE',  ( 0.000000000000000000, 0.000000000000000000, -1.000000000000000000 ) ) ;
#36007 = CARTESIAN_POINT ( 'NONE',  ( 9.041941940379999210, -2.707994276285999646, 5.994456121676999594 ) ) ;
#36008 = EDGE_LOOP ( 'NONE', ( #59147, #20071, #54448, #8681 ) ) ;
#36009 = CARTESIAN_POINT ( 'NONE',  ( 9.176357780411999343, 2.935741164366000522, 6.259844213126999790 ) ) ;
#36011 = DIRECTION ( 'NONE',  ( 0.000000000000000000, 0.000000000000000000, -1.000000000000000000 ) ) ;
#36010 = CARTESIAN_POINT ( 'NONE',  ( 6.578907741853000424, -1.461948210420000116, 0.3790019357670000311 ) ) ;
#36012 = CARTESIAN_POINT ( 'NONE',  ( 7.645335379506589035, -5.356736300262827655, 6.411841797474306048 ) ) ;
#36013 = DIRECTION ( 'NONE',  ( -1.000000000000000000, 0.000000000000000000, 0.000000000000000000 ) ) ;
#36014 = CARTESIAN_POINT ( 'NONE',  ( 1.123382408447999747, 1.635708097465000010, -3.009863393104000195 ) ) ;
#36015 = VERTEX_POINT ( 'NONE', #60736 ) ;
#36016 = FACE_OUTER_BOUND ( 'NONE', #24635, .T. ) ;
#36017 = CARTESIAN_POINT ( 'NONE',  ( 11.07980110216399972, -4.739241740354600552, 7.951464549725199227 ) ) ;
#36018 = EDGE_CURVE ( 'NONE', #28156, #7065, #22344, .T. ) ;
#36019 = CARTESIAN_POINT ( 'NONE',  ( 10.46432998405999903, 2.042755206296999582, 7.723699495214000343 ) ) ;
#36020 = CARTESIAN_POINT ( 'NONE',  ( 10.27967883605999866, 5.739712809045000697, 7.774963411801000923 ) ) ;
#36021 = CARTESIAN_POINT ( 'NONE',  ( 10.98995257254739855, 2.904643075091000171, 7.181435527216799564 ) ) ;
#36022 = CARTESIAN_POINT ( 'NONE',  ( 24.12728201901689573, -3.330896228204782705, 12.51463748290429479 ) ) ;
#36023 = CARTESIAN_POINT ( 'NONE',  ( 17.89107826690647940, 3.595094513005142822, -11.99795484439389170 ) ) ;
#36024 = DIRECTION ( 'NONE',  ( 0.000000000000000000, 0.000000000000000000, 1.000000000000000000 ) ) ;
#36025 = CARTESIAN_POINT ( 'NONE',  ( 25.41677544510499942, -2.809827979128999953, -11.31866138444999770 ) ) ;
#36026 = CARTESIAN_POINT ( 'NONE',  ( 17.85668400807928080, -1.853912555516301630, 13.87670837816644109 ) ) ;
#36027 = CARTESIAN_POINT ( 'NONE',  ( 17.55505043854144631, 0.7192913403693005359, 12.57945229203838267 ) ) ;
#36028 = ORIENTED_EDGE ( 'NONE', *, *, #56907, .T. ) ;
#36029 = CARTESIAN_POINT ( 'NONE',  ( 7.307500000000000107, 0.2999999999999999889, -3.149999999999999911 ) ) ;
#36030 = CARTESIAN_POINT ( 'NONE',  ( 23.59999176271200128, 13.22318677037999812, 4.267778497637999102 ) ) ;
#36031 = VERTEX_POINT ( 'NONE', #34533 ) ;
#36032 = CARTESIAN_POINT ( 'NONE',  ( 9.489763540183334456, 4.327184855449099921, 6.282534154164604701 ) ) ;
#36033 = CARTESIAN_POINT ( 'NONE',  ( 11.56441235500451015, 3.361299021099800388, 8.085115074060599483 ) ) ;
#36034 = CARTESIAN_POINT ( 'NONE',  ( 10.93227693248999977, 2.539877577705000000, 6.453611809651000009 ) ) ;
#36035 = CARTESIAN_POINT ( 'NONE',  ( 9.870875237110999123, 2.904361819252000210, -8.563871667095998674 ) ) ;
#36036 = CARTESIAN_POINT ( 'NONE',  ( 9.708153928322625248, -4.380187932396833794, -8.288028809740389136 ) ) ;
#36037 = CARTESIAN_POINT ( 'NONE',  ( 9.625489929093001606, -3.134630999349000025, 8.626959345509000343 ) ) ;
#36038 = CARTESIAN_POINT ( 'NONE',  ( 18.27776587948808285, -0.05827135643914812396, -12.59987075990256855 ) ) ;
#36039 = CARTESIAN_POINT ( 'NONE',  ( 12.29679984372382506, 2.863892094152995060, -12.35932590995903446 ) ) ;
#36040 = CARTESIAN_POINT ( 'NONE',  ( 11.24441369783139777, -4.043700988887960257, -8.365094684940499903 ) ) ;
#36041 = CARTESIAN_POINT ( 'NONE',  ( 6.964951367667778115, 0.8867442030251825313, 1.153938778527312969 ) ) ;
#36042 = VERTEX_POINT ( 'NONE', #17399 ) ;
#36043 =( REPRESENTATION_RELATIONSHIP ('NONE','NONE', #10823, #27655 ) REPRESENTATION_RELATIONSHIP_WITH_TRANSFORMATION ( #42465 )SHAPE_REPRESENTATION_RELATIONSHIP( ) );
#36044 = CARTESIAN_POINT ( 'NONE',  ( 11.01655351471000088, -6.705640160583000053, -5.522669566710000311 ) ) ;
#36045 =( LENGTH_UNIT ( ) NAMED_UNIT ( * ) SI_UNIT ( .MILLI., .METRE. ) );
#36046 = CARTESIAN_POINT ( 'NONE',  ( 9.769471092180999960, 5.100000000000000533, -6.152188490330000370 ) ) ;
#36047 = CARTESIAN_POINT ( 'NONE',  ( 25.10986374740704008, 11.36610807887094943, -3.264518009230023221 ) ) ;
#36048 = CARTESIAN_POINT ( 'NONE',  ( 8.960616452296999768, 2.899999999999999911, 6.279946362737000243 ) ) ;
#36049 = CARTESIAN_POINT ( 'NONE',  ( 17.82422846108291736, 1.812210939693178924, 12.46899807711483987 ) ) ;
#36050 = B_SPLINE_CURVE_WITH_KNOTS ( 'NONE', 3,
 ( #57979, #47491, #10076, #31413, #47146, #52729, #4824, #32107, #10418, #20227 ),
 .UNSPECIFIED., .F., .F.,
 ( 4, 2, 2, 2, 4 ),
 ( 0.000000000000000000, 0.2499999999999997780, 0.4999999999999995559, 0.7499999999999997780, 1.000000000000000000 ),
 .UNSPECIFIED. ) ;
#36051 = EDGE_CURVE ( 'NONE', #20133, #60155, #60396, .T. ) ;
#36052 = CARTESIAN_POINT ( 'NONE',  ( 12.19349437040516904, 2.125667349631279901, 13.83768917864515480 ) ) ;
#36053 = EDGE_CURVE ( 'NONE', #11254, #41424, #40674, .T. ) ;
#36054 = CARTESIAN_POINT ( 'NONE',  ( 10.93785547196599950, 2.862144528033999880, 6.360512911308666695 ) ) ;
#36055 = VERTEX_POINT ( 'NONE', #29283 ) ;
#36056 = CARTESIAN_POINT ( 'NONE',  ( 12.21982330446825316, -0.2196444115886839188, -12.69744877134248995 ) ) ;
#36057 = LINE ( 'NONE', #9475, #44868 ) ;
#36058 = EDGE_LOOP ( 'NONE', ( #68966, #31639, #20098, #7814 ) ) ;
#36059 = CARTESIAN_POINT ( 'NONE',  ( 12.33239129661528821, -1.934538128658857881, 12.45060726317137423 ) ) ;
#36060 = FACE_BOUND ( 'NONE', #9950, .T. ) ;
#36061 = CARTESIAN_POINT ( 'NONE',  ( 10.59393020684899867, -2.750000000000000000, -7.500000000000000000 ) ) ;
#36062 = CARTESIAN_POINT ( 'NONE',  ( 11.20287750876920008, -4.469200303112399908, 6.771886227364699806 ) ) ;
#36063 = AXIS2_PLACEMENT_3D ( 'NONE', #17369, #34505, #60366 ) ;
#36064 = CARTESIAN_POINT ( 'NONE',  ( 16.03328789001813703, -8.397841793663575416, -8.170414199808828215 ) ) ;
#36065 = B_SPLINE_CURVE_WITH_KNOTS ( 'NONE', 3,
 ( #34298, #55621, #14004, #7720 ),
 .UNSPECIFIED., .F., .F.,
 ( 4, 4 ),
 ( 0.000000000000000000, 1.000000000000000000 ),
 .UNSPECIFIED. ) ;
#36066 = CARTESIAN_POINT ( 'NONE',  ( 0.4251162859547999995, 1.034012873651999787, -3.554373790709000058 ) ) ;
#36067 = CARTESIAN_POINT ( 'NONE',  ( 7.924878289113897800, 5.349357204871084903, 7.500005630225526687 ) ) ;
#36068 = CARTESIAN_POINT ( 'NONE',  ( 12.21438802940094348, 2.898246740288908718, 12.26216014320957370 ) ) ;
#36069 = CARTESIAN_POINT ( 'NONE',  ( 11.09999999999999964, 2.700000000742000417, -5.148510365175999581 ) ) ;
#36070 = CARTESIAN_POINT ( 'NONE',  ( 10.57564694612699974, 3.068007311611700150, -7.871941502982999772 ) ) ;
#36071 = DIRECTION ( 'NONE',  ( 1.000000000000000000, 0.000000000000000000, 0.000000000000000000 ) ) ;
#36072 = EDGE_CURVE ( 'NONE', #19330, #31999, #24023, .T. ) ;
#36073 = CARTESIAN_POINT ( 'NONE',  ( 11.20537028040999949, 2.688545137295000220, -8.273930556758998023 ) ) ;
#36074 = CARTESIAN_POINT ( 'NONE',  ( 8.794772138681999252, 3.523984281974800403, -6.312652778810999621 ) ) ;
#36076 = DIRECTION ( 'NONE',  ( 0.000000000000000000, -1.000000000000000000, 0.000000000000000000 ) ) ;
#36075 = CARTESIAN_POINT ( 'NONE',  ( 10.53521345716899837, -3.075109701058799772, -8.340879262988799780 ) ) ;
#36077 = CARTESIAN_POINT ( 'NONE',  ( 10.08712270112418885, 5.286531262339692283, -7.026829543710713111 ) ) ;
#36078 = ORIENTED_EDGE ( 'NONE', *, *, #52554, .F. ) ;
#36079 = ADVANCED_FACE ( 'NONE', ( #66666 ), #40116, .F. ) ;
#36080 = CARTESIAN_POINT ( 'NONE',  ( 12.21236377911861659, -0.1994069032339068626, 12.69791261745780986 ) ) ;
#36081 = CARTESIAN_POINT ( 'NONE',  ( 10.98768472638000127, 7.408460564924999936, -6.159405844198999169 ) ) ;
#36082 = CARTESIAN_POINT ( 'NONE',  ( 9.634027193201999850, -3.042970193091000031, 8.588108172435999776 ) ) ;
#36083 = CARTESIAN_POINT ( 'NONE',  ( 9.148430433047000321, 3.145249924879699677, 8.027488966151301142 ) ) ;
#36084 = CARTESIAN_POINT ( 'NONE',  ( 9.226900131858625898, 3.814237572305042345, -8.354999759870066711 ) ) ;
#36085 = FACE_OUTER_BOUND ( 'NONE', #65869, .T. ) ;
#36086 = CARTESIAN_POINT ( 'NONE',  ( 12.57359775157570247, -3.080655040460396954, 13.53300991339125225 ) ) ;
#36087 = CARTESIAN_POINT ( 'NONE',  ( 12.20137260070325347, 2.663020830165313324, 13.63749600555738439 ) ) ;
#36088 = FACE_OUTER_BOUND ( 'NONE', #38899, .T. ) ;
#36089 = ORIENTED_EDGE ( 'NONE', *, *, #27624, .T. ) ;
#36090 = CIRCLE ( 'NONE', #19371, 11.50000000000000533 ) ;
#36091 = CARTESIAN_POINT ( 'NONE',  ( 4.421692514211000180, -0.3829406755631999393, -1.067830647061000171 ) ) ;
#36092 = CARTESIAN_POINT ( 'NONE',  ( 10.06122949779699915, -3.290320231472799950, -8.564302809495998758 ) ) ;
#36093 = CARTESIAN_POINT ( 'NONE',  ( 10.98768472639999949, -0.3876847264043000174, 4.945212061661000469 ) ) ;
#36094 = CARTESIAN_POINT ( 'NONE',  ( 11.73589666366019912, -4.039600775206940497, 6.608753462694600067 ) ) ;
#36095 = EDGE_CURVE ( 'NONE', #63766, #11391, #3740, .T. ) ;
#36096 = CARTESIAN_POINT ( 'NONE',  ( 17.74533816909189454, 1.785653880132706872, -12.47283005504979592 ) ) ;
#36097 = CARTESIAN_POINT ( 'NONE',  ( 8.819279415752005136, -3.128895434138999843, -6.198312589903004266 ) ) ;
#36098 = CARTESIAN_POINT ( 'NONE',  ( 18.05156413927919345, 2.879751443193474980, 12.35493952381846050 ) ) ;
#36099 = DIRECTION ( 'NONE',  ( 0.000000000000000000, 0.1807154286440004198, 0.9835354258236025382 ) ) ;
#36100 = CARTESIAN_POINT ( 'NONE',  ( 10.96500214151999941, -2.847408127283999946, -5.071952786765999477 ) ) ;
#36101 = CARTESIAN_POINT ( 'NONE',  ( 24.56666037493200250, 12.04830180860999889, 3.140564670074999842 ) ) ;
#36102 = CARTESIAN_POINT ( 'NONE',  ( 9.642108463020875320, -3.293853022145220688, 8.705313308395860261 ) ) ;
#36103 = CARTESIAN_POINT ( 'NONE',  ( 12.71024384884961478, 0.7243378955762067584, -13.98124959093732400 ) ) ;
#36104 = CARTESIAN_POINT ( 'NONE',  ( 13.75961700471900073, -8.905065757320999253, -7.452879173751000508 ) ) ;
#36105 = CARTESIAN_POINT ( 'NONE',  ( 23.60000000000000142, -2.258942858049999725, -12.29419282279000036 ) ) ;
#36106 = CARTESIAN_POINT ( 'NONE',  ( 18.18004831022902934, 2.496998393545561967, 12.45226267664535413 ) ) ;
#36107 = CARTESIAN_POINT ( 'NONE',  ( 9.053070280414001303, 2.391443348526999912, -6.856688371964000162 ) ) ;
#36109 = CIRCLE ( 'NONE', #36158, 0.9499999999999999556 ) ;
#36108 = CARTESIAN_POINT ( 'NONE',  ( 11.09999999999999964, -7.940796613052000019, 6.945951997396999644 ) ) ;
#36110 = ORIENTED_EDGE ( 'NONE', *, *, #21140, .F. ) ;
#36111 = FACE_OUTER_BOUND ( 'NONE', #30303, .T. ) ;
#36112 = CARTESIAN_POINT ( 'NONE',  ( 18.26121249471881569, 2.684743402744599106, -13.74018592865772881 ) ) ;
#36113 = EDGE_LOOP ( 'NONE', ( #67758, #23697, #69189, #42904, #62186, #60165, #63891, #31505 ) ) ;
#36114 = CARTESIAN_POINT ( 'NONE',  ( 8.653803059789224150, 2.648172424375619727, 7.852957271308079079 ) ) ;
#36115 = CARTESIAN_POINT ( 'NONE',  ( 11.46989666366029859, 3.941571897678119996, 6.185029684353999357 ) ) ;
#36117 = CARTESIAN_POINT ( 'NONE',  ( 4.149992563292000725, -2.000000000000000000, 0.000000000000000000 ) ) ;
#36116 = AXIS2_PLACEMENT_3D ( 'NONE', #48253, #21676, #16095 ) ;
#36118 = LINE ( 'NONE', #14799, #34261 ) ;
#36119 = CARTESIAN_POINT ( 'NONE',  ( 10.98656920625009903, -3.967932847735990531, -6.608450613814399688 ) ) ;
#36120 = CARTESIAN_POINT ( 'NONE',  ( 11.60000000000000142, -3.927017550833200588, -6.447388989144585025 ) ) ;
#36121 = CARTESIAN_POINT ( 'NONE',  ( 11.05853316602999925, -8.013872486471999679, 6.925173420900999410 ) ) ;
#36122 = ORIENTED_EDGE ( 'NONE', *, *, #2406, .F. ) ;
#36123 = CARTESIAN_POINT ( 'NONE',  ( 13.55458079702099994, 9.509022223680998920, 7.924557572090001223 ) ) ;
#36124 = CARTESIAN_POINT ( 'NONE',  ( 10.10682028041000002, 4.294368353031000396, -8.968663198664000191 ) ) ;
#36125 = EDGE_LOOP ( 'NONE', ( #18222, #26437, #44815, #3378 ) ) ;
#36126 = B_SPLINE_CURVE_WITH_KNOTS ( 'NONE', 3,
 ( #67671, #20137, #46370, #51268, #24699 ),
 .UNSPECIFIED., .F., .F.,
 ( 4, 1, 4 ),
 ( 0.000000000000000000, 0.2283572645236016108, 1.000000000000000000 ),
 .UNSPECIFIED. ) ;
#36127 = CARTESIAN_POINT ( 'NONE',  ( 11.10062015617000064, 3.093053541899000169, -6.153678467293999255 ) ) ;
#36128 = DIRECTION ( 'NONE',  ( 0.000000000000000000, 0.000000000000000000, 1.000000000000000000 ) ) ;
#36129 = ORIENTED_EDGE ( 'NONE', *, *, #40789, .T. ) ;
#36130 = CARTESIAN_POINT ( 'NONE',  ( 9.022734463322999332, 4.133249246727800141, 6.227746477418000026 ) ) ;
#36131 = CARTESIAN_POINT ( 'NONE',  ( 17.75782926003070017, -1.908786995103509021, -12.56982197457662664 ) ) ;
#36132 = CARTESIAN_POINT ( 'NONE',  ( 16.39999999485600313, 3.595156957901000094, 11.99794989424000136 ) ) ;
#36133 = EDGE_CURVE ( 'NONE', #35662, #37068, #5617, .T. ) ;
#36134 = EDGE_CURVE ( 'NONE', #44042, #10297, #28172, .T. ) ;
#36135 = CARTESIAN_POINT ( 'NONE',  ( 24.54688887196200042, -12.52317552374000087, -3.000792222368999784 ) ) ;
#36136 = EDGE_CURVE ( 'NONE', #39016, #62424, #42294, .T. ) ;
#36137 = EDGE_CURVE ( 'NONE', #42702, #40516, #69019, .T. ) ;
#36138 = CARTESIAN_POINT ( 'NONE',  ( 8.642077642326000841, 2.899999999999999911, 6.463854830420999953 ) ) ;
#36139 = ORIENTED_EDGE ( 'NONE', *, *, #13803, .T. ) ;
#36140 = CARTESIAN_POINT ( 'NONE',  ( 7.000000000000000000, 0.000000000000000000, 0.000000000000000000 ) ) ;
#36141 = DIRECTION ( 'NONE',  ( 1.000000000000000000, 0.000000000000000000, 0.000000000000000000 ) ) ;
#36142 = CARTESIAN_POINT ( 'NONE',  ( 11.05490012380000131, -5.246473031683000166, -5.052786172115000696 ) ) ;
#36143 = CARTESIAN_POINT ( 'NONE',  ( 8.837278925393343698, 4.883321897350202612, 8.012901425336814043 ) ) ;
#36144 = VECTOR ( 'NONE', #2516, 1000.000000000000000 ) ;
#36145 = CARTESIAN_POINT ( 'NONE',  ( 18.27977752388257571, -0.02332822437944303412, 13.99998565365491210 ) ) ;
#36146 = CARTESIAN_POINT ( 'NONE',  ( 0.5000220334827000235, 2.806761118207999672, -2.090954811877999919 ) ) ;
#36147 = CARTESIAN_POINT ( 'NONE',  ( 10.98277446826000059, -2.518728855032000169, -8.314788219120000434 ) ) ;
#36148 = EDGE_LOOP ( 'NONE', ( #8433, #67069, #31047, #18476 ) ) ;
#36149 = ORIENTED_EDGE ( 'NONE', *, *, #2489, .F. ) ;
#36150 = CARTESIAN_POINT ( 'NONE',  ( 9.368660841232999914, 2.702406276695999754, -6.981052078638000147 ) ) ;
#36151 = CARTESIAN_POINT ( 'NONE',  ( 10.06489140842196406, 5.349900232312646331, -7.500006335289779003 ) ) ;
#36152 = CARTESIAN_POINT ( 'NONE',  ( 12.25852091198461302, -2.803392358766023662, 13.60441894874461610 ) ) ;
#36153 = CARTESIAN_POINT ( 'NONE',  ( 24.14647126608543459, 3.326442287260038988, 12.48027977927276311 ) ) ;
#36154 = CARTESIAN_POINT ( 'NONE',  ( 7.815856925312669290, 3.425834468749924699, 6.252095740542113589 ) ) ;
#36155 = CARTESIAN_POINT ( 'NONE',  ( 10.26990035061499817, 4.231093494672100164, -8.335645555860798694 ) ) ;
#36157 = DIRECTION ( 'NONE',  ( 0.000000000000000000, 1.000000000000000000, 0.000000000000000000 ) ) ;
#36156 = CARTESIAN_POINT ( 'NONE',  ( 9.599784697134998268, -3.380386586585000241, 8.459069166353199165 ) ) ;
#36158 = AXIS2_PLACEMENT_3D ( 'NONE', #50893, #61383, #25004 ) ;
#36159 = CARTESIAN_POINT ( 'NONE',  ( 8.046990059540997109, -3.146252403201002856, 6.173090499042001689 ) ) ;
#36160 = ORIENTED_EDGE ( 'NONE', *, *, #14993, .F. ) ;
#36161 = CARTESIAN_POINT ( 'NONE',  ( 11.04783424078000031, -2.764605797469000148, 5.041477660832000218 ) ) ;
#36162 = AXIS2_PLACEMENT_3D ( 'NONE', #21680, #10509, #68889 ) ;
#36163 = CARTESIAN_POINT ( 'NONE',  ( 10.31726253785999958, -3.438690054218000114, -4.565404970506000026 ) ) ;
#36164 = DIRECTION ( 'NONE',  ( 1.000000000000000000, 0.000000000000000000, 0.000000000000000000 ) ) ;
#36165 = CARTESIAN_POINT ( 'NONE',  ( 12.09999999999999964, -4.883784007588900522, 7.174999999999999822 ) ) ;
#36166 = CARTESIAN_POINT ( 'NONE',  ( 8.200000998245998929, -12.50000000000000000, 0.000000000000000000 ) ) ;
#36167 = CARTESIAN_POINT ( 'NONE',  ( 11.01870309098000078, -5.269007982505999443, -4.994855899974000479 ) ) ;
#36168 = CARTESIAN_POINT ( 'NONE',  ( 10.18367854428788633, 2.796579479970431326, 8.204151721975319944 ) ) ;
#36169 = B_SPLINE_CURVE_WITH_KNOTS ( 'NONE', 3,
 ( #36899, #865, #31651, #22181, #517, #69049, #48070, #43521, #21157, #21491, #42484, #63794, #42825, #15903 ),
 .UNSPECIFIED., .F., .F.,
 ( 4, 2, 2, 2, 2, 2, 4 ),
 ( 0.05661757269142905086, 0.2924631795185714256, 0.4103859829321429564, 0.5283087863457146538, 0.6462315897592861846, 0.7641543931728578265, 1.000000000000000000 ),
 .UNSPECIFIED. ) ;
#36170 = CARTESIAN_POINT ( 'NONE',  ( 10.90000000000000036, 0.000000000000000000, 0.000000000000000000 ) ) ;
#36171 = CARTESIAN_POINT ( 'NONE',  ( 7.994077351562546951, 3.211953255579858446, -6.298056302553895591 ) ) ;
#36172 = CARTESIAN_POINT ( 'NONE',  ( 11.03976354018315753, -3.672815144550900524, 6.282534154164603812 ) ) ;
#36173 = EDGE_CURVE ( 'NONE', #227, #14714, #22983, .T. ) ;
#36174 = CARTESIAN_POINT ( 'NONE',  ( 0.1492968197647682738, 0.8235178986539704038, -3.067640566204680397 ) ) ;
#36175 = CARTESIAN_POINT ( 'NONE',  ( 25.49995777816882025, -10.64590202376374251, -3.788441483803001830 ) ) ;
#36176 = CARTESIAN_POINT ( 'NONE',  ( 3.539384965075000000, -3.233467766375999641, 0.4074197872470000092 ) ) ;
#36177 = ORIENTED_EDGE ( 'NONE', *, *, #27327, .F. ) ;
#36178 = CARTESIAN_POINT ( 'NONE',  ( 12.18201988759300214, 0.05063260980701855818, -12.69986973508909323 ) ) ;
#36179 = CARTESIAN_POINT ( 'NONE',  ( 12.22117151664400225, -2.723004124966011741, -12.39680780188599485 ) ) ;
#36180 = ADVANCED_FACE ( 'NONE', ( #40440 ), #25014, .T. ) ;
#36181 = CARTESIAN_POINT ( 'NONE',  ( 16.10005255078199937, 3.632778330393000132, 11.06917548872000090 ) ) ;
#36182 = CARTESIAN_POINT ( 'NONE',  ( 10.88314899746000108, -5.167567567567999731, 6.822293592207000934 ) ) ;
#36183 = CARTESIAN_POINT ( 'NONE',  ( 10.32340023520120020, 2.820488420191645584, -8.179866073662113379 ) ) ;
#36184 = ORIENTED_EDGE ( 'NONE', *, *, #11042, .F. ) ;
#36185 = CARTESIAN_POINT ( 'NONE',  ( 9.679055905794999859, -2.899999999999999911, 6.571291218949999902 ) ) ;
#36186 = CARTESIAN_POINT ( 'NONE',  ( 17.83819980912012326, 0.5572757172660935954, 12.68354006032474679 ) ) ;
#36187 = CARTESIAN_POINT ( 'NONE',  ( 13.69055856039300068, -11.42191202915999781, -2.091365271848000251 ) ) ;
#36188 = CARTESIAN_POINT ( 'NONE',  ( 10.41964694612699915, 2.813019656517000477, 7.026297514493899499 ) ) ;
#36189 = CARTESIAN_POINT ( 'NONE',  ( 11.35545123989519922, 4.475221369382300196, -8.417769225118700405 ) ) ;
#36190 = VERTEX_POINT ( 'NONE', #35887 ) ;
#36191 = CARTESIAN_POINT ( 'NONE',  ( 11.18483536755999808, -2.599651619047000040, 7.740676724427999922 ) ) ;
#36192 = ORIENTED_EDGE ( 'NONE', *, *, #46755, .T. ) ;
#36193 = CARTESIAN_POINT ( 'NONE',  ( 7.664150527885400521, -2.651202557357406508, 7.676969588268241829 ) ) ;
#36194 = CARTESIAN_POINT ( 'NONE',  ( 7.673644353206999114, -4.696237245142999228, 5.830277424166999900 ) ) ;
#36195 = CARTESIAN_POINT ( 'NONE',  ( 15.83887202961200025, 8.726161303169000405, 7.661206663860999910 ) ) ;
#36196 = ORIENTED_EDGE ( 'NONE', *, *, #23704, .F. ) ;
#36197 = CARTESIAN_POINT ( 'NONE',  ( 23.58296120034879451, 10.22496133173016730, 9.539120963660936425 ) ) ;
#36198 = B_SPLINE_CURVE_WITH_KNOTS ( 'NONE', 3,
 ( #4942, #52845, #26280, #47606, #68563, #46575 ),
 .UNSPECIFIED., .F., .F.,
 ( 4, 2, 4 ),
 ( 0.000000000000000000, 0.1967045975185045814, 0.3934091950370091628 ),
 .UNSPECIFIED. ) ;
#36199 = CARTESIAN_POINT ( 'NONE',  ( 7.563304092220104025, 3.763842522021197290, 8.850238422624055801 ) ) ;
#36200 = CARTESIAN_POINT ( 'NONE',  ( 8.219220280408000789, 5.354408404900999230, -6.419792067946000103 ) ) ;
#36201 = LINE ( 'NONE', #52280, #18635 ) ;
#36202 = DIRECTION ( 'NONE',  ( -1.000000000000000000, 0.000000000000000000, 0.000000000000000000 ) ) ;
#36203 = ORIENTED_EDGE ( 'NONE', *, *, #6255, .F. ) ;
#36204 = CARTESIAN_POINT ( 'NONE',  ( 10.46432358320999967, -2.042767395367000027, 7.723698102088000006 ) ) ;
#36205 = CARTESIAN_POINT ( 'NONE',  ( 12.19790361191645722, -2.648659039907943047, -13.64075350855048185 ) ) ;
#36206 = CARTESIAN_POINT ( 'NONE',  ( 5.521693173017002465, -0.7554284705563544255, 1.310679582531384169 ) ) ;
#36207 = EDGE_LOOP ( 'NONE', ( #48421, #35507, #40767, #48988 ) ) ;
#36208 = CARTESIAN_POINT ( 'NONE',  ( 10.89218817467000200, -2.661900611977999986, -8.236035141896001832 ) ) ;
#36209 = AXIS2_PLACEMENT_3D ( 'NONE', #17289, #17991, #55390 ) ;
#36210 = CARTESIAN_POINT ( 'NONE',  ( 10.98953890776364872, -6.637400546507714161, -5.389624950907599299 ) ) ;
#36211 = VERTEX_POINT ( 'NONE', #62450 ) ;
#36212 = CARTESIAN_POINT ( 'NONE',  ( 23.59112020737914506, -10.18869760917455736, 9.572450890279778690 ) ) ;
#36213 = CARTESIAN_POINT ( 'NONE',  ( 23.97708749418018570, 12.74918579704523935, -3.497816719186660261 ) ) ;
#36214 = CARTESIAN_POINT ( 'NONE',  ( 5.376962934516001269, 1.051792491445999955, 1.148731044744000007 ) ) ;
#36215 = AXIS2_PLACEMENT_3D ( 'NONE', #33106, #65248, #249 ) ;
#36216 = CARTESIAN_POINT ( 'NONE',  ( 5.355026506350999860, 1.500000000000000000, 0.000000000000000000 ) ) ;
#36217 = FACE_OUTER_BOUND ( 'NONE', #44493, .T. ) ;
#36218 = DIRECTION ( 'NONE',  ( 0.000000000000000000, 1.000000000000000000, 0.000000000000000000 ) ) ;
#36219 = CARTESIAN_POINT ( 'NONE',  ( 8.716851002545999094, -2.832432432432000269, 6.822293592207000934 ) ) ;
#36220 = EDGE_CURVE ( 'NONE', #38087, #57647, #41818, .T. ) ;
#36222 = ADVANCED_FACE ( 'NONE', ( #19464 ), #68373, .T. ) ;
#36221 = CARTESIAN_POINT ( 'NONE',  ( 10.90638082498000117, -5.227498618488000126, 6.784459667733999666 ) ) ;
#36223 = ORIENTED_EDGE ( 'NONE', *, *, #60659, .T. ) ;
#36224 = CARTESIAN_POINT ( 'NONE',  ( 10.94501463001509833, -3.527519786474400121, -6.743262887067199784 ) ) ;
#36225 = ORIENTED_EDGE ( 'NONE', *, *, #52700, .T. ) ;
#36226 = CARTESIAN_POINT ( 'NONE',  ( 10.07102359808000003, 4.042170458878000083, 8.920189456109998360 ) ) ;
#36227 = CARTESIAN_POINT ( 'NONE',  ( 11.04782425406999913, -5.235403588978999601, 5.041461677707999911 ) ) ;
#36228 = CARTESIAN_POINT ( 'NONE',  ( 12.30652006878821325, 2.122495540605185749, -13.74632343115108846 ) ) ;
#36229 = CARTESIAN_POINT ( 'NONE',  ( 2.761417138354999690, -1.986395360111999908, -2.934648526694999759 ) ) ;
#36230 = DIRECTION ( 'NONE',  ( 0.000000000000000000, -1.000000000000000000, -0.000000000000000000 ) ) ;
#36231 = CARTESIAN_POINT ( 'NONE',  ( 9.341766659739111134, -5.749051749107375819, -7.541331268112342556 ) ) ;
#36232 = ORIENTED_EDGE ( 'NONE', *, *, #11468, .F. ) ;
#36233 = CARTESIAN_POINT ( 'NONE',  ( 11.01810807141099957, -3.940954591493389891, 6.223352037434000117 ) ) ;
#36234 = CARTESIAN_POINT ( 'NONE',  ( 10.55463379556076831, 2.421258825577123464, -8.251507791233850142 ) ) ;
#36235 = CARTESIAN_POINT ( 'NONE',  ( 10.83253786428999987, 2.899999999999999911, 6.571291218949999902 ) ) ;
#36236 = EDGE_CURVE ( 'NONE', #6697, #56117, #33128, .T. ) ;
#36237 = CARTESIAN_POINT ( 'NONE',  ( 24.53429010490700080, 8.855930189872001534, 9.286429716155000236 ) ) ;
#36239 = DIRECTION ( 'NONE',  ( 0.000000000000000000, -1.000000000000000000, 0.000000000000000000 ) ) ;
#36238 = CARTESIAN_POINT ( 'NONE',  ( 10.46932803217000085, 4.988495740890000363, 6.213106455073000411 ) ) ;
#36240 = VECTOR ( 'NONE', #28715, 1000.000000000000000 ) ;
#36241 = CARTESIAN_POINT ( 'NONE',  ( 11.33456651104149948, 4.112542507956200133, -6.364824110469998963 ) ) ;
#36242 = FACE_OUTER_BOUND ( 'NONE', #68777, .T. ) ;
#36243 = CARTESIAN_POINT ( 'NONE',  ( 10.18491290906799840, 3.451408805716100314, -8.171383386399000415 ) ) ;
#36244 = CARTESIAN_POINT ( 'NONE',  ( 17.65049462686343773, 0.7131288892044757022, 12.57980326738671906 ) ) ;
#36245 = CARTESIAN_POINT ( 'NONE',  ( 6.785601289371999911, -0.8949653936606000171, 0.6576296519798999762 ) ) ;
#36246 = CARTESIAN_POINT ( 'NONE',  ( 11.46989666366029859, 3.941571897678119996, 6.185029684353999357 ) ) ;
#36247 = CARTESIAN_POINT ( 'NONE',  ( 10.66052890781999984, -2.899999999999999911, -6.152188490330000370 ) ) ;
#36248 = ORIENTED_EDGE ( 'NONE', *, *, #58665, .T. ) ;
#36249 = CARTESIAN_POINT ( 'NONE',  ( 8.539831853209999935, -5.633481712366999794, 7.451234046297000368 ) ) ;
#36250 = CARTESIAN_POINT ( 'NONE',  ( 4.000000000000000888, 2.094138670346413100, -0.5626148410812732426 ) ) ;
#36251 = CARTESIAN_POINT ( 'NONE',  ( 8.679055905797000037, 2.899999999999999911, 6.571291218949999902 ) ) ;
#36252 = B_SPLINE_CURVE_WITH_KNOTS ( 'NONE', 3,
 ( #37038, #24828, #31795, #67459 ),
 .UNSPECIFIED., .F., .F.,
 ( 4, 4 ),
 ( 0.000000000000000000, 1.000000000000000000 ),
 .UNSPECIFIED. ) ;
#36253 = ORIENTED_EDGE ( 'NONE', *, *, #62444, .T. ) ;
#36254 = VECTOR ( 'NONE', #33661, 1000.000000000000114 ) ;
#36255 = CARTESIAN_POINT ( 'NONE',  ( 18.53682146000800302, 2.876943948391000205, 12.22927217127999988 ) ) ;
#36256 = AXIS2_PLACEMENT_3D ( 'NONE', #23565, #34761, #66208 ) ;
#36257 = CARTESIAN_POINT ( 'NONE',  ( 11.56322412107030928, 4.054600656575539475, 8.532060764998998792 ) ) ;
#36258 = CARTESIAN_POINT ( 'NONE',  ( 10.88760471959000142, 5.634847467408999222, -7.088990678556999825 ) ) ;
#36259 = ORIENTED_EDGE ( 'NONE', *, *, #66129, .T. ) ;
#36260 = DIRECTION ( 'NONE',  ( 0.000000000000000000, 1.000000000000000000, 0.000000000000000000 ) ) ;
#36261 = CARTESIAN_POINT ( 'NONE',  ( 24.30001129978747443, 3.256147844935088909, -12.15210919425762803 ) ) ;
#36262 = CARTESIAN_POINT ( 'NONE',  ( 10.56733863405299800, 4.788475529394700558, 6.494205428462000107 ) ) ;
#36263 = EDGE_CURVE ( 'NONE', #50471, #57705, #38189, .T. ) ;
#36264 = DIRECTION ( 'NONE',  ( 0.000000000000000000, 1.000000000000000000, 0.000000000000000000 ) ) ;
#36265 = LINE ( 'NONE', #58619, #3321 ) ;
#36266 = VERTEX_POINT ( 'NONE', #4056 ) ;
#36267 = CARTESIAN_POINT ( 'NONE',  ( 7.871384613761001070, -5.129340912189999990, 6.740051747100999968 ) ) ;
#36268 = CARTESIAN_POINT ( 'NONE',  ( 7.566889158767000190, 2.100129367691999871, -7.493434492293999938 ) ) ;
#36269 = AXIS2_PLACEMENT_3D ( 'NONE', #28295, #64984, #12215 ) ;
#36270 = CARTESIAN_POINT ( 'NONE',  ( 8.287139215840040762, -4.779713743860946273, 9.054660631579276142 ) ) ;
#36271 = CARTESIAN_POINT ( 'NONE',  ( 10.02931740696899965, -3.762080884004200154, 6.243107450209000042 ) ) ;
#36272 = ORIENTED_EDGE ( 'NONE', *, *, #25190, .T. ) ;
#36273 = CARTESIAN_POINT ( 'NONE',  ( 10.41219359575999981, -4.853866617716000142, -4.884258404949999743 ) ) ;
#36274 = CARTESIAN_POINT ( 'NONE',  ( 10.43314899746000002, -5.167567567567999731, 6.822293592207000934 ) ) ;
#36275 = ORIENTED_EDGE ( 'NONE', *, *, #15946, .F. ) ;
#36276 = CARTESIAN_POINT ( 'NONE',  ( 12.80505043854146940, -1.875000000000000444, -13.78627172894481667 ) ) ;
#36277 = CARTESIAN_POINT ( 'NONE',  ( 25.60000000000000142, 2.023980670379999847, 11.01542190082000161 ) ) ;
#36278 = ORIENTED_EDGE ( 'NONE', *, *, #18314, .F. ) ;
#36279 = CARTESIAN_POINT ( 'NONE',  ( 9.446306596383999832, -5.231133027468000130, -6.569831606205999819 ) ) ;
#36280 = CARTESIAN_POINT ( 'NONE',  ( 2.405140132543083897, -0.9161175952574773795, -3.408904368339105595 ) ) ;
#36281 = CARTESIAN_POINT ( 'NONE',  ( 11.67403632436368888, 3.023821283238099955, -7.272033745815799755 ) ) ;
#36282 = CARTESIAN_POINT ( 'NONE',  ( 12.26588784977539959, -5.120865761890000201, 7.564049652083489228 ) ) ;
#36283 = DIRECTION ( 'NONE',  ( 0.000000000000000000, -1.000000000000000000, 0.000000000000000000 ) ) ;
#36284 = CARTESIAN_POINT ( 'NONE',  ( 11.16995391537419913, -3.056324258617099776, 6.859089544950699668 ) ) ;
#36285 = CARTESIAN_POINT ( 'NONE',  ( 7.239691113742999562, 4.389299166881000858, 9.135259451319999613 ) ) ;
#36286 = ORIENTED_EDGE ( 'NONE', *, *, #18427, .T. ) ;
#36287 = CARTESIAN_POINT ( 'NONE',  ( 9.096071945540000314, -5.102479135096000817, -6.621020973615999061 ) ) ;
#36288 = CARTESIAN_POINT ( 'NONE',  ( 17.55505043854144276, -0.7192913403693006469, 12.57945229203838444 ) ) ;
#36289 = CARTESIAN_POINT ( 'NONE',  ( 9.948096873516250938, 3.672815144550898303, 6.282534154164604701 ) ) ;
#36290 = ORIENTED_EDGE ( 'NONE', *, *, #7482, .F. ) ;
#36291 = CARTESIAN_POINT ( 'NONE',  ( 12.61477885367313156, -1.785717119372570272, -12.47282100101237212 ) ) ;
#36292 = CARTESIAN_POINT ( 'NONE',  ( 10.24394435321000074, -3.220344030624999743, -6.005416930865999703 ) ) ;
#36293 = CARTESIAN_POINT ( 'NONE',  ( 18.50003594167399967, 2.686563651857999613, 11.33603604486000016 ) ) ;
#36294 = CARTESIAN_POINT ( 'NONE',  ( 17.73974579646600347, -12.04854797699000102, 3.202106586035000202 ) ) ;
#36295 = CARTESIAN_POINT ( 'NONE',  ( 23.58894640129908993, -13.38207337446602629, -4.048532477468460122 ) ) ;
#36296 = CARTESIAN_POINT ( 'NONE',  ( 12.36142641661521147, -3.095968474609000154, -13.65339594101960330 ) ) ;
#36297 = CARTESIAN_POINT ( 'NONE',  ( 10.48133997687999930, -3.815400206859000054, -6.653701289769800020 ) ) ;
#36298 = FACE_OUTER_BOUND ( 'NONE', #28913, .T. ) ;
#36299 = EDGE_CURVE ( 'NONE', #44907, #60364, #20612, .T. ) ;
#36301 = EDGE_CURVE ( 'NONE', #57692, #67708, #62109, .T. ) ;
#36300 = CARTESIAN_POINT ( 'NONE',  ( 17.77874050697768382, -3.164693776342190734, 12.19609433843463187 ) ) ;
#36302 = EDGE_LOOP ( 'NONE', ( #11470, #67361, #44655, #61845 ) ) ;
#36303 = B_SPLINE_CURVE_WITH_KNOTS ( 'NONE', 3,
 ( #13680, #12993, #18231, #60532, #61226, #50735 ),
 .UNSPECIFIED., .F., .F.,
 ( 4, 2, 4 ),
 ( 0.000000000000000000, 0.5000000000000000000, 1.000000000000000000 ),
 .UNSPECIFIED. ) ;
#36304 = ORIENTED_EDGE ( 'NONE', *, *, #15221, .F. ) ;
#36305 = CARTESIAN_POINT ( 'NONE',  ( 5.000000000000000000, 0.000000000000000000, 0.000000000000000000 ) ) ;
#36306 = DIRECTION ( 'NONE',  ( 0.000000000000000000, -1.000000000000000000, 0.000000000000000000 ) ) ;
#36307 = CARTESIAN_POINT ( 'NONE',  ( 10.26195629121000152, -3.399999734730999812, 4.591198190832999515 ) ) ;
#36308 = CARTESIAN_POINT ( 'NONE',  ( 10.70780830849999887, 5.157484706885999692, -6.267808298721999627 ) ) ;
#36309 = B_SPLINE_CURVE_WITH_KNOTS ( 'NONE', 3,
 ( #47997, #96, #64052, #16174, #37500, #58823, #10931, #32274, #38180, #5678, #48335, #21755, #59512, #34691, #22795, #56003, #44832, #6715, #65442 ),
 .UNSPECIFIED., .F., .F.,
 ( 4, 1, 1, 1, 1, 1, 1, 1, 1, 1, 1, 1, 1, 1, 1, 1, 4 ),
 ( 0.000000000000000000, 0.04500088138722610487, 0.1100007829711507901, 0.1750006845550757251, 0.2400005861392325857, 0.3050004877231572986, 0.3700003893070824557, 0.4350002908912390942, 0.5000001924751640292, 0.5650000940590889087, 0.6299999956432456027, 0.6949998972271704822, 0.7599997988110954728, 0.8249997003950201302, 0.8899996019791770463, 0.9549995035631019258, 1.000000000000000000 ),
 .UNSPECIFIED. ) ;
#36310 = CARTESIAN_POINT ( 'NONE',  ( 8.674844125071947687, 5.060684314967137887, 6.220133919708653814 ) ) ;
#36311 = AXIS2_PLACEMENT_3D ( 'NONE', #28060, #28406, #49370 ) ;
#36312 = CARTESIAN_POINT ( 'NONE',  ( 17.96903643132312567, 2.968342805378973992, 12.33002008018445217 ) ) ;
#36313 = DIRECTION ( 'NONE',  ( 0.000000000000000000, 1.000000000000000000, 0.000000000000000000 ) ) ;
#36314 = CARTESIAN_POINT ( 'NONE',  ( 10.55991859298999991, 5.094266430778000121, 6.075406703384000018 ) ) ;
#36315 = VERTEX_POINT ( 'NONE', #47072 ) ;
#36316 = CARTESIAN_POINT ( 'NONE',  ( 3.899999503719000060, 0.000000000000000000, 0.000000000000000000 ) ) ;
#36317 = ORIENTED_EDGE ( 'NONE', *, *, #18421, .T. ) ;
#36318 = CARTESIAN_POINT ( 'NONE',  ( 12.48990506108392395, -3.039826403548177236, 12.30927084193774057 ) ) ;
#36319 = CARTESIAN_POINT ( 'NONE',  ( 8.575665180404380195, 5.349989392515093201, -7.683710349381269289 ) ) ;
#36320 = CARTESIAN_POINT ( 'NONE',  ( 9.632179190069999564, 5.638172764974000550, 6.476627236431999890 ) ) ;
#36321 = EDGE_CURVE ( 'NONE', #49429, #67945, #35214, .T. ) ;
#36322 = CARTESIAN_POINT ( 'NONE',  ( 11.88678751119029897, -5.166297436425000278, 6.889827023674499173 ) ) ;
#36323 = CARTESIAN_POINT ( 'NONE',  ( 9.020585841232000135, 4.920236664407999783, -6.448229650796999834 ) ) ;
#36324 = DIRECTION ( 'NONE',  ( -0.5298945028671029345, -0.5996714985845039703, 0.5996715014211040362 ) ) ;
#36325 = EDGE_CURVE ( 'NONE', #37829, #15559, #62787, .T. ) ;
#36326 = CARTESIAN_POINT ( 'NONE',  ( 10.69041504065829962, 5.024558373595999328, -6.736065107693399945 ) ) ;
#36327 = CARTESIAN_POINT ( 'NONE',  ( 12.47441792805236815, -0.5304820368560169142, 12.68508456201358747 ) ) ;
#36328 = CARTESIAN_POINT ( 'NONE',  ( 11.60000000000000320, 3.450002592736673090, -8.379764693824252930 ) ) ;
#36329 = B_SPLINE_CURVE_WITH_KNOTS ( 'NONE', 3,
 ( #1123, #43436, #64731, #16163 ),
 .UNSPECIFIED., .F., .F.,
 ( 4, 4 ),
 ( 0.000000000000000000, 1.000000000000000000 ),
 .UNSPECIFIED. ) ;
#36330 = CARTESIAN_POINT ( 'NONE',  ( 5.500000000000000000, 11.06886219213000011, -1.536526853569999851 ) ) ;
#36331 = FACE_OUTER_BOUND ( 'NONE', #35868, .T. ) ;
#36332 = ORIENTED_EDGE ( 'NONE', *, *, #56829, .F. ) ;
#36333 = CARTESIAN_POINT ( 'NONE',  ( 8.491329719591000469, 4.851303550474000303, -9.008742670124000540 ) ) ;
#36334 = CARTESIAN_POINT ( 'NONE',  ( 7.481792916052000031, -1.268175574387999882, 0.7201140061520999724 ) ) ;
#36335 = VECTOR ( 'NONE', #29891, 1000.000000000000114 ) ;
#36336 = CARTESIAN_POINT ( 'NONE',  ( 17.75799838104445172, 1.908512137131851860, 13.78121285638385807 ) ) ;
#36337 = CARTESIAN_POINT ( 'NONE',  ( 18.29999330150736014, 11.02846243710159868, -3.754394858750199848 ) ) ;
#36338 = CARTESIAN_POINT ( 'NONE',  ( 10.11476354018233081, 5.217465845835394411, -7.172815144550904520 ) ) ;
#36339 = CARTESIAN_POINT ( 'NONE',  ( 10.20641772631199906, -3.568446272909699957, -8.388315195900499788 ) ) ;
#36340 = ORIENTED_EDGE ( 'NONE', *, *, #55577, .F. ) ;
#36341 = CARTESIAN_POINT ( 'NONE',  ( 2.440293907525000083, 1.849469983415999996, -3.272124421528999960 ) ) ;
#36342 = CARTESIAN_POINT ( 'NONE',  ( 18.17506407531473656, -0.08141364318952959422, -12.69967032936936668 ) ) ;
#36344 = CARTESIAN_POINT ( 'NONE',  ( 11.26396921949000074, 3.857819209177999920, -11.66658462090000015 ) ) ;
#36343 = CARTESIAN_POINT ( 'NONE',  ( 9.841547757529466978, 3.644489497211603535, 9.239081501414979414 ) ) ;
#36345 = CARTESIAN_POINT ( 'NONE',  ( 24.30000000000000071, -2.258942858049999725, 12.29419282279000036 ) ) ;
#36346 = VERTEX_POINT ( 'NONE', #3376 ) ;
#36347 = CARTESIAN_POINT ( 'NONE',  ( 21.72233714749290101, -4.999803429358669504, 0.04433585200820151090 ) ) ;
#36348 = CARTESIAN_POINT ( 'NONE',  ( 18.08647318473503773, -2.829117779091809393, -13.59807435138920439 ) ) ;
#36349 = CARTESIAN_POINT ( 'NONE',  ( 10.99826088462129903, 4.001843064679911244, 8.366195817038299509 ) ) ;
#36350 = CARTESIAN_POINT ( 'NONE',  ( 11.05947712336570632, -5.538520942942948722, 7.349130516419520198 ) ) ;
#36351 = CARTESIAN_POINT ( 'NONE',  ( 9.015543146794000151, -4.175914961544999748, 5.699510287082000026 ) ) ;
#36352 = ORIENTED_EDGE ( 'NONE', *, *, #51855, .F. ) ;
#36353 = CARTESIAN_POINT ( 'NONE',  ( 8.764829719592999169, 5.808262417891000062, 7.446016144116000213 ) ) ;
#36355 = CARTESIAN_POINT ( 'NONE',  ( 10.38053305961999939, -5.283785200568999585, -8.830188095997000275 ) ) ;
#36354 = CARTESIAN_POINT ( 'NONE',  ( 10.72299000889467635, 3.772656371820692911, -8.344040565988990465 ) ) ;
#36356 = CARTESIAN_POINT ( 'NONE',  ( 7.617277775139868368, -4.886096859513470392, 6.002900497088587528 ) ) ;
#36357 = CARTESIAN_POINT ( 'NONE',  ( 17.95719809555263069, -0.4784561392272737579, 13.88891570267564113 ) ) ;
#36359 = CARTESIAN_POINT ( 'NONE',  ( 24.38453493561400265, 3.342915742751000341, 12.19240510248000042 ) ) ;
#36358 = VECTOR ( 'NONE', #68218, 1000.000000000000227 ) ;
#36360 = ORIENTED_EDGE ( 'NONE', *, *, #27979, .F. ) ;
#36361 = CARTESIAN_POINT ( 'NONE',  ( 11.09999999999999964, 0.5000000000000000000, 5.124965750789000296 ) ) ;
#36362 = B_SPLINE_CURVE_WITH_KNOTS ( 'NONE', 3,
 ( #15547, #16224, #16570, #36876, #58878, #10294 ),
 .UNSPECIFIED., .F., .F.,
 ( 4, 1, 1, 4 ),
 ( 0.000000000000000000, 0.3333333333333000081, 0.6666666666667000474, 1.000000000000000000 ),
 .UNSPECIFIED. ) ;
#36363 = CARTESIAN_POINT ( 'NONE',  ( 11.69102897915239936, -3.743141152489600110, 6.529961657816500065 ) ) ;
#36364 = CARTESIAN_POINT ( 'NONE',  ( 9.905792474809000936, 2.698958900805999761, 8.979236532123000103 ) ) ;
#36365 = CARTESIAN_POINT ( 'NONE',  ( 9.465106464520001595, 2.290037071913000322, 6.601704384062999864 ) ) ;
#36366 = VECTOR ( 'NONE', #22705, 999.9999999999998863 ) ;
#36367 = CARTESIAN_POINT ( 'NONE',  ( 10.74379975933729980, 5.078682052940000524, 7.871126858273000515 ) ) ;
#36368 = CARTESIAN_POINT ( 'NONE',  ( 17.80000000001300009, -3.351264566333000072, -11.15757590352999884 ) ) ;
#36369 = CARTESIAN_POINT ( 'NONE',  ( 24.30001680106099826, 12.21047197645999915, -3.271805488357999891 ) ) ;
#36370 = CARTESIAN_POINT ( 'NONE',  ( 21.59999987243000064, 1.172395514003999961E-13, -2.486899575159999765E-14 ) ) ;
#36371 = CARTESIAN_POINT ( 'NONE',  ( 24.44496356267099912, -8.810485190366000197, 8.810508100388000585 ) ) ;
#36372 = CARTESIAN_POINT ( 'NONE',  ( 18.25624423923971662, -2.332236704353563450, 13.80437652844154073 ) ) ;
#36373 = CARTESIAN_POINT ( 'NONE',  ( 17.96849574074740730, 2.968826013471339564, -13.56277633467329125 ) ) ;
#36374 = ORIENTED_EDGE ( 'NONE', *, *, #60838, .T. ) ;
#36375 = DIRECTION ( 'NONE',  ( -1.000000000000000000, 0.000000000000000000, 0.000000000000000000 ) ) ;
#36376 = CARTESIAN_POINT ( 'NONE',  ( 9.705773468360421319, -5.100000000000000533, -6.304440313841761068 ) ) ;
#36377 = ORIENTED_EDGE ( 'NONE', *, *, #31798, .F. ) ;
#36378 = CARTESIAN_POINT ( 'NONE',  ( 12.40000000000000213, 12.27510221496999954, 1.916289661941000144 ) ) ;
#36379 = CARTESIAN_POINT ( 'NONE',  ( 1.700000000000000178, 0.000000000000000000, 0.000000000000000000 ) ) ;
#36380 = CARTESIAN_POINT ( 'NONE',  ( 9.600491906670001185, 5.206545077004999911, 8.585111878242999595 ) ) ;
#36381 = CARTESIAN_POINT ( 'NONE',  ( 10.39355883036999906, 4.089958667033000594, -9.188186800857998549 ) ) ;
#36382 = CARTESIAN_POINT ( 'NONE',  ( 9.074925248765625341, -4.744576382809566617, -7.040502144637257764 ) ) ;
#36383 = CARTESIAN_POINT ( 'NONE',  ( 9.298040139821001304, -4.087076480742000584, 9.429402848390999736 ) ) ;
#36384 = CARTESIAN_POINT ( 'NONE',  ( 18.27977754798708787, -0.02297882141078106538, -12.59998453421652442 ) ) ;
#36385 = CARTESIAN_POINT ( 'NONE',  ( 12.54534433731234877, 3.068834427905941187, -12.30067458026015359 ) ) ;
#36386 = CARTESIAN_POINT ( 'NONE',  ( 11.06795257254739973, -4.963546614172099858, -7.780229861306499295 ) ) ;
#36387 = EDGE_CURVE ( 'NONE', #32326, #22792, #43141, .T. ) ;
#36389 = EDGE_CURVE ( 'NONE', #26858, #30735, #4747, .T. ) ;
#36388 = CARTESIAN_POINT ( 'NONE',  ( 7.224759086135252417, -0.7889424787723180454, 0.8956307892555190886 ) ) ;
#36390 = ORIENTED_EDGE ( 'NONE', *, *, #53040, .F. ) ;
#36391 = B_SPLINE_CURVE_WITH_KNOTS ( 'NONE', 3,
 ( #39482, #7664, #29010, #50317 ),
 .UNSPECIFIED., .F., .F.,
 ( 4, 4 ),
 ( 0.000000000000000000, 1.000000000000000000 ),
 .UNSPECIFIED. ) ;
#36392 = CARTESIAN_POINT ( 'NONE',  ( 24.94498139921191893, -2.983199262474947488, 11.60459641112071871 ) ) ;
#36393 = FACE_OUTER_BOUND ( 'NONE', #66661, .T. ) ;
#36394 = CARTESIAN_POINT ( 'NONE',  ( 24.89076865818686812, 8.576159828362898807, 8.441116150885008551 ) ) ;
#36395 = CONICAL_SURFACE ( 'NONE', #38639, 12.44999944941000081, 0.7853981146832407223 ) ;
#36396 = CARTESIAN_POINT ( 'NONE',  ( 6.981185917753003345, 10.82755309799000010, 3.400726541711003748 ) ) ;
#36397 = CARTESIAN_POINT ( 'NONE',  ( 12.08963668261105617, 2.638435792642065625, 13.74915318082108762 ) ) ;
#36398 = CARTESIAN_POINT ( 'NONE',  ( 10.94797187187000098, -2.864324950622999744, 8.846246404612999825 ) ) ;
#36399 = CARTESIAN_POINT ( 'NONE',  ( 12.42592538289389914, -0.4969854666067609616, -12.68691056894716773 ) ) ;
#36400 = CARTESIAN_POINT ( 'NONE',  ( 12.32690743522623400, -0.5490318484135010557, 13.98923259457975909 ) ) ;
#36401 = ORIENTED_EDGE ( 'NONE', *, *, #19365, .F. ) ;
#36402 = CARTESIAN_POINT ( 'NONE',  ( 24.35145719007200071, 8.929422700512001043, 9.054903155755001265 ) ) ;
#36403 = CARTESIAN_POINT ( 'NONE',  ( 9.709696787963999043, -3.780328739572700325, -6.239790126677999815 ) ) ;
#36404 = FACE_OUTER_BOUND ( 'NONE', #45701, .T. ) ;
#36405 = CARTESIAN_POINT ( 'NONE',  ( 10.06343867337000120, -5.156226070197000411, 6.125223053176999777 ) ) ;
#36406 = CARTESIAN_POINT ( 'NONE',  ( 9.141935773284000533, -3.399999999999999911, -6.632262360512000576 ) ) ;
#36407 = CARTESIAN_POINT ( 'NONE',  ( 12.35159063708299954, -3.174974693948799942, 7.268038553423699533 ) ) ;
#36408 = AXIS2_PLACEMENT_3D ( 'NONE', #13674, #18915, #67480 ) ;
#36409 = ADVANCED_FACE ( 'NONE', ( #24368 ), #51617, .F. ) ;
#36410 = TOROIDAL_SURFACE ( 'NONE', #53134, 6.000000000000000000, 1.000000000000000000 ) ;
#36411 = CARTESIAN_POINT ( 'NONE',  ( 12.11859257910638554, 0.2316996085785973380, 12.59787430930301433 ) ) ;
#36412 = CARTESIAN_POINT ( 'NONE',  ( 9.009297488802992859, 5.100000000000000533, 6.455145051482742424 ) ) ;
#36413 = CARTESIAN_POINT ( 'NONE',  ( 8.133277933996836850, 2.820894615410977746, 8.178702166371902393 ) ) ;
#36414 = CARTESIAN_POINT ( 'NONE',  ( 12.51357205051171562, 1.821485253447863384, 12.46764665430163532 ) ) ;
#36415 = CARTESIAN_POINT ( 'NONE',  ( 9.267891187585000523, -4.645169647889000331, -5.840816811670999975 ) ) ;
#36416 = CARTESIAN_POINT ( 'NONE',  ( 10.37872469555899890, 4.502158848185001006, -6.631215019384099740 ) ) ;
#36417 = CARTESIAN_POINT ( 'NONE',  ( 12.33432433144330354, 11.58110100107862728, -4.770114854518291203 ) ) ;
#36418 = CARTESIAN_POINT ( 'NONE',  ( 10.81187971959000116, 4.614148948243999904, -5.930135044105000475 ) ) ;
#36419 = CARTESIAN_POINT ( 'NONE',  ( 9.807938025973999885, 3.334935831489500124, -6.407263051216999017 ) ) ;
#36421 = CARTESIAN_POINT ( 'NONE',  ( 12.19562994360508590, 2.360937373133742856, 12.48287347411684500 ) ) ;
#36420 = DIRECTION ( 'NONE',  ( 0.000000000000000000, 0.9048270524660052549, -0.4257792915651026910 ) ) ;
#36422 = FACE_OUTER_BOUND ( 'NONE', #1828, .T. ) ;
#36423 = ORIENTED_EDGE ( 'NONE', *, *, #32610, .F. ) ;
#36424 = CARTESIAN_POINT ( 'NONE',  ( 12.29580549790138377, -0.3624889081508343991, 12.69304043450447850 ) ) ;
#36425 = CARTESIAN_POINT ( 'NONE',  ( 10.31059687351633158, 3.370476274536378103, 8.592232985442823434 ) ) ;
#36426 = DIRECTION ( 'NONE',  ( 0.8660254006610920152, 3.948310870465965241E-12, 0.5000000054097949453 ) ) ;
#36427 = CARTESIAN_POINT ( 'NONE',  ( 9.399709346416997846, 4.783195203880800328, 7.871904849557299855 ) ) ;
#36428 = DIRECTION ( 'NONE',  ( 1.000000000000000000, 0.000000000000000000, 0.000000000000000000 ) ) ;
#36429 = CARTESIAN_POINT ( 'NONE',  ( 12.18824001706384763, -2.602861674270837256, 13.65112526288235451 ) ) ;
#36430 = CARTESIAN_POINT ( 'NONE',  ( 12.18817138782660514, 2.600938394344443960, 13.65148521156839045 ) ) ;
#36431 = CARTESIAN_POINT ( 'NONE',  ( 24.30000000000000071, 3.224868684338999980, 12.03537377768999939 ) ) ;
#36432 = ORIENTED_EDGE ( 'NONE', *, *, #28020, .F. ) ;
#36433 = CARTESIAN_POINT ( 'NONE',  ( 4.832209180879999622, -1.128524195065999880, -0.1154945620947999962 ) ) ;
#36434 = CARTESIAN_POINT ( 'NONE',  ( 9.276025935145998602, -4.185743043590700374, -6.234344474498000110 ) ) ;
#36435 = DIRECTION ( 'NONE',  ( 1.000000000000000000, 0.000000000000000000, 0.000000000000000000 ) ) ;
#36436 = CARTESIAN_POINT ( 'NONE',  ( 11.01925056272500036, -2.825232917634000085, 7.482589369563879877 ) ) ;
#36437 = CARTESIAN_POINT ( 'NONE',  ( 18.15589597092046859, 2.672372730248489425, -12.40976522372663737 ) ) ;
#36438 = LINE ( 'NONE', #52516, #66747 ) ;
#36439 = CARTESIAN_POINT ( 'NONE',  ( 18.18005044388380043, 2.499999700417821380, 12.45156116530496604 ) ) ;
#36440 = EDGE_CURVE ( 'NONE', #12675, #26552, #19117, .T. ) ;
#36441 = EDGE_CURVE ( 'NONE', #48090, #15819, #3713, .T. ) ;
#36442 = CARTESIAN_POINT ( 'NONE',  ( 17.74422827371068223, 3.224484589774872401, 13.62361160044438790 ) ) ;
#36443 = CARTESIAN_POINT ( 'NONE',  ( 11.04437549732999813, -2.755184240810999885, -5.169198519660000990 ) ) ;
#36444 = CARTESIAN_POINT ( 'NONE',  ( 11.09992055961999924, -2.373397911211000189, -6.776606350776999577 ) ) ;
#36445 = CARTESIAN_POINT ( 'NONE',  ( 24.44496356267099912, -8.810485190366000197, 8.810508100388000585 ) ) ;
#36446 = CARTESIAN_POINT ( 'NONE',  ( 12.18940025506973335, 0.3858260082455223228, -13.99468631105252037 ) ) ;
#36447 = CARTESIAN_POINT ( 'NONE',  ( 17.55505043854143565, 3.125000000000000000, 12.28373071562070074 ) ) ;
#36448 = DIRECTION ( 'NONE',  ( 1.000000000000000000, -1.386239579945032070E-15, 9.986219791750131332E-15 ) ) ;
#36449 = DIRECTION ( 'NONE',  ( 0.7071067811865475727, -0.7071067811865475727, 0.000000000000000000 ) ) ;
#36450 = VERTEX_POINT ( 'NONE', #35555 ) ;
#36451 = CARTESIAN_POINT ( 'NONE',  ( 9.848670280409999478, 5.002683760508999988, -8.912673867568997821 ) ) ;
#36452 = CARTESIAN_POINT ( 'NONE',  ( 11.05518582084300050, -4.566724035220099509, 8.155074391384399490 ) ) ;
#36453 = EDGE_LOOP ( 'NONE', ( #38292, #27127, #599, #17784 ) ) ;
#36454 = CONICAL_SURFACE ( 'NONE', #30922, 1.150084366273999903, 0.7854618604947302130 ) ;
#36455 = CARTESIAN_POINT ( 'NONE',  ( 24.30000000000000071, 8.756202924575998026, 7.455126447192999883 ) ) ;
#36456 = CARTESIAN_POINT ( 'NONE',  ( 17.95040605897955643, 3.130086699081791490, -13.64560748759990894 ) ) ;
#36457 = ORIENTED_EDGE ( 'NONE', *, *, #15179, .F. ) ;
#36458 = CARTESIAN_POINT ( 'NONE',  ( 10.88813259637009878, 2.844182332072999753, 6.870201387206400057 ) ) ;
#36459 = CARTESIAN_POINT ( 'NONE',  ( 9.491735841231999871, 3.920043641733999884, -9.398198753036000497 ) ) ;
#36460 = CARTESIAN_POINT ( 'NONE',  ( 17.92913687513144794, 3.216295279492275672, -11.40344415250779520 ) ) ;
#36461 = CYLINDRICAL_SURFACE ( 'NONE', #5449, 1.000000000000000000 ) ;
#36462 = CARTESIAN_POINT ( 'NONE',  ( 4.599999999999999645, -3.248109929747638347, 13.61799478206225622 ) ) ;
#36463 = DIRECTION ( 'NONE',  ( 0.7071068156326932863, 0.000000000000000000, -0.7071067467404001938 ) ) ;
#36464 = VERTEX_POINT ( 'NONE', #29979 ) ;
#36465 = FACE_OUTER_BOUND ( 'NONE', #26683, .T. ) ;
#36467 = EDGE_CURVE ( 'NONE', #66715, #31306, #24713, .T. ) ;
#36466 = CARTESIAN_POINT ( 'NONE',  ( 9.187479719595000205, 2.391443348526999912, -6.856688371964000162 ) ) ;
#36468 = ORIENTED_EDGE ( 'NONE', *, *, #4512, .T. ) ;
#36469 = CARTESIAN_POINT ( 'NONE',  ( 11.17811698873999937, 2.762452057009999962, -6.187198315927000536 ) ) ;
#36470 = EDGE_CURVE ( 'NONE', #63258, #50154, #67684, .T. ) ;
#36471 = VERTEX_POINT ( 'NONE', #69073 ) ;
#36472 = CARTESIAN_POINT ( 'NONE',  ( 8.794772138681999252, 3.523984281974800403, 8.687347221188998603 ) ) ;
#36473 = CARTESIAN_POINT ( 'NONE',  ( 18.01423850902973101, -2.075512308681780382, -12.54039470262456568 ) ) ;
#36474 = CARTESIAN_POINT ( 'NONE',  ( 11.35179910620000143, -11.71014626380999957, -1.422059914427000082 ) ) ;
#36475 = DIRECTION ( 'NONE',  ( 0.000000000000000000, 0.000000000000000000, -1.000000000000000000 ) ) ;
#36476 = LINE ( 'NONE', #57800, #34836 ) ;
#36477 = ORIENTED_EDGE ( 'NONE', *, *, #43571, .T. ) ;
#36478 = CARTESIAN_POINT ( 'NONE',  ( 11.86287780003600112, 11.93788271774999998, -3.912105503483000124 ) ) ;
#36479 = CARTESIAN_POINT ( 'NONE',  ( 17.71880694038500437, 12.04903009916999856, -3.200100868470999949 ) ) ;
#36480 = CARTESIAN_POINT ( 'NONE',  ( 7.945608795480825215, -5.314576234847506520, 7.853946780411532380 ) ) ;
#36481 = CARTESIAN_POINT ( 'NONE',  ( 8.410398127216412334, -5.351350780489295467, 7.263115598813800311 ) ) ;
#36482 = AXIS2_PLACEMENT_3D ( 'NONE', #62422, #24687, #2670 ) ;
#36483 = B_SPLINE_CURVE_WITH_KNOTS ( 'NONE', 3,
 ( #68394, #36600, #19489, #14250, #51977, #30001 ),
 .UNSPECIFIED., .F., .F.,
 ( 4, 2, 4 ),
 ( 0.000000000000000000, 0.5000000000000000000, 1.000000000000000000 ),
 .UNSPECIFIED. ) ;
#36484 = EDGE_CURVE ( 'NONE', #18161, #16052, #58495, .T. ) ;
#36485 = CARTESIAN_POINT ( 'NONE',  ( 8.450464158772000189, 3.789127741898000057, -9.388182174781999123 ) ) ;
#36486 = CIRCLE ( 'NONE', #26461, 12.50000000000000000 ) ;
#36487 = CARTESIAN_POINT ( 'NONE',  ( 6.899999438051000133, 0.000000000000000000, 0.000000000000000000 ) ) ;
#36488 = CARTESIAN_POINT ( 'NONE',  ( 10.73506343560000076, -5.202499304193000107, -8.441414596927000247 ) ) ;
#36489 = VERTEX_POINT ( 'NONE', #38289 ) ;
#36490 = VERTEX_POINT ( 'NONE', #48788 ) ;
#36491 = CARTESIAN_POINT ( 'NONE',  ( 9.070310841232000598, 5.361622798585000460, -7.185294144754000634 ) ) ;
#36492 = CIRCLE ( 'NONE', #40945, 11.29999999999999538 ) ;
#36493 = DIRECTION ( 'NONE',  ( 1.000000000000000000, 0.000000000000000000, 0.000000000000000000 ) ) ;
#36494 = CARTESIAN_POINT ( 'NONE',  ( 9.938608878791999501, 3.772542739612499751, 8.478317686146800369 ) ) ;
#36495 = DIRECTION ( 'NONE',  ( 0.7071059447856029578, 0.7071076175865028679, -3.669605936760013587E-09 ) ) ;
#36496 = CARTESIAN_POINT ( 'NONE',  ( 11.09590547754519996, 5.315605332491999846, -7.541753805330609239 ) ) ;
#36497 = CARTESIAN_POINT ( 'NONE',  ( 10.06726717315599906, 3.340104753140699767, -6.937642277832399174 ) ) ;
#36499 = CARTESIAN_POINT ( 'NONE',  ( 7.760448372719867649, 3.361655312119658401, 6.300695999402769587 ) ) ;
#36498 = CARTESIAN_POINT ( 'NONE',  ( 10.28165911260399845, -4.436443689698799986, 6.595367916746299741 ) ) ;
#36500 = PLANE ( 'NONE',  #3986 ) ;
#36501 = ORIENTED_EDGE ( 'NONE', *, *, #9133, .T. ) ;
#36502 = CIRCLE ( 'NONE', #32072, 1.500000000000000000 ) ;
#36503 = CARTESIAN_POINT ( 'NONE',  ( 9.643930206848999376, 5.250000000000000000, -7.500000000000000000 ) ) ;
#36504 = CARTESIAN_POINT ( 'NONE',  ( 8.335542453529990681, -2.897657451248000893, 6.653312621732999865 ) ) ;
#36505 = CARTESIAN_POINT ( 'NONE',  ( 9.633709346416999608, 5.155548326249999924, 8.048718920009699573 ) ) ;
#36506 = LINE ( 'NONE', #14843, #64869 ) ;
#36507 = VECTOR ( 'NONE', #41693, 1000.000000000000000 ) ;
#36508 = CARTESIAN_POINT ( 'NONE',  ( 10.00137895011999944, -3.855365288061999962, 5.709482985498999241 ) ) ;
#36509 = CARTESIAN_POINT ( 'NONE',  ( 18.12484680926279879, 2.757022365696005117, -12.38798834874709875 ) ) ;
#36510 = CARTESIAN_POINT ( 'NONE',  ( 15.86222979673600264, -3.623677739266000231, -11.32125985288999992 ) ) ;
#36511 = CARTESIAN_POINT ( 'NONE',  ( 8.856851002545001350, 2.832432432432000269, -6.822293592207000934 ) ) ;
#36512 = DIRECTION ( 'NONE',  ( 0.000000000000000000, 0.000000000000000000, -1.000000000000000000 ) ) ;
#36513 = CARTESIAN_POINT ( 'NONE',  ( 10.16657120343299958, -4.048688523195909994, -8.503230697164999796 ) ) ;
#36514 = CARTESIAN_POINT ( 'NONE',  ( 11.13351354018304740, -2.750000000000000000, 7.336375382625529795 ) ) ;
#36515 = CARTESIAN_POINT ( 'NONE',  ( 18.50013789939208664, 2.065999734462983189E-14, -11.64999999999999325 ) ) ;
#36516 = CARTESIAN_POINT ( 'NONE',  ( 17.92325670924426362, 1.853371315686558773, 12.46300045701071291 ) ) ;
#36517 = CARTESIAN_POINT ( 'NONE',  ( 2.776473774021000374, 3.125185655655999817, -0.9243923524902999400 ) ) ;
#36518 = ORIENTED_EDGE ( 'NONE', *, *, #2221, .T. ) ;
#36519 = ADVANCED_FACE ( 'NONE', ( #48100 ), #55215, .T. ) ;
#36520 = ADVANCED_FACE ( 'NONE', ( #25306 ), #29555, .T. ) ;
#36521 = CARTESIAN_POINT ( 'NONE',  ( 12.60374982967590185, 0.5917829749564897934, -12.68143435689272280 ) ) ;
#36522 = CARTESIAN_POINT ( 'NONE',  ( 12.18035041863325851, -2.521826826373486874, -12.44645458621850942 ) ) ;
#36523 = DIRECTION ( 'NONE',  ( 1.000000000000000000, 0.000000000000000000, -0.000000000000000000 ) ) ;
#36524 = FACE_OUTER_BOUND ( 'NONE', #64476, .T. ) ;
#36525 = LINE ( 'NONE', #15549, #68383 ) ;
#36526 = ORIENTED_EDGE ( 'NONE', *, *, #6212, .F. ) ;
#36527 = CARTESIAN_POINT ( 'NONE',  ( 18.30017264560542145, -1.838307228410961613, -11.74271423071413523 ) ) ;
#36528 = EDGE_CURVE ( 'NONE', #22723, #32483, #30226, .T. ) ;
#36529 = APPLICATION_PROTOCOL_DEFINITION ( 'draft international standard', 'automotive_design', 1998, #6535 ) ;
#36530 = CARTESIAN_POINT ( 'NONE',  ( 0.6048333392154046084, 0.9397506571931915076, 3.402778030820548416 ) ) ;
#36531 = CARTESIAN_POINT ( 'NONE',  ( 13.64382898362900143, -11.47858090575000034, -2.288513382665999796 ) ) ;
#36532 = CARTESIAN_POINT ( 'NONE',  ( 10.71480780573045699, 2.649489222497333429, 7.676606295960487714 ) ) ;
#36533 = CARTESIAN_POINT ( 'NONE',  ( 13.06531638133300177, 12.22210578456000007, 1.955102404769999858 ) ) ;
#36534 = ORIENTED_EDGE ( 'NONE', *, *, #43735, .T. ) ;
#36535 = AXIS2_PLACEMENT_3D ( 'NONE', #61599, #13716, #24195 ) ;
#36536 = CARTESIAN_POINT ( 'NONE',  ( 11.00366278039000001, -2.264082614160999984, 7.798350693290999835 ) ) ;
#36537 = ORIENTED_EDGE ( 'NONE', *, *, #56274, .T. ) ;
#36538 = CARTESIAN_POINT ( 'NONE',  ( 16.10004050617000004, 3.886235259787000018, 11.90683839252000098 ) ) ;
#36539 = CARTESIAN_POINT ( 'NONE',  ( 8.572269353210000276, -2.606998386752999775, 6.345764833140000505 ) ) ;
#36540 = CARTESIAN_POINT ( 'NONE',  ( 17.64985702823327784, -0.7243378955761968774, -13.98124959093732400 ) ) ;
#36541 = EDGE_LOOP ( 'NONE', ( #3744, #64197, #9079, #43263 ) ) ;
#36542 = CARTESIAN_POINT ( 'NONE',  ( 23.58820312822635756, 10.20123823674837382, 9.561024946571489380 ) ) ;
#36543 = LINE ( 'NONE', #57869, #59511 ) ;
#36544 = CARTESIAN_POINT ( 'NONE',  ( 6.984954719590999339, 2.766448485756999975, -6.536937350656000234 ) ) ;
#36545 = CONICAL_SURFACE ( 'NONE', #45494, 1.899997304679999610, 0.7853981633972997312 ) ;
#36546 = DIRECTION ( 'NONE',  ( 0.7071067811865093811, -0.08614499102994124802, -0.7018397541608093482 ) ) ;
#36547 = CARTESIAN_POINT ( 'NONE',  ( 10.90000000000000036, 0.2500000000000000000, 9.776630298829998011 ) ) ;
#36548 = ORIENTED_EDGE ( 'NONE', *, *, #43260, .T. ) ;
#36549 = CARTESIAN_POINT ( 'NONE',  ( 10.18755811987000115, -5.387486580809999204, 8.640943191857999750 ) ) ;
#36550 = CARTESIAN_POINT ( 'NONE',  ( 21.70000133425200062, 0.000000000000000000, 0.000000000000000000 ) ) ;
#36551 = CARTESIAN_POINT ( 'NONE',  ( 7.307500000000000107, -0.2999999999999999889, -3.149999999999999911 ) ) ;
#36552 = ORIENTED_EDGE ( 'NONE', *, *, #8541, .F. ) ;
#36553 = CARTESIAN_POINT ( 'NONE',  ( 10.72303951155000057, -3.890113427500999421, -8.859339185702999941 ) ) ;
#36554 = AXIS2_PLACEMENT_3D ( 'NONE', #48396, #36883, #15888 ) ;
#36555 = CYLINDRICAL_SURFACE ( 'NONE', #25891, 1.999999999999999778 ) ;
#36556 = VERTEX_POINT ( 'NONE', #51533 ) ;
#36557 = CARTESIAN_POINT ( 'NONE',  ( 4.904219950104667269, 1.237977404532700332, 0.8781525088298995918 ) ) ;
#36558 = CARTESIAN_POINT ( 'NONE',  ( 24.22565383484945656, 12.33873734749843187, -3.306152860255493930 ) ) ;
#36559 = CARTESIAN_POINT ( 'NONE',  ( 5.600000001140999828, 0.000000000000000000, 0.000000000000000000 ) ) ;
#36560 = FACE_OUTER_BOUND ( 'NONE', #8872, .T. ) ;
#36561 = DIRECTION ( 'NONE',  ( -1.000000000000000000, 0.000000000000000000, 0.000000000000000000 ) ) ;
#36562 = LINE ( 'NONE', #52295, #49995 ) ;
#36563 = VECTOR ( 'NONE', #27887, 1000.000000000000000 ) ;
#36564 = CARTESIAN_POINT ( 'NONE',  ( 9.623096873515669003, -2.782534154164605145, -7.827184855449101697 ) ) ;
#36565 = CARTESIAN_POINT ( 'NONE',  ( 10.40516264833000015, -5.216401621862000404, 6.765753642936999768 ) ) ;
#36566 = ORIENTED_EDGE ( 'NONE', *, *, #34188, .F. ) ;
#36567 = CARTESIAN_POINT ( 'NONE',  ( 10.29399293566599916, -3.453258297007899991, -8.170700474995699736 ) ) ;
#36568 = ORIENTED_EDGE ( 'NONE', *, *, #47750, .T. ) ;
#36569 = CARTESIAN_POINT ( 'NONE',  ( 10.72520610419000064, 5.521650664120000940, 6.612990918765000004 ) ) ;
#36570 = CYLINDRICAL_SURFACE ( 'NONE', #35581, 11.84999999999999964 ) ;
#36571 = CARTESIAN_POINT ( 'NONE',  ( 12.80505043854143388, 1.874999999999999112, -13.78631952119025428 ) ) ;
#36572 = CARTESIAN_POINT ( 'NONE',  ( 2.810090735696999964, -3.340490407592999755, -1.609581997777000062 ) ) ;
#36573 = CARTESIAN_POINT ( 'NONE',  ( 25.41679837370699957, 2.809785212777999863, 11.31864426913000088 ) ) ;
#36574 = EDGE_CURVE ( 'NONE', #62089, #61638, #8972, .T. ) ;
#36575 = CARTESIAN_POINT ( 'NONE',  ( 25.30000327618300204, 10.36736154742122018, -5.168041346173460227 ) ) ;
#36576 = CARTESIAN_POINT ( 'NONE',  ( 18.14887598846753036, 0.1995645667416934554, 13.89814765003537644 ) ) ;
#36577 = ORIENTED_EDGE ( 'NONE', *, *, #30204, .T. ) ;
#36578 = EDGE_CURVE ( 'NONE', #16464, #35599, #46501, .T. ) ;
#36579 = CARTESIAN_POINT ( 'NONE',  ( 12.83523642498299999, -11.49802605210000195, 4.818062943702999590 ) ) ;
#36580 = CARTESIAN_POINT ( 'NONE',  ( 10.80072469555900128, -3.429147315060100176, 8.487632181750699445 ) ) ;
#36581 = CARTESIAN_POINT ( 'NONE',  ( 3.217640132543999165, -1.762666431298159475, 3.058252359239895135 ) ) ;
#36582 = CARTESIAN_POINT ( 'NONE',  ( 10.59393020684899867, -2.750000000000000000, -7.500000000000000000 ) ) ;
#36583 = CARTESIAN_POINT ( 'NONE',  ( 9.298691940377999288, -5.159251056493999954, 9.109488373271000583 ) ) ;
#36585 = CARTESIAN_POINT ( 'NONE',  ( 24.35365242081700288, -3.193712117558000774, -11.49150331547998860 ) ) ;
#36584 = CARTESIAN_POINT ( 'NONE',  ( 10.90374609491999891, 3.726846467344000047, 5.900456154266000119 ) ) ;
#36586 = CARTESIAN_POINT ( 'NONE',  ( 11.23195122972050086, 4.507250159094099651, -6.326963915009999440 ) ) ;
#36587 = AXIS2_PLACEMENT_3D ( 'NONE', #17613, #27759, #1182 ) ;
#36588 = CARTESIAN_POINT ( 'NONE',  ( 8.724507172011824352, -4.124235577930278396, -8.374507226493388856 ) ) ;
#36589 = PRESENTATION_LAYER_ASSIGNMENT (  '', '', ( #48873 ) ) ;
#36590 = CARTESIAN_POINT ( 'NONE',  ( 9.906292290062998163, 4.749786674456300872, -7.064651992867799990 ) ) ;
#36591 = CARTESIAN_POINT ( 'NONE',  ( 18.18333067157141514, 0.3597103837127935133, 12.59488153751295769 ) ) ;
#36592 = CARTESIAN_POINT ( 'NONE',  ( 7.215837234118000154, -1.085830440727999946, 0.6165721249222000377 ) ) ;
#36593 = CARTESIAN_POINT ( 'NONE',  ( 11.42834208742529967, 3.293478249981899975, 6.389420067180999752 ) ) ;
#36594 = AXIS2_PLACEMENT_3D ( 'NONE', #58601, #26803, #5799 ) ;
#36595 = FACE_OUTER_BOUND ( 'NONE', #35065, .T. ) ;
#36596 = ORIENTED_EDGE ( 'NONE', *, *, #57794, .F. ) ;
#36597 = CARTESIAN_POINT ( 'NONE',  ( 7.262120559621999760, -4.847802017252000439, 9.065364004483999594 ) ) ;
#36598 = CARTESIAN_POINT ( 'NONE',  ( 9.208105646793001142, -5.057079407184000175, 8.967634647348999621 ) ) ;
#36599 = CARTESIAN_POINT ( 'NONE',  ( 4.000000000000000000, 0.2816038378556621202, -2.150035234257813510 ) ) ;
#36600 = CARTESIAN_POINT ( 'NONE',  ( 6.910969021048729566, 0.2454124519544698679, 1.504446442354156366 ) ) ;
#36601 = EDGE_LOOP ( 'NONE', ( #65768, #23554, #37452, #2592 ) ) ;
#36602 = AXIS2_PLACEMENT_3D ( 'NONE', #47359, #38232, #16219 ) ;
#36603 = CARTESIAN_POINT ( 'NONE',  ( 0.6501162859548000883, 0.8965373106020000371, -3.081807587122999958 ) ) ;
#36604 = CARTESIAN_POINT ( 'NONE',  ( 11.35034208742529849, 3.369365911179700301, 6.508707709313799050 ) ) ;
#36605 = CARTESIAN_POINT ( 'NONE',  ( 10.37239528041000014, 3.992345698584000235, -5.977238432995000572 ) ) ;
#36606 = ORIENTED_EDGE ( 'NONE', *, *, #62563, .T. ) ;
#36607 = EDGE_CURVE ( 'NONE', #12790, #16879, #29804, .T. ) ;
#36608 = CARTESIAN_POINT ( 'NONE',  ( 12.80505043854144276, -0.7192913403693169672, -12.57945229203838267 ) ) ;
#36609 = CARTESIAN_POINT ( 'NONE',  ( 1.849999551004999798, 0.000000000000000000, -1.625000000000000000 ) ) ;
#36610 = CARTESIAN_POINT ( 'NONE',  ( 10.39503166480599994, 2.725152142215999884, 7.410114961806599787 ) ) ;
#36611 = CARTESIAN_POINT ( 'NONE',  ( 13.73125687463581102, -9.567603210565605920, -8.083310008166920468 ) ) ;
#36612 = CARTESIAN_POINT ( 'NONE',  ( 8.721010841230999233, 5.983047240001000411, 7.440798119034999658 ) ) ;
#36613 = ORIENTED_EDGE ( 'NONE', *, *, #58725, .T. ) ;
#36614 = CARTESIAN_POINT ( 'NONE',  ( 11.50001496185000249, 12.52499999999999680, -1.310230436094052653 ) ) ;
#36615 = EDGE_CURVE ( 'NONE', #24944, #68176, #1416, .T. ) ;
#36616 = ADVANCED_FACE ( 'NONE', ( #15844 ), #7779, .T. ) ;
#36617 = DIRECTION ( 'NONE',  ( 0.000000000000000000, 0.000000000000000000, 1.000000000000000000 ) ) ;
#36618 = CARTESIAN_POINT ( 'NONE',  ( 8.171101097212417841, -5.642366377685726242, 6.904702228779299844 ) ) ;
#36619 = CARTESIAN_POINT ( 'NONE',  ( 9.852013376692999813, -5.140392946802999852, 8.079558723821699928 ) ) ;
#36620 = ORIENTED_EDGE ( 'NONE', *, *, #37397, .T. ) ;
#36621 = CARTESIAN_POINT ( 'NONE',  ( 10.90000000346999975, -5.100000000044000892, -5.157071296039999808 ) ) ;
#36622 = B_SPLINE_CURVE_WITH_KNOTS ( 'NONE', 3,
 ( #60696, #1977, #2994, #29595, #50213 ),
 .UNSPECIFIED., .F., .F.,
 ( 4, 1, 4 ),
 ( 0.000000000000000000, 0.5000000000000000000, 1.000000000000000000 ),
 .UNSPECIFIED. ) ;
#36623 = CARTESIAN_POINT ( 'NONE',  ( 10.77195525820100031, -4.120672149427799802, 8.772302877803999976 ) ) ;
#36624 = VERTEX_POINT ( 'NONE', #19561 ) ;
#36625 = CARTESIAN_POINT ( 'NONE',  ( 10.10000000000000142, 0.000000000000000000, 0.000000000000000000 ) ) ;
#36626 = CARTESIAN_POINT ( 'NONE',  ( 25.60000000000000142, -3.623466631435000362, 13.52296156804999860 ) ) ;
#36627 = ORIENTED_EDGE ( 'NONE', *, *, #60554, .T. ) ;
#36628 = CARTESIAN_POINT ( 'NONE',  ( 18.14024860221783442, 0.2197089332467984102, -13.89766776387045866 ) ) ;
#36629 = CARTESIAN_POINT ( 'NONE',  ( 9.712899699504999873, -4.008306780893000187, -8.877926425468999128 ) ) ;
#36630 = CARTESIAN_POINT ( 'NONE',  ( 8.497235841230001085, 3.789127741898000057, -9.388182174781999123 ) ) ;
#36631 = CARTESIAN_POINT ( 'NONE',  ( 10.68546886766499959, 3.433493735705800187, -6.470713638631999665 ) ) ;
#36632 = CARTESIAN_POINT ( 'NONE',  ( 11.51790547754520055, -2.825704134258000266, 7.462730980357120458 ) ) ;
#36633 = CARTESIAN_POINT ( 'NONE',  ( 12.46386834215124928, 3.023758766561084332, -12.31399102038137450 ) ) ;
#36634 = CARTESIAN_POINT ( 'NONE',  ( 11.26841504065830080, -3.085489673376300424, 8.181880472491098288 ) ) ;
#36635 = CARTESIAN_POINT ( 'NONE',  ( 7.641204719590000138, 4.524487726177000013, 9.047753146378999745 ) ) ;
#36636 = EDGE_CURVE ( 'NONE', #58325, #44202, #31093, .T. ) ;
#36637 = ORIENTED_EDGE ( 'NONE', *, *, #50851, .T. ) ;
#36638 = CARTESIAN_POINT ( 'NONE',  ( 9.583513540183334456, 5.250000000000000888, -7.663624617374468428 ) ) ;
#36639 = CARTESIAN_POINT ( 'NONE',  ( 11.49200216175158396, -4.419830582853482071, -8.702070774814039567 ) ) ;
#36640 = CARTESIAN_POINT ( 'NONE',  ( 11.05574479014000211, -5.246314385833000138, 5.054138008665999493 ) ) ;
#36641 = ORIENTED_EDGE ( 'NONE', *, *, #22465, .F. ) ;
#36642 = CARTESIAN_POINT ( 'NONE',  ( 12.19425446308167515, -2.632875717725343012, -12.41961888770621236 ) ) ;
#36643 = CIRCLE ( 'NONE', #44446, 1.250000000000000000 ) ;
#36644 = DIRECTION ( 'NONE',  ( -1.000000000000000000, 0.000000000000000000, 0.000000000000000000 ) ) ;
#36645 = CARTESIAN_POINT ( 'NONE',  ( 17.80000000000000071, 13.72414332887999855, -50.50083396221000243 ) ) ;
#36646 = CARTESIAN_POINT ( 'NONE',  ( 8.975960865537832234, 2.874039072694928088, -7.646523491995670163 ) ) ;
#36647 = CARTESIAN_POINT ( 'NONE',  ( 12.47274432058964422, -1.970265487500629353, -13.77159998682697051 ) ) ;
#36648 = AXIS2_PLACEMENT_3D ( 'NONE', #39255, #37869, #17936 ) ;
#36649 = CARTESIAN_POINT ( 'NONE',  ( 11.46179707368349909, -4.498457171163099844, -6.629085939160999530 ) ) ;
#36650 = CARTESIAN_POINT ( 'NONE',  ( 18.01911383345317930, 3.562435417626197420, 12.00770609665305066 ) ) ;
#36652 = CARTESIAN_POINT ( 'NONE',  ( 17.95027792402082412, -3.083622039298903772, 12.21684579612696453 ) ) ;
#36651 = B_SPLINE_CURVE_WITH_KNOTS ( 'NONE', 3,
 ( #44100, #65399, #17518, #38847 ),
 .UNSPECIFIED., .F., .F.,
 ( 4, 4 ),
 ( 0.000000000000000000, 1.000000000000000000 ),
 .UNSPECIFIED. ) ;
#36654 = ORIENTED_EDGE ( 'NONE', *, *, #45969, .T. ) ;
#36653 = B_SPLINE_CURVE_WITH_KNOTS ( 'NONE', 3,
 ( #43472, #26704, #38210, #37870 ),
 .UNSPECIFIED., .F., .F.,
 ( 4, 4 ),
 ( 0.000000000000000000, 1.000000000000000000 ),
 .UNSPECIFIED. ) ;
#36655 = ORIENTED_EDGE ( 'NONE', *, *, #21208, .F. ) ;
#36656 = VECTOR ( 'NONE', #68589, 1000.000000000000000 ) ;
#36657 = CARTESIAN_POINT ( 'NONE',  ( 0.000000000000000000, 0.000000000000000000, 0.000000000000000000 ) ) ;
#36658 = DIRECTION ( 'NONE',  ( 0.000000000000000000, 1.000000000000000000, 0.000000000000000000 ) ) ;
#36659 = CARTESIAN_POINT ( 'NONE',  ( 5.500000000000000000, -0.2500000000000000000, 9.776630298829998011 ) ) ;
#36660 = CARTESIAN_POINT ( 'NONE',  ( 10.30296826955000000, 4.081263352980999848, -9.025008366823000117 ) ) ;
#36661 = CARTESIAN_POINT ( 'NONE',  ( 10.72303951155000057, -3.890113427500999421, -8.859339185702999941 ) ) ;
#36662 = EDGE_CURVE ( 'NONE', #49930, #65620, #34867, .T. ) ;
#36663 = CARTESIAN_POINT ( 'NONE',  ( 17.99149020822391165, 2.947405452019512317, 12.33598828993208585 ) ) ;
#36664 = CARTESIAN_POINT ( 'NONE',  ( 17.92307254476367007, -3.107335109273783758, -12.21089239123762660 ) ) ;
#36665 = AXIS2_PLACEMENT_3D ( 'NONE', #11760, #61643, #61992 ) ;
#36666 = ORIENTED_EDGE ( 'NONE', *, *, #18509, .T. ) ;
#36667 = EDGE_CURVE ( 'NONE', #49026, #3750, #26436, .T. ) ;
#36668 = CARTESIAN_POINT ( 'NONE',  ( 8.650504956611454688, -4.887017940256735749, -6.482196879590077288 ) ) ;
#36669 = ORIENTED_EDGE ( 'NONE', *, *, #15752, .F. ) ;
#36670 = CARTESIAN_POINT ( 'NONE',  ( 12.51684016020884549, -3.054675744551021754, 12.30488183412682801 ) ) ;
#36671 = CARTESIAN_POINT ( 'NONE',  ( 23.64973524161407425, -10.02113549012734417, -9.687121459438744253 ) ) ;
#36672 = CARTESIAN_POINT ( 'NONE',  ( 10.05691520198999989, 2.453477278391000382, 6.657104391228999773 ) ) ;
#36673 = CARTESIAN_POINT ( 'NONE',  ( 11.85034208742530026, -4.630634088820300143, 6.508707709313799050 ) ) ;
#36674 = DIRECTION ( 'NONE',  ( -1.000000000000000000, -0.000000000000000000, -0.000000000000000000 ) ) ;
#36675 = CARTESIAN_POINT ( 'NONE',  ( 10.90023029886999950, 9.364047981009999688, -6.155772864046999970 ) ) ;
#36676 = B_SPLINE_CURVE_WITH_KNOTS ( 'NONE', 3,
 ( #21838, #37574, #26764, #65172, #58558, #33381, #6795, #53666, #48074, #178 ),
 .UNSPECIFIED., .F., .F.,
 ( 4, 2, 2, 2, 4 ),
 ( 0.000000000000000000, 0.2499999999999997780, 0.4999999999999995559, 0.7499999999999997780, 1.000000000000000000 ),
 .UNSPECIFIED. ) ;
#36677 = CARTESIAN_POINT ( 'NONE',  ( 10.22272469555899832, 4.639546521693399761, -6.393520617113999549 ) ) ;
#36678 = CARTESIAN_POINT ( 'NONE',  ( 12.34842979604855095, -0.4268810874232081276, 12.69034564040269508 ) ) ;
#36679 = CARTESIAN_POINT ( 'NONE',  ( 5.592979883552142262, -12.14034187852487889, -3.752392258526793700 ) ) ;
#36680 = CARTESIAN_POINT ( 'NONE',  ( 9.758140238852000437, 2.901378080241999946, 6.555076849497999625 ) ) ;
#36681 = CARTESIAN_POINT ( 'NONE',  ( 9.092670730108844523, -4.128092163117982771, 8.851211507171084847 ) ) ;
#36682 = ORIENTED_EDGE ( 'NONE', *, *, #7882, .F. ) ;
#36683 = CARTESIAN_POINT ( 'NONE',  ( 9.278070280414000948, 2.546924812613000189, -6.918870225297999887 ) ) ;
#36684 = DIRECTION ( 'NONE',  ( 0.000000000000000000, -1.000000000000000000, 0.000000000000000000 ) ) ;
#36685 = DIRECTION ( 'NONE',  ( 0.000000000000000000, 0.001239076634196941687, -0.9999992323442525866 ) ) ;
#36686 = CARTESIAN_POINT ( 'NONE',  ( 9.125651434942099627, 5.349687154987381454, -7.676802464757987110 ) ) ;
#36687 = CARTESIAN_POINT ( 'NONE',  ( 10.10434687351566474, 5.250000000000001776, -7.336375382625535124 ) ) ;
#36688 = CARTESIAN_POINT ( 'NONE',  ( 10.96533729122639933, -5.140346530769000388, -7.470001566214039990 ) ) ;
#36689 = ORIENTED_EDGE ( 'NONE', *, *, #20203, .F. ) ;
#36690 = CARTESIAN_POINT ( 'NONE',  ( 8.736413463905998711, 4.084156314540369870, -8.382409559052598880 ) ) ;
#36691 = CARTESIAN_POINT ( 'NONE',  ( 6.799999045260999964, -9.295457794069999835, 5.399713664196000629 ) ) ;
#36692 = AXIS2_PLACEMENT_3D ( 'NONE', #8709, #8370, #13622 ) ;
#36695 = CARTESIAN_POINT ( 'NONE',  ( 13.67057712374000289, -9.352787036275000077, -8.106596622149000453 ) ) ;
#36694 = UNCERTAINTY_MEASURE_WITH_UNIT (LENGTH_MEASURE( 1.000000000000000082E-05 ), #64163, 'distance_accuracy_value', 'NONE');
#36693 = CARTESIAN_POINT ( 'NONE',  ( 8.871889158775999817, 2.702406276695999754, -6.981052078638000147 ) ) ;
#36696 = CARTESIAN_POINT ( 'NONE',  ( 18.13616101475819775, -2.730220173702290420, 13.62193317602436338 ) ) ;
#36697 = VERTEX_POINT ( 'NONE', #46475 ) ;
#36698 = CARTESIAN_POINT ( 'NONE',  ( 10.79500540879000070, 3.503955365545999623, 6.168588659884999714 ) ) ;
#36700 = CARTESIAN_POINT ( 'NONE',  ( 17.92067731499820482, -3.006998531728875435, -13.55270476886629361 ) ) ;
#36699 = AXIS2_PLACEMENT_3D ( 'NONE', #18045, #39362, #28891 ) ;
#36701 = CARTESIAN_POINT ( 'NONE',  ( 11.71210404293059959, 3.618181340822599790, 6.722495590581700320 ) ) ;
#36702 = CARTESIAN_POINT ( 'NONE',  ( 24.71770621865795192, -11.77375252400051231, 3.190797026286958271 ) ) ;
#36703 = CARTESIAN_POINT ( 'NONE',  ( 8.924956853209002006, -4.158911960977000000, 5.873536005760000123 ) ) ;
#36704 = ORIENTED_EDGE ( 'NONE', *, *, #4410, .F. ) ;
#36705 = CARTESIAN_POINT ( 'NONE',  ( 8.289114158772999730, 4.310355144869000732, 9.459505265942000918 ) ) ;
#36706 = ADVANCED_FACE ( 'NONE', ( #19903 ), #20243, .F. ) ;
#36707 = EDGE_CURVE ( 'NONE', #5489, #62147, #14997, .T. ) ;
#36709 = FACE_OUTER_BOUND ( 'NONE', #43785, .T. ) ;
#36708 = CARTESIAN_POINT ( 'NONE',  ( 13.69992376746900042, 12.26631831379999937, 2.532779022035999805 ) ) ;
#36710 = CARTESIAN_POINT ( 'NONE',  ( 7.533751553497644693, -3.156652531865319133, 5.968239819955745595 ) ) ;
#36711 = DIRECTION ( 'NONE',  ( 0.000000000000000000, -0.1807154286440004198, -0.9835354258236025382 ) ) ;
#36712 = CARTESIAN_POINT ( 'NONE',  ( 23.91242875217100305, 3.265460742156999885, 12.84041179270000121 ) ) ;
#36713 = EDGE_LOOP ( 'NONE', ( #24052, #46723, #8208, #50824 ) ) ;
#36714 = FACE_OUTER_BOUND ( 'NONE', #59327, .T. ) ;
#36715 = CARTESIAN_POINT ( 'NONE',  ( 11.93718179236249988, -4.209680326224799707, 8.481317998227099864 ) ) ;
#36716 = CARTESIAN_POINT ( 'NONE',  ( 10.40227026081000083, 2.765684886876999649, 9.035354958280999327 ) ) ;
#36717 = CARTESIAN_POINT ( 'NONE',  ( 10.94796973825000030, 2.864322365205000054, 8.846249469408000721 ) ) ;
#36718 = CARTESIAN_POINT ( 'NONE',  ( 11.53148876160955005, 3.209326035813000022, 6.677731919207799294 ) ) ;
#36719 = ORIENTED_EDGE ( 'NONE', *, *, #51140, .T. ) ;
#36720 = B_SPLINE_SURFACE_WITH_KNOTS ( 'NONE', 3, 3, ( 
 ( #51042, #23087, #60844, #12260, #38828, #34633, #49660, #66771, #56290, #8394, #55945, #7009, #2798, #1769, #17855, #12956, #50010, #29739, #23437, #18197, #13645, #7351, #44776, #13311, #66423, #33589, #24472, #50355, #24124, #3143, #29391, #45459, #18544, #28341, #65732 ),
 ( #18889, #39519, #66076, #7706, #40214, #34972, #39173, #60496, #2455, #12605, #34283, #28696, #55604, #23780, #39871, #14333, #9406, #62213, #68134, #35656, #19913, #25153, #52754, #46829, #35985, #46485, #40891, #20252, #25842, #67447, #63229, #41578, #36333, #56970, #25499 ),
 ( #47170, #30409, #4849, #62886, #9071, #67792, #19218, #47516, #51721, #19569, #15007, #14672, #20595, #24815, #57303, #3816, #30749, #57648, #36683, #9754, #58004, #41238, #31102, #52408, #52057, #4501, #35314, #62549, #4161, #68473, #41920, #26193, #15357, #10103, #31438 ),
 ( #40544, #61869, #13988, #56632, #8735, #30080, #51380, #3479, #46141, #20945, #33159, #22309, #48893, #32811, #58339, #37362, #21281, #42611, #63921, #58684, #43650, #47864, #10442, #16714, #31782, #15696, #54476, #54126, #10788, #5198, #38045, #17061, #27917, #63581, #38393 ) ),
 .UNSPECIFIED., .F., .F., .F.,
 ( 4, 4 ),
 ( 4, 1, 1, 1, 1, 1, 1, 1, 1, 1, 1, 1, 1, 1, 1, 1, 1, 1, 1, 1, 1, 1, 1, 1, 1, 1, 1, 1, 1, 1, 1, 1, 4 ),
 ( -0.1039370721279000015, 1.103937072127999963 ),
 ( -0.02000000000000000042, 0.01250000000000000069, 0.04499999999999999833, 0.07749999999999999944, 0.1100000000000000006, 0.1424999999999999878, 0.1749999999999999889, 0.2074999999999999900, 0.2399999999999999911, 0.2725000000000000200, 0.3049999999999999933, 0.3375000000000000222, 0.3699999999999999956, 0.4025000000000000244, 0.4349999999999999978, 0.4675000000000000266, 0.5000000000000000000, 0.5324999999999999734, 0.5649999999999999467, 0.5975000000000000311, 0.6300000000000000044, 0.6624999999999999778, 0.6949999999999999512, 0.7275000000000000355, 0.7600000000000000089, 0.7924999999999999822, 0.8249999999999999556, 0.8575000000000000400, 0.8900000000000000133, 0.9224999999999999867, 0.9549999999999999600, 0.9875000000000000444, 1.020000000000000018 ),
 .UNSPECIFIED. ) ;
#36721 = DIRECTION ( 'NONE',  ( 0.000000000000000000, -1.000000000000000000, 0.000000000000000000 ) ) ;
#36722 = CARTESIAN_POINT ( 'NONE',  ( 12.54704051454017133, 1.807816716204553087, -12.46963574575698352 ) ) ;
#36723 = CARTESIAN_POINT ( 'NONE',  ( 11.37299956498129916, 2.792989229543000107, -7.174999999999999822 ) ) ;
#36724 = EDGE_CURVE ( 'NONE', #5569, #49580, #25685, .T. ) ;
#36725 = CARTESIAN_POINT ( 'NONE',  ( 24.87547482180800174, -2.962908632962999889, -11.62664876782000078 ) ) ;
#36726 = CARTESIAN_POINT ( 'NONE',  ( 17.72088406261403648, -1.806772466812839983, 13.88292461265716504 ) ) ;
#36727 = CARTESIAN_POINT ( 'NONE',  ( 18.14647333857621092, 2.702177529323569694, -13.62849908386765208 ) ) ;
#36728 = ORIENTED_EDGE ( 'NONE', *, *, #35239, .F. ) ;
#36729 = DIRECTION ( 'NONE',  ( 0.000000000000000000, 0.8514543052404082157, -0.5244287998266055073 ) ) ;
#36730 = DIRECTION ( 'NONE',  ( 1.000000000000000000, 0.000000000000000000, 0.000000000000000000 ) ) ;
#36731 = EDGE_LOOP ( 'NONE', ( #44177, #21216, #53653, #16586 ) ) ;
#36732 = CARTESIAN_POINT ( 'NONE',  ( 24.30000000000000071, -12.03537377768999939, 3.224868684338999980 ) ) ;
#36733 = CARTESIAN_POINT ( 'NONE',  ( 11.76133460557259980, 4.139849081322200419, 6.645166161828299778 ) ) ;
#36734 = CARTESIAN_POINT ( 'NONE',  ( 10.97864812944000157, 5.273131703456000352, 7.958028903907000462 ) ) ;
#36735 = CARTESIAN_POINT ( 'NONE',  ( 9.856715971886000460, 4.814120192353000149, -8.929574926876000518 ) ) ;
#36736 = CARTESIAN_POINT ( 'NONE',  ( 7.613778970466999141, 4.858908887722000358, 6.437635593844006188 ) ) ;
#36737 = CARTESIAN_POINT ( 'NONE',  ( 10.27968096967000022, -5.739708848514999850, 7.774962785835000112 ) ) ;
#36738 = CARTESIAN_POINT ( 'NONE',  ( 18.02437627528318131, -0.5483668826291703269, -12.58806376549905082 ) ) ;
#36739 = CARTESIAN_POINT ( 'NONE',  ( 12.27931543958120209, 2.838108479058770506, -12.36635919027451180 ) ) ;
#36740 = B_SPLINE_CURVE_WITH_KNOTS ( 'NONE', 3,
 ( #68554, #15088, #36412, #37103 ),
 .UNSPECIFIED., .F., .F.,
 ( 4, 4 ),
 ( 0.000000000000000000, 1.000000000000000000 ),
 .UNSPECIFIED. ) ;
#36741 = CARTESIAN_POINT ( 'NONE',  ( 10.69872335273220010, -3.650693637952500126, -8.440710326446700051 ) ) ;
#36742 = CARTESIAN_POINT ( 'NONE',  ( 9.202760841230999134, 2.542862824481000317, 7.419808961972999661 ) ) ;
#36743 = ORIENTED_EDGE ( 'NONE', *, *, #66836, .T. ) ;
#36744 = FACE_OUTER_BOUND ( 'NONE', #22002, .T. ) ;
#36745 = FACE_OUTER_BOUND ( 'NONE', #44443, .T. ) ;
#36746 = CARTESIAN_POINT ( 'NONE',  ( 7.000000000000000000, -6.255435840762999966, 3.000000000000000000 ) ) ;
#36747 = CARTESIAN_POINT ( 'NONE',  ( 11.31510034929000241, 9.451872599583003520, 6.816406955572995585 ) ) ;
#36748 = CARTESIAN_POINT ( 'NONE',  ( 12.63921101284453741, 1.806754227364035126, 13.88292698645336642 ) ) ;
#36749 = CARTESIAN_POINT ( 'NONE',  ( 13.69997185827400266, 11.40547114375999982, 2.374390024598000082 ) ) ;
#36750 = VECTOR ( 'NONE', #43219, 1000.000000000000000 ) ;
#36751 = EDGE_CURVE ( 'NONE', #4423, #3413, #27554, .T. ) ;
#36752 = LINE ( 'NONE', #20665, #52667 ) ;
#36753 = CARTESIAN_POINT ( 'NONE',  ( 12.42222097287479698, -0.6205713442106928213, 13.98624562867391496 ) ) ;
#36754 = VERTEX_POINT ( 'NONE', #643 ) ;
#36755 = CARTESIAN_POINT ( 'NONE',  ( 24.36809152945900081, 8.862862741694000235, 8.808753452432000586 ) ) ;
#36756 = CARTESIAN_POINT ( 'NONE',  ( 10.36624205625100004, -4.409476560233800413, -8.565862728991998409 ) ) ;
#36757 = CARTESIAN_POINT ( 'NONE',  ( 13.00000000001300116, 11.52577654661000039, 1.696746661728000038 ) ) ;
#36758 = CARTESIAN_POINT ( 'NONE',  ( 10.87021507563000000, -2.226042145532000305, 7.782753277595999997 ) ) ;
#36759 = CARTESIAN_POINT ( 'NONE',  ( 11.89210538575740017, -3.157545584346100220, 7.701417844014099678 ) ) ;
#36760 = CARTESIAN_POINT ( 'NONE',  ( 8.734020077949999461, 3.936452720224709712, 6.621188087644399367 ) ) ;
#36761 = CARTESIAN_POINT ( 'NONE',  ( 7.790635841228000125, 3.416213390569000197, 6.162512717529000206 ) ) ;
#36762 = CARTESIAN_POINT ( 'NONE',  ( 18.40015514469800095, 2.597921877622999464E-14, 2.051692149506999743E-13 ) ) ;
#36763 = CARTESIAN_POINT ( 'NONE',  ( 12.14402373937349289, 2.776896049134141009, 12.29021278449864418 ) ) ;
#36764 = CARTESIAN_POINT ( 'NONE',  ( 9.443897997121000643, -4.993413662857000723, -9.088148847710000311 ) ) ;
#36765 = CARTESIAN_POINT ( 'NONE',  ( 11.11718313518939816, 3.377550038693600154, -8.287087605365499599 ) ) ;
#36766 = CARTESIAN_POINT ( 'NONE',  ( 12.44187590071328131, 11.55958658085554980, -4.822001495576104801 ) ) ;
#36767 = CARTESIAN_POINT ( 'NONE',  ( 9.991525552923999243, 4.805950298207000593, -8.932431532051998246 ) ) ;
#36768 = CARTESIAN_POINT ( 'NONE',  ( 8.619480666858999385, 4.380700808321400075, -8.576476893896000320 ) ) ;
#36770 = CARTESIAN_POINT ( 'NONE',  ( 17.80000000005199823, 3.345268251980999974, -11.86064071431999878 ) ) ;
#36769 = CARTESIAN_POINT ( 'NONE',  ( 18.21067574918971843, -11.77411897367713323, 3.633863173939181568 ) ) ;
#36771 = PLANE ( 'NONE',  #5099 ) ;
#36772 = VERTEX_POINT ( 'NONE', #16367 ) ;
#36773 = CARTESIAN_POINT ( 'NONE',  ( 12.42592538302026206, 0.4969854667031534667, 12.68691056894229874 ) ) ;
#36774 = CARTESIAN_POINT ( 'NONE',  ( 7.744950122392999958, 2.855953552844000320, 6.776551829089000556 ) ) ;
#36775 = CARTESIAN_POINT ( 'NONE',  ( 9.882266086202999844, -4.932716797830999589, 6.390980246320999925 ) ) ;
#36776 = CARTESIAN_POINT ( 'NONE',  ( 9.526355082327999213, 3.611978631017199959, 8.275336934318801241 ) ) ;
#36777 = DIRECTION ( 'NONE',  ( 0.7071066261840305289, 0.7071069361890305327, -2.950954976001128386E-10 ) ) ;
#36778 = CARTESIAN_POINT ( 'NONE',  ( 12.32580140628885879, -2.098690126660240463, 13.75042779764526912 ) ) ;
#36779 = CARTESIAN_POINT ( 'NONE',  ( 7.000000000000000000, -9.370210309074998634, -5.370210309075000410 ) ) ;
#36780 = CARTESIAN_POINT ( 'NONE',  ( 23.61702258298599943, 2.916534779610000072, -13.53539279049999955 ) ) ;
#36781 = ORIENTED_EDGE ( 'NONE', *, *, #49273, .F. ) ;
#36782 = EDGE_CURVE ( 'NONE', #21554, #43226, #9835, .T. ) ;
#36784 = EDGE_CURVE ( 'NONE', #51368, #67585, #48418, .T. ) ;
#36783 = B_SPLINE_CURVE_WITH_KNOTS ( 'NONE', 3,
 ( #2317, #1980, #33103, #33450 ),
 .UNSPECIFIED., .F., .F.,
 ( 4, 4 ),
 ( 0.000000000000000000, 1.000000000000000000 ),
 .UNSPECIFIED. ) ;
#36785 = CARTESIAN_POINT ( 'NONE',  ( 5.071677236438000058, 1.133895819062999966, -0.03443813753193999960 ) ) ;
#36786 = CARTESIAN_POINT ( 'NONE',  ( 9.301355082327999568, -4.572497688003699601, -6.356045986629998978 ) ) ;
#36787 = CARTESIAN_POINT ( 'NONE',  ( 25.37954957502917708, 3.026737125307685350, 11.38060389463865363 ) ) ;
#36789 = B_SPLINE_CURVE_WITH_KNOTS ( 'NONE', 3,
 ( #20782, #5724, #145, #53288, #20096, #36516, #31624, #10979, #69015, #32318, #30937, #52253, #4349, #20437, #25681, #42455 ),
 .UNSPECIFIED., .F., .F.,
 ( 4, 2, 2, 2, 2, 2, 2, 4 ),
 ( 0.000000000000000000, 0.06249999999999757139, 0.1249999999999951428, 0.2499999999999946154, 0.4999999999999963363, 0.7499999999999981126, 0.8749999999999991118, 1.000000000000000000 ),
 .UNSPECIFIED. ) ;
#36788 = CARTESIAN_POINT ( 'NONE',  ( 10.94125056272499918, -2.966599088466999934, 7.484684486284700178 ) ) ;
#36790 = CARTESIAN_POINT ( 'NONE',  ( 18.06416738895848795, 2.863102795628076347, -12.35955380825000915 ) ) ;
#36791 = CARTESIAN_POINT ( 'NONE',  ( 8.581715799613704121, 5.025392983842594141, 6.195064399343296557 ) ) ;
#36792 = CARTESIAN_POINT ( 'NONE',  ( 17.92143259511064457, 3.006721712956350601, 12.31894844866651439 ) ) ;
#36793 = B_SPLINE_CURVE_WITH_KNOTS ( 'NONE', 3,
 ( #44801, #29420, #22764, #29073, #13335, #28026, #34659, #44465, #24153, #18223, #45486, #7730, #17531, #38861, #50383, #65410, #23808, #33270 ),
 .UNSPECIFIED., .F., .F.,
 ( 4, 2, 2, 2, 2, 2, 2, 2, 4 ),
 ( 0.000000000000000000, 0.1250000000000000278, 0.2500000000000000555, 0.3749999999999999445, 0.4999999999999999445, 0.6249999999999998890, 0.7499999999999998890, 0.8750000000000000000, 1.000000000000000000 ),
 .UNSPECIFIED. ) ;
#36794 = CARTESIAN_POINT ( 'NONE',  ( 18.00298204928587253, 3.099842930792937157, 13.65268125597837212 ) ) ;
#36795 = CARTESIAN_POINT ( 'NONE',  ( 9.619904806657000762, -2.133039813254999917, -7.346564890486999566 ) ) ;
#36796 = CARTESIAN_POINT ( 'NONE',  ( 10.11549555961999936, -2.489199523559999960, -6.434642413229999747 ) ) ;
#36797 = CARTESIAN_POINT ( 'NONE',  ( 9.225036466121004253, 2.649952287134117235, 7.500002258928285315 ) ) ;
#36798 = CARTESIAN_POINT ( 'NONE',  ( 18.30003129334700063, 2.732683817159999862, -11.53064095410000078 ) ) ;
#36799 = CARTESIAN_POINT ( 'NONE',  ( 23.79452173965752948, 9.731929379560703808, -9.426968994335380714 ) ) ;
#36800 = LINE ( 'NONE', #41010, #13068 ) ;
#36801 = DIRECTION ( 'NONE',  ( -1.000000000000000000, 0.000000000000000000, -3.164702532202999971E-14 ) ) ;
#36802 = EDGE_CURVE ( 'NONE', #42751, #24606, #3156, .T. ) ;
#36803 = ORIENTED_EDGE ( 'NONE', *, *, #62270, .F. ) ;
#36804 = CARTESIAN_POINT ( 'NONE',  ( 8.754720280412998434, 5.687930027805999877, -7.109876198051000351 ) ) ;
#36805 = CARTESIAN_POINT ( 'NONE',  ( 11.96179707368349909, -4.498457171163099844, 8.370914060838998694 ) ) ;
#36806 = ORIENTED_EDGE ( 'NONE', *, *, #23214, .T. ) ;
#36807 = B_SPLINE_CURVE_WITH_KNOTS ( 'NONE', 3,
 ( #60374, #44658, #35193, #66985, #50919, #39397, #3358, #29616, #40420, #50231, #65950, #23654 ),
 .UNSPECIFIED., .F., .F.,
 ( 4, 2, 2, 2, 2, 4 ),
 ( 0.000000000000000000, 0.2499999999999754641, 0.3749999999999631961, 0.4374999999999594213, 0.4999999999999557021, 1.000000000000000000 ),
 .UNSPECIFIED. ) ;
#36808 = DIRECTION ( 'NONE',  ( -0.000000000000000000, -0.000000000000000000, 1.000000000000000000 ) ) ;
#36809 = CARTESIAN_POINT ( 'NONE',  ( 11.21149010443640037, -2.862435565199000109, -7.585072163144589652 ) ) ;
#36810 = ORIENTED_EDGE ( 'NONE', *, *, #32610, .T. ) ;
#36811 = ADVANCED_FACE ( 'NONE', ( #49218 ), #66386, .F. ) ;
#36812 = CARTESIAN_POINT ( 'NONE',  ( 11.59966954483535773, 4.638989336656000440, 8.485927942460499196 ) ) ;
#36813 = CARTESIAN_POINT ( 'NONE',  ( 18.02331223755004785, 3.318306765095501820, -11.16743751352750991 ) ) ;
#36814 = CARTESIAN_POINT ( 'NONE',  ( 17.60000000000000142, 52.95171880992000268, -18.02623547589999831 ) ) ;
#36815 = CARTESIAN_POINT ( 'NONE',  ( 11.52677869730533011, -4.403502086956500250, -6.704332466833498927 ) ) ;
#36816 = CARTESIAN_POINT ( 'NONE',  ( 12.44874774236670945, 0.5136130429597132174, -13.88722741725625021 ) ) ;
#36817 = CARTESIAN_POINT ( 'NONE',  ( 7.100652037295501096, 1.104751383945007825, 0.2933445679723732380 ) ) ;
#36818 = CARTESIAN_POINT ( 'NONE',  ( 10.90000000000000036, -1.300000000000000044, -9.662944685757000940 ) ) ;
#36819 = ORIENTED_EDGE ( 'NONE', *, *, #36951, .F. ) ;
#36820 = CARTESIAN_POINT ( 'NONE',  ( 25.29987931604000195, 11.13052921044000065, -3.427478701325000099 ) ) ;
#36821 = CARTESIAN_POINT ( 'NONE',  ( 9.178620280414001797, 2.990001567622999623, -8.695425648791999862 ) ) ;
#36822 = VERTEX_POINT ( 'NONE', #37352 ) ;
#36823 = AXIS2_PLACEMENT_3D ( 'NONE', #16225, #25688, #62737 ) ;
#36824 = CARTESIAN_POINT ( 'NONE',  ( 10.43284001513000092, 3.279325423736999756, -9.029279369994000604 ) ) ;
#36825 =( NAMED_UNIT ( * ) PLANE_ANGLE_UNIT ( ) SI_UNIT ( $, .RADIAN. ) );
#36826 = ORIENTED_EDGE ( 'NONE', *, *, #68833, .F. ) ;
#36827 = CARTESIAN_POINT ( 'NONE',  ( 11.79999999550100220, -11.52577121388000059, -1.696750555870000010 ) ) ;
#36828 = CARTESIAN_POINT ( 'NONE',  ( 18.03321709926674998, -2.902596714178123261, -12.34859794581418413 ) ) ;
#36829 = DIRECTION ( 'NONE',  ( 0.000000000000000000, 0.9905022095861402143, 0.1374968101629056305 ) ) ;
#36830 = DIRECTION ( 'NONE',  ( 0.000000000000000000, 1.000000000000000000, 0.000000000000000000 ) ) ;
#36831 = CARTESIAN_POINT ( 'NONE',  ( 13.55377458794190737, -8.990344585381047082, -7.716059257659925841 ) ) ;
#36832 = ORIENTED_EDGE ( 'NONE', *, *, #49045, .F. ) ;
#36833 = CARTESIAN_POINT ( 'NONE',  ( 12.82792991967100171, 11.81434786598999942, -3.324782598720999793 ) ) ;
#36834 = CARTESIAN_POINT ( 'NONE',  ( 7.100000000000000533, -12.03770622561999915, 3.722046322334000124 ) ) ;
#36835 = CARTESIAN_POINT ( 'NONE',  ( 25.60000000000000142, 0.000000000000000000, 0.000000000000000000 ) ) ;
#36836 = CARTESIAN_POINT ( 'NONE',  ( 10.33253786428999987, 2.899999999999999911, 6.571291218949999902 ) ) ;
#36837 = CARTESIAN_POINT ( 'NONE',  ( 9.096889158776001238, 2.235961884443999459, -6.794506518623999902 ) ) ;
#36838 = CARTESIAN_POINT ( 'NONE',  ( 17.87620400591499958, -3.527529948368999690, 11.96092454128000071 ) ) ;
#36839 = CARTESIAN_POINT ( 'NONE',  ( 10.48735240295000004, -4.351290250877999810, -6.182246784057000788 ) ) ;
#36840 = EDGE_CURVE ( 'NONE', #46556, #11525, #16391, .T. ) ;
#36841 = ADVANCED_FACE ( 'NONE', ( #34875 ), #23920, .F. ) ;
#36842 = ORIENTED_EDGE ( 'NONE', *, *, #45626, .T. ) ;
#36843 = VERTEX_POINT ( 'NONE', #45708 ) ;
#36844 = CARTESIAN_POINT ( 'NONE',  ( 11.09999999999999964, 5.350000000000000533, -7.500000000000000000 ) ) ;
#36845 = PLANE ( 'NONE',  #49979 ) ;
#36846 = CARTESIAN_POINT ( 'NONE',  ( 0.1499942179679999987, -2.750000000000000000, 0.000000000000000000 ) ) ;
#36847 = CARTESIAN_POINT ( 'NONE',  ( 6.084193173016664957, -1.460959015002474937, 0.3926218265389144757 ) ) ;
#36848 = CARTESIAN_POINT ( 'NONE',  ( 11.64122412107036908, 4.062069863985690255, -6.326756392227999015 ) ) ;
#36849 = CARTESIAN_POINT ( 'NONE',  ( 8.775480666858998191, 4.289077172771600388, -8.317400147935998689 ) ) ;
#36851 = FACE_OUTER_BOUND ( 'NONE', #4427, .T. ) ;
#36850 = CARTESIAN_POINT ( 'NONE',  ( 9.800405316139999101, -4.213249376011100722, 6.518487389810699639 ) ) ;
#36852 = CARTESIAN_POINT ( 'NONE',  ( 4.732109839683332986, 0.9218200799623741393, -1.199500263597268690 ) ) ;
#36853 = ORIENTED_EDGE ( 'NONE', *, *, #29876, .F. ) ;
#36854 = DIRECTION ( 'NONE',  ( -1.000000000000000000, 0.000000000000000000, 0.000000000000000000 ) ) ;
#36855 = CARTESIAN_POINT ( 'NONE',  ( 8.500486250726996929, -2.902641158998001458, 6.605591905707999700 ) ) ;
#36856 = CARTESIAN_POINT ( 'NONE',  ( 9.456405316140999773, 3.728406863338599830, 6.249951378708000327 ) ) ;
#36857 = CARTESIAN_POINT ( 'NONE',  ( 5.500000000000000000, -12.87590651766999983, 2.791353855799999728 ) ) ;
#36858 = CARTESIAN_POINT ( 'NONE',  ( 10.18755811987000115, -5.387486580809999204, 8.640943191857999750 ) ) ;
#36859 = CARTESIAN_POINT ( 'NONE',  ( 18.06426550929511166, 2.862542805010156233, -12.35969564690516975 ) ) ;
#36860 = CARTESIAN_POINT ( 'NONE',  ( 16.43176826122700263, -3.316188843241000050, -11.22344245815999919 ) ) ;
#36861 = EDGE_CURVE ( 'NONE', #4517, #39722, #59730, .T. ) ;
#36862 = ADVANCED_FACE ( 'NONE', ( #56193 ), #50260, .F. ) ;
#36863 = CARTESIAN_POINT ( 'NONE',  ( 14.04832727683000115, 8.838110522795000534, 7.948685794524999793 ) ) ;
#36864 = AXIS2_PLACEMENT_3D ( 'NONE', #52453, #36730, #5245 ) ;
#36865 = CARTESIAN_POINT ( 'NONE',  ( 7.935762780894745738, 2.895074738935549341, -6.665507318599334319 ) ) ;
#36866 = CARTESIAN_POINT ( 'NONE',  ( 8.800809814040999157, -3.469640109842400122, -8.185876144228299012 ) ) ;
#36867 = EDGE_CURVE ( 'NONE', #42419, #26260, #68890, .T. ) ;
#36868 = CARTESIAN_POINT ( 'NONE',  ( 17.60000001287599858, 11.53033693765999779, -4.891431908114999949 ) ) ;
#36869 = B_SPLINE_SURFACE_WITH_KNOTS ( 'NONE', 3, 3, ( 
 ( #66741, #56942, #13958, #55919, #61840, #40858, #30379, #8023, #51687, #39840, #3113, #35629, #3785, #25123, #2772, #9038, #66049, #61162, #34944, #46109, #18859, #8367, #24099, #67415, #18170, #13280, #19540, #29711, #39492, #14302, #60814, #12927, #34606, #29360, #50673, #19881, #15323, #67755, #47485, #68101, #31406, #25464, #46456, #20562, #15666, #41209, #47141, #20218, #5514, #69143, #31753, #10411, #68791, #41545, #26503, #58309, #41889, #36297, #16002, #62519, #14638, #4128, #63888, #42246, #37331, #9720, #20908 ),
 ( #10756, #57617, #53071, #63194, #46797, #9371, #21251, #5170, #35956, #47834, #57972, #63551, #57270, #68442, #36649, #14974, #30716, #42580, #52026, #58655, #32100, #31069, #62856, #52375, #10070, #36995, #53417, #4470, #25808, #52721, #4818, #26160, #28226, #48861, #273, #64230, #6546, #64577, #37675, #21587, #59005, #16687, #38716, #54445, #65272, #42925, #17386, #27194, #22622, #22282, #60035, #54097, #64917, #6193, #11442, #38015, #12148, #11105, #1307, #32440, #16347, #53756, #970, #11790, #43966, #49541, #59340 ),
 ( #48513, #26855, #33476, #32783, #48168, #5853, #622, #54791, #43623, #21931, #43269, #6890, #27536, #17031, #59689, #33130, #38364, #27888, #49200, #32591, #47982, #36809, #84, #37483, #11592, #37148, #59150, #64039, #26316, #10229, #22087, #11253, #6348, #53905, #58810, #43073, #58128, #21401, #42735, #15818, #31564, #772, #52883, #43432, #64726, #31910, #4982, #47644, #10914, #48320, #6005, #425, #37828, #42398, #16160, #26666, #54246, #32258, #20722, #68954, #27345, #53224, #21067, #42050, #63705, #5324, #16842 ),
 ( #48667, #58465, #38164, #53567, #59494, #5662, #27003, #21741, #64380, #16501, #32935, #10571, #47298, #68602, #15483, #63355, #60541, #2162, #55646, #55987, #54950, #2496, #44128, #60885, #65068, #23130, #55298, #7393, #33285, #18240, #28739, #23821, #45158, #33977, #50055, #65426, #49348, #50396, #28387, #23478, #39914, #27696, #66120, #54601, #17188, #49012, #44817, #38519, #7746, #22432, #66464, #39215, #18586, #39561, #61232, #59840, #11947, #6699, #28040, #1463, #13001, #34327, #22778, #1119, #43774, #17548, #13348 ) ),
 .UNSPECIFIED., .F., .F., .F.,
 ( 4, 4 ),
 ( 4, 1, 1, 1, 1, 1, 1, 1, 1, 1, 1, 1, 1, 1, 1, 1, 1, 1, 1, 1, 1, 1, 1, 1, 1, 1, 1, 1, 1, 1, 1, 1, 1, 1, 1, 1, 1, 1, 1, 1, 1, 1, 1, 1, 1, 1, 1, 1, 1, 1, 1, 1, 1, 1, 1, 1, 1, 1, 1, 1, 1, 1, 1, 1, 4 ),
 ( -0.02000000000000000042, 1.020000000000000018 ),
 ( 0.008747244164287000176, 0.02453926110774999961, 0.04033127805120999970, 0.05612329499467000327, 0.07191531193812999989, 0.08770732888158999652, 0.1034993458251000087, 0.1192913627684999978, 0.1350833797120000179, 0.1508753966553999792, 0.1666674135988999994, 0.1824594305423999918, 0.1982514474858000086, 0.2140434644293000011, 0.2298354813727000179, 0.2456274983162000103, 0.2614195152596999749, 0.2772115322030999640, 0.2930035491465999842, 0.3087955660900000288, 0.3245875830334999934, 0.3403795999769999581, 0.3561716169204000026, 0.3719636338639000228, 0.3877556508073999875, 0.4035476677507999765, 0.4193396846942999967, 0.4351317016376999858, 0.4509237185811999504, 0.4667157355247000261, 0.4825077524681000152, 0.4982997694115999798, 0.5140917863550000799, 0.5298838032985000446, 0.5456758202420000092, 0.5614678371854000538, 0.5772598541289000185, 0.5930518710723000630, 0.6088438880158000277, 0.6246359049592999924, 0.6404279219027000369, 0.6562199388462000016, 0.6720119557896999662, 0.6878039727331000108, 0.7035959896765999755, 0.7193880066200000201, 0.7351800235634999847, 0.7509720405069999494, 0.7667640574504001050, 0.7825560743939000696, 0.7983480913373000032, 0.8141401082808000789, 0.8299321252243000435, 0.8457241421676999771, 0.8615161591112000528, 0.8773081760545999863, 0.8931001929981000620, 0.9088922099416000266, 0.9246842268849999602, 0.9404762438285000359, 0.9562682607720000005, 0.9720602777153999341, 0.9878522946589000098, 1.003644311601999961, 1.019436328545999970 ),
 .UNSPECIFIED. ) ;
#36870 = CARTESIAN_POINT ( 'NONE',  ( 10.31498017945871126, -2.650031506806249659, -7.499998780888571304 ) ) ;
#36871 = CARTESIAN_POINT ( 'NONE',  ( 5.684131419941360619, 13.00367204040951385, -2.123909547228391759 ) ) ;
#36872 = CARTESIAN_POINT ( 'NONE',  ( 29.60000000000000142, 0.000000000000000000, 0.000000000000000000 ) ) ;
#36873 = ORIENTED_EDGE ( 'NONE', *, *, #52271, .F. ) ;
#36874 = CARTESIAN_POINT ( 'NONE',  ( 12.18028569061553057, 0.01996654564806132556, -12.69998441237379971 ) ) ;
#36875 = CARTESIAN_POINT ( 'NONE',  ( 8.241912900173000267, -4.599999999999999645, 6.117539782833000928 ) ) ;
#36876 = CARTESIAN_POINT ( 'NONE',  ( 5.440293061358000060, -12.88483958404999896, 2.133988467673999967 ) ) ;
#36877 = CARTESIAN_POINT ( 'NONE',  ( 24.72545694048200104, 3.605123969772000336, -12.13009300416999992 ) ) ;
#36878 = CARTESIAN_POINT ( 'NONE',  ( 9.317462135714000837, 5.100000000000000533, 6.571291218949999902 ) ) ;
#36879 = ORIENTED_EDGE ( 'NONE', *, *, #39533, .T. ) ;
#36880 = CARTESIAN_POINT ( 'NONE',  ( 0.7000000000000000666, -1.154700538379000108, 0.000000000000000000 ) ) ;
#36881 = CARTESIAN_POINT ( 'NONE',  ( 10.56080513895999928, -2.973119161490000106, -6.929150654994399083 ) ) ;
#36882 = CARTESIAN_POINT ( 'NONE',  ( 18.06967961654933674, 0.3547743933919684789, 12.69333341030383444 ) ) ;
#36883 = DIRECTION ( 'NONE',  ( 1.000000000000000000, 0.000000000000000000, 0.000000000000000000 ) ) ;
#36884 = CARTESIAN_POINT ( 'NONE',  ( 11.02755399909320566, 4.133346405062087392, -8.778526265510098625 ) ) ;
#36885 = CARTESIAN_POINT ( 'NONE',  ( 11.23589666366019912, 3.960399224793059947, -8.391246537305399045 ) ) ;
#36886 = ORIENTED_EDGE ( 'NONE', *, *, #41995, .T. ) ;
#36887 = CARTESIAN_POINT ( 'NONE',  ( 10.89228096335999929, -3.998355205482000851, 9.261304730013998565 ) ) ;
#36888 = CARTESIAN_POINT ( 'NONE',  ( 8.741501215035997419, -4.228777700933000538, -8.375893644236599656 ) ) ;
#36890 = ORIENTED_EDGE ( 'NONE', *, *, #22746, .T. ) ;
#36889 = B_SPLINE_CURVE_WITH_KNOTS ( 'NONE', 3,
 ( #30665, #68390, #41836, #57219, #45716, #19135 ),
 .UNSPECIFIED., .F., .F.,
 ( 4, 2, 4 ),
 ( 0.000000000000000000, 0.5000000000000000000, 1.000000000000000000 ),
 .UNSPECIFIED. ) ;
#36891 = ADVANCED_FACE ( 'NONE', ( #7608 ), #12860, .T. ) ;
#36892 = CARTESIAN_POINT ( 'NONE',  ( 6.953073139469000630, -9.233001678504999532, 5.200628701625999994 ) ) ;
#36893 = CARTESIAN_POINT ( 'NONE',  ( 7.326308059621999824, -3.394845988290999816, 9.388942682504000103 ) ) ;
#36894 = LINE ( 'NONE', #168, #41150 ) ;
#36895 = ORIENTED_EDGE ( 'NONE', *, *, #59294, .T. ) ;
#36896 = CARTESIAN_POINT ( 'NONE',  ( 23.56797307596834656, 10.32882671279216780, 9.435355520811883778 ) ) ;
#36897 = CARTESIAN_POINT ( 'NONE',  ( 7.183854719589999327, 5.564636229952000690, -7.532446618777999703 ) ) ;
#36898 = CARTESIAN_POINT ( 'NONE',  ( 18.43348807395466338, 2.701964790437661357, -11.40102144998395062 ) ) ;
#36899 = CARTESIAN_POINT ( 'NONE',  ( 7.115095033390245405, 5.350161709276040511, -7.499994210608702083 ) ) ;
#36900 = ORIENTED_EDGE ( 'NONE', *, *, #11426, .F. ) ;
#36901 = CARTESIAN_POINT ( 'NONE',  ( 9.538434317036999843, -5.620900626097999897, 7.423100105894999245 ) ) ;
#36902 = CARTESIAN_POINT ( 'NONE',  ( 11.60000000000000142, 3.599560744838743886, 8.403338258880264533 ) ) ;
#36903 = CARTESIAN_POINT ( 'NONE',  ( 9.332144816391007680, -3.783447583457012264, 6.534094574943864586 ) ) ;
#36904 = ORIENTED_EDGE ( 'NONE', *, *, #37913, .F. ) ;
#36905 = FACE_OUTER_BOUND ( 'NONE', #26049, .T. ) ;
#36906 = ORIENTED_EDGE ( 'NONE', *, *, #61403, .F. ) ;
#36907 = CARTESIAN_POINT ( 'NONE',  ( 4.978010115736667629, 0.04029576578756273453, 1.517272597181324789 ) ) ;
#36908 = CARTESIAN_POINT ( 'NONE',  ( 18.18005043853800373, 0.02024535615111898099, -13.89999992470869472 ) ) ;
#36909 = CARTESIAN_POINT ( 'NONE',  ( 17.78508576848220812, -0.5812174491462164250, -12.68209204657794409 ) ) ;
#36910 = VECTOR ( 'NONE', #19025, 1000.000000000000114 ) ;
#36911 = CARTESIAN_POINT ( 'NONE',  ( 11.79999999684100054, -12.15995044155999949, -2.000340912084999978 ) ) ;
#36912 = DIRECTION ( 'NONE',  ( 0.000000000000000000, 0.7614089499631907509, 0.6482718649732928107 ) ) ;
#36913 = DIRECTION ( 'NONE',  ( -1.000000000000000000, 0.000000000000000000, 0.000000000000000000 ) ) ;
#36914 = CARTESIAN_POINT ( 'NONE',  ( 12.80505043854143210, 3.124999999999999556, 13.52078605991414939 ) ) ;
#36915 = EDGE_LOOP ( 'NONE', ( #14489, #51470, #69158, #44105 ) ) ;
#36916 = CARTESIAN_POINT ( 'NONE',  ( 8.244326721667006197, -4.955553483043997787, 6.175174249266997428 ) ) ;
#36917 = B_SPLINE_CURVE_WITH_KNOTS ( 'NONE', 3,
 ( #5685, #6369, #54270, #58829, #32279, #10590, #38187, #10938, #11615, #53590, #42755, #68975, #15835, #16862, #43453, #64058, #27027, #16180 ),
 .UNSPECIFIED., .F., .F.,
 ( 4, 2, 2, 2, 2, 2, 2, 2, 4 ),
 ( 0.000000000000000000, 0.1250000000000000000, 0.2500000000000000000, 0.3750000000000000000, 0.5000000000000000000, 0.6250000000000000000, 0.7500000000000000000, 0.8750000000000000000, 1.000000000000000000 ),
 .UNSPECIFIED. ) ;
#36918 = VERTEX_POINT ( 'NONE', #28246 ) ;
#36919 = CARTESIAN_POINT ( 'NONE',  ( 10.61382428715999993, 3.385080336122999967, 5.849521480782000182 ) ) ;
#36920 = CARTESIAN_POINT ( 'NONE',  ( 10.75915165876999957, 5.387277012365999873, -6.278112168454999420 ) ) ;
#36921 = VECTOR ( 'NONE', #59882, 1000.000000000000000 ) ;
#36922 = DIRECTION ( 'NONE',  ( 1.000000000000000000, 0.000000000000000000, 0.000000000000000000 ) ) ;
#36923 = CARTESIAN_POINT ( 'NONE',  ( 12.29449213756044124, 2.138932443162071539, -13.74345175514785922 ) ) ;
#36924 = CARTESIAN_POINT ( 'NONE',  ( 5.200000000000000178, 0.000000000000000000, 0.000000000000000000 ) ) ;
#36925 = CARTESIAN_POINT ( 'NONE',  ( 8.316694475082000437, 2.898380349184999982, 6.611503672649000407 ) ) ;
#36926 = DIRECTION ( 'NONE',  ( 0.000000000000000000, 1.000000000000000000, 0.000000000000000000 ) ) ;
#36927 = DIRECTION ( 'NONE',  ( -0.9999999999999998890, 4.498712764241000040E-09, -1.506424703057999482E-08 ) ) ;
#36928 = EDGE_CURVE ( 'NONE', #18734, #33797, #55158, .T. ) ;
#36929 = EDGE_CURVE ( 'NONE', #27423, #44223, #47378, .T. ) ;
#36930 = VERTEX_POINT ( 'NONE', #4414 ) ;
#36931 = CARTESIAN_POINT ( 'NONE',  ( 12.40965214746187684, 0.4840331164351866500, 13.88865521358243882 ) ) ;
#36932 = CARTESIAN_POINT ( 'NONE',  ( 11.90425819896749893, -5.255890247626999745, 7.263238376356399684 ) ) ;
#36933 = DIRECTION ( 'NONE',  ( 1.000000000000000000, 0.000000000000000000, 0.000000000000000000 ) ) ;
#36934 = DIRECTION ( 'NONE',  ( 0.000000000000000000, -0.000000000000000000, 1.000000000000000000 ) ) ;
#36935 = CARTESIAN_POINT ( 'NONE',  ( 9.041941940379999210, -2.707994276285999646, 5.994456121676999594 ) ) ;
#36937 = CARTESIAN_POINT ( 'NONE',  ( 12.37550370467983818, -11.46556593385705369, 4.499409319922215822 ) ) ;
#36936 = CARTESIAN_POINT ( 'NONE',  ( 5.000000000000000000, 0.000000000000000000, 0.000000000000000000 ) ) ;
#36938 = CARTESIAN_POINT ( 'NONE',  ( 11.57656516821460890, 4.899536366368299589, -8.407828142327998577 ) ) ;
#36939 = CARTESIAN_POINT ( 'NONE',  ( 25.36465286085400095, -11.12555525505000098, 3.380130932433000002 ) ) ;
#36940 = CARTESIAN_POINT ( 'NONE',  ( 9.171747021775997766, 3.348327362764200288, -8.071865996877098937 ) ) ;
#36941 = B_SPLINE_CURVE_WITH_KNOTS ( 'NONE', 1,
 ( #32944, #32267 ),
 .UNSPECIFIED., .F., .F.,
 ( 2, 2 ),
 ( 0.000000000000000000, 1.000000000000000000 ),
 .UNSPECIFIED. ) ;
#36942 = CARTESIAN_POINT ( 'NONE',  ( 18.23387849499154711, 0.2528603812084199154, 12.59746735456353051 ) ) ;
#36943 = CARTESIAN_POINT ( 'NONE',  ( 6.795200891081000449, -1.129313230629999998, -0.5879231567111999901 ) ) ;
#36944 = FACE_OUTER_BOUND ( 'NONE', #37706, .T. ) ;
#36945 = ORIENTED_EDGE ( 'NONE', *, *, #60976, .F. ) ;
#36946 = CARTESIAN_POINT ( 'NONE',  ( 7.647245559622000144, -5.850279024084999335, 6.784181137144999596 ) ) ;
#36947 = CARTESIAN_POINT ( 'NONE',  ( 9.608904719592000987, 4.946705552514000459, -6.253848946732999181 ) ) ;
#36948 = CARTESIAN_POINT ( 'NONE',  ( 17.55505043854143565, 3.248147246781391217, 13.61798588129781074 ) ) ;
#36949 = DIRECTION ( 'NONE',  ( -1.000000000000000000, 0.000000000000000000, 0.000000000000000000 ) ) ;
#36950 = EDGE_LOOP ( 'NONE', ( #11135, #57621, #46003, #4764 ) ) ;
#36951 = EDGE_CURVE ( 'NONE', #29419, #13267, #4756, .T. ) ;
#36952 = CARTESIAN_POINT ( 'NONE',  ( 18.26281931570200356, 2.856833007231000199, 11.95042392763000016 ) ) ;
#36953 = VECTOR ( 'NONE', #27449, 1000.000000000000000 ) ;
#36954 = FACE_OUTER_BOUND ( 'NONE', #32560, .T. ) ;
#36955 = CARTESIAN_POINT ( 'NONE',  ( 10.61443584123000150, 5.287628373050000441, -7.937241318065001217 ) ) ;
#36956 = ORIENTED_EDGE ( 'NONE', *, *, #40020, .T. ) ;
#36957 = CARTESIAN_POINT ( 'NONE',  ( 9.227255459545911975, 4.629538885478623023, -6.407745725917160406 ) ) ;
#36958 = CARTESIAN_POINT ( 'NONE',  ( 18.28104795956118522, -2.296528561422030545, 12.39041189979879398 ) ) ;
#36959 = CARTESIAN_POINT ( 'NONE',  ( 10.17764828895399809, 5.001141961424000471, 6.953185708700699408 ) ) ;
#36960 = CARTESIAN_POINT ( 'NONE',  ( 11.09999999999999964, -2.899999999999999911, 4.467422426380999845 ) ) ;
#36961 = CARTESIAN_POINT ( 'NONE',  ( 7.239691113742999562, 4.389299166881000858, 9.135259451319999613 ) ) ;
#36962 = VERTEX_POINT ( 'NONE', #41149 ) ;
#36963 = CARTESIAN_POINT ( 'NONE',  ( 11.49999144015000319, 3.886253129992999877, -11.90689313971000018 ) ) ;
#36964 = CARTESIAN_POINT ( 'NONE',  ( 15.66247398912732436, 8.798600188463543859, 7.938011626707100810 ) ) ;
#36965 = CARTESIAN_POINT ( 'NONE',  ( 8.541089604138797142, -3.299759450154362117, 5.908022738197796109 ) ) ;
#36966 = CARTESIAN_POINT ( 'NONE',  ( 10.82145113417867677, -3.276884167680957027, -7.991114136793449951 ) ) ;
#36967 = EDGE_LOOP ( 'NONE', ( #32477, #2397, #36853, #68340, #34144 ) ) ;
#36968 = CARTESIAN_POINT ( 'NONE',  ( 15.86053068095500151, -3.820355458042000052, -11.67812044351000011 ) ) ;
#36969 = B_SPLINE_CURVE_WITH_KNOTS ( 'NONE', 3,
 ( #38252, #6433, #53989, #43513 ),
 .UNSPECIFIED., .F., .F.,
 ( 4, 4 ),
 ( 0.000000000000000000, 1.000000000000000000 ),
 .UNSPECIFIED. ) ;
#36970 = CARTESIAN_POINT ( 'NONE',  ( 6.125859839683334584, -1.460959015002473382, -0.3926218265389205819 ) ) ;
#36971 = ORIENTED_EDGE ( 'NONE', *, *, #15417, .F. ) ;
#36972 = EDGE_CURVE ( 'NONE', #26055, #24760, #551, .T. ) ;
#36973 = CARTESIAN_POINT ( 'NONE',  ( 11.00000000000000000, 4.991767524623399233, -7.174999999999999822 ) ) ;
#36974 = DIRECTION ( 'NONE',  ( -1.000000000000000000, 0.000000000000000000, 0.000000000000000000 ) ) ;
#36975 = CLOSED_SHELL ( 'NONE', ( #66959, #40390, #37437, #50675, #9212, #12312, #64629, #54225, #44860, #65340, #39873, #13303, #2878, #63784, #64293, #8022, #8716, #46404, #40398, #18876, #51054, #46009, #50608, #9878, #18873, #12535, #32545, #47603, #34975, #43922, #67292, #15692, #55990, #3192, #18726, #24225, #39394, #39706, #24356, #17700, #13889 ) ) ;
#36976 = CARTESIAN_POINT ( 'NONE',  ( 17.80000000009400196, -3.216307036143000175, -11.40341376487999980 ) ) ;
#36977 = CARTESIAN_POINT ( 'NONE',  ( 21.35000154058000277, 12.59999999999999964, 0.000000000000000000 ) ) ;
#36978 = CARTESIAN_POINT ( 'NONE',  ( 24.45617572612135504, -8.883484012707175026, -9.170518742179092797 ) ) ;
#36979 = CARTESIAN_POINT ( 'NONE',  ( 11.47500581613029880, 4.988618570924500339, -8.134817373646898275 ) ) ;
#36980 = CARTESIAN_POINT ( 'NONE',  ( 11.22191429142990060, -3.974927396630719922, 8.816028813488999916 ) ) ;
#36981 = FACE_OUTER_BOUND ( 'NONE', #32675, .T. ) ;
#36982 = CARTESIAN_POINT ( 'NONE',  ( 10.72272469555899832, -3.360453478306600239, 8.606479382885998675 ) ) ;
#36983 = ORIENTED_EDGE ( 'NONE', *, *, #55535, .T. ) ;
#36984 = CARTESIAN_POINT ( 'NONE',  ( 8.475642219593000348, 5.095085596809999728, 6.286981168432999922 ) ) ;
#36985 = VERTEX_POINT ( 'NONE', #9660 ) ;
#36986 = CARTESIAN_POINT ( 'NONE',  ( 7.770167205733136129, 2.851533015163007168, 6.786995571359490498 ) ) ;
#36987 = CARTESIAN_POINT ( 'NONE',  ( 7.583058059622000080, -4.763531818439999732, 5.668890958491999754 ) ) ;
#36988 = CARTESIAN_POINT ( 'NONE',  ( 10.05226354018249779, 5.092232985442822546, 6.870476274536374994 ) ) ;
#36989 = ORIENTED_EDGE ( 'NONE', *, *, #1401, .T. ) ;
#36990 = CARTESIAN_POINT ( 'NONE',  ( 12.49937493268697075, -3.045244672522429585, -12.30765407517399979 ) ) ;
#36991 = CARTESIAN_POINT ( 'NONE',  ( 11.83099708403000072, 9.769906715298992239, -5.688772285757997871 ) ) ;
#36992 = CARTESIAN_POINT ( 'NONE',  ( 25.29987333571600061, -10.83443035398000021, -3.855530949778000149 ) ) ;
#36993 = CARTESIAN_POINT ( 'NONE',  ( 8.982564767455606614, 2.896581991245595233, -7.795647801703331936 ) ) ;
#36994 = CARTESIAN_POINT ( 'NONE',  ( 12.29798916261921704, -1.995979084551876559, -13.85698889012213186 ) ) ;
#36995 = CARTESIAN_POINT ( 'NONE',  ( 11.19102897915239936, -3.743141152489600110, -8.470038342183499935 ) ) ;
#36996 = DIRECTION ( 'NONE',  ( 0.000000000000000000, -0.1218274111675001353, -0.9925512993736016476 ) ) ;
#36997 = CARTESIAN_POINT ( 'NONE',  ( 18.23147373744593480, -2.220711592698070280, 12.40276429823314075 ) ) ;
#36998 = ORIENTED_EDGE ( 'NONE', *, *, #55658, .T. ) ;
#36999 = ORIENTED_EDGE ( 'NONE', *, *, #31932, .T. ) ;
#37000 = DIRECTION ( 'NONE',  ( 0.000000000000000000, 0.000000000000000000, 1.000000000000000000 ) ) ;
#37001 = FACE_OUTER_BOUND ( 'NONE', #39506, .T. ) ;
#37002 = DIRECTION ( 'NONE',  ( 0.000000000000000000, 0.000000000000000000, -1.000000000000000000 ) ) ;
#37003 = CARTESIAN_POINT ( 'NONE',  ( 10.75911768454999873, 4.477564074640000058, -5.708570851020999370 ) ) ;
#37004 = LINE ( 'NONE', #32792, #5297 ) ;
#37005 = CARTESIAN_POINT ( 'NONE',  ( 17.88331607686618341, 1.943250335976817622, -12.56477475324372683 ) ) ;
#37006 = CARTESIAN_POINT ( 'NONE',  ( 7.698447294381004724, 2.921226879009002797, -6.534475276641003916 ) ) ;
#37007 = EDGE_CURVE ( 'NONE', #12411, #62256, #58861, .T. ) ;
#37009 = ADVANCED_FACE ( 'NONE', ( #68044 ), #20159, .F. ) ;
#37008 = CARTESIAN_POINT ( 'NONE',  ( 17.79128410735117782, -1.798519029228340615, -12.47099317247096906 ) ) ;
#37010 = AXIS2_PLACEMENT_3D ( 'NONE', #8886, #29549, #35800 ) ;
#37011 = ORIENTED_EDGE ( 'NONE', *, *, #59561, .F. ) ;
#37012 = CARTESIAN_POINT ( 'NONE',  ( 8.740166936413396925, -4.651882090383574919, -6.316683530224510790 ) ) ;
#37013 = EDGE_CURVE ( 'NONE', #4, #63146, #3723, .T. ) ;
#37014 = ADVANCED_FACE ( 'NONE', ( #25060 ), #61550, .F. ) ;
#37015 = CARTESIAN_POINT ( 'NONE',  ( 10.02991192131000098, 2.506457833269999824, 6.215406506815000398 ) ) ;
#37016 = CARTESIAN_POINT ( 'NONE',  ( 9.526355082327999213, -4.388021368982800041, -6.724663065681199647 ) ) ;
#37017 = CARTESIAN_POINT ( 'NONE',  ( 10.18908827523999960, 5.907871695079999874, 7.801541097952000570 ) ) ;
#37018 = CARTESIAN_POINT ( 'NONE',  ( 11.02946886766499901, -4.430164648092599577, 8.281567006984099422 ) ) ;
#37019 = CARTESIAN_POINT ( 'NONE',  ( 9.517835841233001304, 4.883347899767999323, -6.417062834774999835 ) ) ;
#37020 = CARTESIAN_POINT ( 'NONE',  ( 11.58902763632552002, 3.213494089586499847, -7.137085349939700230 ) ) ;
#37021 = CARTESIAN_POINT ( 'NONE',  ( 11.08630703507021309, 2.236024944707789786, -7.580658295093686050 ) ) ;
#37022 = CONICAL_SURFACE ( 'NONE', #61619, 1.150087858351999781, 0.7854644967339313721 ) ;
#37023 = CARTESIAN_POINT ( 'NONE',  ( 8.257250525884806791, 3.704169666136653660, -8.842725691832136192 ) ) ;
#37024 = CARTESIAN_POINT ( 'NONE',  ( 10.06843885510000014, 4.148608506723999945, 8.941445591976998841 ) ) ;
#37025 = CARTESIAN_POINT ( 'NONE',  ( 11.25913761803000135, -3.706864829039000053, 11.29572955805999968 ) ) ;
#37026 = VERTEX_POINT ( 'NONE', #35564 ) ;
#37027 = DIRECTION ( 'NONE',  ( 1.000000000000000000, 0.000000000000000000, 0.000000000000000000 ) ) ;
#37028 = CARTESIAN_POINT ( 'NONE',  ( 6.895370762210000670, -1.248147532381999936, -0.07834881647112000580 ) ) ;
#37029 = CARTESIAN_POINT ( 'NONE',  ( 10.99590832059627132, -2.534418414327098468, 6.542952895858777929 ) ) ;
#37030 = CARTESIAN_POINT ( 'NONE',  ( 9.156894352917975155, 5.179846900956039057, -8.179877273890650002 ) ) ;
#37031 = CARTESIAN_POINT ( 'NONE',  ( 24.31006797060300073, 8.914161087288000829, -8.860056390205999222 ) ) ;
#37032 = CARTESIAN_POINT ( 'NONE',  ( 11.16225954179439839, -3.122605388210700106, -8.229019074832200076 ) ) ;
#37033 = ORIENTED_EDGE ( 'NONE', *, *, #27928, .T. ) ;
#37034 = CARTESIAN_POINT ( 'NONE',  ( 5.536712913963323324, -12.19258561490754111, 3.773936784948052292 ) ) ;
#37035 = CARTESIAN_POINT ( 'NONE',  ( 9.271640687504833167, -2.873222873817937284, 6.752018918866299124 ) ) ;
#37037 = CARTESIAN_POINT ( 'NONE',  ( 13.55279538703999975, -9.560508190731999534, -7.863756665013000635 ) ) ;
#37036 = CARTESIAN_POINT ( 'NONE',  ( 9.559179719593000613, 4.038835765825999680, -5.935509327774999733 ) ) ;
#37038 = CARTESIAN_POINT ( 'NONE',  ( 10.76685100253999927, 2.832432432432000269, 6.822293592207000934 ) ) ;
#37039 = ORIENTED_EDGE ( 'NONE', *, *, #7971, .T. ) ;
#37040 = CARTESIAN_POINT ( 'NONE',  ( 10.85069631730999973, 4.478098874537000285, 6.162039661770999821 ) ) ;
#37041 = CARTESIAN_POINT ( 'NONE',  ( 18.08101717074209347, -2.837770499550322789, -13.59594328884928416 ) ) ;
#37042 = CARTESIAN_POINT ( 'NONE',  ( 11.81056516821459823, 4.609678151793300316, 6.884701936848800052 ) ) ;
#37043 = CARTESIAN_POINT ( 'NONE',  ( 24.44496488041000148, -12.03536727282999941, 3.224852091355999928 ) ) ;
#37044 = CARTESIAN_POINT ( 'NONE',  ( 9.208105646793001142, -5.057079407184000175, 8.967634647348999621 ) ) ;
#37045 = ORIENTED_EDGE ( 'NONE', *, *, #31679, .F. ) ;
#37046 = CARTESIAN_POINT ( 'NONE',  ( 9.251926658770999623, 5.159258275969999197, 9.109498396691998678 ) ) ;
#37048 = CARTESIAN_POINT ( 'NONE',  ( 10.94847055962000049, -3.841065069379000274, -9.341805385095000247 ) ) ;
#37047 = CARTESIAN_POINT ( 'NONE',  ( 10.55068303964747578, 3.428091289053144308, -6.838932659516637536 ) ) ;
#37049 = CARTESIAN_POINT ( 'NONE',  ( 7.469483898962876900, -2.313341745386989334, 7.073925100461147863 ) ) ;
#37050 = CARTESIAN_POINT ( 'NONE',  ( 24.44496356299600137, 12.03536643057000077, 3.224849944858999784 ) ) ;
#37051 = CARTESIAN_POINT ( 'NONE',  ( 2.072248059201999837, -3.125150066150999884, -0.9245224406458000255 ) ) ;
#37052 = EDGE_LOOP ( 'NONE', ( #26039, #11962, #67065, #4321 ) ) ;
#37054 = CARTESIAN_POINT ( 'NONE',  ( 23.85399058234839487, 13.23042188477195147, 3.489531688373534557 ) ) ;
#37053 = VECTOR ( 'NONE', #66898, 1000.000000000000000 ) ;
#37055 = CARTESIAN_POINT ( 'NONE',  ( 12.12994988689360021, -3.481863023525599843, 6.483720595741000459 ) ) ;
#37056 = CARTESIAN_POINT ( 'NONE',  ( 10.78089701270000056, 5.735299658853000082, 7.801561896854000366 ) ) ;
#37057 = EDGE_CURVE ( 'NONE', #60421, #12823, #62795, .T. ) ;
#37058 = CARTESIAN_POINT ( 'NONE',  ( 11.03918313518939875, 3.292400735470800033, 6.605241151424599444 ) ) ;
#37059 = ORIENTED_EDGE ( 'NONE', *, *, #43881, .T. ) ;
#37060 = B_SPLINE_CURVE_WITH_KNOTS ( 'NONE', 3,
 ( #44236, #7155, #45262, #29185 ),
 .UNSPECIFIED., .F., .F.,
 ( 4, 4 ),
 ( 0.000000000000000000, 0.1252897355259763035 ),
 .UNSPECIFIED. ) ;
#37061 = CARTESIAN_POINT ( 'NONE',  ( 24.01908879469848301, -3.345608066011616533, 12.71187805225699030 ) ) ;
#37062 = EDGE_CURVE ( 'NONE', #57947, #11817, #6038, .T. ) ;
#37063 = DIRECTION ( 'NONE',  ( -0.7071067811865955344, -0.7011937529517955348, 0.09125415509064935260 ) ) ;
#37064 = CARTESIAN_POINT ( 'NONE',  ( 11.30502344389999969, -5.125258734743999511, 8.182900850620900002 ) ) ;
#37065 = CARTESIAN_POINT ( 'NONE',  ( 25.18907804500399905, -2.894871919440999974, -11.44764655394999942 ) ) ;
#37066 = CARTESIAN_POINT ( 'NONE',  ( 17.97013316094033542, -1.919230625394033662, 13.86782606946093743 ) ) ;
#37067 = LINE ( 'NONE', #69195, #66230 ) ;
#37068 = VERTEX_POINT ( 'NONE', #15943 ) ;
#37069 = CARTESIAN_POINT ( 'NONE',  ( 15.39999999998900293, -9.471998555523999386, -8.194929586088999685 ) ) ;
#37070 = CYLINDRICAL_SURFACE ( 'NONE', #30190, 1.350000000000000533 ) ;
#37071 = ORIENTED_EDGE ( 'NONE', *, *, #28774, .F. ) ;
#37072 = CARTESIAN_POINT ( 'NONE',  ( 10.97719478263000070, -5.298911744033000026, 4.940093110104999852 ) ) ;
#37073 = CARTESIAN_POINT ( 'NONE',  ( 10.84641504065830020, 4.804462279649600376, 8.099826052678000821 ) ) ;
#37074 = AXIS2_PLACEMENT_3D ( 'NONE', #31852, #37093, #32537 ) ;
#37075 = CARTESIAN_POINT ( 'NONE',  ( 9.199602729599000384, 2.551394566582000145, 7.536605852160000119 ) ) ;
#37076 = CARTESIAN_POINT ( 'NONE',  ( 10.46009300862000124, 2.565654508827999614, -6.975684004278000394 ) ) ;
#37077 = CARTESIAN_POINT ( 'NONE',  ( 8.821633776942626071, -3.275060658047592277, -7.989893149673591211 ) ) ;
#37078 = CARTESIAN_POINT ( 'NONE',  ( 9.667080975990000269, -4.541622198376999542, 5.824041840233000755 ) ) ;
#37079 = CARTESIAN_POINT ( 'NONE',  ( 17.90798944145351967, -0.6284163952874818326, -12.58432055988357767 ) ) ;
#37080 = CARTESIAN_POINT ( 'NONE',  ( 12.47149800528992536, 3.028907606620561577, -12.31248708663812685 ) ) ;
#37081 = CARTESIAN_POINT ( 'NONE',  ( 11.45764291764649911, -5.132124077409000229, -7.360052904210999891 ) ) ;
#37082 = CARTESIAN_POINT ( 'NONE',  ( 9.138573341230998182, 2.933833973450999721, 8.496479443567000800 ) ) ;
#37083 = ORIENTED_EDGE ( 'NONE', *, *, #48779, .F. ) ;
#37084 = APPLICATION_PROTOCOL_DEFINITION ( 'draft international standard', 'automotive_design', 1998, #11030 ) ;
#37085 = CYLINDRICAL_SURFACE ( 'NONE', #33616, 1.350000000000000533 ) ;
#37086 = CYLINDRICAL_SURFACE ( 'NONE', #39468, 1.350000000000000533 ) ;
#37087 = CARTESIAN_POINT ( 'NONE',  ( 8.606334483814224612, 2.950802682660377485, -6.230750935425441561 ) ) ;
#37088 = FACE_OUTER_BOUND ( 'NONE', #6779, .T. ) ;
#37089 = CARTESIAN_POINT ( 'NONE',  ( 11.12487846393999824, 6.581954511489999327, 5.643507977536000197 ) ) ;
#37090 = CARTESIAN_POINT ( 'NONE',  ( 11.14434846828000047, 10.07921384928999942, 5.729912880222999938 ) ) ;
#37091 = CARTESIAN_POINT ( 'NONE',  ( 9.242852049159891337, -2.682263764936901662, 7.207900080852989610 ) ) ;
#37092 = EDGE_CURVE ( 'NONE', #35599, #19259, #66419, .T. ) ;
#37093 = DIRECTION ( 'NONE',  ( -1.000000000000000000, 0.000000000000000000, 0.000000000000000000 ) ) ;
#37094 = ADVANCED_FACE ( 'NONE', ( #5459 ), #54034, .F. ) ;
#37095 = ORIENTED_EDGE ( 'NONE', *, *, #18487, .F. ) ;
#37096 = CARTESIAN_POINT ( 'NONE',  ( 12.32338852522668660, -1.942342658536881483, 12.44939237451325731 ) ) ;
#37097 = CARTESIAN_POINT ( 'NONE',  ( 10.18893802597399834, -4.593629475532499562, -6.524634174392399899 ) ) ;
#37098 = CARTESIAN_POINT ( 'NONE',  ( 13.84412491599044159, -8.835575362389704424, -7.593298916478498306 ) ) ;
#37099 = CARTESIAN_POINT ( 'NONE',  ( 10.93728138146000006, -5.425439422033999648, 7.240583766112999697 ) ) ;
#37100 = CARTESIAN_POINT ( 'NONE',  ( 11.37518447801629939, -3.134012688501500055, 7.519093628927509876 ) ) ;
#37101 = VECTOR ( 'NONE', #28366, 1000.000000000000000 ) ;
#37102 = CARTESIAN_POINT ( 'NONE',  ( 8.741072744221000335, 3.937347817007940343, 6.633566614602499634 ) ) ;
#37103 = CARTESIAN_POINT ( 'NONE',  ( 8.970944094206998898, 5.100000000000000533, 6.571291218949999902 ) ) ;
#37104 = CARTESIAN_POINT ( 'NONE',  ( 7.766851002543999627, -2.832432432432000269, 6.822293592207000934 ) ) ;
#37105 = CARTESIAN_POINT ( 'NONE',  ( 12.17603179862374674, 2.838932078785884716, 12.27602983002081771 ) ) ;
#37106 = CARTESIAN_POINT ( 'NONE',  ( 9.175772138681999479, 3.575113238066399912, -6.440186012775000357 ) ) ;
#37107 = CARTESIAN_POINT ( 'NONE',  ( 11.01872200990539952, 3.052519557825900343, -7.169497859994799605 ) ) ;
#37108 = CARTESIAN_POINT ( 'NONE',  ( 11.09999999999999964, 2.700000000000000178, -6.461133846875999787 ) ) ;
#37109 = CARTESIAN_POINT ( 'NONE',  ( 10.62256721958999961, 2.471460423959999986, -8.210789473540000216 ) ) ;
#37110 = EDGE_CURVE ( 'NONE', #54335, #53667, #1250, .T. ) ;
#37111 = CARTESIAN_POINT ( 'NONE',  ( 9.200038493598999167, 4.925784867300699865, -6.617216466537199970 ) ) ;
#37113 = CARTESIAN_POINT ( 'NONE',  ( 18.17614054498634957, -0.08113966125565957865, 12.69973816840999170 ) ) ;
#37112 = CARTESIAN_POINT ( 'NONE',  ( 18.15867081906211311, -11.79498723463443177, 3.559233470735385652 ) ) ;
#37114 = CARTESIAN_POINT ( 'NONE',  ( 8.962848138711493107, 5.333207449751190765, 7.284311848532326827 ) ) ;
#37115 = VERTEX_POINT ( 'NONE', #59631 ) ;
#37116 = VECTOR ( 'NONE', #68858, 999.9999999999998863 ) ;
#37117 = CARTESIAN_POINT ( 'NONE',  ( 0.8334276407239999962, 1.717122193005000019, 2.769960469742999809 ) ) ;
#37118 = CARTESIAN_POINT ( 'NONE',  ( 10.15434687351570631, 5.250000000000002665, 7.663624617374463988 ) ) ;
#37119 = CARTESIAN_POINT ( 'NONE',  ( 10.99934110471000004, -5.081022574063999819, 8.239050178861999640 ) ) ;
#37120 = CARTESIAN_POINT ( 'NONE',  ( 8.802265421554999136, 3.811499292588199861, 6.524915741324599949 ) ) ;
#37121 = CARTESIAN_POINT ( 'NONE',  ( 23.56971544161007159, -3.042705470371831478, -13.65412327231683243 ) ) ;
#37122 = CARTESIAN_POINT ( 'NONE',  ( 12.42293806700078385, -2.994693046128884539, 13.55600569395198995 ) ) ;
#37123 = CARTESIAN_POINT ( 'NONE',  ( 12.21587634993881188, 2.708625115168846520, 13.62694294273322804 ) ) ;
#37124 = CARTESIAN_POINT ( 'NONE',  ( 23.58471847246500275, 3.197974897699999985, -13.62073867207999989 ) ) ;
#37125 = VERTEX_POINT ( 'NONE', #10694 ) ;
#37126 = CARTESIAN_POINT ( 'NONE',  ( 5.003257791993000581, 0.7138878598698999989, -0.8816291593956999684 ) ) ;
#37127 = CARTESIAN_POINT ( 'NONE',  ( 9.503988259786000370, -4.167373623506299474, -8.768215461831999846 ) ) ;
#37128 = CARTESIAN_POINT ( 'NONE',  ( 8.455992358812000731, -4.599999999999999645, 6.571291218949999902 ) ) ;
#37129 = DIRECTION ( 'NONE',  ( 1.000000000000000000, 0.000000000000000000, 0.000000000000000000 ) ) ;
#37130 = CARTESIAN_POINT ( 'NONE',  ( 18.09722825099190402, 2.811571021179180452, -12.37353494292365497 ) ) ;
#37131 = CARTESIAN_POINT ( 'NONE',  ( 9.803275160948500044, -5.099670516381894281, 8.115397037630309285 ) ) ;
#37132 = CARTESIAN_POINT ( 'NONE',  ( 17.88923853191783664, 3.028508370112690251, 12.31258559103103245 ) ) ;
#37133 = CARTESIAN_POINT ( 'NONE',  ( 9.487899699504998452, -4.011292643094999555, -9.373220388412001114 ) ) ;
#37134 = CARTESIAN_POINT ( 'NONE',  ( 24.45999053249100186, 11.93730388424000033, 3.254644296425999617 ) ) ;
#37135 = EDGE_CURVE ( 'NONE', #66793, #25777, #62208, .T. ) ;
#37136 = CARTESIAN_POINT ( 'NONE',  ( 12.61577834523377817, 1.811481987173967578, 13.88231333970316506 ) ) ;
#37137 = B_SPLINE_SURFACE_WITH_KNOTS ( 'NONE', 3, 3, ( 
 ( #22791, #29099, #17201, #6710, #6360, #50409, #1129, #45171, #16853, #1821, #33644, #38886, #38176, #22443, #65080, #38530, #1473, #11959, #8448, #9125, #67161, #29795, #35369, #30464, #62269, #52115, #36040, #30133, #40264, #46544, #40947, #13360, #24868, #24527, #19626, #25556, #57356, #67507, #18940, #3533, #51098, #61584, #67849, #9460, #3200, #46196, #66827, #56000, #30802, #51775, #19274, #14388, #57025, #19971, #35708, #3873, #25207, #41294, #51436, #13700, #40602, #62601, #56345, #8105, #14725, #61928, #2851 ),
 ( #14042, #45852, #4220, #56691, #8790, #66476, #18600, #39927, #61245, #34686, #29448, #35030, #50755, #24179, #45517, #5257, #4907, #13, #5936, #16431, #47916, #68531, #53155, #58061, #20653, #26936, #37760, #31492, #26596, #47228, #36386, #59085, #10845, #47576, #42665, #37417, #48249, #21336, #63972, #16087, #58738, #10499, #41979, #68882, #53501, #36741, #57703, #32187, #20999, #52463, #5591, #355, #63285, #11187, #58394, #9813, #31839, #42334, #21670, #43006, #31162, #64312, #32523, #63636, #62939, #26249, #53839 ),
 ( #46882, #10163, #68189, #15754, #20307, #15414, #41633, #15063, #52814, #4561, #25899, #37081, #54880, #23413, #44749, #33559, #704, #22017, #6982, #66050, #49632, #60471, #65707, #34254, #18171, #59425, #33908, #22709, #27279, #12578, #59773, #43364, #38100, #7325, #64664, #12928, #16768, #28666, #55225, #11523, #38803, #6278, #48601, #49283, #55576, #32867, #39493, #54181, #28309, #27622, #48948, #17477, #1055, #49982, #27972, #22367, #65358, #2094, #1737, #43706, #23056, #39145, #60815, #17829, #65001, #17116, #38450 ),
 ( #60127, #44407, #6634, #1393, #11875, #33214, #54534, #44053, #12234, #66396, #45431, #29361, #51688, #23753, #45089, #19191, #50674, #62520, #3786, #41210, #34945, #8708, #3114, #56259, #46457, #51013, #46110, #25124, #18860, #13621, #30052, #8024, #66742, #50329, #67756, #18519, #30380, #51354, #45771, #24445, #8368, #29712, #62181, #67078, #39841, #40187, #40514, #61503, #19541, #61841, #13959, #35287, #40859, #3446, #14639, #19882, #56601, #2773, #56943, #24783, #61163, #67417, #14303, #35630, #35957, #7676, #9039 ) ),
 .UNSPECIFIED., .F., .F., .F.,
 ( 4, 4 ),
 ( 4, 1, 1, 1, 1, 1, 1, 1, 1, 1, 1, 1, 1, 1, 1, 1, 1, 1, 1, 1, 1, 1, 1, 1, 1, 1, 1, 1, 1, 1, 1, 1, 1, 1, 1, 1, 1, 1, 1, 1, 1, 1, 1, 1, 1, 1, 1, 1, 1, 1, 1, 1, 1, 1, 1, 1, 1, 1, 1, 1, 1, 1, 1, 1, 4 ),
 ( -0.02000000000000000042, 1.020000000000000018 ),
 ( 0.008747244164287000176, 0.02453926110774999961, 0.04033127805120999970, 0.05612329499467000327, 0.07191531193812999989, 0.08770732888158999652, 0.1034993458251000087, 0.1192913627684999978, 0.1350833797120000179, 0.1508753966553999792, 0.1666674135988999994, 0.1824594305423999918, 0.1982514474858000086, 0.2140434644293000011, 0.2298354813727000179, 0.2456274983162000103, 0.2614195152596999749, 0.2772115322030999640, 0.2930035491465999842, 0.3087955660900000288, 0.3245875830334999934, 0.3403795999769999581, 0.3561716169204000026, 0.3719636338639000228, 0.3877556508073999875, 0.4035476677507999765, 0.4193396846942999967, 0.4351317016376999858, 0.4509237185811999504, 0.4667157355247000261, 0.4825077524681000152, 0.4982997694115999798, 0.5140917863550000799, 0.5298838032985000446, 0.5456758202420000092, 0.5614678371854000538, 0.5772598541289000185, 0.5930518710723000630, 0.6088438880158000277, 0.6246359049592999924, 0.6404279219027000369, 0.6562199388462000016, 0.6720119557896999662, 0.6878039727331000108, 0.7035959896765999755, 0.7193880066200000201, 0.7351800235634999847, 0.7509720405069999494, 0.7667640574504001050, 0.7825560743939000696, 0.7983480913373000032, 0.8141401082808000789, 0.8299321252243000435, 0.8457241421676999771, 0.8615161591112000528, 0.8773081760545999863, 0.8931001929981000620, 0.9088922099416000266, 0.9246842268849999602, 0.9404762438285000359, 0.9562682607720000005, 0.9720602777153999341, 0.9878522946589000098, 1.003644311601999961, 1.019436328545999970 ),
 .UNSPECIFIED. ) ;
#37138 = CARTESIAN_POINT ( 'NONE',  ( 11.50001544675000531, -12.31773593200242090, 2.620250046283704837 ) ) ;
#37139 = CARTESIAN_POINT ( 'NONE',  ( 4.599999999999999645, -0.7302158263239085789, 13.98094363220830871 ) ) ;
#37140 = CARTESIAN_POINT ( 'NONE',  ( 8.798455008774128672, -3.051544939223430397, -7.736326407956449103 ) ) ;
#37141 = CARTESIAN_POINT ( 'NONE',  ( 24.57034583260499971, 12.57146371045999977, -2.966472501429000097 ) ) ;
#37142 = ORIENTED_EDGE ( 'NONE', *, *, #1674, .T. ) ;
#37143 = CARTESIAN_POINT ( 'NONE',  ( 8.506095280410999493, 2.305580295895999665, -7.860904109308999743 ) ) ;
#37144 = CARTESIAN_POINT ( 'NONE',  ( 11.86749010443640096, -3.136214309321499805, 7.435402237490909449 ) ) ;
#37145 = ORIENTED_EDGE ( 'NONE', *, *, #31675, .T. ) ;
#37146 = CIRCLE ( 'NONE', #59445, 2.099999999999998757 ) ;
#37147 = DIRECTION ( 'NONE',  ( 1.000000000000000000, 0.000000000000000000, 0.000000000000000000 ) ) ;
#37148 = CARTESIAN_POINT ( 'NONE',  ( 11.11302897915239818, -3.708003626182200030, -8.602736702002999891 ) ) ;
#37149 = ORIENTED_EDGE ( 'NONE', *, *, #30017, .F. ) ;
#37150 = DIRECTION ( 'NONE',  ( 0.000000000000000000, 0.9999808993455937545, 0.006180691221632959691 ) ) ;
#37151 = CYLINDRICAL_SURFACE ( 'NONE', #28890, 11.84999999999999964 ) ;
#37152 = CARTESIAN_POINT ( 'NONE',  ( 18.16715644869600155, -3.024463723863999753, 11.49930835314999911 ) ) ;
#37153 = CARTESIAN_POINT ( 'NONE',  ( 11.31900581613029821, -3.249313226592100534, -7.982035256002799173 ) ) ;
#37154 = CARTESIAN_POINT ( 'NONE',  ( 9.758513540182331525, -3.836375382625526687, -6.250000000000000888 ) ) ;
#37155 = CARTESIAN_POINT ( 'NONE',  ( 6.778816671981999775, -0.8882170986559999593, 0.6661914818925001036 ) ) ;
#37156 = CARTESIAN_POINT ( 'NONE',  ( 13.27439970770000066, 11.71097706365999969, 2.049245155247000127 ) ) ;
#37157 = EDGE_LOOP ( 'NONE', ( #19960, #64303, #32421, #57038 ) ) ;
#37158 = CARTESIAN_POINT ( 'NONE',  ( 9.418385841233000377, 3.251172436837000301, -6.320036569851000152 ) ) ;
#37159 = ORIENTED_EDGE ( 'NONE', *, *, #52574, .F. ) ;
#37160 = VECTOR ( 'NONE', #44306, 1000.000000000000114 ) ;
#37161 = CARTESIAN_POINT ( 'NONE',  ( 16.09997386696500143, 8.350085070477001992, 8.123950967096998710 ) ) ;
#37162 = ORIENTED_EDGE ( 'NONE', *, *, #57971, .F. ) ;
#37163 = CARTESIAN_POINT ( 'NONE',  ( 8.845430433046999497, 2.911395389258000233, 8.171806809244198888 ) ) ;
#37164 = CARTESIAN_POINT ( 'NONE',  ( 17.57591570971905170, -3.124999463061048921, -12.28373083832239132 ) ) ;
#37165 = CARTESIAN_POINT ( 'NONE',  ( 17.77392020236939985, 11.85836615397808025, -3.313854778486285291 ) ) ;
#37166 = DIRECTION ( 'NONE',  ( 0.9999999999998953060, 4.575885588343982003E-07, -2.007390825282990779E-09 ) ) ;
#37167 = EDGE_CURVE ( 'NONE', #55522, #23367, #13896, .T. ) ;
#37168 = CARTESIAN_POINT ( 'NONE',  ( 12.52788616429852198, 0.5605600754933556251, 13.88478672247769552 ) ) ;
#37169 = EDGE_CURVE ( 'NONE', #30230, #60711, #39682, .T. ) ;
#37170 = ORIENTED_EDGE ( 'NONE', *, *, #30074, .T. ) ;
#37171 = CARTESIAN_POINT ( 'NONE',  ( 12.01716035628400192, 11.91307312420999942, -3.686993282830000052 ) ) ;
#37172 = CARTESIAN_POINT ( 'NONE',  ( 18.35816574290100078, 11.69157926155999938, -4.070931047779999368 ) ) ;
#37173 = CARTESIAN_POINT ( 'NONE',  ( 9.277558426223626142, 4.358884483112399622, 6.702043737600841489 ) ) ;
#37174 = CARTESIAN_POINT ( 'NONE',  ( 12.80505043854143388, 3.248109929747637015, -13.61799478206225444 ) ) ;
#37175 = CARTESIAN_POINT ( 'NONE',  ( 11.59999999999999964, 3.116215992411100366, 7.174999999999999822 ) ) ;
#37176 = CARTESIAN_POINT ( 'NONE',  ( 18.01722669115800102, -3.499390932422000056, 11.96939125376999868 ) ) ;
#37177 = CARTESIAN_POINT ( 'NONE',  ( 9.976697000975999430, -4.172225768856000272, -6.147144998063999388 ) ) ;
#37178 = B_SPLINE_CURVE_WITH_KNOTS ( 'NONE', 3,
 ( #23314, #50571, #39391, #60712 ),
 .UNSPECIFIED., .F., .F.,
 ( 4, 4 ),
 ( 0.000000000000000000, 1.000000000000000000 ),
 .UNSPECIFIED. ) ;
#37179 = ORIENTED_EDGE ( 'NONE', *, *, #68958, .F. ) ;
#37180 = ORIENTED_EDGE ( 'NONE', *, *, #19477, .T. ) ;
#37181 = CARTESIAN_POINT ( 'NONE',  ( 11.13228700150999906, 5.320905268945000266, -4.957687855802999088 ) ) ;
#37182 = CARTESIAN_POINT ( 'NONE',  ( 11.50001258332000020, 11.56502147876000031, 1.404302031979000054 ) ) ;
#37183 = CARTESIAN_POINT ( 'NONE',  ( 1.280140132540750653, -3.408904368339108260, 0.9161175952574674985 ) ) ;
#37184 = DIRECTION ( 'NONE',  ( 0.000000000000000000, 0.7071067811865995312, 0.7071067811864953923 ) ) ;
#37185 = CARTESIAN_POINT ( 'NONE',  ( 11.83003632436370012, 2.756744593645999775, -7.209663534847899236 ) ) ;
#37186 = ADVANCED_FACE ( 'NONE', ( #6484 ), #43906, .T. ) ;
#37187 = CARTESIAN_POINT ( 'NONE',  ( 9.965950584426998660, 4.344127791340399725, -6.704208565179699875 ) ) ;
#37189 = CARTESIAN_POINT ( 'NONE',  ( 10.26027384100999917, -3.427607989534000144, 4.531780802426999877 ) ) ;
#37188 = CARTESIAN_POINT ( 'NONE',  ( 10.81357120343299982, -4.048688523195909994, 6.496769302834999316 ) ) ;
#37190 = FACE_OUTER_BOUND ( 'NONE', #33588, .T. ) ;
#37191 = ORIENTED_EDGE ( 'NONE', *, *, #19176, .F. ) ;
#37192 = AXIS2_PLACEMENT_3D ( 'NONE', #11554, #18546, #60498 ) ;
#37193 = ADVANCED_FACE ( 'NONE', ( #11725 ), #59279, .F. ) ;
#37194 = CARTESIAN_POINT ( 'NONE',  ( 9.716846873515667227, 4.768183399968648040, -6.500416447002277387 ) ) ;
#37195 = CARTESIAN_POINT ( 'NONE',  ( 5.500000000000000000, 13.04986661130000059, 1.811520473896000016 ) ) ;
#37196 = CARTESIAN_POINT ( 'NONE',  ( 10.29226717315700057, 3.026371913119300316, 8.329718467866699783 ) ) ;
#37197 = CARTESIAN_POINT ( 'NONE',  ( 5.700000000000000178, -13.03908314092542753, -1.889202648615756486 ) ) ;
#37198 = CARTESIAN_POINT ( 'NONE',  ( 9.471368011205999693, -2.030678448189000118, 7.549764202121000523 ) ) ;
#37199 = CARTESIAN_POINT ( 'NONE',  ( 18.03251246674827257, 2.904216811361305162, -12.34819510225365669 ) ) ;
#37200 = CARTESIAN_POINT ( 'NONE',  ( 16.18329442974999921, -3.298233714334000144, -11.32377282473999891 ) ) ;
#37201 = DIRECTION ( 'NONE',  ( 0.000000000000000000, -1.000000000000000000, 0.000000000000000000 ) ) ;
#37202 = CARTESIAN_POINT ( 'NONE',  ( 7.047500695249826919, 4.967648385114367571, -6.408980097745973659 ) ) ;
#37203 = AXIS2_PLACEMENT_3D ( 'NONE', #8243, #65322, #56479 ) ;
#37204 = CARTESIAN_POINT ( 'NONE',  ( 9.535355082327999554, -4.388021368982800041, -6.724663065681199647 ) ) ;
#37205 = CARTESIAN_POINT ( 'NONE',  ( 6.254548602795000356, -0.8406263976572999619, -1.204107458873000081 ) ) ;
#37206 = CARTESIAN_POINT ( 'NONE',  ( 6.999999999999999112, 9.352249708179474652, -4.701180404399401880 ) ) ;
#37207 = VECTOR ( 'NONE', #7852, 1000.000000000000000 ) ;
#37208 = CARTESIAN_POINT ( 'NONE',  ( 0.5000220334827000235, 3.499749845413000049, -0.04184518527856000147 ) ) ;
#37209 = ORIENTED_EDGE ( 'NONE', *, *, #36072, .T. ) ;
#37210 = CARTESIAN_POINT ( 'NONE',  ( 12.20137806200446029, -0.1622035078961271970, -12.69861136640060195 ) ) ;
#37211 = CARTESIAN_POINT ( 'NONE',  ( 8.228368194306998618, -4.806758213702000404, 6.177034600996000435 ) ) ;
#37212 = CARTESIAN_POINT ( 'NONE',  ( 11.00000000000000000, -5.058572498595999889, -7.825000000000000178 ) ) ;
#37213 = FACE_OUTER_BOUND ( 'NONE', #31256, .T. ) ;
#37214 = CARTESIAN_POINT ( 'NONE',  ( 1.623890132540958486, 2.150913519912194261, 2.798833948393636195 ) ) ;
#37215 = ORIENTED_EDGE ( 'NONE', *, *, #37700, .F. ) ;
#37216 = CARTESIAN_POINT ( 'NONE',  ( 3.800000448357999883, 1.625000000000000000, 0.000000000000000000 ) ) ;
#37217 = CARTESIAN_POINT ( 'NONE',  ( 10.77368717260499942, -4.539928529895099985, -8.381256426168800289 ) ) ;
#37218 = DIRECTION ( 'NONE',  ( 1.000000000000000000, 0.000000000000000000, 0.000000000000000000 ) ) ;
#37219 = FACE_OUTER_BOUND ( 'NONE', #16169, .T. ) ;
#37220 = CARTESIAN_POINT ( 'NONE',  ( 11.10391045180383962, 5.129049487418003928, -8.114538794791117837 ) ) ;
#37221 = CARTESIAN_POINT ( 'NONE',  ( 11.40211496860029783, 4.793947479907100018, -7.093139000852099585 ) ) ;
#37222 = ORIENTED_EDGE ( 'NONE', *, *, #20396, .F. ) ;
#37223 = B_SPLINE_CURVE_WITH_KNOTS ( 'NONE', 3,
 ( #35247, #46072, #67378, #25775, #4092, #25429, #46762, #48133, #6157, #16310, #58274, #53381, #11071, #32064, #32744 ),
 .UNSPECIFIED., .F., .F.,
 ( 4, 2, 2, 2, 1, 2, 2, 4 ),
 ( 0.000000000000000000, 0.2500000000000199840, 0.3750000000000303646, 0.4375000000000324185, 0.4687500000000315858, 0.4843750000000310307, 0.5000000000000305311, 1.000000000000000000 ),
 .UNSPECIFIED. ) ;
#37224 = CARTESIAN_POINT ( 'NONE',  ( 10.78089914631999946, -5.735295708369000600, 7.801561210335000496 ) ) ;
#37225 = CARTESIAN_POINT ( 'NONE',  ( 8.797364180957998769, -4.070567455836420656, -8.475895758763700272 ) ) ;
#37226 = ORIENTED_EDGE ( 'NONE', *, *, #29718, .F. ) ;
#37227 = FACE_OUTER_BOUND ( 'NONE', #35776, .T. ) ;
#37228 = CARTESIAN_POINT ( 'NONE',  ( 8.187144353207999714, -4.968144979409999884, 5.971795951526999602 ) ) ;
#37229 = DIRECTION ( 'NONE',  ( 0.000000000000000000, -1.000000000000000000, 0.000000000000000000 ) ) ;
#37230 = PRODUCT_RELATED_PRODUCT_CATEGORY ( 'part', '', ( #23773 ) ) ;
#37231 = ORIENTED_EDGE ( 'NONE', *, *, #19972, .F. ) ;
#37232 = CARTESIAN_POINT ( 'NONE',  ( 9.906851002540999929, -2.832432432432000269, -6.822293592207000934 ) ) ;
#37233 = CARTESIAN_POINT ( 'NONE',  ( 7.166135841225999670, 2.502464354543000091, -6.330838737160999763 ) ) ;
#37234 = CARTESIAN_POINT ( 'NONE',  ( 9.427263540183332680, -4.629523725463626782, -8.592232985442821658 ) ) ;
#37235 = FACE_OUTER_BOUND ( 'NONE', #14629, .T. ) ;
#37236 = ORIENTED_EDGE ( 'NONE', *, *, #34272, .T. ) ;
#37237 = CARTESIAN_POINT ( 'NONE',  ( 10.09697182628999990, -5.253379538902000156, 8.530665717066000298 ) ) ;
#37238 = AXIS2_PLACEMENT_3D ( 'NONE', #14885, #68349, #20468 ) ;
#37239 = CARTESIAN_POINT ( 'NONE',  ( 11.59999999999999787, 3.905927825748639837, 8.528759793293470892 ) ) ;
#37240 = DIRECTION ( 'NONE',  ( 0.000000000000000000, -1.000000000000000000, -0.000000000000000000 ) ) ;
#37241 = ORIENTED_EDGE ( 'NONE', *, *, #45006, .F. ) ;
#37242 = CIRCLE ( 'NONE', #41681, 1.775000326287000219 ) ;
#37243 = DIRECTION ( 'NONE',  ( 1.000000000000000000, 7.105427357289000429E-14, 1.065814103592999999E-13 ) ) ;
#37244 = ORIENTED_EDGE ( 'NONE', *, *, #49105, .T. ) ;
#37245 = DIRECTION ( 'NONE',  ( -1.000000000000000000, 0.000000000000000000, 0.000000000000000000 ) ) ;
#37246 = CARTESIAN_POINT ( 'NONE',  ( 17.97079960141762811, -1.890785106268467075, -12.45732622342820584 ) ) ;
#37247 = DIRECTION ( 'NONE',  ( 0.000000000000000000, -1.000000000000000000, 0.000000000000000000 ) ) ;
#37248 = CARTESIAN_POINT ( 'NONE',  ( 11.59999999999999964, 4.935123867447916979, -6.791171049664775694 ) ) ;
#37249 = LINE ( 'NONE', #41466, #24135 ) ;
#37250 = CARTESIAN_POINT ( 'NONE',  ( 11.59999999999999964, 5.207010770456999893, -7.825000000000000178 ) ) ;
#37251 = DIRECTION ( 'NONE',  ( 0.000000000000000000, -1.000000000000000000, 0.000000000000000000 ) ) ;
#37252 = VERTEX_POINT ( 'NONE', #48800 ) ;
#37253 = EDGE_CURVE ( 'NONE', #23714, #3814, #49616, .T. ) ;
#37254 = CARTESIAN_POINT ( 'NONE',  ( 7.954655249370001791, -5.133340916889001626, 6.761736834907998706 ) ) ;
#37255 = EDGE_CURVE ( 'NONE', #855, #16959, #18883, .T. ) ;
#37256 = EDGE_LOOP ( 'NONE', ( #8670, #32060, #58294, #21896 ) ) ;
#37257 = CARTESIAN_POINT ( 'NONE',  ( 9.799251915619999309, 4.057329420971000467, 9.430703183047999261 ) ) ;
#37258 = CARTESIAN_POINT ( 'NONE',  ( 10.91060165877000188, 4.702351492776999820, -9.210043641106000933 ) ) ;
#37259 = CARTESIAN_POINT ( 'NONE',  ( 11.01922882085999866, -5.268778362341000054, 4.995697847266999503 ) ) ;
#37260 = CARTESIAN_POINT ( 'NONE',  ( 12.76347793713366130, 1.876036575608650780, -13.78616487348347519 ) ) ;
#37261 = CARTESIAN_POINT ( 'NONE',  ( 11.59999999999999964, -4.883784007588900522, -7.825000000000000178 ) ) ;
#37262 = SURFACE_STYLE_USAGE ( .BOTH. , #5447 ) ;
#37263 = CARTESIAN_POINT ( 'NONE',  ( 18.12876426765905435, -0.2481576080865494083, 13.89702325994033671 ) ) ;
#37264 = CIRCLE ( 'NONE', #29502, 1.300160515709999576 ) ;
#37265 = CARTESIAN_POINT ( 'NONE',  ( 9.299840153678500698, -5.532928100317616504, -6.657476841886525776 ) ) ;
#37266 = VERTEX_POINT ( 'NONE', #32722 ) ;
#37267 = CARTESIAN_POINT ( 'NONE',  ( 12.83143828159500188, -11.44347076768000093, 4.696252053897000067 ) ) ;
#37268 = CARTESIAN_POINT ( 'NONE',  ( 11.97810404293059960, -4.563346034752700398, 6.352848032645000309 ) ) ;
#37269 = DIRECTION ( 'NONE',  ( 0.000000000000000000, 1.000000000000000000, 0.000000000000000000 ) ) ;
#37270 = CARTESIAN_POINT ( 'NONE',  ( 8.400066940379998570, -2.800111029801999774, 9.079936276749000612 ) ) ;
#37272 = CARTESIAN_POINT ( 'NONE',  ( 0.7000000000000000666, -1.154700538379000108, 0.000000000000000000 ) ) ;
#37271 = CARTESIAN_POINT ( 'NONE',  ( 10.00637913184999839, 5.119263020957999899, 8.420380450036001108 ) ) ;
#37273 = CARTESIAN_POINT ( 'NONE',  ( 10.39918582084299992, 3.253651555277099927, -6.637298362509499228 ) ) ;
#37274 = B_SPLINE_CURVE_WITH_KNOTS ( 'NONE', 3,
 ( #68331, #36532, #31637, #11328, #52266, #57856, #65151, #33710, #6083, #22507, #54679, #16915 ),
 .UNSPECIFIED., .F., .F.,
 ( 4, 2, 2, 2, 2, 4 ),
 ( 0.1253171456473068379, 0.2189680742877681552, 0.3126190029282295280, 0.4999208602091519404, 0.6872227174900742419, 0.8745245747709966544 ),
 .UNSPECIFIED. ) ;
#37275 = EDGE_CURVE ( 'NONE', #27251, #46140, #21345, .T. ) ;
#37276 = CARTESIAN_POINT ( 'NONE',  ( 15.99981196018700125, 1.318944953255000000E-13, -6.750155989720999729E-14 ) ) ;
#37277 = CARTESIAN_POINT ( 'NONE',  ( 9.779646554150998483, 4.419749732651400365, -8.258629096756299859 ) ) ;
#37278 = CARTESIAN_POINT ( 'NONE',  ( 18.10141690196193309, -0.3036663359794732342, 12.69511825016612860 ) ) ;
#37279 = B_SPLINE_SURFACE_WITH_KNOTS ( 'NONE', 3, 3, ( 
 ( #11380, #7184, #27474, #43558, #38651, #6483, #34109, #1249, #43905, #18030, #33066, #22563, #17681, #1593, #2285, #50182, #54733, #28521, #23603, #12432, #49832, #44262, #32721, #54033, #65208, #11724, #12780, #39344, #59974, #65558, #17325, #48799, #60324, #12084, #55428, #49481, #16969, #7519, #16630, #64510, #60665, #33415, #39006, #6833, #37958, #59278, #6135, #908, #28165, #22221, #33763, #38300, #59630, #54382, #27832, #55078, #23264, #44608, #65902, #24294, #51885, #67612, #45963, #13812, #19045, #13132, #51212 ),
 ( #61014, #34460, #50868, #61356, #62381, #19739, #40373, #3308, #66935, #29211, #40713, #29566, #14498, #29907, #23953, #57134, #66249, #3980, #41061, #35143, #24643, #2965, #9231, #18371, #44945, #35817, #45631, #8218, #55773, #8901, #56455, #39693, #61694, #34796, #67273, #8560, #7876, #51545, #66593, #3641, #24978, #56107, #30570, #19388, #62040, #50522, #2622, #45287, #18712, #40045, #14156, #35483, #46312, #13477, #56804, #30241, #36156, #57469, #126, #20418, #63746, #68299, #57819, #9576, #30918, #41746, #52231 ),
 ( #42435, #10963, #15858, #32303, #31604, #37188, #9928, #63048, #53611, #48023, #15523, #26709, #47687, #58507, #63402, #26361, #4670, #68646, #46658, #58853, #21443, #5371, #10612, #14836, #15174, #46997, #36498, #31266, #52576, #42778, #4331, #25665, #31952, #26012, #41407, #25320, #53269, #47341, #67963, #37527, #20764, #42094, #20078, #62713, #21110, #36850, #64085, #16203, #58170, #10271, #52926, #5022, #68998, #53948, #49058, #16888, #44524, #59544, #54294, #28434, #43477, #11639, #28083, #11995, #12691, #60586, #65118 ),
 ( #38922, #33332, #21787, #64425, #32980, #22136, #23175, #49748, #1164, #54649, #27745, #59196, #1508, #6396, #65819, #59886, #6051, #17943, #27050, #34028, #1857, #43821, #6743, #22479, #39263, #48363, #5709, #470, #17241, #38215, #43121, #60243, #38563, #16547, #49397, #64774, #22826, #44174, #37877, #12345, #27390, #33678, #54996, #65470, #11298, #17595, #7097, #32638, #48717, #819, #29130, #34374, #56378, #50790, #56725, #60933, #2885, #50438, #66168, #18287, #30164, #2540, #24560, #23867, #18631, #39606, #13045 ) ),
 .UNSPECIFIED., .F., .F., .F.,
 ( 4, 4 ),
 ( 4, 1, 1, 1, 1, 1, 1, 1, 1, 1, 1, 1, 1, 1, 1, 1, 1, 1, 1, 1, 1, 1, 1, 1, 1, 1, 1, 1, 1, 1, 1, 1, 1, 1, 1, 1, 1, 1, 1, 1, 1, 1, 1, 1, 1, 1, 1, 1, 1, 1, 1, 1, 1, 1, 1, 1, 1, 1, 1, 1, 1, 1, 1, 1, 4 ),
 ( -0.02000000000000000042, 1.020000000000000018 ),
 ( -0.02000000000000000042, -0.003749999999999999861, 0.01250000000000000069, 0.02875000000000000125, 0.04499999999999999833, 0.06124999999999999889, 0.07749999999999999944, 0.09375000000000000000, 0.1100000000000000006, 0.1262500000000000011, 0.1424999999999999878, 0.1587500000000000022, 0.1749999999999999889, 0.1912500000000000033, 0.2074999999999999900, 0.2237500000000000044, 0.2399999999999999911, 0.2562499999999999778, 0.2725000000000000200, 0.2887500000000000067, 0.3049999999999999933, 0.3212499999999999800, 0.3375000000000000222, 0.3537500000000000089, 0.3699999999999999956, 0.3862499999999999822, 0.4025000000000000244, 0.4187500000000000111, 0.4349999999999999978, 0.4512499999999999845, 0.4675000000000000266, 0.4837500000000000133, 0.5000000000000000000, 0.5162499999999999867, 0.5324999999999999734, 0.5487499999999999600, 0.5649999999999999467, 0.5812500000000000444, 0.5975000000000000311, 0.6137500000000000178, 0.6300000000000000044, 0.6462499999999999911, 0.6624999999999999778, 0.6787499999999999645, 0.6949999999999999512, 0.7112500000000000488, 0.7275000000000000355, 0.7437500000000000222, 0.7600000000000000089, 0.7762499999999999956, 0.7924999999999999822, 0.8087499999999999689, 0.8249999999999999556, 0.8412500000000000533, 0.8575000000000000400, 0.8737500000000000266, 0.8900000000000000133, 0.9062500000000000000, 0.9224999999999999867, 0.9387499999999999734, 0.9549999999999999600, 0.9712499999999999467, 0.9875000000000000444, 1.003749999999999920, 1.020000000000000018 ),
 .UNSPECIFIED. ) ;
#37280 = CARTESIAN_POINT ( 'NONE',  ( 6.894825288116000372, 0.2042423412131999794, -1.256697851460000237 ) ) ;
#37281 = CARTESIAN_POINT ( 'NONE',  ( 24.03014912280099935, 9.409787345911999168, 9.736160099024999681 ) ) ;
#37282 = ORIENTED_EDGE ( 'NONE', *, *, #38600, .T. ) ;
#37283 = CARTESIAN_POINT ( 'NONE',  ( 7.352706853207999771, -4.773080213113000347, 8.927399220053999329 ) ) ;
#37284 = CARTESIAN_POINT ( 'NONE',  ( 9.021064158776001207, 4.883347899767999323, -6.417062834774999835 ) ) ;
#37285 = DIRECTION ( 'NONE',  ( -0.000000000000000000, 1.000000000000000000, 0.000000000000000000 ) ) ;
#37286 = DIRECTION ( 'NONE',  ( 0.000000000000000000, -1.000000000000000000, 0.000000000000000000 ) ) ;
#37287 = ORIENTED_EDGE ( 'NONE', *, *, #12873, .T. ) ;
#37288 = AXIS2_PLACEMENT_3D ( 'NONE', #64954, #33513, #49931 ) ;
#37289 = CARTESIAN_POINT ( 'NONE',  ( 0.7573593903515000170, -3.617551005558000021, 0.7847820700415000239 ) ) ;
#37290 = CARTESIAN_POINT ( 'NONE',  ( 17.55505043854143565, 3.125000000000000000, 13.52078605991414939 ) ) ;
#37291 = CARTESIAN_POINT ( 'NONE',  ( 10.99306084123000105, 4.495422912016000083, -6.233618171705999522 ) ) ;
#37292 = ORIENTED_EDGE ( 'NONE', *, *, #10872, .T. ) ;
#37293 = CARTESIAN_POINT ( 'NONE',  ( 9.352250488097009651, 2.907725329094806188, -6.870455438679060833 ) ) ;
#37294 = DIRECTION ( 'NONE',  ( 0.000000000000000000, -0.1333333333333049098, -0.9910712498212373989 ) ) ;
#37295 = CARTESIAN_POINT ( 'NONE',  ( 10.29657053952199952, 3.497746311184500190, 8.675184076076000395 ) ) ;
#37296 = CARTESIAN_POINT ( 'NONE',  ( 23.66004879239100234, 0.000000000000000000, 0.000000000000000000 ) ) ;
#37297 = CARTESIAN_POINT ( 'NONE',  ( 7.629823341228000544, 4.763536573491999881, 5.668879554882000349 ) ) ;
#37298 = EDGE_LOOP ( 'NONE', ( #43480, #67721, #56333, #56905 ) ) ;
#37299 = CARTESIAN_POINT ( 'NONE',  ( 11.50001496185000249, 6.312855374401662445, -10.89679704397376447 ) ) ;
#37300 = CARTESIAN_POINT ( 'NONE',  ( 8.096145280407000655, 4.514357753279999663, -8.978030925517998639 ) ) ;
#37301 = CARTESIAN_POINT ( 'NONE',  ( 8.414745334144418720, -2.420441346954531614, 8.227856752513583061 ) ) ;
#37302 = CARTESIAN_POINT ( 'NONE',  ( 9.497405316140000053, -4.271593136661399726, 6.249951378708000327 ) ) ;
#37303 = VERTEX_POINT ( 'NONE', #37272 ) ;
#37304 = CARTESIAN_POINT ( 'NONE',  ( 11.29999334531184552, 11.74553346643965668, 1.558194258341519811 ) ) ;
#37305 = CARTESIAN_POINT ( 'NONE',  ( 11.64596081258699911, 11.57456368445000017, 1.729631387595999881 ) ) ;
#37306 = ORIENTED_EDGE ( 'NONE', *, *, #67686, .F. ) ;
#37307 = CARTESIAN_POINT ( 'NONE',  ( 11.09999999999999964, 4.000000000000000000, -7.500000000000000000 ) ) ;
#37308 = CARTESIAN_POINT ( 'NONE',  ( 13.50018479229300006, 11.60142623882999935, 2.415183939829000259 ) ) ;
#37309 = CARTESIAN_POINT ( 'NONE',  ( 17.63737865760589330, 0.6198980793944587342, -13.88138779565238501 ) ) ;
#37310 = EDGE_CURVE ( 'NONE', #19021, #47311, #48102, .T. ) ;
#37311 = EDGE_CURVE ( 'NONE', #25355, #14617, #26165, .T. ) ;
#37312 = ORIENTED_EDGE ( 'NONE', *, *, #15998, .T. ) ;
#37313 = CARTESIAN_POINT ( 'NONE',  ( 27.09999999999999787, -1.808321269955000243E-12, 9.250000000000000000 ) ) ;
#37314 = PRESENTATION_STYLE_ASSIGNMENT (( #43602 ) ) ;
#37315 = CARTESIAN_POINT ( 'NONE',  ( 10.19809687351667016, -3.672815144550895639, 8.717465845835397076 ) ) ;
#37316 = AXIS2_PLACEMENT_3D ( 'NONE', #19680, #2226, #66185 ) ;
#37317 = CARTESIAN_POINT ( 'NONE',  ( 12.42229329081240152, 2.994506204212079137, -12.32251488760203628 ) ) ;
#37318 = CARTESIAN_POINT ( 'NONE',  ( 11.85502763632550050, -5.160433036184000066, 8.035454525731699604 ) ) ;
#37319 = VERTEX_POINT ( 'NONE', #23954 ) ;
#37320 = CARTESIAN_POINT ( 'NONE',  ( 7.614801658771000348, 3.326263523254000098, 8.794511546544999447 ) ) ;
#37321 = EDGE_LOOP ( 'NONE', ( #55453, #55143, #29784, #24399 ) ) ;
#37322 = CARTESIAN_POINT ( 'NONE',  ( 25.60000000000000142, -9.517611874540000017, 8.103398312166000039 ) ) ;
#37323 = CARTESIAN_POINT ( 'NONE',  ( 15.83043922992600017, -9.441080823466998950, -8.288885697152998944 ) ) ;
#37324 = CARTESIAN_POINT ( 'NONE',  ( 11.01654498872999888, 6.706008375310999803, -5.523030698055999999 ) ) ;
#37325 = VERTEX_POINT ( 'NONE', #44263 ) ;
#37326 = CARTESIAN_POINT ( 'NONE',  ( 12.18014475499754212, -2.522932601087060966, -12.44621172798972353 ) ) ;
#37327 = DIRECTION ( 'NONE',  ( -1.000000000000000000, 0.000000000000000000, 0.000000000000000000 ) ) ;
#37328 = CARTESIAN_POINT ( 'NONE',  ( 23.60000000000000142, 1.954819123156861016, 13.79162281801090195 ) ) ;
#37329 = CARTESIAN_POINT ( 'NONE',  ( 10.88351354018293904, 2.750000000000000000, 7.663624617374469317 ) ) ;
#37330 = CARTESIAN_POINT ( 'NONE',  ( 12.32410271629026255, -1.971482746313082179, -13.86049503924169457 ) ) ;
#37331 = CARTESIAN_POINT ( 'NONE',  ( 10.30903300763299946, -3.402282662142699809, -8.126922218169600143 ) ) ;
#37332 = LINE ( 'NONE', #47486, #1815 ) ;
#37333 = CARTESIAN_POINT ( 'NONE',  ( 18.00816351061650522, -3.042045466722126612, 12.22726353680069344 ) ) ;
#37334 = ORIENTED_EDGE ( 'NONE', *, *, #59255, .T. ) ;
#37335 = CARTESIAN_POINT ( 'NONE',  ( 9.002831022981437670, -8.696154316442465060, 6.348875575362916024 ) ) ;
#37336 = ADVANCED_FACE ( 'NONE', ( #33764 ), #55789, .F. ) ;
#37337 = VERTEX_POINT ( 'NONE', #28166 ) ;
#37338 = DIRECTION ( 'NONE',  ( 0.000000000000000000, 0.000000000000000000, 1.000000000000000000 ) ) ;
#37339 = DIRECTION ( 'NONE',  ( 1.000000000000000000, 0.000000000000000000, 0.000000000000000000 ) ) ;
#37340 = CARTESIAN_POINT ( 'NONE',  ( 11.79999999497874796, -3.261294161473140107, 11.32146851427815193 ) ) ;
#37341 = EDGE_CURVE ( 'NONE', #51168, #7076, #24295, .T. ) ;
#37342 = CARTESIAN_POINT ( 'NONE',  ( 10.05205635875000070, 2.669891600604999748, -8.791543746052999708 ) ) ;
#37343 = CARTESIAN_POINT ( 'NONE',  ( 23.58885774780335609, -10.33110206683957877, -9.338943755861244256 ) ) ;
#37344 = CARTESIAN_POINT ( 'NONE',  ( 24.30001131207184528, 12.15210920089874413, 3.256147846716761940 ) ) ;
#37345 = CARTESIAN_POINT ( 'NONE',  ( 16.39999999231800132, 3.216285993016000155, 11.40340220863999932 ) ) ;
#37346 = CARTESIAN_POINT ( 'NONE',  ( 8.776575450301999481, 3.932070968445029902, -8.439408300974900357 ) ) ;
#37347 = ORIENTED_EDGE ( 'NONE', *, *, #15752, .T. ) ;
#37348 = CARTESIAN_POINT ( 'NONE',  ( 11.55670819615736278, -4.620649663933218854, -6.880644002891320277 ) ) ;
#37349 = CARTESIAN_POINT ( 'NONE',  ( 12.27338658866630716, -2.829189413748181892, 12.36878769217040919 ) ) ;
#37350 = DIRECTION ( 'NONE',  ( 1.000000000000000000, 0.000000000000000000, 0.000000000000000000 ) ) ;
#37351 = CARTESIAN_POINT ( 'NONE',  ( 11.77234208742519961, -4.554746427620499638, 6.627995351445298944 ) ) ;
#37352 = CARTESIAN_POINT ( 'NONE',  ( 7.871384581343000342, 5.129340811002999878, 6.740051537885999977 ) ) ;
#37353 = AXIS2_PLACEMENT_3D ( 'NONE', #26232, #64906, #15046 ) ;
#37354 = CARTESIAN_POINT ( 'NONE',  ( 11.41672066707849886, 4.741156262620799922, -7.051685395375099752 ) ) ;
#37355 = ADVANCED_FACE ( 'NONE', ( #65903 ), #1594, .F. ) ;
#37356 = CARTESIAN_POINT ( 'NONE',  ( 12.79472656276096032, -0.6249999662751115626, 12.67928921590351798 ) ) ;
#37357 = CONICAL_SURFACE ( 'NONE', #30673, 1.349999998858999906, 0.7853981633972997312 ) ;
#37358 = CARTESIAN_POINT ( 'NONE',  ( 8.349704787027532049, 2.649832477958418586, -7.761626529551069353 ) ) ;
#37359 = CARTESIAN_POINT ( 'NONE',  ( 9.447841622600000377, 5.447457912891000120, 7.431328695644999982 ) ) ;
#37360 = CARTESIAN_POINT ( 'NONE',  ( 11.74274107869599959, -3.315287298500999569, 11.22371330986000082 ) ) ;
#37361 = ORIENTED_EDGE ( 'NONE', *, *, #39670, .T. ) ;
#37362 = CARTESIAN_POINT ( 'NONE',  ( 9.517835841233001304, 4.883347899767999323, -6.417062834774999835 ) ) ;
#37363 = CARTESIAN_POINT ( 'NONE',  ( 7.227452085661000503, 0.5737759661892000151, 1.111209200203999936 ) ) ;
#37364 = CARTESIAN_POINT ( 'NONE',  ( 17.81482613222762268, 3.068547461637707308, 13.53623828841520726 ) ) ;
#37365 = CARTESIAN_POINT ( 'NONE',  ( 9.365090231804463983, 2.650133164351947013, -7.500005474590564880 ) ) ;
#37366 = APPLICATION_CONTEXT ( 'automotive_design' ) ;
#37367 = CARTESIAN_POINT ( 'NONE',  ( 10.63652412174386264, 4.781907488123494865, 4.773914205728686966 ) ) ;
#37368 = AXIS2_PLACEMENT_3D ( 'NONE', #13608, #39478, #24432 ) ;
#37369 = CARTESIAN_POINT ( 'NONE',  ( 11.03918313518939875, -4.707599264529200411, -8.394758848575399668 ) ) ;
#37370 = EDGE_LOOP ( 'NONE', ( #56235, #37039, #67219, #8710 ) ) ;
#37371 = CARTESIAN_POINT ( 'NONE',  ( 6.965816936038000229, -1.147328252452000097, 0.8605332073374000190 ) ) ;
#37372 = CARTESIAN_POINT ( 'NONE',  ( 13.73140886085690582, 8.907522817021753525, 7.508769385438491817 ) ) ;
#37375 = DIRECTION ( 'NONE',  ( 1.000000000000000000, 0.000000000000000000, 0.000000000000000000 ) ) ;
#37374 = CARTESIAN_POINT ( 'NONE',  ( 9.550320280412000429, 2.370176859044999862, -6.912649125838000508 ) ) ;
#37373 = UNCERTAINTY_MEASURE_WITH_UNIT (LENGTH_MEASURE( 1.000000000000000082E-05 ), #67587, 'distance_accuracy_value', 'NONE');
#37376 = CARTESIAN_POINT ( 'NONE',  ( 25.26997866307398155, 11.52971827777785307, -2.996576611362720577 ) ) ;
#37377 = ORIENTED_EDGE ( 'NONE', *, *, #12810, .T. ) ;
#37378 = CARTESIAN_POINT ( 'NONE',  ( 11.09425120759000016, 2.431871068503000277, 7.769513029648000391 ) ) ;
#37379 = CARTESIAN_POINT ( 'NONE',  ( 18.11274618065391095, -2.217676902473667777, -13.72925005197111048 ) ) ;
#37380 = CARTESIAN_POINT ( 'NONE',  ( 11.85979573085659844, 4.840012015667699785, 7.354650721737899133 ) ) ;
#37381 = CARTESIAN_POINT ( 'NONE',  ( 10.29378083128999855, -3.483628580733000302, 6.176326635498999629 ) ) ;
#37382 = CARTESIAN_POINT ( 'NONE',  ( 7.149102686541000118, -4.351670788182000038, 8.977200644264000218 ) ) ;
#37383 = ORIENTED_EDGE ( 'NONE', *, *, #20347, .T. ) ;
#37384 = CARTESIAN_POINT ( 'NONE',  ( 9.630961809707432764, -5.349948547046357028, -7.768702954767688240 ) ) ;
#37386 = CARTESIAN_POINT ( 'NONE',  ( 11.05391814679000184, -5.159486550382999859, -8.487149456222999433 ) ) ;
#37385 = CARTESIAN_POINT ( 'NONE',  ( 10.31021345716899873, 4.636538040886300394, -8.078719053813800954 ) ) ;
#37387 = CARTESIAN_POINT ( 'NONE',  ( 7.742845422086257479, -5.491633101817720686, 8.395373286608034391 ) ) ;
#37388 = CARTESIAN_POINT ( 'NONE',  ( 10.96080136920999948, -2.054580854576999904, 7.810082699133999995 ) ) ;
#37389 = DIRECTION ( 'NONE',  ( 0.000000000000000000, -1.000000000000000000, 0.000000000000000000 ) ) ;
#37390 = ORIENTED_EDGE ( 'NONE', *, *, #59428, .F. ) ;
#37391 = CARTESIAN_POINT ( 'NONE',  ( 9.643930206848999376, 5.250000000000000000, -7.500000000000000000 ) ) ;
#37392 = CARTESIAN_POINT ( 'NONE',  ( 12.20379573085659963, -2.893744357957000357, 7.308581953418300081 ) ) ;
#37393 = CARTESIAN_POINT ( 'NONE',  ( 10.88733729122639993, 2.722429312291999803, 7.533608309972310124 ) ) ;
#37394 = PRODUCT_DEFINITION_FORMATION_WITH_SPECIFIED_SOURCE ( 'ANY', '', #3134, .NOT_KNOWN. ) ;
#37395 = ORIENTED_EDGE ( 'NONE', *, *, #63072, .T. ) ;
#37396 = EDGE_CURVE ( 'NONE', #34183, #37319, #2286, .T. ) ;
#37397 = EDGE_CURVE ( 'NONE', #42800, #24493, #19473, .T. ) ;
#37398 = CARTESIAN_POINT ( 'NONE',  ( 9.360279719594000625, 3.031907308384000022, -8.729608011560001657 ) ) ;
#37399 = EDGE_CURVE ( 'NONE', #54794, #66938, #63056, .T. ) ;
#37400 = CARTESIAN_POINT ( 'NONE',  ( 12.38926598778390620, 1.890730539229748652, -12.45733450583996849 ) ) ;
#37401 = CARTESIAN_POINT ( 'NONE',  ( 12.18277869730536977, -4.531392946702499813, 8.547856079839998955 ) ) ;
#37402 = CARTESIAN_POINT ( 'NONE',  ( 25.47111444092800170, -2.702220074950000051, -11.27947351919000063 ) ) ;
#37403 = CARTESIAN_POINT ( 'NONE',  ( 18.06384107466247357, 2.863137910860089175, -13.58970737937452533 ) ) ;
#37404 = VERTEX_POINT ( 'NONE', #13133 ) ;
#37405 = CARTESIAN_POINT ( 'NONE',  ( 11.09999999999999964, -1.300000000000000044, -9.662944685757000940 ) ) ;
#37406 = CARTESIAN_POINT ( 'NONE',  ( 23.98816739749597104, 9.385742420920845319, 9.282132427818025278 ) ) ;
#37407 = ORIENTED_EDGE ( 'NONE', *, *, #42718, .F. ) ;
#37408 = CARTESIAN_POINT ( 'NONE',  ( 9.573096873516668381, 5.217465845835396188, 7.172815144550900968 ) ) ;
#37410 = CARTESIAN_POINT ( 'NONE',  ( 10.60026222744819790, 3.225465054973100099, 6.861998062869400172 ) ) ;
#37409 = VECTOR ( 'NONE', #21712, 1000.000000000000000 ) ;
#37411 = CARTESIAN_POINT ( 'NONE',  ( 11.09999999999999964, -5.299524241844999928, -5.124965750789000296 ) ) ;
#37412 = CARTESIAN_POINT ( 'NONE',  ( 10.47212119989999835, 2.640756834784999896, -8.505248851866998194 ) ) ;
#37413 = CARTESIAN_POINT ( 'NONE',  ( 8.251334741087001490, 4.957169262993001091, 6.172567036706003485 ) ) ;
#37414 = CARTESIAN_POINT ( 'NONE',  ( 9.351499161061999743, -4.821938821912000073, 8.950150764319998231 ) ) ;
#37415 = CARTESIAN_POINT ( 'NONE',  ( 17.55505043854144631, -0.7192913403693169672, -12.57945229203838267 ) ) ;
#37416 = CARTESIAN_POINT ( 'NONE',  ( 9.074999999999999289, 4.417172942406000224, 8.783926296998000538 ) ) ;
#37417 = CARTESIAN_POINT ( 'NONE',  ( 10.94487616594229884, -4.303437140848100029, -6.543508100188799581 ) ) ;
#37418 = CARTESIAN_POINT ( 'NONE',  ( 8.085170280410000743, 2.431401017850999935, 7.958393275880999873 ) ) ;
#37419 = VERTEX_POINT ( 'NONE', #29212 ) ;
#37420 = CARTESIAN_POINT ( 'NONE',  ( 24.71800958153259842, -3.123417170972841106, 11.79150745397447153 ) ) ;
#37421 = CARTESIAN_POINT ( 'NONE',  ( 24.67921430886200085, -8.727631620858000261, -9.158313288899000426 ) ) ;
#37422 = CARTESIAN_POINT ( 'NONE',  ( 11.75750014570500035, 12.43407951582999971, 1.799970604841000021 ) ) ;
#37423 = CARTESIAN_POINT ( 'NONE',  ( 17.95087979294694591, 3.083166700081128475, 12.21696069964854736 ) ) ;
#37424 = CARTESIAN_POINT ( 'NONE',  ( 10.90000000000000036, 0.2500000000000000000, -4.902439024389999567 ) ) ;
#37425 = CARTESIAN_POINT ( 'NONE',  ( 10.95123291824999967, 9.911369087126999489, 5.636315692926999965 ) ) ;
#37426 = CARTESIAN_POINT ( 'NONE',  ( 12.40293124252145418, -0.4784650742344930818, -12.68786664692594535 ) ) ;
#37427 = DIRECTION ( 'NONE',  ( 0.7071067617951957152, 0.000000000000000000, -0.7071068005778986532 ) ) ;
#37428 = VECTOR ( 'NONE', #38634, 1000.000000000000000 ) ;
#37429 = ORIENTED_EDGE ( 'NONE', *, *, #42192, .T. ) ;
#37430 = CARTESIAN_POINT ( 'NONE',  ( 24.70770306079000278, 8.718110200638999885, 9.202866107698000064 ) ) ;
#37431 = CARTESIAN_POINT ( 'NONE',  ( 9.479721904869998994, -3.004358235431599855, -8.058956102599799109 ) ) ;
#37432 = CARTESIAN_POINT ( 'NONE',  ( 13.92027728201558112, -8.815475954240428180, -7.616421984250669297 ) ) ;
#37433 = CARTESIAN_POINT ( 'NONE',  ( 5.599997304680200294, 13.94845324556000143, -4.312847325879000770 ) ) ;
#37434 = CARTESIAN_POINT ( 'NONE',  ( 11.51872200990539952, -4.947480442174099657, 7.830502140005199507 ) ) ;
#37435 = B_SPLINE_SURFACE_WITH_KNOTS ( 'NONE', 3, 3, ( 
 ( #24321, #8242, #8925, #19761 ),
 ( #56478, #29930, #29589, #2987 ),
 ( #28901, #7900, #62403, #45985 ),
 ( #2309, #67297, #23631, #66273 ),
 ( #2648, #45312, #66618, #18740 ),
 ( #61382, #34822, #26037, #36877 ) ),
 .UNSPECIFIED., .F., .F., .F.,
 ( 4, 1, 1, 4 ),
 ( 4, 4 ),
 ( 0.1811037619699999990, 0.3333333333333000081, 0.6666666666667000474, 0.8725156331704999602 ),
 ( -0.1256563615239000009, 1.125656361510000147 ),
 .UNSPECIFIED. ) ;
#37436 = CARTESIAN_POINT ( 'NONE',  ( 10.20641772631199906, 4.431553727090300043, -8.388315195900499788 ) ) ;
#37437 = ADVANCED_FACE ( 'NONE', ( #24979, #41747 ), #4671, .T. ) ;
#37438 = CARTESIAN_POINT ( 'NONE',  ( 12.53842182639420599, 0.6689867242971689887, 12.58222862546947241 ) ) ;
#37439 = CARTESIAN_POINT ( 'NONE',  ( 8.710288521113000115, 3.647046440108700160, 6.715449042252499723 ) ) ;
#37440 = CARTESIAN_POINT ( 'NONE',  ( 9.606444982449859893, 5.179832995385928562, -8.179900027810633745 ) ) ;
#37441 = EDGE_CURVE ( 'NONE', #13672, #67648, #14157, .T. ) ;
#37442 = CARTESIAN_POINT ( 'NONE',  ( 12.48081329218149627, 1.836727633573117080, 12.46541050266128181 ) ) ;
#37444 = CARTESIAN_POINT ( 'NONE',  ( 8.432510841230001830, 5.430400319332999715, 7.210801214872999410 ) ) ;
#37443 = CARTESIAN_POINT ( 'NONE',  ( 9.074455549952999078, 4.888629236328500660, -6.783011486330899231 ) ) ;
#37445 = CARTESIAN_POINT ( 'NONE',  ( 11.69559063708295987, 5.086518862378000883, -7.805482129094999166 ) ) ;
#37446 = CARTESIAN_POINT ( 'NONE',  ( 7.924470805432005882, 3.443171588504001068, -6.303962341916999890 ) ) ;
#37447 = CARTESIAN_POINT ( 'NONE',  ( 10.07762665876999897, 2.169012810937000157, -7.244984731085000185 ) ) ;
#37448 = CARTESIAN_POINT ( 'NONE',  ( 10.06122949779699915, 4.709679768527199606, -8.564302809495998758 ) ) ;
#37450 = CARTESIAN_POINT ( 'NONE',  ( 12.29671722859782079, 2.864281468083856197, 12.35920955626090745 ) ) ;
#37449 = DIRECTION ( 'NONE',  ( 0.000000000000000000, -1.000000000000000000, 0.000000000000000000 ) ) ;
#37451 = CARTESIAN_POINT ( 'NONE',  ( 11.23627509987186102, -4.272452942476324012, -6.249999999999999112 ) ) ;
#37452 = ORIENTED_EDGE ( 'NONE', *, *, #35366, .T. ) ;
#37453 = CARTESIAN_POINT ( 'NONE',  ( 1.119519337369000000, -0.3298644081521999727, -3.242294882329999961 ) ) ;
#37454 = CARTESIAN_POINT ( 'NONE',  ( 10.39393020684999946, 2.750000000000000000, 7.500000000000000000 ) ) ;
#37455 = AXIS2_PLACEMENT_3D ( 'NONE', #28196, #6860, #49510 ) ;
#37456 = CARTESIAN_POINT ( 'NONE',  ( 7.766851002543999627, 2.832432432432000269, 6.822293592207000934 ) ) ;
#37457 = CARTESIAN_POINT ( 'NONE',  ( 11.09999999999999964, -4.000000000000000000, 7.500000000000000000 ) ) ;
#37458 = CARTESIAN_POINT ( 'NONE',  ( 12.41482009541962128, -2.988314721215474812, 13.55768135971568356 ) ) ;
#37459 = CARTESIAN_POINT ( 'NONE',  ( 12.19231142706649429, 2.623190749813627765, 13.64650702413893768 ) ) ;
#37460 = CARTESIAN_POINT ( 'NONE',  ( 8.716851002545999094, -2.832432432432000269, 6.822293592207000934 ) ) ;
#37461 = ORIENTED_EDGE ( 'NONE', *, *, #485, .T. ) ;
#37462 = CARTESIAN_POINT ( 'NONE',  ( 4.637486820977999358, 1.251140238606999855, -0.2478373488106999922 ) ) ;
#37463 = CARTESIAN_POINT ( 'NONE',  ( 18.16451541383442247, 2.360124911612616394, -13.70214797745896895 ) ) ;
#37464 = CARTESIAN_POINT ( 'NONE',  ( 10.26685100253999927, -2.832432432432000269, 6.822293592207000934 ) ) ;
#37465 = CARTESIAN_POINT ( 'NONE',  ( 8.023148997453999343, 5.167567567567999731, -6.822293592207000934 ) ) ;
#37466 = CARTESIAN_POINT ( 'NONE',  ( 18.12629019086303828, 2.246197018143532009, -12.50711533121134167 ) ) ;
#37467 = CARTESIAN_POINT ( 'NONE',  ( 9.129282595918652987, -2.750056606219162703, -7.730023426265350217 ) ) ;
#37468 = CARTESIAN_POINT ( 'NONE',  ( 17.98440366585261074, 2.954302470115874435, 12.33403020158356078 ) ) ;
#37469 = EDGE_CURVE ( 'NONE', #9641, #67407, #11308, .T. ) ;
#37470 = FACE_OUTER_BOUND ( 'NONE', #37052, .T. ) ;
#37471 = CARTESIAN_POINT ( 'NONE',  ( 10.25880564679000173, -2.491773655925000330, -7.289938045981000592 ) ) ;
#37472 = CARTESIAN_POINT ( 'NONE',  ( 4.802943173016458900, 1.199500263597271799, -0.9218200799623701425 ) ) ;
#37473 = EDGE_CURVE ( 'NONE', #64186, #37678, #65225, .T. ) ;
#37474 = DIRECTION ( 'NONE',  ( -0.7071042364840377514, 0.08614528851969455170, 0.7018422814366376272 ) ) ;
#37475 = ADVANCED_FACE ( 'NONE', ( #25666 ), #41062, .F. ) ;
#37476 = CARTESIAN_POINT ( 'NONE',  ( 24.62773497368900166, 12.19918623920000122, 3.045383383698999857 ) ) ;
#37477 = CARTESIAN_POINT ( 'NONE',  ( 11.01053724730969918, -4.948425591258600598, -7.174999999999999822 ) ) ;
#37478 = ORIENTED_EDGE ( 'NONE', *, *, #38625, .T. ) ;
#37479 = CARTESIAN_POINT ( 'NONE',  ( 8.465229719592999302, 2.567871051582000241, -6.869011921437000012 ) ) ;
#37480 = CARTESIAN_POINT ( 'NONE',  ( 11.27672335273219950, -3.698477709264200275, 6.687976048055599421 ) ) ;
#37481 = ORIENTED_EDGE ( 'NONE', *, *, #21607, .F. ) ;
#37482 = CARTESIAN_POINT ( 'NONE',  ( 13.52727141073982331, 12.35275327559081582, 2.070326479558311839 ) ) ;
#37483 = CARTESIAN_POINT ( 'NONE',  ( 11.16225954179439839, -3.122605388210700106, -8.229019074832200076 ) ) ;
#37485 = ORIENTED_EDGE ( 'NONE', *, *, #44458, .T. ) ;
#37484 = B_SPLINE_CURVE_WITH_KNOTS ( 'NONE', 3,
 ( #67456, #13998, #51730, #35324, #25163, #45807, #8744, #66087, #56641, #51394, #23790, #60853, #40224, #2807, #34293, #8404, #67118, #45468, #61540, #55614, #29055, #50366, #19228, #3489, #19581, #2466, #45125, #66432, #62222, #13656, #18554, #14341, #40554, #61201, #13320, #34644, #55954, #29749, #51051, #24134, #66783, #46837, #36342, #19921, #21290, #14680 ),
 .UNSPECIFIED., .F., .F.,
 ( 4, 2, 2, 2, 2, 2, 2, 2, 2, 2, 2, 2, 2, 2, 1, 2, 2, 2, 2, 2, 1, 2, 2, 4 ),
 ( 0.000000000000000000, 0.06247329711058760560, 0.09370994566588143615, 0.1249465942211752667, 0.1405649184988197742, 0.1561832427764643094, 0.1874198913317580151, 0.2030382156094048540, 0.2186565398870516930, 0.2264657020258750708, 0.2342748641646984209, 0.2498931884423491734, 0.2811298369976507061, 0.2889389991364761379, 0.2967481612753015141, 0.3123664855529522666, 0.3279848098306030746, 0.3436031341082538271, 0.3748397826635555541, 0.3904581069412053074, 0.4060764312188550051, 0.4373130797741529019, 0.4685497283294507986, 0.4997863768847486954 ),
 .UNSPECIFIED. ) ;
#37486 = CARTESIAN_POINT ( 'NONE',  ( 11.84388784977539899, 2.744254309011999737, 7.571757098260779806 ) ) ;
#37487 = CARTESIAN_POINT ( 'NONE',  ( 23.99448051247391334, 3.345746474086601641, -12.75760653321332327 ) ) ;
#37488 = VECTOR ( 'NONE', #38037, 1000.000000000000000 ) ;
#37489 = CARTESIAN_POINT ( 'NONE',  ( 9.957462135714001406, -5.100000000000000533, -6.571291218949999902 ) ) ;
#37490 = CARTESIAN_POINT ( 'NONE',  ( 10.44635971519499940, -3.540377183549800133, -6.735384833238199143 ) ) ;
#37491 = CARTESIAN_POINT ( 'NONE',  ( 12.76469414194129115, 0.6249999999999995559, -13.88107975724710741 ) ) ;
#37492 = CARTESIAN_POINT ( 'NONE',  ( 11.44749694427000186, 3.679776032594999968, -11.11060924501999914 ) ) ;
#37493 = CARTESIAN_POINT ( 'NONE',  ( 13.69055856039300068, 11.42191202915999781, 2.091365271848000251 ) ) ;
#37494 = VERTEX_POINT ( 'NONE', #67964 ) ;
#37495 = CARTESIAN_POINT ( 'NONE',  ( 9.120035841232999374, 5.288433695693000480, -8.041290150997999930 ) ) ;
#37496 = VERTEX_POINT ( 'NONE', #66936 ) ;
#37497 = EDGE_CURVE ( 'NONE', #31811, #65585, #13813, .T. ) ;
#37498 = B_SPLINE_CURVE_WITH_KNOTS ( 'NONE', 3,
 ( #6723, #1488, #54975, #24192, #40960, #45183, #3213, #7770, #2521, #29807, #24540, #35382, #3886, #25220, #14054, #41306, #56703, #29461, #14403, #62615, #35719, #56356, #46211, #13374, #66490, #29112, #18611, #57036, #62283, #66839, #67174, #67518, #23848, #9138, #3544, #8804, #34699, #39939, #50769, #61257, #67860, #30143, #50418, #45865, #46557, #35042, #19985, #56010, #14737, #24881, #18950, #30474, #45528, #2863, #8117, #36056, #40279, #61596, #13713, #51789, #8462, #19288, #51110, #40613, #61941, #51450, #19639, #15073, #26606, #16443, #21348, #68893, #53166, #48261, #64321, #37426, #47588, #68542, #9824, #36399, #62950, #4921, #63298, #31172, #15764, #57716, #43018, #42675, #25569, #57370, #25909, #52474, #4572 ),
 .UNSPECIFIED., .F., .F.,
 ( 4, 2, 2, 2, 2, 2, 2, 2, 2, 1, 1, 2, 2, 2, 2, 2, 2, 2, 2, 2, 2, 2, 2, 2, 2, 2, 2, 2, 2, 2, 2, 2, 2, 1, 1, 2, 2, 2, 2, 1, 2, 2, 2, 2, 2, 2, 2, 2, 4 ),
 ( 0.000000000000000000, 0.03124999999998657324, 0.06249999999997314648, 0.09374999999995972666, 0.1093749999999517192, 0.1249999999999437117, 0.1562499999999277522, 0.1718749999999209244, 0.1874999999999141242, 0.2031249999999072964, 0.2109374999999048816, 0.2148437499999037159, 0.2187499999999025779, 0.2499999999998959166, 0.2656249999998932521, 0.2734374999998928080, 0.2812499999998923084, 0.2968749999998929190, 0.3124999999998935296, 0.3437499999998948619, 0.3593749999998955835, 0.3749999999998963052, 0.4062499999998969158, 0.4374999999998974709, 0.4999999999998985256, 0.5312499999998990807, 0.5624999999998996358, 0.5937499999999001910, 0.6093749999999005240, 0.6249999999999007461, 0.6562499999999023004, 0.6718749999999037437, 0.6874999999999050759, 0.7031249999999065192, 0.7109374999999072964, 0.7148437499999084066, 0.7187499999999094058, 0.7499999999999189537, 0.7656249999999230615, 0.7734374999999250599, 0.7773437499999261702, 0.7812499999999272804, 0.7968749999999314992, 0.8124999999999358291, 0.8437499999999442668, 0.8593749999999483746, 0.8749999999999525935, 0.9374999999999763522, 1.000000000000000000 ),
 .UNSPECIFIED. ) ;
#37499 = VECTOR ( 'NONE', #27399, 1000.000000000000000 ) ;
#37500 = CARTESIAN_POINT ( 'NONE',  ( 0.2212347920160371018, 2.507835299313069477, -2.070680120134882785 ) ) ;
#37501 = VERTEX_POINT ( 'NONE', #68300 ) ;
#37502 = CARTESIAN_POINT ( 'NONE',  ( 7.400000000000000355, 0.000000000000000000, 0.000000000000000000 ) ) ;
#37503 = CARTESIAN_POINT ( 'NONE',  ( 18.16680584898033146, -2.371606440122840276, -12.48054868302275366 ) ) ;
#37504 = AXIS2_PLACEMENT_3D ( 'NONE', #68018, #47748, #42499 ) ;
#37505 = CARTESIAN_POINT ( 'NONE',  ( 24.99828499555314565, -8.543280344662843362, 8.328740866081538741 ) ) ;
#37506 = CARTESIAN_POINT ( 'NONE',  ( 4.599999999999999645, -0.7192913403693023122, 12.57945229203838267 ) ) ;
#37507 = CARTESIAN_POINT ( 'NONE',  ( 18.18005044388383240, -2.499999700414728743, -12.45156116530568902 ) ) ;
#37508 = CARTESIAN_POINT ( 'NONE',  ( 12.18402495282434472, 0.07112389991331898031, 13.89976024287835799 ) ) ;
#37509 = ORIENTED_EDGE ( 'NONE', *, *, #60920, .F. ) ;
#37510 = CARTESIAN_POINT ( 'NONE',  ( 12.26982956731400165, 11.56648533137999912, -4.655999611355000845 ) ) ;
#37511 = CARTESIAN_POINT ( 'NONE',  ( 17.61881199949500143, 11.55156539432999985, -4.942255484049000280 ) ) ;
#37512 = CARTESIAN_POINT ( 'NONE',  ( 9.505520750864626223, 3.872956735472087964, 8.365674464137100586 ) ) ;
#37513 = CARTESIAN_POINT ( 'NONE',  ( 5.196297656737999482, 0.2173479397978999861, 1.166870994638999903 ) ) ;
#37514 = CARTESIAN_POINT ( 'NONE',  ( 9.743314158772999889, 5.149303692842000402, -5.987168472229000393 ) ) ;
#37515 = CARTESIAN_POINT ( 'NONE',  ( 18.16350100824700320, -3.138009765975000143, 11.88148072165000002 ) ) ;
#37516 = CARTESIAN_POINT ( 'NONE',  ( 10.06728329455999926, -4.192861215955000276, -5.985050974557999837 ) ) ;
#37517 = ORIENTED_EDGE ( 'NONE', *, *, #24482, .T. ) ;
#37518 = ORIENTED_EDGE ( 'NONE', *, *, #57825, .T. ) ;
#37519 = CARTESIAN_POINT ( 'NONE',  ( 8.921135841230999119, 3.292387953886000140, -6.294868737226000377 ) ) ;
#37520 = EDGE_CURVE ( 'NONE', #66492, #46708, #43016, .T. ) ;
#37521 = CARTESIAN_POINT ( 'NONE',  ( 10.16000000000000014, 4.496968146123999865, -8.755198255949000696 ) ) ;
#37522 = CARTESIAN_POINT ( 'NONE',  ( 17.79083366726184678, -1.825854556040602095, 13.88043960113447284 ) ) ;
#37523 = CYLINDRICAL_SURFACE ( 'NONE', #20145, 2.000000000000000000 ) ;
#37524 = CARTESIAN_POINT ( 'NONE',  ( 0.1499942179680000265, 2.402872127494068533, -1.384928887584814028 ) ) ;
#37525 = CARTESIAN_POINT ( 'NONE',  ( 11.09999999999999964, 5.299999999999999822, 6.469505845987999493 ) ) ;
#37526 = CARTESIAN_POINT ( 'NONE',  ( 9.763317406968999634, 4.161254277581000416, -8.351883209406098629 ) ) ;
#37528 = CARTESIAN_POINT ( 'NONE',  ( 8.344265712141698543, 4.916725855472337869, -6.188913847335090423 ) ) ;
#37527 = CARTESIAN_POINT ( 'NONE',  ( 9.952380199233999747, -3.003429752324399793, 7.625259896924899472 ) ) ;
#37529 = ORIENTED_EDGE ( 'NONE', *, *, #3016, .T. ) ;
#37530 = B_SPLINE_CURVE_WITH_KNOTS ( 'NONE', 3,
 ( #15240, #49036, #63115, #32958 ),
 .UNSPECIFIED., .F., .F.,
 ( 4, 4 ),
 ( 0.000000000000000000, 1.000000000000000000 ),
 .UNSPECIFIED. ) ;
#37531 = CARTESIAN_POINT ( 'NONE',  ( 9.215289122285998502, -4.861979632688999686, 8.938813901364000003 ) ) ;
#37532 = CARTESIAN_POINT ( 'NONE',  ( 9.668897997121000287, -4.730747404809998891, -8.668230005597001409 ) ) ;
#37533 = CARTESIAN_POINT ( 'NONE',  ( 9.893930206848999376, -5.250000000000000000, 7.500000000000000000 ) ) ;
#37534 = CARTESIAN_POINT ( 'NONE',  ( 10.09196524370999981, -3.841385669346000231, 5.536421174581999338 ) ) ;
#37535 = CARTESIAN_POINT ( 'NONE',  ( 18.15150620829238548, 2.686947401609460329, -12.40607332099752469 ) ) ;
#37536 = CARTESIAN_POINT ( 'NONE',  ( 11.09999999999999964, -2.700000000000000178, -5.157071250680000496 ) ) ;
#37537 = DIRECTION ( 'NONE',  ( 1.000000000000000000, 0.000000000000000000, -3.330080301313000417E-14 ) ) ;
#37538 = CARTESIAN_POINT ( 'NONE',  ( 9.332721904869998752, -3.243980311826100138, -7.924431591189499358 ) ) ;
#37539 = AXIS2_PLACEMENT_3D ( 'NONE', #2148, #18224, #7038 ) ;
#37540 = CARTESIAN_POINT ( 'NONE',  ( 5.879775144119999908, -0.03703453004475999732, -1.321780775251000017 ) ) ;
#37541 = CARTESIAN_POINT ( 'NONE',  ( 7.000000000000000000, 8.307879248642999315, -4.307879248643000203 ) ) ;
#37542 = CARTESIAN_POINT ( 'NONE',  ( 0.1499942179680000542, -2.199046806507067853, -1.689975037551103121 ) ) ;
#37543 = ORIENTED_EDGE ( 'NONE', *, *, #51522, .T. ) ;
#37544 = CARTESIAN_POINT ( 'NONE',  ( 12.22015141286114392, -0.2205037192104029042, -12.69742880170240085 ) ) ;
#37545 = CARTESIAN_POINT ( 'NONE',  ( 17.55505043854144276, -0.7302158263239199032, -13.98094363220830871 ) ) ;
#37546 = CARTESIAN_POINT ( 'NONE',  ( 24.34832162658637600, 3.224867771844263320, -12.03537037221818728 ) ) ;
#37547 = CARTESIAN_POINT ( 'NONE',  ( 25.31010614027100303, -8.472730232543000284, 8.045075953992999018 ) ) ;
#37548 = CARTESIAN_POINT ( 'NONE',  ( 10.19837725606034162, 4.679950664087191292, -8.679651447172831880 ) ) ;
#37549 = ORIENTED_EDGE ( 'NONE', *, *, #65257, .F. ) ;
#37550 = CARTESIAN_POINT ( 'NONE',  ( 7.527700667618229424, -5.079562351722092473, 8.329181850972373624 ) ) ;
#37551 = EDGE_CURVE ( 'NONE', #23998, #34256, #6356, .T. ) ;
#37552 = CONTEXT_DEPENDENT_SHAPE_REPRESENTATION ( #57894, #48368 ) ;
#37553 = EDGE_CURVE ( 'NONE', #40048, #67932, #56312, .T. ) ;
#37554 = CARTESIAN_POINT ( 'NONE',  ( 11.56833327354034857, -4.746587807672299597, -7.011667014989399149 ) ) ;
#37555 = DIRECTION ( 'NONE',  ( -1.000000000000000000, 0.000000000000000000, -1.233561263588000078E-14 ) ) ;
#37556 = CARTESIAN_POINT ( 'NONE',  ( 23.60000000000000142, 2.258942858049999725, 12.29419282279000036 ) ) ;
#37557 = LINE ( 'NONE', #4701, #54027 ) ;
#37558 = CARTESIAN_POINT ( 'NONE',  ( 10.40480513895999870, 4.779740423663599636, -7.066537524675499782 ) ) ;
#37559 = ORIENTED_EDGE ( 'NONE', *, *, #6394, .F. ) ;
#37560 = CARTESIAN_POINT ( 'NONE',  ( 10.44675369521999997, -2.885048926231000177, 8.863479194807000638 ) ) ;
#37561 = CARTESIAN_POINT ( 'NONE',  ( 8.749283493600000128, -3.910012670022149806, -8.350279134800100422 ) ) ;
#37562 = VERTEX_POINT ( 'NONE', #46659 ) ;
#37563 = CARTESIAN_POINT ( 'NONE',  ( 11.01978213580999899, -2.731808064604999586, 4.996583140031000347 ) ) ;
#37564 = CARTESIAN_POINT ( 'NONE',  ( 7.968183059622999664, -2.280579276705999803, 6.510290672242000198 ) ) ;
#37565 = CARTESIAN_POINT ( 'NONE',  ( 9.120514158775000269, 5.306366356490000769, -7.996450761531000317 ) ) ;
#37566 = ORIENTED_EDGE ( 'NONE', *, *, #5781, .T. ) ;
#37567 = CARTESIAN_POINT ( 'NONE',  ( 6.470987436302001683, 0.1781225934829054336, 1.521768030474604627 ) ) ;
#37568 = CARTESIAN_POINT ( 'NONE',  ( 6.967235841227999771, 4.499022151374000522, -9.333214642871000777 ) ) ;
#37569 = FACE_OUTER_BOUND ( 'NONE', #15982, .T. ) ;
#37570 = CARTESIAN_POINT ( 'NONE',  ( 7.881896300820000256, 5.128252728555000139, 6.737017011364999419 ) ) ;
#37571 = EDGE_LOOP ( 'NONE', ( #56088, #20452, #31911, #28643 ) ) ;
#37572 = CARTESIAN_POINT ( 'NONE',  ( 11.11845396862999991, -5.767021056207999763, 7.178419201465000121 ) ) ;
#37573 = DIRECTION ( 'NONE',  ( 0.000000000000000000, 1.000000000000000000, -1.290201028711000169E-14 ) ) ;
#37574 = CARTESIAN_POINT ( 'NONE',  ( 11.13220574173981170, 5.136173005413450454, -6.911917091190552753 ) ) ;
#37575 = VERTEX_POINT ( 'NONE', #67613 ) ;
#37576 = ADVANCED_FACE ( 'NONE', ( #16889 ), #11640, .T. ) ;
#37577 = AXIS2_PLACEMENT_3D ( 'NONE', #59081, #11182, #5587 ) ;
#37578 = CARTESIAN_POINT ( 'NONE',  ( 8.929547492598356229, 4.733899445644309978, -8.304419251562590532 ) ) ;
#37579 = CARTESIAN_POINT ( 'NONE',  ( 10.57656694038000111, -5.344897889496000865, -7.298883676216999739 ) ) ;
#37580 = VERTEX_POINT ( 'NONE', #471 ) ;
#37581 = CARTESIAN_POINT ( 'NONE',  ( 4.990308476675333615, -0.1973919536007287812, 1.504917372998084701 ) ) ;
#37582 = CARTESIAN_POINT ( 'NONE',  ( 17.79030838958610872, -1.799800542995207309, -12.47079474911150143 ) ) ;
#37583 = EDGE_CURVE ( 'NONE', #56175, #25126, #43894, .T. ) ;
#37584 = CARTESIAN_POINT ( 'NONE',  ( 4.955910294413000017, -1.341011414409000180, 0.4561942916552000349 ) ) ;
#37585 = CARTESIAN_POINT ( 'NONE',  ( 11.60000000000000320, 5.139199170149531426, -7.074412716661199418 ) ) ;
#37586 = CARTESIAN_POINT ( 'NONE',  ( 15.90567905817900218, 3.588626488247999902, 11.74852861413999960 ) ) ;
#37587 = CARTESIAN_POINT ( 'NONE',  ( 11.25158531382730054, 4.272452942476326676, 8.749999999999998224 ) ) ;
#37588 = LINE ( 'NONE', #191, #22072 ) ;
#37589 = CIRCLE ( 'NONE', #53211, 0.7499999936418002555 ) ;
#37590 = B_SPLINE_CURVE_WITH_KNOTS ( 'NONE', 3,
 ( #43469, #38912, #66160, #49387 ),
 .UNSPECIFIED., .F., .F.,
 ( 4, 4 ),
 ( 0.000000000000000000, 1.000000000000000000 ),
 .UNSPECIFIED. ) ;
#37591 = EDGE_LOOP ( 'NONE', ( #40191, #38995, #51003, #49729 ) ) ;
#37592 = CARTESIAN_POINT ( 'NONE',  ( 8.734020077949999461, 3.936452720224709712, -8.378811912355599745 ) ) ;
#37593 = ORIENTED_EDGE ( 'NONE', *, *, #24191, .F. ) ;
#37594 = CARTESIAN_POINT ( 'NONE',  ( 10.39106065309000115, 4.025321035224999733, 9.261125884460000179 ) ) ;
#37595 = CARTESIAN_POINT ( 'NONE',  ( 10.72128915877000033, 4.673511966357999370, -5.778393480304000462 ) ) ;
#37596 = B_SPLINE_CURVE_WITH_KNOTS ( 'NONE', 3,
 ( #64811, #59927, #53990, #43159, #43857, #17280, #23219, #1899, #7475, #16588, #44567, #43514, #28474, #33371, #65859, #65158, #59580, #12037, #33719, #22174, #54333, #64465, #28829 ),
 .UNSPECIFIED., .F., .F.,
 ( 4, 2, 2, 1, 2, 2, 2, 2, 1, 1, 2, 2, 4 ),
 ( 0.000000000000000000, 0.2500000000000036082, 0.3750000000000054401, 0.4375000000000017208, 0.4687499999999983347, 0.4999999999999949485, 0.6249999999999795719, 0.6874999999999711342, 0.7187499999999680256, 0.7343749999999659162, 0.7421874999999619194, 0.7499999999999579225, 1.000000000000000000 ),
 .UNSPECIFIED. ) ;
#37597 = CARTESIAN_POINT ( 'NONE',  ( 17.98957057434314066, -12.09691025065527903, 3.246626905778224881 ) ) ;
#37598 = CIRCLE ( 'NONE', #52118, 13.17499999999999893 ) ;
#37599 = CARTESIAN_POINT ( 'NONE',  ( 12.39034978066170645, 2.032288297489022177, -13.76160266677045563 ) ) ;
#37600 = DIRECTION ( 'NONE',  ( -1.055605809059559446E-16, -0.9835354258236025382, 0.1807154286440004198 ) ) ;
#37601 = SURFACE_STYLE_FILL_AREA ( #31336 ) ;
#37602 = CARTESIAN_POINT ( 'NONE',  ( 17.83221471278435999, -0.5605600754933578456, 13.88478672247769730 ) ) ;
#37603 = CARTESIAN_POINT ( 'NONE',  ( 11.50000000000000000, -5.058572498595999889, 7.174999999999999822 ) ) ;
#37604 = ORIENTED_EDGE ( 'NONE', *, *, #55932, .F. ) ;
#37605 = EDGE_CURVE ( 'NONE', #47308, #25728, #10578, .T. ) ;
#37606 = CARTESIAN_POINT ( 'NONE',  ( 12.42340929153268902, 0.4950008743410382883, 13.88813607082127355 ) ) ;
#37607 = CARTESIAN_POINT ( 'NONE',  ( 11.92887348028849992, -5.124210964533999935, 6.892162778124999889 ) ) ;
#37608 = CARTESIAN_POINT ( 'NONE',  ( 18.08719402094173034, -0.3285636530950700740, -13.89479065952098935 ) ) ;
#37609 = CARTESIAN_POINT ( 'NONE',  ( 7.577019353207000485, -5.480312458445999901, 8.192326492433998908 ) ) ;
#37611 = CARTESIAN_POINT ( 'NONE',  ( 10.26685100253999927, -2.832432432432000269, 6.822293592207000934 ) ) ;
#37610 = CARTESIAN_POINT ( 'NONE',  ( 10.59344747867000081, 5.297752619853000944, 8.474195539311001113 ) ) ;
#37612 = CARTESIAN_POINT ( 'NONE',  ( 10.62072335273219892, 4.397090433355999473, -8.569396700949999612 ) ) ;
#37613 = DIRECTION ( 'NONE',  ( -1.000000000000000000, 0.000000000000000000, 0.000000000000000000 ) ) ;
#37614 = CARTESIAN_POINT ( 'NONE',  ( 9.475696787962998968, 4.148886440911999429, -6.645868410478299459 ) ) ;
#37615 = CARTESIAN_POINT ( 'NONE',  ( 18.15598060823833038, -0.1720826094844742082, 12.69843621396828226 ) ) ;
#37616 = CARTESIAN_POINT ( 'NONE',  ( 7.057926398363000509, -1.325960607972999750, 0.7529263492304999472 ) ) ;
#37617 = LINE ( 'NONE', #220, #13158 ) ;
#37618 = EDGE_LOOP ( 'NONE', ( #47951, #43353, #28510, #65952, #35674, #4088, #708, #65857, #4565, #23457, #60789, #33281 ) ) ;
#37619 = CARTESIAN_POINT ( 'NONE',  ( 9.214144353209000826, -5.421531391267000011, 6.381128921159999301 ) ) ;
#37620 = CARTESIAN_POINT ( 'NONE',  ( 9.269689158774999882, 3.135494838036999798, -8.598037907310999373 ) ) ;
#37621 = CARTESIAN_POINT ( 'NONE',  ( 5.599999999371999770, -1.300000000000000044, 9.662944685757000940 ) ) ;
#37622 = FACE_OUTER_BOUND ( 'NONE', #12817, .T. ) ;
#37623 = ORIENTED_EDGE ( 'NONE', *, *, #15083, .T. ) ;
#37624 = AXIS2_PLACEMENT_3D ( 'NONE', #55325, #17927, #44845 ) ;
#37625 = CARTESIAN_POINT ( 'NONE',  ( 13.49980696792483137, -11.54838492169068331, -4.420196298692892434 ) ) ;
#37626 = PRESENTATION_LAYER_ASSIGNMENT (  '', '', ( #18685 ) ) ;
#37627 = CARTESIAN_POINT ( 'NONE',  ( 11.11123293495519881, 3.108594079907299967, 7.535834283667469435 ) ) ;
#37628 = CARTESIAN_POINT ( 'NONE',  ( 11.14451084122999980, 5.035416949823999566, -8.381520599479999944 ) ) ;
#37629 = ORIENTED_EDGE ( 'NONE', *, *, #32381, .F. ) ;
#37630 = CARTESIAN_POINT ( 'NONE',  ( 5.263359839683333874, 1.310679582531388387, -0.7554284705563470981 ) ) ;
#37631 = CARTESIAN_POINT ( 'NONE',  ( 11.14975833414749928, -4.796537143354000499, -7.825000000000000178 ) ) ;
#37632 = CARTESIAN_POINT ( 'NONE',  ( 17.67439832720110005, 3.190335184669548241, -12.18941280901077739 ) ) ;
#37633 = LINE ( 'NONE', #58967, #15288 ) ;
#37635 = CARTESIAN_POINT ( 'NONE',  ( 7.795982780410000146, 3.164805384346000228, 9.104735843897000080 ) ) ;
#37634 = AXIS2_PLACEMENT_3D ( 'NONE', #62530, #14649, #45778 ) ;
#37636 = VERTEX_POINT ( 'NONE', #64775 ) ;
#37637 = CARTESIAN_POINT ( 'NONE',  ( 8.710288521113000115, 3.647046440108700160, 6.715449042252499723 ) ) ;
#37638 = EDGE_CURVE ( 'NONE', #26116, #19641, #30515, .T. ) ;
#37639 = ADVANCED_FACE ( 'NONE', ( #36851 ), #45191, .F. ) ;
#37640 = B_SPLINE_CURVE_WITH_KNOTS ( 'NONE', 3,
 ( #59464, #26637, #47954, #32905 ),
 .UNSPECIFIED., .F., .F.,
 ( 4, 4 ),
 ( 0.000000000000000000, 1.000000000000000000 ),
 .UNSPECIFIED. ) ;
#37641 = CARTESIAN_POINT ( 'NONE',  ( 7.060779719589000081, 3.391196421714000042, -9.121921547671998809 ) ) ;
#37642 = CARTESIAN_POINT ( 'NONE',  ( 8.296621455525475142, -4.598534371660971232, 9.142000767755396495 ) ) ;
#37643 = AXIS2_PLACEMENT_3D ( 'NONE', #46499, #67803, #41248 ) ;
#37644 = EDGE_CURVE ( 'NONE', #61281, #11902, #55529, .T. ) ;
#37645 = CARTESIAN_POINT ( 'NONE',  ( 10.87068169682078178, -3.126090202221432079, -7.480731692978241476 ) ) ;
#37646 = EDGE_LOOP ( 'NONE', ( #41517, #30612, #1342, #35655, #15341 ) ) ;
#37647 = CARTESIAN_POINT ( 'NONE',  ( 16.04506009312500225, -3.874776422117000241, -11.85383417895000058 ) ) ;
#37648 = CARTESIAN_POINT ( 'NONE',  ( 6.188359839683334584, -0.7554284705563480973, -1.310679582531387277 ) ) ;
#37649 = VERTEX_POINT ( 'NONE', #61278 ) ;
#37650 = FACE_OUTER_BOUND ( 'NONE', #59053, .T. ) ;
#37651 = CARTESIAN_POINT ( 'NONE',  ( 18.29983863916000075, -2.861762957209999847, 11.98830831200999825 ) ) ;
#37652 = CARTESIAN_POINT ( 'NONE',  ( 17.77562957671592869, 0.5851376999905949505, -13.88342059653408533 ) ) ;
#37653 = ORIENTED_EDGE ( 'NONE', *, *, #24242, .T. ) ;
#37654 = CARTESIAN_POINT ( 'NONE',  ( 11.11532707317000046, -8.027733648058999805, 6.810713678640000879 ) ) ;
#37655 = CARTESIAN_POINT ( 'NONE',  ( 10.63263472587000180, 7.502444384430999591, 6.008454772957000145 ) ) ;
#37656 = VECTOR ( 'NONE', #30970, 1000.000000000000000 ) ;
#37657 = CARTESIAN_POINT ( 'NONE',  ( 10.64902344389989963, 3.116469856398800253, -6.963800219468099684 ) ) ;
#37658 = CARTESIAN_POINT ( 'NONE',  ( 11.29997960521317957, 3.569935952926198031, -11.29784959202355488 ) ) ;
#37659 = CARTESIAN_POINT ( 'NONE',  ( 11.33810672858430024, -5.021298157087000114, 8.268288002587098617 ) ) ;
#37660 = ORIENTED_EDGE ( 'NONE', *, *, #67944, .F. ) ;
#37661 = CARTESIAN_POINT ( 'NONE',  ( 9.272295280408998863, 3.705846972803000128, 9.096435887808000942 ) ) ;
#37662 = ORIENTED_EDGE ( 'NONE', *, *, #59063, .F. ) ;
#37663 = ADVANCED_FACE ( 'NONE', ( #17242 ), #1165, .T. ) ;
#37664 = CARTESIAN_POINT ( 'NONE',  ( 9.129428851719998406, 5.099284414202999827, 6.151604790022999758 ) ) ;
#37665 = CARTESIAN_POINT ( 'NONE',  ( 16.13494720760600032, -9.102952917978999636, -8.658486291235998777 ) ) ;
#37666 = CARTESIAN_POINT ( 'NONE',  ( 10.96506373917000055, 5.561809752472999691, -4.905726767165999647 ) ) ;
#37667 = EDGE_LOOP ( 'NONE', ( #41837, #35820, #19610, #9695 ) ) ;
#37668 = CARTESIAN_POINT ( 'NONE',  ( 12.30608813017797409, -2.123066299447895044, -12.53144042021394178 ) ) ;
#37669 = ADVANCED_FACE ( 'NONE', ( #59887, #11996 ), #54650, .T. ) ;
#37670 = DIRECTION ( 'NONE',  ( 0.5000000000000169864, 0.000000000000000000, -0.8660254037844288266 ) ) ;
#37671 = PLANE ( 'NONE',  #53873 ) ;
#37672 = DIRECTION ( 'NONE',  ( -1.000000000000000000, 0.000000000000000000, -1.776356839426000147E-14 ) ) ;
#37673 = CARTESIAN_POINT ( 'NONE',  ( 12.61605721975967498, -1.812633401299081903, -13.88216159563417307 ) ) ;
#37674 = B_SPLINE_CURVE_WITH_KNOTS ( 'NONE', 3,
 ( #66263, #28180, #34123, #23966 ),
 .UNSPECIFIED., .F., .F.,
 ( 4, 4 ),
 ( 0.000000000000000000, 1.000000000000000000 ),
 .UNSPECIFIED. ) ;
#37675 = CARTESIAN_POINT ( 'NONE',  ( 10.87103032197929942, -3.416314376401300201, -6.683751296690399357 ) ) ;
#37676 = CARTESIAN_POINT ( 'NONE',  ( 7.130360733670636719, 1.109723905055048920, -0.6386155440974740083 ) ) ;
#37677 = CARTESIAN_POINT ( 'NONE',  ( 18.08628618592430826, -2.970581112497159282, 12.24483314193593131 ) ) ;
#37678 = VERTEX_POINT ( 'NONE', #49398 ) ;
#37679 = CARTESIAN_POINT ( 'NONE',  ( 11.84388784977539899, -5.255745690988000263, -7.428242901739219306 ) ) ;
#37680 = ORIENTED_EDGE ( 'NONE', *, *, #36951, .T. ) ;
#37681 = VECTOR ( 'NONE', #7378, 1000.000000000000000 ) ;
#37682 = CARTESIAN_POINT ( 'NONE',  ( 11.42397234076999979, -12.13750352647000064, -1.893412522203000048 ) ) ;
#37683 = CARTESIAN_POINT ( 'NONE',  ( 13.00000000005200107, 12.15994572112000149, 2.000334444851999738 ) ) ;
#37684 = CARTESIAN_POINT ( 'NONE',  ( 10.43284001513000092, 3.279325423736999756, -9.029279369994000604 ) ) ;
#37685 = CARTESIAN_POINT ( 'NONE',  ( 12.79999999824000589, -12.03389405692475478, 3.206111686008664918 ) ) ;
#37686 = COLOUR_RGB ( '', 0.09019608, 0.27058824, 0.51372549) ;
#37687 = CARTESIAN_POINT ( 'NONE',  ( 18.14129716922916558, 2.282346377865474008, -12.49966253006683381 ) ) ;
#37688 = CARTESIAN_POINT ( 'NONE',  ( 7.859795284898003942, 2.854589328742001886, -6.788356039251000063 ) ) ;
#37689 = CARTESIAN_POINT ( 'NONE',  ( 10.50285691784999997, 5.158890929072000198, 8.369954994793999958 ) ) ;
#37690 = ORIENTED_EDGE ( 'NONE', *, *, #5284, .F. ) ;
#37691 = AXIS2_PLACEMENT_3D ( 'NONE', #14246, #46057, #35231 ) ;
#37692 = CARTESIAN_POINT ( 'NONE',  ( 18.44504292973000048, 2.664685748803000021, 11.39637496735000077 ) ) ;
#37693 = CARTESIAN_POINT ( 'NONE',  ( 9.566963020987998334, 5.215925787220999865, 6.177726425586999248 ) ) ;
#37694 = CARTESIAN_POINT ( 'NONE',  ( 23.66004879239100234, 3.393652551760000247, -13.50507492672999987 ) ) ;
#37695 = CARTESIAN_POINT ( 'NONE',  ( 11.52812378248509795, -4.416893162838900544, 8.288725998710999576 ) ) ;
#37696 = CARTESIAN_POINT ( 'NONE',  ( 17.89159592529800236, 3.376698609984999599, -11.11057657535000054 ) ) ;
#37697 = AXIS2_PLACEMENT_3D ( 'NONE', #6861, #13508, #39727 ) ;
#37698 = CARTESIAN_POINT ( 'NONE',  ( 11.12958489392000061, 8.838800255109999782, -6.730293042198999487 ) ) ;
#37699 = CARTESIAN_POINT ( 'NONE',  ( 12.20981273398931499, -0.1908418880314488031, 12.69807545005479810 ) ) ;
#37700 = EDGE_CURVE ( 'NONE', #52892, #37325, #38923, .T. ) ;
#37701 = EDGE_CURVE ( 'NONE', #4545, #62414, #68020, .T. ) ;
#37702 = CARTESIAN_POINT ( 'NONE',  ( 23.73828294872599898, -9.840026834037999492, -9.652156658315000470 ) ) ;
#37703 = CARTESIAN_POINT ( 'NONE',  ( 10.15000066238999921, -1.190159082397999942E-13, -1.213918169242000045E-13 ) ) ;
#37704 = AXIS2_PLACEMENT_3D ( 'NONE', #24096, #39141, #8020 ) ;
#37705 = B_SPLINE_SURFACE_WITH_KNOTS ( 'NONE', 3, 3, ( 
 ( #62007, #437, #32270, #22097 ),
 ( #92, #10237, #16511, #10926 ),
 ( #64048, #63714, #58819, #64738 ),
 ( #37493, #58137, #42744, #47652 ),
 ( #37840, #27356, #21077, #16168 ),
 ( #25978, #48678, #21751, #37156 ),
 ( #27013, #59161, #53579, #5672 ),
 ( #48330, #21410, #31572, #58475 ),
 ( #9896, #10580, #43085, #64390 ),
 ( #11265, #42060, #31919, #52891 ) ),
 .UNSPECIFIED., .F., .F., .F.,
 ( 4, 1, 1, 1, 1, 1, 1, 4 ),
 ( 4, 4 ),
 ( 0.04183311431308000400, 0.1428571428570999946, 0.2857142857143000203, 0.4285714285713999594, 0.5714285714286000406, 0.7142857142856999797, 0.8571428571429000609, 0.9292981235707000742 ),
 ( -0.1917799910644999994, 1.191756862851000021 ),
 .UNSPECIFIED. ) ;
#37706 = EDGE_LOOP ( 'NONE', ( #35100, #22672, #31124, #25467 ) ) ;
#37707 = DIRECTION ( 'NONE',  ( -0.7071063750894808209, 0.7071071872833809557, -1.205032604263965641E-09 ) ) ;
#37708 = CARTESIAN_POINT ( 'NONE',  ( 7.061411423934999654, 0.6837059483940000071, -1.047162964378999916 ) ) ;
#37709 = CARTESIAN_POINT ( 'NONE',  ( 18.16473232272955229, 2.360987313248031239, 13.70192779769509528 ) ) ;
#37710 = CARTESIAN_POINT ( 'NONE',  ( 24.36958145701300182, 8.861545501478000020, -8.807436093351999062 ) ) ;
#37711 = CARTESIAN_POINT ( 'NONE',  ( 10.54687750876899877, -4.617914354660699772, -8.458891008702400072 ) ) ;
#37712 = ORIENTED_EDGE ( 'NONE', *, *, #18338, .F. ) ;
#37713 = CARTESIAN_POINT ( 'NONE',  ( 6.998282674564999972, -1.401716800305999877, -2.564925509195000141E-10 ) ) ;
#37714 = CARTESIAN_POINT ( 'NONE',  ( 9.362885841227999606, 3.677414437776999723, 9.250745771096999803 ) ) ;
#37716 = CARTESIAN_POINT ( 'NONE',  ( 10.89393020684959978, -5.250000000000000000, -7.500000000000000000 ) ) ;
#37715 = CARTESIAN_POINT ( 'NONE',  ( 9.699495280410998177, 5.048004622677000341, -6.120508709481000231 ) ) ;
#37717 = CARTESIAN_POINT ( 'NONE',  ( 10.63445696039368116, 3.217964742311511195, 4.772905834338354580 ) ) ;
#37718 = ORIENTED_EDGE ( 'NONE', *, *, #59386, .T. ) ;
#37719 = CARTESIAN_POINT ( 'NONE',  ( 10.98286939055999945, 3.998514186275999638, 9.091062412789998604 ) ) ;
#37720 = CARTESIAN_POINT ( 'NONE',  ( 18.22207129059747288, -2.231684076289582208, -13.82098807703153476 ) ) ;
#37721 = CARTESIAN_POINT ( 'NONE',  ( 10.87103032197929942, 4.583685623598699799, 8.316248703309600643 ) ) ;
#37722 = CARTESIAN_POINT ( 'NONE',  ( 10.81579453138999902, -5.374572909254000663, 6.698726302909000729 ) ) ;
#37723 = CARTESIAN_POINT ( 'NONE',  ( 7.229683059621999419, -2.630475685621000093, 6.995953627589999613 ) ) ;
#37724 = ORIENTED_EDGE ( 'NONE', *, *, #49130, .F. ) ;
#37725 = CARTESIAN_POINT ( 'NONE',  ( 24.66122485234200212, 12.38509973078999948, -2.963735973613000230 ) ) ;
#37726 = AXIS2_PLACEMENT_3D ( 'NONE', #27702, #16507, #44487 ) ;
#37727 = EDGE_CURVE ( 'NONE', #47262, #19317, #60934, .T. ) ;
#37728 = ADVANCED_FACE ( 'NONE', ( #7098 ), #23970, .F. ) ;
#37730 = CARTESIAN_POINT ( 'NONE',  ( 11.19050685320999960, -2.516759970060999940, -6.840363309917000478 ) ) ;
#37729 = CYLINDRICAL_SURFACE ( 'NONE', #54610, 1.250000000000000222 ) ;
#37731 = CARTESIAN_POINT ( 'NONE',  ( 7.753453601445883692, -5.352470295837787440, 8.593756411513149729 ) ) ;
#37732 = CARTESIAN_POINT ( 'NONE',  ( 9.629020610622001541, -5.794331084664000819, 7.414872097535999629 ) ) ;
#37733 = CARTESIAN_POINT ( 'NONE',  ( 1.547746615352999955, -3.258362327980000028, 0.06604197684371000687 ) ) ;
#37734 = ORIENTED_EDGE ( 'NONE', *, *, #49582, .F. ) ;
#37735 = CARTESIAN_POINT ( 'NONE',  ( 24.99826494465212434, -11.48456307779601637, -3.234320738292375097 ) ) ;
#37736 = ADVANCED_FACE ( 'NONE', ( #52148 ), #14758, .F. ) ;
#37737 = CARTESIAN_POINT ( 'NONE',  ( 11.32179975933729921, -3.051121678931899783, 7.826467126457498757 ) ) ;
#37738 = CARTESIAN_POINT ( 'NONE',  ( 10.71503032197929883, 4.743378537856500543, 8.539569492647999027 ) ) ;
#37739 = ORIENTED_EDGE ( 'NONE', *, *, #66088, .T. ) ;
#37740 = CARTESIAN_POINT ( 'NONE',  ( 8.912754719595000097, 2.481540185810000132, -7.878707153279001396 ) ) ;
#37741 = CARTESIAN_POINT ( 'NONE',  ( 12.21279934347909801, 2.064970636307569052, -12.42964156345203719 ) ) ;
#37742 = CARTESIAN_POINT ( 'NONE',  ( 11.55435090131019926, -2.880552878538999995, 6.807613609764599616 ) ) ;
#37743 = ORIENTED_EDGE ( 'NONE', *, *, #41271, .T. ) ;
#37744 = CARTESIAN_POINT ( 'NONE',  ( 7.947155777501817120, 4.876130771725635249, -6.371895583161996335 ) ) ;
#37745 = CARTESIAN_POINT ( 'NONE',  ( 18.08128123658401520, 2.837338021505997343, -13.59610410465670682 ) ) ;
#37746 = VERTEX_POINT ( 'NONE', #40630 ) ;
#37747 = CARTESIAN_POINT ( 'NONE',  ( 8.368316940379001423, -4.780993534312999671, 6.267212032957000467 ) ) ;
#37748 = CARTESIAN_POINT ( 'NONE',  ( 5.721693173017332157, 0.7554284705563509839, -1.310679582531386167 ) ) ;
#37749 = ORIENTED_EDGE ( 'NONE', *, *, #40469, .T. ) ;
#37750 = CARTESIAN_POINT ( 'NONE',  ( 12.34734069910711263, -3.038294257956349664, -12.22819623478419260 ) ) ;
#37751 = ADVANCED_FACE ( 'NONE', ( #66857 ), #14077, .F. ) ;
#37752 = CARTESIAN_POINT ( 'NONE',  ( 11.26487482311540056, 4.930401445321599851, 7.124095752359899336 ) ) ;
#37753 = CARTESIAN_POINT ( 'NONE',  ( 10.19255830160000009, 2.560287027313000063, 7.664549200117999561 ) ) ;
#37754 = CARTESIAN_POINT ( 'NONE',  ( 10.32702465212000043, 5.663794543395000325, -6.682030833630000721 ) ) ;
#37755 = CYLINDRICAL_SURFACE ( 'NONE', #37577, 11.50000000000000178 ) ;
#37756 = CARTESIAN_POINT ( 'NONE',  ( 9.500008250440000523, -2.279684233303000074, 7.877691491255999878 ) ) ;
#37757 = CARTESIAN_POINT ( 'NONE',  ( 17.78855914542206307, -0.6810629908227162632, -12.58158054216573696 ) ) ;
#37758 = VECTOR ( 'NONE', #25868, 1000.000000000000114 ) ;
#37759 = DIRECTION ( 'NONE',  ( 0.7071068468348109537, 0.000000000000000000, -0.7071067155382779745 ) ) ;
#37760 = CARTESIAN_POINT ( 'NONE',  ( 11.16641369783139837, -4.050626550392200542, -8.502191501283999031 ) ) ;
#37761 = CARTESIAN_POINT ( 'NONE',  ( 9.395323341230000125, 5.146726419831999522, 6.597424767138000412 ) ) ;
#37762 = ORIENTED_EDGE ( 'NONE', *, *, #18254, .T. ) ;
#37763 =( NAMED_UNIT ( * ) SI_UNIT ( $, .STERADIAN. ) SOLID_ANGLE_UNIT ( ) );
#37764 = CARTESIAN_POINT ( 'NONE',  ( 24.63609268136318420, -3.161156455721329195, 11.86232637917242627 ) ) ;
#37765 = CARTESIAN_POINT ( 'NONE',  ( 9.254613120524085801, 2.734600818827677582, 7.018933991638915515 ) ) ;
#37766 = CARTESIAN_POINT ( 'NONE',  ( 16.39999999308669842, 3.302282894619416265, 11.70823727156336425 ) ) ;
#37767 = PRODUCT_DEFINITION_SHAPE ( 'NONE', 'NONE',  #69203 ) ;
#37768 = CARTESIAN_POINT ( 'NONE',  ( 18.26479085099338562, 2.332519703358803209, 12.38222476794584814 ) ) ;
#37769 = CARTESIAN_POINT ( 'NONE',  ( 11.12373268272000004, 6.329904650298000313, 5.418930548134000880 ) ) ;
#37770 = FACE_OUTER_BOUND ( 'NONE', #1068, .T. ) ;
#37771 = DIRECTION ( 'NONE',  ( 1.000000000000000000, 0.000000000000000000, 0.000000000000000000 ) ) ;
#37772 = CARTESIAN_POINT ( 'NONE',  ( 9.843930206850000530, -5.250000000000000000, -7.500000000000000000 ) ) ;
#37773 = ORIENTED_EDGE ( 'NONE', *, *, #9295, .T. ) ;
#37774 = CARTESIAN_POINT ( 'NONE',  ( 12.10652924560090860, -2.286704390305614787, 12.39076728011198547 ) ) ;
#37775 = B_SPLINE_CURVE_WITH_KNOTS ( 'NONE', 3,
 ( #2915, #45237, #45914, #9529, #66542, #41361, #13428, #30192, #30872, #52186, #14107, #61307, #9186, #24593, #56057, #61995, #3937, #51498 ),
 .UNSPECIFIED., .F., .F.,
 ( 4, 2, 2, 2, 2, 2, 2, 2, 4 ),
 ( 0.000000000000000000, 0.1250000000000000000, 0.2500000000000000000, 0.3750000000000000000, 0.5000000000000000000, 0.6250000000000000000, 0.7500000000000000000, 0.8750000000000000000, 1.000000000000000000 ),
 .UNSPECIFIED. ) ;
#37776 = CARTESIAN_POINT ( 'NONE',  ( 9.074455549952999078, -3.111370763671500228, -6.783011486330899231 ) ) ;
#37777 = CARTESIAN_POINT ( 'NONE',  ( 7.773264358664000007, -2.859518314699000197, 6.768377407145999669 ) ) ;
#37778 = CARTESIAN_POINT ( 'NONE',  ( 10.56492304196000021, -4.212244324161999565, 8.933470634735002136 ) ) ;
#37779 = CARTESIAN_POINT ( 'NONE',  ( 11.14949279009019989, -4.260984538213099526, 6.531063508962500208 ) ) ;
#37780 = CARTESIAN_POINT ( 'NONE',  ( 11.48225819896749833, 2.879005208331999910, -7.711331004020999913 ) ) ;
#37781 = CARTESIAN_POINT ( 'NONE',  ( 12.14465108362473877, 0.2970375428997805711, 12.59650273238872487 ) ) ;
#37782 = ADVANCED_FACE ( 'NONE', ( #3905 ), #41666, .F. ) ;
#37783 = EDGE_CURVE ( 'NONE', #59809, #13672, #38943, .T. ) ;
#37784 = CARTESIAN_POINT ( 'NONE',  ( 0.1538438179258999894, 2.601420761213999899, -2.147952162500999851 ) ) ;
#37785 = CARTESIAN_POINT ( 'NONE',  ( 9.679376605108515719, 4.176514373757539644, -8.850130121363157798 ) ) ;
#37786 = VECTOR ( 'NONE', #56126, 1000.000000000000000 ) ;
#37787 = CARTESIAN_POINT ( 'NONE',  ( 12.30801118402048111, 2.879457308712139785, 12.35502813289141599 ) ) ;
#37788 = CARTESIAN_POINT ( 'NONE',  ( 25.60000000000000142, 10.55164198324999880, 3.754898126455999741 ) ) ;
#37789 = CARTESIAN_POINT ( 'NONE',  ( 10.64533863405319991, 4.703785194191100416, -8.397761948794601139 ) ) ;
#37790 = CARTESIAN_POINT ( 'NONE',  ( 8.339994183033994091, 2.871570486036998382, -6.342248726812004911 ) ) ;
#37791 = CARTESIAN_POINT ( 'NONE',  ( 10.08211611373999972, 4.728047954991999369, -8.793974144431000894 ) ) ;
#37792 = CARTESIAN_POINT ( 'NONE',  ( 24.30000000000000071, 10.83443035398000021, -3.855530949778000149 ) ) ;
#37794 = CARTESIAN_POINT ( 'NONE',  ( 18.06407908469787316, -0.3627935497759613437, 12.69302875402486741 ) ) ;
#37793 = CARTESIAN_POINT ( 'NONE',  ( 9.777068864297932649, 2.899999999999999911, -6.444141223371950389 ) ) ;
#37795 = FACE_OUTER_BOUND ( 'NONE', #25911, .T. ) ;
#37796 = EDGE_LOOP ( 'NONE', ( #64181, #41161, #7692, #39434 ) ) ;
#37797 = AXIS2_PLACEMENT_3D ( 'NONE', #69040, #4369, #26749 ) ;
#37798 = CARTESIAN_POINT ( 'NONE',  ( 12.28050398199685134, 0.3399395274153702573, 12.69387965975142407 ) ) ;
#37799 = CARTESIAN_POINT ( 'NONE',  ( 9.669776904377568982, -2.899999999999999911, -6.174048679210142332 ) ) ;
#37800 = CARTESIAN_POINT ( 'NONE',  ( 11.92270903091197987, -11.93179002798757615, 3.810633631265414767 ) ) ;
#37801 = CARTESIAN_POINT ( 'NONE',  ( 9.019772138681998896, 3.677371150249499898, 8.304747519296199698 ) ) ;
#37802 = B_SPLINE_CURVE_WITH_KNOTS ( 'NONE', 3,
 ( #14182, #57161, #46687, #14863, #20447, #19766, #41774, #51915, #56483, #3336, #36530, #51574, #67991, #45990, #25694, #14529, #41091, #47372 ),
 .UNSPECIFIED., .F., .F.,
 ( 4, 2, 2, 2, 2, 2, 2, 2, 4 ),
 ( 0.000000000000000000, 0.1250000000000000278, 0.2500000000000000000, 0.3749999999999999445, 0.4999999999999999445, 0.6249999999999998890, 0.7499999999999998890, 0.8750000000000000000, 1.000000000000000000 ),
 .UNSPECIFIED. ) ;
#37803 = B_SPLINE_CURVE_WITH_KNOTS ( 'NONE', 3,
 ( #35639, #57280, #46120, #56610 ),
 .UNSPECIFIED., .F., .F.,
 ( 4, 4 ),
 ( 0.000000000000000000, 1.000000000000000000 ),
 .UNSPECIFIED. ) ;
#37804 = CARTESIAN_POINT ( 'NONE',  ( 12.24916914324846573, -2.049138926831462815, 13.84922804760273607 ) ) ;
#37805 = CARTESIAN_POINT ( 'NONE',  ( 10.87581074856900010, -5.172583146916752028, 6.999756549658378901 ) ) ;
#37806 = LINE ( 'NONE', #59127, #67871 ) ;
#37807 = VERTEX_POINT ( 'NONE', #43041 ) ;
#37808 = FACE_OUTER_BOUND ( 'NONE', #36008, .T. ) ;
#37809 = AXIS2_PLACEMENT_3D ( 'NONE', #55838, #2349, #8288 ) ;
#37810 = PLANE ( 'NONE',  #55330 ) ;
#37811 = DIRECTION ( 'NONE',  ( 1.000000000000000000, 0.000000000000000000, 0.000000000000000000 ) ) ;
#37812 = CARTESIAN_POINT ( 'NONE',  ( 18.23289209645828990, -3.217460216940595696, 11.19708622233677175 ) ) ;
#37813 = EDGE_CURVE ( 'NONE', #14861, #28055, #33957, .T. ) ;
#37814 = CARTESIAN_POINT ( 'NONE',  ( 18.11622138774303892, 2.775899412256286336, -12.38303361670991443 ) ) ;
#37815 = CARTESIAN_POINT ( 'NONE',  ( 9.762620115047001335, -4.656877754660387225, 8.575407073603340535 ) ) ;
#37816 = CARTESIAN_POINT ( 'NONE',  ( 10.99826088462129903, 4.001843064679911244, 8.366195817038299509 ) ) ;
#37817 = FACE_OUTER_BOUND ( 'NONE', #3327, .T. ) ;
#37818 = CARTESIAN_POINT ( 'NONE',  ( 10.29666814679000097, -2.755511079787000384, -6.622434938646999392 ) ) ;
#37819 = CARTESIAN_POINT ( 'NONE',  ( 11.08380555355832620, -3.999999927290649460, -9.033895164528411570 ) ) ;
#37820 = CARTESIAN_POINT ( 'NONE',  ( 18.30000000000000071, 2.818741034879777008, -11.83575128182368452 ) ) ;
#37821 = CARTESIAN_POINT ( 'NONE',  ( 24.19015592859265951, 9.083557491131649897, -9.071480578485305202 ) ) ;
#37822 = CARTESIAN_POINT ( 'NONE',  ( 11.00000000000000000, -4.968589424331200100, -7.174999999999999822 ) ) ;
#37823 = ORIENTED_EDGE ( 'NONE', *, *, #23375, .T. ) ;
#37824 = CARTESIAN_POINT ( 'NONE',  ( 9.541460841232000334, 2.824732249080000202, -8.992748220058999209 ) ) ;
#37825 = CARTESIAN_POINT ( 'NONE',  ( 11.35056919669530018, -3.169300617545700138, 7.254567470917099747 ) ) ;
#37826 = VERTEX_POINT ( 'NONE', #36770 ) ;
#37827 = CARTESIAN_POINT ( 'NONE',  ( 17.63808658539560170, -3.119809217581025251, 13.52227901589168901 ) ) ;
#37828 = CARTESIAN_POINT ( 'NONE',  ( 10.44841638348500013, -5.108333310975999630, -7.230023356477299323 ) ) ;
#37829 = VERTEX_POINT ( 'NONE', #59116 ) ;
#37830 = CARTESIAN_POINT ( 'NONE',  ( 10.73213259636989925, 3.092475607087700418, 7.005495010505599751 ) ) ;
#37831 = CARTESIAN_POINT ( 'NONE',  ( 6.261564796991104132, -0.7389267608984831925, 0.8596156481332365429 ) ) ;
#37832 = EDGE_CURVE ( 'NONE', #43973, #46125, #5628, .T. ) ;
#37833 = CARTESIAN_POINT ( 'NONE',  ( 10.36180282789683638, -2.874603711584070354, -6.749639981064813554 ) ) ;
#37834 = CARTESIAN_POINT ( 'NONE',  ( 10.02314899745999988, -5.167567567567999731, -6.822293592207000934 ) ) ;
#37835 = DIRECTION ( 'NONE',  ( 1.000000000000000000, 0.000000000000000000, 0.000000000000000000 ) ) ;
#37836 = CARTESIAN_POINT ( 'NONE',  ( 12.23148617192921073, -0.2485195352517245160, -13.89701485918576296 ) ) ;
#37837 = CARTESIAN_POINT ( 'NONE',  ( 5.500000000000000000, -0.5000000000000000000, -9.662944685757000940 ) ) ;
#37838 = CIRCLE ( 'NONE', #45688, 12.42499880353999941 ) ;
#37839 = CARTESIAN_POINT ( 'NONE',  ( 11.01003172897000049, -3.180716007396000133, -6.283809484240999943 ) ) ;
#37840 = CARTESIAN_POINT ( 'NONE',  ( 13.58722619340700177, 11.45202530529999940, 1.920069653109999885 ) ) ;
#37841 = ORIENTED_EDGE ( 'NONE', *, *, #3319, .F. ) ;
#37842 = DIRECTION ( 'NONE',  ( 0.000000000000000000, 0.000000000000000000, 1.000000000000000000 ) ) ;
#37843 = ORIENTED_EDGE ( 'NONE', *, *, #52477, .T. ) ;
#37844 = CARTESIAN_POINT ( 'NONE',  ( 10.28774346735000123, 5.077605961126000267, -5.991341245382999503 ) ) ;
#37845 = SURFACE_SIDE_STYLE ('',( #42750 ) ) ;
#37846 = ORIENTED_EDGE ( 'NONE', *, *, #62426, .T. ) ;
#37847 = LINE ( 'NONE', #28404, #62692 ) ;
#37848 = CARTESIAN_POINT ( 'NONE',  ( 17.82007478097248665, -3.066051200070172289, -12.30148382826351572 ) ) ;
#37849 = CARTESIAN_POINT ( 'NONE',  ( 10.40299135172147693, 4.795252583382552558, 7.862853843651285146 ) ) ;
#37850 = CARTESIAN_POINT ( 'NONE',  ( 9.050000000000000711, -7.679126935408000065, -5.093340497782000043 ) ) ;
#37851 = B_SPLINE_SURFACE_WITH_KNOTS ( 'NONE', 3, 3, ( 
 ( #67978, #30588, #52250, #31281, #4686, #56818, #51558, #4346, #62396, #68662, #41762, #3998, #20779, #3656, #24994, #47012, #14514, #51899, #25336, #46672, #58872, #143, #27761, #38580, #32315, #6069, #48038, #54311, #26725, #22493, #48733, #27404, #11313, #43136, #16900 ),
 ( #10977, #12012, #835, #22150, #65135, #15873, #6760, #21461, #42795, #43492, #64439, #49071, #53286, #16563, #64103, #42452, #63763, #16217, #37540, #38231, #53628, #5722, #64789, #27065, #59905, #48381, #6412, #59557, #488, #21802, #11657, #37890, #17256, #59210, #32652 ),
 ( #32997, #33348, #47702, #53963, #1183, #43835, #54664, #69013, #21126, #37205, #58523, #10628, #31974, #5386, #2224, #7455, #55358, #14352, #23538, #28806, #38937, #19936, #18303, #40913, #50117, #39279, #66183, #62235, #24836, #14692, #67812, #60948, #1876, #9093, #2555 ),
 ( #36010, #3836, #39627, #34391, #34045, #62572, #1523, #28100, #46510, #44878, #60601, #65488, #35677, #13062, #49413, #55708, #17961, #7806, #29147, #57326, #56991, #49765, #30432, #51743, #12711, #22843, #50454, #46163, #41257, #17614, #44190, #23194, #7114, #67471, #19593 ) ),
 .UNSPECIFIED., .F., .F., .F.,
 ( 4, 4 ),
 ( 4, 1, 1, 1, 1, 1, 1, 1, 1, 1, 1, 1, 1, 1, 1, 1, 1, 1, 1, 1, 1, 1, 1, 1, 1, 1, 1, 1, 1, 1, 1, 1, 4 ),
 ( -0.02636945251836000231, 1.026369452518000047 ),
 ( -0.02000000000000000042, 0.01250000000000000069, 0.04499999999999999833, 0.07749999999999999944, 0.1100000000000000006, 0.1424999999999999878, 0.1749999999999999889, 0.2074999999999999900, 0.2399999999999999911, 0.2725000000000000200, 0.3049999999999999933, 0.3375000000000000222, 0.3699999999999999956, 0.4025000000000000244, 0.4349999999999999978, 0.4675000000000000266, 0.5000000000000000000, 0.5324999999999999734, 0.5649999999999999467, 0.5975000000000000311, 0.6300000000000000044, 0.6624999999999999778, 0.6949999999999999512, 0.7275000000000000355, 0.7600000000000000089, 0.7924999999999999822, 0.8249999999999999556, 0.8575000000000000400, 0.8900000000000000133, 0.9224999999999999867, 0.9549999999999999600, 0.9875000000000000444, 1.020000000000000018 ),
 .UNSPECIFIED. ) ;
#37852 = CARTESIAN_POINT ( 'NONE',  ( 11.24052627608000066, -2.774025043188999895, 6.782107572692000375 ) ) ;
#37853 = CARTESIAN_POINT ( 'NONE',  ( 5.500000000000000000, 0.000000000000000000, 0.000000000000000000 ) ) ;
#37854 = CARTESIAN_POINT ( 'NONE',  ( 12.18201982513761372, 0.05063168410658506341, 13.89988098555966012 ) ) ;
#37855 = ORIENTED_EDGE ( 'NONE', *, *, #38201, .T. ) ;
#37856 = CARTESIAN_POINT ( 'NONE',  ( 7.137771682458000200, 5.278582711742999756, -7.933273873238999130 ) ) ;
#37857 = CARTESIAN_POINT ( 'NONE',  ( 17.61698155344500094, 11.49709674579000129, -4.820194475709000059 ) ) ;
#37858 = B_SPLINE_CURVE_WITH_KNOTS ( 'NONE', 3,
 ( #29872, #24945, #41026, #62348 ),
 .UNSPECIFIED., .F., .F.,
 ( 4, 4 ),
 ( 0.000000000000000000, 0.5000000000000044409 ),
 .UNSPECIFIED. ) ;
#37859 = CARTESIAN_POINT ( 'NONE',  ( 10.30371347217102596, 4.589291630936049415, 6.869346568680468224 ) ) ;
#37860 = CARTESIAN_POINT ( 'NONE',  ( 4.339059043195999443, 0.6480827609324999461, -1.333028937737999797 ) ) ;
#37861 = CARTESIAN_POINT ( 'NONE',  ( 9.892489158770999325, 5.099602161831000124, -9.049221499261999924 ) ) ;
#37862 = CARTESIAN_POINT ( 'NONE',  ( 17.82671363066053871, 12.11440107311990211, -3.181008590938710245 ) ) ;
#37863 = CARTESIAN_POINT ( 'NONE',  ( 10.82564972918999935, -5.331162346451000289, -8.542142527201001201 ) ) ;
#37864 = EDGE_CURVE ( 'NONE', #2054, #95, #29535, .T. ) ;
#37865 = EDGE_CURVE ( 'NONE', #16664, #10274, #48843, .T. ) ;
#37866 = ORIENTED_EDGE ( 'NONE', *, *, #62391, .T. ) ;
#37867 = B_SPLINE_CURVE_WITH_KNOTS ( 'NONE', 3,
 ( #25958, #68247, #18993, #13756 ),
 .UNSPECIFIED., .F., .F.,
 ( 4, 4 ),
 ( 0.000000000000000000, 1.000000000000000000 ),
 .UNSPECIFIED. ) ;
#37868 = CARTESIAN_POINT ( 'NONE',  ( 21.59999987243000064, 1.172395514003999961E-13, 13.89999852641997613 ) ) ;
#37869 = DIRECTION ( 'NONE',  ( 1.000000000000000000, 0.000000000000000000, 0.000000000000000000 ) ) ;
#37870 = CARTESIAN_POINT ( 'NONE',  ( 10.90437023801000116, -5.099522774867000230, 5.132565236215000049 ) ) ;
#37871 = EDGE_CURVE ( 'NONE', #18819, #44093, #28797, .T. ) ;
#37872 = ADVANCED_FACE ( 'NONE', ( #48978 ), #30605, .F. ) ;
#37873 = LINE ( 'NONE', #6739, #36921 ) ;
#37874 = CARTESIAN_POINT ( 'NONE',  ( 5.865443173016668510, 1.500000000000000000, 0.1963495408493652339 ) ) ;
#37875 = FACE_OUTER_BOUND ( 'NONE', #7729, .T. ) ;
#37876 = CARTESIAN_POINT ( 'NONE',  ( 9.356038493598999750, 4.726907342723099426, -6.806856425099999441 ) ) ;
#37878 = CARTESIAN_POINT ( 'NONE',  ( 4.399712213706658659, 0.7365302470552868019, -1.068880257431492398 ) ) ;
#37877 = CARTESIAN_POINT ( 'NONE',  ( 9.899709346416999622, -3.216804796119200116, 7.871904849557299855 ) ) ;
#37879 = CARTESIAN_POINT ( 'NONE',  ( 7.428159769834000059, -3.524402284009999331, 6.653317709399996005 ) ) ;
#37880 = ORIENTED_EDGE ( 'NONE', *, *, #37813, .F. ) ;
#37881 = CARTESIAN_POINT ( 'NONE',  ( 11.51145123989532948, 4.605239108938600445, 6.331134574721999364 ) ) ;
#37882 = CARTESIAN_POINT ( 'NONE',  ( 10.34020413671000149, -4.202027362542999356, 9.459588031742001135 ) ) ;
#37883 = CARTESIAN_POINT ( 'NONE',  ( 9.380417874594000338, 2.822750429186000165, 6.999532383170999239 ) ) ;
#37884 = CARTESIAN_POINT ( 'NONE',  ( 5.500000000000000000, -12.87590651766999983, -2.791353855799999728 ) ) ;
#37885 = CARTESIAN_POINT ( 'NONE',  ( 10.37373728961999930, -2.215269876326000364, 7.703982265807999497 ) ) ;
#37886 = CARTESIAN_POINT ( 'NONE',  ( 23.58885196634466297, -13.25333333387674273, 4.277492436922254448 ) ) ;
#37887 = CARTESIAN_POINT ( 'NONE',  ( 25.34480063931457394, 11.16380230704550591, -3.340454812006480978 ) ) ;
#37888 = EDGE_CURVE ( 'NONE', #30450, #58602, #54567, .T. ) ;
#37889 = CARTESIAN_POINT ( 'NONE',  ( 9.837292290062999101, -3.131390070940299974, -6.995659746333000584 ) ) ;
#37890 = CARTESIAN_POINT ( 'NONE',  ( 5.224388989100000380, -1.212815126404999999, 0.5269083208682000530 ) ) ;
#37891 = CARTESIAN_POINT ( 'NONE',  ( 10.85376078907948028, -3.141705924399422312, 7.334408124199476298 ) ) ;
#37892 = PLANE ( 'NONE',  #45115 ) ;
#37893 = ORIENTED_EDGE ( 'NONE', *, *, #34022, .F. ) ;
#37894 = CARTESIAN_POINT ( 'NONE',  ( 12.79472656276095854, 0.6249999662751102303, -12.67928921590352154 ) ) ;
#37895 = CARTESIAN_POINT ( 'NONE',  ( 10.77672335273219950, 4.301522290735800169, -8.312023951944400579 ) ) ;
#37896 = DIRECTION ( 'NONE',  ( 0.000000000000000000, 0.000000000000000000, 1.000000000000000000 ) ) ;
#37897 = CARTESIAN_POINT ( 'NONE',  ( 7.933148997457998952, -5.167567567567999731, 6.822293592207000934 ) ) ;
#37898 = CARTESIAN_POINT ( 'NONE',  ( 1.030140132541691678, 3.408904368339106483, -0.9161175952574748260 ) ) ;
#37899 = ORIENTED_EDGE ( 'NONE', *, *, #8989, .F. ) ;
#37900 = CARTESIAN_POINT ( 'NONE',  ( 7.641998701183679188, -3.319571644187112813, 8.680369833195172191 ) ) ;
#37901 = CARTESIAN_POINT ( 'NONE',  ( 10.69568717260499824, -4.466067913030199676, -8.260703168378098482 ) ) ;
#37902 = CARTESIAN_POINT ( 'NONE',  ( 18.18005043824377154, 1.329526366183796371E-10, 12.70000000088145420 ) ) ;
#37903 = CONICAL_SURFACE ( 'NONE', #27895, 1.150068028907000661, 0.7854495265279701766 ) ;
#37904 = CARTESIAN_POINT ( 'NONE',  ( 10.48976354018275003, -3.672815144550900524, 6.282534154164604701 ) ) ;
#37905 = CARTESIAN_POINT ( 'NONE',  ( 10.97028665956023197, 3.257584962274628904, -8.549395343567624650 ) ) ;
#37906 = CARTESIAN_POINT ( 'NONE',  ( 10.28014141025500017, 4.417352327511700594, -8.243346240911998635 ) ) ;
#37907 = EDGE_LOOP ( 'NONE', ( #28, #66631, #46661, #55141, #31726, #68479 ) ) ;
#37908 = CARTESIAN_POINT ( 'NONE',  ( 10.85738557828999973, -2.754556666341999804, 8.976367391363998749 ) ) ;
#37909 = CARTESIAN_POINT ( 'NONE',  ( 9.099999886593998610, 3.268496584495999908E-13, 3.613587358477999789E-14 ) ) ;
#37910 = ORIENTED_EDGE ( 'NONE', *, *, #24021, .F. ) ;
#37911 = DIRECTION ( 'NONE',  ( -0.7071063294819032174, 0.7071072328909032700, -8.604691786090042874E-10 ) ) ;
#37912 = CARTESIAN_POINT ( 'NONE',  ( 17.80000000009400196, 3.216307036143000175, 11.40341376487999980 ) ) ;
#37913 = EDGE_CURVE ( 'NONE', #8238, #60967, #45513, .T. ) ;
#37914 = CARTESIAN_POINT ( 'NONE',  ( 9.717214158771000143, 3.990126737362999609, -8.809457313313998839 ) ) ;
#37915 = ORIENTED_EDGE ( 'NONE', *, *, #23349, .T. ) ;
#37916 = CARTESIAN_POINT ( 'NONE',  ( 6.437855742029999107, 0.7705900885230198005, 1.324272068856591211 ) ) ;
#37917 = CARTESIAN_POINT ( 'NONE',  ( 7.523070280405000254, 2.267583043933999676, -7.494013172964999470 ) ) ;
#37918 = EDGE_CURVE ( 'NONE', #59647, #60944, #38131, .T. ) ;
#37919 = DIRECTION ( 'NONE',  ( 1.000000000000000000, 0.000000000000000000, 0.000000000000000000 ) ) ;
#37920 = CARTESIAN_POINT ( 'NONE',  ( 9.453817378629960189, 5.259207081053330235, 7.986245092988616179 ) ) ;
#37921 = ORIENTED_EDGE ( 'NONE', *, *, #19342, .F. ) ;
#37922 = CARTESIAN_POINT ( 'NONE',  ( 10.22109127278999807, -2.983266195621000261, 8.764707262515999631 ) ) ;
#37923 = CARTESIAN_POINT ( 'NONE',  ( 25.19216650927900147, 11.35756831782000020, -3.218651103263999946 ) ) ;
#37924 = CARTESIAN_POINT ( 'NONE',  ( 11.14975833414749928, 3.203462856645999945, 7.174999999999999822 ) ) ;
#37925 = ORIENTED_EDGE ( 'NONE', *, *, #24475, .T. ) ;
#37926 = CARTESIAN_POINT ( 'NONE',  ( 8.832144816391009456, 4.216552416542988624, -8.465905425056138967 ) ) ;
#37927 = CARTESIAN_POINT ( 'NONE',  ( 10.53870444038000009, -5.103398787993000063, -6.705198626796000205 ) ) ;
#37928 = EDGE_LOOP ( 'NONE', ( #41584, #53759, #2759, #30212 ) ) ;
#37929 = CARTESIAN_POINT ( 'NONE',  ( 9.584000818238999742, 3.111278474435999808, 7.032008172796599510 ) ) ;
#37930 = CARTESIAN_POINT ( 'NONE',  ( 18.14736049945649299, 0.1997550941124134616, -13.89807248760371117 ) ) ;
#37931 = CARTESIAN_POINT ( 'NONE',  ( 4.648022794411000191, 0.6982277932244000951, -1.232437744370999955 ) ) ;
#37932 = CARTESIAN_POINT ( 'NONE',  ( 11.59999999999999964, 4.590480015894798704, -6.540686298265705467 ) ) ;
#37933 = CARTESIAN_POINT ( 'NONE',  ( 24.51105731435045598, 11.97394790521814301, -3.208410371361174018 ) ) ;
#37934 = CARTESIAN_POINT ( 'NONE',  ( 7.100000000000000533, 5.221516520829000640, -8.074802043613001246 ) ) ;
#37935 = CARTESIAN_POINT ( 'NONE',  ( 23.95415663622134161, 12.78629371929804925, 3.518569764782334630 ) ) ;
#37936 = B_SPLINE_CURVE_WITH_KNOTS ( 'NONE', 3,
 ( #6663, #65388, #32899, #66427, #12963, #34287, #28004, #17861, #50361, #65034, #2460, #33248, #23784, #49313, #1426, #44090, #38835, #34978, #19576, #8739, #34637, #8398, #25503 ),
 .UNSPECIFIED., .F., .F.,
 ( 4, 2, 2, 1, 2, 2, 2, 2, 1, 1, 2, 2, 4 ),
 ( 0.000000000000000000, 0.2500000000000463518, 0.3750000000000697775, 0.4375000000000831002, 0.4687500000000872635, 0.5000000000000913714, 0.6250000000000957012, 0.6875000000000990319, 0.7187500000001006972, 0.7343750000001003642, 0.7421875000001036948, 0.7500000000001070255, 1.000000000000000000 ),
 .UNSPECIFIED. ) ;
#37937 = CARTESIAN_POINT ( 'NONE',  ( 9.325456588376336953, -3.988345520164779945, 9.239772568469039271 ) ) ;
#37938 = ORIENTED_EDGE ( 'NONE', *, *, #41348, .T. ) ;
#37939 = CARTESIAN_POINT ( 'NONE',  ( 9.910633732652998518, 2.107262079134000210, 7.885285091859000062 ) ) ;
#37940 = CARTESIAN_POINT ( 'NONE',  ( 10.19121415877000203, 3.990707652596999555, -5.651362387566000400 ) ) ;
#37941 = CARTESIAN_POINT ( 'NONE',  ( 13.49998535730551019, 12.08447166622788771, 2.429352492459241120 ) ) ;
#37942 = CARTESIAN_POINT ( 'NONE',  ( 12.80505043854143388, 1.787816316115912407, -13.88537766212463431 ) ) ;
#37943 = DIRECTION ( 'NONE',  ( 0.000000000000000000, 0.000000000000000000, -1.000000000000000000 ) ) ;
#37944 = CARTESIAN_POINT ( 'NONE',  ( 9.719606904206999687, -5.967761543230999166, 7.406644089178000101 ) ) ;
#37945 = CARTESIAN_POINT ( 'NONE',  ( 17.71746485746498223, -0.6038715862870289719, 13.88233985103439494 ) ) ;
#37946 = CARTESIAN_POINT ( 'NONE',  ( 25.25799098492100114, -2.569256426743999899, 11.37081265261999974 ) ) ;
#37947 = EDGE_LOOP ( 'NONE', ( #39033, #2679, #32347, #34753 ) ) ;
#37948 = ORIENTED_EDGE ( 'NONE', *, *, #47837, .T. ) ;
#37949 = LINE ( 'NONE', #204, #45537 ) ;
#37950 = ADVANCED_FACE ( 'NONE', ( #39524 ), #59806, .T. ) ;
#37951 = CARTESIAN_POINT ( 'NONE',  ( 12.41269542047506391, -0.4865081001745747424, -13.88853895923323378 ) ) ;
#37952 = EDGE_CURVE ( 'NONE', #38805, #27228, #37936, .T. ) ;
#37953 = CARTESIAN_POINT ( 'NONE',  ( 7.236065714745352651, -2.650241189008525566, 7.323011948609822852 ) ) ;
#37954 = CARTESIAN_POINT ( 'NONE',  ( 17.94293712298191679, -0.4901002082654778436, -13.88836944287707098 ) ) ;
#37955 = CARTESIAN_POINT ( 'NONE',  ( 7.988543146792999927, -3.566638198986999964, 5.743608852252999775 ) ) ;
#37957 = VECTOR ( 'NONE', #46444, 1000.000000000000000 ) ;
#37956 = CARTESIAN_POINT ( 'NONE',  ( 24.63781023927800007, 8.684869114355000974, 8.585175602391000638 ) ) ;
#37959 = CARTESIAN_POINT ( 'NONE',  ( 17.91921746558384498, 11.21561494459062480, -3.152940210887823724 ) ) ;
#37958 = CARTESIAN_POINT ( 'NONE',  ( 9.981734463323000739, -3.866750753272200303, 6.227746477418000026 ) ) ;
#37960 = CARTESIAN_POINT ( 'NONE',  ( 10.12841772631199966, 4.490588993294299947, -8.509834072393999804 ) ) ;
#37961 = CARTESIAN_POINT ( 'NONE',  ( 24.35145719007200071, -8.929422700512001043, -9.054903155755001265 ) ) ;
#37962 = CARTESIAN_POINT ( 'NONE',  ( 18.30000077768849565, 11.66744147158535405, -3.971919865264926575 ) ) ;
#37963 = CARTESIAN_POINT ( 'NONE',  ( 18.17481334264689607, 0.08139242733401001739, 12.69965452654166960 ) ) ;
#37964 = CARTESIAN_POINT ( 'NONE',  ( 11.05851190073833301, -5.258511900738333189, 6.537362761296000357 ) ) ;
#37965 = CARTESIAN_POINT ( 'NONE',  ( 12.79999999734009464, 10.99220013531737372, -4.481500379774075782 ) ) ;
#37966 = VERTEX_POINT ( 'NONE', #40896 ) ;
#37967 = CARTESIAN_POINT ( 'NONE',  ( 7.545269353206999874, -2.302293129340000188, 6.875167727519000849 ) ) ;
#37968 = CARTESIAN_POINT ( 'NONE',  ( 8.573539158775000502, 5.361622798585000460, -7.185294144754000634 ) ) ;
#37969 = CARTESIAN_POINT ( 'NONE',  ( 5.000000000000000000, 0.000000000000000000, 0.000000000000000000 ) ) ;
#37970 = EDGE_CURVE ( 'NONE', #33345, #41213, #25157, .T. ) ;
#37971 = CARTESIAN_POINT ( 'NONE',  ( 10.98768472569999943, 5.449702578894000560, 4.945212061318999375 ) ) ;
#37972 = CARTESIAN_POINT ( 'NONE',  ( 0.3460379451994000100, -2.198759671591000053, -2.775001775783000113 ) ) ;
#37973 = CARTESIAN_POINT ( 'NONE',  ( 11.52677869730533011, 3.596497913043499750, 8.295667533166499297 ) ) ;
#37974 = CARTESIAN_POINT ( 'NONE',  ( 2.313974293799999860, -3.372637136287000015, -1.659426359180999899 ) ) ;
#37975 = ORIENTED_EDGE ( 'NONE', *, *, #15139, .F. ) ;
#37976 = DIRECTION ( 'NONE',  ( 0.000000000000000000, -0.7158784314710767704, 0.6982249432342778617 ) ) ;
#37977 = CARTESIAN_POINT ( 'NONE',  ( 8.150000662387999029, 3.037570195374000164E-13, -3.945735770681999509E-14 ) ) ;
#37978 = CARTESIAN_POINT ( 'NONE',  ( 17.95027792402079569, 3.083622039298902884, -12.21684579612696808 ) ) ;
#37979 = CARTESIAN_POINT ( 'NONE',  ( 15.66247398912731725, -8.798600188463547411, -7.938011626707102586 ) ) ;
#37980 = CARTESIAN_POINT ( 'NONE',  ( 7.577017219590000074, 5.480308727866000318, 8.192324747680999053 ) ) ;
#37981 = ORIENTED_EDGE ( 'NONE', *, *, #67347, .F. ) ;
#37982 = CARTESIAN_POINT ( 'NONE',  ( 5.477930087360999956, -0.8125565852189000626, 1.395285458375999932 ) ) ;
#37983 = CARTESIAN_POINT ( 'NONE',  ( 7.756929719584999994, 3.458959908335999867, -5.854223596299999777 ) ) ;
#37984 = CARTESIAN_POINT ( 'NONE',  ( 8.531899004865357128, -3.122575144635288069, 5.996049329724215227 ) ) ;
#37985 = CARTESIAN_POINT ( 'NONE',  ( 11.50000302521714701, -12.42140736507980137, -1.609561362244301241 ) ) ;
#37986 = ORIENTED_EDGE ( 'NONE', *, *, #67383, .F. ) ;
#37987 = CARTESIAN_POINT ( 'NONE',  ( 10.98768472567999943, 5.449702577258999980, -4.945212061305999107 ) ) ;
#37988 = CARTESIAN_POINT ( 'NONE',  ( 11.35563158142000262, 11.71552011691000139, 1.381878615183999903 ) ) ;
#37989 = VERTEX_POINT ( 'NONE', #3483 ) ;
#37990 = CARTESIAN_POINT ( 'NONE',  ( 24.69609986848488248, 3.134121630126239122, -11.81029131445869673 ) ) ;
#37992 = CARTESIAN_POINT ( 'NONE',  ( 8.312776266199000119, 10.52971825582000065, -4.244445611735000234 ) ) ;
#37991 = VECTOR ( 'NONE', #23462, 1000.000000000000000 ) ;
#37993 = CARTESIAN_POINT ( 'NONE',  ( 17.59617041303008378, -0.6239795106976184780, -13.88114172264460322 ) ) ;
#37994 = VERTEX_POINT ( 'NONE', #46832 ) ;
#37995 = CARTESIAN_POINT ( 'NONE',  ( 10.44862608313071917, -4.356257174807515398, -9.239447894061358468 ) ) ;
#37996 = CARTESIAN_POINT ( 'NONE',  ( 8.298515680831000552, 8.052744916463998592, 4.948539300261999507 ) ) ;
#37997 = CARTESIAN_POINT ( 'NONE',  ( 10.69568717260499824, 3.533932086969799879, -8.260703168378098482 ) ) ;
#37998 = ADVANCED_FACE ( 'NONE', ( #55949 ), #65279, .T. ) ;
#37999 = CARTESIAN_POINT ( 'NONE',  ( 5.000000000000000000, -3.441691376337999159E-14, 1.598721155459999804E-14 ) ) ;
#38000 = CARTESIAN_POINT ( 'NONE',  ( 10.69810941423799910, -3.053977294209000437, 8.359277272599898723 ) ) ;
#38001 = VERTEX_POINT ( 'NONE', #9076 ) ;
#38002 = CARTESIAN_POINT ( 'NONE',  ( 8.604017219593000476, 5.165497731316000873, 8.645531386060000045 ) ) ;
#38003 = ORIENTED_EDGE ( 'NONE', *, *, #41840, .F. ) ;
#38004 = VECTOR ( 'NONE', #7364, 1000.000000000000114 ) ;
#38005 = CARTESIAN_POINT ( 'NONE',  ( 8.630000000000000782, 4.924138593003999809, -8.484107647018999998 ) ) ;
#38006 = CARTESIAN_POINT ( 'NONE',  ( 15.58628609634500073, -9.247881098673000011, -8.227358011109998870 ) ) ;
#38007 = FACE_OUTER_BOUND ( 'NONE', #39759, .T. ) ;
#38008 = EDGE_LOOP ( 'NONE', ( #20048, #37549, #35112, #41736, #935, #56849, #25626, #66963 ) ) ;
#38009 = B_SPLINE_SURFACE_WITH_KNOTS ( 'NONE', 3, 3, ( 
 ( #33573, #34620, #1406, #17842 ),
 ( #54893, #11888, #33228, #66064 ),
 ( #55240, #18183, #54547, #39505 ),
 ( #12942, #2441, #34268, #7691 ) ),
 .UNSPECIFIED., .F., .F., .F.,
 ( 4, 4 ),
 ( 4, 4 ),
 ( 0.7363163806532000422, 1.013499456067999960 ),
 ( -0.0005287450254680999126, 0.02696599629895000266 ),
 .UNSPECIFIED. ) ;
#38010 = CARTESIAN_POINT ( 'NONE',  ( 12.34565325027257998, -2.076107717502759353, -12.54027567175044311 ) ) ;
#38011 = PLANE ( 'NONE',  #65618 ) ;
#38012 = CARTESIAN_POINT ( 'NONE',  ( 23.89320776801300283, -8.928716006355012169, 8.952507060126997374 ) ) ;
#38013 = CARTESIAN_POINT ( 'NONE',  ( 24.17844198652961296, -3.317834083975258253, -12.42307627910415313 ) ) ;
#38014 = CARTESIAN_POINT ( 'NONE',  ( 12.17501771842806768, -2.156544773268137316, -13.83291087807201691 ) ) ;
#38015 = CARTESIAN_POINT ( 'NONE',  ( 10.45257053952200010, -4.394359323863099576, -6.577269499510100204 ) ) ;
#38016 = CARTESIAN_POINT ( 'NONE',  ( 12.07922409836651489, -2.296075726970902675, 12.39049400503303922 ) ) ;
#38017 = CARTESIAN_POINT ( 'NONE',  ( 18.26259847173845330, -2.320949922530737286, 12.38441499264346390 ) ) ;
#38018 = EDGE_LOOP ( 'NONE', ( #14481, #54125, #36332, #13398 ) ) ;
#38019 = CARTESIAN_POINT ( 'NONE',  ( 11.26723293495529887, -5.173938955706000264, -7.452807962566580180 ) ) ;
#38020 = ORIENTED_EDGE ( 'NONE', *, *, #5201, .T. ) ;
#38021 = LINE ( 'NONE', #43629, #61279 ) ;
#38022 = CARTESIAN_POINT ( 'NONE',  ( 9.544414158773999901, 2.173570076733999823, -8.023168429484000441 ) ) ;
#38023 = CARTESIAN_POINT ( 'NONE',  ( 10.31499646082999888, 5.458376174241999834, -8.355105941236999456 ) ) ;
#38024 = CARTESIAN_POINT ( 'NONE',  ( 10.91944543538999923, -3.268376408192000149, -6.413937436229999456 ) ) ;
#38025 = CARTESIAN_POINT ( 'NONE',  ( 24.53428991268900106, -12.47024905405999995, -3.026245386525999947 ) ) ;
#38026 = CARTESIAN_POINT ( 'NONE',  ( 24.22000602247700130, -12.94771364386000201, 3.132628870380000041 ) ) ;
#38027 = CARTESIAN_POINT ( 'NONE',  ( 17.33333333161133538, 3.595161661651967933, 11.99793472338499711 ) ) ;
#38028 = VERTEX_POINT ( 'NONE', #18548 ) ;
#38029 = CARTESIAN_POINT ( 'NONE',  ( 18.44720874474599981, 2.702894824448000222, 11.38760777189999907 ) ) ;
#38030 = ADVANCED_FACE ( 'NONE', ( #56295 ), #14336, .F. ) ;
#38031 = CARTESIAN_POINT ( 'NONE',  ( 11.25041981190000051, 5.730782764036999488, 8.122675980938000251 ) ) ;
#38032 = EDGE_CURVE ( 'NONE', #47095, #2906, #46490, .T. ) ;
#38033 = DIRECTION ( 'NONE',  ( 0.000000000000000000, -0.2461538461538895495, 0.9692307692307581268 ) ) ;
#38034 = B_SPLINE_CURVE_WITH_KNOTS ( 'NONE', 3,
 ( #66191, #55719, #39988, #61302 ),
 .UNSPECIFIED., .F., .F.,
 ( 4, 4 ),
 ( 0.8746295857519847949, 1.000000000000000000 ),
 .UNSPECIFIED. ) ;
#38035 = CARTESIAN_POINT ( 'NONE',  ( 11.23724174883999893, -4.024531238983009906, 6.608211443991299561 ) ) ;
#38036 = CARTESIAN_POINT ( 'NONE',  ( 17.75907622778400352, 3.376089723145999866, -11.11072845602000037 ) ) ;
#38037 = DIRECTION ( 'NONE',  ( -1.000000000000000000, 0.000000000000000000, 2.886579864060000134E-14 ) ) ;
#38038 = CONICAL_SURFACE ( 'NONE', #68181, 1.725000594299999968, 0.7853984795078434722 ) ;
#38039 = CARTESIAN_POINT ( 'NONE',  ( 10.18658456763778375, 5.723604601771135059, 7.204491886445339333 ) ) ;
#38040 = CARTESIAN_POINT ( 'NONE',  ( 23.58681704922799938, -10.27308883388000105, -9.418745758480000063 ) ) ;
#38041 = CARTESIAN_POINT ( 'NONE',  ( 23.55066264645300222, -10.43161032036999813, 9.390903619644999978 ) ) ;
#38042 = AXIS2_PLACEMENT_3D ( 'NONE', #38553, #23509, #65460 ) ;
#38043 = CARTESIAN_POINT ( 'NONE',  ( 11.80443633831200145, -3.376482451534999818, 11.11063790749999924 ) ) ;
#38044 = ORIENTED_EDGE ( 'NONE', *, *, #59112, .T. ) ;
#38045 = CARTESIAN_POINT ( 'NONE',  ( 8.771960841230001193, 3.061731693614000438, -8.535706278603999664 ) ) ;
#38046 = CARTESIAN_POINT ( 'NONE',  ( 7.227324660199999862, 1.322954291153000117, 0.3512839726887999614 ) ) ;
#38047 = CARTESIAN_POINT ( 'NONE',  ( 18.16363222863425264, 2.642680409073417280, 13.64211442534931606 ) ) ;
#38048 = EDGE_CURVE ( 'NONE', #22879, #21434, #56270, .T. ) ;
#38049 = CARTESIAN_POINT ( 'NONE',  ( 24.53002386606100060, 8.771528676252001944, -8.897041952684000776 ) ) ;
#38050 = CARTESIAN_POINT ( 'NONE',  ( 10.46887750876899936, -4.692271380433699512, -8.574279626736998949 ) ) ;
#38051 = EDGE_LOOP ( 'NONE', ( #39748, #17046, #56693, #33264 ) ) ;
#38052 = CARTESIAN_POINT ( 'NONE',  ( 5.634824896761482016, -12.09997259267829506, 3.741298181620987151 ) ) ;
#38053 = ADVANCED_FACE ( 'NONE', ( #30412 ), #2802, .T. ) ;
#38054 = CARTESIAN_POINT ( 'NONE',  ( 7.149100552923999707, 4.351669901925999895, 8.977196921526999773 ) ) ;
#38056 = DIRECTION ( 'NONE',  ( 0.000000000000000000, -0.1623203401144080182, 0.9867381147929490393 ) ) ;
#38055 = CARTESIAN_POINT ( 'NONE',  ( 9.450870280412999591, 2.928319778732999978, -8.861178115809998701 ) ) ;
#38057 = CARTESIAN_POINT ( 'NONE',  ( 2.352367082289130717, 1.876785584549146568, 2.663032597268895518 ) ) ;
#38058 = ORIENTED_EDGE ( 'NONE', *, *, #24080, .F. ) ;
#38059 = CARTESIAN_POINT ( 'NONE',  ( 10.37026939687000038, 5.571553923009999743, 7.748385725654999945 ) ) ;
#38060 = CARTESIAN_POINT ( 'NONE',  ( 17.85704948507095224, -1.853727412078939762, -13.87673533860537489 ) ) ;
#38061 = CARTESIAN_POINT ( 'NONE',  ( 11.51102763632551884, 3.088851714329700293, 7.920427941950599404 ) ) ;
#38062 = CARTESIAN_POINT ( 'NONE',  ( 10.96207173348999930, -5.399846879528999999, 7.743266618618998898 ) ) ;
#38063 = CARTESIAN_POINT ( 'NONE',  ( 7.895830451470996714, 3.177662910779999628, 6.240430379278997464 ) ) ;
#38064 = EDGE_LOOP ( 'NONE', ( #9190, #61062, #2077, #2896 ) ) ;
#38065 = FACE_BOUND ( 'NONE', #9698, .T. ) ;
#38067 = CARTESIAN_POINT ( 'NONE',  ( 10.81188185321000006, -4.614147550108000928, -5.930138617968999881 ) ) ;
#38066 = DIRECTION ( 'NONE',  ( 4.514773433173149668E-07, -0.9999999999995329292, 8.545138996459277929E-07 ) ) ;
#38068 = CARTESIAN_POINT ( 'NONE',  ( 7.807026942100614875, -4.385935279688806254, 9.196252002095368638 ) ) ;
#38069 = CARTESIAN_POINT ( 'NONE',  ( 10.27814441345999974, -5.521593622715999850, 8.751220666652999469 ) ) ;
#38070 = CARTESIAN_POINT ( 'NONE',  ( 8.472537864290000442, 2.899999999999999911, -6.571291218949999902 ) ) ;
#38071 = ORIENTED_EDGE ( 'NONE', *, *, #61114, .F. ) ;
#38072 = CARTESIAN_POINT ( 'NONE',  ( 25.05002157598449841, -11.42810647003321378, -3.253264283331835038 ) ) ;
#38073 = CARTESIAN_POINT ( 'NONE',  ( 11.76072066707849828, -3.023932655881500065, 8.090408888831799317 ) ) ;
#38074 = CARTESIAN_POINT ( 'NONE',  ( 8.056015159639001055, 3.481518869265999072, 6.232552614174998951 ) ) ;
#38075 = CARTESIAN_POINT ( 'NONE',  ( 11.62579573085663043, 5.239377455231000624, 7.285547569258399747 ) ) ;
#38076 = ORIENTED_EDGE ( 'NONE', *, *, #31487, .F. ) ;
#38077 = CARTESIAN_POINT ( 'NONE',  ( 9.260829719593999698, 4.861259245430999520, -8.806664389576001284 ) ) ;
#38078 = AXIS2_PLACEMENT_3D ( 'NONE', #45891, #67202, #9164 ) ;
#38079 = CARTESIAN_POINT ( 'NONE',  ( 12.18657262959517595, 2.104614846739864209, -12.42298765743896816 ) ) ;
#38080 = CARTESIAN_POINT ( 'NONE',  ( 12.25203632436370071, -5.109717061557999429, 7.759151359668400083 ) ) ;
#38081 = CARTESIAN_POINT ( 'NONE',  ( 7.959937255769798270, 5.013283352723129305, -6.497370493178895146 ) ) ;
#38082 = CARTESIAN_POINT ( 'NONE',  ( 25.59997324745700098, 8.218963665694001719, 8.043524865688999270 ) ) ;
#38084 = ORIENTED_EDGE ( 'NONE', *, *, #64761, .T. ) ;
#38083 = B_SPLINE_CURVE_WITH_KNOTS ( 'NONE', 3,
 ( #6499, #7200, #51479, #59643, #46242, #14086, #49848, #45563, #44276, #3576 ),
 .UNSPECIFIED., .F., .F.,
 ( 4, 2, 2, 2, 4 ),
 ( 0.000000000000000000, 0.1250000005483845322, 0.2500000010967690645, 0.3750000016451535134, 0.5000000021935380179 ),
 .UNSPECIFIED. ) ;
#38085 = CARTESIAN_POINT ( 'NONE',  ( 8.881816940380000247, -4.977917894183000236, 6.416767031887000705 ) ) ;
#38086 = CARTESIAN_POINT ( 'NONE',  ( 23.84021450726483238, 9.641930377286131559, 9.401241262644600027 ) ) ;
#38087 = VERTEX_POINT ( 'NONE', #62552 ) ;
#38088 = DIRECTION ( 'NONE',  ( -1.000000000000000000, 0.000000000000000000, 0.000000000000000000 ) ) ;
#38089 = CARTESIAN_POINT ( 'NONE',  ( 10.33364828895399867, 4.760196147278000112, 7.084788038520800413 ) ) ;
#38090 = PRODUCT_DEFINITION ( 'UNKNOWN', '', #22866, #41588 ) ;
#38091 = CARTESIAN_POINT ( 'NONE',  ( 25.29987261391899978, -8.756202924575998026, 7.455126447192999883 ) ) ;
#38092 = EDGE_CURVE ( 'NONE', #23962, #23956, #7981, .T. ) ;
#38093 = CARTESIAN_POINT ( 'NONE',  ( 10.71983649979000042, 3.571741329336999726, -5.696148467328000287 ) ) ;
#38094 = CARTESIAN_POINT ( 'NONE',  ( 4.599999999999999645, 1.760845406083394460, -12.47635457398814651 ) ) ;
#38095 = CARTESIAN_POINT ( 'NONE',  ( 10.35616740164000049, -2.777283710737999733, 8.995265811011998736 ) ) ;
#38096 = PLANE ( 'NONE',  #48844 ) ;
#38097 = CARTESIAN_POINT ( 'NONE',  ( 17.74345815918222868, -0.6949735217938798337, -12.58082105808779971 ) ) ;
#38098 = VECTOR ( 'NONE', #53846, 999.9999999999998863 ) ;
#38099 = CARTESIAN_POINT ( 'NONE',  ( 12.18396690406853544, 2.429413046084606620, -12.46775848778887408 ) ) ;
#38100 = CARTESIAN_POINT ( 'NONE',  ( 10.94072200990529886, -5.077092948368999714, -7.124286150322599376 ) ) ;
#38101 = CARTESIAN_POINT ( 'NONE',  ( 9.176357780411999343, 2.935741164366000522, 6.259844213126999790 ) ) ;
#38102 = VERTEX_POINT ( 'NONE', #4166 ) ;
#38103 =( NAMED_UNIT ( * ) PLANE_ANGLE_UNIT ( ) SI_UNIT ( $, .RADIAN. ) );
#38104 = CARTESIAN_POINT ( 'NONE',  ( 9.143927823787141307, 5.249988444743199700, -7.499999844943244121 ) ) ;
#38105 = CARTESIAN_POINT ( 'NONE',  ( 24.30001694670299983, 8.938702829764999080, 8.938676122491999720 ) ) ;
#38106 = LINE ( 'NONE', #32532, #38098 ) ;
#38107 = CARTESIAN_POINT ( 'NONE',  ( 18.23388167758333367, 2.733449996235734147, 12.29993400349665222 ) ) ;
#38108 = CARTESIAN_POINT ( 'NONE',  ( 11.07071178722999960, 6.643972308597000165, 5.583263443185999542 ) ) ;
#38109 = CARTESIAN_POINT ( 'NONE',  ( 11.12552327284000064, 8.121114117777999297, 6.768012205397000436 ) ) ;
#38110 = CARTESIAN_POINT ( 'NONE',  ( 10.48677454732762726, -3.921486932049647489, 8.371417217572535208 ) ) ;
#38111 = CARTESIAN_POINT ( 'NONE',  ( 9.885596873516499627, -5.092232985442824322, -8.129523725463620565 ) ) ;
#38112 = EDGE_CURVE ( 'NONE', #9405, #46731, #61347, .T. ) ;
#38113 = ORIENTED_EDGE ( 'NONE', *, *, #50157, .F. ) ;
#38114 = CARTESIAN_POINT ( 'NONE',  ( 12.37983597880429265, -3.063558859249374766, 12.22189795429198966 ) ) ;
#38115 = EDGE_CURVE ( 'NONE', #53930, #25788, #32902, .T. ) ;
#38116 = CARTESIAN_POINT ( 'NONE',  ( 9.908304848515998131, -3.086535948898899928, -7.917643062525700159 ) ) ;
#38117 = CARTESIAN_POINT ( 'NONE',  ( 10.23809632363000155, 2.752447932331000047, 6.820051270595000048 ) ) ;
#38118 = FACE_OUTER_BOUND ( 'NONE', #68566, .T. ) ;
#38119 = EDGE_CURVE ( 'NONE', #12504, #42732, #51311, .T. ) ;
#38120 = CARTESIAN_POINT ( 'NONE',  ( 10.50180110216399854, 3.143606124884799957, -6.976989117212499814 ) ) ;
#38121 = CARTESIAN_POINT ( 'NONE',  ( 12.10431270533525527, -0.1860047152749652044, 12.59864695008082336 ) ) ;
#38122 = CARTESIAN_POINT ( 'NONE',  ( 9.138573341230998182, 2.933833973450999721, 8.496479443567000800 ) ) ;
#38123 = CARTESIAN_POINT ( 'NONE',  ( 9.629022744239000176, 5.794335169544999609, 7.414871903737999759 ) ) ;
#38124 = CARTESIAN_POINT ( 'NONE',  ( 12.80505043854143388, 3.124999999999999556, 12.28373071562070074 ) ) ;
#38125 = CARTESIAN_POINT ( 'NONE',  ( 9.934999999999998721, 4.640430492595999823, -9.117542781427999898 ) ) ;
#38126 = CARTESIAN_POINT ( 'NONE',  ( 11.40841235500449891, 3.158861363519000154, -6.729431436870699557 ) ) ;
#38127 = CARTESIAN_POINT ( 'NONE',  ( 10.47530200610951034, -5.350262918594152595, 7.499984559551212904 ) ) ;
#38128 = CARTESIAN_POINT ( 'NONE',  ( 10.33453278041000090, 3.295703187163999459, -6.149878749787999865 ) ) ;
#38129 = CARTESIAN_POINT ( 'NONE',  ( 9.587263606520032511, 3.377808641629922892, 8.716806737539613437 ) ) ;
#38131 = LINE ( 'NONE', #1773, #22860 ) ;
#38130 = CARTESIAN_POINT ( 'NONE',  ( 7.969753415490000492, 5.131577060784002775, 6.757500301899002970 ) ) ;
#38132 = DIRECTION ( 'NONE',  ( 0.000000000000000000, 0.1807154286440005586, 0.9835354258236025382 ) ) ;
#38133 = VERTEX_POINT ( 'NONE', #31785 ) ;
#38134 = CARTESIAN_POINT ( 'NONE',  ( 12.40587394961001166, 0.4809228688204498225, 12.68774147672023744 ) ) ;
#38135 = EDGE_CURVE ( 'NONE', #65197, #5301, #27313, .T. ) ;
#38136 = CARTESIAN_POINT ( 'NONE',  ( 23.77343862489363602, -9.774797336595577590, -9.437290416679315896 ) ) ;
#38137 = CARTESIAN_POINT ( 'NONE',  ( 12.44187590071209826, -11.55958658085556046, 4.822001495576079044 ) ) ;
#38138 = CARTESIAN_POINT ( 'NONE',  ( 9.197076168957998732, 3.560025096655699883, 6.752918994396699404 ) ) ;
#38139 = AXIS2_PLACEMENT_3D ( 'NONE', #46855, #36013, #57329 ) ;
#38140 = CARTESIAN_POINT ( 'NONE',  ( 12.14421144042239931, -2.819066901275895098, 13.71325475029871477 ) ) ;
#38141 = CARTESIAN_POINT ( 'NONE',  ( 10.92363156114900136, -4.684311564990209398, 6.424401362931539516 ) ) ;
#38142 = CARTESIAN_POINT ( 'NONE',  ( 23.91176682606199932, 3.265437890189999859, -12.84181129811999966 ) ) ;
#38143 = ORIENTED_EDGE ( 'NONE', *, *, #8748, .T. ) ;
#38144 = DIRECTION ( 'NONE',  ( 1.000000000000000000, 0.000000000000000000, 0.000000000000000000 ) ) ;
#38145 = CARTESIAN_POINT ( 'NONE',  ( 11.09999999999999964, -4.000000000000000000, -7.500000000000000000 ) ) ;
#38146 = CARTESIAN_POINT ( 'NONE',  ( 7.779438594805999863, -3.186699643285999972, 6.422256653932000070 ) ) ;
#38147 = CARTESIAN_POINT ( 'NONE',  ( 10.70271159698171992, -5.100000000000000533, 6.305985889763628727 ) ) ;
#38148 = CARTESIAN_POINT ( 'NONE',  ( 18.50007554376851715, -2.772760791832214800, 11.31557096909616966 ) ) ;
#38149 = CARTESIAN_POINT ( 'NONE',  ( 17.77409395429256023, -11.41728060638866538, 4.609654547496091936 ) ) ;
#38150 = CARTESIAN_POINT ( 'NONE',  ( 10.23809632363000155, 2.752447932331000047, 6.820051270595000048 ) ) ;
#38151 = CARTESIAN_POINT ( 'NONE',  ( 10.55518582084299872, 3.433275964779900047, 8.155074391384399490 ) ) ;
#38152 = CONICAL_SURFACE ( 'NONE', #52678, 0.9999998338055000602, 0.7853981908209605178 ) ;
#38153 = CARTESIAN_POINT ( 'NONE',  ( 10.86225948028000055, -2.934717151119000000, -5.172334369529000497 ) ) ;
#38154 = CARTESIAN_POINT ( 'NONE',  ( 10.71315564678999976, -2.619204038425999581, -8.142086897834001746 ) ) ;
#38155 = CARTESIAN_POINT ( 'NONE',  ( 25.60000000000000142, -2.258942858049999725, 12.29419282279000036 ) ) ;
#38156 = CARTESIAN_POINT ( 'NONE',  ( 11.50001544675000176, -12.52500000000000036, 0.000000000000000000 ) ) ;
#38157 = CARTESIAN_POINT ( 'NONE',  ( 24.66271477989500127, 12.38330044149000031, 2.963253076001000075 ) ) ;
#38158 = FACE_OUTER_BOUND ( 'NONE', #28461, .T. ) ;
#38159 = ORIENTED_EDGE ( 'NONE', *, *, #53598, .T. ) ;
#38160 = CARTESIAN_POINT ( 'NONE',  ( 7.416780799524962831, 2.408868269339266455, 8.205667337080191359 ) ) ;
#38161 = CARTESIAN_POINT ( 'NONE',  ( 11.78949010443639978, -2.999324937259999935, 7.425165037173959703 ) ) ;
#38162 = ORIENTED_EDGE ( 'NONE', *, *, #53176, .T. ) ;
#38163 = CARTESIAN_POINT ( 'NONE',  ( 17.98481728017923942, -2.046093834626821817, 13.75931539188737496 ) ) ;
#38164 = CARTESIAN_POINT ( 'NONE',  ( 11.60118044953561878, -2.866798846279000390, -8.090905336380599167 ) ) ;
#38165 = ORIENTED_EDGE ( 'NONE', *, *, #52309, .T. ) ;
#38166 = CARTESIAN_POINT ( 'NONE',  ( 10.85168717260509830, 3.386210853237200169, 6.498190316041999814 ) ) ;
#38167 = CARTESIAN_POINT ( 'NONE',  ( 6.455467915152659941, 0.005977207969617732465, -1.133219647842097499 ) ) ;
#38168 = CARTESIAN_POINT ( 'NONE',  ( 24.13226547067089101, 3.329776921202292517, -12.50568236576632764 ) ) ;
#38169 = EDGE_CURVE ( 'NONE', #60441, #55462, #44649, .T. ) ;
#38170 = CARTESIAN_POINT ( 'NONE',  ( 9.819055905797000605, -2.899999999999999911, -6.571291218949999902 ) ) ;
#38171 = EDGE_CURVE ( 'NONE', #39230, #57495, #10107, .T. ) ;
#38172 = DIRECTION ( 'NONE',  ( 0.000000000000000000, -1.000000000000000000, 0.000000000000000000 ) ) ;
#38173 = CARTESIAN_POINT ( 'NONE',  ( 0.1500002361980000143, 0.000000000000000000, 0.000000000000000000 ) ) ;
#38174 = CARTESIAN_POINT ( 'NONE',  ( 9.599999931441001166, -2.935682118448999844, 6.844464000216799349 ) ) ;
#38175 = CARTESIAN_POINT ( 'NONE',  ( 9.831596185961002377, -3.539228349258999984, -8.956015611440999891 ) ) ;
#38176 = CARTESIAN_POINT ( 'NONE',  ( 11.58902763632552002, -4.786505910413500153, -7.137085349939700230 ) ) ;
#38177 = ORIENTED_EDGE ( 'NONE', *, *, #7827, .F. ) ;
#38178 = CARTESIAN_POINT ( 'NONE',  ( 9.667010841233000917, 4.769103072373000352, -8.666849124598000387 ) ) ;
#38179 = EDGE_LOOP ( 'NONE', ( #36457, #34451, #61311, #43258, #43752, #61378, #42326, #44143, #1552, #60609 ) ) ;
#38180 = CARTESIAN_POINT ( 'NONE',  ( 0.3857633700769134144, 0.6253109423643958831, 3.191549458069821821 ) ) ;
#38181 = AXIS2_PLACEMENT_3D ( 'NONE', #61319, #13438, #33723 ) ;
#38182 =( NAMED_UNIT ( * ) PLANE_ANGLE_UNIT ( ) SI_UNIT ( $, .RADIAN. ) );
#38183 = EDGE_LOOP ( 'NONE', ( #14553, #14671, #13015, #4015, #62476 ) ) ;
#38184 = LINE ( 'NONE', #59516, #44853 ) ;
#38185 = FILL_AREA_STYLE_COLOUR ( '', #49532 ) ;
#38186 = CARTESIAN_POINT ( 'NONE',  ( 10.74760529021567734, 4.040385281810796592, 6.626811228128840270 ) ) ;
#38187 = CARTESIAN_POINT ( 'NONE',  ( 10.31059687351633158, 3.370476274536378103, -6.407767014557176566 ) ) ;
#38188 = CARTESIAN_POINT ( 'NONE',  ( 9.498096873515667227, -4.327184855449103473, -8.717465845835393523 ) ) ;
#38190 = DIRECTION ( 'NONE',  ( 1.000000000000000000, 0.000000000000000000, 0.000000000000000000 ) ) ;
#38189 = B_SPLINE_CURVE_WITH_KNOTS ( 'NONE', 3,
 ( #30997, #57202, #9305, #40784 ),
 .UNSPECIFIED., .F., .F.,
 ( 4, 4 ),
 ( 0.000000000000000000, 0.1836163425310833319 ),
 .UNSPECIFIED. ) ;
#38191 = DIRECTION ( 'NONE',  ( 0.000000000000000000, -0.9586234969500269099, -0.2846769943204078834 ) ) ;
#38192 = B_SPLINE_CURVE_WITH_KNOTS ( 'NONE', 3,
 ( #14371, #15395, #53818, #63618 ),
 .UNSPECIFIED., .F., .F.,
 ( 4, 4 ),
 ( 0.000000000000000000, 1.000000000000000000 ),
 .UNSPECIFIED. ) ;
#38193 = CARTESIAN_POINT ( 'NONE',  ( 12.21985227486504400, 0.2197089332467950795, 13.89766776387047642 ) ) ;
#38194 = ORIENTED_EDGE ( 'NONE', *, *, #38711, .T. ) ;
#38195 = CARTESIAN_POINT ( 'NONE',  ( 10.93769855012999948, 2.936883479403999964, 4.920828759365000415 ) ) ;
#38196 = ADVANCED_FACE ( 'NONE', ( #4852 ), #43917, .F. ) ;
#38197 = CARTESIAN_POINT ( 'NONE',  ( 10.49316300899723764, -4.959452674051987309, 8.606795388839010741 ) ) ;
#38198 = CARTESIAN_POINT ( 'NONE',  ( 9.936116252963625328, 4.581155023945095550, 8.154057418782388211 ) ) ;
#38199 = CARTESIAN_POINT ( 'NONE',  ( 4.249401635788000675, -0.8829617685141000205, -1.096690919835000111 ) ) ;
#38200 = VECTOR ( 'NONE', #63651, 999.9999999999998863 ) ;
#38201 = EDGE_CURVE ( 'NONE', #15133, #48764, #15010, .T. ) ;
#38202 = CARTESIAN_POINT ( 'NONE',  ( 8.458179719589999479, 5.332332124071999857, -8.487089944253000340 ) ) ;
#38203 = CARTESIAN_POINT ( 'NONE',  ( 10.52314899745999988, 5.167567567567999731, -6.822293592207000934 ) ) ;
#38204 = CIRCLE ( 'NONE', #47152, 12.79999953825000070 ) ;
#38205 = CARTESIAN_POINT ( 'NONE',  ( 10.66852499011999988, -4.435470817312999969, -5.866470266317000082 ) ) ;
#38206 = ORIENTED_EDGE ( 'NONE', *, *, #40023, .F. ) ;
#38207 = DIRECTION ( 'NONE',  ( 1.000000000000000000, 0.000000000000000000, 0.000000000000000000 ) ) ;
#38208 = DIRECTION ( 'NONE',  ( 1.000000000000000000, 0.000000000000000000, 0.000000000000000000 ) ) ;
#38209 = CARTESIAN_POINT ( 'NONE',  ( 4.503351004233334010, -1.211624111678819782, 0.9172058655087356183 ) ) ;
#38210 = CARTESIAN_POINT ( 'NONE',  ( 10.94916232721328164, -5.139975539640455615, 5.103975416952581945 ) ) ;
#38211 = CARTESIAN_POINT ( 'NONE',  ( 11.81056516821459823, 4.609678151793300316, -8.115298063151199059 ) ) ;
#38212 = CARTESIAN_POINT ( 'NONE',  ( 8.751496707488000126, 4.081676005979390176, -8.356402621895700378 ) ) ;
#38213 = CARTESIAN_POINT ( 'NONE',  ( 11.18923293495519822, 2.967327562101000016, -7.458486839450950256 ) ) ;
#38214 = CARTESIAN_POINT ( 'NONE',  ( 9.254721904869999349, 4.875830726371099821, -7.991693846894699860 ) ) ;
#38216 = CARTESIAN_POINT ( 'NONE',  ( 8.336034600740228839, 4.707624567763986079, -6.071688517621553594 ) ) ;
#38215 = CARTESIAN_POINT ( 'NONE',  ( 10.12767167105699961, -4.855035690642299784, 7.356396684460199786 ) ) ;
#38217 = CARTESIAN_POINT ( 'NONE',  ( 10.91080643070814205, 2.803404389955949760, -6.850777194058569997 ) ) ;
#38218 = EDGE_LOOP ( 'NONE', ( #18331, #51562, #59534, #12302 ) ) ;
#38219 = B_SPLINE_CURVE_WITH_KNOTS ( 'NONE', 3,
 ( #36708, #63253, #46851, #10812, #68847, #20274 ),
 .UNSPECIFIED., .F., .F.,
 ( 4, 2, 4 ),
 ( 0.000000000000000000, 0.5000000000000000000, 1.000000000000000000 ),
 .UNSPECIFIED. ) ;
#38220 = EDGE_CURVE ( 'NONE', #40403, #19021, #6220, .T. ) ;
#38221 = CARTESIAN_POINT ( 'NONE',  ( 11.26723293495529887, 2.826061044294000180, 7.547192037433419820 ) ) ;
#38222 = CARTESIAN_POINT ( 'NONE',  ( 7.799092354096995194, -3.518505934209000152, 6.398021147088998717 ) ) ;
#38223 = CARTESIAN_POINT ( 'NONE',  ( 10.36624205625100004, 3.590523439766200031, 6.434137271007999814 ) ) ;
#38224 = CARTESIAN_POINT ( 'NONE',  ( 11.09999999999999964, 5.556627878592999004, -5.124965741051999757 ) ) ;
#38225 = CARTESIAN_POINT ( 'NONE',  ( 10.84168850528999961, -2.681008214828000114, 6.554752254946000889 ) ) ;
#38226 = DIRECTION ( 'NONE',  ( 0.000000000000000000, -0.5000000000000169864, 0.8660254037844288266 ) ) ;
#38227 = LINE ( 'NONE', #8746, #55523 ) ;
#38228 = B_SPLINE_CURVE_WITH_KNOTS ( 'NONE', 3,
 ( #37507, #58487, #25991, #5687, #6031, #26339, #21764, #63380, #10939, #15155, #42417, #68279, #41723, #68977, #63723, #5348, #43101, #64403, #53243, #53928 ),
 .UNSPECIFIED., .F., .F.,
 ( 4, 2, 2, 2, 2, 2, 2, 2, 2, 4 ),
 ( 0.5011597829110069346, 0.5050569721070143903, 0.5089541613030218459, 0.5167485396950372012, 0.5323372964790684669, 0.5635148100471309984, 0.5946923236151935299, 0.6258698371832560614, 0.7505798914555037449, 1.000000000000000000 ),
 .UNSPECIFIED. ) ;
#38229 = CARTESIAN_POINT ( 'NONE',  ( 9.989267173155999657, -4.764472860199700399, -6.848522029265999400 ) ) ;
#38230 = AXIS2_PLACEMENT_3D ( 'NONE', #6678, #65048, #1443 ) ;
#38231 = CARTESIAN_POINT ( 'NONE',  ( 5.829360824503000416, -0.8123280412348000690, -1.043359539020999982 ) ) ;
#38232 = DIRECTION ( 'NONE',  ( 0.000000000000000000, 0.9659258262890757507, 0.2588190451024934835 ) ) ;
#38233 = CARTESIAN_POINT ( 'NONE',  ( 24.56351374471499938, -3.482977112968999922, 12.16506632497999973 ) ) ;
#38234 = CARTESIAN_POINT ( 'NONE',  ( 12.03979707368350027, -4.430269712815499972, 8.251775607861899786 ) ) ;
#38235 = CARTESIAN_POINT ( 'NONE',  ( 11.41672066707849886, 4.741156262620799922, -7.051685395375099752 ) ) ;
#38236 = CARTESIAN_POINT ( 'NONE',  ( 8.214872468085966162, -2.885034057788420370, 6.708591534144135338 ) ) ;
#38237 = DIRECTION ( 'NONE',  ( 1.000000000000000000, 0.000000000000000000, 0.000000000000000000 ) ) ;
#38238 = CARTESIAN_POINT ( 'NONE',  ( 29.60000000000000142, 0.000000000000000000, 0.000000000000000000 ) ) ;
#38239 = VERTEX_POINT ( 'NONE', #9757 ) ;
#38240 = CARTESIAN_POINT ( 'NONE',  ( 7.517309937294106348, -5.180920709765818088, 8.180401817406641740 ) ) ;
#38241 = ITEM_DEFINED_TRANSFORMATION ( 'NONE', 'NONE', #40732,  #9676 ) ;
#38242 = B_SPLINE_CURVE_WITH_KNOTS ( 'NONE', 3,
 ( #8019, #13617, #29357, #8363, #45767, #67075, #19188, #36993, #36646, #31751 ),
 .UNSPECIFIED., .F., .F.,
 ( 4, 2, 2, 2, 4 ),
 ( 0.3934091950370091628, 0.5450568962777566639, 0.6967045975185042206, 0.8483522987592517772, 1.000000000000000000 ),
 .UNSPECIFIED. ) ;
#38243 = CARTESIAN_POINT ( 'NONE',  ( 10.93990547754509812, -2.967013601007999934, -7.532784233952049213 ) ) ;
#38244 = CARTESIAN_POINT ( 'NONE',  ( 11.09999999999999964, -2.700000000000000178, 5.160242730440000258 ) ) ;
#38245 = CARTESIAN_POINT ( 'NONE',  ( 10.47934687351612659, -3.836375382625532904, 6.249999999999999112 ) ) ;
#38246 = DIRECTION ( 'NONE',  ( 0.000000000000000000, 1.000000000000000000, 0.000000000000000000 ) ) ;
#38248 = VECTOR ( 'NONE', #66189, 999.9999999999998863 ) ;
#38247 = CARTESIAN_POINT ( 'NONE',  ( 13.73682146000800053, 12.29517900649999973, 2.580790095973999776 ) ) ;
#38249 = ORIENTED_EDGE ( 'NONE', *, *, #40725, .T. ) ;
#38250 = CARTESIAN_POINT ( 'NONE',  ( 18.08663229464169930, 2.829323725363764641, -13.59808899811970484 ) ) ;
#38251 = ORIENTED_EDGE ( 'NONE', *, *, #2827, .F. ) ;
#38252 = CARTESIAN_POINT ( 'NONE',  ( 12.79999998712400178, 11.53033693765999779, -4.891431908114999949 ) ) ;
#38253 = CARTESIAN_POINT ( 'NONE',  ( 11.09999868801999945, 0.5000013103249000279, -9.776630274038000223 ) ) ;
#38254 = CARTESIAN_POINT ( 'NONE',  ( 15.56012107570600023, 8.822147194309000184, 7.967418575816001436 ) ) ;
#38255 = EDGE_CURVE ( 'NONE', #62822, #28970, #64673, .T. ) ;
#38256 = ORIENTED_EDGE ( 'NONE', *, *, #2140, .F. ) ;
#38257 = CARTESIAN_POINT ( 'NONE',  ( 0.000000000000000000, 2.899969545325999931, -0.3811992978302039536 ) ) ;
#38258 = EDGE_CURVE ( 'NONE', #67742, #65964, #29578, .T. ) ;
#38259 = CARTESIAN_POINT ( 'NONE',  ( 17.67418791246058873, 1.797344534875185529, -13.88414834504120599 ) ) ;
#38260 = CARTESIAN_POINT ( 'NONE',  ( 8.061185841224999038, 2.494419548310999879, -8.658783402411998509 ) ) ;
#38261 = CARTESIAN_POINT ( 'NONE',  ( 9.906851002540999929, -2.832432432432000269, -6.822293592207000934 ) ) ;
#38262 = EDGE_CURVE ( 'NONE', #5496, #68419, #16265, .T. ) ;
#38263 = CARTESIAN_POINT ( 'NONE',  ( 9.525000000000000355, 4.417172942406000224, 8.783926296998000538 ) ) ;
#38264 = ORIENTED_EDGE ( 'NONE', *, *, #66773, .T. ) ;
#38265 = CARTESIAN_POINT ( 'NONE',  ( 10.90374822854000136, -3.726845778959999578, 5.900452123196999743 ) ) ;
#38266 = CARTESIAN_POINT ( 'NONE',  ( 11.60000000000000142, 3.430179236374870655, 8.269794803757207546 ) ) ;
#38267 = CARTESIAN_POINT ( 'NONE',  ( 11.27769289846838241, 2.954326301843319680, 7.175017342370984430 ) ) ;
#38268 = VERTEX_POINT ( 'NONE', #45298 ) ;
#38269 = CARTESIAN_POINT ( 'NONE',  ( 6.252943173016667799, 1.199500263597271577, -0.9218200799623702535 ) ) ;
#38270 = CARTESIAN_POINT ( 'NONE',  ( 10.38725444037999956, -2.888666857901000196, -6.716331201355000502 ) ) ;
#38271 = ORIENTED_EDGE ( 'NONE', *, *, #43349, .F. ) ;
#38272 = CARTESIAN_POINT ( 'NONE',  ( 9.987254614702999689, 2.893436332050999926, 7.218483930889299849 ) ) ;
#38273 = FACE_OUTER_BOUND ( 'NONE', #34471, .T. ) ;
#38274 = CARTESIAN_POINT ( 'NONE',  ( 4.453300434508999928, -0.3367241447620000216, 1.520685311087999869 ) ) ;
#38275 = CARTESIAN_POINT ( 'NONE',  ( 11.60000000000000142, 4.187315255316414131, -6.446733142248666226 ) ) ;
#38276 = CARTESIAN_POINT ( 'NONE',  ( 24.67921580255100267, 8.727633792449999817, 9.158312800479000870 ) ) ;
#38277 = CARTESIAN_POINT ( 'NONE',  ( 9.393077698596744796, 2.713274643879884263, -7.026852155855150883 ) ) ;
#38278 = B_SPLINE_SURFACE_WITH_KNOTS ( 'NONE', 3, 3, ( 
 ( #49126, #12422, #43199, #12770 ),
 ( #43546, #28155, #33054, #64846 ),
 ( #34096, #6473, #49469, #22209 ),
 ( #7509, #28508, #43893, #22898 ),
 ( #48789, #18018, #49822, #23254 ),
 ( #54721, #44596, #65196, #65889 ),
 ( #37946, #11714, #59268, #17315 ),
 ( #27463, #38640, #16957, #11371 ) ),
 .UNSPECIFIED., .F., .F., .F.,
 ( 4, 1, 1, 1, 1, 4 ),
 ( 4, 4 ),
 ( 0.008355857670640998852, 0.05882352941176000050, 0.1176470588234999892, 0.1764705882353000133, 0.2352941176471000095, 0.2534691232731000055 ),
 ( -0.1830855917210000017, 1.182949831419999986 ),
 .UNSPECIFIED. ) ;
#38279 = CARTESIAN_POINT ( 'NONE',  ( 10.19190035061499877, 4.267716286314199969, 6.531924610394499453 ) ) ;
#38280 = CARTESIAN_POINT ( 'NONE',  ( 9.339877582927117672, -3.667929758882994218, 9.210246940688463724 ) ) ;
#38281 = ORIENTED_EDGE ( 'NONE', *, *, #31262, .T. ) ;
#38282 = DIRECTION ( 'NONE',  ( 1.000000000000000000, 0.000000000000000000, 0.000000000000000000 ) ) ;
#38283 = CARTESIAN_POINT ( 'NONE',  ( 5.599999999407000217, -1.300000000000000044, -9.662944685757000940 ) ) ;
#38284 = CARTESIAN_POINT ( 'NONE',  ( 10.64393020684969926, 5.250000000000000000, -7.500000000000000000 ) ) ;
#38285 = CARTESIAN_POINT ( 'NONE',  ( 12.18118526251762646, 2.542711865659281312, -13.66432766657963427 ) ) ;
#38286 = AXIS2_PLACEMENT_3D ( 'NONE', #33938, #56293, #2122 ) ;
#38287 = DIRECTION ( 'NONE',  ( 1.000000000000000000, 0.000000000000000000, 0.000000000000000000 ) ) ;
#38288 = CARTESIAN_POINT ( 'NONE',  ( 11.08492081570999943, -3.668392767032000013, 5.558160538745999801 ) ) ;
#38289 = CARTESIAN_POINT ( 'NONE',  ( 5.500000000000000000, 12.65263727151999795, -3.063503113339999917 ) ) ;
#38290 = DIRECTION ( 'NONE',  ( 0.000000000000000000, 1.000000000000000000, 0.000000000000000000 ) ) ;
#38291 = ORIENTED_EDGE ( 'NONE', *, *, #44232, .F. ) ;
#38292 = ORIENTED_EDGE ( 'NONE', *, *, #61788, .T. ) ;
#38293 = CARTESIAN_POINT ( 'NONE',  ( 10.07770645819999977, 4.622041375574999833, 5.671348593713000596 ) ) ;
#38294 = CARTESIAN_POINT ( 'NONE',  ( 12.24298788041087782, -0.2740979068391591889, 13.89637745338051111 ) ) ;
#38295 = CARTESIAN_POINT ( 'NONE',  ( 12.30787805051431150, -0.3788776035274156184, -13.89305317345212032 ) ) ;
#38296 = CARTESIAN_POINT ( 'NONE',  ( 11.00000000000000000, -2.920245322398999921, -7.825000000000000178 ) ) ;
#38297 = FACE_OUTER_BOUND ( 'NONE', #56315, .T. ) ;
#38298 = CARTESIAN_POINT ( 'NONE',  ( 9.026933059621999433, -4.852736108563000528, 8.683927195503999386 ) ) ;
#38299 = DIRECTION ( 'NONE',  ( -1.000000000000000000, 0.000000000000000000, 0.000000000000000000 ) ) ;
#38301 = CARTESIAN_POINT ( 'NONE',  ( 9.716851002543000604, 2.832432432432000269, 6.822293592207000934 ) ) ;
#38300 = CARTESIAN_POINT ( 'NONE',  ( 9.804430433047000903, -5.088604610742000212, 8.171806809244198888 ) ) ;
#38302 = PRESENTATION_LAYER_ASSIGNMENT (  '', '', ( #62845 ) ) ;
#38303 = CARTESIAN_POINT ( 'NONE',  ( 10.29657053952199952, 3.497746311184500190, -6.324815923923999605 ) ) ;
#38304 = CARTESIAN_POINT ( 'NONE',  ( 24.40628504395400000, -8.880942544344001988, -9.006432928708999697 ) ) ;
#38305 = EDGE_CURVE ( 'NONE', #52369, #21254, #44619, .T. ) ;
#38306 = CARTESIAN_POINT ( 'NONE',  ( 8.457129882803000598, 5.100036551512999949, -6.571411952062999440 ) ) ;
#38307 = CARTESIAN_POINT ( 'NONE',  ( 18.06882650195507978, -0.3560396104572058906, 12.69328656575055980 ) ) ;
#38308 = CARTESIAN_POINT ( 'NONE',  ( 6.999999691988000095, -12.36734761319999798, -2.759114534468000368 ) ) ;
#38309 = EDGE_CURVE ( 'NONE', #38790, #38001, #23831, .T. ) ;
#38310 = CARTESIAN_POINT ( 'NONE',  ( 24.51193477385900010, 8.843600298101000234, 9.168347890893999264 ) ) ;
#38311 = ORIENTED_EDGE ( 'NONE', *, *, #30658, .T. ) ;
#38312 = CARTESIAN_POINT ( 'NONE',  ( 8.032370559622998840, -3.524751762020000179, 5.573845465339999805 ) ) ;
#38313 = CARTESIAN_POINT ( 'NONE',  ( 8.275189158773001097, 3.061731693614000438, -8.535706278603999664 ) ) ;
#38314 = CARTESIAN_POINT ( 'NONE',  ( 11.09999965054999826, -2.398081733189999864E-14, -12.24999851416000141 ) ) ;
#38315 = CARTESIAN_POINT ( 'NONE',  ( 23.89320776801300283, 8.313844348326997036, -8.526065359053994541 ) ) ;
#38316 = CARTESIAN_POINT ( 'NONE',  ( 0.5761782687131999925, -3.296907118028000294, 0.7152224222591000435 ) ) ;
#38317 = CARTESIAN_POINT ( 'NONE',  ( 10.90346005378009941, 4.786957292481900161, 7.920222357891399945 ) ) ;
#38318 = CARTESIAN_POINT ( 'NONE',  ( 11.18237334122999904, 4.516636732814999888, -8.757876389238999693 ) ) ;
#38319 = EDGE_LOOP ( 'NONE', ( #52063, #33631, #9723, #51016 ) ) ;
#38320 = CARTESIAN_POINT ( 'NONE',  ( 12.10797143991210767, -0.1980440493285478276, -12.59844852634975254 ) ) ;
#38321 = CARTESIAN_POINT ( 'NONE',  ( 8.999999001754000361, 0.000000000000000000, 0.000000000000000000 ) ) ;
#38322 = CARTESIAN_POINT ( 'NONE',  ( 18.24534165125340479, 2.701041880525440586, -12.30709158425920613 ) ) ;
#38323 = DIRECTION ( 'NONE',  ( 1.000000000000000000, 0.000000000000000000, 0.000000000000000000 ) ) ;
#38324 = CARTESIAN_POINT ( 'NONE',  ( 7.448642219589999947, 4.628941086829000184, 5.991667691044999522 ) ) ;
#38325 = ORIENTED_EDGE ( 'NONE', *, *, #10392, .F. ) ;
#38326 = CARTESIAN_POINT ( 'NONE',  ( 6.385387840465999609, 0.9584732047324999726, 1.299486219972000089 ) ) ;
#38327 = B_SPLINE_CURVE_WITH_KNOTS ( 'NONE', 3,
 ( #61630, #13746, #66871, #35416 ),
 .UNSPECIFIED., .F., .F.,
 ( 4, 4 ),
 ( 0.000000000000000000, 1.000000000000000000 ),
 .UNSPECIFIED. ) ;
#38328 = CIRCLE ( 'NONE', #8199, 2.000000000000000888 ) ;
#38329 = CARTESIAN_POINT ( 'NONE',  ( 7.996695280407001505, 5.564823112884000444, -7.478368060284999785 ) ) ;
#38331 = CARTESIAN_POINT ( 'NONE',  ( 10.52323372634000087, 3.325642821414999784, 5.689987891230000372 ) ) ;
#38330 = CARTESIAN_POINT ( 'NONE',  ( 8.380713240912069040, -2.878415775774842533, 8.829883092763182617 ) ) ;
#38332 = CARTESIAN_POINT ( 'NONE',  ( 13.92020863221766902, 9.472241403191404174, 8.194648738509947350 ) ) ;
#38333 = ORIENTED_EDGE ( 'NONE', *, *, #7398, .F. ) ;
#38334 = CARTESIAN_POINT ( 'NONE',  ( 17.10000000000000142, 3.283787102340999464, 11.28049554847999936 ) ) ;
#38335 =( NAMED_UNIT ( * ) PLANE_ANGLE_UNIT ( ) SI_UNIT ( $, .RADIAN. ) );
#38336 = EDGE_LOOP ( 'NONE', ( #26409, #17575, #2463, #47416 ) ) ;
#38337 = CARTESIAN_POINT ( 'NONE',  ( 24.56711102116320689, 3.188703611083238965, -11.92333255138484560 ) ) ;
#38338 = CARTESIAN_POINT ( 'NONE',  ( 16.39956681845000119, 3.250692199830000018, 11.33777344299000056 ) ) ;
#38339 = CARTESIAN_POINT ( 'NONE',  ( 17.65055117253431050, 0.7242550212506057017, -13.98125389334239443 ) ) ;
#38340 = ORIENTED_EDGE ( 'NONE', *, *, #29066, .T. ) ;
#38341 = CARTESIAN_POINT ( 'NONE',  ( 10.54640350404223526, -2.480438647385216022, -8.419559847284382670 ) ) ;
#38342 = EDGE_CURVE ( 'NONE', #50218, #25777, #2977, .T. ) ;
#38343 = CARTESIAN_POINT ( 'NONE',  ( 17.60000003185799855, -12.11983897296999935, 3.159727888982000188 ) ) ;
#38344 = CARTESIAN_POINT ( 'NONE',  ( 8.200000998245998929, 0.000000000000000000, 0.000000000000000000 ) ) ;
#38345 = CARTESIAN_POINT ( 'NONE',  ( 11.37299956498129916, 2.792989229543000107, -7.174999999999999822 ) ) ;
#38346 = EDGE_CURVE ( 'NONE', #7896, #27999, #57122, .T. ) ;
#38347 = CARTESIAN_POINT ( 'NONE',  ( 11.09195391537400077, -2.942766577210000012, 6.781965272201699868 ) ) ;
#38348 = ORIENTED_EDGE ( 'NONE', *, *, #9080, .T. ) ;
#38349 = CARTESIAN_POINT ( 'NONE',  ( 8.705989158774000813, 2.542862824481000317, 7.419808961972999661 ) ) ;
#38350 = EDGE_CURVE ( 'NONE', #53307, #14947, #65414, .T. ) ;
#38351 = CARTESIAN_POINT ( 'NONE',  ( 17.57920308108771934, -1.787817001021373420, 13.88537754104227417 ) ) ;
#38352 = VERTEX_POINT ( 'NONE', #33774 ) ;
#38353 = CARTESIAN_POINT ( 'NONE',  ( 10.08351354018333446, -2.750000000000000000, 7.336375382625531572 ) ) ;
#38354 = CARTESIAN_POINT ( 'NONE',  ( 15.47616489729399980, -9.395071224208001226, -8.199988963223999505 ) ) ;
#38355 = B_SPLINE_CURVE_WITH_KNOTS ( 'NONE', 3,
 ( #30255, #14170, #9591, #67288, #40729, #62054 ),
 .UNSPECIFIED., .F., .F.,
 ( 4, 1, 1, 4 ),
 ( 0.000000000000000000, 0.3333333333333000081, 0.6666666666667000474, 1.000000000000000000 ),
 .UNSPECIFIED. ) ;
#38356 = CARTESIAN_POINT ( 'NONE',  ( 11.07074946250000025, 5.433303208544999485, -5.078292924949999509 ) ) ;
#38357 = VERTEX_POINT ( 'NONE', #56119 ) ;
#38358 = CARTESIAN_POINT ( 'NONE',  ( 12.18110988575103804, -2.462234709496985641, -12.46028276222759423 ) ) ;
#38359 = VECTOR ( 'NONE', #53511, 1000.000000000000000 ) ;
#38360 = CARTESIAN_POINT ( 'NONE',  ( 10.72934687351609639, 3.836375382625535124, -6.249999999999999112 ) ) ;
#38361 = CARTESIAN_POINT ( 'NONE',  ( 7.441372165042849041, 4.549423936828223880, -9.274025057497155444 ) ) ;
#38362 = CARTESIAN_POINT ( 'NONE',  ( 11.95284386393252873, -3.097320422761385750, 7.824986766837089824 ) ) ;
#38363 = CARTESIAN_POINT ( 'NONE',  ( 12.08963668261109525, -2.638435792642062960, -13.74915318082108939 ) ) ;
#38364 = CARTESIAN_POINT ( 'NONE',  ( 11.33456651104149948, -3.887457492043800311, -6.364824110469998963 ) ) ;
#38365 = DIRECTION ( 'NONE',  ( 0.8660254037844288266, 0.000000000000000000, -0.5000000000000169864 ) ) ;
#38366 = CARTESIAN_POINT ( 'NONE',  ( 17.72222400754431249, -1.779821952440184818, 12.47366250980180524 ) ) ;
#38367 = ORIENTED_EDGE ( 'NONE', *, *, #35845, .F. ) ;
#38368 = CARTESIAN_POINT ( 'NONE',  ( 25.44993529014200107, -2.258942858049999725, 12.29419282279000036 ) ) ;
#38369 = EDGE_LOOP ( 'NONE', ( #62617, #595, #65444 ) ) ;
#38370 = EDGE_CURVE ( 'NONE', #26690, #56577, #41291, .T. ) ;
#38371 = CARTESIAN_POINT ( 'NONE',  ( 11.53944595909000270, -12.46266292589999836, -1.587625155185000025 ) ) ;
#38372 = CARTESIAN_POINT ( 'NONE',  ( 9.883629719592001095, 5.656948148960999845, -6.994239053114000626 ) ) ;
#38373 = CARTESIAN_POINT ( 'NONE',  ( 10.68055531501999944, 2.768167480619000198, -6.114404645958000373 ) ) ;
#38374 = CARTESIAN_POINT ( 'NONE',  ( 9.741009892375998902, -3.588529236307000048, -8.800227248412999970 ) ) ;
#38375 = CARTESIAN_POINT ( 'NONE',  ( 11.73052404082913469, -5.045680872279848295, 7.824990945864982450 ) ) ;
#38376 = CARTESIAN_POINT ( 'NONE',  ( 24.23191122837300426, 12.46786376384999961, 3.269411384671000231 ) ) ;
#38377 = CARTESIAN_POINT ( 'NONE',  ( 17.60000000024299993, 11.86189249994999884, -3.298671769835999967 ) ) ;
#38378 = VERTEX_POINT ( 'NONE', #59172 ) ;
#38379 = DIRECTION ( 'NONE',  ( -1.000000000000000000, 0.000000000000000000, 0.000000000000000000 ) ) ;
#38380 = CARTESIAN_POINT ( 'NONE',  ( 10.40227026081000083, 2.765684886876999649, 9.035354958280999327 ) ) ;
#38381 = B_SPLINE_CURVE_WITH_KNOTS ( 'NONE', 3,
 ( #15079, #37432, #37098, #58754, #5607, #68548 ),
 .UNSPECIFIED., .F., .F.,
 ( 4, 2, 4 ),
 ( 0.000000000000000000, 0.5000000000000000000, 1.000000000000000000 ),
 .UNSPECIFIED. ) ;
#38382 = CARTESIAN_POINT ( 'NONE',  ( 2.123890132542666453, 2.150913519912194261, 2.798833948393636195 ) ) ;
#38383 = CARTESIAN_POINT ( 'NONE',  ( 18.43348807395470956, -2.701964790437650255, 11.40102144998400213 ) ) ;
#38384 = CARTESIAN_POINT ( 'NONE',  ( 17.96012107570599881, 3.168891391480999520, -11.45723209283999999 ) ) ;
#38385 = CIRCLE ( 'NONE', #20518, 1.350000000000000533 ) ;
#38386 = CARTESIAN_POINT ( 'NONE',  ( 10.30903300763299946, 4.597717337857299746, -8.126922218169600143 ) ) ;
#38387 = CARTESIAN_POINT ( 'NONE',  ( 7.100000000000070699, 4.845481125806140099, -8.600290376098520539 ) ) ;
#38388 = CARTESIAN_POINT ( 'NONE',  ( 23.64143804138000249, -10.11749648602000029, -9.385403416437998914 ) ) ;
#38389 = CARTESIAN_POINT ( 'NONE',  ( 24.51038808216000220, -8.845036404463000324, 9.169859949269000055 ) ) ;
#38390 = CARTESIAN_POINT ( 'NONE',  ( 24.62620337099072998, 3.584633747643987345, -12.20158770655988789 ) ) ;
#38391 = EDGE_CURVE ( 'NONE', #31887, #66938, #17128, .T. ) ;
#38392 = ORIENTED_EDGE ( 'NONE', *, *, #14993, .T. ) ;
#38393 = CARTESIAN_POINT ( 'NONE',  ( 8.622785841227999626, 5.189036231907000030, -8.048606212067999977 ) ) ;
#38394 = CARTESIAN_POINT ( 'NONE',  ( 7.094619556280000516, 1.049447144279999966, -0.6801946707396000491 ) ) ;
#38395 = CARTESIAN_POINT ( 'NONE',  ( 18.14812703077569367, 2.302545424703879462, 13.71331074879213219 ) ) ;
#38396 = DIRECTION ( 'NONE',  ( 1.000000000000000000, 0.000000000000000000, 0.000000000000000000 ) ) ;
#38397 = CARTESIAN_POINT ( 'NONE',  ( 10.93656785386839836, -5.060279460151999587, -8.213529149347399638 ) ) ;
#38398 = ORIENTED_EDGE ( 'NONE', *, *, #12499, .T. ) ;
#38399 =( GEOMETRIC_REPRESENTATION_CONTEXT ( 3 ) GLOBAL_UNCERTAINTY_ASSIGNED_CONTEXT ( ( #23879 ) ) GLOBAL_UNIT_ASSIGNED_CONTEXT ( ( #62404, #66619, #25167 ) ) REPRESENTATION_CONTEXT ( 'NONE', 'WORKASPACE' ) );
#38400 = CARTESIAN_POINT ( 'NONE',  ( 25.08547525503900033, 2.791087243097000403, -11.47628568378999958 ) ) ;
#38401 = CARTESIAN_POINT ( 'NONE',  ( 8.181107780410998842, 5.485785046334999748, 8.532070739720001740 ) ) ;
#38402 = AXIS2_PLACEMENT_3D ( 'NONE', #61729, #12466, #33452 ) ;
#38404 = CARTESIAN_POINT ( 'NONE',  ( 11.30000000000000071, -18.88101580703000337, -3.105963843451999828 ) ) ;
#38403 = CARTESIAN_POINT ( 'NONE',  ( 9.898395280408998076, 3.987760651117999711, -9.123263301387000368 ) ) ;
#38405 = LINE ( 'NONE', #27234, #1179 ) ;
#38406 = VERTEX_POINT ( 'NONE', #6368 ) ;
#38407 = CARTESIAN_POINT ( 'NONE',  ( 10.11260611051000069, 3.359887741436999864, 5.859127722154000573 ) ) ;
#38408 = CARTESIAN_POINT ( 'NONE',  ( 18.18532329594574648, -2.156378744708864925, -13.83294935661368363 ) ) ;
#38409 = CARTESIAN_POINT ( 'NONE',  ( 10.99410672858429905, 3.198097575668700010, 8.103244025831999764 ) ) ;
#38410 = CARTESIAN_POINT ( 'NONE',  ( 9.924739995124999936, -5.060461104229999840, 8.686133300732999274 ) ) ;
#38411 = CARTESIAN_POINT ( 'NONE',  ( 8.434803823919004628, 2.901237182992001173, 6.624660446101000133 ) ) ;
#38413 = VERTEX_POINT ( 'NONE', #38895 ) ;
#38412 = AXIS2_PLACEMENT_3D ( 'NONE', #34734, #29150, #2559 ) ;
#38414 = CARTESIAN_POINT ( 'NONE',  ( 8.099999999999999645, -12.35000000006999876, 0.000000000000000000 ) ) ;
#38416 = CARTESIAN_POINT ( 'NONE',  ( 11.11478185320999934, -2.548220588762000194, -8.356740464335999263 ) ) ;
#38415 = CARTESIAN_POINT ( 'NONE',  ( 12.79342929296800158, -12.04986812289999953, 3.196648259943000170 ) ) ;
#38417 = CARTESIAN_POINT ( 'NONE',  ( 7.898434181710118906, -2.601011730887146989, 8.533201786423413537 ) ) ;
#38418 = CARTESIAN_POINT ( 'NONE',  ( 9.285188841453999586, -5.269672295101000437, 8.747824102203999530 ) ) ;
#38419 = CARTESIAN_POINT ( 'NONE',  ( 11.76077869730539938, -4.595338376575799799, -6.326049646822999861 ) ) ;
#38420 = ORIENTED_EDGE ( 'NONE', *, *, #23940, .T. ) ;
#38421 = CARTESIAN_POINT ( 'NONE',  ( 6.949999692291999764, -2.604139126561000230E-12, 1.310063169058000104E-14 ) ) ;
#38422 = CARTESIAN_POINT ( 'NONE',  ( 11.85918179236250047, -4.238363971154499588, 8.615559381441000752 ) ) ;
#38423 = CARTESIAN_POINT ( 'NONE',  ( 8.160036350658002036, 2.891230335795000883, 6.361714733157999291 ) ) ;
#38424 = CARTESIAN_POINT ( 'NONE',  ( 11.33041235500449950, 3.057642534728299832, 8.363295307663500822 ) ) ;
#38425 = ORIENTED_EDGE ( 'NONE', *, *, #13886, .F. ) ;
#38426 = B_SPLINE_SURFACE_WITH_KNOTS ( 'NONE', 3, 3, ( 
 ( #64198, #53724, #11753, #28193, #65238, #33790, #17353, #55106, #54412, #60002, #11408, #43235, #7212, #1621, #38326, #49508, #1276, #12113, #16999, #49163, #27501, #22246, #240, #12457, #22936, #44288, #33441, #58970, #16656, #588, #21897, #64539, #37982, #65586, #27160 ),
 ( #38681, #48136, #54757, #21555, #6512, #6856, #32747, #59306, #42891, #17711, #59656, #39034, #22591, #60349, #33095, #43933, #48827, #43584, #16313, #11074, #32409, #5821, #48481, #54063, #6160, #936, #64885, #27857, #18397, #51237, #7549, #18055, #45657, #39372, #44635 ),
 ( #65927, #40397, #60691, #28903, #2651, #39723, #67300, #13162, #7903, #3334, #66275, #34490, #50895, #34825, #35508, #14180, #18743, #61720, #62066, #66964, #13839, #56137, #12808, #34137, #55801, #44971, #45988, #24667, #23979, #8245, #50551, #55454, #24324, #29241, #19417 ),
 ( #45314, #66621, #29933, #28549, #56828, #61385, #40074, #61041, #35169, #40741, #13505, #50210, #2990, #19070, #2311, #23633, #29592, #56481, #8585, #49859, #1972, #23294, #4008, #15202, #26388, #4697, #26040, #47369, #41773, #46685, #51912, #42464, #4358, #47023, #20105 ) ),
 .UNSPECIFIED., .F., .F., .F.,
 ( 4, 4 ),
 ( 4, 1, 1, 1, 1, 1, 1, 1, 1, 1, 1, 1, 1, 1, 1, 1, 1, 1, 1, 1, 1, 1, 1, 1, 1, 1, 1, 1, 1, 1, 1, 1, 4 ),
 ( -0.02636945251836000231, 1.026369452518000047 ),
 ( -0.02000000000000000042, 0.01250000000000000069, 0.04499999999999999833, 0.07749999999999999944, 0.1100000000000000006, 0.1424999999999999878, 0.1749999999999999889, 0.2074999999999999900, 0.2399999999999999911, 0.2725000000000000200, 0.3049999999999999933, 0.3375000000000000222, 0.3699999999999999956, 0.4025000000000000244, 0.4349999999999999978, 0.4675000000000000266, 0.5000000000000000000, 0.5324999999999999734, 0.5649999999999999467, 0.5975000000000000311, 0.6300000000000000044, 0.6624999999999999778, 0.6949999999999999512, 0.7275000000000000355, 0.7600000000000000089, 0.7924999999999999822, 0.8249999999999999556, 0.8575000000000000400, 0.8900000000000000133, 0.9224999999999999867, 0.9549999999999999600, 0.9875000000000000444, 1.020000000000000018 ),
 .UNSPECIFIED. ) ;
#38427 = CARTESIAN_POINT ( 'NONE',  ( 8.672989158774999652, 4.728328492779000136, -8.692725459657999920 ) ) ;
#38428 = CARTESIAN_POINT ( 'NONE',  ( 23.68333479628300253, 13.13544135902000143, -3.948726516682999677 ) ) ;
#38429 = CARTESIAN_POINT ( 'NONE',  ( 12.13037555192277850, 2.744322634620807388, -12.29751256722372865 ) ) ;
#38430 = EDGE_CURVE ( 'NONE', #30974, #66075, #411, .T. ) ;
#38431 = CARTESIAN_POINT ( 'NONE',  ( 11.55946005378019947, -2.963614890480000152, 8.053412743695298914 ) ) ;
#38432 = EDGE_CURVE ( 'NONE', #11189, #10274, #57999, .T. ) ;
#38433 = ORIENTED_EDGE ( 'NONE', *, *, #65999, .T. ) ;
#38434 = CARTESIAN_POINT ( 'NONE',  ( 9.106448366594660726, 5.179987832526970593, -8.180032552820186709 ) ) ;
#38435 = AXIS2_PLACEMENT_3D ( 'NONE', #57556, #20503, #62459 ) ;
#38436 = LINE ( 'NONE', #61409, #31656 ) ;
#38437 = ORIENTED_EDGE ( 'NONE', *, *, #55010, .T. ) ;
#38438 = CARTESIAN_POINT ( 'NONE',  ( 8.560879440379000727, -4.228293421747000735, 8.941387937291999322 ) ) ;
#38439 = CARTESIAN_POINT ( 'NONE',  ( 5.607109839683542596, -1.199500263597270244, -0.9218200799623728070 ) ) ;
#38440 = ORIENTED_EDGE ( 'NONE', *, *, #21523, .F. ) ;
#38441 = CARTESIAN_POINT ( 'NONE',  ( 10.08525341940465303, -2.214675259024396770, -7.596661910983709021 ) ) ;
#38442 = CARTESIAN_POINT ( 'NONE',  ( 10.89564560330029863, 4.307504762655200103, 8.455191956516999952 ) ) ;
#38443 = CARTESIAN_POINT ( 'NONE',  ( 10.79702055961999818, -5.792859009854000263, -7.049265738992000152 ) ) ;
#38444 = CARTESIAN_POINT ( 'NONE',  ( 11.04497253829999970, 2.754551879881000254, -5.177000083688999332 ) ) ;
#38445 = CARTESIAN_POINT ( 'NONE',  ( 18.46719854810600125, -11.76170593772999950, 4.414464320434000832 ) ) ;
#38446 = CARTESIAN_POINT ( 'NONE',  ( 9.232128830620874638, 3.792804146276640864, -6.256996123608767668 ) ) ;
#38447 = CARTESIAN_POINT ( 'NONE',  ( 13.82798078375900275, 9.420238147574000465, 8.170996254510999535 ) ) ;
#38448 = CARTESIAN_POINT ( 'NONE',  ( 18.15028814309356164, -0.1908418880314467214, -12.69807545005481053 ) ) ;
#38449 = CARTESIAN_POINT ( 'NONE',  ( 12.21592886438546977, 2.708773148307667356, -12.40049785801472737 ) ) ;
#38450 = CARTESIAN_POINT ( 'NONE',  ( 10.12841772631199966, -3.509411006705700053, -8.509834072393999804 ) ) ;
#38451 = CARTESIAN_POINT ( 'NONE',  ( 8.417489158772999858, 2.029098103856999735, 7.726995416028000108 ) ) ;
#38452 = ORIENTED_EDGE ( 'NONE', *, *, #52920, .T. ) ;
#38453 = EDGE_CURVE ( 'NONE', #2543, #46546, #47102, .T. ) ;
#38454 = AXIS2_PLACEMENT_3D ( 'NONE', #4630, #58809, #68601 ) ;
#38455 =( NAMED_UNIT ( * ) SI_UNIT ( $, .STERADIAN. ) SOLID_ANGLE_UNIT ( ) );
#38456 = CARTESIAN_POINT ( 'NONE',  ( 8.228368194306998618, -4.806758213702000404, 6.177034600996000435 ) ) ;
#38457 = LINE ( 'NONE', #65363, #47250 ) ;
#38458 = CARTESIAN_POINT ( 'NONE',  ( 11.35563386585000067, 12.29158615273999899, 1.473028240582999970 ) ) ;
#38459 = ADVANCED_FACE ( 'NONE', ( #40234 ), #45818, .T. ) ;
#38460 = CONICAL_SURFACE ( 'NONE', #52931, 1.700000581162000035, 0.7853984839373144844 ) ;
#38461 = CARTESIAN_POINT ( 'NONE',  ( 18.27481983568690183, 2.390134998303168778, 12.37124935920178714 ) ) ;
#38462 = CARTESIAN_POINT ( 'NONE',  ( 13.50000000000339639, -9.396284335645857411, -7.729197028970922645 ) ) ;
#38463 = CARTESIAN_POINT ( 'NONE',  ( 11.07076162495999938, 7.299628065904999019, 6.238550388720000228 ) ) ;
#38464 = CARTESIAN_POINT ( 'NONE',  ( 7.734298960010000279, -9.034081823845999892, -5.540645505838000417 ) ) ;
#38465 = B_SPLINE_CURVE_WITH_KNOTS ( 'NONE', 3,
 ( #32325, #22850, #60266, #7122, #27414, #48390, #33701, #1191, #22500 ),
 .UNSPECIFIED., .F., .F.,
 ( 4, 1, 2, 2, 4 ),
 ( 0.000000000000000000, 0.2499999999999994449, 0.3749999999999998335, 0.5000000000000002220, 1.000000000000000000 ),
 .UNSPECIFIED. ) ;
#38466 = DIRECTION ( 'NONE',  ( -1.000000000000000000, 0.000000000000000000, 0.000000000000000000 ) ) ;
#38467 = VERTEX_POINT ( 'NONE', #60865 ) ;
#38468 = CARTESIAN_POINT ( 'NONE',  ( 12.14412415395002398, -2.776584135961364108, 12.29026848248285475 ) ) ;
#38469 = CARTESIAN_POINT ( 'NONE',  ( 9.251759580228998914, -5.110528875107000601, -7.234556850645999404 ) ) ;
#38470 = CARTESIAN_POINT ( 'NONE',  ( 24.36504260745899941, -3.372670036896999513, -12.24415025393999912 ) ) ;
#38471 = CARTESIAN_POINT ( 'NONE',  ( 8.322761924339483031, 2.900588934367011706, -6.581379904120886692 ) ) ;
#38472 = CARTESIAN_POINT ( 'NONE',  ( 11.60533460557258323, 4.184174550317700358, -8.625775273268001087 ) ) ;
#38473 = CARTESIAN_POINT ( 'NONE',  ( 12.11827192994441482, -0.2307628456012699170, 12.59789151516662997 ) ) ;
#38474 = CARTESIAN_POINT ( 'NONE',  ( 8.817635841231000526, 3.894644548817000285, 6.044465307984999924 ) ) ;
#38475 = CARTESIAN_POINT ( 'NONE',  ( 9.215291255903000689, 4.861981595026999337, 8.938817176893000038 ) ) ;
#38476 = CARTESIAN_POINT ( 'NONE',  ( 12.57326805540220072, 3.080523641713201144, 12.29716358636311213 ) ) ;
#38477 = ORIENTED_EDGE ( 'NONE', *, *, #8071, .F. ) ;
#38478 = DIRECTION ( 'NONE',  ( -1.000000000000000000, 0.000000000000000000, -9.258974054407000394E-14 ) ) ;
#38479 = CARTESIAN_POINT ( 'NONE',  ( 10.76841504065829902, 4.914510326623699576, -6.818119527508899935 ) ) ;
#38480 = CARTESIAN_POINT ( 'NONE',  ( 17.78803358707871141, -0.6812425322175436060, 12.58157083403807164 ) ) ;
#38481 = CARTESIAN_POINT ( 'NONE',  ( 11.32240614981507854, 4.732436490098000270, 7.017906081141798147 ) ) ;
#38483 = CARTESIAN_POINT ( 'NONE',  ( 17.63846197668645743, -0.6206501420433685468, 12.67957965403709863 ) ) ;
#38482 = CARTESIAN_POINT ( 'NONE',  ( 8.086080172061008042, 4.921420473137001927, 6.235316328396007357 ) ) ;
#38484 = CARTESIAN_POINT ( 'NONE',  ( 10.97364560330029981, -3.734560974198899874, -6.675475461903199736 ) ) ;
#38485 = CARTESIAN_POINT ( 'NONE',  ( 10.97499895057999986, -2.398081733189999864E-14, 0.000000000000000000 ) ) ;
#38486 = ORIENTED_EDGE ( 'NONE', *, *, #62610, .T. ) ;
#38487 = VECTOR ( 'NONE', #51239, 1000.000000000000000 ) ;
#38488 = CARTESIAN_POINT ( 'NONE',  ( 2.200310191360999923, 2.483819732826999971, -1.905290611529000033 ) ) ;
#38489 = CARTESIAN_POINT ( 'NONE',  ( 18.29995268966800026, 2.861739928647000220, 11.98821236628000086 ) ) ;
#38490 = CARTESIAN_POINT ( 'NONE',  ( 12.25178171628779111, -12.07365382811727628, 3.333154641342844116 ) ) ;
#38491 = DIRECTION ( 'NONE',  ( 0.000000000000000000, 0.4998826579293299543, -0.8660931406618508355 ) ) ;
#38492 = CARTESIAN_POINT ( 'NONE',  ( 12.27274079034943455, -2.022162746929206278, 13.85319239000171265 ) ) ;
#38493 = CARTESIAN_POINT ( 'NONE',  ( 7.975339216757242333, 5.350090185752605976, 7.499980949462685231 ) ) ;
#38494 = CARTESIAN_POINT ( 'NONE',  ( 23.85180091069500108, 3.519844699246999831, -13.16782481969999807 ) ) ;
#38495 = CARTESIAN_POINT ( 'NONE',  ( 13.43590051321700152, -12.19118104410000036, -2.154281854449000555 ) ) ;
#38496 = ORIENTED_EDGE ( 'NONE', *, *, #66910, .F. ) ;
#38497 = DIRECTION ( 'NONE',  ( -1.000000000000000000, 0.000000000000000000, 0.000000000000000000 ) ) ;
#38498 = PLANE ( 'NONE',  #634 ) ;
#38499 = FACE_OUTER_BOUND ( 'NONE', #50019, .T. ) ;
#38500 = CARTESIAN_POINT ( 'NONE',  ( 12.80505043854144276, -0.7192913403693169672, -12.57945229203838267 ) ) ;
#38501 = CARTESIAN_POINT ( 'NONE',  ( 13.99999999308669629, -9.069400206872137105, -8.107642827045808076 ) ) ;
#38502 = CARTESIAN_POINT ( 'NONE',  ( 18.09877017944540611, 2.191112624880879434, -12.51823083080036270 ) ) ;
#38503 = PLANE ( 'NONE',  #19835 ) ;
#38504 = AXIS2_PLACEMENT_3D ( 'NONE', #8866, #67237, #19704 ) ;
#38505 = CARTESIAN_POINT ( 'NONE',  ( 10.45672469555900008, 4.433465011431599656, 8.249937779480299938 ) ) ;
#38506 = DIRECTION ( 'NONE',  ( 0.000000000000000000, -1.000000000000000000, 0.000000000000000000 ) ) ;
#38507 = CARTESIAN_POINT ( 'NONE',  ( 10.31966935320999923, -4.764591648058999596, -5.997654637741999473 ) ) ;
#38508 = CARTESIAN_POINT ( 'NONE',  ( 7.000000000000000000, 0.5292307692307999245, -2.083846153846000249 ) ) ;
#38509 = CARTESIAN_POINT ( 'NONE',  ( 9.309135711596999485, -5.864995026133001055, -7.324074232821000230 ) ) ;
#38510 = CARTESIAN_POINT ( 'NONE',  ( 0.4687253537224814193, 1.074401066710667818, -3.341895325573862596 ) ) ;
#38511 = EDGE_CURVE ( 'NONE', #33492, #47043, #51064, .T. ) ;
#38512 = CARTESIAN_POINT ( 'NONE',  ( 11.06049777433069892, -4.851452298509800087, -7.174999999999999822 ) ) ;
#38514 = EDGE_CURVE ( 'NONE', #19484, #53681, #59605, .T. ) ;
#38513 = B_SPLINE_CURVE_WITH_KNOTS ( 'NONE', 3,
 ( #35919, #61800, #46414, #34899, #67038, #4433, #30010, #25081, #56558, #8664, #3408, #19149, #62478, #19499, #25425, #52339, #4089, #62817 ),
 .UNSPECIFIED., .F., .F.,
 ( 4, 2, 2, 2, 2, 2, 2, 2, 4 ),
 ( 0.000000000000000000, 0.1250000000000000000, 0.2500000000000000000, 0.3750000000000000000, 0.5000000000000000000, 0.6250000000000000000, 0.7500000000000000000, 0.8750000000000000000, 1.000000000000000000 ),
 .UNSPECIFIED. ) ;
#38515 = ORIENTED_EDGE ( 'NONE', *, *, #10088, .F. ) ;
#38516 = CARTESIAN_POINT ( 'NONE',  ( 9.044210841233001119, 2.773858540272000184, -8.951250717848999727 ) ) ;
#38517 = ORIENTED_EDGE ( 'NONE', *, *, #1914, .F. ) ;
#38518 = CARTESIAN_POINT ( 'NONE',  ( 18.14041819333149519, -2.719953065120092273, 13.62436182279261843 ) ) ;
#38519 = CARTESIAN_POINT ( 'NONE',  ( 10.49349279008999858, -4.332388355267299929, -8.734031750754999379 ) ) ;
#38520 = VERTEX_POINT ( 'NONE', #2817 ) ;
#38521 = CARTESIAN_POINT ( 'NONE',  ( 11.36056039236529891, 4.891071240644300211, 7.456633480985620288 ) ) ;
#38522 = CARTESIAN_POINT ( 'NONE',  ( 5.453635137985188841, -0.01427739589657720659, -1.132912223412962271 ) ) ;
#38523 = CARTESIAN_POINT ( 'NONE',  ( 23.65869700875494885, 3.166258104914992266, -13.42481195133845162 ) ) ;
#38524 = B_SPLINE_CURVE_WITH_KNOTS ( 'NONE', 3,
 ( #8888, #36142, #68284, #20404, #46297 ),
 .UNSPECIFIED., .F., .F.,
 ( 4, 1, 4 ),
 ( 0.000000000000000000, 0.5000000000000000000, 1.000000000000000000 ),
 .UNSPECIFIED. ) ;
#38525 = CARTESIAN_POINT ( 'NONE',  ( 17.79222771582700346, -3.377813322129000095, 11.11021622646999951 ) ) ;
#38526 = CARTESIAN_POINT ( 'NONE',  ( 12.35624619792629986, -1.936672541246387436, -13.86556857871296344 ) ) ;
#38527 = CARTESIAN_POINT ( 'NONE',  ( 9.643930206848999376, -2.750000000000000000, -7.500000000000000000 ) ) ;
#38528 = CARTESIAN_POINT ( 'NONE',  ( 17.84362596415753544, 0.6599616342123957313, -12.58270523616455527 ) ) ;
#38529 = CARTESIAN_POINT ( 'NONE',  ( 10.51140025105000042, -2.326718149302000160, -7.741209600718000239 ) ) ;
#38530 = CARTESIAN_POINT ( 'NONE',  ( 11.51518179236248862, -4.180996681294200101, -6.652923384986699773 ) ) ;
#38531 = ORIENTED_EDGE ( 'NONE', *, *, #33626, .T. ) ;
#38532 = CARTESIAN_POINT ( 'NONE',  ( 9.020585841232000135, 4.920236664407999783, -6.448229650796999834 ) ) ;
#38533 = ORIENTED_EDGE ( 'NONE', *, *, #16520, .T. ) ;
#38534 = CARTESIAN_POINT ( 'NONE',  ( 9.856851002545999663, 2.832432432432000269, -6.822293592207000934 ) ) ;
#38535 = VERTEX_POINT ( 'NONE', #19239 ) ;
#38536 = CARTESIAN_POINT ( 'NONE',  ( 10.93769906941999892, 2.936877991120999898, -4.920829195977000303 ) ) ;
#38537 = CARTESIAN_POINT ( 'NONE',  ( 1.700000379347999857, 1.775000379263000028, -7.150855879635999901E-10 ) ) ;
#38538 = EDGE_CURVE ( 'NONE', #67391, #7601, #24148, .T. ) ;
#38539 = CARTESIAN_POINT ( 'NONE',  ( 10.33103907547007694, 4.774162136902415199, 7.100484084056944312 ) ) ;
#38540 = CARTESIAN_POINT ( 'NONE',  ( 9.341834235717472623, 3.000408294236256435, 8.268200207948643410 ) ) ;
#38541 = DIRECTION ( 'NONE',  ( 0.000000000000000000, 0.000000000000000000, 1.000000000000000000 ) ) ;
#38542 = B_SPLINE_CURVE_WITH_KNOTS ( 'NONE', 3,
 ( #23685, #65292, #60061, #33497 ),
 .UNSPECIFIED., .F., .F.,
 ( 4, 4 ),
 ( 0.000000000000000000, 1.000000000000000000 ),
 .UNSPECIFIED. ) ;
#38543 = CARTESIAN_POINT ( 'NONE',  ( 10.18239901426000138, -2.607725299334000102, 7.783410967795999724 ) ) ;
#38544 = CARTESIAN_POINT ( 'NONE',  ( 11.80000000000000071, 14.76315775485999993, -50.50083396221000243 ) ) ;
#38545 = CARTESIAN_POINT ( 'NONE',  ( 12.47427908008582342, 0.5306878043354071872, 13.88636785578044375 ) ) ;
#38546 = VERTEX_POINT ( 'NONE', #3166 ) ;
#38547 = CARTESIAN_POINT ( 'NONE',  ( 10.97867121346000019, 2.873849435084999904, 4.940815226079000588 ) ) ;
#38548 = CARTESIAN_POINT ( 'NONE',  ( 10.83325146359777591, 5.014643093291043741, -4.869878762730592392 ) ) ;
#38549 = CARTESIAN_POINT ( 'NONE',  ( 10.13874943042162613, 3.152062997842154157, 7.284280020558234980 ) ) ;
#38550 = CARTESIAN_POINT ( 'NONE',  ( 5.250092101183000182, -0.5193948854954000272, 0.9696677542920000281 ) ) ;
#38551 = CARTESIAN_POINT ( 'NONE',  ( 9.924495280410999598, 4.946705552514000459, -6.253848946732999181 ) ) ;
#38552 = TOROIDAL_SURFACE ( 'NONE', #44115, 12.35000000006999876, 0.5000000000000000000 ) ;
#38553 = CARTESIAN_POINT ( 'NONE',  ( 5.500000000000000000, -1.199999999999999956, 9.776630298829998011 ) ) ;
#38554 = CARTESIAN_POINT ( 'NONE',  ( 11.19120431613999855, -3.005395205805000192, -6.023553580263000029 ) ) ;
#38555 = ORIENTED_EDGE ( 'NONE', *, *, #59294, .F. ) ;
#38556 = CARTESIAN_POINT ( 'NONE',  ( 8.731616107288068918, 4.000002263255227675, -8.381579007094499545 ) ) ;
#38557 = CARTESIAN_POINT ( 'NONE',  ( 9.600000000000001421, -12.34999999999999964, -4.046978686977000011E-05 ) ) ;
#38558 = FACE_OUTER_BOUND ( 'NONE', #46484, .T. ) ;
#38559 = LINE ( 'NONE', #27384, #41359 ) ;
#38560 = CARTESIAN_POINT ( 'NONE',  ( 9.099999999999999645, 0.000000000000000000, 0.000000000000000000 ) ) ;
#38561 = CARTESIAN_POINT ( 'NONE',  ( 11.43856039236529831, 5.032284719763000069, -7.550239075043479353 ) ) ;
#38562 = CARTESIAN_POINT ( 'NONE',  ( 9.508013376692998619, 3.104586782631499897, -7.044942343771899651 ) ) ;
#38564 = CARTESIAN_POINT ( 'NONE',  ( 0.000000000000000000, 0.000000000000000000, 0.000000000000000000 ) ) ;
#38563 = CARTESIAN_POINT ( 'NONE',  ( 10.05168422951000018, -4.611171355610000688, 8.114961396014498618 ) ) ;
#38565 = FACE_OUTER_BOUND ( 'NONE', #69076, .T. ) ;
#38566 = EDGE_LOOP ( 'NONE', ( #60886, #53289, #59525, #51537 ) ) ;
#38567 = CARTESIAN_POINT ( 'NONE',  ( 10.64902344389989963, 3.116469856398800253, 8.036199780531900316 ) ) ;
#38568 = CARTESIAN_POINT ( 'NONE',  ( 10.77462219945999955, -5.575466189878000911, 8.682669263022999573 ) ) ;
#38569 = EDGE_CURVE ( 'NONE', #23593, #40087, #43763, .T. ) ;
#38570 = EDGE_CURVE ( 'NONE', #42800, #79, #55278, .T. ) ;
#38571 = CARTESIAN_POINT ( 'NONE',  ( 9.606367640780998585, 4.538247246588100303, 8.506987760366000018 ) ) ;
#38572 = CARTESIAN_POINT ( 'NONE',  ( 9.682824781140627834, 3.392296711160748490, -8.129467220476902511 ) ) ;
#38573 = CARTESIAN_POINT ( 'NONE',  ( 9.509907746701999898, -5.077451867123000007, 8.469011304701000498 ) ) ;
#38574 = CARTESIAN_POINT ( 'NONE',  ( 5.000000004731000480, 0.05000000473133000417, 3.150000012852999909 ) ) ;
#38575 = CARTESIAN_POINT ( 'NONE',  ( 11.84748603848200155, 3.299681227315999887, -11.83395064283000053 ) ) ;
#38576 = CONICAL_SURFACE ( 'NONE', #9370, 0.8999999994071996579, 0.7853981633972997312 ) ;
#38577 = AXIS2_PLACEMENT_3D ( 'NONE', #68352, #53578, #53915 ) ;
#38578 = CARTESIAN_POINT ( 'NONE',  ( 9.685317406968998455, -3.813190776280700245, -8.486886322867700727 ) ) ;
#38579 = LINE ( 'NONE', #59904, #7537 ) ;
#38580 = CARTESIAN_POINT ( 'NONE',  ( 5.706658963913000093, 0.06352927768877000836, 1.174369886990999978 ) ) ;
#38581 = B_SPLINE_SURFACE_WITH_KNOTS ( 'NONE', 3, 3, ( 
 ( #52464, #4564, #9462, #8451, #3534, #8791, #51437, #29796, #46197, #67508, #19627, #40948, #57026, #9126, #25208, #53156, #27626, #48602, #707, #58739, #21671, #14, #63973, #26597, #43009, #6279, #37082, #36742, #356, #5593, #37761, #53840, #10500, #59427, #41980 ),
 ( #15415, #20654, #59086, #10846, #21337, #10165, #42666, #32188, #54182, #31840, #32525, #37418, #68883, #52815, #64665, #5937, #48949, #27280, #53503, #16432, #31495, #16090, #26937, #58397, #4908, #43365, #26250, #16769, #38101, #5258, #47577, #21001, #48250, #64313, #22018 ),
 ( #63287, #47918, #42335, #63637, #58062, #32868, #15755, #11188, #11524, #7677, #1739, #61164, #55921, #33215, #23057, #2095, #34608, #12237, #8025, #54537, #55226, #39842, #29362, #1056, #6983, #13283, #22368, #11876, #44750, #29022, #50330, #23415, #12929, #33560, #27973 ),
 ( #22710, #60816, #66053, #54881, #65359, #43707, #23756, #28310, #65002, #2429, #45090, #39148, #18172, #49633, #44408, #65708, #39494, #17118, #17478, #38451, #49983, #7326, #34255, #55578, #59774, #38804, #66397, #18520, #6635, #60472, #49284, #1394, #44055, #28668, #60128 ) ),
 .UNSPECIFIED., .F., .F., .F.,
 ( 4, 4 ),
 ( 4, 1, 1, 1, 1, 1, 1, 1, 1, 1, 1, 1, 1, 1, 1, 1, 1, 1, 1, 1, 1, 1, 1, 1, 1, 1, 1, 1, 1, 1, 1, 1, 4 ),
 ( -0.1039370721279000015, 1.103937072127999963 ),
 ( -0.02000000000000000042, 0.01250000000000000069, 0.04499999999999999833, 0.07749999999999999944, 0.1100000000000000006, 0.1424999999999999878, 0.1749999999999999889, 0.2074999999999999900, 0.2399999999999999911, 0.2725000000000000200, 0.3049999999999999933, 0.3375000000000000222, 0.3699999999999999956, 0.4025000000000000244, 0.4349999999999999978, 0.4675000000000000266, 0.5000000000000000000, 0.5324999999999999734, 0.5649999999999999467, 0.5975000000000000311, 0.6300000000000000044, 0.6624999999999999778, 0.6949999999999999512, 0.7275000000000000355, 0.7600000000000000089, 0.7924999999999999822, 0.8249999999999999556, 0.8575000000000000400, 0.8900000000000000133, 0.9224999999999999867, 0.9549999999999999600, 0.9875000000000000444, 1.020000000000000018 ),
 .UNSPECIFIED. ) ;
#38582 = CARTESIAN_POINT ( 'NONE',  ( 10.47363156114899851, -4.684311564990208510, 6.424401362931538628 ) ) ;
#38583 = CARTESIAN_POINT ( 'NONE',  ( 24.40628504395400000, -3.359328441570999857, 12.19433831731000062 ) ) ;
#38584 = CARTESIAN_POINT ( 'NONE',  ( 9.472537864290000442, 2.899999999999999911, -6.571291218949999902 ) ) ;
#38585 = CARTESIAN_POINT ( 'NONE',  ( 11.39210538575740017, 4.842454415653899780, -7.298582155985900322 ) ) ;
#38586 = CARTESIAN_POINT ( 'NONE',  ( 12.26191093050522340, 2.190091418697194481, -13.73433605229142884 ) ) ;
#38587 = CARTESIAN_POINT ( 'NONE',  ( 2.059804692936264114, 2.284309548437588600, -2.477449380090549269 ) ) ;
#38588 = CARTESIAN_POINT ( 'NONE',  ( 13.99999999231800096, -8.833253877201999060, -7.896562762484000686 ) ) ;
#38589 = ORIENTED_EDGE ( 'NONE', *, *, #52748, .T. ) ;
#38590 = CARTESIAN_POINT ( 'NONE',  ( 11.43320764420671054, -12.36501421780136667, -1.521867707432055905 ) ) ;
#38591 = CARTESIAN_POINT ( 'NONE',  ( 12.72332061973729012, 0.6199690124688018722, -13.88138352397877462 ) ) ;
#38592 = CARTESIAN_POINT ( 'NONE',  ( 7.725062132959652494, -2.650631715052233162, 7.500008390440855877 ) ) ;
#38593 = EDGE_CURVE ( 'NONE', #55299, #26398, #26301, .T. ) ;
#38594 = CARTESIAN_POINT ( 'NONE',  ( 9.940795537695231943, -5.100000000000000533, 6.662590550615205665 ) ) ;
#38595 = CARTESIAN_POINT ( 'NONE',  ( 3.500000000000000000, -1.789730407083999886, 2.652709005895000249 ) ) ;
#38596 = CARTESIAN_POINT ( 'NONE',  ( 21.65000086032551252, 3.970157536060000036E-13, 1.776356839399999796E-13 ) ) ;
#38597 = CARTESIAN_POINT ( 'NONE',  ( 13.46122879894100066, 12.02747180725999954, 2.509215126660999662 ) ) ;
#38598 = ORIENTED_EDGE ( 'NONE', *, *, #60534, .T. ) ;
#38599 = VECTOR ( 'NONE', #47008, 1000.000000000000000 ) ;
#38600 = EDGE_CURVE ( 'NONE', #42097, #7255, #13667, .T. ) ;
#38601 = DIRECTION ( 'NONE',  ( 0.000000000000000000, -0.9478160162686030121, -0.3188178152248009600 ) ) ;
#38602 = CARTESIAN_POINT ( 'NONE',  ( 17.69802269633222735, 1.891226317878778485, -13.78388397175237223 ) ) ;
#38603 = ORIENTED_EDGE ( 'NONE', *, *, #10957, .T. ) ;
#38604 = DIRECTION ( 'NONE',  ( 0.000000000000000000, 1.000000000000000000, 0.000000000000000000 ) ) ;
#38605 = DIRECTION ( 'NONE',  ( 0.7071067617951957152, 0.000000000000000000, -0.7071068005778986532 ) ) ;
#38606 = VECTOR ( 'NONE', #44049, 1000.000000000000000 ) ;
#38607 = CARTESIAN_POINT ( 'NONE',  ( 8.275189158773001097, 3.061731693614000438, -8.535706278603999664 ) ) ;
#38608 = LINE ( 'NONE', #514, #33108 ) ;
#38609 = LINE ( 'NONE', #17985, #26670 ) ;
#38610 = B_SPLINE_CURVE_WITH_KNOTS ( 'NONE', 3,
 ( #38091, #59418, #21329, #53494 ),
 .UNSPECIFIED., .F., .F.,
 ( 4, 4 ),
 ( 0.000000000000000000, 1.000000000000000000 ),
 .UNSPECIFIED. ) ;
#38611 = CARTESIAN_POINT ( 'NONE',  ( 7.066685841226999720, 2.417988323708999854, -8.552044326954000297 ) ) ;
#38612 = CARTESIAN_POINT ( 'NONE',  ( 9.933536308083233735, -2.899999999999999911, -6.665341197415429519 ) ) ;
#38613 = CARTESIAN_POINT ( 'NONE',  ( 10.25851354018233152, -3.836375382625526687, 8.749999999999996447 ) ) ;
#38614 = ORIENTED_EDGE ( 'NONE', *, *, #29372, .T. ) ;
#38615 = CARTESIAN_POINT ( 'NONE',  ( 10.37874387220000116, -4.882732524430000609, 6.350796477317000921 ) ) ;
#38616 = CARTESIAN_POINT ( 'NONE',  ( 18.07078568654538842, -2.853178104785935698, -13.59212922195714413 ) ) ;
#38617 = DIRECTION ( 'NONE',  ( 0.000000000000000000, 0.9905022095861402143, -0.1374968101629056305 ) ) ;
#38618 = ORIENTED_EDGE ( 'NONE', *, *, #28897, .T. ) ;
#38619 = DIRECTION ( 'NONE',  ( 0.000000000000000000, -0.9565994702956990281, 0.2914059941558995726 ) ) ;
#38620 = CARTESIAN_POINT ( 'NONE',  ( 11.22022944037999892, -3.883088694641999794, -8.854817792072001481 ) ) ;
#38621 = ORIENTED_EDGE ( 'NONE', *, *, #52495, .T. ) ;
#38622 = CARTESIAN_POINT ( 'NONE',  ( 8.773468108405998223, 4.966402032527499344, 7.226304214866999587 ) ) ;
#38623 = CARTESIAN_POINT ( 'NONE',  ( 17.98022888730381652, -3.063516777430836502, -12.22190850126833794 ) ) ;
#38624 = CARTESIAN_POINT ( 'NONE',  ( 4.613813072189000053, 0.1210501919378999952, -1.411301419693000048 ) ) ;
#38625 = EDGE_CURVE ( 'NONE', #57125, #46362, #19525, .T. ) ;
#38626 = CARTESIAN_POINT ( 'NONE',  ( 8.025716582962996171, 5.094285164475001793, -6.419293649061996732 ) ) ;
#38627 = DIRECTION ( 'NONE',  ( -1.000000000000000000, 0.000000000000000000, 0.000000000000000000 ) ) ;
#38628 = CARTESIAN_POINT ( 'NONE',  ( 23.56666365135700403, 2.009474831917003268, 11.63289034803000455 ) ) ;
#38629 = CARTESIAN_POINT ( 'NONE',  ( 10.24255864497999902, 4.790758628877400227, 6.880692865553299953 ) ) ;
#38630 = CARTESIAN_POINT ( 'NONE',  ( 12.80505043854144276, 0.6951438842159390896, 13.94765567169528531 ) ) ;
#38631 = ORIENTED_EDGE ( 'NONE', *, *, #13413, .T. ) ;
#38632 = CARTESIAN_POINT ( 'NONE',  ( 10.90000000000000036, 0.2500000000000000000, -9.776630298829998011 ) ) ;
#38633 = CARTESIAN_POINT ( 'NONE',  ( 10.33453278041000090, 3.295703187163999459, -6.149878749787999865 ) ) ;
#38634 = DIRECTION ( 'NONE',  ( -1.000000000000000000, 0.000000000000000000, -1.275169027325000072E-14 ) ) ;
#38635 = CARTESIAN_POINT ( 'NONE',  ( 12.56965099582936674, 1.826966356815474368, -13.88028256676998495 ) ) ;
#38636 = CARTESIAN_POINT ( 'NONE',  ( 10.06430484851600049, -2.836617618740000069, -8.031907719862799055 ) ) ;
#38637 = CARTESIAN_POINT ( 'NONE',  ( 9.285188841453999586, -5.269672295101000437, 8.747824102203999530 ) ) ;
#38638 = CARTESIAN_POINT ( 'NONE',  ( 18.24183043734545251, -0.2342631834278660341, 13.99804438501501380 ) ) ;
#38639 = AXIS2_PLACEMENT_3D ( 'NONE', #46476, #35978, #39949 ) ;
#38640 = CARTESIAN_POINT ( 'NONE',  ( 25.37646586244400382, -2.613422027899000355, 11.31776839467000073 ) ) ;
#38641 = ORIENTED_EDGE ( 'NONE', *, *, #32928, .F. ) ;
#38642 = ORIENTED_EDGE ( 'NONE', *, *, #33583, .F. ) ;
#38643 = CARTESIAN_POINT ( 'NONE',  ( 8.450464158772000189, 3.789127741898000057, -9.388182174781999123 ) ) ;
#38644 = CARTESIAN_POINT ( 'NONE',  ( 12.60522794357327747, -0.5937363471729734110, 13.88293910736614301 ) ) ;
#38645 = CARTESIAN_POINT ( 'NONE',  ( 10.84580110216399973, -5.090698144635000588, 8.166103548914600552 ) ) ;
#38646 = CARTESIAN_POINT ( 'NONE',  ( 7.277749419310966417, -2.920727118723208005, 6.671122885330429853 ) ) ;
#38647 = FACE_OUTER_BOUND ( 'NONE', #59410, .T. ) ;
#38648 = B_SPLINE_CURVE_WITH_KNOTS ( 'NONE', 3,
 ( #66651, #19101, #50234, #65611 ),
 .UNSPECIFIED., .F., .F.,
 ( 4, 4 ),
 ( 0.000000000000000000, 1.000000000000000000 ),
 .UNSPECIFIED. ) ;
#38649 = CARTESIAN_POINT ( 'NONE',  ( 8.475644353210000759, -5.095088356574999366, 6.286978111459999852 ) ) ;
#38650 = CARTESIAN_POINT ( 'NONE',  ( 25.00270600450344105, 8.478844049630730240, -8.837091021818228143 ) ) ;
#38652 = CARTESIAN_POINT ( 'NONE',  ( 10.96866170142999941, -5.808833653407999620, 4.931298558683999467 ) ) ;
#38651 = CARTESIAN_POINT ( 'NONE',  ( 10.99490035061499960, -3.659038130401700339, 6.267064942904999825 ) ) ;
#38653 = DIRECTION ( 'NONE',  ( 1.000000000000000000, 0.000000000000000000, 0.000000000000000000 ) ) ;
#38654 = AXIS2_PLACEMENT_3D ( 'NONE', #66867, #25249, #40990 ) ;
#38655 = CARTESIAN_POINT ( 'NONE',  ( 24.25374608244500152, -8.963954835242001096, -8.909854536156000648 ) ) ;
#38656 = B_SPLINE_CURVE_WITH_KNOTS ( 'NONE', 3,
 ( #15757, #49988, #44752, #22021, #11880, #64668, #49636, #17482, #55229, #7329, #65362, #23417, #38806, #11529, #65710, #60130 ),
 .UNSPECIFIED., .F., .F.,
 ( 4, 2, 2, 2, 2, 2, 2, 4 ),
 ( 0.000000000000000000, 0.06249999999999912570, 0.1249999999999982514, 0.2499999999999985012, 0.3749999999999987232, 0.4999999999999990008, 0.7499999999999994449, 1.000000000000000000 ),
 .UNSPECIFIED. ) ;
#38657 = CARTESIAN_POINT ( 'NONE',  ( 8.766480666858997850, 4.289077172771600388, -8.317400147935998689 ) ) ;
#38658 = ADVANCED_FACE ( 'NONE', ( #40914 ), #13382, .F. ) ;
#38659 = ADVANCED_FACE ( 'NONE', ( #9094 ), #2758, .T. ) ;
#38660 = CARTESIAN_POINT ( 'NONE',  ( 18.13628167719501505, -0.2299973361971393848, 12.69720198919503495 ) ) ;
#38661 = DIRECTION ( 'NONE',  ( 0.000000000000000000, 1.000000000000000000, 0.000000000000000000 ) ) ;
#38662 = CARTESIAN_POINT ( 'NONE',  ( 18.16744427651242688, -2.624922643435798619, -12.42158156183114848 ) ) ;
#38663 = ORIENTED_EDGE ( 'NONE', *, *, #40024, .F. ) ;
#38665 = CARTESIAN_POINT ( 'NONE',  ( 3.458495577646333974, 3.039910566627586963, -1.793659031961971628 ) ) ;
#38664 = CARTESIAN_POINT ( 'NONE',  ( 9.294724726289000927, -4.148132978932999926, 9.337467253566000380 ) ) ;
#38666 = CARTESIAN_POINT ( 'NONE',  ( 8.323770280408998801, 5.332332124071999857, -8.487089944253000340 ) ) ;
#38667 = EDGE_CURVE ( 'NONE', #48162, #2906, #19622, .T. ) ;
#38668 = DIRECTION ( 'NONE',  ( -1.000000000000000000, 0.000000000000000000, 0.000000000000000000 ) ) ;
#38669 = CARTESIAN_POINT ( 'NONE',  ( 23.89320776801300283, 8.862674798062995407, -7.304122743114001004 ) ) ;
#38670 = CARTESIAN_POINT ( 'NONE',  ( 0.6584425577435999433, -2.301202007355999779, -2.466905145517999998 ) ) ;
#38671 = CARTESIAN_POINT ( 'NONE',  ( 9.502457028859783605, 2.587963025190172850, 6.404785931707032809 ) ) ;
#38672 = CARTESIAN_POINT ( 'NONE',  ( 2.161381769351999882, 2.835781239812999566, -1.921535772062000103 ) ) ;
#38673 = ORIENTED_EDGE ( 'NONE', *, *, #19311, .F. ) ;
#38674 = B_SPLINE_CURVE_WITH_KNOTS ( 'NONE', 3,
 ( #60160, #37793, #32898, #27657 ),
 .UNSPECIFIED., .F., .F.,
 ( 4, 4 ),
 ( 0.000000000000000000, 1.000000000000000000 ),
 .UNSPECIFIED. ) ;
#38675 = CARTESIAN_POINT ( 'NONE',  ( 12.08965323865563768, -0.1172743548790659562, -12.59945959730644205 ) ) ;
#38676 = CARTESIAN_POINT ( 'NONE',  ( 6.916399741278000057, 12.19468928278000064, -3.104275424020000340 ) ) ;
#38677 = CARTESIAN_POINT ( 'NONE',  ( 17.55505043854143565, 3.199751711897557804, -12.18694338143115630 ) ) ;
#38678 = CARTESIAN_POINT ( 'NONE',  ( 8.424688440789097399, -5.350083765069893360, 7.500019236172019710 ) ) ;
#38679 = CARTESIAN_POINT ( 'NONE',  ( 8.116920280410999666, 5.773189794777000117, 7.141495931231999883 ) ) ;
#38680 = ORIENTED_EDGE ( 'NONE', *, *, #60534, .F. ) ;
#38681 = CARTESIAN_POINT ( 'NONE',  ( 6.961818577609000691, -1.329569516000000062, 0.3446834961110000206 ) ) ;
#38682 = CARTESIAN_POINT ( 'NONE',  ( 7.350270280410000190, 3.562914451704999763, -5.997303864335000512 ) ) ;
#38684 = CARTESIAN_POINT ( 'NONE',  ( 10.35616100078999935, 2.777276096020000029, 8.995275123087999702 ) ) ;
#38683 = CARTESIAN_POINT ( 'NONE',  ( 8.558667133076065525, -3.651697308196094838, 5.795658283814029588 ) ) ;
#38685 = CARTESIAN_POINT ( 'NONE',  ( 11.55300581613033906, 5.107584469683000172, -8.211208432468300344 ) ) ;
#38686 = VERTEX_POINT ( 'NONE', #52083 ) ;
#38687 = CARTESIAN_POINT ( 'NONE',  ( 10.02314899745999988, -5.167567567567999731, -6.822293592207000934 ) ) ;
#38688 = AXIS2_PLACEMENT_3D ( 'NONE', #6176, #44653, #22608 ) ;
#38689 = DIRECTION ( 'NONE',  ( -1.000000000000000000, 0.000000000000000000, 0.000000000000000000 ) ) ;
#38690 = ORIENTED_EDGE ( 'NONE', *, *, #63620, .F. ) ;
#38691 = CARTESIAN_POINT ( 'NONE',  ( 12.07922409836661792, 2.296075727005074008, -12.39049400502616827 ) ) ;
#38692 = DIRECTION ( 'NONE',  ( 0.000000000000000000, -0.2461538461537955136, 0.9692307692307821076 ) ) ;
#38693 = CONICAL_SURFACE ( 'NONE', #14094, 2.325000277643999969, 0.7853982725543797727 ) ;
#38694 = CARTESIAN_POINT ( 'NONE',  ( 18.12459203954894704, -0.2581888431706746978, -13.89679013629344517 ) ) ;
#38695 = EDGE_LOOP ( 'NONE', ( #11346, #30135, #62065, #38853 ) ) ;
#38696 = CARTESIAN_POINT ( 'NONE',  ( 10.38344113585631412, -5.519338294115820887, -8.419368937664973629 ) ) ;
#38697 = FACE_OUTER_BOUND ( 'NONE', #26069, .T. ) ;
#38698 = CARTESIAN_POINT ( 'NONE',  ( 11.06967835872019812, 3.245266201729799960, -7.024326263066900111 ) ) ;
#38699 = DIRECTION ( 'NONE',  ( 0.7071067486699967874, -0.7071068137030968037, 9.022793105466955192E-11 ) ) ;
#38700 = CARTESIAN_POINT ( 'NONE',  ( 18.23777283046791098, -3.105167776281877234, 11.92942829619372702 ) ) ;
#38701 = VERTEX_POINT ( 'NONE', #57327 ) ;
#38702 = CARTESIAN_POINT ( 'NONE',  ( 8.064114158772998309, 4.228291488957999888, 8.941375734143997889 ) ) ;
#38703 = CARTESIAN_POINT ( 'NONE',  ( 23.51521505635600207, -13.45855365459000019, -4.318323883769999760 ) ) ;
#38704 = APPLICATION_CONTEXT ( 'automotive_design' ) ;
#38705 = DIRECTION ( 'NONE',  ( 1.000000000000000000, 0.000000000000000000, 0.000000000000000000 ) ) ;
#38706 = AXIS2_PLACEMENT_3D ( 'NONE', #32133, #53446, #48198 ) ;
#38707 = B_SPLINE_CURVE_WITH_KNOTS ( 'NONE', 3,
 ( #47461, #46430, #25441, #67733 ),
 .UNSPECIFIED., .F., .F.,
 ( 4, 4 ),
 ( 0.000000000000000000, 1.000000000000000000 ),
 .UNSPECIFIED. ) ;
#38708 = CARTESIAN_POINT ( 'NONE',  ( 15.83590051321700010, -9.131200976137998637, -8.359844154751998602 ) ) ;
#38709 = ORIENTED_EDGE ( 'NONE', *, *, #8989, .T. ) ;
#38710 = CARTESIAN_POINT ( 'NONE',  ( 12.73227166903755680, -1.879164230820285830, -12.57473389636349204 ) ) ;
#38711 = EDGE_CURVE ( 'NONE', #16924, #37496, #10129, .T. ) ;
#38712 = CARTESIAN_POINT ( 'NONE',  ( 0.4529763571839853786, 3.676114825633475335E-06, -3.452897576335808072 ) ) ;
#38713 = DIRECTION ( 'NONE',  ( 0.000000000000000000, 0.000000000000000000, -1.000000000000000000 ) ) ;
#38714 = CARTESIAN_POINT ( 'NONE',  ( 13.00000000005200107, -12.15994572112000149, -2.000334444851999738 ) ) ;
#38715 = CARTESIAN_POINT ( 'NONE',  ( 11.50001544675000176, -12.52500000000000036, 0.000000000000000000 ) ) ;
#38716 = CARTESIAN_POINT ( 'NONE',  ( 10.77256919669529900, -3.037654633983899899, -7.784327714719899483 ) ) ;
#38717 = CARTESIAN_POINT ( 'NONE',  ( 12.78440343889028874, -0.6249994633519880827, -13.88107975068472300 ) ) ;
#38718 = CARTESIAN_POINT ( 'NONE',  ( 18.01290626049240728, -2.925915981747412076, 12.34209597222820420 ) ) ;
#38719 = ORIENTED_EDGE ( 'NONE', *, *, #62642, .T. ) ;
#38720 = CARTESIAN_POINT ( 'NONE',  ( 10.97124174884019965, -4.036194082918090231, -8.815770025351000072 ) ) ;
#38721 = VERTEX_POINT ( 'NONE', #31128 ) ;
#38722 = CARTESIAN_POINT ( 'NONE',  ( 11.72764643456600098, -12.22218869479000070, -1.954421350659000023 ) ) ;
#38723 = CARTESIAN_POINT ( 'NONE',  ( 9.336654719594999818, 5.095038542659000136, -6.157541456184000062 ) ) ;
#38724 = CARTESIAN_POINT ( 'NONE',  ( 3.502409213219000339, -3.069775387992999871, 0.006882399294532000333 ) ) ;
#38725 = CARTESIAN_POINT ( 'NONE',  ( 10.53865751177000121, -3.647233463439000012, -6.014125921456000334 ) ) ;
#38726 = CARTESIAN_POINT ( 'NONE',  ( 11.59999999999999964, 3.116215992411100366, -7.825000000000000178 ) ) ;
#38727 = CARTESIAN_POINT ( 'NONE',  ( 9.573148997458000409, 5.167567567567999731, -6.822293592207000934 ) ) ;
#38728 = DIRECTION ( 'NONE',  ( -1.000000000000000000, 0.000000000000000000, 0.000000000000000000 ) ) ;
#38729 = ORIENTED_EDGE ( 'NONE', *, *, #7911, .F. ) ;
#38730 = CARTESIAN_POINT ( 'NONE',  ( 1.885432296257667062, -1.713969392196469155, -3.070236115647939634 ) ) ;
#38731 = CARTESIAN_POINT ( 'NONE',  ( 10.89874804681000064, 2.834828962328999502, 9.088465460431999432 ) ) ;
#38732 = CARTESIAN_POINT ( 'NONE',  ( 2.228056799209332972, -2.150913519912213800, 2.798833948393621540 ) ) ;
#38733 = LINE ( 'NONE', #12510, #8648 ) ;
#38734 = CARTESIAN_POINT ( 'NONE',  ( 18.23176382712000176, 2.916721637292999603, -11.52766586543999949 ) ) ;
#38735 = CARTESIAN_POINT ( 'NONE',  ( 11.53564291764652872, 3.004110626587600308, -7.376893506359599506 ) ) ;
#38736 = CYLINDRICAL_SURFACE ( 'NONE', #49224, 0.4999999999999998335 ) ;
#38737 = CARTESIAN_POINT ( 'NONE',  ( 10.01163399569799850, 5.134843509922999871, -7.625954975973699312 ) ) ;
#38738 = EDGE_CURVE ( 'NONE', #35994, #55227, #10315, .T. ) ;
#38739 = CARTESIAN_POINT ( 'NONE',  ( 24.33740314120300141, -8.940160201810000373, -9.046312361204000396 ) ) ;
#38740 = ADVANCED_FACE ( 'NONE', ( #69192 ), #42931, .T. ) ;
#38741 = CARTESIAN_POINT ( 'NONE',  ( 24.02032928698500314, -9.295255963207001315, 9.130110662804000299 ) ) ;
#38742 = DIRECTION ( 'NONE',  ( 1.000000000000000000, 0.000000000000000000, 0.000000000000000000 ) ) ;
#38743 = ORIENTED_EDGE ( 'NONE', *, *, #28667, .T. ) ;
#38744 = CARTESIAN_POINT ( 'NONE',  ( 7.988543146792999927, -3.566638198986999964, 5.743608852252999775 ) ) ;
#38745 = CARTESIAN_POINT ( 'NONE',  ( 10.06233042975999936, -5.062748727288000516, -8.618689820632001286 ) ) ;
#38746 = ADVANCED_FACE ( 'NONE', ( #36709 ), #50779, .F. ) ;
#38747 = EDGE_CURVE ( 'NONE', #33649, #40201, #3621, .T. ) ;
#38748 = CARTESIAN_POINT ( 'NONE',  ( 17.98492955360209322, 2.046199355803458353, 13.75924933913552728 ) ) ;
#38749 = CARTESIAN_POINT ( 'NONE',  ( 23.56666365135700403, -2.488348886664998538, 11.45224114467999499 ) ) ;
#38750 = CARTESIAN_POINT ( 'NONE',  ( 10.59195391537400077, -2.942766577210000012, -8.218034727798299244 ) ) ;
#38751 = VERTEX_POINT ( 'NONE', #45051 ) ;
#38752 = TOROIDAL_SURFACE ( 'NONE', #30976, 10.75000000000000000, 1.500000000000000000 ) ;
#38753 = CARTESIAN_POINT ( 'NONE',  ( 25.36465219829700146, 2.635499547415999899, -11.32507936926000092 ) ) ;
#38754 = CARTESIAN_POINT ( 'NONE',  ( 7.769579719591000355, 2.431401017850999935, 7.958393275880999873 ) ) ;
#38756 = CARTESIAN_POINT ( 'NONE',  ( 9.832537864288001472, -2.899999999999999911, 6.571291218949999902 ) ) ;
#38755 = CARTESIAN_POINT ( 'NONE',  ( 9.541460841232000334, 2.824732249080000202, -8.992748220058999209 ) ) ;
#38757 = CARTESIAN_POINT ( 'NONE',  ( 3.232623315315109824, 2.781099406263673579, -1.696921006577742030 ) ) ;
#38758 = ORIENTED_EDGE ( 'NONE', *, *, #39534, .F. ) ;
#38759 = CARTESIAN_POINT ( 'NONE',  ( 10.16829701902000060, 4.567214950372999738, 5.832525041908999341 ) ) ;
#38760 = VECTOR ( 'NONE', #6533, 1000.000000000000000 ) ;
#38761 = CARTESIAN_POINT ( 'NONE',  ( 18.08737871041812539, -2.022152854634004182, -13.85319383421289530 ) ) ;
#38762 = CARTESIAN_POINT ( 'NONE',  ( 11.11718313518939816, 3.377550038693600154, 6.712912394634500401 ) ) ;
#38763 = CARTESIAN_POINT ( 'NONE',  ( 10.51654446536000087, -4.930670681812999945, 8.573593359022000371 ) ) ;
#38764 = CARTESIAN_POINT ( 'NONE',  ( 7.411012926802005296, 3.233242541571998085, 6.481873309613996881 ) ) ;
#38765 = ORIENTED_EDGE ( 'NONE', *, *, #54865, .T. ) ;
#38766 = CARTESIAN_POINT ( 'NONE',  ( 8.960616452296999768, -2.899999999999999911, 6.279946362737000243 ) ) ;
#38767 = EDGE_CURVE ( 'NONE', #11746, #57153, #67021, .T. ) ;
#38769 = CARTESIAN_POINT ( 'NONE',  ( 10.90246814679000131, -4.554787328265999413, -6.081873034041000103 ) ) ;
#38768 = CARTESIAN_POINT ( 'NONE',  ( 12.69408977940800121, -11.93156085714000092, 3.263088413970000268 ) ) ;
#38770 = CARTESIAN_POINT ( 'NONE',  ( 7.806861305538506102, -4.389447504349804241, 9.195466472809515679 ) ) ;
#38771 = CARTESIAN_POINT ( 'NONE',  ( 11.27109998545999936, -5.469594811916000054, 8.504700858852999090 ) ) ;
#38772 = CARTESIAN_POINT ( 'NONE',  ( 10.17500046684972936, -2.650307855384914202, 7.500001770945068813 ) ) ;
#38773 = CARTESIAN_POINT ( 'NONE',  ( 10.23396314288000042, -2.882742046518000034, 7.735518817439499983 ) ) ;
#38774 = VERTEX_POINT ( 'NONE', #46421 ) ;
#38775 = DIRECTION ( 'NONE',  ( 0.000000000000000000, 1.000000000000000000, 0.000000000000000000 ) ) ;
#38776 = CARTESIAN_POINT ( 'NONE',  ( 11.83041235500449950, -4.942357465271699724, 8.363295307663500822 ) ) ;
#38777 = ORIENTED_EDGE ( 'NONE', *, *, #1278, .F. ) ;
#38778 = CARTESIAN_POINT ( 'NONE',  ( 8.205377021103002377, 3.106081841748002059, 6.107037662485001128 ) ) ;
#38779 = ORIENTED_EDGE ( 'NONE', *, *, #1827, .F. ) ;
#38780 = CARTESIAN_POINT ( 'NONE',  ( 9.012204719595001023, 3.161445734422999809, -6.178649910536000434 ) ) ;
#38781 = CARTESIAN_POINT ( 'NONE',  ( 23.58444978062600228, 13.25734564952999861, -4.306384313474000081 ) ) ;
#38782 = CARTESIAN_POINT ( 'NONE',  ( 12.40918755490006831, 3.083210392534602828, -12.21694967330944870 ) ) ;
#38783 = CARTESIAN_POINT ( 'NONE',  ( 12.17403632436368888, -4.976178716761900489, 7.727966254184200245 ) ) ;
#38784 = CARTESIAN_POINT ( 'NONE',  ( 7.946914507420710372, 4.862230276086360270, -6.362913330584241578 ) ) ;
#38785 = AXIS2_PLACEMENT_3D ( 'NONE', #18138, #27591, #64635 ) ;
#38786 = CARTESIAN_POINT ( 'NONE',  ( 11.09999999999999964, -4.000000000000000000, -7.500000000000000000 ) ) ;
#38787 = VERTEX_POINT ( 'NONE', #19506 ) ;
#38788 = CYLINDRICAL_SURFACE ( 'NONE', #26946, 0.4999999999999998335 ) ;
#38789 = CARTESIAN_POINT ( 'NONE',  ( 5.575859839683415586, -1.460959015002473826, -0.3926218265389207485 ) ) ;
#38790 = VERTEX_POINT ( 'NONE', #20877 ) ;
#38791 = CARTESIAN_POINT ( 'NONE',  ( 10.96226112747999970, -2.399999999999999911, -6.571291218949999902 ) ) ;
#38792 = CARTESIAN_POINT ( 'NONE',  ( 10.32949413291699869, 4.912929163218899831, 7.916546720849799712 ) ) ;
#38793 = ADVANCED_FACE ( 'NONE', ( #19849 ), #40823, .F. ) ;
#38794 =( GEOMETRIC_REPRESENTATION_CONTEXT ( 3 ) GLOBAL_UNCERTAINTY_ASSIGNED_CONTEXT ( ( #2218 ) ) GLOBAL_UNIT_ASSIGNED_CONTEXT ( ( #30891, #52548, #68272 ) ) REPRESENTATION_CONTEXT ( 'NONE', 'WORKASPACE' ) );
#38795 = CARTESIAN_POINT ( 'NONE',  ( 24.35365242081700288, 2.582848009804000533, -11.10541636511000085 ) ) ;
#38796 = CARTESIAN_POINT ( 'NONE',  ( 10.13061872827999998, 2.189311095934999951, -7.101639631284999865 ) ) ;
#38797 = CARTESIAN_POINT ( 'NONE',  ( 5.700000000124999744, 0.5292307632381000326, -2.083846155497000030 ) ) ;
#38798 = CARTESIAN_POINT ( 'NONE',  ( 7.100000000000000533, 12.59999999999999964, 0.000000000000000000 ) ) ;
#38799 = CARTESIAN_POINT ( 'NONE',  ( 12.49912319420862872, -3.045104416349984966, -13.54255671968480357 ) ) ;
#38800 = CARTESIAN_POINT ( 'NONE',  ( 18.17481334264689607, -0.08139242733401015617, -12.69965452654168026 ) ) ;
#38801 = EDGE_CURVE ( 'NONE', #48331, #22433, #39593, .T. ) ;
#38802 = FACE_OUTER_BOUND ( 'NONE', #899, .T. ) ;
#38803 = CARTESIAN_POINT ( 'NONE',  ( 10.74379975933729980, -2.921317947059999920, -7.128873141726999485 ) ) ;
#38804 = CARTESIAN_POINT ( 'NONE',  ( 8.802614158774000330, 3.975069902178000270, 9.483774112875002160 ) ) ;
#38805 = VERTEX_POINT ( 'NONE', #41856 ) ;
#38806 = CARTESIAN_POINT ( 'NONE',  ( 11.60000000000000142, -3.674136214561154468, -8.622936771936917211 ) ) ;
#38807 = CARTESIAN_POINT ( 'NONE',  ( 10.61503919148196218, -5.349978903665073560, -7.499997722305344006 ) ) ;
#38808 = CARTESIAN_POINT ( 'NONE',  ( 11.80577368593200305, 12.32791529894999982, 1.878576500660000148 ) ) ;
#38809 = CARTESIAN_POINT ( 'NONE',  ( 18.08778676580599409, 1.991706414748727783, 12.44159931028328359 ) ) ;
#38810 = CARTESIAN_POINT ( 'NONE',  ( 10.81905590578999998, 2.899999999999999911, -6.571291218949999902 ) ) ;
#38811 = CARTESIAN_POINT ( 'NONE',  ( 9.285195242305000818, 5.269680202247999823, 8.747831873285999649 ) ) ;
#38812 = B_SPLINE_CURVE_WITH_KNOTS ( 'NONE', 3,
 ( #39542, #53626, #7374, #17876 ),
 .UNSPECIFIED., .F., .F.,
 ( 4, 4 ),
 ( 0.000000000000000000, 1.000000000000000000 ),
 .UNSPECIFIED. ) ;
#38813 = AXIS2_PLACEMENT_3D ( 'NONE', #62146, #13242, #3071 ) ;
#38814 = CARTESIAN_POINT ( 'NONE',  ( 10.41078710578162791, -3.243350240173176413, 7.939332914627393656 ) ) ;
#38815 = DIRECTION ( 'NONE',  ( 0.000000000000000000, 0.000000000000000000, -1.000000000000000000 ) ) ;
#38816 = ORIENTED_EDGE ( 'NONE', *, *, #31365, .F. ) ;
#38817 = CARTESIAN_POINT ( 'NONE',  ( 12.08949137858164669, -2.599319321963736495, 12.32899351683632005 ) ) ;
#38818 = CARTESIAN_POINT ( 'NONE',  ( 9.606367640780998585, -3.461752753411900141, -6.493012239633999982 ) ) ;
#38819 = CARTESIAN_POINT ( 'NONE',  ( 11.79999999684100054, -12.15995044155999949, -2.000340912084999978 ) ) ;
#38820 = CARTESIAN_POINT ( 'NONE',  ( 8.351726203237999968, -5.100872937112000294, 6.601389982007999535 ) ) ;
#38821 = CARTESIAN_POINT ( 'NONE',  ( 11.33456651104149948, 4.112542507956200133, -6.364824110469998963 ) ) ;
#38822 = ORIENTED_EDGE ( 'NONE', *, *, #41609, .F. ) ;
#38823 = CARTESIAN_POINT ( 'NONE',  ( 12.30048768357420563, -0.5166535389540105605, 12.58940585649086508 ) ) ;
#38824 = CARTESIAN_POINT ( 'NONE',  ( 8.689260841231000398, 2.550241116032999855, 7.666973618349000041 ) ) ;
#38825 = CARTESIAN_POINT ( 'NONE',  ( 9.719613305057999142, 5.967773797872000685, 7.406643507784999692 ) ) ;
#38826 = CARTESIAN_POINT ( 'NONE',  ( 12.39079901834617559, 2.968443430305769848, 12.32999838110539592 ) ) ;
#38827 = ORIENTED_EDGE ( 'NONE', *, *, #37275, .F. ) ;
#38828 = CARTESIAN_POINT ( 'NONE',  ( 9.793039158772000263, 5.817107086401000160, -6.945352709928000579 ) ) ;
#38829 = CARTESIAN_POINT ( 'NONE',  ( 10.42380110216399913, 3.026453990125600235, -6.905442784147899360 ) ) ;
#38831 = EDGE_CURVE ( 'NONE', #6697, #4626, #16133, .T. ) ;
#38830 = AXIS2_PLACEMENT_3D ( 'NONE', #2682, #45343, #67669 ) ;
#38832 = EDGE_CURVE ( 'NONE', #58820, #38546, #25779, .T. ) ;
#38833 = CARTESIAN_POINT ( 'NONE',  ( 9.624831031535665105, 2.894183647070226240, 8.301356454186311851 ) ) ;
#38835 = CARTESIAN_POINT ( 'NONE',  ( 24.74122213638286283, 11.75038693034401582, 3.191108129339069066 ) ) ;
#38834 = DIRECTION ( 'NONE',  ( -1.000000000000000000, 9.336940512380999085E-10, 4.862374338246000196E-11 ) ) ;
#38836 = CARTESIAN_POINT ( 'NONE',  ( 9.326138961223998436, -3.281636118526699786, 7.014550357332099750 ) ) ;
#38837 = CARTESIAN_POINT ( 'NONE',  ( 11.19518313518939934, -4.537300658085600347, -8.179416362154199760 ) ) ;
#38838 = DIRECTION ( 'NONE',  ( 0.000000000000000000, 0.9565994702956989171, 0.2914059941558995170 ) ) ;
#38839 = ORIENTED_EDGE ( 'NONE', *, *, #20347, .F. ) ;
#38840 = VECTOR ( 'NONE', #39908, 1000.000000000000114 ) ;
#38841 = B_SPLINE_CURVE_WITH_KNOTS ( 'NONE', 3,
 ( #39031, #22933, #66617, #17350, #54754, #12805, #49505, #6853, #18394, #28190, #23291, #2308, #18052, #60688, #40070, #55451, #39719, #18738, #33787, #7209, #23630, #56133, #22588, #61381, #1618, #7545, #8241, #29588, #28900, #65583, #7899 ),
 .UNSPECIFIED., .F., .F.,
 ( 4, 2, 2, 1, 1, 2, 2, 2, 1, 2, 2, 2, 2, 2, 2, 2, 4 ),
 ( 0.000000000000000000, 0.06249999999999727995, 0.09374999999999585054, 0.1093749999999960310, 0.1171874999999960032, 0.1210937499999974465, 0.1249999999999988898, 0.1874999999999890643, 0.2187499999999843459, 0.2343749999999831524, 0.2499999999999819311, 0.3749999999999888978, 0.4374999999999925060, 0.4687499999999932832, 0.4999999999999941158, 0.7499999999999971134, 1.000000000000000000 ),
 .UNSPECIFIED. ) ;
#38842 = CARTESIAN_POINT ( 'NONE',  ( 1.739384680100000136, 3.214278412021000175, -0.5382386926684999962 ) ) ;
#38843 = LINE ( 'NONE', #53875, #50122 ) ;
#38844 = VECTOR ( 'NONE', #41174, 1000.000000000000000 ) ;
#38845 = LINE ( 'NONE', #27666, #18453 ) ;
#38846 = CARTESIAN_POINT ( 'NONE',  ( 9.374380199233998567, 4.860242402105300563, 7.608124715612800237 ) ) ;
#38847 = CARTESIAN_POINT ( 'NONE',  ( 11.00000000000000000, -3.008232475376599879, -7.174999999999999822 ) ) ;
#38849 = CARTESIAN_POINT ( 'NONE',  ( 12.11714050632482298, -2.287289704013994562, 13.81189467606769306 ) ) ;
#38848 = VECTOR ( 'NONE', #8228, 1000.000000000000000 ) ;
#38850 = CARTESIAN_POINT ( 'NONE',  ( 11.04796807867000119, 2.753385297824999967, 5.093099052209000277 ) ) ;
#38851 = CARTESIAN_POINT ( 'NONE',  ( 24.02041540912000173, 3.259263043209999822, -12.61480718775999854 ) ) ;
#38852 = CARTESIAN_POINT ( 'NONE',  ( 23.60000648208766805, 13.25016727112855186, 4.189782993036962999 ) ) ;
#38853 = ORIENTED_EDGE ( 'NONE', *, *, #33227, .F. ) ;
#38854 = CARTESIAN_POINT ( 'NONE',  ( 7.479583333330875661, 3.823285413235573582, -6.150000000000000355 ) ) ;
#38855 = ADVANCED_FACE ( 'NONE', ( #57584 ), #17217, .T. ) ;
#38856 = CARTESIAN_POINT ( 'NONE',  ( 17.55505043854147118, -2.500000000000000000, -25.00000000000000000 ) ) ;
#38857 = CARTESIAN_POINT ( 'NONE',  ( 9.814910518647794291, 2.650130971540564317, -7.499994893876710478 ) ) ;
#38858 = CIRCLE ( 'NONE', #66797, 0.5000000000000001110 ) ;
#38859 = FACE_OUTER_BOUND ( 'NONE', #53303, .T. ) ;
#38860 = CARTESIAN_POINT ( 'NONE',  ( 1.419020781218000016, 0.7707009544374999743, -3.678912518181000291 ) ) ;
#38861 = CARTESIAN_POINT ( 'NONE',  ( 1.948890132539667031, 2.798833948393634863, -2.150913519912196925 ) ) ;
#38862 = CARTESIAN_POINT ( 'NONE',  ( 17.99286279921835785, 2.053846844283184758, -12.54442212638278242 ) ) ;
#38863 = CARTESIAN_POINT ( 'NONE',  ( 18.30000000000000071, 52.95171880992000268, -18.02623547589999831 ) ) ;
#38864 = CARTESIAN_POINT ( 'NONE',  ( 10.67826222744820086, 3.331419131587999960, 6.949274830123499669 ) ) ;
#38865 = CONICAL_SURFACE ( 'NONE', #14317, 2.100034213237000014, 0.7853981633972997312 ) ;
#38866 = CARTESIAN_POINT ( 'NONE',  ( 15.65828218294664254, 9.154335746262503903, 8.252742830647335381 ) ) ;
#38867 = CARTESIAN_POINT ( 'NONE',  ( 10.81188185321000006, -4.614147550108000928, -5.930138617968999881 ) ) ;
#38868 = CARTESIAN_POINT ( 'NONE',  ( 11.35394403557610410, 3.574442861579692376, -11.79291672678741421 ) ) ;
#38869 = CARTESIAN_POINT ( 'NONE',  ( 12.09999999995609876, -11.00695867695318420, 3.817557008989782563 ) ) ;
#38870 = CARTESIAN_POINT ( 'NONE',  ( 12.19822292038682221, -2.649955820708161713, 12.41539170522314706 ) ) ;
#38871 = VERTEX_POINT ( 'NONE', #29593 ) ;
#38872 = CARTESIAN_POINT ( 'NONE',  ( 10.99600479835999955, -8.064994891046000092, -6.834771013433999620 ) ) ;
#38873 = ORIENTED_EDGE ( 'NONE', *, *, #19334, .T. ) ;
#38874 = CARTESIAN_POINT ( 'NONE',  ( 18.15689837892993097, -2.331154328543900700, 13.70782442673660206 ) ) ;
#38875 = LINE ( 'NONE', #60197, #19629 ) ;
#38876 = ORIENTED_EDGE ( 'NONE', *, *, #3466, .T. ) ;
#38877 = CARTESIAN_POINT ( 'NONE',  ( 11.48522412107029922, 4.047131449166419870, 8.390877922225699947 ) ) ;
#38878 = CARTESIAN_POINT ( 'NONE',  ( 6.277723390171241924, -0.9000774111393842203, 0.6873532864722641245 ) ) ;
#38879 = CARTESIAN_POINT ( 'NONE',  ( 24.11584421453913762, 3.333336234422446420, -12.53522527563100653 ) ) ;
#38880 = CARTESIAN_POINT ( 'NONE',  ( 9.442843574488000158, 2.691255504502000129, 6.269523028052000235 ) ) ;
#38881 = CARTESIAN_POINT ( 'NONE',  ( 8.508401286604998504, 5.100000004859538194, -6.571371713575075546 ) ) ;
#38882 = CARTESIAN_POINT ( 'NONE',  ( 10.78976354018291239, -4.327184855449096368, 8.717465845835395299 ) ) ;
#38883 = CARTESIAN_POINT ( 'NONE',  ( 11.56566386073000174, 3.232480401124999680, -11.43828361194000109 ) ) ;
#38884 = EDGE_CURVE ( 'NONE', #15849, #15877, #23692, .T. ) ;
#38885 = CARTESIAN_POINT ( 'NONE',  ( 10.99479839230999900, -3.850614833844999918, -9.347951988117998212 ) ) ;
#38886 = CARTESIAN_POINT ( 'NONE',  ( 11.61364291764652812, -4.859654669415900408, -7.393734108507599601 ) ) ;
#38887 = ORIENTED_EDGE ( 'NONE', *, *, #34333, .T. ) ;
#38888 = CARTESIAN_POINT ( 'NONE',  ( 10.52209773956086458, -3.051556286204309743, -5.005589990389688104 ) ) ;
#38889 = ORIENTED_EDGE ( 'NONE', *, *, #59986, .F. ) ;
#38890 = CYLINDRICAL_SURFACE ( 'NONE', #35915, 0.5000000000000002220 ) ;
#38891 = B_SPLINE_CURVE_WITH_KNOTS ( 'NONE', 3,
 ( #25882, #41617, #26580, #31822, #68173 ),
 .UNSPECIFIED., .F., .F.,
 ( 4, 1, 4 ),
 ( 0.000000000000000000, 0.5000000000000000000, 1.000000000000000000 ),
 .UNSPECIFIED. ) ;
#38892 = VERTEX_POINT ( 'NONE', #57854 ) ;
#38893 = CARTESIAN_POINT ( 'NONE',  ( 11.50004200479687633, -11.55567552917520935, -1.481524094250667556 ) ) ;
#38894 = CARTESIAN_POINT ( 'NONE',  ( 10.28599623668000085, -4.700321302673000190, 5.006347807457999899 ) ) ;
#38895 = CARTESIAN_POINT ( 'NONE',  ( 0.1499942179679999987, 2.750000000000000000, 0.000000000000000000 ) ) ;
#38896 = CARTESIAN_POINT ( 'NONE',  ( 10.08963399569799790, 5.271405458160000279, -7.641111829547599932 ) ) ;
#38897 = CARTESIAN_POINT ( 'NONE',  ( 12.21869931586264002, 2.282676242266353128, 13.71712068105209603 ) ) ;
#38898 = CARTESIAN_POINT ( 'NONE',  ( 9.479212726990999371, -4.071727350623000063, 9.089303488377000306 ) ) ;
#38899 = EDGE_LOOP ( 'NONE', ( #55905, #19498, #7769, #34675, #64809 ) ) ;
#38900 = VECTOR ( 'NONE', #53941, 1000.000000000000000 ) ;
#38901 = CYLINDRICAL_SURFACE ( 'NONE', #34820, 0.5000000000000004441 ) ;
#38902 = CARTESIAN_POINT ( 'NONE',  ( 12.30894494036362019, 0.5330308249010283772, 13.98985951701901520 ) ) ;
#38903 = ORIENTED_EDGE ( 'NONE', *, *, #38831, .F. ) ;
#38904 = CARTESIAN_POINT ( 'NONE',  ( 7.254771682458000193, 3.668692617901999853, -8.939602259005999585 ) ) ;
#38905 = CARTESIAN_POINT ( 'NONE',  ( 18.36663043076582724, 2.717294527786511704, 11.46570543779412787 ) ) ;
#38906 = CARTESIAN_POINT ( 'NONE',  ( 23.58678704957500116, -3.018899350941000037, -13.60646675873000078 ) ) ;
#38907 = CARTESIAN_POINT ( 'NONE',  ( 5.074249783945999681, -0.3757116368264999950, 1.356905753638999901 ) ) ;
#38908 = CARTESIAN_POINT ( 'NONE',  ( 10.21398584123000042, 3.990126737362999609, -8.809457313313998839 ) ) ;
#38909 = CYLINDRICAL_SURFACE ( 'NONE', #41393, 12.50000000000000000 ) ;
#38910 = CARTESIAN_POINT ( 'NONE',  ( 10.56270535986999981, -2.509383044034000143, -8.602408326857998944 ) ) ;
#38911 = VECTOR ( 'NONE', #62602, 1000.000000000000114 ) ;
#38912 = CARTESIAN_POINT ( 'NONE',  ( 7.877465178218598041, -5.139684893972532365, 6.768899977688172420 ) ) ;
#38913 = DIRECTION ( 'NONE',  ( -0.000000000000000000, -0.000000000000000000, 1.000000000000000000 ) ) ;
#38914 = CARTESIAN_POINT ( 'NONE',  ( 5.000000004241000440, 0.05000000424131000043, -3.149999962200000336 ) ) ;
#38915 = PLANE ( 'NONE',  #30780 ) ;
#38916 = PLANE ( 'NONE',  #34690 ) ;
#38917 = CARTESIAN_POINT ( 'NONE',  ( 12.43982406843060851, -0.6284010951954579483, 12.58437167746757623 ) ) ;
#38918 = EDGE_CURVE ( 'NONE', #59040, #65610, #46340, .T. ) ;
#38919 = EDGE_CURVE ( 'NONE', #40232, #4735, #37802, .T. ) ;
#38920 = CARTESIAN_POINT ( 'NONE',  ( 11.60988784977536348, 3.148894096305599799, -7.451365240271489832 ) ) ;
#38921 = CARTESIAN_POINT ( 'NONE',  ( 9.811963142879999822, 4.982812171771600518, -7.292822454528599785 ) ) ;
#38923 = LINE ( 'NONE', #39607, #9379 ) ;
#38922 = CARTESIAN_POINT ( 'NONE',  ( 10.83688779216199904, -3.198058499272899979, 7.210800365544999480 ) ) ;
#38924 = CARTESIAN_POINT ( 'NONE',  ( 11.27934687351631382, -4.163624617374463988, 8.750000000000001776 ) ) ;
#38925 = EDGE_LOOP ( 'NONE', ( #18268, #44017, #61538, #12643 ) ) ;
#38926 = CARTESIAN_POINT ( 'NONE',  ( 11.22567835872029995, 3.006051690924700370, 8.126439557340900066 ) ) ;
#38927 = CARTESIAN_POINT ( 'NONE',  ( 9.657547180956999711, -5.333447643521000536, 6.049925825719999928 ) ) ;
#38928 = CARTESIAN_POINT ( 'NONE',  ( 10.18893802597399834, 3.406370524467499994, 8.475365825607600101 ) ) ;
#38929 = PLANE ( 'NONE',  #17987 ) ;
#38930 = CARTESIAN_POINT ( 'NONE',  ( 9.634027193201999850, -3.042970193091000031, 8.588108172435999776 ) ) ;
#38931 = CARTESIAN_POINT ( 'NONE',  ( 11.09999803709000155, -1.199999999999999956, 9.776630298829998011 ) ) ;
#38932 = DIRECTION ( 'NONE',  ( 9.901258578469000068E-11, -9.901224327269000045E-11, -1.000000000000000000 ) ) ;
#38933 = ORIENTED_EDGE ( 'NONE', *, *, #43405, .T. ) ;
#38934 = EDGE_CURVE ( 'NONE', #38871, #23293, #32001, .T. ) ;
#38935 = CARTESIAN_POINT ( 'NONE',  ( 8.900113844317997902, -3.746347404385800051, -6.528144732449299603 ) ) ;
#38936 = CARTESIAN_POINT ( 'NONE',  ( 11.10000000009000054, 2.699999999911000259, 6.571291220400000022 ) ) ;
#38937 = CARTESIAN_POINT ( 'NONE',  ( 5.699991087009000701, -1.413039514337999902, -0.3998085520867999954 ) ) ;
#38938 = EDGE_CURVE ( 'NONE', #42472, #18819, #57868, .T. ) ;
#38939 = CARTESIAN_POINT ( 'NONE',  ( 6.999999999999999112, 9.785203231686947944, -4.607313921344089458 ) ) ;
#38940 = AXIS2_PLACEMENT_3D ( 'NONE', #45016, #1319, #28595 ) ;
#38941 = CARTESIAN_POINT ( 'NONE',  ( 24.25374608244500152, -3.234182954713999969, 12.21793987376999979 ) ) ;
#38942 = CARTESIAN_POINT ( 'NONE',  ( 12.72277096606028479, 0.6196453797482972536, -12.67964297675818308 ) ) ;
#38943 = B_SPLINE_CURVE_WITH_KNOTS ( 'NONE', 3,
 ( #62633, #8138, #45884, #9157, #67194, #4252, #68219, #14422, #40296, #15097, #46916, #19306, #13731, #25240, #20337, #36421, #67537, #29484, #50791, #61615, #35063, #56379, #8482, #35400, #30165, #30494, #51468, #20003, #3565, #46576, #24900, #46230, #51807, #15445, #31192, #4943, #5971, #32558, #53190, #16124, #10532, #43395, #27310, #26630, #31524, #42365, #53536, #5288, #52846, #26281, #25930, #47948, #57735, #52498, #31872, #48, #37450, #53870, #48634, #64007, #58771, #736, #4594, #47260, #21706, #68564, #47607 ),
 .UNSPECIFIED., .F., .F.,
 ( 4, 2, 2, 2, 2, 2, 2, 2, 2, 2, 2, 2, 2, 2, 1, 1, 1, 2, 2, 2, 2, 2, 2, 2, 2, 2, 2, 2, 2, 2, 2, 2, 2, 2, 4 ),
 ( 0.000000000000000000, 0.1250000000000538458, 0.2500000000001076916, 0.3125000000001355582, 0.3437500000001494915, 0.3750000000001633693, 0.4062500000001773026, 0.4218750000001832978, 0.4375000000001892930, 0.4687500000002018385, 0.4843750000002080558, 0.5000000000002141620, 0.5156250000002204903, 0.5312500000002265965, 0.5468750000002328138, 0.5546875000002357003, 0.5585937500002366995, 0.5605468750002376987, 0.5625000000002385869, 0.5781250000002332579, 0.5859375000002308154, 0.5898437500002297051, 0.5937500000002284839, 0.6093750000002220446, 0.6171875000002184919, 0.6250000000002148282, 0.6406250000002076117, 0.6562500000002002842, 0.6718750000001930678, 0.6875000000001857403, 0.7187500000001714184, 0.7343750000001633138, 0.7500000000001553202, 0.8750000000000777156, 1.000000000000000000 ),
 .UNSPECIFIED. ) ;
#38944 = B_SPLINE_CURVE_WITH_KNOTS ( 'NONE', 3,
 ( #42163, #31669, #36564, #6027, #27367, #47060, #68363, #58231, #11616, #48692, #38188, #30987, #43796, #20826, #41468, #15586, #30635, #49034 ),
 .UNSPECIFIED., .F., .F.,
 ( 4, 2, 2, 2, 2, 2, 2, 2, 4 ),
 ( 0.000000000000000000, 0.1250000000000000000, 0.2500000000000000000, 0.3750000000000000000, 0.5000000000000000000, 0.6250000000000000000, 0.7500000000000000000, 0.8750000000000000000, 1.000000000000000000 ),
 .UNSPECIFIED. ) ;
#38945 = CARTESIAN_POINT ( 'NONE',  ( 11.65871932425156920, 3.852858594438699935, -8.492622906483498824 ) ) ;
#38946 = DIRECTION ( 'NONE',  ( 0.000000000000000000, 1.000000000000000000, 0.000000000000000000 ) ) ;
#38948 = DIRECTION ( 'NONE',  ( 1.000000000000000000, 0.000000000000000000, 0.000000000000000000 ) ) ;
#38947 = CIRCLE ( 'NONE', #12147, 11.84999999999999964 ) ;
#38949 = CARTESIAN_POINT ( 'NONE',  ( 12.15446082633427771, 2.110350925085022311, 12.42276656535977075 ) ) ;
#38950 = ORIENTED_EDGE ( 'NONE', *, *, #67649, .F. ) ;
#38951 = LINE ( 'NONE', #23203, #53372 ) ;
#38952 = CARTESIAN_POINT ( 'NONE',  ( 12.78109991897669673, -0.7302151993337216984, -13.98094363222392111 ) ) ;
#38953 = CARTESIAN_POINT ( 'NONE',  ( 11.11486084871780022, 5.207010770456999893, 7.825000000000000178 ) ) ;
#38954 = CARTESIAN_POINT ( 'NONE',  ( 24.78219853511300030, -8.655325328077999814, -9.168174285775998911 ) ) ;
#38955 = CARTESIAN_POINT ( 'NONE',  ( 4.900006121741999010, 2.000000000000000000, 0.000000000000000000 ) ) ;
#38956 = CARTESIAN_POINT ( 'NONE',  ( 6.999999999999999112, 9.047814540315521015, 4.692211904642501707 ) ) ;
#38957 = CARTESIAN_POINT ( 'NONE',  ( 13.73936233968600185, 12.30487262812000004, 2.534071019599000163 ) ) ;
#38958 = ORIENTED_EDGE ( 'NONE', *, *, #50292, .F. ) ;
#38959 = CARTESIAN_POINT ( 'NONE',  ( 11.79999999771000141, 3.595163221087000149, -11.99793848941000007 ) ) ;
#38960 = CARTESIAN_POINT ( 'NONE',  ( 17.84276413147952312, 1.945066902726407365, -13.77561296414734038 ) ) ;
#38961 = ORIENTED_EDGE ( 'NONE', *, *, #21347, .F. ) ;
#38962 = CARTESIAN_POINT ( 'NONE',  ( 25.46373029971899982, -8.354610197568000274, -8.148451206582999262 ) ) ;
#38963 = CARTESIAN_POINT ( 'NONE',  ( 9.059370559623998176, -4.192917962110999319, 5.525484568403999930 ) ) ;
#38964 = CARTESIAN_POINT ( 'NONE',  ( 9.269689158774999882, 3.135494838036999798, -8.598037907310999373 ) ) ;
#38965 = CARTESIAN_POINT ( 'NONE',  ( 23.96074323759690472, -12.77529261571510588, 3.513705325918512923 ) ) ;
#38966 = CARTESIAN_POINT ( 'NONE',  ( 11.63611496860034933, -2.828587461987000395, -6.899705789500199415 ) ) ;
#38967 = CARTESIAN_POINT ( 'NONE',  ( 17.55505043854144276, 0.6250000000000001110, -12.67928921589118474 ) ) ;
#38968 = CARTESIAN_POINT ( 'NONE',  ( 10.93333333333530710, -5.319670837134319541, 7.972931767323275132 ) ) ;
#38969 = ORIENTED_EDGE ( 'NONE', *, *, #22077, .F. ) ;
#38970 = CARTESIAN_POINT ( 'NONE',  ( 8.343110571751518378, 3.605921234441439971, -6.059113279906364724 ) ) ;
#38971 = CARTESIAN_POINT ( 'NONE',  ( 18.16782992325282819, -2.622990444980092928, -13.64655204333130278 ) ) ;
#38972 = CARTESIAN_POINT ( 'NONE',  ( 17.63765675170532532, -1.875000000000000666, 13.78631904427528809 ) ) ;
#38973 = ORIENTED_EDGE ( 'NONE', *, *, #37110, .T. ) ;
#38974 = CARTESIAN_POINT ( 'NONE',  ( 10.61721774768000159, 5.045603402166999985, -6.386910706193999587 ) ) ;
#38975 = CARTESIAN_POINT ( 'NONE',  ( 11.33381694038000020, -2.642393655627000015, -7.577897390831000557 ) ) ;
#38976 = ORIENTED_EDGE ( 'NONE', *, *, #49392, .F. ) ;
#38977 = CARTESIAN_POINT ( 'NONE',  ( 8.900113844317997902, 4.253652595614200393, 8.471855267550699509 ) ) ;
#38978 = CARTESIAN_POINT ( 'NONE',  ( 18.12596594012301665, -2.036641643015561609, -12.43431447687783020 ) ) ;
#38979 = LINE ( 'NONE', #60297, #63731 ) ;
#38980 = CARTESIAN_POINT ( 'NONE',  ( 15.86395943152100330, 3.857419000648000029, 11.66670712924999975 ) ) ;
#38981 = PLANE ( 'NONE',  #46350 ) ;
#38982 = EDGE_CURVE ( 'NONE', #47459, #53505, #21709, .T. ) ;
#38983 = CARTESIAN_POINT ( 'NONE',  ( 9.155417874594000693, 3.202096358337300330, 7.160798403412399260 ) ) ;
#38984 = CARTESIAN_POINT ( 'NONE',  ( 13.42725895571207140, -12.36922847561405803, -1.970373770729125562 ) ) ;
#38985 = VERTEX_POINT ( 'NONE', #43504 ) ;
#38986 = CARTESIAN_POINT ( 'NONE',  ( 11.02445190299000011, 3.404087387974999768, 5.822483872269000216 ) ) ;
#38987 = CARTESIAN_POINT ( 'NONE',  ( 10.62256721958999961, 2.471460423959999986, -8.210789473540000216 ) ) ;
#38988 = CARTESIAN_POINT ( 'NONE',  ( 13.48771849468917061, 12.09748862696537763, 2.366366213948144281 ) ) ;
#38989 = CARTESIAN_POINT ( 'NONE',  ( 12.49074413817427853, 3.040604467177680181, -13.54382360563872822 ) ) ;
#38990 = CARTESIAN_POINT ( 'NONE',  ( 9.811013376692999444, -5.140392946802999852, -6.920441276178300072 ) ) ;
#38991 = CARTESIAN_POINT ( 'NONE',  ( 10.58844302970999962, -3.754658547780000521, 5.545362468768000319 ) ) ;
#38992 = CARTESIAN_POINT ( 'NONE',  ( 17.93874521385978582, -0.6200266137005079337, 13.98626978124057807 ) ) ;
#38993 = CARTESIAN_POINT ( 'NONE',  ( 17.55505043854144276, 0.6250000000000001110, 13.88107975066923316 ) ) ;
#38994 = ORIENTED_EDGE ( 'NONE', *, *, #7971, .F. ) ;
#38995 = ORIENTED_EDGE ( 'NONE', *, *, #30478, .F. ) ;
#38996 = AXIS2_PLACEMENT_3D ( 'NONE', #42617, #5885, #38396 ) ;
#38997 = CARTESIAN_POINT ( 'NONE',  ( 9.237204719595000668, 3.071719032003000116, -6.037263251225000182 ) ) ;
#38998 = CARTESIAN_POINT ( 'NONE',  ( 12.25734203455823135, -0.3012395220628200643, 13.89560941713585684 ) ) ;
#38999 = CARTESIAN_POINT ( 'NONE',  ( 12.57406875483051856, -0.5808247544188634981, -13.88366201036165570 ) ) ;
#39000 = CARTESIAN_POINT ( 'NONE',  ( 11.00008140503725329, -2.915874161187789859, -7.367730262387956586 ) ) ;
#39001 = PLANE ( 'NONE',  #1554 ) ;
#39002 = EDGE_CURVE ( 'NONE', #7917, #40162, #60800, .T. ) ;
#39003 = EDGE_CURVE ( 'NONE', #34244, #2041, #63433, .T. ) ;
#39004 = CARTESIAN_POINT ( 'NONE',  ( 8.283081853209001366, -2.376522687267000222, 7.686981355459999499 ) ) ;
#39005 = CARTESIAN_POINT ( 'NONE',  ( 8.710288521113000115, 3.647046440108700160, -8.284550957747498501 ) ) ;
#39007 = DIRECTION ( 'NONE',  ( 0.000000000000000000, 0.9916377111174247139, -0.1290528957048031888 ) ) ;
#39006 = CARTESIAN_POINT ( 'NONE',  ( 10.03239275768699912, -3.136549968260000210, 6.556157624301499176 ) ) ;
#39008 = CARTESIAN_POINT ( 'NONE',  ( 10.05041772631199848, 4.549624259497900169, -8.631352948887998977 ) ) ;
#39009 = EDGE_CURVE ( 'NONE', #52535, #23213, #19478, .T. ) ;
#39010 = CARTESIAN_POINT ( 'NONE',  ( 7.000000000000000000, -0.2897247358851999799, -3.000000000000000000 ) ) ;
#39011 = CARTESIAN_POINT ( 'NONE',  ( 17.94405014054366987, 11.44468665172112942, -4.547234080929012379 ) ) ;
#39012 = CARTESIAN_POINT ( 'NONE',  ( 17.69772537084632091, 0.6088395004560440693, 12.68034807294329447 ) ) ;
#39013 = B_SPLINE_SURFACE_WITH_KNOTS ( 'NONE', 1, 3, ( 
 ( #29060, #50370, #2470, #23796, #66439, #45472, #66789, #40228, #8410, #25168, #10122, #26208, #47881, #57663, #30764, #36004, #3830, #31120, #62903, #31454, #46503, #31800, #58020, #52772, #53116, #5218, #15024, #37379, #47536, #20268, #52423, #67806, #32148, #46845, #52074, #4867, #68490, #26554, #9421, #20614, #68149, #41938, #68841, #21297, #20959, #42627, #41594, #42297, #63246, #19930, #63595, #41251, #15713, #69185, #63937, #36348, #37041, #9769, #16048, #25856, #4520, #58356, #62566, #15371, #14685, #57320, #47189, #36700, #10458, #58701, #10804, #4178, #25517, #48211, #33173, #23017, #6591, #17432, #22668, #60429, #44011, #59049, #21634, #5557, #53464, #49241 ),
 ( #44365, #1351, #318, #65316, #16393, #32485, #27581, #64623, #65664, #38060, #32825, #6935, #21978, #59384, #27932, #59732, #12537, #39105, #43665, #17787, #38761, #12192, #5896, #26899, #42969, #54141, #38408, #64276, #6239, #60086, #37720, #16731, #27238, #33520, #43319, #11151, #53799, #11485, #48562, #54839, #28270, #666, #11833, #49590, #48907, #1015, #22323, #1697, #64962, #17075, #54490, #45731, #2730, #34900, #13238, #7983, #55181, #67376, #56559, #13918, #67039, #23369, #2386, #55533, #19150, #33866, #50285, #13580, #12885, #44709, #50972, #66006, #49939, #19500, #40472, #23710, #39451, #3068, #51314, #62142, #28625, #3409, #24401, #56216, #24744, #45045 ) ),
 .UNSPECIFIED., .F., .F., .F.,
 ( 2, 2 ),
 ( 4, 2, 2, 2, 2, 2, 2, 2, 2, 2, 2, 2, 2, 2, 2, 2, 2, 2, 2, 2, 2, 2, 2, 2, 2, 2, 2, 2, 2, 2, 2, 2, 2, 2, 2, 2, 2, 2, 2, 2, 2, 2, 4 ),
 ( 0.000000000000000000, 1.000000000000000000 ),
 ( 0.000000000000000000, 7.142680049747107468E-05, 0.0001428536009949421494, 0.0002142804014924132240, 0.0002857072019898842987, 0.0003571340024873553734, 0.0004285608029848264481, 0.0004999876034822974685, 0.0005357010037310330330, 0.0005714144039797685974, 0.0006071278042285041619, 0.0006428412044772397263, 0.0007142680049747107468, 0.0007856948054721817672, 0.0008214082057209173317, 0.0008571216059696528961, 0.0008928350062183884606, 0.0009285484064671239166, 0.0009999752069645949371, 0.001071402007462066066, 0.001142828807959537195, 0.001214255608457008324, 0.001285682408954479453, 0.001321395809203215017, 0.001357109209451950581, 0.001428536009949421494, 0.001499962810446892406, 0.001535676210695627970, 0.001571389610944363534, 0.001607103011193099099, 0.001642816411441834663, 0.001714243211939305792, 0.001785670012436776921, 0.001821383412685512269, 0.001857096812934247833, 0.001928523613431718745, 0.001964237013680454093, 0.001999950413929189874, 0.002035663814177925655, 0.002071377214426661003, 0.002142804014924132132, 0.002214230815421603261, 0.002285657615919074390 ),
 .UNSPECIFIED. ) ;
#39014 = DIRECTION ( 'NONE',  ( -1.000000000000000000, 0.000000000000000000, 0.000000000000000000 ) ) ;
#39015 = CARTESIAN_POINT ( 'NONE',  ( 4.149992563292000725, -2.000000000000000000, 0.000000000000000000 ) ) ;
#39016 = VERTEX_POINT ( 'NONE', #31986 ) ;
#39018 = CARTESIAN_POINT ( 'NONE',  ( 10.94452754078378121, 4.508448539877488059, 8.211034235888378774 ) ) ;
#39017 = CARTESIAN_POINT ( 'NONE',  ( 11.63220574173980992, -2.863826994586552654, 8.088082908809447247 ) ) ;
#39019 = CARTESIAN_POINT ( 'NONE',  ( 9.699495280410998177, 5.048004622677000341, -6.120508709481000231 ) ) ;
#39020 = CARTESIAN_POINT ( 'NONE',  ( 12.54469325725306916, -1.931433442391065958, 13.77773667378076006 ) ) ;
#39021 = CARTESIAN_POINT ( 'NONE',  ( 10.30204095393061081, -2.650238144765123760, -7.719132294906671632 ) ) ;
#39022 = CARTESIAN_POINT ( 'NONE',  ( 24.44496488009700030, 8.810487470433001178, 8.810507756548000557 ) ) ;
#39023 = B_SPLINE_CURVE_WITH_KNOTS ( 'NONE', 3,
 ( #40745, #62069, #35512, #8933, #3670, #9961, #47028, #31298, #52959, #41776, #5056, #42470, #16580, #42128, #64118, #69031, #52608, #15206 ),
 .UNSPECIFIED., .F., .F.,
 ( 4, 2, 2, 2, 2, 2, 2, 2, 4 ),
 ( 0.000000000000000000, 0.1250000000000000000, 0.2500000000000000000, 0.3750000000000000000, 0.5000000000000000000, 0.6250000000000000000, 0.7500000000000000000, 0.8750000000000000000, 1.000000000000000000 ),
 .UNSPECIFIED. ) ;
#39024 = B_SPLINE_SURFACE_WITH_KNOTS ( 'NONE', 3, 3, ( 
 ( #20714, #47635, #37476, #42388 ),
 ( #10907, #11582, #32251, #64372 ),
 ( #32926, #43065, #53560, #38157 ),
 ( #54238, #6693, #2491, #1113 ),
 ( #17892, #39555, #1456, #50045 ),
 ( #66459, #65418, #50391, #60879 ) ),
 .UNSPECIFIED., .F., .F., .F.,
 ( 4, 1, 1, 4 ),
 ( 4, 4 ),
 ( 0.1423941366080999915, 0.3333333333333000081, 0.6666666666667000474, 0.8219462302419999755 ),
 ( -0.1256563615234000120, 1.125656361508000192 ),
 .UNSPECIFIED. ) ;
#39025 = EDGE_CURVE ( 'NONE', #61432, #68324, #16231, .T. ) ;
#39026 = CARTESIAN_POINT ( 'NONE',  ( 8.610875063856999745, -4.757997781751000410, 5.934102420827000124 ) ) ;
#39027 = CARTESIAN_POINT ( 'NONE',  ( 3.548931641198000086, 2.181374122857000053, -2.586569627374999847 ) ) ;
#39028 = ORIENTED_EDGE ( 'NONE', *, *, #63369, .T. ) ;
#39029 = CARTESIAN_POINT ( 'NONE',  ( 12.11487221662461167, -0.2205548374446903714, -12.59807454672507809 ) ) ;
#39030 = CARTESIAN_POINT ( 'NONE',  ( 12.07240408529959907, -4.732472998177641443, 7.982112976485220557 ) ) ;
#39031 = CARTESIAN_POINT ( 'NONE',  ( 24.30001683613300045, -12.21047198529999989, -3.271805531187999883 ) ) ;
#39032 = CARTESIAN_POINT ( 'NONE',  ( 8.181107780410998842, 5.485785046334999748, 8.532070739720001740 ) ) ;
#39033 = ORIENTED_EDGE ( 'NONE', *, *, #32444, .T. ) ;
#39034 = CARTESIAN_POINT ( 'NONE',  ( 6.457675381438999551, -1.400415568386000009, 0.4419997549869000286 ) ) ;
#39035 = CARTESIAN_POINT ( 'NONE',  ( 8.634260841228998729, 5.171553746019000641, -8.261796965435999951 ) ) ;
#39037 = CARTESIAN_POINT ( 'NONE',  ( 25.30000327618300204, 10.83443035398000021, -3.855530949778000149 ) ) ;
#39036 = DIRECTION ( 'NONE',  ( 0.000000000000000000, -0.5000000000000168754, 0.8660254037844288266 ) ) ;
#39038 = CARTESIAN_POINT ( 'NONE',  ( 10.92968717260509948, 3.312350236372100021, -8.622362941748999532 ) ) ;
#39039 = ORIENTED_EDGE ( 'NONE', *, *, #27025, .T. ) ;
#39040 = CARTESIAN_POINT ( 'NONE',  ( 10.98768472567999943, 5.449702577258999980, -4.945212061305999107 ) ) ;
#39041 = CARTESIAN_POINT ( 'NONE',  ( 10.06489140842196406, 5.349900232312646331, -7.500006335289779003 ) ) ;
#39042 = VERTEX_POINT ( 'NONE', #59224 ) ;
#39043 = DIRECTION ( 'NONE',  ( 0.000000000000000000, 1.000000000000000000, 0.000000000000000000 ) ) ;
#39044 = CARTESIAN_POINT ( 'NONE',  ( 15.90542051561399894, 3.482376784026000038, 11.36410125839000074 ) ) ;
#39045 = CARTESIAN_POINT ( 'NONE',  ( 17.91054527438923216, -0.5141525164327350739, -13.88720023103245360 ) ) ;
#39046 = ORIENTED_EDGE ( 'NONE', *, *, #57433, .F. ) ;
#39047 = CARTESIAN_POINT ( 'NONE',  ( 6.750663127261000263, -9.312586504099000351, 5.427957373207999758 ) ) ;
#39048 = DIRECTION ( 'NONE',  ( 0.000000000000000000, -4.343197676503999927E-12, 1.000000000000000000 ) ) ;
#39049 = CARTESIAN_POINT ( 'NONE',  ( 7.441339158769000761, 3.563552687850000122, -6.172381771908999504 ) ) ;
#39050 = CARTESIAN_POINT ( 'NONE',  ( 8.599999986286999132, -4.750000013710600655, -7.499999999961952213 ) ) ;
#39051 = CARTESIAN_POINT ( 'NONE',  ( 17.79999999998900151, 3.595165934733000057, 11.99793354950999991 ) ) ;
#39052 = ORIENTED_EDGE ( 'NONE', *, *, #15529, .T. ) ;
#39053 = CARTESIAN_POINT ( 'NONE',  ( 12.80505043854146940, -1.836970230372604318, -12.54239289408378255 ) ) ;
#39054 = CARTESIAN_POINT ( 'NONE',  ( 24.02092288169400192, -12.55342276724000072, -3.484368012066000109 ) ) ;
#39055 = CARTESIAN_POINT ( 'NONE',  ( 12.56916471290668547, -1.825881566109255338, 13.88043612360053203 ) ) ;
#39056 = ORIENTED_EDGE ( 'NONE', *, *, #67709, .T. ) ;
#39057 = CARTESIAN_POINT ( 'NONE',  ( 23.72389732855361189, 13.12882099560536631, -3.830240572390830600 ) ) ;
#39058 = CARTESIAN_POINT ( 'NONE',  ( 10.90000000296000060, 2.899999999990999999, 5.160242730682999657 ) ) ;
#39059 = CARTESIAN_POINT ( 'NONE',  ( 10.90000000162999960, 2.899999999992999733, -5.160242739096000619 ) ) ;
#39060 = ADVANCED_FACE ( 'NONE', ( #49085 ), #5794, .T. ) ;
#39061 = PLANE ( 'NONE',  #49790 ) ;
#39062 = DIRECTION ( 'NONE',  ( 0.000000000000000000, 1.000000000000000000, 0.000000000000000000 ) ) ;
#39063 = EDGE_CURVE ( 'NONE', #63182, #11912, #31635, .T. ) ;
#39064 = CARTESIAN_POINT ( 'NONE',  ( 5.940443173017124323, -0.1963495408493673156, 1.499999999999999556 ) ) ;
#39065 = CARTESIAN_POINT ( 'NONE',  ( 17.81516833538384859, -3.068391096118999517, 12.30080513712135826 ) ) ;
#39066 = EDGE_LOOP ( 'NONE', ( #22698, #45816, #16499, #54165 ) ) ;
#39067 = CARTESIAN_POINT ( 'NONE',  ( 11.76077869730539938, -4.595338376575799799, -6.326049646822999861 ) ) ;
#39068 = ORIENTED_EDGE ( 'NONE', *, *, #54658, .F. ) ;
#39069 = CARTESIAN_POINT ( 'NONE',  ( 11.44793382097000034, -12.36841772234000025, -1.594008128907999922 ) ) ;
#39070 = CARTESIAN_POINT ( 'NONE',  ( 8.367589158771000513, 5.461114003844000031, -8.582501063019000398 ) ) ;
#39071 = CARTESIAN_POINT ( 'NONE',  ( 3.257664066220000265, 1.608864567386000033, -2.971833076323999734 ) ) ;
#39072 = CARTESIAN_POINT ( 'NONE',  ( 9.766127544684000128, -4.735430008785999512, -8.791396910319001279 ) ) ;
#39073 = DIRECTION ( 'NONE',  ( 1.000000000000000000, 0.000000000000000000, 0.000000000000000000 ) ) ;
#39074 = CARTESIAN_POINT ( 'NONE',  ( 24.63625387988400206, 12.49728986131000141, 2.949034213397000226 ) ) ;
#39075 = CARTESIAN_POINT ( 'NONE',  ( 8.383148997457999130, -5.167567567567999731, 6.822293592207000934 ) ) ;
#39076 = B_SPLINE_CURVE_WITH_KNOTS ( 'NONE', 3,
 ( #35901, #18457, #57217, #39780 ),
 .UNSPECIFIED., .F., .F.,
 ( 4, 4 ),
 ( 0.000000000000000000, 1.000000000000000000 ),
 .UNSPECIFIED. ) ;
#39077 = ORIENTED_EDGE ( 'NONE', *, *, #53066, .F. ) ;
#39078 = PLANE ( 'NONE',  #64833 ) ;
#39079 = CARTESIAN_POINT ( 'NONE',  ( 10.95257053952200010, -4.394359323863099576, 8.422730500489899796 ) ) ;
#39080 = CARTESIAN_POINT ( 'NONE',  ( 11.06923869026000062, 5.425682056982999768, 8.012911262916999178 ) ) ;
#39081 = CARTESIAN_POINT ( 'NONE',  ( 8.849999778957998942, -4.000000000000000000, -7.500000000000000000 ) ) ;
#39082 = CYLINDRICAL_SURFACE ( 'NONE', #17588, 1.250000000000000222 ) ;
#39083 = CARTESIAN_POINT ( 'NONE',  ( 11.03333333333435640, 2.969278270712281564, 8.594189652917812339 ) ) ;
#39084 = CARTESIAN_POINT ( 'NONE',  ( 10.43210941423799909, 4.641185166475500168, -6.917608226833099394 ) ) ;
#39085 = ADVANCED_FACE ( 'NONE', ( #43150 ), #11670, .F. ) ;
#39086 = CARTESIAN_POINT ( 'NONE',  ( 10.30896519935103761, 4.355941342076152800, 9.241073271048676929 ) ) ;
#39087 = CARTESIAN_POINT ( 'NONE',  ( 9.935646554150999066, 4.552790318865400643, -8.499078230848398974 ) ) ;
#39088 = CARTESIAN_POINT ( 'NONE',  ( 23.58459662445000049, -10.19731050088000046, 9.579719261187998214 ) ) ;
#39089 = CARTESIAN_POINT ( 'NONE',  ( 8.114525141030208388, 5.047092373262178633, -6.489789622603527874 ) ) ;
#39090 = VERTEX_POINT ( 'NONE', #27775 ) ;
#39091 = CARTESIAN_POINT ( 'NONE',  ( 8.785191940379998954, -5.414909314743000301, 8.890670256079998168 ) ) ;
#39092 = CARTESIAN_POINT ( 'NONE',  ( 10.18225119159999892, -4.505165106450999879, -8.732017808253001334 ) ) ;
#39093 = CARTESIAN_POINT ( 'NONE',  ( 17.74496479089903289, 1.812889415971022933, 13.88212816151363782 ) ) ;
#39094 = CARTESIAN_POINT ( 'NONE',  ( 11.09999999999999964, -2.646159083949000124, 6.745271721726000536 ) ) ;
#39095 = CARTESIAN_POINT ( 'NONE',  ( 10.27610941423800028, -3.155589807313900153, -6.733017893878099791 ) ) ;
#39096 = ORIENTED_EDGE ( 'NONE', *, *, #1822, .F. ) ;
#39097 = CARTESIAN_POINT ( 'NONE',  ( 24.69899867863799869, 3.637718165649999946, -12.18533513769000010 ) ) ;
#39098 = CARTESIAN_POINT ( 'NONE',  ( 7.924357780410000274, 2.432118421226999949, 6.597517552098000060 ) ) ;
#39099 = EDGE_CURVE ( 'NONE', #31558, #16664, #47717, .T. ) ;
#39101 = CARTESIAN_POINT ( 'NONE',  ( 11.09590547754519996, 5.315605332491999846, 7.458246194669389872 ) ) ;
#39100 = CARTESIAN_POINT ( 'NONE',  ( 19.89999890908300273, 12.52500000000000036, 0.000000000000000000 ) ) ;
#39102 = CARTESIAN_POINT ( 'NONE',  ( 10.79701415876999882, 5.792870175253000298, -7.049262931951000510 ) ) ;
#39103 = ORIENTED_EDGE ( 'NONE', *, *, #7617, .T. ) ;
#39104 = CARTESIAN_POINT ( 'NONE',  ( 10.33536974457000035, 5.153692264686000613, 8.830864265869999841 ) ) ;
#39105 = CARTESIAN_POINT ( 'NONE',  ( 18.05368493555554821, -1.987806113122535523, -13.85816345346370504 ) ) ;
#39106 = CARTESIAN_POINT ( 'NONE',  ( 10.86687616594229944, 3.655053560864600204, 8.587337146608000182 ) ) ;
#39107 = CARTESIAN_POINT ( 'NONE',  ( 9.520803773887999810, -3.270557529354000348, 5.711489293131999823 ) ) ;
#39108 = CARTESIAN_POINT ( 'NONE',  ( 9.026933059621999433, -4.852736108563000528, 8.683927195503999386 ) ) ;
#39109 = EDGE_LOOP ( 'NONE', ( #44384, #35791, #13961 ) ) ;
#39110 = CARTESIAN_POINT ( 'NONE',  ( 24.51228084553499897, 12.11225741666999944, -3.153589928160999811 ) ) ;
#39112 = CARTESIAN_POINT ( 'NONE',  ( 10.08211398012999993, -4.728049789772000189, -8.793977405422999993 ) ) ;
#39111 = CARTESIAN_POINT ( 'NONE',  ( 12.34907277967800177, -11.89802509695999966, 3.395950604129000183 ) ) ;
#39113 = VECTOR ( 'NONE', #55213, 1000.000000000000000 ) ;
#39114 = CARTESIAN_POINT ( 'NONE',  ( 8.062962586773856799, -3.740282130435375496, 5.779432715689869937 ) ) ;
#39115 = CARTESIAN_POINT ( 'NONE',  ( 9.104016254283999743, -5.045864843302999780, 8.527867871227000407 ) ) ;
#39116 = CARTESIAN_POINT ( 'NONE',  ( 9.928735088624382144, -5.349822375552029108, 7.563678388627733007 ) ) ;
#39117 = CARTESIAN_POINT ( 'NONE',  ( 10.68144474310099845, -2.984290294633999974, 7.007085334055199510 ) ) ;
#39118 = ORIENTED_EDGE ( 'NONE', *, *, #38305, .T. ) ;
#39119 = CARTESIAN_POINT ( 'NONE',  ( 24.14062715026257422, -9.153323484003220045, 9.127327582134411088 ) ) ;
#39120 = CARTESIAN_POINT ( 'NONE',  ( 11.04687750876899877, -4.617914354660699772, 6.541108991297599928 ) ) ;
#39121 = ORIENTED_EDGE ( 'NONE', *, *, #1965, .T. ) ;
#39122 = CYLINDRICAL_SURFACE ( 'NONE', #761, 0.6999999999999992895 ) ;
#39123 = VERTEX_POINT ( 'NONE', #59571 ) ;
#39124 = CARTESIAN_POINT ( 'NONE',  ( 9.591185841232000797, 2.173570076733999823, -8.023168429484000441 ) ) ;
#39125 = CARTESIAN_POINT ( 'NONE',  ( 23.86982554649200239, 13.28496237665000024, -3.447284652217000200 ) ) ;
#39126 = DIRECTION ( 'NONE',  ( 0.000000000000000000, 0.000000000000000000, -1.000000000000000000 ) ) ;
#39127 = CARTESIAN_POINT ( 'NONE',  ( 12.08949137858161293, 2.599319321963733387, -12.32899351683632005 ) ) ;
#39128 = CARTESIAN_POINT ( 'NONE',  ( 11.98522412107029922, -3.952868550833580130, 8.390877922225699947 ) ) ;
#39129 = CARTESIAN_POINT ( 'NONE',  ( 30.60000000000000142, 0.000000000000000000, 8.250000000000000000 ) ) ;
#39130 = EDGE_LOOP ( 'NONE', ( #42250, #28939, #31597 ) ) ;
#39131 = CARTESIAN_POINT ( 'NONE',  ( 7.983191940377000861, -5.321924421352999701, 8.118250081378000971 ) ) ;
#39132 = CARTESIAN_POINT ( 'NONE',  ( 25.30000327618300204, -2.078227429405999693, 11.31065739696999906 ) ) ;
#39133 = EDGE_LOOP ( 'NONE', ( #58891, #65871, #38515, #19262 ) ) ;
#39134 = CARTESIAN_POINT ( 'NONE',  ( 12.15399652902990546, -2.797872959086246336, -12.28545279959702619 ) ) ;
#39135 = CARTESIAN_POINT ( 'NONE',  ( 10.25564828895399927, 4.880669054351300495, 7.018986873610899124 ) ) ;
#39136 = CARTESIAN_POINT ( 'NONE',  ( 10.34267055962000015, -5.750479631840000216, -8.094412205797999249 ) ) ;
#39137 = CARTESIAN_POINT ( 'NONE',  ( 10.40558702164999971, 5.599341344818000721, -8.437759619346000051 ) ) ;
#39138 = CARTESIAN_POINT ( 'NONE',  ( 18.54231177413599951, -11.92501070728000023, 3.951221890208000520 ) ) ;
#39139 = ADVANCED_FACE ( 'NONE', ( #54324 ), #11617, .F. ) ;
#39140 = CARTESIAN_POINT ( 'NONE',  ( 8.204580816340637739, -2.648164948733253699, 7.853008025111919643 ) ) ;
#39141 = DIRECTION ( 'NONE',  ( 1.000000000000000000, 0.000000000000000000, 0.000000000000000000 ) ) ;
#39142 = EDGE_CURVE ( 'NONE', #4046, #30003, #29280, .T. ) ;
#39143 = CARTESIAN_POINT ( 'NONE',  ( 17.98256582722315144, -0.4560270868711831516, -12.68898073362800893 ) ) ;
#39144 = DIRECTION ( 'NONE',  ( -0.8660254037844288266, 4.668797665416159739E-13, 0.5000000000000169864 ) ) ;
#39145 = CARTESIAN_POINT ( 'NONE',  ( 10.22687885159599830, -2.867290578374000365, -7.364871923548499844 ) ) ;
#39146 = EDGE_CURVE ( 'NONE', #19263, #30607, #40436, .T. ) ;
#39147 = EDGE_CURVE ( 'NONE', #59588, #19638, #48225, .T. ) ;
#39148 = CARTESIAN_POINT ( 'NONE',  ( 7.903989158771000056, 2.095715612964000218, 8.056490963156001328 ) ) ;
#39149 = EDGE_LOOP ( 'NONE', ( #1659, #51660, #258, #18418 ) ) ;
#39150 = SHAPE_REPRESENTATION_RELATIONSHIP ( 'NONE' , 'NONE' ,  #8579, #6030 ) ;
#39151 = CARTESIAN_POINT ( 'NONE',  ( 9.099999931440999390, 5.064317881551000156, -8.155535999783198875 ) ) ;
#39152 = LINE ( 'NONE', #60475, #17093 ) ;
#39153 = CARTESIAN_POINT ( 'NONE',  ( 10.51655086620999846, 4.930662802525000110, 8.573584269714999095 ) ) ;
#39154 = CARTESIAN_POINT ( 'NONE',  ( 23.58568928767000372, -3.200696684098000233, 13.61875409421000072 ) ) ;
#39155 = CARTESIAN_POINT ( 'NONE',  ( 18.02785359611323912, 2.090732611440657251, 12.53755739145393555 ) ) ;
#39156 = FACE_OUTER_BOUND ( 'NONE', #59460, .T. ) ;
#39157 = B_SPLINE_CURVE_WITH_KNOTS ( 'NONE', 3,
 ( #64183, #26108, #5469, #43217 ),
 .UNSPECIFIED., .F., .F.,
 ( 4, 4 ),
 ( 0.000000000000000000, 1.000000000000000000 ),
 .UNSPECIFIED. ) ;
#39158 = CARTESIAN_POINT ( 'NONE',  ( 10.77462860031000069, 5.575476001419000127, 8.682676628339999425 ) ) ;
#39159 = CARTESIAN_POINT ( 'NONE',  ( 10.38545795859862686, -3.143868186573851364, 7.680473230592850697 ) ) ;
#39160 = DIRECTION ( 'NONE',  ( -1.000000000000000000, 0.000000000000000000, 0.000000000000000000 ) ) ;
#39161 = ORIENTED_EDGE ( 'NONE', *, *, #45404, .T. ) ;
#39162 = CARTESIAN_POINT ( 'NONE',  ( 12.41914228198398717, -3.089530644545724680, 12.21535262842080805 ) ) ;
#39163 = CARTESIAN_POINT ( 'NONE',  ( 10.08359632033899800, -4.802737635155300389, -7.172402329663099430 ) ) ;
#39164 = CARTESIAN_POINT ( 'NONE',  ( 9.472537864290000442, 2.899999999999999911, -6.571291218949999902 ) ) ;
#39165 = CARTESIAN_POINT ( 'NONE',  ( 9.150818738817875442, 4.951062758656399332, 8.326721469190600189 ) ) ;
#39166 = B_SPLINE_SURFACE_WITH_KNOTS ( 'NONE', 3, 3, ( 
 ( #65661, #18469, #23366, #28267, #44361, #45042, #28622, #44706, #17783, #39102, #29313, #12532, #24050, #60426, #13576, #66347, #50626, #45728, #33863, #34897, #39795, #67036, #2727, #60767, #56213, #45385, #8322, #66003, #18126, #34561, #12882, #50967, #7628, #61118, #55872 ),
 ( #7979, #66695, #3065, #24398, #51309, #8997, #3406, #26115, #41503, #36258, #62474, #31028, #15282, #30340, #47443, #56898, #14257, #62815, #63505, #4431, #30007, #68398, #3743, #67372, #46067, #68060, #25078, #8660, #20866, #4087, #51646, #46412, #19497, #40814, #9678 ),
 ( #25769, #52337, #47098, #67713, #20175, #4773, #20521, #35242, #35916, #19839, #41847, #46757, #14596, #51981, #41169, #57230, #14934, #35584, #42204, #63153, #24741, #56556, #9330, #62138, #30675, #36605, #57931, #25423, #68749, #57575, #52679, #10028, #31367, #42883, #54403 ),
 ( #5476, #16303, #6503, #43924, #31709, #64190, #38318, #37628, #26812, #27152, #27493, #37291, #232, #58962, #10371, #27848, #15624, #6152, #48473, #63848, #43576, #36955, #11066, #59646, #32059, #48818, #53030, #32400, #58269, #5126, #53715, #5811, #43224, #11745, #33087 ) ),
 .UNSPECIFIED., .F., .F., .F.,
 ( 4, 4 ),
 ( 4, 1, 1, 1, 1, 1, 1, 1, 1, 1, 1, 1, 1, 1, 1, 1, 1, 1, 1, 1, 1, 1, 1, 1, 1, 1, 1, 1, 1, 1, 1, 1, 4 ),
 ( -0.1039370721279000015, 1.103937072127999963 ),
 ( 0.2233333333344000027, 0.2480800653604999795, 0.2728267973865999840, 0.2975735294126999886, 0.3223202614387999931, 0.3470669934649999733, 0.3718137254910999778, 0.3965604575171999824, 0.4213071895433000424, 0.4460539215694000470, 0.4708006535954999960, 0.4955473856216000006, 0.5202941176476999496, 0.5450408496738000652, 0.5697875816999000698, 0.5945343137260000743, 0.6192810457521999989, 0.6440277777783000035, 0.6687745098044000081, 0.6935212418305000126, 0.7182679738566000172, 0.7430147058827000217, 0.7677614379088000263, 0.7925081699349000308, 0.8172549019609999243, 0.8420016339870999289, 0.8667483660132000445, 0.8914950980394000801, 0.9162418300655000847, 0.9409885620915999782, 0.9657352941176999828, 0.9904820261437999873, 1.015228758169999912 ),
 .UNSPECIFIED. ) ;
#39167 = CARTESIAN_POINT ( 'NONE',  ( 10.94072200990529886, 2.922907051630999842, -7.124286150322599376 ) ) ;
#39168 = CARTESIAN_POINT ( 'NONE',  ( 12.32674677874978642, -0.5406785836137757428, 12.58839662496522749 ) ) ;
#39169 = CARTESIAN_POINT ( 'NONE',  ( 7.443295280410000103, 4.698356649019999942, 8.789431186081998248 ) ) ;
#39170 = CARTESIAN_POINT ( 'NONE',  ( 10.83668832355999889, 4.288537082977999404, 9.448742031664000507 ) ) ;
#39171 = CARTESIAN_POINT ( 'NONE',  ( 12.42261142450839984, 2.994360094170045450, 12.32252841079978189 ) ) ;
#39172 = EDGE_LOOP ( 'NONE', ( #7773, #3938, #24952, #18173 ) ) ;
#39173 = CARTESIAN_POINT ( 'NONE',  ( 9.784179719593000257, 4.042991257420999851, -5.768106221333000327 ) ) ;
#39174 = CARTESIAN_POINT ( 'NONE',  ( 11.15810538575740019, 5.242981041160000188, -7.202822423614300362 ) ) ;
#39175 = DIRECTION ( 'NONE',  ( 0.000000000000000000, 0.9466492601157000530, -0.3222656952305000266 ) ) ;
#39177 = CARTESIAN_POINT ( 'NONE',  ( 18.03457482790186361, -0.4008908244505982599, 12.69148415474440661 ) ) ;
#39176 = CARTESIAN_POINT ( 'NONE',  ( 7.790629440376999781, -3.416208448044999901, 6.162501393933999871 ) ) ;
#39178 = CARTESIAN_POINT ( 'NONE',  ( 10.08400081823899974, -4.888721525563999748, 7.032008172796599510 ) ) ;
#39179 = CARTESIAN_POINT ( 'NONE',  ( 10.38287885159599888, -3.139900861731399928, -7.397393329751199786 ) ) ;
#39180 = EDGE_LOOP ( 'NONE', ( #4048, #56009, #11099, #15829 ) ) ;
#39181 = CARTESIAN_POINT ( 'NONE',  ( 1.262565185690999847, 3.233448155534000001, 0.4075532224664999981 ) ) ;
#39182 = CARTESIAN_POINT ( 'NONE',  ( 24.09352403733791448, -9.221943116806739837, -9.178216524599347892 ) ) ;
#39183 = ADVANCED_FACE ( 'NONE', ( #7821 ), #23209, .T. ) ;
#39184 = CARTESIAN_POINT ( 'NONE',  ( 9.456149159797570647, -5.077028306801780744, 7.790330864865199878 ) ) ;
#39185 = CARTESIAN_POINT ( 'NONE',  ( 17.98398272107413121, -2.954699841461171150, 13.56644208774973137 ) ) ;
#39186 = CARTESIAN_POINT ( 'NONE',  ( 24.70770306036100195, -12.32897093773000030, 2.948671853035999657 ) ) ;
#39187 = EDGE_CURVE ( 'NONE', #42842, #34621, #57003, .T. ) ;
#39188 = CARTESIAN_POINT ( 'NONE',  ( 12.17479962224113166, -2.156383435693121520, 13.83294862407085724 ) ) ;
#39189 = DIRECTION ( 'NONE',  ( 0.000000000000000000, 1.000000000000000000, 0.000000000000000000 ) ) ;
#39190 = DIRECTION ( 'NONE',  ( 0.000000000000000000, 1.000000000000000000, 0.000000000000000000 ) ) ;
#39191 = CARTESIAN_POINT ( 'NONE',  ( 13.46122879894100066, -12.02747180725999954, -2.509215126660999662 ) ) ;
#39192 = EDGE_LOOP ( 'NONE', ( #15498, #25640, #1, #32417, #22369, #40571, #53004, #44726, #68472, #52686, #47892, #60830 ) ) ;
#39193 = AXIS2_PLACEMENT_3D ( 'NONE', #68307, #8568, #19746 ) ;
#39194 = CARTESIAN_POINT ( 'NONE',  ( 7.469166666664250442, 3.646640356114970505, -6.185136886497774711 ) ) ;
#39195 = CARTESIAN_POINT ( 'NONE',  ( 9.536859343794805710, 5.286513823918975952, -7.027110704272522490 ) ) ;
#39196 = CARTESIAN_POINT ( 'NONE',  ( 7.383137037416592996, -2.829917722523448642, 8.817307441672506130 ) ) ;
#39197 = CARTESIAN_POINT ( 'NONE',  ( 12.80505043854146763, -3.248147246781390329, -13.61798588129781074 ) ) ;
#39198 = CARTESIAN_POINT ( 'NONE',  ( 0.9422012868096000249, 1.794790469053999971, -3.302590565797000277 ) ) ;
#39199 = ORIENTED_EDGE ( 'NONE', *, *, #66211, .T. ) ;
#39200 = CARTESIAN_POINT ( 'NONE',  ( 10.61503919148293740, 5.349978903665603802, -7.499997722305280945 ) ) ;
#39201 = AXIS2_PLACEMENT_3D ( 'NONE', #29025, #8713, #40866 ) ;
#39202 = CARTESIAN_POINT ( 'NONE',  ( 17.92245882712028759, 1.993980507605455310, -12.55520606452098775 ) ) ;
#39203 = DIRECTION ( 'NONE',  ( 1.000000000000000000, 0.000000000000000000, 0.000000000000000000 ) ) ;
#39204 = CARTESIAN_POINT ( 'NONE',  ( 11.31825954179440075, 4.666231193203100425, 6.946434658287599540 ) ) ;
#39206 = CARTESIAN_POINT ( 'NONE',  ( 11.00000000000000000, 3.031410575668799900, -7.174999999999999822 ) ) ;
#39205 = VECTOR ( 'NONE', #54470, 1000.000000000000000 ) ;
#39207 = CARTESIAN_POINT ( 'NONE',  ( 11.33381694038000020, -2.642393655627000015, -7.577897390831000557 ) ) ;
#39208 = CARTESIAN_POINT ( 'NONE',  ( 4.605026506348999682, -1.500000000000000000, 0.000000000000000000 ) ) ;
#39209 = DIRECTION ( 'NONE',  ( 5.369763710129195918E-06, 0.9999999999350365210, -1.005448450480035185E-05 ) ) ;
#39210 = CARTESIAN_POINT ( 'NONE',  ( 12.20841262064594268, -2.686198882981354785, 12.40625987442081346 ) ) ;
#39211 = ORIENTED_EDGE ( 'NONE', *, *, #59963, .T. ) ;
#39212 = CARTESIAN_POINT ( 'NONE',  ( 8.745860841232000027, 4.178200486578000472, -5.608493638783999202 ) ) ;
#39213 = ORIENTED_EDGE ( 'NONE', *, *, #43025, .F. ) ;
#39214 = CARTESIAN_POINT ( 'NONE',  ( 18.14815926393673706, -2.301857555364728913, 13.71350736626465761 ) ) ;
#39215 = CARTESIAN_POINT ( 'NONE',  ( 10.39503166480599994, -5.274847857784000560, -7.589885038193400213 ) ) ;
#39216 = ORIENTED_EDGE ( 'NONE', *, *, #65999, .F. ) ;
#39217 = CARTESIAN_POINT ( 'NONE',  ( 11.60477869730532774, 3.532552483170099844, 8.421761806503198500 ) ) ;
#39218 = CARTESIAN_POINT ( 'NONE',  ( 6.003027306108891459, 0.6725737735649598426, -0.9715352586480965336 ) ) ;
#39219 = CARTESIAN_POINT ( 'NONE',  ( 17.80000000005199823, -3.345268251980999974, -11.86064071431999878 ) ) ;
#39220 = CARTESIAN_POINT ( 'NONE',  ( 9.566963020987998334, 5.215925787220999865, 6.177726425586999248 ) ) ;
#39221 = CARTESIAN_POINT ( 'NONE',  ( 12.15689047902494835, -2.896806234243965328, -13.69773071446984858 ) ) ;
#39222 = CARTESIAN_POINT ( 'NONE',  ( 9.654346873515669003, -2.749999999999998668, -7.336375382625537789 ) ) ;
#39223 = EDGE_CURVE ( 'NONE', #24634, #509, #63673, .T. ) ;
#39224 = CARTESIAN_POINT ( 'NONE',  ( 11.40156680346000151, 3.471758886279999956, -11.27177987500999912 ) ) ;
#39225 = CARTESIAN_POINT ( 'NONE',  ( 10.38153277269999997, -2.772136814285999673, -8.408084799892998618 ) ) ;
#39226 = CARTESIAN_POINT ( 'NONE',  ( 4.000000000000000000, -1.082895748633089683, -1.878475312369199957 ) ) ;
#39227 = EDGE_CURVE ( 'NONE', #25280, #67407, #53655, .T. ) ;
#39228 = EDGE_CURVE ( 'NONE', #63228, #11689, #66159, .T. ) ;
#39229 = CARTESIAN_POINT ( 'NONE',  ( 23.60000000000000142, 0.000000000000000000, 0.000000000000000000 ) ) ;
#39230 = VERTEX_POINT ( 'NONE', #14450 ) ;
#39231 = CARTESIAN_POINT ( 'NONE',  ( 3.999999855301999752, 2.524999655449999825, 0.000000000000000000 ) ) ;
#39232 = CARTESIAN_POINT ( 'NONE',  ( 10.71434555259480348, 3.092585117345866497, -4.811875879314510662 ) ) ;
#39233 = CARTESIAN_POINT ( 'NONE',  ( 10.57161764893999845, -5.198524786722999558, 4.692090250997000389 ) ) ;
#39234 = B_SPLINE_CURVE_WITH_KNOTS ( 'NONE', 3,
 ( #22130, #28077, #43471, #30157 ),
 .UNSPECIFIED., .F., .F.,
 ( 4, 4 ),
 ( 0.000000000000000000, 1.000000000000000000 ),
 .UNSPECIFIED. ) ;
#39235 = CARTESIAN_POINT ( 'NONE',  ( 4.599999999999999645, -0.7192913403693119712, -12.57945229203838267 ) ) ;
#39236 = CARTESIAN_POINT ( 'NONE',  ( 9.289752973821549631, 3.672827138550766257, 8.717426404466650069 ) ) ;
#39237 = CARTESIAN_POINT ( 'NONE',  ( 12.21194158638444272, 2.301857635319167983, 13.71345735897205209 ) ) ;
#39238 = CARTESIAN_POINT ( 'NONE',  ( 10.76010362286999822, -4.535387425205000156, 6.001717576299999024 ) ) ;
#39239 = ORIENTED_EDGE ( 'NONE', *, *, #22070, .F. ) ;
#39240 = CARTESIAN_POINT ( 'NONE',  ( 7.849513827001898036, 2.927712334411324946, -6.623875161447396742 ) ) ;
#39241 = CARTESIAN_POINT ( 'NONE',  ( 12.54917863858678118, 0.6836428945794205125, 13.98330131869062321 ) ) ;
#39242 = ORIENTED_EDGE ( 'NONE', *, *, #13448, .T. ) ;
#39243 = CARTESIAN_POINT ( 'NONE',  ( 12.78082384918899983, 11.55157311154999888, -4.942237549596000257 ) ) ;
#39244 = CARTESIAN_POINT ( 'NONE',  ( 10.45187389798759270, -5.320777371542467549, 7.955754976780856857 ) ) ;
#39245 = EDGE_CURVE ( 'NONE', #60041, #8802, #49571, .T. ) ;
#39246 = B_SPLINE_CURVE_WITH_KNOTS ( 'NONE', 3,
 ( #48991, #43755, #1792, #7032 ),
 .UNSPECIFIED., .F., .F.,
 ( 4, 4 ),
 ( 0.000000000000000000, 1.000000000000000000 ),
 .UNSPECIFIED. ) ;
#39247 = CARTESIAN_POINT ( 'NONE',  ( 24.15330281760600073, -3.593703394715999977, -12.72474830072999907 ) ) ;
#39248 = CARTESIAN_POINT ( 'NONE',  ( 4.529075847544000055, -1.038563345233000090, 1.255970712535000144 ) ) ;
#39249 = CARTESIAN_POINT ( 'NONE',  ( 8.938854719593997800, 5.597201461420000967, -8.171008079894999554 ) ) ;
#39250 = CARTESIAN_POINT ( 'NONE',  ( 12.80505043854146940, -1.875000000000000000, 13.78631952119025073 ) ) ;
#39251 = CARTESIAN_POINT ( 'NONE',  ( 11.07336076184000007, -2.375557098086999996, -8.393541296344000813 ) ) ;
#39252 = CARTESIAN_POINT ( 'NONE',  ( 6.960892430994999991, -9.225317279141998839, -5.198338520859000056 ) ) ;
#39253 = AXIS2_PLACEMENT_3D ( 'NONE', #32194, #53508, #5598 ) ;
#39254 = CYLINDRICAL_SURFACE ( 'NONE', #12512, 0.5000000000000002220 ) ;
#39255 = CARTESIAN_POINT ( 'NONE',  ( 20.00000000000000000, 0.000000000000000000, 0.000000000000000000 ) ) ;
#39256 = CARTESIAN_POINT ( 'NONE',  ( 9.304144223516997769, -2.772050158355999994, -8.125211791007998841 ) ) ;
#39257 = CARTESIAN_POINT ( 'NONE',  ( 10.87518447801629939, 4.865987311498500389, -7.480906371072489236 ) ) ;
#39258 = CARTESIAN_POINT ( 'NONE',  ( 1.167640132542000275, -1.762666431298160141, 3.058252359239895579 ) ) ;
#39259 = B_SPLINE_CURVE_WITH_KNOTS ( 'NONE', 3,
 ( #44641, #28912, #29249, #28201 ),
 .UNSPECIFIED., .F., .F.,
 ( 4, 4 ),
 ( 0.000000000000000000, 1.000000000000000000 ),
 .UNSPECIFIED. ) ;
#39260 = B_SPLINE_CURVE_WITH_KNOTS ( 'NONE', 3,
 ( #15788, #68225, #20344, #10200, #14765, #67889, #57397, #63323, #3571, #4949, #47613, #58434, #24904, #19665, #62309, #14426, #35743, #57062 ),
 .UNSPECIFIED., .F., .F.,
 ( 4, 2, 2, 2, 2, 2, 2, 2, 4 ),
 ( 0.000000000000000000, 0.1250000000000000555, 0.2500000000000001110, 0.3750000000000001665, 0.5000000000000002220, 0.6250000000000001110, 0.7500000000000001110, 0.8750000000000000000, 1.000000000000000000 ),
 .UNSPECIFIED. ) ;
#39261 = CARTESIAN_POINT ( 'NONE',  ( 10.68546886766499959, 3.433493735705800187, -6.470713638631999665 ) ) ;
#39262 = CARTESIAN_POINT ( 'NONE',  ( 8.849455549952999434, 4.781695603001899997, -6.869290649434700136 ) ) ;
#39264 = CARTESIAN_POINT ( 'NONE',  ( 10.91901409926999911, -2.752141321853000200, 4.977018749245999629 ) ) ;
#39263 = CARTESIAN_POINT ( 'NONE',  ( 10.25431740696899929, -3.838745722419000028, 6.648116790593900483 ) ) ;
#39265 = CARTESIAN_POINT ( 'NONE',  ( 8.221178267935991713, -3.443155653785000769, 6.131664341583003441 ) ) ;
#39266 = VERTEX_POINT ( 'NONE', #15129 ) ;
#39267 = CARTESIAN_POINT ( 'NONE',  ( 10.97635090131019986, 4.999207052587699707, 6.881982988766500497 ) ) ;
#39268 = CARTESIAN_POINT ( 'NONE',  ( 9.034116535116000435, -4.695350938297000454, 8.660677768253002284 ) ) ;
#39269 = CARTESIAN_POINT ( 'NONE',  ( 9.707684229509998985, 3.195116560491999991, 8.309874741421300115 ) ) ;
#39270 = CARTESIAN_POINT ( 'NONE',  ( 10.75851354018298522, -3.836375382625526687, -6.250000000000000888 ) ) ;
#39271 = CARTESIAN_POINT ( 'NONE',  ( 9.166075977534999808, -4.023333687735000552, 9.122281080215000060 ) ) ;
#39272 = ADVANCED_FACE ( 'NONE', ( #67914 ), #41358, .T. ) ;
#39273 = CARTESIAN_POINT ( 'NONE',  ( 12.80000000000000071, -10.78295181803999903, 4.410266442048000002 ) ) ;
#39274 = CARTESIAN_POINT ( 'NONE',  ( 11.82312259374200103, 3.643624473348999970, -12.02372562982000126 ) ) ;
#39275 = ORIENTED_EDGE ( 'NONE', *, *, #63540, .F. ) ;
#39276 = CARTESIAN_POINT ( 'NONE',  ( 9.102747021775998704, -4.754947163618299832, -8.162493079567200382 ) ) ;
#39277 = DIRECTION ( 'NONE',  ( 1.000000000000000000, 0.000000000000000000, 0.000000000000000000 ) ) ;
#39278 = B_SPLINE_CURVE_WITH_KNOTS ( 'NONE', 3,
 ( #8447, #25206, #46543, #19970 ),
 .UNSPECIFIED., .F., .F.,
 ( 4, 4 ),
 ( 0.000000000000000000, 1.000000000000000000 ),
 .UNSPECIFIED. ) ;
#39279 = CARTESIAN_POINT ( 'NONE',  ( 5.447919488923999687, 1.422967556274000067, 0.3628923349178999613 ) ) ;
#39280 = CARTESIAN_POINT ( 'NONE',  ( 9.189494650919995067, -2.900751414380998039, -6.630304163275999585 ) ) ;
#39281 = CARTESIAN_POINT ( 'NONE',  ( 25.39994675527853474, 8.680020655622051606, 7.390263983914236334 ) ) ;
#39282 = B_SPLINE_CURVE_WITH_KNOTS ( 'NONE', 3,
 ( #42280, #19915, #56972, #62551, #25502, #20254, #26195, #4503, #62215, #41923 ),
 .UNSPECIFIED., .F., .F.,
 ( 4, 2, 2, 2, 4 ),
 ( 0.1253970409990855239, 0.3126921946255971640, 0.4999873482521087764, 0.6872825018786201667, 0.8745776555051315571 ),
 .UNSPECIFIED. ) ;
#39283 = CARTESIAN_POINT ( 'NONE',  ( 11.62133729122639991, -4.865898216891100247, 7.522778681411049995 ) ) ;
#39284 = CARTESIAN_POINT ( 'NONE',  ( 11.14179841651039915, 3.646693590264900031, -8.439215328713499886 ) ) ;
#39285 = LINE ( 'NONE', #49772, #59950 ) ;
#39286 = CARTESIAN_POINT ( 'NONE',  ( 9.685492310842999331, -4.505165106450999879, -8.732017808253001334 ) ) ;
#39287 = LINE ( 'NONE', #64447, #17038 ) ;
#39288 = ORIENTED_EDGE ( 'NONE', *, *, #35325, .F. ) ;
#39289 = LINE ( 'NONE', #12721, #3118 ) ;
#39290 = CARTESIAN_POINT ( 'NONE',  ( 12.52839348839893141, 0.5608030988280865436, -13.88477341743901050 ) ) ;
#39291 = CARTESIAN_POINT ( 'NONE',  ( 13.73869549901200315, -8.889050979574999900, -7.612322772148999661 ) ) ;
#39292 = CARTESIAN_POINT ( 'NONE',  ( 11.41486084871699802, 2.792989229543000107, -7.825000000000000178 ) ) ;
#39293 = CARTESIAN_POINT ( 'NONE',  ( 13.66714157633443705, -11.44713007569920471, -2.165075719400535892 ) ) ;
#39294 = CARTESIAN_POINT ( 'NONE',  ( 7.000000000000000888, 8.702830230118003385, 4.583331007515480060 ) ) ;
#39295 = CARTESIAN_POINT ( 'NONE',  ( 5.630600923344116993, 12.10404814139731222, -3.742416328825069360 ) ) ;
#39296 = ORIENTED_EDGE ( 'NONE', *, *, #29958, .T. ) ;
#39297 = CONICAL_SURFACE ( 'NONE', #23673, 12.72499970924999957, 0.7853981386146715593 ) ;
#39298 = CARTESIAN_POINT ( 'NONE',  ( 18.16667230414093126, 2.370970514942110974, -13.69998174157045412 ) ) ;
#39299 = ORIENTED_EDGE ( 'NONE', *, *, #35531, .F. ) ;
#39300 = CARTESIAN_POINT ( 'NONE',  ( 1.284778341492999868E-07, 0.000000000000000000, 0.000000000000000000 ) ) ;
#39301 = CARTESIAN_POINT ( 'NONE',  ( 8.353308059623998361, -2.800111029801999774, 9.079936276749000612 ) ) ;
#39302 = CARTESIAN_POINT ( 'NONE',  ( 9.260829719593999698, 4.861259245430999520, -8.806664389576001284 ) ) ;
#39303 = CARTESIAN_POINT ( 'NONE',  ( 23.89493773356269202, -12.87862618918174817, 3.583998245011372319 ) ) ;
#39304 = CARTESIAN_POINT ( 'NONE',  ( 11.34523293495530005, -5.315205473512000012, -7.447129085684729866 ) ) ;
#39305 = CARTESIAN_POINT ( 'NONE',  ( 18.00675905371507923, 0.4321659195651227359, -12.69010673282157597 ) ) ;
#39306 = FACE_OUTER_BOUND ( 'NONE', #43338, .T. ) ;
#39307 = EDGE_LOOP ( 'NONE', ( #62467, #67116, #57718 ) ) ;
#39308 = CARTESIAN_POINT ( 'NONE',  ( 10.75110221171000013, -2.822135527917999820, 6.655890318096999714 ) ) ;
#39309 = EDGE_CURVE ( 'NONE', #7194, #61329, #18094, .T. ) ;
#39310 = EDGE_CURVE ( 'NONE', #60101, #67640, #67565, .T. ) ;
#39311 = CARTESIAN_POINT ( 'NONE',  ( 17.96842299892580996, -2.968890910988948750, -13.56270300416616692 ) ) ;
#39312 = CARTESIAN_POINT ( 'NONE',  ( 9.925639158771000226, 4.357364160690000432, -9.282962013144999247 ) ) ;
#39313 = ORIENTED_EDGE ( 'NONE', *, *, #49391, .T. ) ;
#39314 = AXIS2_PLACEMENT_3D ( 'NONE', #16107, #48266, #47593 ) ;
#39315 = CARTESIAN_POINT ( 'NONE',  ( 10.17309652395999997, 4.709165316578000748, -8.664874001714000684 ) ) ;
#39316 = ORIENTED_EDGE ( 'NONE', *, *, #40833, .T. ) ;
#39317 = CARTESIAN_POINT ( 'NONE',  ( 8.925442991499998868, 3.936771438983030169, 8.502419298200999620 ) ) ;
#39318 = CARTESIAN_POINT ( 'NONE',  ( 18.17657007421214743, -2.109712673715142373, -12.42212297180517133 ) ) ;
#39319 = VECTOR ( 'NONE', #6214, 1000.000000000000000 ) ;
#39320 = CARTESIAN_POINT ( 'NONE',  ( 24.44496483130000186, -3.224879855413000040, 12.03535978074999946 ) ) ;
#39321 = DIRECTION ( 'NONE',  ( 1.000000000000000000, 0.000000000000000000, 0.000000000000000000 ) ) ;
#39322 = CARTESIAN_POINT ( 'NONE',  ( 11.82333928233100018, -11.49420271256999904, -1.652349626741000055 ) ) ;
#39323 = CARTESIAN_POINT ( 'NONE',  ( 9.307392757686999474, 4.585219941293200208, 6.860292594369099106 ) ) ;
#39324 = FACE_OUTER_BOUND ( 'NONE', #50656, .T. ) ;
#39325 = ORIENTED_EDGE ( 'NONE', *, *, #33395, .F. ) ;
#39326 = CYLINDRICAL_SURFACE ( 'NONE', #40351, 0.6999999999999992895 ) ;
#39327 = CARTESIAN_POINT ( 'NONE',  ( 11.09178278040999999, 4.578541652803000517, -8.908598806528001290 ) ) ;
#39328 = EDGE_CURVE ( 'NONE', #39916, #66715, #16990, .T. ) ;
#39329 = CARTESIAN_POINT ( 'NONE',  ( 10.97053692116999990, -5.147214819045999867, -5.024239345603000118 ) ) ;
#39330 = CARTESIAN_POINT ( 'NONE',  ( 12.26319456176230105, 2.811641923064096549, -13.60240885908115160 ) ) ;
#39331 = CARTESIAN_POINT ( 'NONE',  ( 10.54555864497999984, -2.992894514506000192, -8.288745882156399958 ) ) ;
#39332 = EDGE_CURVE ( 'NONE', #24493, #34006, #44034, .T. ) ;
#39333 = CARTESIAN_POINT ( 'NONE',  ( 11.20904026220999938, -5.937811873294999820, 7.147336919140999001 ) ) ;
#39334 = CARTESIAN_POINT ( 'NONE',  ( 17.74345116425200075, -0.7055305429986051813, 13.98221279804358197 ) ) ;
#39335 = CARTESIAN_POINT ( 'NONE',  ( 7.717562990494335473, -2.846244519028975795, 6.797277674502598011 ) ) ;
#39336 = EDGE_LOOP ( 'NONE', ( #29034, #9112, #59869, #7223 ) ) ;
#39337 = ORIENTED_EDGE ( 'NONE', *, *, #17526, .T. ) ;
#39338 = CARTESIAN_POINT ( 'NONE',  ( 9.295789158775001226, 5.835196551504000517, -7.008466539623000813 ) ) ;
#39339 = CARTESIAN_POINT ( 'NONE',  ( 12.40292999696741028, -0.4784640315611758399, 13.88891505533309711 ) ) ;
#39340 = CARTESIAN_POINT ( 'NONE',  ( 10.56498513754060653, -5.349957030113857925, -7.500000808964294663 ) ) ;
#39341 = CARTESIAN_POINT ( 'NONE',  ( 23.57797122970793069, 3.138867034835534753, -13.63060662545491830 ) ) ;
#39342 = CARTESIAN_POINT ( 'NONE',  ( 8.641808059624999316, -2.933824946949000090, 8.496487880080000110 ) ) ;
#39343 = CARTESIAN_POINT ( 'NONE',  ( 11.50000000000000000, -4.968589424331200100, 7.825000000000000178 ) ) ;
#39346 = B_SPLINE_CURVE_WITH_KNOTS ( 'NONE', 3,
 ( #1632, #55464, #945, #7221 ),
 .UNSPECIFIED., .F., .F.,
 ( 4, 4 ),
 ( 0.000000000000000000, 1.000000000000000000 ),
 .UNSPECIFIED. ) ;
#39345 = CARTESIAN_POINT ( 'NONE',  ( 10.96507314189000049, -6.669294869020999883, 5.364414917161000496 ) ) ;
#39344 = CARTESIAN_POINT ( 'NONE',  ( 10.41232996542199984, -4.888489908445900589, 6.579690231462300254 ) ) ;
#39347 = CARTESIAN_POINT ( 'NONE',  ( 10.69041504065829962, 5.024558373595999328, -6.736065107693399945 ) ) ;
#39348 = ORIENTED_EDGE ( 'NONE', *, *, #5481, .F. ) ;
#39349 = AXIS2_PLACEMENT_3D ( 'NONE', #14893, #3111, #37247 ) ;
#39350 = CARTESIAN_POINT ( 'NONE',  ( 7.398321641533604165, 3.320456282957297223, -6.320831307949290157 ) ) ;
#39351 = CARTESIAN_POINT ( 'NONE',  ( 8.791809814040998816, 4.530359890157599878, -8.185876144228299012 ) ) ;
#39352 = CARTESIAN_POINT ( 'NONE',  ( 17.59627748481874576, 0.6237239846186465320, 12.67937377942300614 ) ) ;
#39353 = DIRECTION ( 'NONE',  ( 0.000000000000000000, 0.000000000000000000, -1.000000000000000000 ) ) ;
#39354 = CARTESIAN_POINT ( 'NONE',  ( 17.86986266959569036, -3.040316756274647148, -12.30911383021075700 ) ) ;
#39355 = ORIENTED_EDGE ( 'NONE', *, *, #21267, .F. ) ;
#39357 = DIRECTION ( 'NONE',  ( 1.000000000000000000, -3.552713678852000294E-14, -5.329070518279000085E-14 ) ) ;
#39356 = CARTESIAN_POINT ( 'NONE',  ( 11.29998658800000122, 3.824194713071000340, -11.71675648045999907 ) ) ;
#39358 = CARTESIAN_POINT ( 'NONE',  ( 8.233179719589999834, 5.203550244299999683, -8.391678825488000371 ) ) ;
#39359 = CYLINDRICAL_SURFACE ( 'NONE', #2969, 1.350000000000000533 ) ;
#39360 = CARTESIAN_POINT ( 'NONE',  ( 8.046447522772005811, -5.096470895078004659, 6.454903582004997808 ) ) ;
#39361 = AXIS2_PLACEMENT_3D ( 'NONE', #12837, #66305, #6887 ) ;
#39362 = DIRECTION ( 'NONE',  ( 1.000000000000000000, 0.000000000000000000, 0.000000000000000000 ) ) ;
#39363 = CARTESIAN_POINT ( 'NONE',  ( 5.500000000000000000, -0.2500000000000000000, -3.149999999999999911 ) ) ;
#39364 = CARTESIAN_POINT ( 'NONE',  ( 2.404564854619000158, -3.223169239229000116, -1.585884214500000056 ) ) ;
#39365 = PRODUCT_DEFINITION ( 'UNKNOWN', '', #63066, #20607 ) ;
#39366 = ORIENTED_EDGE ( 'NONE', *, *, #65837, .T. ) ;
#39367 = CARTESIAN_POINT ( 'NONE',  ( 12.09164653790447552, 0.1286734328892400470, -12.59934825840596773 ) ) ;
#39368 = DIRECTION ( 'NONE',  ( 0.000000000000000000, 0.000000000000000000, -1.000000000000000000 ) ) ;
#39369 = CYLINDRICAL_SURFACE ( 'NONE', #48776, 0.6999999999999992895 ) ;
#39370 = CARTESIAN_POINT ( 'NONE',  ( 8.502045280412000139, 3.869396554003000421, 5.695652484872999466 ) ) ;
#39371 = EDGE_LOOP ( 'NONE', ( #56110, #69037, #9281, #28334 ) ) ;
#39372 = CARTESIAN_POINT ( 'NONE',  ( 5.365365123072000308, -0.1429527940584000290, 1.396516134632999950 ) ) ;
#39373 = CARTESIAN_POINT ( 'NONE',  ( 7.739210841226999982, 3.554387346680000004, -8.824570035521999145 ) ) ;
#39374 = B_SPLINE_CURVE_WITH_KNOTS ( 'NONE', 3,
 ( #61677, #66917, #29192, #51867, #35463, #25302, #30220, #2604, #24961, #23932 ),
 .UNSPECIFIED., .F., .F.,
 ( 4, 2, 2, 2, 4 ),
 ( 0.000000000000000000, 0.2499999999999995559, 0.4999999999999991118, 0.7499999999999995559, 1.000000000000000000 ),
 .UNSPECIFIED. ) ;
#39376 = CARTESIAN_POINT ( 'NONE',  ( 10.74207053302655446, 3.170338597610619757, -8.579608023176378495 ) ) ;
#39375 = CARTESIAN_POINT ( 'NONE',  ( 9.160535748954998780, 2.900115872948000106, -6.152093930328999427 ) ) ;
#39377 = CARTESIAN_POINT ( 'NONE',  ( 11.83003632436370012, 2.756744593645999775, -7.209663534847899236 ) ) ;
#39378 = ORIENTED_EDGE ( 'NONE', *, *, #67301, .T. ) ;
#39379 = FACE_OUTER_BOUND ( 'NONE', #11795, .T. ) ;
#39380 = VERTEX_POINT ( 'NONE', #6612 ) ;
#39381 = CARTESIAN_POINT ( 'NONE',  ( 9.468462140533970839, -5.148144707188508029, 8.212636205154785429 ) ) ;
#39382 = CARTESIAN_POINT ( 'NONE',  ( 24.39664881864633372, 12.09373461225363577, -3.240506422828615118 ) ) ;
#39383 = CARTESIAN_POINT ( 'NONE',  ( 17.83170738868395233, -0.5608030988280895413, -13.88477341743901050 ) ) ;
#39384 = ORIENTED_EDGE ( 'NONE', *, *, #22474, .T. ) ;
#39385 = CARTESIAN_POINT ( 'NONE',  ( 10.93606915609024810, 9.383178346453151519, -6.183004993341985056 ) ) ;
#39386 = CARTESIAN_POINT ( 'NONE',  ( 8.883148997460001084, -5.167567567567999731, 6.822293592207000934 ) ) ;
#39387 = CARTESIAN_POINT ( 'NONE',  ( 8.137489158770998543, 5.171553746019000641, -8.261796965435999951 ) ) ;
#39388 = CARTESIAN_POINT ( 'NONE',  ( 8.455992358812000731, -5.100000000000000533, 6.571291218949999902 ) ) ;
#39389 = CARTESIAN_POINT ( 'NONE',  ( 18.17514718079836200, -2.578773340686874693, 12.43289648649885670 ) ) ;
#39390 = ORIENTED_EDGE ( 'NONE', *, *, #39805, .F. ) ;
#39391 = CARTESIAN_POINT ( 'NONE',  ( 24.45617574064404209, 8.883483999841056189, 9.170518729239159228 ) ) ;
#39392 = EDGE_CURVE ( 'NONE', #24287, #50813, #63696, .T. ) ;
#39394 = ADVANCED_FACE ( 'NONE', ( #5318 ), #64981, .T. ) ;
#39393 = B_SPLINE_CURVE_WITH_KNOTS ( 'NONE', 3,
 ( #30295, #15580, #41121, #9633, #14554, #35872, #30630, #51599, #51940, #4038, #25376, #57882, #9983, #4727, #46713, #52631, #68356, #68016, #20134, #41462, #25721, #26071 ),
 .UNSPECIFIED., .F., .F.,
 ( 4, 2, 2, 2, 2, 2, 2, 2, 2, 2, 4 ),
 ( 0.000000000000000000, 0.1249999999999995559, 0.2499999999999991118, 0.3124999999999991673, 0.3749999999999992228, 0.4999999999999993339, 0.6249999999999994449, 0.7499999999999995559, 0.8124999999999996669, 0.8749999999999997780, 1.000000000000000000 ),
 .UNSPECIFIED. ) ;
#39395 = B_SPLINE_CURVE_WITH_KNOTS ( 'NONE', 3,
 ( #68965, #57784, #31235, #52542, #47307, #68612, #20731 ),
 .UNSPECIFIED., .F., .F.,
 ( 4, 1, 1, 1, 4 ),
 ( 0.000000000000000000, 0.2500000590475000006, 0.5000000002693999468, 0.7499999414914000351, 1.000000000000000000 ),
 .UNSPECIFIED. ) ;
#39396 = CARTESIAN_POINT ( 'NONE',  ( 23.62018009300800259, -13.19635161574000115, -4.176881764676999786 ) ) ;
#39397 = CARTESIAN_POINT ( 'NONE',  ( 10.99691776498582207, 5.205777403464205477, 6.655421476746652409 ) ) ;
#39398 = VECTOR ( 'NONE', #5805, 1000.000000000000227 ) ;
#39399 = CARTESIAN_POINT ( 'NONE',  ( 12.07940096941462471, -2.330761819134298918, 13.80597083266311564 ) ) ;
#39400 = ORIENTED_EDGE ( 'NONE', *, *, #37888, .T. ) ;
#39401 = CARTESIAN_POINT ( 'NONE',  ( 25.29995873461299993, 11.13046969959000165, 3.427501705020000067 ) ) ;
#39402 = CARTESIAN_POINT ( 'NONE',  ( 0.3738300074506999970, -3.373808768376999723, -1.182108054635000026E-09 ) ) ;
#39403 = LINE ( 'NONE', #23659, #66155 ) ;
#39404 = CARTESIAN_POINT ( 'NONE',  ( 10.08521345716899908, -3.075109701058799772, -8.340879262988799780 ) ) ;
#39405 = CARTESIAN_POINT ( 'NONE',  ( 5.500000000000000000, -1.315736040608999957, -10.71955403322999878 ) ) ;
#39406 = CARTESIAN_POINT ( 'NONE',  ( 1.700000000000000178, 0.000000000000000000, 0.000000000000000000 ) ) ;
#39407 = CARTESIAN_POINT ( 'NONE',  ( 17.63949335857240186, -1.765638956106267310, 12.47567715783345221 ) ) ;
#39408 = ORIENTED_EDGE ( 'NONE', *, *, #53264, .T. ) ;
#39409 = CARTESIAN_POINT ( 'NONE',  ( 11.19434208742519843, -4.478858766422799675, -8.252717006421999457 ) ) ;
#39410 = VERTEX_POINT ( 'NONE', #4625 ) ;
#39411 = AXIS2_PLACEMENT_3D ( 'NONE', #30615, #40757, #68342 ) ;
#39412 = CARTESIAN_POINT ( 'NONE',  ( 25.29995823066400362, -11.13046982544999963, 3.427501264366999756 ) ) ;
#39413 = CARTESIAN_POINT ( 'NONE',  ( 9.734454719592999794, 3.021734963141999852, -6.070209284876999511 ) ) ;
#39414 = CARTESIAN_POINT ( 'NONE',  ( 2.747903870626000167, 3.209484249071000050, -0.1891215843542000119 ) ) ;
#39415 = ADVANCED_FACE ( 'NONE', ( #31903 ), #1033, .F. ) ;
#39416 = CARTESIAN_POINT ( 'NONE',  ( 10.89218817467000200, -2.661900611977999986, -8.236035141896001832 ) ) ;
#39417 = DIRECTION ( 'NONE',  ( 0.000000000000000000, -0.1333333333333049098, 0.9910712498212373989 ) ) ;
#39418 = FACE_OUTER_BOUND ( 'NONE', #25013, .T. ) ;
#39420 = CARTESIAN_POINT ( 'NONE',  ( 10.59393020684899867, 5.250000000000000000, -7.500000000000000000 ) ) ;
#39419 = B_SPLINE_CURVE_WITH_KNOTS ( 'NONE', 3,
 ( #11379, #17324, #49136, #39005 ),
 .UNSPECIFIED., .F., .F.,
 ( 4, 4 ),
 ( 0.000000000000000000, 1.000000000000000000 ),
 .UNSPECIFIED. ) ;
#39421 = ORIENTED_EDGE ( 'NONE', *, *, #62643, .F. ) ;
#39422 = CYLINDRICAL_SURFACE ( 'NONE', #60359, 0.5000000000000002220 ) ;
#39423 = CARTESIAN_POINT ( 'NONE',  ( 11.96179707368349909, -4.498457171163099844, 8.370914060838998694 ) ) ;
#39424 = CARTESIAN_POINT ( 'NONE',  ( 8.404999999999999361, 5.190914425723000214, -8.768195054477999406 ) ) ;
#39425 = CARTESIAN_POINT ( 'NONE',  ( 25.34480935285659697, -2.689020825566641459, 11.33835534259811695 ) ) ;
#39426 = CARTESIAN_POINT ( 'NONE',  ( 10.34393020684899867, 2.750000000000000000, -7.500000000000000000 ) ) ;
#39427 = CARTESIAN_POINT ( 'NONE',  ( 11.09166666666771839, 2.528771982359670822, 6.972956482935108724 ) ) ;
#39428 = CARTESIAN_POINT ( 'NONE',  ( 11.07210672858429845, 3.307795442047700263, -6.979277962544199632 ) ) ;
#39429 = CARTESIAN_POINT ( 'NONE',  ( 7.100000000000000533, 5.326087788487999575, -7.247035225330000330 ) ) ;
#39430 = CARTESIAN_POINT ( 'NONE',  ( 9.454392757686999715, 4.770706668257700400, -8.342464052342599246 ) ) ;
#39431 = CARTESIAN_POINT ( 'NONE',  ( 24.32733123024100053, -9.023571280490999769, 9.340699019152999938 ) ) ;
#39432 = CARTESIAN_POINT ( 'NONE',  ( 0.8233524344999001432, -2.161873583226317397, -2.781123199319127437 ) ) ;
#39433 = CARTESIAN_POINT ( 'NONE',  ( 10.76588584123000025, 3.166544027818999574, -8.574484964885998650 ) ) ;
#39434 = ORIENTED_EDGE ( 'NONE', *, *, #34880, .F. ) ;
#39435 = CARTESIAN_POINT ( 'NONE',  ( 8.245293146793999384, -4.282999948634999221, 9.286791354293999490 ) ) ;
#39436 = AXIS2_PLACEMENT_3D ( 'NONE', #40589, #56331, #51085 ) ;
#39437 = CARTESIAN_POINT ( 'NONE',  ( 18.27992102884630654, 2.544330805874857049, 13.76687901878135456 ) ) ;
#39438 = FACE_OUTER_BOUND ( 'NONE', #14247, .T. ) ;
#39439 = CARTESIAN_POINT ( 'NONE',  ( 10.44426222744799837, -4.986443098259000450, -8.312555471636301263 ) ) ;
#39440 = ORIENTED_EDGE ( 'NONE', *, *, #39142, .F. ) ;
#39441 = B_SPLINE_CURVE_WITH_KNOTS ( 'NONE', 3,
 ( #53308, #59232, #1205, #6091 ),
 .UNSPECIFIED., .F., .F.,
 ( 4, 4 ),
 ( 0.000000000000000000, 1.000000000000000000 ),
 .UNSPECIFIED. ) ;
#39442 = CARTESIAN_POINT ( 'NONE',  ( 12.09999922233642522, -11.66744139996562701, 3.971920075675145156 ) ) ;
#39443 = CARTESIAN_POINT ( 'NONE',  ( 8.192489158772998437, 2.550241116032999855, 7.666973618349000041 ) ) ;
#39445 = CARTESIAN_POINT ( 'NONE',  ( 10.92968717260509948, 3.312350236372100021, 6.377637058250999580 ) ) ;
#39444 = CARTESIAN_POINT ( 'NONE',  ( 8.447510841229000533, 4.933589693325000525, -9.154576215408999573 ) ) ;
#39446 = CARTESIAN_POINT ( 'NONE',  ( 3.999999855301999752, 0.000000000000000000, 0.000000000000000000 ) ) ;
#39447 = ADVANCED_FACE ( 'NONE', ( #15477 ), #50472, .T. ) ;
#39448 = EDGE_LOOP ( 'NONE', ( #35259, #13623, #5148, #28734, #15255, #56996, #12985, #13715 ) ) ;
#39449 = ADVANCED_FACE ( 'NONE', ( #3090 ), #24075, .T. ) ;
#39450 = CARTESIAN_POINT ( 'NONE',  ( 10.52323372634000087, 3.325642821414999784, 5.689987891230000372 ) ) ;
#39451 = CARTESIAN_POINT ( 'NONE',  ( 17.81237950545467896, -3.200707792931491547, -13.62921448194398977 ) ) ;
#39452 = CARTESIAN_POINT ( 'NONE',  ( 10.59610807141099897, 4.052703327804870526, 6.360477084256999980 ) ) ;
#39453 = CARTESIAN_POINT ( 'NONE',  ( 9.332935524889000689, -5.100347267927999972, 8.693464469215999912 ) ) ;
#39454 = CARTESIAN_POINT ( 'NONE',  ( 8.385058059625000837, -4.977917894183000236, 6.416767031887000705 ) ) ;
#39455 = EDGE_LOOP ( 'NONE', ( #26598, #65537, #58643, #27180 ) ) ;
#39456 = CARTESIAN_POINT ( 'NONE',  ( 11.75744248190100016, -3.642994321184000128, 12.02392698342999999 ) ) ;
#39457 = CARTESIAN_POINT ( 'NONE',  ( 1.448890132540874953, 2.798833948393634863, -2.150913519912196925 ) ) ;
#39458 = CARTESIAN_POINT ( 'NONE',  ( 8.083009592828254597, -4.188654535187550820, 5.770339112206491983 ) ) ;
#39459 = AXIS2_PLACEMENT_3D ( 'NONE', #34488, #1357, #29590 ) ;
#39460 = CARTESIAN_POINT ( 'NONE',  ( 11.18051369187999988, -5.340070732632000272, 8.416150632189001612 ) ) ;
#39461 = CARTESIAN_POINT ( 'NONE',  ( 23.55064464012300363, 2.917691328521999861, 13.72936262135999996 ) ) ;
#39462 = CARTESIAN_POINT ( 'NONE',  ( 9.828696787963000503, -3.803923679411099990, 8.624850445389000697 ) ) ;
#39463 = ORIENTED_EDGE ( 'NONE', *, *, #28985, .T. ) ;
#39464 = CARTESIAN_POINT ( 'NONE',  ( 24.77777987740767429, -11.71376540346410344, -3.192706928545757439 ) ) ;
#39465 = CARTESIAN_POINT ( 'NONE',  ( 12.02733460557258915, -3.793662715184400014, 6.238754009183999472 ) ) ;
#39466 = ORIENTED_EDGE ( 'NONE', *, *, #55660, .F. ) ;
#39467 = CARTESIAN_POINT ( 'NONE',  ( 8.969356963619999235, 2.880642974985999860, 7.500000000085178087 ) ) ;
#39468 = AXIS2_PLACEMENT_3D ( 'NONE', #47580, #53507, #15758 ) ;
#39469 = EDGE_LOOP ( 'NONE', ( #46590, #50441, #182, #36728 ) ) ;
#39470 = CARTESIAN_POINT ( 'NONE',  ( 9.401145280412999128, 3.927090956378999742, -9.230892435423001530 ) ) ;
#39471 = CARTESIAN_POINT ( 'NONE',  ( 10.80502344389999791, 2.874741265256000489, -6.817099149379099110 ) ) ;
#39472 = DIRECTION ( 'NONE',  ( 1.000000000000000000, 0.000000000000000000, 0.000000000000000000 ) ) ;
#39473 = CARTESIAN_POINT ( 'NONE',  ( 12.57303446153994031, 1.919568987556538486, -12.56805043247348586 ) ) ;
#39474 = CARTESIAN_POINT ( 'NONE',  ( 11.98225819896750011, -5.120994791668000090, 7.288668995979000087 ) ) ;
#39475 = CARTESIAN_POINT ( 'NONE',  ( 11.94366954483529852, -3.514796851401900124, 8.248643701125299543 ) ) ;
#39476 = EDGE_CURVE ( 'NONE', #49363, #33712, #33740, .T. ) ;
#39477 = ORIENTED_EDGE ( 'NONE', *, *, #52920, .F. ) ;
#39478 = DIRECTION ( 'NONE',  ( 1.000000000000000000, 0.000000000000000000, 0.000000000000000000 ) ) ;
#39479 = ADVANCED_FACE ( 'NONE', ( #45412 ), #39297, .F. ) ;
#39480 = ORIENTED_EDGE ( 'NONE', *, *, #35675, .T. ) ;
#39481 = CARTESIAN_POINT ( 'NONE',  ( 8.443894353209000059, -2.905864338704999827, 8.940687151810998046 ) ) ;
#39482 = CARTESIAN_POINT ( 'NONE',  ( 25.29987261391899978, -8.756202924575998026, 7.455126447192999883 ) ) ;
#39483 = VERTEX_POINT ( 'NONE', #67060 ) ;
#39484 = CARTESIAN_POINT ( 'NONE',  ( 12.17603179862378404, -2.838932078785886048, -12.27602983002082304 ) ) ;
#39485 = CARTESIAN_POINT ( 'NONE',  ( 11.03918313518939875, 3.292400735470800033, 6.605241151424599444 ) ) ;
#39486 = CARTESIAN_POINT ( 'NONE',  ( 10.94847055962000049, -3.841065069379000274, -9.341805385095000247 ) ) ;
#39487 = CARTESIAN_POINT ( 'NONE',  ( 25.59997239626699894, 8.218962773316999204, -8.043525096612999192 ) ) ;
#39488 = CARTESIAN_POINT ( 'NONE',  ( 18.21574065333400227, -11.85428844745999832, 3.556939559956999730 ) ) ;
#39489 = CARTESIAN_POINT ( 'NONE',  ( 11.00000000000000000, 4.991767524623399233, -7.174999999999999822 ) ) ;
#39490 = CARTESIAN_POINT ( 'NONE',  ( 12.18114782263376483, -2.542296328577542841, -13.66436634302259812 ) ) ;
#39491 = CARTESIAN_POINT ( 'NONE',  ( 18.16373151406918041, 0.1422617729927601049, -12.69893308522357422 ) ) ;
#39492 = CARTESIAN_POINT ( 'NONE',  ( 11.19518313518939934, -4.537300658085600347, -8.179416362154199760 ) ) ;
#39493 = CARTESIAN_POINT ( 'NONE',  ( 10.59610807141099897, -3.947296672195129918, -8.639522915742999132 ) ) ;
#39494 = CARTESIAN_POINT ( 'NONE',  ( 8.224926658773000554, 5.629399530851999955, 8.631829656822000985 ) ) ;
#39495 = ORIENTED_EDGE ( 'NONE', *, *, #59648, .F. ) ;
#39496 = VECTOR ( 'NONE', #36674, 1000.000000000000000 ) ;
#39497 = CARTESIAN_POINT ( 'NONE',  ( 12.10941541359317775, -11.07487266634617029, 3.615341447084566173 ) ) ;
#39498 = CARTESIAN_POINT ( 'NONE',  ( 7.474999999999999645, 5.349999999999999645, 7.500000000000000000 ) ) ;
#39499 = CARTESIAN_POINT ( 'NONE',  ( 10.21237770872999917, 4.072568038926999812, -8.861829932786999819 ) ) ;
#39500 = EDGE_CURVE ( 'NONE', #14587, #9931, #61649, .T. ) ;
#39501 = CARTESIAN_POINT ( 'NONE',  ( 18.11779302252796597, 2.227307244339884917, 12.51093773244155472 ) ) ;
#39502 = CARTESIAN_POINT ( 'NONE',  ( 18.38069952315600020, 3.381269036354999979, -12.09968217836000015 ) ) ;
#39503 = CARTESIAN_POINT ( 'NONE',  ( 10.00138108374000012, 3.855364958793999985, 5.709478909302000638 ) ) ;
#39504 = CARTESIAN_POINT ( 'NONE',  ( 11.28192504596561996, 4.908977993420656105, 7.174999814284952926 ) ) ;
#39505 = CARTESIAN_POINT ( 'NONE',  ( 8.727215710425999973, 3.626036035117899736, 6.691239224408199071 ) ) ;
#39506 = EDGE_LOOP ( 'NONE', ( #35984, #62504, #16221, #27862 ) ) ;
#39507 = CARTESIAN_POINT ( 'NONE',  ( 12.78419053748688405, -1.875000590519850574, 12.57545628621517864 ) ) ;
#39508 = CARTESIAN_POINT ( 'NONE',  ( 9.072442991499999110, -4.063228561016970275, -6.497580701799000380 ) ) ;
#39509 = CARTESIAN_POINT ( 'NONE',  ( 24.72544608131600086, -3.605127478668999963, -12.13010612098000074 ) ) ;
#39510 = CARTESIAN_POINT ( 'NONE',  ( 11.09999999999999964, -5.449702618175999547, 5.124965750789000296 ) ) ;
#39511 = AXIS2_PLACEMENT_3D ( 'NONE', #60276, #66199, #7471 ) ;
#39512 = CARTESIAN_POINT ( 'NONE',  ( 10.81764560330029923, 4.349570499512200428, -6.414140625063999401 ) ) ;
#39513 = CARTESIAN_POINT ( 'NONE',  ( 12.22921692136010563, -0.4376617689587176674, 12.59240970319242514 ) ) ;
#39514 = AXIS2_PLACEMENT_3D ( 'NONE', #22787, #54254, #28047 ) ;
#39515 = CARTESIAN_POINT ( 'NONE',  ( 8.406107780410998487, 5.342170561818999630, 8.432311822615000452 ) ) ;
#39516 = CARTESIAN_POINT ( 'NONE',  ( 9.409314688805999083, 2.634692233435000031, 8.920311306029999443 ) ) ;
#39517 = CARTESIAN_POINT ( 'NONE',  ( 12.26133075698773212, 2.191112520879995973, 12.51819442860477771 ) ) ;
#39518 = ORIENTED_EDGE ( 'NONE', *, *, #17034, .F. ) ;
#39519 = CARTESIAN_POINT ( 'NONE',  ( 10.01622971959000097, 4.325866256860000369, -9.125812605905000652 ) ) ;
#39520 = CARTESIAN_POINT ( 'NONE',  ( 10.19810941423799910, 4.946022705791000007, -6.640722727400100389 ) ) ;
#39521 = B_SPLINE_CURVE_WITH_KNOTS ( 'NONE', 3,
 ( #7931, #17737, #13188, #8272 ),
 .UNSPECIFIED., .F., .F.,
 ( 4, 4 ),
 ( 0.000000000000000000, 1.000000000000000000 ),
 .UNSPECIFIED. ) ;
#39522 = CARTESIAN_POINT ( 'NONE',  ( 5.403413393859333169, 0.4964519701263342411, 1.434320509598691507 ) ) ;
#39524 = FACE_OUTER_BOUND ( 'NONE', #17718, .T. ) ;
#39523 = CARTESIAN_POINT ( 'NONE',  ( 8.239941940377999430, -2.735207418315000361, 6.771977475428999860 ) ) ;
#39525 = CARTESIAN_POINT ( 'NONE',  ( 9.300809814040999157, -3.469640109842400122, 6.814123855771700100 ) ) ;
#39526 = CARTESIAN_POINT ( 'NONE',  ( 10.53057053952199951, -4.340412141385700195, -6.703496287302799672 ) ) ;
#39527 = EDGE_LOOP ( 'NONE', ( #48841, #26582, #61177, #23081 ) ) ;
#39528 = B_SPLINE_CURVE_WITH_KNOTS ( 'NONE', 3,
 ( #32038, #11721, #22560, #557 ),
 .UNSPECIFIED., .F., .F.,
 ( 4, 4 ),
 ( 0.000000000000000000, 1.000000000000000000 ),
 .UNSPECIFIED. ) ;
#39529 = CARTESIAN_POINT ( 'NONE',  ( 2.163748887004999677, -2.164574875407999865, -2.655056891479000036 ) ) ;
#39530 = CARTESIAN_POINT ( 'NONE',  ( 9.832537864288001472, -2.899999999999999911, 6.571291218949999902 ) ) ;
#39531 = CARTESIAN_POINT ( 'NONE',  ( 9.442941355974877382, -4.954666522228584391, 8.051224688103600258 ) ) ;
#39532 = DIRECTION ( 'NONE',  ( 0.000000000000000000, -1.000000000000000000, 0.000000000000000000 ) ) ;
#39533 = EDGE_CURVE ( 'NONE', #49185, #16649, #25917, .T. ) ;
#39534 = EDGE_CURVE ( 'NONE', #66560, #24689, #7854, .T. ) ;
#39535 = CARTESIAN_POINT ( 'NONE',  ( 8.710288521113000115, 3.647046440108700160, -8.284550957747498501 ) ) ;
#39536 = CARTESIAN_POINT ( 'NONE',  ( 12.44048633593779840, -3.149516123668035128, 13.64113935299650393 ) ) ;
#39537 = DIRECTION ( 'NONE',  ( 1.000000000000000000, 0.000000000000000000, 0.000000000000000000 ) ) ;
#39538 = CARTESIAN_POINT ( 'NONE',  ( 15.89994436294300151, 8.847904542234999781, 8.580301953175000662 ) ) ;
#39539 = CARTESIAN_POINT ( 'NONE',  ( 13.06531638133300177, -12.22210578456000007, -1.955102404769999858 ) ) ;
#39540 = ORIENTED_EDGE ( 'NONE', *, *, #43735, .F. ) ;
#39541 = EDGE_CURVE ( 'NONE', #7173, #28639, #48706, .T. ) ;
#39542 = CARTESIAN_POINT ( 'NONE',  ( 10.53521345716899837, -3.075109701058799772, -8.340879262988799780 ) ) ;
#39543 = CARTESIAN_POINT ( 'NONE',  ( 10.87376707297999978, 5.064086065370999812, 5.106852026787000121 ) ) ;
#39544 = CARTESIAN_POINT ( 'NONE',  ( 7.423512759997511701, -2.354253581828240627, 8.063754798790684575 ) ) ;
#39545 = CARTESIAN_POINT ( 'NONE',  ( 10.57960558317873279, -4.353252721116731117, 8.851706718789644768 ) ) ;
#39546 = CARTESIAN_POINT ( 'NONE',  ( 0.6084276407238999873, 1.980426728703999828, 3.194707851357999839 ) ) ;
#39547 = EDGE_LOOP ( 'NONE', ( #15065, #22088, #35436, #32949 ) ) ;
#39548 = CARTESIAN_POINT ( 'NONE',  ( 10.69839231854705908, 4.679932939043758289, -8.679767489842406647 ) ) ;
#39549 = CARTESIAN_POINT ( 'NONE',  ( 17.97023714413479567, 2.032719534845758069, -12.54827100236067139 ) ) ;
#39550 = CARTESIAN_POINT ( 'NONE',  ( 10.73931450027999901, 2.763002390638999994, 6.801034082888999244 ) ) ;
#39551 = CARTESIAN_POINT ( 'NONE',  ( 10.38287885159599888, 4.860099138268600072, 7.602606670248799325 ) ) ;
#39552 = CARTESIAN_POINT ( 'NONE',  ( 18.50001572531399674, 1.956586078199225032, 12.40985500087345095 ) ) ;
#39553 = CARTESIAN_POINT ( 'NONE',  ( 10.80374194038000013, -2.766944173105999827, -8.073385940268000383 ) ) ;
#39554 = CARTESIAN_POINT ( 'NONE',  ( 12.80505043854143388, 1.798896937388929640, -12.50938852236267529 ) ) ;
#39555 = CARTESIAN_POINT ( 'NONE',  ( 24.36504260745899941, 12.29008018610999819, 3.201257196435000285 ) ) ;
#39556 = CARTESIAN_POINT ( 'NONE',  ( 12.25778805737674837, -2.802014929519743180, 12.37607946563144878 ) ) ;
#39557 = ORIENTED_EDGE ( 'NONE', *, *, #28904, .T. ) ;
#39558 = CARTESIAN_POINT ( 'NONE',  ( 8.086348386990133363, 4.224401473857131606, 5.771886138180387427 ) ) ;
#39559 = VERTEX_POINT ( 'NONE', #13259 ) ;
#39560 = CARTESIAN_POINT ( 'NONE',  ( 18.25550288558785894, -2.707593611552288060, 13.73570038168180041 ) ) ;
#39561 = CARTESIAN_POINT ( 'NONE',  ( 10.34580110216399973, -5.090698144635000588, -6.833896451085399448 ) ) ;
#39562 = ORIENTED_EDGE ( 'NONE', *, *, #56232, .T. ) ;
#39563 = CARTESIAN_POINT ( 'NONE',  ( 8.968532939428907724, -5.344941310868764006, 7.382699998430346078 ) ) ;
#39564 = CARTESIAN_POINT ( 'NONE',  ( 18.49996808500600309, -0.9036517527673039174, 11.65000000008756054 ) ) ;
#39565 = CARTESIAN_POINT ( 'NONE',  ( 4.149992563291999836, 1.747525841223985354, -1.007210908820209472 ) ) ;
#39567 = CARTESIAN_POINT ( 'NONE',  ( 24.30000000000000071, 3.224868684338999980, 12.03537377768999939 ) ) ;
#39566 = CIRCLE ( 'NONE', #11646, 1.900000000000000577 ) ;
#39568 = CARTESIAN_POINT ( 'NONE',  ( 9.719613305057999142, 5.967773797872000685, 7.406643507784999692 ) ) ;
#39569 = CARTESIAN_POINT ( 'NONE',  ( 10.29094007826000023, 2.903522982536999919, -8.310916170934000036 ) ) ;
#39570 = CARTESIAN_POINT ( 'NONE',  ( 11.10000000001000053, 7.524088986311000760, -6.497786318682999607 ) ) ;
#39571 = CARTESIAN_POINT ( 'NONE',  ( 11.84835150974899953, 3.192438788486000156, -11.44998398973999976 ) ) ;
#39572 = CARTESIAN_POINT ( 'NONE',  ( 10.78636854442000192, -5.666037955714999796, -7.787004779180999314 ) ) ;
#39573 = CARTESIAN_POINT ( 'NONE',  ( 9.934999999999998721, -4.640430492595999823, -9.117542781427999898 ) ) ;
#39574 = CARTESIAN_POINT ( 'NONE',  ( 10.69003253712258505, -2.945770442954086299, -5.060380188079816044 ) ) ;
#39575 = ORIENTED_EDGE ( 'NONE', *, *, #50328, .F. ) ;
#39576 = CARTESIAN_POINT ( 'NONE',  ( 8.824071121570657539, 4.974071175014780799, -7.248446557932072487 ) ) ;
#39577 = CARTESIAN_POINT ( 'NONE',  ( 11.14975833414749928, -4.796537143354000499, -7.825000000000000178 ) ) ;
#39578 =( LENGTH_UNIT ( ) NAMED_UNIT ( * ) SI_UNIT ( .MILLI., .METRE. ) );
#39579 = ADVANCED_FACE ( 'NONE', ( #49957 ), #59636, .F. ) ;
#39580 = CARTESIAN_POINT ( 'NONE',  ( 11.04422294928000170, 7.351868426856999150, 6.139941188252000082 ) ) ;
#39581 = CARTESIAN_POINT ( 'NONE',  ( 9.279336721442295044, 3.836368765436817263, 8.749993199158911494 ) ) ;
#39582 = CARTESIAN_POINT ( 'NONE',  ( 12.18760440664038391, 2.401006893892606353, 13.69392356709390945 ) ) ;
#39583 = CARTESIAN_POINT ( 'NONE',  ( 9.924739995124999936, -5.060461104229999840, 8.686133300732999274 ) ) ;
#39584 = ORIENTED_EDGE ( 'NONE', *, *, #19365, .T. ) ;
#39585 = EDGE_CURVE ( 'NONE', #58094, #36031, #5360, .T. ) ;
#39586 = CARTESIAN_POINT ( 'NONE',  ( 6.799999999999999822, -9.295462635088998837, -5.399710584805999858 ) ) ;
#39587 = CARTESIAN_POINT ( 'NONE',  ( 12.61399518047280210, -0.5951713840684291768, 13.88284414672552991 ) ) ;
#39588 = ORIENTED_EDGE ( 'NONE', *, *, #65735, .F. ) ;
#39589 = CARTESIAN_POINT ( 'NONE',  ( 23.73952401786024780, 13.33635412649179308, -3.648243621897288236 ) ) ;
#39590 = LINE ( 'NONE', #60913, #48538 ) ;
#39591 = CARTESIAN_POINT ( 'NONE',  ( 8.897621218489625505, 4.818672874536578554, 7.808718305523518310 ) ) ;
#39592 = CARTESIAN_POINT ( 'NONE',  ( 8.513406929461279304, 3.194994825692138996, 5.997290436226018429 ) ) ;
#39593 = CIRCLE ( 'NONE', #35155, 1.350000000000000533 ) ;
#39594 = B_SPLINE_SURFACE_WITH_KNOTS ( 'NONE', 3, 3, ( 
 ( #44556, #12025, #60270, #12724 ),
 ( #50816, #33361, #2911, #6774 ),
 ( #49423, #34742, #56053, #49778 ),
 ( #1536, #22854, #23206, #65848 ),
 ( #17972, #39291, #46607, #52181 ),
 ( #36104, #45910, #61641, #35428 ),
 ( #62998, #14448, #57764, #52525 ),
 ( #30522, #29855, #62665, #67222 ),
 ( #47289, #4282, #51836, #14785 ) ),
 .UNSPECIFIED., .F., .F., .F.,
 ( 4, 1, 1, 1, 1, 1, 4 ),
 ( 4, 4 ),
 ( 0.02209653170519000273, 0.1666666666667000196, 0.3333333333333000081, 0.5000000000000000000, 0.6666666666667000474, 0.8333333333333000637, 0.9492823795161999811 ),
 ( -0.1916656884162999952, 1.191851428473000185 ),
 .UNSPECIFIED. ) ;
#39595 = CARTESIAN_POINT ( 'NONE',  ( 9.386379719595000282, 5.673443217382001080, -7.051790060464000476 ) ) ;
#39596 = CARTESIAN_POINT ( 'NONE',  ( 10.05226354018249779, 5.092232985442822546, -8.129523725463625894 ) ) ;
#39597 = CARTESIAN_POINT ( 'NONE',  ( 11.12455582848000013, 7.801067643070999758, -6.682512661172999913 ) ) ;
#39598 = LINE ( 'NONE', #7430, #16415 ) ;
#39599 = DIRECTION ( 'NONE',  ( 0.000000000000000000, -0.8648648648648720183, 0.5020047465136825426 ) ) ;
#39600 = FACE_OUTER_BOUND ( 'NONE', #43512, .T. ) ;
#39601 = CARTESIAN_POINT ( 'NONE',  ( 9.348145925901000908, -2.626678530444999993, -7.387134320497999340 ) ) ;
#39602 = CARTESIAN_POINT ( 'NONE',  ( 10.38287885159599888, 4.860099138268600072, -7.397393329751199786 ) ) ;
#39603 = CARTESIAN_POINT ( 'NONE',  ( 1.209306799208499816, -3.058252359239909790, 1.762666431298136382 ) ) ;
#39604 = CARTESIAN_POINT ( 'NONE',  ( 10.44635971519499940, 4.459622816450200311, -6.735384833238199143 ) ) ;
#39605 = CARTESIAN_POINT ( 'NONE',  ( 10.03791290906799993, 3.277531639390499851, -8.384179803770500428 ) ) ;
#39607 = CARTESIAN_POINT ( 'NONE',  ( 25.44994642811700203, 0.000000000000000000, -11.34994642770978501 ) ) ;
#39606 = CARTESIAN_POINT ( 'NONE',  ( 9.224265421554999733, -4.162714371335800578, 6.658304367510099908 ) ) ;
#39608 = AXIS2_PLACEMENT_3D ( 'NONE', #40966, #19292, #25225 ) ;
#39609 = CARTESIAN_POINT ( 'NONE',  ( 10.94076550314999885, -5.140765503144999471, -6.571291218949999902 ) ) ;
#39610 = ORIENTED_EDGE ( 'NONE', *, *, #61399, .T. ) ;
#39611 = CARTESIAN_POINT ( 'NONE',  ( 11.35034208742529849, 3.369365911179700301, 6.508707709313799050 ) ) ;
#39612 = VECTOR ( 'NONE', #67226, 1000.000000000000114 ) ;
#39613 = CARTESIAN_POINT ( 'NONE',  ( 10.06343867337000120, -5.156226070197000411, 6.125223053176999777 ) ) ;
#39614 = CARTESIAN_POINT ( 'NONE',  ( 9.958963142879998287, 4.982812171771600518, 7.707177545471399327 ) ) ;
#39615 = DIRECTION ( 'NONE',  ( 0.000000000000000000, -0.6884191022827257367, -0.7253131321107084695 ) ) ;
#39616 = EDGE_CURVE ( 'NONE', #54068, #13653, #49366, .T. ) ;
#39617 = B_SPLINE_CURVE_WITH_KNOTS ( 'NONE', 3,
 ( #52149, #53538, #20004, #42701 ),
 .UNSPECIFIED., .F., .F.,
 ( 4, 4 ),
 ( 0.000000000000000000, 1.000000000000000000 ),
 .UNSPECIFIED. ) ;
#39618 = CARTESIAN_POINT ( 'NONE',  ( 9.137549407199999862, -2.995696424181999884, 8.544763501938000161 ) ) ;
#39619 = CARTESIAN_POINT ( 'NONE',  ( 12.52739587005665101, 3.060316261552512795, 13.53846823646895103 ) ) ;
#39620 = ORIENTED_EDGE ( 'NONE', *, *, #17175, .T. ) ;
#39621 = EDGE_CURVE ( 'NONE', #21925, #13467, #17886, .T. ) ;
#39622 = EDGE_CURVE ( 'NONE', #11254, #11902, #39740, .T. ) ;
#39623 = APPLICATION_CONTEXT ( 'automotive_design' ) ;
#39624 = AXIS2_PLACEMENT_3D ( 'NONE', #44208, #28467, #43508 ) ;
#39625 = CARTESIAN_POINT ( 'NONE',  ( 8.720797255587999786, -2.859210004667000149, -7.451702546394010085 ) ) ;
#39626 = CARTESIAN_POINT ( 'NONE',  ( 9.677263540183330903, -3.370476274536371442, -6.407767014557179230 ) ) ;
#39627 = CARTESIAN_POINT ( 'NONE',  ( 6.528493422235999155, -1.019889730527999916, 1.251756626546000062 ) ) ;
#39628 = CARTESIAN_POINT ( 'NONE',  ( 8.393806199904998877, -2.909809943507001950, -6.638007308765000225 ) ) ;
#39629 = DIRECTION ( 'NONE',  ( -0.9709491189737906591, -0.2392860387987982285, 0.000000000000000000 ) ) ;
#39630 = CARTESIAN_POINT ( 'NONE',  ( 11.58487348028854846, 3.117292544139400157, -7.977261354519500358 ) ) ;
#39631 = CARTESIAN_POINT ( 'NONE',  ( 12.80505043854143388, 1.875000000000000000, -13.78631952119025428 ) ) ;
#39632 = CARTESIAN_POINT ( 'NONE',  ( 9.101385834542000453, -4.783349162191000481, -6.231236652334000148 ) ) ;
#39633 = CARTESIAN_POINT ( 'NONE',  ( 10.52052890781999928, 2.899999999999999911, 6.152188490330000370 ) ) ;
#39634 = ORIENTED_EDGE ( 'NONE', *, *, #577, .T. ) ;
#39635 = FACE_OUTER_BOUND ( 'NONE', #45745, .T. ) ;
#39636 = CARTESIAN_POINT ( 'NONE',  ( 12.70318375531252286, 0.6169787192598745751, -13.88156336867696616 ) ) ;
#39637 = CARTESIAN_POINT ( 'NONE',  ( 8.279780186038228962, 3.802829437883106234, 6.095677095145819457 ) ) ;
#39638 = DIRECTION ( 'NONE',  ( 0.000000000000000000, -0.7614089499631913061, -0.6482718649732923666 ) ) ;
#39639 = EDGE_CURVE ( 'NONE', #2324, #17007, #55818, .T. ) ;
#39640 = CARTESIAN_POINT ( 'NONE',  ( 10.41476354018330852, -5.217465845835395299, -7.827184855449099921 ) ) ;
#39641 = CARTESIAN_POINT ( 'NONE',  ( 11.09999999999999964, 5.340540480602000706, -6.721892539640999864 ) ) ;
#39642 = CARTESIAN_POINT ( 'NONE',  ( 13.51587707751000167, 12.16770442808000041, 2.286102833273000012 ) ) ;
#39643 = ORIENTED_EDGE ( 'NONE', *, *, #18338, .T. ) ;
#39644 = SURFACE_STYLE_FILL_AREA ( #17978 ) ;
#39645 = CARTESIAN_POINT ( 'NONE',  ( 17.94601859325906545, 2.012274714637017681, -13.76488447091686673 ) ) ;
#39646 = ORIENTED_EDGE ( 'NONE', *, *, #49304, .F. ) ;
#39647 = CARTESIAN_POINT ( 'NONE',  ( 24.84564481170258432, -8.580162300291068078, -9.011334502445274452 ) ) ;
#39648 = CARTESIAN_POINT ( 'NONE',  ( 2.623890132543956977, 2.150913519912194261, 2.798833948393636195 ) ) ;
#39649 = CARTESIAN_POINT ( 'NONE',  ( 9.839810841229999383, 5.817107086401000160, -6.945352709928000579 ) ) ;
#39650 = AXIS2_PLACEMENT_3D ( 'NONE', #20226, #62862, #14980 ) ;
#39651 = CARTESIAN_POINT ( 'NONE',  ( 11.52755399909320921, -3.866653594937912608, 6.221473734489903151 ) ) ;
#39652 = CARTESIAN_POINT ( 'NONE',  ( 17.57920308108768381, 1.787817001021368313, -13.88537754104227417 ) ) ;
#39653 = CARTESIAN_POINT ( 'NONE',  ( 9.264236589623052964, -4.933094564478333943, -6.039157063336917375 ) ) ;
#39654 = CARTESIAN_POINT ( 'NONE',  ( 4.825859839683332986, 1.460959015002472494, 0.3926218265389232465 ) ) ;
#39655 = EDGE_LOOP ( 'NONE', ( #15327, #46358, #5362, #54431 ) ) ;
#39656 = CARTESIAN_POINT ( 'NONE',  ( 9.882266086202999844, -4.932716797830999589, 6.390980246320999925 ) ) ;
#39657 = CARTESIAN_POINT ( 'NONE',  ( 10.09999999999999964, 0.000000000000000000, -11.84999999999999964 ) ) ;
#39658 = FACE_OUTER_BOUND ( 'NONE', #67096, .T. ) ;
#39659 = ORIENTED_EDGE ( 'NONE', *, *, #4827, .F. ) ;
#39660 = CARTESIAN_POINT ( 'NONE',  ( 10.21237770872999917, 4.072568038926999812, -8.861829932786999819 ) ) ;
#39661 = ORIENTED_EDGE ( 'NONE', *, *, #22785, .T. ) ;
#39662 = CARTESIAN_POINT ( 'NONE',  ( 9.455342523874998406, 2.871335344632000020, 7.672773098917999413 ) ) ;
#39663 = CARTESIAN_POINT ( 'NONE',  ( 18.17347573203825917, -2.104651709959060479, -12.42298141210392615 ) ) ;
#39664 = VECTOR ( 'NONE', #48290, 1000.000000000000000 ) ;
#39665 = EDGE_CURVE ( 'NONE', #3005, #43316, #29951, .T. ) ;
#39666 = CARTESIAN_POINT ( 'NONE',  ( 24.30000000000000071, -11.77655473258999841, -4.190794510628000680 ) ) ;
#39667 = LINE ( 'NONE', #30468, #37207 ) ;
#39668 = CARTESIAN_POINT ( 'NONE',  ( 24.35365242081699932, 3.253466243142002057, 12.21167519476998464 ) ) ;
#39669 = B_SPLINE_CURVE_WITH_KNOTS ( 'NONE', 3,
 ( #37822, #37477, #10563, #38512, #49005, #22427 ),
 .UNSPECIFIED., .F., .F.,
 ( 4, 1, 1, 4 ),
 ( 0.000000000000000000, 0.3333333333333000081, 0.6666666666667000474, 1.000000000000000000 ),
 .UNSPECIFIED. ) ;
#39670 = EDGE_CURVE ( 'NONE', #35486, #26545, #33807, .T. ) ;
#39671 = CARTESIAN_POINT ( 'NONE',  ( 9.636671671056999955, 3.144964309357700216, 7.356396684460199786 ) ) ;
#39672 = CARTESIAN_POINT ( 'NONE',  ( 9.419101312255003577, -2.376585296233752143, 8.156356589247646838 ) ) ;
#39673 = ORIENTED_EDGE ( 'NONE', *, *, #28689, .F. ) ;
#39674 = CARTESIAN_POINT ( 'NONE',  ( 8.281500452969403625, -5.066926970486362869, 6.455544745802533235 ) ) ;
#39675 = CARTESIAN_POINT ( 'NONE',  ( 10.13035471959000056, 2.409325917207000511, -8.058043919563999680 ) ) ;
#39676 = DIRECTION ( 'NONE',  ( 1.069977439982493646E-11, 1.000000000000000000, -6.186023915333288444E-12 ) ) ;
#39677 = CARTESIAN_POINT ( 'NONE',  ( 12.32491409494622836, 3.065531103753988518, -13.66026219579215173 ) ) ;
#39678 = CARTESIAN_POINT ( 'NONE',  ( 11.09393020684900044, -2.750000000000000000, 7.500000000000000000 ) ) ;
#39679 = CARTESIAN_POINT ( 'NONE',  ( 10.96580795178999956, -4.930647899304999804, 6.170539049947000088 ) ) ;
#39680 = CARTESIAN_POINT ( 'NONE',  ( 18.10090605892218107, -0.4811670829680718686, 13.99174107639406195 ) ) ;
#39681 = CARTESIAN_POINT ( 'NONE',  ( 17.88331607686893321, -1.943250335979559429, 12.56477475324056847 ) ) ;
#39682 = B_SPLINE_CURVE_WITH_KNOTS ( 'NONE', 3,
 ( #10354, #43559, #48454, #562, #26795 ),
 .UNSPECIFIED., .F., .F.,
 ( 4, 1, 4 ),
 ( 0.000000000000000000, 0.5000000000000000000, 1.000000000000000000 ),
 .UNSPECIFIED. ) ;
#39683 = B_SPLINE_CURVE_WITH_KNOTS ( 'NONE', 3,
 ( #52807, #46534, #41286, #15407, #30455, #67841 ),
 .UNSPECIFIED., .F., .F.,
 ( 4, 2, 4 ),
 ( 0.000000000000000000, 0.5000000000000000000, 1.000000000000000000 ),
 .UNSPECIFIED. ) ;
#39684 = ORIENTED_EDGE ( 'NONE', *, *, #32363, .F. ) ;
#39685 = ORIENTED_EDGE ( 'NONE', *, *, #40750, .F. ) ;
#39686 = CARTESIAN_POINT ( 'NONE',  ( 8.997439158776000312, 2.773858540272000184, -8.951250717848999727 ) ) ;
#39687 = CARTESIAN_POINT ( 'NONE',  ( 12.21982127435327214, -0.2196390008458968812, 13.89766917373561839 ) ) ;
#39688 = CIRCLE ( 'NONE', #48615, 0.6999999999999992895 ) ;
#39689 = CARTESIAN_POINT ( 'NONE',  ( 12.24478949869565447, -2.777190625952814962, 13.61075457644798448 ) ) ;
#39690 = DIRECTION ( 'NONE',  ( -1.000000000000000000, 0.000000000000000000, 0.000000000000000000 ) ) ;
#39691 = CARTESIAN_POINT ( 'NONE',  ( 7.101308059622001068, -3.554853390786000045, 8.889491623367000273 ) ) ;
#39692 = CARTESIAN_POINT ( 'NONE',  ( 11.49977531252999974, 12.49365449110755222, 1.022561121909975057 ) ) ;
#39694 = DIRECTION ( 'NONE',  ( 3.910744185214936488E-06, 0.9659310281233842721, 0.2587996307825956022 ) ) ;
#39693 = CARTESIAN_POINT ( 'NONE',  ( 10.23301337669299826, -5.017903082085999777, 8.017308190024898806 ) ) ;
#39695 = CARTESIAN_POINT ( 'NONE',  ( 10.66579975933730040, 5.208485784810999775, -7.084213409908699965 ) ) ;
#39696 = EDGE_LOOP ( 'NONE', ( #62748, #30899, #15339, #40543, #39974, #17025 ) ) ;
#39697 = CARTESIAN_POINT ( 'NONE',  ( 7.356653345687266032, 2.795129470416956696, -6.794966557345468061 ) ) ;
#39698 = CARTESIAN_POINT ( 'NONE',  ( 10.95489937859999863, -2.662062732762999762, -4.890147771044999203 ) ) ;
#39699 = DIRECTION ( 'NONE',  ( -1.000000000000000000, 0.000000000000000000, 0.000000000000000000 ) ) ;
#39700 = CARTESIAN_POINT ( 'NONE',  ( 12.19608323749910639, -0.1421782557229003263, 12.69895087450873383 ) ) ;
#39701 = CARTESIAN_POINT ( 'NONE',  ( 18.16243401504203447, -2.647653207482971727, -12.41593780944610437 ) ) ;
#39702 = ORIENTED_EDGE ( 'NONE', *, *, #47750, .F. ) ;
#39704 = CARTESIAN_POINT ( 'NONE',  ( 11.08126742035591228, 3.231380926423224054, 7.893373809886144343 ) ) ;
#39703 = DIRECTION ( 'NONE',  ( -1.000000000000000000, 0.000000000000000000, 0.000000000000000000 ) ) ;
#39705 = CARTESIAN_POINT ( 'NONE',  ( 8.953620280414000376, 2.881930053949999682, -8.823338183322999129 ) ) ;
#39706 = ADVANCED_FACE ( 'NONE', ( #49876 ), #50910, .T. ) ;
#39707 = EDGE_CURVE ( 'NONE', #28572, #9350, #1988, .T. ) ;
#39708 =( BOUNDED_SURFACE ( )  B_SPLINE_SURFACE ( 3, 3, ( 
 ( #17470, #44742, #1048, #12920 ),
 ( #38795, #49625, #66040, #55568 ),
 ( #33552, #22360, #28302, #43698 ),
 ( #12571, #1386, #60119, #45082 ) ),
 .UNSPECIFIED., .F., .F., .T. ) 
 B_SPLINE_SURFACE_WITH_KNOTS ( ( 4, 4 ),
 ( 4, 4 ),
 ( 0.000000000000000000, 1.000000000000000000 ),
 ( 0.000000000000000000, 1.000000000000000000 ),
 .UNSPECIFIED. ) 
 GEOMETRIC_REPRESENTATION_ITEM ( )  RATIONAL_B_SPLINE_SURFACE ( (
 ( 1.512182578520000042, 1.160176301760999840, 1.160176301760999840, 1.512182578520000042),
 ( 1.111288591041000196, 0.8526025270081000196, 0.8526025270081000196, 1.111288591041000196),
 ( 1.111288591041000196, 0.8526025270081000196, 0.8526025270081000196, 1.111288591041000196),
 ( 1.512182578520000042, 1.160176301760999840, 1.160176301760999840, 1.512182578520000042) ) ) 
 REPRESENTATION_ITEM ( '' )  SURFACE ( )  );
#39709 = DIRECTION ( 'NONE',  ( 1.000000000000000000, 0.000000000000000000, 0.000000000000000000 ) ) ;
#39710 = CARTESIAN_POINT ( 'NONE',  ( 10.76426088462129904, 4.002719309691810778, 8.778009775371000245 ) ) ;
#39711 = VECTOR ( 'NONE', #8911, 1000.000000000000000 ) ;
#39712 = LINE ( 'NONE', #13493, #37786 ) ;
#39713 = VECTOR ( 'NONE', #49743, 1000.000000000000000 ) ;
#39714 = CYLINDRICAL_SURFACE ( 'NONE', #56623, 1.500000000000000000 ) ;
#39715 = CARTESIAN_POINT ( 'NONE',  ( 2.113699819910999977, 1.185225022173999943, -3.001128720719000054 ) ) ;
#39716 = ORIENTED_EDGE ( 'NONE', *, *, #15247, .F. ) ;
#39717 = CARTESIAN_POINT ( 'NONE',  ( 12.27537049189642637, 0.4912829912815125932, -12.59042165808840075 ) ) ;
#39718 = CARTESIAN_POINT ( 'NONE',  ( 10.99695204966289630, -2.814806026439112596, 5.073559010014569992 ) ) ;
#39719 = CARTESIAN_POINT ( 'NONE',  ( 24.00946646489260061, -12.69708847614298364, -3.467516079534666673 ) ) ;
#39720 = CARTESIAN_POINT ( 'NONE',  ( 8.256676658772999389, 2.876288091423999660, 6.568897128359000526 ) ) ;
#39721 = DIRECTION ( 'NONE',  ( 0.000000000000000000, 0.000000000000000000, -1.000000000000000000 ) ) ;
#39722 = VERTEX_POINT ( 'NONE', #2669 ) ;
#39723 = CARTESIAN_POINT ( 'NONE',  ( 6.681205881262999746, 1.240385862733000000, 0.4581726639353000397 ) ) ;
#39724 = CARTESIAN_POINT ( 'NONE',  ( 10.91724622068368866, 9.661695380177112824, 5.909120167440196525 ) ) ;
#39725 = EDGE_CURVE ( 'NONE', #46011, #53731, #12497, .T. ) ;
#39727 = DIRECTION ( 'NONE',  ( 0.000000000000000000, 0.000000000000000000, 1.000000000000000000 ) ) ;
#39726 = CARTESIAN_POINT ( 'NONE',  ( 8.555928920931012982, -3.595744531712468106, 5.807944245245301396 ) ) ;
#39728 = CARTESIAN_POINT ( 'NONE',  ( 11.28118179236249929, 3.732952383914999839, 8.749800764654999341 ) ) ;
#39729 = CARTESIAN_POINT ( 'NONE',  ( 11.67766954483535891, 4.715882430684499305, -6.395429936871999566 ) ) ;
#39730 = ORIENTED_EDGE ( 'NONE', *, *, #40346, .T. ) ;
#39731 = FACE_OUTER_BOUND ( 'NONE', #52762, .T. ) ;
#39732 = ORIENTED_EDGE ( 'NONE', *, *, #19083, .F. ) ;
#39733 = EDGE_CURVE ( 'NONE', #64166, #4182, #11053, .T. ) ;
#39734 = DIRECTION ( 'NONE',  ( 1.000000000000000000, 0.000000000000000000, 0.000000000000000000 ) ) ;
#39735 = CARTESIAN_POINT ( 'NONE',  ( 9.010191940380000375, -5.040796345420999636, 8.522966281393001609 ) ) ;
#39736 = CARTESIAN_POINT ( 'NONE',  ( 18.20560607722003610, -0.3231860383015854876, -13.99628497142876249 ) ) ;
#39737 = ORIENTED_EDGE ( 'NONE', *, *, #61959, .T. ) ;
#39738 = CARTESIAN_POINT ( 'NONE',  ( 10.96710728122044287, 8.735833061596222748, -6.507096358675760861 ) ) ;
#39739 = DIRECTION ( 'NONE',  ( 0.000000000000000000, 0.000000000000000000, -1.000000000000000000 ) ) ;
#39740 = LINE ( 'NONE', #7921, #9145 ) ;
#39741 = CARTESIAN_POINT ( 'NONE',  ( 0.2000000000000000389, 0.000000000000000000, 0.000000000000000000 ) ) ;
#39742 = CARTESIAN_POINT ( 'NONE',  ( 18.13624123192029813, -2.730018939419430968, 12.39502206876364099 ) ) ;
#39743 = VERTEX_POINT ( 'NONE', #66978 ) ;
#39744 = CARTESIAN_POINT ( 'NONE',  ( 7.871551658771999804, 4.780986922229000236, 6.267222470044999660 ) ) ;
#39745 = CARTESIAN_POINT ( 'NONE',  ( 23.66566003730900292, -13.24658845605999957, -3.907283439093999888 ) ) ;
#39746 = CARTESIAN_POINT ( 'NONE',  ( 9.748096873515667227, 4.327184855449106138, 8.717465845835393523 ) ) ;
#39747 = FACE_OUTER_BOUND ( 'NONE', #18140, .T. ) ;
#39748 = ORIENTED_EDGE ( 'NONE', *, *, #63288, .T. ) ;
#39749 = CARTESIAN_POINT ( 'NONE',  ( 25.44993786153500182, 9.517611874540000017, -8.103398312166000039 ) ) ;
#39750 = CIRCLE ( 'NONE', #29733, 2.250000000000000000 ) ;
#39751 = CARTESIAN_POINT ( 'NONE',  ( 10.86301932002748138, 2.749999999999999112, -7.799851088612627770 ) ) ;
#39752 = CARTESIAN_POINT ( 'NONE',  ( 7.000000000000000000, 0.8000000000000000444, -3.149999999999999911 ) ) ;
#39753 = CARTESIAN_POINT ( 'NONE',  ( 23.79457394410595228, -3.298060182730888634, -13.14148511287618604 ) ) ;
#39754 = CARTESIAN_POINT ( 'NONE',  ( 11.08757144985999865, 2.712428550139000194, 6.571291218949999902 ) ) ;
#39755 = B_SPLINE_CURVE_WITH_KNOTS ( 'NONE', 3,
 ( #55775, #40715, #2967, #3310, #50524, #23955 ),
 .UNSPECIFIED., .F., .F.,
 ( 4, 2, 4 ),
 ( 0.000000000000000000, 0.1967045975185045814, 0.3934091950370091628 ),
 .UNSPECIFIED. ) ;
#39756 = ADVANCED_FACE ( 'NONE', ( #24686 ), #66290, .F. ) ;
#39757 = CARTESIAN_POINT ( 'NONE',  ( 12.18107303550440257, 0.04113803725886392565, -13.89993798560270122 ) ) ;
#39758 = CARTESIAN_POINT ( 'NONE',  ( 17.98134286629680645, -1.897806848213326791, 12.45626380386397791 ) ) ;
#39759 = EDGE_LOOP ( 'NONE', ( #34652, #29496, #56856, #48679 ) ) ;
#39760 = CARTESIAN_POINT ( 'NONE',  ( 11.43856039236529831, -2.967715280237000375, -7.550239075043479353 ) ) ;
#39761 = ORIENTED_EDGE ( 'NONE', *, *, #48233, .T. ) ;
#39762 = CARTESIAN_POINT ( 'NONE',  ( 0.1499942179680000265, 2.402872127494067644, 1.384928887584814916 ) ) ;
#39763 = VECTOR ( 'NONE', #18970, 1000.000000000000114 ) ;
#39764 = CARTESIAN_POINT ( 'NONE',  ( 8.988579719593998263, 4.902869380824999901, -8.978557145469999057 ) ) ;
#39765 = CARTESIAN_POINT ( 'NONE',  ( 3.460492249740999782, -2.775615920636000045, 1.622391736872000001 ) ) ;
#39766 = CARTESIAN_POINT ( 'NONE',  ( 11.02205565301999890, -2.309485172892000282, -7.515673712097999726 ) ) ;
#39767 = CIRCLE ( 'NONE', #45357, 11.50000000000000178 ) ;
#39768 = LINE ( 'NONE', #2699, #54001 ) ;
#39769 = CARTESIAN_POINT ( 'NONE',  ( 24.25865930858300246, 12.09696615184000024, 3.327219372371000183 ) ) ;
#39770 = ORIENTED_EDGE ( 'NONE', *, *, #60409, .F. ) ;
#39771 = CARTESIAN_POINT ( 'NONE',  ( 11.93718179236249988, -4.209680326224799707, 8.481317998227099864 ) ) ;
#39772 = CARTESIAN_POINT ( 'NONE',  ( 9.137543006348998631, 2.995704926864999784, 8.544754656710999541 ) ) ;
#39773 = FACE_OUTER_BOUND ( 'NONE', #35632, .T. ) ;
#39774 = CARTESIAN_POINT ( 'NONE',  ( 11.29996927726999978, -12.23272628844000032, -1.505586261403999870 ) ) ;
#39775 = CARTESIAN_POINT ( 'NONE',  ( 10.90833333333429067, 5.360760283597206133, 7.292330520109749692 ) ) ;
#39776 = CARTESIAN_POINT ( 'NONE',  ( 10.29262282008599882, 4.451581486939200083, -8.228386593078399258 ) ) ;
#39777 = CARTESIAN_POINT ( 'NONE',  ( 10.96262032192263902, 2.824326349884676013, -6.677398119062115889 ) ) ;
#39778 = CARTESIAN_POINT ( 'NONE',  ( 10.18692546752099837, 2.997990738918999920, -7.430575645513339822 ) ) ;
#39779 = CARTESIAN_POINT ( 'NONE',  ( 18.03319509584025582, -0.5408165383911034407, 12.58839068838662811 ) ) ;
#39780 = CARTESIAN_POINT ( 'NONE',  ( 9.140753410162000492, -5.100000000000000533, 6.175944241622000064 ) ) ;
#39781 = CARTESIAN_POINT ( 'NONE',  ( 8.082873386424997975, 5.111739203374999541, -6.679001318365999751 ) ) ;
#39782 = CARTESIAN_POINT ( 'NONE',  ( 10.53871084122999946, 5.103389446345000025, -6.705205355781999721 ) ) ;
#39783 = EDGE_LOOP ( 'NONE', ( #63017, #18323, #24344, #40849 ) ) ;
#39784 = CARTESIAN_POINT ( 'NONE',  ( 7.629816940376999312, -4.763531818439999732, 5.668890958491999754 ) ) ;
#39785 = EDGE_CURVE ( 'NONE', #51086, #31394, #59398, .T. ) ;
#39786 = ADVANCED_FACE ( 'NONE', ( #44652 ), #27256, .T. ) ;
#39787 = CARTESIAN_POINT ( 'NONE',  ( 18.27904986288414690, 2.473365887482175118, 13.77980577478706792 ) ) ;
#39788 = CARTESIAN_POINT ( 'NONE',  ( 23.60205915885299888, -2.504446818059999469, 12.27382285987999211 ) ) ;
#39789 = CARTESIAN_POINT ( 'NONE',  ( 10.05862282008599884, -3.333723918618700210, -8.574682153725998290 ) ) ;
#39790 = ORIENTED_EDGE ( 'NONE', *, *, #47453, .T. ) ;
#39791 = CARTESIAN_POINT ( 'NONE',  ( 8.475642219593000348, 5.095085596809999728, 6.286981168432999922 ) ) ;
#39792 = CIRCLE ( 'NONE', #48723, 2.000000000000000000 ) ;
#39794 = CARTESIAN_POINT ( 'NONE',  ( 9.212681907068999365, -4.225805508133200661, 6.635485632555699453 ) ) ;
#39793 = CARTESIAN_POINT ( 'NONE',  ( 10.16858376188599955, -4.731143729777899765, -7.965979387614599894 ) ) ;
#39795 = CARTESIAN_POINT ( 'NONE',  ( 10.38052665877000003, 5.283793195606000026, -8.830196380017000024 ) ) ;
#39796 = ORIENTED_EDGE ( 'NONE', *, *, #22162, .T. ) ;
#39797 = CARTESIAN_POINT ( 'NONE',  ( 9.409415556003999370, 2.113395950889999764, 7.914199712930999553 ) ) ;
#39798 = CARTESIAN_POINT ( 'NONE',  ( 13.49980696793000057, -9.514462421839999351, -7.834836582454001608 ) ) ;
#39799 = CARTESIAN_POINT ( 'NONE',  ( 11.35918179236250047, 3.761636028845500412, 8.615559381441000752 ) ) ;
#39800 = CARTESIAN_POINT ( 'NONE',  ( 9.242349231304000767, -5.206700957550999931, 8.808818370147001531 ) ) ;
#39801 = CARTESIAN_POINT ( 'NONE',  ( 8.056015159639001055, 3.481518869265999072, 6.232552614174998951 ) ) ;
#39802 = ORIENTED_EDGE ( 'NONE', *, *, #41513, .F. ) ;
#39803 = FACE_OUTER_BOUND ( 'NONE', #50913, .T. ) ;
#39804 = CARTESIAN_POINT ( 'NONE',  ( 13.99999999231800096, 8.833253877201999060, 7.896562762484000686 ) ) ;
#39805 = EDGE_CURVE ( 'NONE', #65648, #57880, #24443, .T. ) ;
#39806 = CARTESIAN_POINT ( 'NONE',  ( 7.901443686586306470, -2.563629936457297198, 8.480909633787742763 ) ) ;
#39807 = CARTESIAN_POINT ( 'NONE',  ( 11.06924082387999952, -5.425685649895999774, 8.012912555523998392 ) ) ;
#39809 = CARTESIAN_POINT ( 'NONE',  ( 10.47769598648999967, -2.990523684589000197, -8.101059042556599366 ) ) ;
#39808 = AXIS2_PLACEMENT_3D ( 'NONE', #51478, #45562, #30505 ) ;
#39810 = CARTESIAN_POINT ( 'NONE',  ( 9.248138961223999033, -3.167792625045000143, 6.937618199889199033 ) ) ;
#39811 = VERTEX_POINT ( 'NONE', #60285 ) ;
#39812 = LINE ( 'NONE', #61134, #18758 ) ;
#39813 = CARTESIAN_POINT ( 'NONE',  ( 11.09610807141099897, -3.947296672195129918, 6.360477084256999980 ) ) ;
#39814 = ORIENTED_EDGE ( 'NONE', *, *, #25647, .T. ) ;
#39815 = EDGE_CURVE ( 'NONE', #42619, #2862, #66207, .T. ) ;
#39816 = CARTESIAN_POINT ( 'NONE',  ( 8.982564767455604837, 2.896581991245594789, 7.204352198296668064 ) ) ;
#39817 = ORIENTED_EDGE ( 'NONE', *, *, #64503, .T. ) ;
#39818 = CARTESIAN_POINT ( 'NONE',  ( 10.01832872737000102, -5.491975933468000726, -7.893788029530999673 ) ) ;
#39819 = B_SPLINE_CURVE_WITH_KNOTS ( 'NONE', 3,
 ( #33041, #49455, #17302, #55053 ),
 .UNSPECIFIED., .F., .F.,
 ( 4, 4 ),
 ( 0.000000000000000000, 1.000000000000000000 ),
 .UNSPECIFIED. ) ;
#39820 = CARTESIAN_POINT ( 'NONE',  ( 9.541460841232000334, 2.824732249080000202, -8.992748220058999209 ) ) ;
#39821 = CARTESIAN_POINT ( 'NONE',  ( 10.88813259637009878, 2.844182332072999753, -8.129798612793599943 ) ) ;
#39822 = DIRECTION ( 'NONE',  ( 1.000000000000000000, 0.000000000000000000, 0.000000000000000000 ) ) ;
#39823 = CARTESIAN_POINT ( 'NONE',  ( 12.27745450063681432, 2.164896879444428102, -12.52337953207688059 ) ) ;
#39824 = CARTESIAN_POINT ( 'NONE',  ( 11.51872200990539952, -4.947480442174099657, 7.830502140005199507 ) ) ;
#39825 = CARTESIAN_POINT ( 'NONE',  ( 11.02435971519499880, -3.467537960339900138, 8.385788382729799650 ) ) ;
#39826 = ORIENTED_EDGE ( 'NONE', *, *, #38667, .T. ) ;
#39827 = CARTESIAN_POINT ( 'NONE',  ( 9.164680296029999340, 2.899999999999999911, -6.162130047625999474 ) ) ;
#39828 = ORIENTED_EDGE ( 'NONE', *, *, #25310, .T. ) ;
#39829 = CARTESIAN_POINT ( 'NONE',  ( 7.481081853206999810, -2.374041291348000016, 8.293390875797999939 ) ) ;
#39830 = CARTESIAN_POINT ( 'NONE',  ( 7.934990594362998806, 3.391823837616000148, -6.294741454024999960 ) ) ;
#39831 = EDGE_LOOP ( 'NONE', ( #57168, #4370, #22657, #192 ) ) ;
#39832 = CARTESIAN_POINT ( 'NONE',  ( 12.32336322858531474, -1.942450600934338745, -12.44937554728605100 ) ) ;
#39833 = CARTESIAN_POINT ( 'NONE',  ( 10.40333997687999990, 4.213854445120500003, 8.480416814141699788 ) ) ;
#39834 = CARTESIAN_POINT ( 'NONE',  ( 9.964045559621999004, -3.485908552077000344, -9.275738075927998594 ) ) ;
#39835 = CARTESIAN_POINT ( 'NONE',  ( 5.099999999649000415, -1.199999999999999956, -9.776630298829998011 ) ) ;
#39836 = CARTESIAN_POINT ( 'NONE',  ( 17.60891751954699913, -11.55195517866999921, 4.941472061358999746 ) ) ;
#39837 = CARTESIAN_POINT ( 'NONE',  ( 7.550000000000000711, -4.000000000000000000, 8.849999999999999645 ) ) ;
#39838 = CARTESIAN_POINT ( 'NONE',  ( 12.18760440664042122, -2.401006893892608129, -13.69392356709392544 ) ) ;
#39839 = CARTESIAN_POINT ( 'NONE',  ( 17.96738117868769535, -0.4698014501121463016, -12.68830453558793003 ) ) ;
#39840 = CARTESIAN_POINT ( 'NONE',  ( 11.66287348028854964, -4.761955701524100526, -7.911973420841600380 ) ) ;
#39841 = CARTESIAN_POINT ( 'NONE',  ( 10.56733863405299800, -3.211524470605299886, -8.505794571537999005 ) ) ;
#39842 = CARTESIAN_POINT ( 'NONE',  ( 8.636454719592999041, 3.869396554003000421, 5.695652484872999466 ) ) ;
#39843 = ORIENTED_EDGE ( 'NONE', *, *, #34022, .T. ) ;
#39844 = VECTOR ( 'NONE', #62081, 1000.000000000000000 ) ;
#39845 = CARTESIAN_POINT ( 'NONE',  ( 10.89999568968999988, -1.433323842147000038, -10.65402156160000047 ) ) ;
#39846 = CARTESIAN_POINT ( 'NONE',  ( 10.58718478751724312, -5.286440948693045705, -7.026985308887813808 ) ) ;
#39847 = CARTESIAN_POINT ( 'NONE',  ( 10.09453415443000068, 5.362844031509000686, -7.550030311027999375 ) ) ;
#39848 = CONICAL_SURFACE ( 'NONE', #43180, 11.75016914289000169, 0.7854125553233202162 ) ;
#39849 = CARTESIAN_POINT ( 'NONE',  ( 17.92067275948977212, 3.101661042832197790, 12.21227817455808307 ) ) ;
#39850 = EDGE_CURVE ( 'NONE', #2231, #664, #56130, .T. ) ;
#39851 = CARTESIAN_POINT ( 'NONE',  ( 18.16350100824700320, 3.138009765975000143, -11.88148072165000002 ) ) ;
#39852 = ADVANCED_FACE ( 'NONE', ( #2583 ), #66554, .F. ) ;
#39853 = CARTESIAN_POINT ( 'NONE',  ( 10.12550053024000007, 5.788811067708000024, 7.335561454339999621 ) ) ;
#39854 = AXIS2_PLACEMENT_3D ( 'NONE', #29685, #2067, #67056 ) ;
#39855 = CARTESIAN_POINT ( 'NONE',  ( 9.129428851719998406, -5.099284414202999827, 6.151604790022999758 ) ) ;
#39856 = CARTESIAN_POINT ( 'NONE',  ( 12.70786224242106677, 0.7192245859875908698, -12.57945610904468303 ) ) ;
#39857 = ORIENTED_EDGE ( 'NONE', *, *, #55004, .F. ) ;
#39858 = CARTESIAN_POINT ( 'NONE',  ( 12.33224723617690088, -2.090732662878786563, 12.53759506087955167 ) ) ;
#39859 = CARTESIAN_POINT ( 'NONE',  ( 9.880963142879998884, -3.151633609938700342, -7.321163726496699553 ) ) ;
#39860 = CARTESIAN_POINT ( 'NONE',  ( 9.813360311708999362, 5.349397258738000538, 6.657026394682000081 ) ) ;
#39861 = B_SPLINE_CURVE_WITH_KNOTS ( 'NONE', 3,
 ( #21428, #5697, #807, #38203 ),
 .UNSPECIFIED., .F., .F.,
 ( 4, 4 ),
 ( 0.8745855536721935941, 1.000000000000000000 ),
 .UNSPECIFIED. ) ;
#39862 = CARTESIAN_POINT ( 'NONE',  ( 9.171146261768624797, 4.712741083356099203, 8.539225147222756718 ) ) ;
#39863 = CIRCLE ( 'NONE', #10795, 2.499999999999999556 ) ;
#39864 = CARTESIAN_POINT ( 'NONE',  ( 10.62072335273219892, 4.397090433355999473, -8.569396700949999612 ) ) ;
#39865 = CARTESIAN_POINT ( 'NONE',  ( 12.27431907826859714, 0.3302353423713642044, 12.69422546839060395 ) ) ;
#39866 = CARTESIAN_POINT ( 'NONE',  ( 8.995176658772999545, 2.707986230053999854, 5.994446745591000436 ) ) ;
#39867 = CARTESIAN_POINT ( 'NONE',  ( 10.65550720192000078, 4.237674045823999869, 9.105219676299999065 ) ) ;
#39868 = VECTOR ( 'NONE', #11940, 1000.000000000000114 ) ;
#39869 = CARTESIAN_POINT ( 'NONE',  ( 12.33197597414241997, 2.091428098900828925, 12.53741636228079948 ) ) ;
#39870 = ORIENTED_EDGE ( 'NONE', *, *, #11700, .T. ) ;
#39871 = CARTESIAN_POINT ( 'NONE',  ( 9.386379719595000282, 5.673443217382001080, -7.051790060464000476 ) ) ;
#39872 = CARTESIAN_POINT ( 'NONE',  ( 10.59195391537400077, 5.057233422790000432, -8.218034727798299244 ) ) ;
#39873 = ADVANCED_FACE ( 'NONE', ( #34069 ), #12740, .F. ) ;
#39874 = ADVANCED_FACE ( 'NONE', ( #1904 ), #50830, .T. ) ;
#39875 = DIRECTION ( 'NONE',  ( 0.000000000000000000, 0.3380237670531082705, 0.9411375738473234387 ) ) ;
#39877 = CARTESIAN_POINT ( 'NONE',  ( 3.250973465878000290, -3.500000000000000000, 0.000000000000000000 ) ) ;
#39876 = CARTESIAN_POINT ( 'NONE',  ( 7.726441940376999717, -2.630475685621000093, 6.995953627589999613 ) ) ;
#39878 = CARTESIAN_POINT ( 'NONE',  ( 9.805380199233999505, -3.003429752324399793, 7.625259896924899472 ) ) ;
#39879 = CARTESIAN_POINT ( 'NONE',  ( 11.58902763632552002, -4.786505910413500153, -7.137085349939700230 ) ) ;
#39880 = ORIENTED_EDGE ( 'NONE', *, *, #36173, .T. ) ;
#39881 = EDGE_CURVE ( 'NONE', #20140, #1557, #45926, .T. ) ;
#39882 = CARTESIAN_POINT ( 'NONE',  ( 1.639247443156000017, -2.867416142353000463, -1.874231387797000048 ) ) ;
#39883 = CARTESIAN_POINT ( 'NONE',  ( 9.099999999999999645, 0.000000000000000000, 0.000000000000000000 ) ) ;
#39884 = CARTESIAN_POINT ( 'NONE',  ( 12.79999999975700042, 11.86189249994999884, -3.298671769835999967 ) ) ;
#39885 = DIRECTION ( 'NONE',  ( 0.000000000000000000, -1.000000000000000000, -3.072868395130999887E-14 ) ) ;
#39886 = CARTESIAN_POINT ( 'NONE',  ( 16.39999999379500295, 3.351248059343999941, 11.15756683833000018 ) ) ;
#39887 = CARTESIAN_POINT ( 'NONE',  ( 12.50373643672537582, -3.182160109867291808, 13.63355731004866556 ) ) ;
#39888 = CARTESIAN_POINT ( 'NONE',  ( 25.29987654162099986, 9.517611874540000017, 8.103398312166000039 ) ) ;
#39889 = DIRECTION ( 'NONE',  ( 1.000000000000000000, 0.000000000000000000, 0.000000000000000000 ) ) ;
#39890 = CARTESIAN_POINT ( 'NONE',  ( 13.68724299200000161, -12.36060503258000054, -2.247042498203000171 ) ) ;
#39891 = ORIENTED_EDGE ( 'NONE', *, *, #29374, .F. ) ;
#39892 = CARTESIAN_POINT ( 'NONE',  ( 8.534482780410998615, 3.011620138462000273, 8.801434747080000065 ) ) ;
#39893 = CARTESIAN_POINT ( 'NONE',  ( 11.04497253870000151, 5.245448120407000481, 5.177000073770999578 ) ) ;
#39894 = CARTESIAN_POINT ( 'NONE',  ( 7.395800130882417278, -2.637111068654788060, 8.607766089379190078 ) ) ;
#39895 = CIRCLE ( 'NONE', #10828, 12.24999851416000141 ) ;
#39896 = CARTESIAN_POINT ( 'NONE',  ( 1.284778341492999868E-07, 2.574999650349000024, 0.000000000000000000 ) ) ;
#39897 = CARTESIAN_POINT ( 'NONE',  ( 1.504838003975000005, -2.867416142353000463, -1.874231387797000048 ) ) ;
#39898 = ORIENTED_EDGE ( 'NONE', *, *, #52522, .F. ) ;
#39899 = CARTESIAN_POINT ( 'NONE',  ( 8.620740978634000129, -4.599999999999999645, 5.898823289756999877 ) ) ;
#39900 = EDGE_CURVE ( 'NONE', #63935, #60029, #62800, .T. ) ;
#39901 = CARTESIAN_POINT ( 'NONE',  ( 11.09999999999999964, 2.899999999999999911, 4.467422426380999845 ) ) ;
#39902 = CARTESIAN_POINT ( 'NONE',  ( 11.27765994926999937, 3.273804980682999854, 6.368305648407000419 ) ) ;
#39903 = CARTESIAN_POINT ( 'NONE',  ( 11.65871932425156920, 3.852858594438699935, 6.507377093516500288 ) ) ;
#39904 = CARTESIAN_POINT ( 'NONE',  ( 9.549696181504765846, -3.998651493754463271, 8.867000060670704897 ) ) ;
#39905 = LINE ( 'NONE', #18919, #65038 ) ;
#39906 = CIRCLE ( 'NONE', #29885, 0.6999999999999992895 ) ;
#39907 = LINE ( 'NONE', #55291, #43398 ) ;
#39908 = DIRECTION ( 'NONE',  ( -0.8660254037844288266, -3.264431060564110057E-14, 0.5000000000000169864 ) ) ;
#39909 = CARTESIAN_POINT ( 'NONE',  ( 12.18214412808147884, -2.552249690271653826, 12.43927262873609685 ) ) ;
#39910 = CARTESIAN_POINT ( 'NONE',  ( 7.810465616207683759, 4.327298288918835389, 9.232443200123778837 ) ) ;
#39911 = VERTEX_POINT ( 'NONE', #63363 ) ;
#39912 = CIRCLE ( 'NONE', #22020, 12.50000000000000178 ) ;
#39913 = CARTESIAN_POINT ( 'NONE',  ( 18.27871553590501108, -2.567375067704839253, 13.76260043498214181 ) ) ;
#39914 = CARTESIAN_POINT ( 'NONE',  ( 10.66579975933730040, -2.791514215189000225, -7.084213409908699965 ) ) ;
#39915 = EDGE_LOOP ( 'NONE', ( #8461, #6006, #22756 ) ) ;
#39916 = VERTEX_POINT ( 'NONE', #15490 ) ;
#39917 = CARTESIAN_POINT ( 'NONE',  ( 10.48791429142999831, 4.016993441347180394, 8.391963954669400039 ) ) ;
#39918 = CARTESIAN_POINT ( 'NONE',  ( 5.500000000000000000, -13.94845324556000143, 4.312847325879000770 ) ) ;
#39919 = CARTESIAN_POINT ( 'NONE',  ( 3.999999173945999686, -1.825000327749000117, 0.000000000000000000 ) ) ;
#39920 = CARTESIAN_POINT ( 'NONE',  ( 10.02991192131000098, 2.506457833269999824, 6.215406506815000398 ) ) ;
#39921 = CARTESIAN_POINT ( 'NONE',  ( 10.05525296965999971, 5.223856410664000194, -6.898317050646999959 ) ) ;
#39922 = CARTESIAN_POINT ( 'NONE',  ( 9.972537864286000087, -2.899999999999999911, -6.571291218949999902 ) ) ;
#39923 = CARTESIAN_POINT ( 'NONE',  ( 9.569799020577001158, -4.064052785562999759, 8.919253808370999792 ) ) ;
#39924 = CARTESIAN_POINT ( 'NONE',  ( 11.61719580513100247, 3.441045665385999985, -11.09087012887000157 ) ) ;
#39925 = CIRCLE ( 'NONE', #22027, 0.5500000000000000444 ) ;
#39926 = CARTESIAN_POINT ( 'NONE',  ( 10.36629943602999937, -5.852732332139999549, -7.568014220767000033 ) ) ;
#39927 = CARTESIAN_POINT ( 'NONE',  ( 11.63410404293056999, -4.442327784369100030, -8.400720262063998689 ) ) ;
#39928 = CARTESIAN_POINT ( 'NONE',  ( 10.74230018269611797, -2.926900783495216096, -5.077338026010398409 ) ) ;
#39929 = ORIENTED_EDGE ( 'NONE', *, *, #38832, .F. ) ;
#39930 = CARTESIAN_POINT ( 'NONE',  ( 9.819055905797000605, 2.899999999999999911, -6.571291218949999902 ) ) ;
#39931 = DIRECTION ( 'NONE',  ( 0.000000000000000000, 1.000000000000000000, 0.000000000000000000 ) ) ;
#39932 = CARTESIAN_POINT ( 'NONE',  ( 10.80457650502840927, -2.650115154242059123, -7.676668932391375044 ) ) ;
#39933 = CARTESIAN_POINT ( 'NONE',  ( 9.321001730958840881, 3.231794228473278352, 8.499596153627864581 ) ) ;
#39934 = EDGE_CURVE ( 'NONE', #438, #28572, #4685, .T. ) ;
#39935 = CARTESIAN_POINT ( 'NONE',  ( 12.18828317886887902, 2.603111844536875275, 13.65101713889819557 ) ) ;
#39936 = EDGE_CURVE ( 'NONE', #11746, #31922, #24604, .T. ) ;
#39937 = CARTESIAN_POINT ( 'NONE',  ( 9.722771884505998941, -5.493781611190000191, 6.566828939965000167 ) ) ;
#39938 = EDGE_LOOP ( 'NONE', ( #66603, #63119, #62170, #47730, #50215, #40144, #49881, #50570 ) ) ;
#39939 = CARTESIAN_POINT ( 'NONE',  ( 12.24748280279661472, 0.2825744476584710618, -12.69577188568926474 ) ) ;
#39940 = CARTESIAN_POINT ( 'NONE',  ( 12.48353988083098365, 0.6549277419692597357, 13.98467727287826889 ) ) ;
#39941 = ORIENTED_EDGE ( 'NONE', *, *, #577, .F. ) ;
#39942 = DIRECTION ( 'NONE',  ( 0.000000000000000000, -0.7071067811865475727, -0.7071067811865475727 ) ) ;
#39943 = DIRECTION ( 'NONE',  ( 0.000000000000000000, 0.8648648648648720183, -0.5020047465136825426 ) ) ;
#39944 = CARTESIAN_POINT ( 'NONE',  ( 23.95106197147099891, -3.419222116214999829, -12.90055402021999953 ) ) ;
#39945 = DIRECTION ( 'NONE',  ( 1.000000000000000000, 0.000000000000000000, 0.000000000000000000 ) ) ;
#39946 = VECTOR ( 'NONE', #32916, 1000.000000000000000 ) ;
#39947 =( GEOMETRIC_REPRESENTATION_CONTEXT ( 3 ) GLOBAL_UNCERTAINTY_ASSIGNED_CONTEXT ( ( #7802 ) ) GLOBAL_UNIT_ASSIGNED_CONTEXT ( ( #48604, #31842, #63975 ) ) REPRESENTATION_CONTEXT ( 'NONE', 'WORKASPACE' ) );
#39948 = CARTESIAN_POINT ( 'NONE',  ( 9.384624721950221016, 2.899999999999999911, 6.445686799063069294 ) ) ;
#39949 = DIRECTION ( 'NONE',  ( 0.000000000000000000, 0.000000000000000000, -1.000000000000000000 ) ) ;
#39950 = CARTESIAN_POINT ( 'NONE',  ( 0.1866496906522999988, 2.306917309723999665, 2.681989686974000087 ) ) ;
#39951 = CARTESIAN_POINT ( 'NONE',  ( 11.09999999999999964, -4.000000000000000000, 7.500000000000000000 ) ) ;
#39952 = AXIS2_PLACEMENT_3D ( 'NONE', #51815, #57400, #56387 ) ;
#39953 = CARTESIAN_POINT ( 'NONE',  ( 12.36610530618393433, 3.052942130732427373, 12.22454734379039287 ) ) ;
#39954 = B_SPLINE_CURVE_WITH_KNOTS ( 'NONE', 3,
 ( #4623, #40322, #3258, #24926 ),
 .UNSPECIFIED., .F., .F.,
 ( 4, 4 ),
 ( 0.000000000000000000, 0.1253171456473068379 ),
 .UNSPECIFIED. ) ;
#39955 = CARTESIAN_POINT ( 'NONE',  ( 9.568154437819998748, -5.318469253323000245, -7.099528416287999910 ) ) ;
#39956 = CARTESIAN_POINT ( 'NONE',  ( 10.72749279009019929, 3.774717370312400178, -8.336388861178200216 ) ) ;
#39957 = DIRECTION ( 'NONE',  ( 0.000000000000000000, -0.1218274111675001353, 0.9925512993736016476 ) ) ;
#39958 = FACE_OUTER_BOUND ( 'NONE', #27606, .T. ) ;
#39959 = CARTESIAN_POINT ( 'NONE',  ( 9.227380199234000102, 5.132898093246000215, -7.357604921762999517 ) ) ;
#39961 = CARTESIAN_POINT ( 'NONE',  ( 11.14011782775999926, -2.672921762942999990, 4.984811564083999613 ) ) ;
#39960 = CARTESIAN_POINT ( 'NONE',  ( 15.95296092448800174, -8.433319028468000411, -8.247373098099998856 ) ) ;
#39962 = CARTESIAN_POINT ( 'NONE',  ( 23.62276920851202888, -13.40178483158021550, 3.911135730022063939 ) ) ;
#39963 = EDGE_LOOP ( 'NONE', ( #678, #34789, #33826, #25528, #27869, #63927, #30477, #45742 ) ) ;
#39964 = CIRCLE ( 'NONE', #63333, 0.2000000000000007327 ) ;
#39965 = EDGE_CURVE ( 'NONE', #20104, #15326, #34483, .T. ) ;
#39966 = CARTESIAN_POINT ( 'NONE',  ( 9.709999999999999076, -4.496968146123999865, -8.755198255949000696 ) ) ;
#39967 = CARTESIAN_POINT ( 'NONE',  ( 9.939319226872999735, -2.638101016021999978, 6.328632621050000573 ) ) ;
#39968 = CARTESIAN_POINT ( 'NONE',  ( 8.973138961223998677, 4.946050868436800307, 6.860686042446299204 ) ) ;
#39969 = CARTESIAN_POINT ( 'NONE',  ( 10.13874943042162613, 3.152062997842154157, -7.715719979441764131 ) ) ;
#39970 = AXIS2_PLACEMENT_3D ( 'NONE', #44027, #28992, #7996 ) ;
#39971 = CARTESIAN_POINT ( 'NONE',  ( 9.573148997458000409, -5.167567567567999731, -6.822293592207000934 ) ) ;
#39972 = FACE_OUTER_BOUND ( 'NONE', #57539, .T. ) ;
#39973 = PRODUCT_DEFINITION_CONTEXT ( 'detailed design', #11030, 'design' ) ;
#39974 = ORIENTED_EDGE ( 'NONE', *, *, #51055, .F. ) ;
#39975 = CARTESIAN_POINT ( 'NONE',  ( 8.796784697134999220, -3.380386586585000241, -6.540930833646799947 ) ) ;
#39976 = CARTESIAN_POINT ( 'NONE',  ( 11.33810207955129812, 4.796537143354000499, 7.174999999999999822 ) ) ;
#39977 = B_SPLINE_CURVE_WITH_KNOTS ( 'NONE', 3,
 ( #26636, #21372, #62976, #64349, #10199, #63322 ),
 .UNSPECIFIED., .F., .F.,
 ( 4, 2, 4 ),
 ( 0.000000000000000000, 0.5000000000000000000, 1.000000000000000000 ),
 .UNSPECIFIED. ) ;
#39978 = PRODUCT_DEFINITION_SHAPE ( 'NONE', 'NONE',  #57742 ) ;
#39979 = EDGE_CURVE ( 'NONE', #61812, #21138, #4297, .T. ) ;
#39980 = CARTESIAN_POINT ( 'NONE',  ( 17.60337015074822276, 1.762344248314549944, -12.47614295832086206 ) ) ;
#39981 = CARTESIAN_POINT ( 'NONE',  ( 7.000000000000000000, 7.356634010774431687, 3.356634010774432575 ) ) ;
#39982 = CYLINDRICAL_SURFACE ( 'NONE', #37316, 1.100000000000000089 ) ;
#39983 = CARTESIAN_POINT ( 'NONE',  ( 11.41256651104150066, 4.098999650273559503, -6.501426055769400136 ) ) ;
#39984 = CYLINDRICAL_SURFACE ( 'NONE', #10786, 1.350000000000000533 ) ;
#39985 = CARTESIAN_POINT ( 'NONE',  ( 9.191972128127998687, -4.867164667115999599, -6.095483598963999938 ) ) ;
#39986 = CARTESIAN_POINT ( 'NONE',  ( 25.19548556333399958, 11.71503697860999971, 2.904522712328000189 ) ) ;
#39987 = ORIENTED_EDGE ( 'NONE', *, *, #18312, .F. ) ;
#39988 = CARTESIAN_POINT ( 'NONE',  ( 9.897088546675218979, -5.285903972627228775, 7.026783966727966124 ) ) ;
#39989 = CARTESIAN_POINT ( 'NONE',  ( 12.08961512266908755, -0.1188263301541226807, -13.99950072926553979 ) ) ;
#39990 = CYLINDRICAL_SURFACE ( 'NONE', #13147, 1.000000000000000444 ) ;
#39991 = CARTESIAN_POINT ( 'NONE',  ( 11.43028911132391556, 2.855999340945334808, -8.059011948032956951 ) ) ;
#39992 = CARTESIAN_POINT ( 'NONE',  ( 9.758079719591000512, 4.905765359186999852, -8.776126235875999271 ) ) ;
#39993 = CARTESIAN_POINT ( 'NONE',  ( 11.99056651104150006, -3.914543207408039738, 8.361971998931499783 ) ) ;
#39994 = VERTEX_POINT ( 'NONE', #46621 ) ;
#39995 = DIRECTION ( 'NONE',  ( -1.000000000000000000, 0.000000000000000000, 0.000000000000000000 ) ) ;
#39996 = CARTESIAN_POINT ( 'NONE',  ( 18.15957959476899930, 2.341019627110876744, -13.70589624875886692 ) ) ;
#39997 = ORIENTED_EDGE ( 'NONE', *, *, #18191, .F. ) ;
#39998 = CARTESIAN_POINT ( 'NONE',  ( 8.497376085219444874, 4.829144488946226055, 8.579037299257318949 ) ) ;
#39999 = CARTESIAN_POINT ( 'NONE',  ( 24.99826568414079375, 2.941276671990348923, 11.56308286680369335 ) ) ;
#40000 = VECTOR ( 'NONE', #20616, 1000.000000000000000 ) ;
#40001 = CARTESIAN_POINT ( 'NONE',  ( 9.161379719595000637, 5.511689883260999956, -7.095113581311000672 ) ) ;
#40002 = CARTESIAN_POINT ( 'NONE',  ( 13.86901036581968860, -9.187486520156699754, -8.213234632844541139 ) ) ;
#40003 = CARTESIAN_POINT ( 'NONE',  ( 11.27234208742519783, -4.554746427620499638, -8.372004648554700168 ) ) ;
#40004 = CARTESIAN_POINT ( 'NONE',  ( 17.90980607984480244, 0.5146431972870012528, -12.68596244101704151 ) ) ;
#40005 = FACE_OUTER_BOUND ( 'NONE', #11401, .T. ) ;
#40006 = VERTEX_POINT ( 'NONE', #8522 ) ;
#40007 = CARTESIAN_POINT ( 'NONE',  ( 8.666729817973333638, -2.899999999999999911, 6.535479089440332956 ) ) ;
#40008 = B_SPLINE_CURVE_WITH_KNOTS ( 'NONE', 3,
 ( #60171, #12276, #7023, #65746 ),
 .UNSPECIFIED., .F., .F.,
 ( 4, 4 ),
 ( 0.000000000000000000, 1.000000000000000000 ),
 .UNSPECIFIED. ) ;
#40009 = CARTESIAN_POINT ( 'NONE',  ( 18.17607324740604824, -2.571217238407994987, -13.65805047069065381 ) ) ;
#40010 = CARTESIAN_POINT ( 'NONE',  ( 18.02726358178263766, -2.088564957048818727, 13.75219797955875123 ) ) ;
#40011 = ORIENTED_EDGE ( 'NONE', *, *, #56523, .F. ) ;
#40012 = VECTOR ( 'NONE', #21139, 1000.000000000000000 ) ;
#40013 = CARTESIAN_POINT ( 'NONE',  ( 10.48734600210000067, 4.351287276768000645, -6.182257940481999725 ) ) ;
#40014 = CARTESIAN_POINT ( 'NONE',  ( 10.10000000000000142, 0.000000000000000000, 0.000000000000000000 ) ) ;
#40015 = ORIENTED_EDGE ( 'NONE', *, *, #67162, .F. ) ;
#40016 = CARTESIAN_POINT ( 'NONE',  ( 9.202051052051999136, 5.120555153167999585, 7.280704316743199733 ) ) ;
#40017 = CARTESIAN_POINT ( 'NONE',  ( 18.21592075161434465, -2.776565552903150103, -12.29027267990593231 ) ) ;
#40018 = CARTESIAN_POINT ( 'NONE',  ( 9.477263540182331525, 3.370476274536374106, 6.407767014557177454 ) ) ;
#40019 = CARTESIAN_POINT ( 'NONE',  ( 23.89320776801300283, 2.594336453666000075, 11.06325219639999347 ) ) ;
#40020 = EDGE_CURVE ( 'NONE', #4182, #9109, #19703, .T. ) ;
#40021 = EDGE_CURVE ( 'NONE', #9159, #17467, #25632, .T. ) ;
#40022 = CARTESIAN_POINT ( 'NONE',  ( 17.55505043854144276, 0.7302158263239086899, 13.98094363220831049 ) ) ;
#40023 = EDGE_CURVE ( 'NONE', #60967, #25005, #66896, .T. ) ;
#40024 = EDGE_CURVE ( 'NONE', #53988, #58219, #40676, .T. ) ;
#40025 = CARTESIAN_POINT ( 'NONE',  ( 9.406895376471270609, -2.504060814039583249, 8.387610628396673818 ) ) ;
#40026 = EDGE_LOOP ( 'NONE', ( #58040, #14456, #51779, #5049 ) ) ;
#40027 = CARTESIAN_POINT ( 'NONE',  ( 24.53428985367600390, -3.614319203926000146, 12.31267510079000083 ) ) ;
#40028 = CARTESIAN_POINT ( 'NONE',  ( 10.67529528041000120, 3.066676902634999813, -8.703232886886000941 ) ) ;
#40029 = CARTESIAN_POINT ( 'NONE',  ( 10.21685100254000034, 2.832432432432000269, 6.822293592207000934 ) ) ;
#40030 = CARTESIAN_POINT ( 'NONE',  ( 12.14279580514167023, 2.220721880347445332, -13.82275356517831888 ) ) ;
#40031 = CARTESIAN_POINT ( 'NONE',  ( 9.912329965421998068, -4.888489908445900589, -8.420309768537698858 ) ) ;
#40032 = CARTESIAN_POINT ( 'NONE',  ( 10.12549839661999940, -5.788806995403000144, 7.335561828691000485 ) ) ;
#40033 = CARTESIAN_POINT ( 'NONE',  ( 18.08578335600534714, 0.3302328523437053631, 13.89472426752322853 ) ) ;
#40034 = CARTESIAN_POINT ( 'NONE',  ( 7.847544949947995008, 5.056324060593960112, 6.597935295888344598 ) ) ;
#40035 = ORIENTED_EDGE ( 'NONE', *, *, #324, .F. ) ;
#40036 = ORIENTED_EDGE ( 'NONE', *, *, #35828, .F. ) ;
#40037 = CARTESIAN_POINT ( 'NONE',  ( 9.485829719593997567, 4.953415418491999844, -8.946479654552000227 ) ) ;
#40038 = CARTESIAN_POINT ( 'NONE',  ( 0.000000000000000000, 5.100000000000000533, 7.500000000000000000 ) ) ;
#40039 = CARTESIAN_POINT ( 'NONE',  ( 7.454905163714801830, -5.316162339229765443, 7.145932548772795379 ) ) ;
#40040 = CARTESIAN_POINT ( 'NONE',  ( 9.270843198681054886, -5.086512213758866530, 8.869463831023999489 ) ) ;
#40041 = EDGE_CURVE ( 'NONE', #63209, #9530, #28168, .T. ) ;
#40043 = CARTESIAN_POINT ( 'NONE',  ( 24.13681596746900127, 9.106586331126999667, -8.984417095254999097 ) ) ;
#40042 = APPLICATION_CONTEXT ( 'automotive_design' ) ;
#40044 = CARTESIAN_POINT ( 'NONE',  ( 10.32055864497999842, 4.682585200569199912, -8.034587760591801242 ) ) ;
#40046 = CARTESIAN_POINT ( 'NONE',  ( 11.01815802025999957, -5.555209496388000545, 4.991732544280999662 ) ) ;
#40045 = CARTESIAN_POINT ( 'NONE',  ( 9.777088727410999880, -5.137817193984000497, 7.404572115919599185 ) ) ;
#40047 = CARTESIAN_POINT ( 'NONE',  ( 10.46166951222540753, 5.351570712698046961, 7.263306442112579475 ) ) ;
#40048 = VERTEX_POINT ( 'NONE', #30203 ) ;
#40049 = CARTESIAN_POINT ( 'NONE',  ( 10.56717786912000001, -2.828865965284999895, 4.740087349777999393 ) ) ;
#40050 = AXIS2_PLACEMENT_3D ( 'NONE', #26868, #27206, #21946 ) ;
#40051 = CARTESIAN_POINT ( 'NONE',  ( 24.35365242081699932, -12.20235406300999514, -3.288253180468997172 ) ) ;
#40052 = CARTESIAN_POINT ( 'NONE',  ( 18.11112283403659262, 0.2853680816562754741, 12.69568625917503013 ) ) ;
#40053 = CARTESIAN_POINT ( 'NONE',  ( 12.18002295456098594, -0.03981407404452855930, 12.70000161046437981 ) ) ;
#40054 = VECTOR ( 'NONE', #3323, 1000.000000000000114 ) ;
#40055 = CARTESIAN_POINT ( 'NONE',  ( 17.96892410185106215, -2.968447989615301985, -12.32999203180362180 ) ) ;
#40056 = ORIENTED_EDGE ( 'NONE', *, *, #14606, .T. ) ;
#40058 = CARTESIAN_POINT ( 'NONE',  ( 7.936034956448000166, 3.387779868797000216, -6.294138482426000714 ) ) ;
#40057 = DIRECTION ( 'NONE',  ( 1.000000000000000000, 0.000000000000000000, 0.000000000000000000 ) ) ;
#40059 = CARTESIAN_POINT ( 'NONE',  ( 8.795585841232000490, 5.251032986819000214, -6.070151079272999795 ) ) ;
#40060 = CARTESIAN_POINT ( 'NONE',  ( 17.55505043854143565, 1.875000000000000000, 12.57541666120756041 ) ) ;
#40061 = CARTESIAN_POINT ( 'NONE',  ( 8.493356027204001180, -5.097500218784999149, 6.607661537772998805 ) ) ;
#40062 = CARTESIAN_POINT ( 'NONE',  ( 24.44496356232399847, -3.224881240379999792, -12.03535804424000055 ) ) ;
#40063 = ADVANCED_FACE ( 'NONE', ( #51177 ), #46034, .T. ) ;
#40064 = CARTESIAN_POINT ( 'NONE',  ( 8.603645510037827293, -4.706833859777778351, 5.918599468013924891 ) ) ;
#40065 = CARTESIAN_POINT ( 'NONE',  ( 3.172249383735999739, -0.9192862011598000871, 3.644624677705999627 ) ) ;
#40066 = ORIENTED_EDGE ( 'NONE', *, *, #9483, .T. ) ;
#40067 = CARTESIAN_POINT ( 'NONE',  ( 12.27431907826859714, -0.3302353423713667580, -12.69422546839061461 ) ) ;
#40068 = CARTESIAN_POINT ( 'NONE',  ( 7.783734131047877369, -2.886512552566496748, 6.705439129923228769 ) ) ;
#40069 = EDGE_CURVE ( 'NONE', #46988, #63961, #27787, .T. ) ;
#40070 = CARTESIAN_POINT ( 'NONE',  ( 24.03569461241779237, -12.65453166998849177, -3.444226028244401494 ) ) ;
#40071 = CARTESIAN_POINT ( 'NONE',  ( 7.422239158771000156, 5.361039412362000434, 6.973453640356000349 ) ) ;
#40072 = CARTESIAN_POINT ( 'NONE',  ( 13.60016906737400078, -1.856292897172999960E-13, -4.263256414560999963E-14 ) ) ;
#40073 = ORIENTED_EDGE ( 'NONE', *, *, #54615, .T. ) ;
#40074 = CARTESIAN_POINT ( 'NONE',  ( 6.551836143767999943, 1.130384497037000058, -0.3246714051208999807 ) ) ;
#40075 = CARTESIAN_POINT ( 'NONE',  ( 7.689485841227000407, 4.413443707129999893, -8.834960942136000028 ) ) ;
#40077 = FACE_OUTER_BOUND ( 'NONE', #11058, .T. ) ;
#40076 = CARTESIAN_POINT ( 'NONE',  ( 11.09999999999999964, -5.599999999999999645, -6.571291218949999902 ) ) ;
#40078 = CONICAL_SURFACE ( 'NONE', #991, 13.94234653057000095, 1.233427434088239627 ) ;
#40079 = CARTESIAN_POINT ( 'NONE',  ( 10.17349413291699811, 5.162701151235999930, 8.030511425625498134 ) ) ;
#40080 = CARTESIAN_POINT ( 'NONE',  ( 10.64914416493166449, -4.811858819934198728, -7.823998238890133905 ) ) ;
#40081 = ORIENTED_EDGE ( 'NONE', *, *, #38171, .T. ) ;
#40082 = CARTESIAN_POINT ( 'NONE',  ( 11.09424907396999949, -2.431867116603999790, 7.769513708858000633 ) ) ;
#40083 = EDGE_LOOP ( 'NONE', ( #50, #35454, #26728, #8093 ) ) ;
#40084 = CARTESIAN_POINT ( 'NONE',  ( 15.90003771078200145, -3.695138809391000034, -11.25918926437999978 ) ) ;
#40085 = CARTESIAN_POINT ( 'NONE',  ( 8.598668146794999245, -2.376522687267000222, 7.686981355459999499 ) ) ;
#40086 = CARTESIAN_POINT ( 'NONE',  ( 18.08442884140762175, -0.4994936913945470236, -13.99109680828866864 ) ) ;
#40087 = VERTEX_POINT ( 'NONE', #11263 ) ;
#40088 = CARTESIAN_POINT ( 'NONE',  ( 10.98926421552158317, 7.704176194080371687, -6.385256007597936545 ) ) ;
#40089 = CARTESIAN_POINT ( 'NONE',  ( 25.29989727901499919, -2.078227429405999693, -11.31065739696999906 ) ) ;
#40090 = CARTESIAN_POINT ( 'NONE',  ( 17.55505043854147118, -3.125000000000000000, 13.52084414783465860 ) ) ;
#40091 = CARTESIAN_POINT ( 'NONE',  ( 25.39409999158950271, 8.421103250990364941, -8.066018968039331938 ) ) ;
#40092 = CARTESIAN_POINT ( 'NONE',  ( 11.57299956498199833, -2.792989229543000107, 7.174999999999999822 ) ) ;
#40093 = EDGE_LOOP ( 'NONE', ( #35841, #55042, #21824, #67714 ) ) ;
#40094 = CARTESIAN_POINT ( 'NONE',  ( 9.595487457706001422, -3.928425191288000384, 5.531324308465000783 ) ) ;
#40095 = CARTESIAN_POINT ( 'NONE',  ( 12.37676482144654955, -2.955308392773306814, -13.56622858938219522 ) ) ;
#40096 = DIRECTION ( 'NONE',  ( 1.000000000000000000, 0.000000000000000000, 0.000000000000000000 ) ) ;
#40097 = CARTESIAN_POINT ( 'NONE',  ( 12.35647036338150606, -1.936369888838089137, 13.86561402904640161 ) ) ;
#40098 = ORIENTED_EDGE ( 'NONE', *, *, #60051, .F. ) ;
#40099 = FACE_OUTER_BOUND ( 'NONE', #64236, .T. ) ;
#40100 = CARTESIAN_POINT ( 'NONE',  ( 10.90987534547535098, 2.900005126128452737, 5.097495377258621119 ) ) ;
#40101 = CARTESIAN_POINT ( 'NONE',  ( 6.881640499830017355, 5.514763025938938412, -8.366926484462830160 ) ) ;
#40102 = CARTESIAN_POINT ( 'NONE',  ( 10.05333291544899943, -3.468906853242414989, -8.658936933361781385 ) ) ;
#40103 = CARTESIAN_POINT ( 'NONE',  ( 9.679055905794999859, -2.899999999999999911, 6.571291218949999902 ) ) ;
#40104 = AXIS2_PLACEMENT_3D ( 'NONE', #13569, #43999, #27920 ) ;
#40105 = CARTESIAN_POINT ( 'NONE',  ( 12.27985112600388717, 0.3389646381316557822, -13.89444110642640773 ) ) ;
#40106 = EDGE_CURVE ( 'NONE', #12254, #1557, #36941, .T. ) ;
#40108 = EDGE_CURVE ( 'NONE', #3750, #66643, #46974, .T. ) ;
#40107 = CARTESIAN_POINT ( 'NONE',  ( 18.14833460798325859, -2.303170370814867862, 12.49527837666171415 ) ) ;
#40109 = ORIENTED_EDGE ( 'NONE', *, *, #16089, .T. ) ;
#40110 = CARTESIAN_POINT ( 'NONE',  ( 11.31900581613029821, -3.249313226592100534, -7.982035256002799173 ) ) ;
#40111 = ORIENTED_EDGE ( 'NONE', *, *, #64901, .F. ) ;
#40112 = CARTESIAN_POINT ( 'NONE',  ( 17.55505043854143565, 1.875000000000000000, 13.78627172894481667 ) ) ;
#40113 = CARTESIAN_POINT ( 'NONE',  ( 9.974220280410998285, 5.496789211521000418, -7.043125396300999874 ) ) ;
#40114 = CARTESIAN_POINT ( 'NONE',  ( 3.048079248832999966, -2.851054910039999779, 1.814310612331999861 ) ) ;
#40115 = CARTESIAN_POINT ( 'NONE',  ( 10.99479839230999900, -3.850614833844999918, -9.347951988117998212 ) ) ;
#40116 = PLANE ( 'NONE',  #30557 ) ;
#40117 = CARTESIAN_POINT ( 'NONE',  ( 9.008370456395944359, -5.237385890216453177, 8.039653529976170887 ) ) ;
#40118 = ORIENTED_EDGE ( 'NONE', *, *, #59738, .F. ) ;
#40119 = CARTESIAN_POINT ( 'NONE',  ( 11.88379707368349969, -4.566644629509899467, 8.490052513816499058 ) ) ;
#40120 = CARTESIAN_POINT ( 'NONE',  ( 9.972850246170999355, 5.044468801812000081, 6.258104779495000436 ) ) ;
#40121 = CARTESIAN_POINT ( 'NONE',  ( 18.49996808500599954, -1.807259461627081842, -11.54438823547436499 ) ) ;
#40122 = EDGE_CURVE ( 'NONE', #3478, #51145, #21089, .T. ) ;
#40123 = DIRECTION ( 'NONE',  ( -0.8660254037844288266, 0.000000000000000000, 0.5000000000000169864 ) ) ;
#40124 = B_SPLINE_CURVE_WITH_KNOTS ( 'NONE', 3,
 ( #62022, #9215, #41387, #14817 ),
 .UNSPECIFIED., .F., .F.,
 ( 4, 4 ),
 ( 0.000000000000000000, 1.000000000000000000 ),
 .UNSPECIFIED. ) ;
#40126 = CARTESIAN_POINT ( 'NONE',  ( 9.211683426218488790, 2.668681544687872886, 7.727204560920537979 ) ) ;
#40125 = CARTESIAN_POINT ( 'NONE',  ( 11.11845610223999969, 5.767025078915000158, 7.178418469370999588 ) ) ;
#40127 = CARTESIAN_POINT ( 'NONE',  ( 11.26072066707849828, 4.976067344118500380, -6.909591111168198907 ) ) ;
#40128 = DIRECTION ( 'NONE',  ( 0.000000000000000000, 0.4998826579293298988, -0.8660931406618509465 ) ) ;
#40129 = CARTESIAN_POINT ( 'NONE',  ( 10.28824205624999877, 3.639798001706899822, -8.437601616732200327 ) ) ;
#40130 = CARTESIAN_POINT ( 'NONE',  ( 17.57900174287143358, -0.7192906882580816230, 12.57945229568000478 ) ) ;
#40131 = DIRECTION ( 'NONE',  ( -0.000000000000000000, 0.7916053084224905501, 0.6110327615417471270 ) ) ;
#40132 = CARTESIAN_POINT ( 'NONE',  ( 8.109941913477543451, 5.060294156615178451, -6.518531832221441391 ) ) ;
#40133 = PLANE ( 'NONE',  #27669 ) ;
#40134 = ORIENTED_EDGE ( 'NONE', *, *, #14218, .F. ) ;
#40135 = CARTESIAN_POINT ( 'NONE',  ( 7.475043146792000215, -3.276313010012999793, 5.841993238691999935 ) ) ;
#40136 = CARTESIAN_POINT ( 'NONE',  ( 18.11095118117829728, 2.049130080444090396, 13.84922935676121902 ) ) ;
#40137 = CARTESIAN_POINT ( 'NONE',  ( 23.57793118131190724, 3.116419977577632672, 13.63419877650960821 ) ) ;
#40138 = CARTESIAN_POINT ( 'NONE',  ( 24.30000000000000071, -8.810505093353000916, -8.810505093353000916 ) ) ;
#40139 = ORIENTED_EDGE ( 'NONE', *, *, #3319, .T. ) ;
#40140 = CARTESIAN_POINT ( 'NONE',  ( 8.449239158774000558, 5.458692773671000253, 7.456452194274000078 ) ) ;
#40141 = CARTESIAN_POINT ( 'NONE',  ( 0.7886440402156557061, -3.499437203200495894, 0.5186531736757357125 ) ) ;
#40143 = B_SPLINE_CURVE_WITH_KNOTS ( 'NONE', 3,
 ( #65052, #38501, #50729, #66801 ),
 .UNSPECIFIED., .F., .F.,
 ( 4, 4 ),
 ( 0.000000000000000000, 1.000000000000000000 ),
 .UNSPECIFIED. ) ;
#40142 = CARTESIAN_POINT ( 'NONE',  ( 4.599999999999999645, -1.787797342887044394, -13.88538010501570952 ) ) ;
#40144 = ORIENTED_EDGE ( 'NONE', *, *, #38309, .T. ) ;
#40145 = CARTESIAN_POINT ( 'NONE',  ( 8.649445371194000032, 5.100000000000000533, -6.459601070175000181 ) ) ;
#40146 = CARTESIAN_POINT ( 'NONE',  ( 9.234799632564795857, -4.972103827131938658, -6.117919078289220103 ) ) ;
#40147 = CARTESIAN_POINT ( 'NONE',  ( 10.79303032197930001, 4.663532080728800544, 8.427909097977700270 ) ) ;
#40148 = ADVANCED_FACE ( 'NONE', ( #6014 ), #67181, .T. ) ;
#40149 = CARTESIAN_POINT ( 'NONE',  ( 11.20563089100999932, -3.509133048232999652, 6.118191305996999674 ) ) ;
#40150 = CARTESIAN_POINT ( 'NONE',  ( 9.947288403111267385, 2.899999999999999911, 6.305985889562331970 ) ) ;
#40151 = ORIENTED_EDGE ( 'NONE', *, *, #6375, .F. ) ;
#40152 = CARTESIAN_POINT ( 'NONE',  ( 11.80707028823900195, -3.411567914393000223, 11.89801974982000132 ) ) ;
#40153 = CARTESIAN_POINT ( 'NONE',  ( 10.87946694038000039, -2.817416132545000007, -6.828662897514999663 ) ) ;
#40154 = CARTESIAN_POINT ( 'NONE',  ( 7.963612997803560134, -2.289570113972569487, 7.184898621721505840 ) ) ;
#40155 = CARTESIAN_POINT ( 'NONE',  ( 9.600494040286998043, -5.206548117663999165, 8.585114612872999373 ) ) ;
#40156 = CARTESIAN_POINT ( 'NONE',  ( 10.68035971519489813, -3.321859513918399731, -6.371865185335000348 ) ) ;
#40157 = CARTESIAN_POINT ( 'NONE',  ( 10.53791290906799993, -4.722468360609500593, 6.615820196229499572 ) ) ;
#40158 = ORIENTED_EDGE ( 'NONE', *, *, #33791, .T. ) ;
#40159 = CARTESIAN_POINT ( 'NONE',  ( 18.50001572531400029, -2.908166856580999937, 12.18270046149000052 ) ) ;
#40160 = B_SPLINE_CURVE_WITH_KNOTS ( 'NONE', 3,
 ( #22001, #63623, #15739, #47904 ),
 .UNSPECIFIED., .F., .F.,
 ( 4, 4 ),
 ( 0.000000000000000000, 1.000000000000000000 ),
 .UNSPECIFIED. ) ;
#40161 = CARTESIAN_POINT ( 'NONE',  ( 11.58425954179440076, -3.017023678917100327, 6.683254058608399717 ) ) ;
#40162 = VERTEX_POINT ( 'NONE', #37837 ) ;
#40163 = CARTESIAN_POINT ( 'NONE',  ( 12.80505043854146940, -3.125000000000000000, 12.28374638332999780 ) ) ;
#40164 = EDGE_LOOP ( 'NONE', ( #41902, #12358, #1996, #63450 ) ) ;
#40165 = CARTESIAN_POINT ( 'NONE',  ( 9.441140818749000019, -4.011292643094999555, -9.373220388412001114 ) ) ;
#40166 = CARTESIAN_POINT ( 'NONE',  ( 8.953620280414000376, 2.881930053949999682, -8.823338183322999129 ) ) ;
#40167 = CARTESIAN_POINT ( 'NONE',  ( 13.99999999231800096, -8.833253877201999060, -7.896562762484000686 ) ) ;
#40168 = DIRECTION ( 'NONE',  ( 1.000000000000000000, 0.000000000000000000, 0.000000000000000000 ) ) ;
#40169 = CARTESIAN_POINT ( 'NONE',  ( 12.36861073370954323, 2.947405515254781783, -12.33600917780097284 ) ) ;
#40170 = CARTESIAN_POINT ( 'NONE',  ( 11.14949279009019989, -4.260984538213099526, 6.531063508962500208 ) ) ;
#40171 = CARTESIAN_POINT ( 'NONE',  ( 11.65278751119019951, -4.790480620979200133, 7.086443476450299706 ) ) ;
#40172 = ORIENTED_EDGE ( 'NONE', *, *, #51829, .T. ) ;
#40173 = CARTESIAN_POINT ( 'NONE',  ( 7.572781938258273726, 4.464961194226365393, 8.785435224012646316 ) ) ;
#40174 = CARTESIAN_POINT ( 'NONE',  ( 8.406105646793999853, -5.342173944271999986, 8.432314172168000610 ) ) ;
#40175 = DIRECTION ( 'NONE',  ( -1.000000000000000000, 0.000000000000000000, 0.000000000000000000 ) ) ;
#40176 = ORIENTED_EDGE ( 'NONE', *, *, #50265, .T. ) ;
#40177 = B_SPLINE_SURFACE_WITH_KNOTS ( 'NONE', 1, 3, ( 
 ( #58075, #31175, #62954, #68201, #41309, #21351, #21013, #20320, #52479, #4575, #42350, #20668, #62618, #4925, #31506, #14740, #41994, #42679, #63301, #15428, #26261, #53169, #41647, #63988, #15767, #36059, #37096, #58409, #26610, #16104, #5271, #58752, #32204, #57374, #53517, #26952, #67866, #52132, #46898, #48264, #43022, #1069, #65015, #6646, #44423, #65721, #54549, #37774, #27987, #49647, #65372, #27640, #55242, #32539, #64324, #11539, #43378, #17493, #38817, #60143, #12249, #33575, #32882, #64678, #7339, #1753, #38468, #23074, #1408, #54895, #17133, #49296, #48960, #22380, #16785, #371, #59100, #60485, #6995, #59788, #28327, #6295, #17845, #21688, #38114, #22724, #39162, #12594, #16446, #44071, #43721, #33922, #33231, #11202, #53854, #5953, #27294, #48618, #719, #22031, #59439, #54193, #11890, #66759 ),
 ( #55591, #39507, #19207, #13635, #56277, #61856, #61178, #45785, #7693, #2110, #45103, #46126, #3465, #24112, #67433, #62199, #40531, #40202, #60831, #3129, #29035, #67097, #56957, #13977, #61520, #24461, #19557, #35645, #8723, #18875, #39858, #50344, #2444, #34271, #24801, #13298, #23768, #12944, #28682, #55935, #18531, #8384, #35302, #66412, #45446, #8037, #30066, #34960, #34622, #29377, #50689, #23427, #51369, #29726, #2786, #51030, #56618, #40879, #14320, #44765, #49999, #66066, #18185, #57635, #31770, #31088, #68120, #20580, #35973, #47504, #37349, #42265, #41906, #4835, #69160, #16020, #58327, #68457, #20239, #30736, #57287, #14657, #53087, #62873, #9390, #41225, #9059, #36318, #41564, #36670, #68808, #4147, #25828, #9740, #10428, #63212, #14992, #25487, #52044, #51706, #5187, #10090, #46814, #52396 ) ),
 .UNSPECIFIED., .F., .F., .F.,
 ( 2, 2 ),
 ( 4, 2, 2, 2, 2, 2, 2, 2, 2, 2, 2, 2, 2, 2, 2, 2, 2, 2, 2, 2, 2, 2, 2, 2, 2, 2, 2, 2, 2, 2, 2, 2, 2, 2, 2, 2, 2, 2, 2, 2, 2, 2, 2, 2, 2, 2, 2, 2, 2, 2, 2, 4 ),
 ( 0.000000000000000000, 1.000000000000000000 ),
 ( 0.000000000000000000, 7.157624699936001862E-05, 0.0001431524939987200372, 0.0002147287409980800559, 0.0002326228027479200402, 0.0002505168644977600516, 0.0002863049879974400745, 0.0003220931114971200973, 0.0003578812349968001202, 0.0003936693584964801431, 0.0004294574819961601117, 0.0004652456054958400804, 0.0005010337289955201032, 0.0005368218524952001261, 0.0005726099759948801490, 0.0006441862229942401947, 0.0006799743464939202175, 0.0007157624699936002404, 0.0007336565317434402518, 0.0007515505934932802633, 0.0007873387169929602861, 0.0008589149639923202234, 0.0008947030874920001379, 0.0009304912109916801607, 0.0009662793344913601836, 0.001002067457991040206, 0.001073643704990400252, 0.001145219951989760298, 0.001216796198989120344, 0.001288372445988480389, 0.001359948692987840435, 0.001395736816487520458, 0.001431524939987200481, 0.001467313063486880504, 0.001503101186986560527, 0.001574677433985920572, 0.001646253680985280618, 0.001682041804484960424, 0.001717829927984640447, 0.001735723989734480350, 0.001753618051484320470, 0.001789406174984000276, 0.001860982421983360321, 0.001896770545483040344, 0.001932558668982720367, 0.001968346792482400173, 0.001986240854232240293, 0.002004134915982080413, 0.002075711162981440459, 0.002147287409980800504, 0.002218863656980160550, 0.002290439903979520596 ),
 .UNSPECIFIED. ) ;
#40178 = CARTESIAN_POINT ( 'NONE',  ( 12.27207149905419925, -1.992391748285590181, -12.44148121715491584 ) ) ;
#40179 = CARTESIAN_POINT ( 'NONE',  ( 10.23103300763299828, 4.692441239783899931, 6.773725604892799623 ) ) ;
#40180 = CARTESIAN_POINT ( 'NONE',  ( 10.05463185321000097, -3.531218470783999752, -9.119231780812000920 ) ) ;
#40181 = CARTESIAN_POINT ( 'NONE',  ( 6.799999999999923439, 5.456597484868973780, -8.185422748483164312 ) ) ;
#40182 = CARTESIAN_POINT ( 'NONE',  ( 17.76385332268500150, -3.526697956045000026, -11.96114712952999959 ) ) ;
#40183 = CARTESIAN_POINT ( 'NONE',  ( 24.36504260833099877, -8.917410148446000662, 9.042893056734001789 ) ) ;
#40184 = CARTESIAN_POINT ( 'NONE',  ( 12.37622832409311791, -2.954798090471129068, -13.56635979911537859 ) ) ;
#40185 = CARTESIAN_POINT ( 'NONE',  ( 17.66769993992418364, -0.6148490057825423127, -12.67995724530760526 ) ) ;
#40186 = CARTESIAN_POINT ( 'NONE',  ( 7.856038276909000473, 2.869044596334999753, -6.744487387516000076 ) ) ;
#40187 = CARTESIAN_POINT ( 'NONE',  ( 10.54272335273199879, -3.555125495332600138, -8.698083075453000745 ) ) ;
#40188 = EDGE_CURVE ( 'NONE', #67955, #46460, #29406, .T. ) ;
#40190 = EDGE_CURVE ( 'NONE', #37746, #5733, #48676, .T. ) ;
#40189 = CARTESIAN_POINT ( 'NONE',  ( 8.616995677562000466, -4.876077402042000131, 5.996974966533000106 ) ) ;
#40191 = ORIENTED_EDGE ( 'NONE', *, *, #9016, .F. ) ;
#40192 = ORIENTED_EDGE ( 'NONE', *, *, #23041, .F. ) ;
#40193 = CARTESIAN_POINT ( 'NONE',  ( 8.492064203080353479, -4.378336071229006699, 5.973114860761890910 ) ) ;
#40194 = CARTESIAN_POINT ( 'NONE',  ( 8.058915628308520596, 4.678948124125482444, 8.679023822939951671 ) ) ;
#40195 = CARTESIAN_POINT ( 'NONE',  ( 10.88015784977000067, 2.793131772868000073, -6.864962922767000819 ) ) ;
#40196 = CARTESIAN_POINT ( 'NONE',  ( 13.49999720188826480, 11.61513859405367022, 2.353594668653353317 ) ) ;
#40197 = CARTESIAN_POINT ( 'NONE',  ( 17.57925770490771100, 3.199697828486423923, 12.18695748817155078 ) ) ;
#40198 = CYLINDRICAL_SURFACE ( 'NONE', #4859, 1.350000000000000089 ) ;
#40199 = DIRECTION ( 'NONE',  ( 1.000000000000000000, 0.000000000000000000, 0.000000000000000000 ) ) ;
#40200 = CARTESIAN_POINT ( 'NONE',  ( 8.050967101794888947, 5.350251359469498702, -7.263554191733096133 ) ) ;
#40201 = VERTEX_POINT ( 'NONE', #1127 ) ;
#40202 = CARTESIAN_POINT ( 'NONE',  ( 12.49885887340288981, -1.955044097548215509, 12.56200003178136448 ) ) ;
#40203 = CARTESIAN_POINT ( 'NONE',  ( 9.655013376692998861, -4.895413217368500547, -7.044942343771899651 ) ) ;
#40204 = CARTESIAN_POINT ( 'NONE',  ( 9.388624299788999039, 4.079402096444999515, 9.259357173634999327 ) ) ;
#40205 = EDGE_CURVE ( 'NONE', #36985, #15157, #65021, .T. ) ;
#40206 = DIRECTION ( 'NONE',  ( 0.000000000000000000, -1.000000000000000000, 0.000000000000000000 ) ) ;
#40207 = ADVANCED_FACE ( 'NONE', ( #63713 ), #26103, .F. ) ;
#40208 = CARTESIAN_POINT ( 'NONE',  ( 10.86687616594229944, 3.655053560864600204, -6.412662853391999818 ) ) ;
#40209 = CARTESIAN_POINT ( 'NONE',  ( 12.23574065127465182, 0.2580991232524050827, 12.69647497719789619 ) ) ;
#40210 = CARTESIAN_POINT ( 'NONE',  ( 8.315517219592001297, 5.485785046334999748, 8.532070739720001740 ) ) ;
#40211 = CARTESIAN_POINT ( 'NONE',  ( 9.385781899350000401, 4.980865465981000106, 6.433345686594999613 ) ) ;
#40212 = CARTESIAN_POINT ( 'NONE',  ( 12.61159012396487000, 1.905606515074949714, 12.57035430044310154 ) ) ;
#40213 = VERTEX_POINT ( 'NONE', #28396 ) ;
#40214 = CARTESIAN_POINT ( 'NONE',  ( 9.883629719592001095, 5.656948148960999845, -6.994239053114000626 ) ) ;
#40215 = CARTESIAN_POINT ( 'NONE',  ( 10.12841772631199966, 4.490588993294299947, -8.509834072393999804 ) ) ;
#40216 = CARTESIAN_POINT ( 'NONE',  ( 10.85106741697583210, -3.434344919155746023, 9.175967010814426672 ) ) ;
#40218 = CARTESIAN_POINT ( 'NONE',  ( 3.271725677054833525, -3.409621058607596567, -0.9125531287176791295 ) ) ;
#40217 = CARTESIAN_POINT ( 'NONE',  ( 7.892605646791999163, -5.480312458445999901, 8.192326492433998908 ) ) ;
#40219 = CARTESIAN_POINT ( 'NONE',  ( 10.43860887879199950, -4.227457260387500249, 8.478317686146800369 ) ) ;
#40220 = VECTOR ( 'NONE', #20555, 1000.000000000000000 ) ;
#40221 = CARTESIAN_POINT ( 'NONE',  ( 10.84641504065830020, -3.195537720350400068, -6.900173947321999179 ) ) ;
#40222 = EDGE_LOOP ( 'NONE', ( #58466, #4230, #19075, #38003, #66198, #15493 ) ) ;
#40223 = CARTESIAN_POINT ( 'NONE',  ( 2.381491312999000076, 2.737733327009000295, -2.100062873276000275 ) ) ;
#40224 = CARTESIAN_POINT ( 'NONE',  ( 17.88388243140133227, -0.5319787654676457755, -12.68500714331955237 ) ) ;
#40225 = CARTESIAN_POINT ( 'NONE',  ( 9.310863317747999801, -3.039136629551499880, 7.499999999926881600 ) ) ;
#40226 = CARTESIAN_POINT ( 'NONE',  ( 7.000000000000000888, -6.725378844700938608, 3.045375366903437797 ) ) ;
#40227 = CARTESIAN_POINT ( 'NONE',  ( 8.731616107288068918, 4.000002263255227675, -8.381579007094499545 ) ) ;
#40228 = CARTESIAN_POINT ( 'NONE',  ( 17.75799838104448369, -1.908512137131851416, -13.78121285638385807 ) ) ;
#40229 = CARTESIAN_POINT ( 'NONE',  ( 12.80505043854144276, -0.6250000000000001110, -25.00000000000000000 ) ) ;
#40230 = CARTESIAN_POINT ( 'NONE',  ( 17.55505043854144276, 0.000000000000000000, -25.00000000000000000 ) ) ;
#40231 = FACE_OUTER_BOUND ( 'NONE', #34161, .T. ) ;
#40232 = VERTEX_POINT ( 'NONE', #2172 ) ;
#40233 = CARTESIAN_POINT ( 'NONE',  ( 9.138573341230998182, 2.933833973450999721, 8.496479443567000800 ) ) ;
#40234 = FACE_OUTER_BOUND ( 'NONE', #60377, .T. ) ;
#40235 = CARTESIAN_POINT ( 'NONE',  ( 21.70000133425200062, 0.000000000000000000, 0.000000000000000000 ) ) ;
#40236 = CARTESIAN_POINT ( 'NONE',  ( 17.63676827353077314, -0.6210358159598048378, 13.88132258802016494 ) ) ;
#40237 = CARTESIAN_POINT ( 'NONE',  ( 0.6624568971868999290, 2.744051942617999895, -1.815777288092999875 ) ) ;
#40238 = ORIENTED_EDGE ( 'NONE', *, *, #32070, .T. ) ;
#40239 = CARTESIAN_POINT ( 'NONE',  ( 11.59999999999999964, 5.179498027601999510, 7.825000000000000178 ) ) ;
#40240 = CARTESIAN_POINT ( 'NONE',  ( 11.03105082652855984, -2.697932356969752199, -8.692104167685684502 ) ) ;
#40241 = CARTESIAN_POINT ( 'NONE',  ( 10.70441484796999987, 3.444517850837000239, 6.009055070331999815 ) ) ;
#40242 = CARTESIAN_POINT ( 'NONE',  ( 11.11718313518939816, 3.377550038693600154, 6.712912394634500401 ) ) ;
#40243 = CARTESIAN_POINT ( 'NONE',  ( 9.537173706499428860, -4.215401811041904701, 8.849618031277087127 ) ) ;
#40244 = CARTESIAN_POINT ( 'NONE',  ( 9.365000000002998704, -2.649999999999999911, -7.500000000000000000 ) ) ;
#40245 = CARTESIAN_POINT ( 'NONE',  ( 4.600000127571202135, 3.375077994860000042E-14, 1.048050535245999973E-13 ) ) ;
#40246 = DIRECTION ( 'NONE',  ( -1.000000000000000000, 0.000000000000000000, 0.000000000000000000 ) ) ;
#40247 = CARTESIAN_POINT ( 'NONE',  ( 12.19400419524981238, -2.631361540944479049, 12.42001554595805857 ) ) ;
#40248 = CARTESIAN_POINT ( 'NONE',  ( 8.421727527370212130, 2.365161250210713995, 8.132627738500831427 ) ) ;
#40249 = EDGE_LOOP ( 'NONE', ( #3772, #6427 ) ) ;
#40250 = CARTESIAN_POINT ( 'NONE',  ( 17.81510163565847904, -1.931577867956977723, 13.77771208381435386 ) ) ;
#40251 = FACE_OUTER_BOUND ( 'NONE', #2417, .T. ) ;
#40252 = VERTEX_POINT ( 'NONE', #65780 ) ;
#40253 = ORIENTED_EDGE ( 'NONE', *, *, #9966, .T. ) ;
#40254 = CARTESIAN_POINT ( 'NONE',  ( 7.000000000000000000, -9.735955015381000166, 5.735955015381000166 ) ) ;
#40255 = CARTESIAN_POINT ( 'NONE',  ( 9.666846873516668381, 4.768183399968648040, -6.500416447002280051 ) ) ;
#40256 = CIRCLE ( 'NONE', #61455, 2.725000000000000089 ) ;
#40257 = CARTESIAN_POINT ( 'NONE',  ( 8.705629240797998492, -4.228941919214900480, -8.376522367004298530 ) ) ;
#40258 = CARTESIAN_POINT ( 'NONE',  ( 11.05639637898999972, 5.030226177531999632, 6.028288223959999748 ) ) ;
#40259 = CARTESIAN_POINT ( 'NONE',  ( 9.741003491525001223, 3.588532719919999892, -8.800216240366001585 ) ) ;
#40260 = CARTESIAN_POINT ( 'NONE',  ( 8.630000000000000782, 4.924138593003999809, -8.484107647018999998 ) ) ;
#40261 = CARTESIAN_POINT ( 'NONE',  ( 9.423521818475000700, -4.993993578306000103, 8.578110568283999982 ) ) ;
#40262 = CARTESIAN_POINT ( 'NONE',  ( 18.14418133822494283, 0.4193891200559174970, -12.59302195412780456 ) ) ;
#40263 = CARTESIAN_POINT ( 'NONE',  ( 10.40558062080000035, -5.599331384652000310, -8.437753779290000367 ) ) ;
#40264 = CARTESIAN_POINT ( 'NONE',  ( 11.19518313518939934, -4.537300658085600347, -8.179416362154199760 ) ) ;
#40265 = EDGE_CURVE ( 'NONE', #11589, #39123, #23722, .T. ) ;
#40267 = ADVANCED_FACE ( 'NONE', ( #33294, #7060 ), #60895, .T. ) ;
#40266 = PLANE ( 'NONE',  #3178 ) ;
#40269 = VERTEX_POINT ( 'NONE', #24177 ) ;
#40268 = B_SPLINE_CURVE_WITH_KNOTS ( 'NONE', 3,
 ( #65784, #13013, #34341, #23141, #59505, #11604, #17908, #55657, #39226, #50066, #55308, #23835 ),
 .UNSPECIFIED., .F., .F.,
 ( 4, 2, 2, 2, 2, 4 ),
 ( 0.000000000000000000, 0.06249999999999998612, 0.1249999999999999722, 0.2500000000000000000, 0.3750000000000000000, 0.5000000000000000000 ),
 .UNSPECIFIED. ) ;
#40270 = CIRCLE ( 'NONE', #77, 2.524999655449999825 ) ;
#40271 = CARTESIAN_POINT ( 'NONE',  ( 11.07204542438999972, -6.380876855756000054, -5.350213802198999780 ) ) ;
#40272 = ADVANCED_FACE ( 'NONE', ( #29097 ), #64643, .T. ) ;
#40273 = CARTESIAN_POINT ( 'NONE',  ( 24.70907584035216686, 8.654457188012020907, 8.608358926410405232 ) ) ;
#40274 = CARTESIAN_POINT ( 'NONE',  ( 9.075651506909604649, 5.234436409784954947, 7.432209138388947700 ) ) ;
#40275 = CARTESIAN_POINT ( 'NONE',  ( 9.152455549953000258, 4.995562869655000071, -6.696732323226999739 ) ) ;
#40276 = CARTESIAN_POINT ( 'NONE',  ( 12.08611717550374820, 2.614944066661588185, 13.75364144501312680 ) ) ;
#40277 = CARTESIAN_POINT ( 'NONE',  ( 10.70441271436000008, -3.444516450945999786, 6.009051312948000323 ) ) ;
#40278 = EDGE_LOOP ( 'NONE', ( #48463, #22899, #9992, #65517 ) ) ;
#40279 = CARTESIAN_POINT ( 'NONE',  ( 12.22418410610920247, -0.2308773532682540375, -12.69717962855014193 ) ) ;
#40280 = CARTESIAN_POINT ( 'NONE',  ( 12.80505043854144276, -0.6250000000000006661, 13.88107975066923316 ) ) ;
#40281 = VERTEX_POINT ( 'NONE', #15234 ) ;
#40282 = DIRECTION ( 'NONE',  ( 0.000000000000000000, 1.000000000000000000, 0.000000000000000000 ) ) ;
#40283 = CARTESIAN_POINT ( 'NONE',  ( 10.56819717210643361, -5.125396288428698988, -6.749639981086813734 ) ) ;
#40284 = CARTESIAN_POINT ( 'NONE',  ( 24.45265319665800163, -3.540849845907999782, -12.31960893685999991 ) ) ;
#40285 = DIRECTION ( 'NONE',  ( 1.000000000000000000, 0.000000000000000000, 0.000000000000000000 ) ) ;
#40286 = EDGE_CURVE ( 'NONE', #24623, #28630, #8577, .T. ) ;
#40287 = CARTESIAN_POINT ( 'NONE',  ( 8.615121458427411838, 5.349954800205006578, -7.499992720895565235 ) ) ;
#40288 = CARTESIAN_POINT ( 'NONE',  ( 0.2194555633787999838, -2.757152670777000214, 2.469952924947999673 ) ) ;
#40289 = CARTESIAN_POINT ( 'NONE',  ( 8.154130060498527399, 2.684642961096642022, 7.853228170896760396 ) ) ;
#40290 = CARTESIAN_POINT ( 'NONE',  ( 12.27385967125947097, 2.970546648634948994, 12.24484150081281086 ) ) ;
#40291 = CARTESIAN_POINT ( 'NONE',  ( 9.438732219486000830, -2.462132291381999849, -7.373611177161000008 ) ) ;
#40292 = CARTESIAN_POINT ( 'NONE',  ( 10.77672335273219950, 4.301522290735800169, -8.312023951944400579 ) ) ;
#40293 = CARTESIAN_POINT ( 'NONE',  ( 11.56833327354034857, 3.253412192327699959, -7.011667014989399149 ) ) ;
#40294 = CARTESIAN_POINT ( 'NONE',  ( 10.18988779216199880, 5.056118594996999782, -7.880862084500499520 ) ) ;
#40296 = CARTESIAN_POINT ( 'NONE',  ( 12.26155906745207602, 2.190709282217770948, 12.51827377313525780 ) ) ;
#40295 = CARTESIAN_POINT ( 'NONE',  ( 16.04720874474600123, -8.391565830097999168, -8.158729932893001191 ) ) ;
#40297 = DIRECTION ( 'NONE',  ( -1.000000000000000000, 0.000000000000000000, 0.000000000000000000 ) ) ;
#40298 = ORIENTED_EDGE ( 'NONE', *, *, #5087, .F. ) ;
#40299 = VECTOR ( 'NONE', #47842, 1000.000000000000000 ) ;
#40300 = CARTESIAN_POINT ( 'NONE',  ( 4.550000802215999229, 3.641531520771000148E-13, 3.197442310919999608E-14 ) ) ;
#40301 = CARTESIAN_POINT ( 'NONE',  ( 10.62197618263000010, -5.779779175739000685, 7.256573549370999743 ) ) ;
#40302 = CARTESIAN_POINT ( 'NONE',  ( 9.452380199233999747, 4.996570247675600207, 7.625259896924899472 ) ) ;
#40303 = CARTESIAN_POINT ( 'NONE',  ( 9.049596101582626062, 3.436622489763541122, -6.830568860986387492 ) ) ;
#40304 = CIRCLE ( 'NONE', #3461, 0.6999999999999992895 ) ;
#40305 = DIRECTION ( 'NONE',  ( 1.000000000000000000, 0.000000000000000000, 0.000000000000000000 ) ) ;
#40306 = CARTESIAN_POINT ( 'NONE',  ( 12.29692076506693965, 2.864061239608792331, 13.58942221845736853 ) ) ;
#40307 = CARTESIAN_POINT ( 'NONE',  ( 17.80000000009400196, -3.216307036143000175, -11.40341376487999980 ) ) ;
#40308 = ORIENTED_EDGE ( 'NONE', *, *, #5781, .F. ) ;
#40309 = CARTESIAN_POINT ( 'NONE',  ( 9.075405316139999456, -4.242421256336299962, -8.615780615741000403 ) ) ;
#40310 = DIRECTION ( 'NONE',  ( 0.000000000000000000, 0.2714570858282905341, 0.9624505444715651947 ) ) ;
#40311 = CARTESIAN_POINT ( 'NONE',  ( 18.03677854873447117, 1.942400312675097052, -12.44938339399086935 ) ) ;
#40312 = CARTESIAN_POINT ( 'NONE',  ( 11.05016464426000056, -2.767526642700999684, 5.012714206629000024 ) ) ;
#40313 = CARTESIAN_POINT ( 'NONE',  ( 0.7000000000000000666, 0.5773502691895999739, 1.000000000000000000 ) ) ;
#40314 = EDGE_CURVE ( 'NONE', #65865, #7350, #52763, .T. ) ;
#40315 = ADVANCED_FACE ( 'NONE', ( #26073 ), #60557, .F. ) ;
#40316 = CARTESIAN_POINT ( 'NONE',  ( 7.722357335211003537, 2.834201928695000650, 6.826641520477001457 ) ) ;
#40317 = CARTESIAN_POINT ( 'NONE',  ( 9.837330429757999539, -5.176458967229000230, -8.738385553646999426 ) ) ;
#40318 = CARTESIAN_POINT ( 'NONE',  ( 0.8738901325418791943, -2.150913519912200922, -2.798833948393631754 ) ) ;
#40319 = ORIENTED_EDGE ( 'NONE', *, *, #7036, .F. ) ;
#40320 = CARTESIAN_POINT ( 'NONE',  ( 17.74675502965012086, 3.228624035226697053, -13.62268076944971362 ) ) ;
#40321 = CARTESIAN_POINT ( 'NONE',  ( 12.75735126819566290, 0.7290235424212195836, -13.98100605002522734 ) ) ;
#40322 = CARTESIAN_POINT ( 'NONE',  ( 10.75304154458061312, 2.714670728013289569, 7.026954893539028468 ) ) ;
#40323 = DIRECTION ( 'NONE',  ( 0.000000000000000000, 0.7614089499631907509, -0.6482718649732929217 ) ) ;
#40324 = CARTESIAN_POINT ( 'NONE',  ( 2.811390132544666187, -3.500000000000000888, -0.4581489286485119217 ) ) ;
#40325 = FACE_OUTER_BOUND ( 'NONE', #8655, .T. ) ;
#40326 = CARTESIAN_POINT ( 'NONE',  ( 12.13825819896753977, -4.851203879749700576, 7.339530235223699073 ) ) ;
#40327 = ORIENTED_EDGE ( 'NONE', *, *, #50518, .T. ) ;
#40328 = CARTESIAN_POINT ( 'NONE',  ( 9.198378269148916431, -4.679948058550536416, -8.679637038427665985 ) ) ;
#40329 = CARTESIAN_POINT ( 'NONE',  ( 18.23515949175303064, 2.264077836046911596, -13.81573184862659431 ) ) ;
#40330 = ORIENTED_EDGE ( 'NONE', *, *, #54444, .F. ) ;
#40331 = CARTESIAN_POINT ( 'NONE',  ( 10.06068422951000052, -4.611171355610000688, 8.114961396014498618 ) ) ;
#40332 = CARTESIAN_POINT ( 'NONE',  ( 10.86501009699205866, -2.649983380499685737, -7.500000587580680111 ) ) ;
#40333 = CARTESIAN_POINT ( 'NONE',  ( 8.605545280412000508, 3.122811675949999977, -6.006064052396999919 ) ) ;
#40334 = CARTESIAN_POINT ( 'NONE',  ( 23.97711676181098639, -12.74913932280401063, 3.497788515081389882 ) ) ;
#40335 = CARTESIAN_POINT ( 'NONE',  ( 11.02301463001509774, -3.452642973349600464, -6.623338154204899908 ) ) ;
#40336 = CARTESIAN_POINT ( 'NONE',  ( 9.346315804487350221, -5.086028406228472853, -6.305450188067585060 ) ) ;
#40337 = CARTESIAN_POINT ( 'NONE',  ( 11.79999999684100054, -12.15995044155999949, -2.000340912084999978 ) ) ;
#40338 = ORIENTED_EDGE ( 'NONE', *, *, #42337, .F. ) ;
#40339 = CARTESIAN_POINT ( 'NONE',  ( 9.893930206848997599, 2.750000000000000000, -7.500000000000000000 ) ) ;
#40340 = DIRECTION ( 'NONE',  ( -0.7071067774168207087, 0.5091094021823148186, 0.4907215319718147839 ) ) ;
#40342 = EDGE_CURVE ( 'NONE', #33729, #21093, #4387, .T. ) ;
#40341 = CARTESIAN_POINT ( 'NONE',  ( 18.17590806569061002, -2.418078130838746453, 13.69056546384896755 ) ) ;
#40343 = ORIENTED_EDGE ( 'NONE', *, *, #33706, .T. ) ;
#40344 = CARTESIAN_POINT ( 'NONE',  ( 9.976690600124999975, 4.172224310749999887, -6.147156451669999910 ) ) ;
#40345 = CARTESIAN_POINT ( 'NONE',  ( 0.000000000000000000, 0.000000000000000000, 0.000000000000000000 ) ) ;
#40346 = EDGE_CURVE ( 'NONE', #12493, #29053, #11917, .T. ) ;
#40347 = ORIENTED_EDGE ( 'NONE', *, *, #25356, .F. ) ;
#40348 = CARTESIAN_POINT ( 'NONE',  ( 10.11188779216199940, 5.183207142131999845, 7.073306690476799830 ) ) ;
#40349 = CARTESIAN_POINT ( 'NONE',  ( 17.94652436847578869, -2.012680451140230975, -12.55183781965936340 ) ) ;
#40350 = CARTESIAN_POINT ( 'NONE',  ( 3.899999681170999821, 0.000000000000000000, 0.000000000000000000 ) ) ;
#40351 = AXIS2_PLACEMENT_3D ( 'NONE', #6466, #60647, #33397 ) ;
#40352 = CARTESIAN_POINT ( 'NONE',  ( 24.61098151538899970, -12.21941909980999874, -3.050810341055000041 ) ) ;
#40353 = CARTESIAN_POINT ( 'NONE',  ( 9.354552855434715042, -3.358379027116748183, 9.116748975407924505 ) ) ;
#40354 = EDGE_LOOP ( 'NONE', ( #14816, #39557, #25395, #47540 ) ) ;
#40355 = CARTESIAN_POINT ( 'NONE',  ( 24.30001694968100168, 3.271769180623000040, -12.21048179117000032 ) ) ;
#40356 = CARTESIAN_POINT ( 'NONE',  ( 9.921080006317001931, -4.920709323926390155, -9.006083254704995156 ) ) ;
#40357 = CARTESIAN_POINT ( 'NONE',  ( 11.09999999999999964, 0.5000000000000000000, -5.124965750789000296 ) ) ;
#40358 = CARTESIAN_POINT ( 'NONE',  ( 12.15287239299856559, 2.198919866763858089, -13.82623858331040267 ) ) ;
#40359 = CARTESIAN_POINT ( 'NONE',  ( 9.203113844318000503, -3.676949563211899807, -6.262250912840999106 ) ) ;
#40360 = CARTESIAN_POINT ( 'NONE',  ( 10.93227479887999998, -2.539880901735999785, 6.453614191797999666 ) ) ;
#40361 = EDGE_CURVE ( 'NONE', #32483, #47064, #21945, .T. ) ;
#40362 = CARTESIAN_POINT ( 'NONE',  ( 18.02418602114746093, 0.5568603909045788392, 13.98892293345219962 ) ) ;
#40363 = AXIS2_PLACEMENT_3D ( 'NONE', #21323, #31150, #4546 ) ;
#40364 = CARTESIAN_POINT ( 'NONE',  ( 10.93785547196599950, -2.862144528033999880, 6.360512911308666695 ) ) ;
#40365 = ORIENTED_EDGE ( 'NONE', *, *, #54536, .T. ) ;
#40366 = ORIENTED_EDGE ( 'NONE', *, *, #6042, .F. ) ;
#40367 = CARTESIAN_POINT ( 'NONE',  ( 8.681370280410998674, 2.949305648881000330, -8.659807625323999503 ) ) ;
#40368 = CARTESIAN_POINT ( 'NONE',  ( 9.286567869848370904, 4.827162169466027386, 9.039452245500738670 ) ) ;
#40369 = CARTESIAN_POINT ( 'NONE',  ( 12.20440283798329517, -2.672818875560375673, 13.63528575797814568 ) ) ;
#40370 = CARTESIAN_POINT ( 'NONE',  ( 24.05250980246030679, 3.342975859377496750, 12.65038706989959927 ) ) ;
#40371 = CARTESIAN_POINT ( 'NONE',  ( 23.51693413382500353, 10.50595995297999963, -9.452639959603999387 ) ) ;
#40372 = CARTESIAN_POINT ( 'NONE',  ( 17.99211270977099986, -3.227071166021000082, -11.34499727797000013 ) ) ;
#40374 = CARTESIAN_POINT ( 'NONE',  ( 2.360701334807637330, 2.284289129262892626, -2.477459195523546764 ) ) ;
#40373 = CARTESIAN_POINT ( 'NONE',  ( 10.86624205625100004, -4.409476560233800413, 6.434137271007999814 ) ) ;
#40375 = CARTESIAN_POINT ( 'NONE',  ( 4.555026506349999948, -1.500000000000000000, 0.000000000000000000 ) ) ;
#40376 = ORIENTED_EDGE ( 'NONE', *, *, #68270, .F. ) ;
#40377 = CARTESIAN_POINT ( 'NONE',  ( 12.75652363867536110, -0.7301778992647613986, 13.98094561311457440 ) ) ;
#40378 = CARTESIAN_POINT ( 'NONE',  ( 23.60205915885299888, -11.72032963060998867, -3.891881970952999481 ) ) ;
#40379 = CARTESIAN_POINT ( 'NONE',  ( 10.02091161619000026, -4.911674715448000050, -6.466751564808000730 ) ) ;
#40380 = CARTESIAN_POINT ( 'NONE',  ( 18.02541143671232504, 0.4116921281473247540, 12.69102089861179472 ) ) ;
#40381 = CARTESIAN_POINT ( 'NONE',  ( 18.17985377383712020, -2.516953534672679016, -12.44759707709438246 ) ) ;
#40382 = CARTESIAN_POINT ( 'NONE',  ( 8.615121458427411838, 5.349954800205006578, -7.499992720895565235 ) ) ;
#40383 = CARTESIAN_POINT ( 'NONE',  ( 9.975298369746390392, 5.350379160513678123, 7.499985214262784083 ) ) ;
#40384 = B_SPLINE_CURVE_WITH_KNOTS ( 'NONE', 3,
 ( #20710, #58453, #10557, #68588 ),
 .UNSPECIFIED., .F., .F.,
 ( 4, 4 ),
 ( 0.000000000000000000, 1.000000000000000000 ),
 .UNSPECIFIED. ) ;
#40385 = CARTESIAN_POINT ( 'NONE',  ( 10.19810941423799910, 4.946022705791000007, 8.359277272599898723 ) ) ;
#40386 = CARTESIAN_POINT ( 'NONE',  ( 7.890669420221000152, 4.660296061153999858, 6.322498784873999078 ) ) ;
#40387 = DIRECTION ( 'NONE',  ( 1.000000000000000000, 0.000000000000000000, 0.000000000000000000 ) ) ;
#40388 = ORIENTED_EDGE ( 'NONE', *, *, #33792, .F. ) ;
#40389 = EDGE_CURVE ( 'NONE', #25486, #59995, #34914, .T. ) ;
#40390 = ADVANCED_FACE ( 'NONE', ( #66739 ), #59066, .F. ) ;
#40391 = CARTESIAN_POINT ( 'NONE',  ( 12.32674677874978286, 0.5406785836137721901, -12.58839662496522749 ) ) ;
#40392 = CARTESIAN_POINT ( 'NONE',  ( 12.72212784909656946, -1.875000000000001110, -12.57541659658316924 ) ) ;
#40393 = CARTESIAN_POINT ( 'NONE',  ( 16.09997386696500143, 4.522001505202922544, 10.77728718286269149 ) ) ;
#40394 = CARTESIAN_POINT ( 'NONE',  ( 8.705989158774000813, 2.542862824481000317, 7.419808961972999661 ) ) ;
#40395 = CARTESIAN_POINT ( 'NONE',  ( 6.799999999999999822, 0.000000000000000000, 0.000000000000000000 ) ) ;
#40396 = EDGE_LOOP ( 'NONE', ( #65695, #49316, #29287, #62220 ) ) ;
#40397 = CARTESIAN_POINT ( 'NONE',  ( 6.866058386525000223, -1.131649478240000173, 0.5631818380099999910 ) ) ;
#40398 = ADVANCED_FACE ( 'NONE', ( #37808 ), #53858, .T. ) ;
#40399 = CARTESIAN_POINT ( 'NONE',  ( 10.92037236908235620, 9.620066740324960008, 5.957247158094110873 ) ) ;
#40400 = CARTESIAN_POINT ( 'NONE',  ( 10.61705858902311306, 5.079493225103655973, -8.329679463145396312 ) ) ;
#40401 = CARTESIAN_POINT ( 'NONE',  ( 1.553056799207125138, 2.798833948393625537, 2.150913519912209360 ) ) ;
#40402 = CARTESIAN_POINT ( 'NONE',  ( 10.51925056272499859, 5.174767082365999471, -7.517410630436119234 ) ) ;
#40403 = VERTEX_POINT ( 'NONE', #49681 ) ;
#40404 = CARTESIAN_POINT ( 'NONE',  ( 9.722771884505998941, -5.493781611190000191, 6.566828939965000167 ) ) ;
#40405 = VERTEX_POINT ( 'NONE', #43412 ) ;
#40406 = CARTESIAN_POINT ( 'NONE',  ( 16.10005255078199937, -3.632778330393000132, -11.06917548872000090 ) ) ;
#40407 = CARTESIAN_POINT ( 'NONE',  ( 7.790629440376999781, -3.416208448044999901, 6.162501393933999871 ) ) ;
#40408 = VECTOR ( 'NONE', #30898, 1000.000000000000227 ) ;
#40409 = CARTESIAN_POINT ( 'NONE',  ( 18.27776594916669239, 0.05915529127692104039, -13.99988012777929036 ) ) ;
#40410 = ORIENTED_EDGE ( 'NONE', *, *, #5232, .F. ) ;
#40411 = CARTESIAN_POINT ( 'NONE',  ( 10.98384919964044570, 8.157961774527716869, -6.541894492409994655 ) ) ;
#40412 = CARTESIAN_POINT ( 'NONE',  ( 10.26195629121000152, -4.600000265269999389, 4.591198190832999515 ) ) ;
#40413 = CARTESIAN_POINT ( 'NONE',  ( 7.099999886593999499, -1.865174681369999698E-13, 1.040815226917999900E-13 ) ) ;
#40414 = CARTESIAN_POINT ( 'NONE',  ( 16.39999999231800132, -3.216285993016000155, -11.40340220863999932 ) ) ;
#40415 = CARTESIAN_POINT ( 'NONE',  ( 18.08697361609490173, -2.828309738116514094, 12.36901404293088724 ) ) ;
#40416 = ORIENTED_EDGE ( 'NONE', *, *, #69169, .F. ) ;
#40417 = CARTESIAN_POINT ( 'NONE',  ( 2.178056799207042538, -2.150913519912214245, 2.798833948393621984 ) ) ;
#40418 = CARTESIAN_POINT ( 'NONE',  ( 12.20879664879744908, -2.687389840232196736, -13.63187458904427629 ) ) ;
#40419 = CARTESIAN_POINT ( 'NONE',  ( 11.09999999999999964, -5.772457065253999708, -5.146041223417999966 ) ) ;
#40420 = CARTESIAN_POINT ( 'NONE',  ( 10.99214179192066254, 5.203944559837983874, 6.668820502926433136 ) ) ;
#40421 = LINE ( 'NONE', #29960, #59366 ) ;
#40422 = ORIENTED_EDGE ( 'NONE', *, *, #45546, .T. ) ;
#40423 = CARTESIAN_POINT ( 'NONE',  ( 11.09999999999999964, 4.000000000000000000, 7.500000000000000000 ) ) ;
#40424 = CARTESIAN_POINT ( 'NONE',  ( 10.92028665956053324, 3.257584962274628460, -8.549395343567624650 ) ) ;
#40425 = CARTESIAN_POINT ( 'NONE',  ( 3.500000000000000000, 3.499738125128000199, -0.04281419768536000314 ) ) ;
#40426 = CARTESIAN_POINT ( 'NONE',  ( 23.80953449760752605, -3.305759387292704243, -13.11171555762221530 ) ) ;
#40427 = CARTESIAN_POINT ( 'NONE',  ( 3.021806799210415839, 3.408904368339103375, 0.9161175952574877046 ) ) ;
#40428 = CARTESIAN_POINT ( 'NONE',  ( 12.20096535489426692, -0.1616183441363955586, -13.89875400931294180 ) ) ;
#40429 = CARTESIAN_POINT ( 'NONE',  ( 17.77761373051713178, -1.915879702936831519, 12.56867159344775153 ) ) ;
#40430 = ORIENTED_EDGE ( 'NONE', *, *, #24084, .T. ) ;
#40431 = CARTESIAN_POINT ( 'NONE',  ( 11.27234208742519783, -4.554746427620499638, -8.372004648554700168 ) ) ;
#40432 = ORIENTED_EDGE ( 'NONE', *, *, #17841, .T. ) ;
#40433 = CARTESIAN_POINT ( 'NONE',  ( 9.924742128742000347, 5.060458431729999873, 8.686130311522999747 ) ) ;
#40434 = LINE ( 'NONE', #46032, #19953 ) ;
#40435 = CARTESIAN_POINT ( 'NONE',  ( 9.915635841230999503, 3.210851187372000037, -6.346613542714999667 ) ) ;
#40436 = CIRCLE ( 'NONE', #42640, 13.92493900950999475 ) ;
#40437 = CARTESIAN_POINT ( 'NONE',  ( 2.516671991354999527, 3.690792505019000025, -0.3576329073664999969 ) ) ;
#40438 = CARTESIAN_POINT ( 'NONE',  ( 10.56270535986999981, -2.509383044034000143, -8.602408326857998944 ) ) ;
#40439 = EDGE_CURVE ( 'NONE', #8229, #42155, #15872, .T. ) ;
#40440 = FACE_OUTER_BOUND ( 'NONE', #9903, .T. ) ;
#40441 = CARTESIAN_POINT ( 'NONE',  ( 9.002566322894800521, -5.272342554236079337, 7.950847953095180998 ) ) ;
#40442 = VERTEX_POINT ( 'NONE', #59470 ) ;
#40443 = ADVANCED_FACE ( 'NONE', ( #22062 ), #49328, .F. ) ;
#40444 = CARTESIAN_POINT ( 'NONE',  ( 11.41610672858429965, -4.911600290708499905, 8.185766014210599906 ) ) ;
#40445 = CARTESIAN_POINT ( 'NONE',  ( 9.696080515601000371, 2.554416243104999928, 7.600685069647000525 ) ) ;
#40446 = CARTESIAN_POINT ( 'NONE',  ( 11.00000000000000000, 5.079754677601000523, -7.825000000000000178 ) ) ;
#40447 = LINE ( 'NONE', #9658, #28781 ) ;
#40449 = CARTESIAN_POINT ( 'NONE',  ( 11.02319144466311052, -2.880026002252477291, -7.824989718906223857 ) ) ;
#40448 = CARTESIAN_POINT ( 'NONE',  ( 11.14698693981000055, 5.129806801114000336, 5.886034047559999927 ) ) ;
#40450 = AXIS2_PLACEMENT_3D ( 'NONE', #53180, #57727, #52488 ) ;
#40451 = CARTESIAN_POINT ( 'NONE',  ( 10.42795525820099911, 3.905250696375530239, -6.501013802764199490 ) ) ;
#40452 = DIRECTION ( 'NONE',  ( -1.000000000000000000, 0.000000000000000000, 0.000000000000000000 ) ) ;
#40453 = CARTESIAN_POINT ( 'NONE',  ( 8.871822372493998188, 3.671800173070400408, -8.573651380901999630 ) ) ;
#40454 = CARTESIAN_POINT ( 'NONE',  ( 17.93788416347130976, -0.6112845611542790936, 12.58516990776527145 ) ) ;
#40455 = CARTESIAN_POINT ( 'NONE',  ( 24.50549018585800098, 3.501736898117000063, 12.23514954116999931 ) ) ;
#40456 = CARTESIAN_POINT ( 'NONE',  ( 0.7600208369539874775, -3.500000000000000000, -0.3979241631804403267 ) ) ;
#40457 = LINE ( 'NONE', #15271, #42193 ) ;
#40458 = ORIENTED_EDGE ( 'NONE', *, *, #35675, .F. ) ;
#40459 = CARTESIAN_POINT ( 'NONE',  ( 8.218894353209000414, -3.011617647609999615, 8.801438026873999121 ) ) ;
#40460 = CARTESIAN_POINT ( 'NONE',  ( 17.60327209889952726, 1.789008353514935479, 13.88522434179080456 ) ) ;
#40461 = CARTESIAN_POINT ( 'NONE',  ( 5.000030787343000327, -1.679270695423617177, -1.290525307673965782 ) ) ;
#40462 = FACE_OUTER_BOUND ( 'NONE', #63849, .T. ) ;
#40463 = ORIENTED_EDGE ( 'NONE', *, *, #2355, .T. ) ;
#40464 = CARTESIAN_POINT ( 'NONE',  ( 17.75870478550200104, 3.641518898264000548, 12.02435208579999859 ) ) ;
#40466 = CARTESIAN_POINT ( 'NONE',  ( 11.59456039236534330, 5.314711678001000195, 7.436015812896529020 ) ) ;
#40465 = CARTESIAN_POINT ( 'NONE',  ( 9.028772138681999238, -4.322628849750500102, -6.695252480703800302 ) ) ;
#40467 = CARTESIAN_POINT ( 'NONE',  ( 3.500000000000000000, -2.946081722130999836, 0.9972449351501998516 ) ) ;
#40468 = ORIENTED_EDGE ( 'NONE', *, *, #57294, .T. ) ;
#40469 = EDGE_CURVE ( 'NONE', #46383, #43332, #67277, .T. ) ;
#40470 = CARTESIAN_POINT ( 'NONE',  ( 8.610944094208999644, 5.100000000000000533, -6.571291218949999902 ) ) ;
#40472 = CARTESIAN_POINT ( 'NONE',  ( 17.84552141390807378, -3.187082727966597417, -13.63240720791674931 ) ) ;
#40471 = B_SPLINE_CURVE_WITH_KNOTS ( 'NONE', 3,
 ( #43479, #27392, #60588, #28085 ),
 .UNSPECIFIED., .F., .F.,
 ( 4, 4 ),
 ( 0.000000000000000000, 1.000000000000000000 ),
 .UNSPECIFIED. ) ;
#40473 = CARTESIAN_POINT ( 'NONE',  ( 10.32533997688000049, 4.243109097101799954, 8.614534918052999757 ) ) ;
#40474 = CARTESIAN_POINT ( 'NONE',  ( 24.30001694391200218, -12.21047201246000036, 3.271805662802000025 ) ) ;
#40475 = CARTESIAN_POINT ( 'NONE',  ( 10.98768472638000127, 7.408460511344000743, 6.159405790617999976 ) ) ;
#40476 = ORIENTED_EDGE ( 'NONE', *, *, #21303, .F. ) ;
#40477 = LINE ( 'NONE', #40822, #5355 ) ;
#40478 = ADVANCED_FACE ( 'NONE', ( #59822 ), #43054, .T. ) ;
#40479 = EDGE_CURVE ( 'NONE', #64314, #43855, #59130, .T. ) ;
#40480 = CARTESIAN_POINT ( 'NONE',  ( 10.18308064679000147, -2.953580299898999950, -8.606287508253000595 ) ) ;
#40481 = CARTESIAN_POINT ( 'NONE',  ( 8.060203937213300307, -3.679481436877252154, 5.790105483359396565 ) ) ;
#40482 = CARTESIAN_POINT ( 'NONE',  ( 10.34521071928999980, -2.724119865955000108, 6.497322598008000050 ) ) ;
#40483 = CARTESIAN_POINT ( 'NONE',  ( 10.60235971519489873, -3.394698737128500010, -6.493038401303000029 ) ) ;
#40484 = CARTESIAN_POINT ( 'NONE',  ( 9.575405316139999456, -4.242421256336299962, 6.384219384258999597 ) ) ;
#40485 = ORIENTED_EDGE ( 'NONE', *, *, #66687, .F. ) ;
#40487 = CARTESIAN_POINT ( 'NONE',  ( 10.35302581057999838, -4.581018032643999760, -4.861894197833000142 ) ) ;
#40486 = TOROIDAL_SURFACE ( 'NONE', #20376, 12.20000000000000107, 0.6999999999999999556 ) ;
#40488 = CARTESIAN_POINT ( 'NONE',  ( 11.21503032197930061, -3.256621462143499901, 8.539569492647999027 ) ) ;
#40489 = ORIENTED_EDGE ( 'NONE', *, *, #27664, .F. ) ;
#40490 = CARTESIAN_POINT ( 'NONE',  ( 24.30000000000000071, -9.240454295252998662, -8.250504801592001058 ) ) ;
#40491 = ORIENTED_EDGE ( 'NONE', *, *, #45922, .F. ) ;
#40492 = CARTESIAN_POINT ( 'NONE',  ( 9.798320215454998205, -2.757678812098000254, -6.584768124342000206 ) ) ;
#40493 = CARTESIAN_POINT ( 'NONE',  ( 8.415504719592000527, 2.469361196073999842, -7.826019481986000059 ) ) ;
#40494 = CARTESIAN_POINT ( 'NONE',  ( 11.80233327354039830, 2.898463260143000042, -6.779499720266399798 ) ) ;
#40495 = DIRECTION ( 'NONE',  ( 0.000000000000000000, 1.000000000000000000, 0.000000000000000000 ) ) ;
#40496 = CARTESIAN_POINT ( 'NONE',  ( 12.28874679351406307, 2.147634260983757759, -12.52674262693623142 ) ) ;
#40497 = CARTESIAN_POINT ( 'NONE',  ( 11.32179975933729921, -3.051121678931899783, 7.826467126457498757 ) ) ;
#40498 = CARTESIAN_POINT ( 'NONE',  ( 8.528448341230999930, 2.472348777564000066, 6.234194744024999402 ) ) ;
#40499 = EDGE_CURVE ( 'NONE', #50417, #60537, #31141, .T. ) ;
#40500 = VERTEX_POINT ( 'NONE', #33265 ) ;
#40501 = CARTESIAN_POINT ( 'NONE',  ( 7.742593052214973959, 2.625666041398489359, 7.178124245676486659 ) ) ;
#40502 = VECTOR ( 'NONE', #42920, 1000.000000000000000 ) ;
#40503 = CARTESIAN_POINT ( 'NONE',  ( 7.443293146792999693, -4.698358408974000255, 8.789434435623999065 ) ) ;
#40504 = CARTESIAN_POINT ( 'NONE',  ( 24.12730417462044130, 9.172513492733058271, 9.141935095995247451 ) ) ;
#40505 = ORIENTED_EDGE ( 'NONE', *, *, #44565, .F. ) ;
#40506 = CARTESIAN_POINT ( 'NONE',  ( 12.18809860077016971, -2.859021363400004567, -12.27136516364851815 ) ) ;
#40507 = CARTESIAN_POINT ( 'NONE',  ( 11.61759063708296047, 5.217265640542000149, 7.157757529645699890 ) ) ;
#40508 = CARTESIAN_POINT ( 'NONE',  ( 10.62256935321000029, -2.471463903746000224, -8.210787855397999380 ) ) ;
#40509 = CARTESIAN_POINT ( 'NONE',  ( 10.82309687351639660, 2.782534154164606921, 7.827184855449101697 ) ) ;
#40510 = CARTESIAN_POINT ( 'NONE',  ( 18.23043922992600230, -3.518658233831999826, -12.06062508533999988 ) ) ;
#40511 = CARTESIAN_POINT ( 'NONE',  ( 24.66271478023099917, -8.757902662108000058, 9.242626226729999672 ) ) ;
#40512 = CARTESIAN_POINT ( 'NONE',  ( 12.45019282332729382, -3.154806840457492711, -13.63991304855491471 ) ) ;
#40513 = DIRECTION ( 'NONE',  ( -1.000000000000000000, 0.000000000000000000, 0.000000000000000000 ) ) ;
#40514 = CARTESIAN_POINT ( 'NONE',  ( 10.51810807141099779, -3.940954591493389891, -8.776647962565998995 ) ) ;
#40515 = FACE_OUTER_BOUND ( 'NONE', #37157, .T. ) ;
#40516 = VERTEX_POINT ( 'NONE', #12284 ) ;
#40517 = B_SPLINE_CURVE_WITH_KNOTS ( 'NONE', 3,
 ( #27772, #22159, #27075, #32327 ),
 .UNSPECIFIED., .F., .F.,
 ( 4, 4 ),
 ( 0.000000000000000000, 1.000000000000000000 ),
 .UNSPECIFIED. ) ;
#40518 = ORIENTED_EDGE ( 'NONE', *, *, #33055, .F. ) ;
#40519 = SURFACE_STYLE_FILL_AREA ( #25471 ) ;
#40520 = DIRECTION ( 'NONE',  ( 0.000000000000000000, 1.000000000000000000, 0.000000000000000000 ) ) ;
#40521 = CARTESIAN_POINT ( 'NONE',  ( 8.079724940884538853, 4.352763894256345800, 8.815588961478567853 ) ) ;
#40522 = CARTESIAN_POINT ( 'NONE',  ( 9.675534850247000662, 4.656736118461000551, -8.653212384786000300 ) ) ;
#40523 = B_SPLINE_CURVE_WITH_KNOTS ( 'NONE', 3,
 ( #20816, #25032, #52628, #46364 ),
 .UNSPECIFIED., .F., .F.,
 ( 4, 4 ),
 ( 0.000000000000000000, 0.2180895000437835241 ),
 .UNSPECIFIED. ) ;
#40524 = CARTESIAN_POINT ( 'NONE',  ( 27.64127793187000037, 4.599999999999999645, -4.505338571134999803 ) ) ;
#40525 = CARTESIAN_POINT ( 'NONE',  ( 17.55505043854143565, 1.875000000000000000, 12.57541666120756041 ) ) ;
#40526 = CARTESIAN_POINT ( 'NONE',  ( 8.350387243830999395, 4.599999999999999645, -6.632262360512000576 ) ) ;
#40527 = CARTESIAN_POINT ( 'NONE',  ( 9.600491906670001185, 5.206545077004999911, 8.585111878242999595 ) ) ;
#40528 = ADVANCED_FACE ( 'NONE', ( #22410 ), #40486, .F. ) ;
#40529 = CARTESIAN_POINT ( 'NONE',  ( 10.32340023520112027, -2.820488420190699230, -8.179866073662411807 ) ) ;
#40530 = ORIENTED_EDGE ( 'NONE', *, *, #28539, .T. ) ;
#40531 = CARTESIAN_POINT ( 'NONE',  ( 12.51690604397277795, -1.945290150052898515, 12.56367745121459834 ) ) ;
#40532 = CARTESIAN_POINT ( 'NONE',  ( 8.802265421554999136, -4.188500707411799695, -8.475084258675400051 ) ) ;
#40533 = CARTESIAN_POINT ( 'NONE',  ( 10.57224177473000104, 4.020426023752999178, 8.920668579831000145 ) ) ;
#40534 = CARTESIAN_POINT ( 'NONE',  ( 11.63746005378019888, -2.838900981960999825, 8.120007936598501175 ) ) ;
#40535 = AXIS2_PLACEMENT_3D ( 'NONE', #30082, #7708, #39875 ) ;
#40536 = PRODUCT_DEFINITION_SHAPE ( 'NONE', 'NONE',  #43225 ) ;
#40537 = CARTESIAN_POINT ( 'NONE',  ( 11.25656651104150008, 4.126085365637900182, -6.228222165170999247 ) ) ;
#40538 = CARTESIAN_POINT ( 'NONE',  ( 12.18402519556254404, -0.07112609253419358013, 12.69973757146476245 ) ) ;
#40539 = CARTESIAN_POINT ( 'NONE',  ( 9.278329719590999503, 5.791553967443999973, 7.752111263209999770 ) ) ;
#40540 = B_SPLINE_CURVE_WITH_KNOTS ( 'NONE', 3,
 ( #27201, #62864, #5861, #52383, #47843, #48521, #630, #31761, #5177, #52730 ),
 .UNSPECIFIED., .F., .F.,
 ( 4, 2, 2, 2, 4 ),
 ( 0.000000000000000000, 0.2500000000000004441, 0.5000000000000008882, 0.7500000000000004441, 1.000000000000000000 ),
 .UNSPECIFIED. ) ;
#40541 = CARTESIAN_POINT ( 'NONE',  ( 10.71756692516999898, 3.040224182812999665, 8.808452309630000698 ) ) ;
#40542 = CARTESIAN_POINT ( 'NONE',  ( 12.51634965191642301, 1.945578265428328457, 12.56358890505709169 ) ) ;
#40543 = ORIENTED_EDGE ( 'NONE', *, *, #67603, .F. ) ;
#40544 = CARTESIAN_POINT ( 'NONE',  ( 10.21398584123000042, 3.990126737362999609, -8.809457313313998839 ) ) ;
#40545 = CARTESIAN_POINT ( 'NONE',  ( 10.37041638348499895, 2.758294858530000226, -7.197535585171899619 ) ) ;
#40546 = CARTESIAN_POINT ( 'NONE',  ( 10.67395468736628672, -5.666583699971932120, 6.945968662367498325 ) ) ;
#40548 = CARTESIAN_POINT ( 'NONE',  ( 3.302853993820082490, -2.804141251808610402, -2.143609296475933679 ) ) ;
#40547 = CARTESIAN_POINT ( 'NONE',  ( 8.496691940379001551, -5.198566224659999513, 8.332559954171999905 ) ) ;
#40549 = CARTESIAN_POINT ( 'NONE',  ( 10.23976354018233259, 3.672815144550903632, -6.282534154164605589 ) ) ;
#40550 = CARTESIAN_POINT ( 'NONE',  ( 10.67410807141119911, -3.953638752893899877, -8.502397868920999358 ) ) ;
#40551 = ORIENTED_EDGE ( 'NONE', *, *, #67944, .T. ) ;
#40552 = AXIS2_PLACEMENT_3D ( 'NONE', #53399, #5498, #10738 ) ;
#40553 = CARTESIAN_POINT ( 'NONE',  ( 1.634474105091999974, -2.924745949230000086, 2.085595834630999956 ) ) ;
#40554 = CARTESIAN_POINT ( 'NONE',  ( 18.09779212077640764, -0.3101159433354428452, -12.69490728026826432 ) ) ;
#40555 = AXIS2_PLACEMENT_3D ( 'NONE', #68984, #62700, #63730 ) ;
#40557 = LINE ( 'NONE', #56643, #64429 ) ;
#40556 = CARTESIAN_POINT ( 'NONE',  ( 12.79999999838119962, 11.94789761932849004, -3.252399792653988264 ) ) ;
#40558 = CARTESIAN_POINT ( 'NONE',  ( 11.79999998956225937, -3.428554832065387359, 11.90642801602077228 ) ) ;
#40559 = CARTESIAN_POINT ( 'NONE',  ( 10.18240541510999897, 2.607737086676999994, 7.783408568367999436 ) ) ;
#40560 = CARTESIAN_POINT ( 'NONE',  ( 12.38095956647856610, -3.110256499846533185, 13.65014134263123857 ) ) ;
#40561 = CARTESIAN_POINT ( 'NONE',  ( 11.86486084871759950, -5.207010770456999893, 7.174999999999999822 ) ) ;
#40562 = CARTESIAN_POINT ( 'NONE',  ( 9.390726590333203561, -5.236125653078060438, 6.940982610062651048 ) ) ;
#40563 = CARTESIAN_POINT ( 'NONE',  ( 7.330275273710999961, -4.426925773067000414, 9.293310812901001583 ) ) ;
#40564 = EDGE_LOOP ( 'NONE', ( #44382, #54582, #25603, #32672 ) ) ;
#40565 = CARTESIAN_POINT ( 'NONE',  ( 7.866204719590000671, 4.580608786027000612, 9.213365309690999538 ) ) ;
#40566 = ADVANCED_FACE ( 'NONE', ( #44459 ), #28218, .F. ) ;
#40567 = CARTESIAN_POINT ( 'NONE',  ( 5.199999999962999553, -1.376649744612000070, -11.21582968308000083 ) ) ;
#40568 = CARTESIAN_POINT ( 'NONE',  ( 7.433994579421323579, -2.292697518400240053, 7.832234419706870732 ) ) ;
#40569 = CARTESIAN_POINT ( 'NONE',  ( 10.47530200610951034, -5.350262918594152595, 7.499984559551212904 ) ) ;
#40570 = CARTESIAN_POINT ( 'NONE',  ( 1.886293599501000173, -2.100427248507999778, 2.706108474410000131 ) ) ;
#40571 = ORIENTED_EDGE ( 'NONE', *, *, #37311, .T. ) ;
#40572 = CARTESIAN_POINT ( 'NONE',  ( 0.8095474569573147816, 3.020249054117508436, 1.336761677555526218 ) ) ;
#40573 = B_SPLINE_CURVE_WITH_KNOTS ( 'NONE', 3,
 ( #8313, #3058, #30333, #25417 ),
 .UNSPECIFIED., .F., .F.,
 ( 4, 4 ),
 ( 0.6083653520376346435, 1.000000000000000000 ),
 .UNSPECIFIED. ) ;
#40574 = CARTESIAN_POINT ( 'NONE',  ( 12.10948876160955479, -4.695527826393099957, 6.776679950459500112 ) ) ;
#40575 = DIRECTION ( 'NONE',  ( 1.000000000000000000, 0.000000000000000000, 0.000000000000000000 ) ) ;
#40576 = CARTESIAN_POINT ( 'NONE',  ( 9.332933391271998502, 5.100349772922000646, 8.693467186193998941 ) ) ;
#40577 = CARTESIAN_POINT ( 'NONE',  ( 11.77359063708300013, 4.955772084214699724, 7.231278212164300001 ) ) ;
#40578 = CARTESIAN_POINT ( 'NONE',  ( 24.30000000000000071, -11.49391741900999975, 4.090215442373000165 ) ) ;
#40579 = CARTESIAN_POINT ( 'NONE',  ( 18.30000000000000071, -2.775703640144308260, -11.68316444257406772 ) ) ;
#40580 = CARTESIAN_POINT ( 'NONE',  ( 18.02561562912592663, 0.4118363585311526354, -13.89180007025484720 ) ) ;
#40581 = CARTESIAN_POINT ( 'NONE',  ( 12.80505043854144276, 0.6249999999999994449, -13.88107975066922428 ) ) ;
#40582 = CARTESIAN_POINT ( 'NONE',  ( 11.16486084871730000, 5.207010770456999893, -7.174999999999999822 ) ) ;
#40583 = CONICAL_SURFACE ( 'NONE', #47276, 1.150079926948000208, 0.7854585090185547402 ) ;
#40584 = EDGE_CURVE ( 'NONE', #19975, #53136, #64401, .T. ) ;
#40585 = CARTESIAN_POINT ( 'NONE',  ( 7.866984495661538013, 3.121299587659922103, 9.063503846007870735 ) ) ;
#40586 = EDGE_LOOP ( 'NONE', ( #48791, #39348, #36596, #7619, #34892 ) ) ;
#40587 = CONICAL_SURFACE ( 'NONE', #66235, 11.34994642770999818, 0.7853934433894341760 ) ;
#40588 = CARTESIAN_POINT ( 'NONE',  ( 17.69802269633226288, -1.891226317878778485, 13.78388397175237046 ) ) ;
#40589 = CARTESIAN_POINT ( 'NONE',  ( 9.099999931440999390, 4.000000000000000000, 7.500000000000000000 ) ) ;
#40590 = VERTEX_POINT ( 'NONE', #22759 ) ;
#40591 = ORIENTED_EDGE ( 'NONE', *, *, #8194, .T. ) ;
#40592 = EDGE_CURVE ( 'NONE', #13624, #59040, #32237, .T. ) ;
#40593 = CARTESIAN_POINT ( 'NONE',  ( 24.76117126521998557, -3.101100257814066730, -11.75475255056689505 ) ) ;
#40594 = CARTESIAN_POINT ( 'NONE',  ( 9.771013540183334456, 3.231816600031359066, -6.500416447002272058 ) ) ;
#40595 = CARTESIAN_POINT ( 'NONE',  ( 24.30000000000000071, 0.000000000000000000, 0.000000000000000000 ) ) ;
#40596 = CARTESIAN_POINT ( 'NONE',  ( 9.910790522921001156, 3.869345236050000025, 5.882548872612999524 ) ) ;
#40597 = CARTESIAN_POINT ( 'NONE',  ( 10.91943903453000075, 3.268382602297999817, -6.413946631105000407 ) ) ;
#40598 = CARTESIAN_POINT ( 'NONE',  ( 9.049596101582626062, -4.563377510236459322, -6.830568860986387492 ) ) ;
#40599 = CARTESIAN_POINT ( 'NONE',  ( 9.514108112060000622, -4.887639888682999256, 8.462756667353000140 ) ) ;
#40600 = CARTESIAN_POINT ( 'NONE',  ( 18.27393049982691764, 0.09400131084486958166, -12.59965472429369093 ) ) ;
#40601 = CARTESIAN_POINT ( 'NONE',  ( 10.90000000000000036, 0.2500000000000000000, 4.902439024389999567 ) ) ;
#40602 = CARTESIAN_POINT ( 'NONE',  ( 10.40749413291699987, -3.211956830789300277, -7.140435631538599281 ) ) ;
#40603 = CARTESIAN_POINT ( 'NONE',  ( 12.80505043854146940, -1.760845406083394016, 12.47635457398814829 ) ) ;
#40604 = ORIENTED_EDGE ( 'NONE', *, *, #39733, .T. ) ;
#40605 = FACE_OUTER_BOUND ( 'NONE', #57788, .T. ) ;
#40606 = CARTESIAN_POINT ( 'NONE',  ( 24.81125947960093114, 8.606650034182759867, 8.517985928714615795 ) ) ;
#40607 = VECTOR ( 'NONE', #38541, 1000.000000000000000 ) ;
#40608 = CARTESIAN_POINT ( 'NONE',  ( 5.000030787343002103, 2.099962892531005654, -0.2748844998327801270 ) ) ;
#40609 = CARTESIAN_POINT ( 'NONE',  ( 9.887000818240000655, 2.868129552070000088, -8.096031607030200306 ) ) ;
#40610 = CARTESIAN_POINT ( 'NONE',  ( 12.12491761308580074, 2.264077311857957575, 13.81573193591466797 ) ) ;
#40611 = CARTESIAN_POINT ( 'NONE',  ( 10.46754921866999943, -2.318350880468999620, 6.549783596838000044 ) ) ;
#40612 = VERTEX_POINT ( 'NONE', #26982 ) ;
#40613 = CARTESIAN_POINT ( 'NONE',  ( 12.29062685731073401, -0.3550721707632966129, -12.69332222954723655 ) ) ;
#40614 = CARTESIAN_POINT ( 'NONE',  ( 12.64055492385137747, -0.7115697451012007457, 13.98190580764195801 ) ) ;
#40615 = ORIENTED_EDGE ( 'NONE', *, *, #35696, .F. ) ;
#40616 = FACE_OUTER_BOUND ( 'NONE', #25885, .T. ) ;
#40617 = DIRECTION ( 'NONE',  ( -1.000000000000000000, 0.000000000000000000, 0.000000000000000000 ) ) ;
#40618 = DIRECTION ( 'NONE',  ( 0.7660444431190069903, 0.000000000000000000, 0.6427876096865049460 ) ) ;
#40619 = CARTESIAN_POINT ( 'NONE',  ( 8.486008579191000933, 3.399999999999999911, 5.976611076844000614 ) ) ;
#40620 = CARTESIAN_POINT ( 'NONE',  ( 23.59999462723899910, 13.22316330987000121, -4.267799687262000319 ) ) ;
#40621 = CARTESIAN_POINT ( 'NONE',  ( 17.60000000000000142, -11.23412379136000006, 3.084957477885999833 ) ) ;
#40622 = CARTESIAN_POINT ( 'NONE',  ( 8.070721554491719019, 3.646115526505103510, 8.813957122113052378 ) ) ;
#40623 = CARTESIAN_POINT ( 'NONE',  ( 5.000000000000000000, 0.2999999999999999889, -9.776630298829998011 ) ) ;
#40624 = PLANE ( 'NONE',  #40798 ) ;
#40625 = CARTESIAN_POINT ( 'NONE',  ( 11.73671932425159881, 3.872987101045399783, -8.356835045446798560 ) ) ;
#40626 = CARTESIAN_POINT ( 'NONE',  ( 8.436987556243993325, 2.901283824935000144, -6.624026488670998525 ) ) ;
#40627 = CARTESIAN_POINT ( 'NONE',  ( 12.80505043854144276, 0.6878608935795413881, -12.61273126665598454 ) ) ;
#40628 = CARTESIAN_POINT ( 'NONE',  ( 9.683304848515998486, 5.038423216181000086, -7.974775391194199869 ) ) ;
#40630 = CARTESIAN_POINT ( 'NONE',  ( 10.98768472569999943, 5.449702578894000560, 4.945212061318999375 ) ) ;
#40629 = CARTESIAN_POINT ( 'NONE',  ( 15.84051303026600266, -8.692957937327999929, -7.975472622866001338 ) ) ;
#40631 = LINE ( 'NONE', #62305, #66528 ) ;
#40632 = ORIENTED_EDGE ( 'NONE', *, *, #28545, .F. ) ;
#40633 = CONICAL_SURFACE ( 'NONE', #4891, 2.100030785748999929, 0.7853981633972997312 ) ;
#40634 = CARTESIAN_POINT ( 'NONE',  ( 10.36325056272499978, 4.892034740700499817, 7.486779603004729111 ) ) ;
#40635 = CARTESIAN_POINT ( 'NONE',  ( 10.12549839661999940, -5.788806995403000144, 7.335561828691000485 ) ) ;
#40636 = CARTESIAN_POINT ( 'NONE',  ( 10.31357120343299982, 3.951311476804090006, 6.496769302834999316 ) ) ;
#40637 = CARTESIAN_POINT ( 'NONE',  ( 11.09999999999999964, 4.000000000000000000, -7.500000000000000000 ) ) ;
#40638 = CARTESIAN_POINT ( 'NONE',  ( 4.699998537092440642, 0.000000000000000000, 0.000000000000000000 ) ) ;
#40639 = CARTESIAN_POINT ( 'NONE',  ( 12.60065541206203932, 3.091968277202242987, 13.52988132686268230 ) ) ;
#40640 = CARTESIAN_POINT ( 'NONE',  ( 23.56666365135700403, 9.114812703071004663, -8.684180617907001576 ) ) ;
#40641 = ORIENTED_EDGE ( 'NONE', *, *, #44282, .F. ) ;
#40642 = EDGE_CURVE ( 'NONE', #21416, #46623, #17877, .T. ) ;
#40643 = ADVANCED_FACE ( 'NONE', ( #5639 ), #6951, .T. ) ;
#40644 = AXIS2_PLACEMENT_3D ( 'NONE', #8339, #45744, #57589 ) ;
#40645 = CARTESIAN_POINT ( 'NONE',  ( 8.594151519676998419, -3.975306837623020062, -8.641543873690000765 ) ) ;
#40646 = DIRECTION ( 'NONE',  ( 1.000000000000000000, 0.000000000000000000, 0.000000000000000000 ) ) ;
#40647 = CARTESIAN_POINT ( 'NONE',  ( 11.90211496860029960, -3.206052520092899982, 7.906860999147899527 ) ) ;
#40648 = CARTESIAN_POINT ( 'NONE',  ( 17.57591323121269511, 3.124999405572034927, -12.28374652565520009 ) ) ;
#40649 = CARTESIAN_POINT ( 'NONE',  ( 2.511390132542666631, 3.499999999999998224, 0.4581489286485194157 ) ) ;
#40650 = CONICAL_SURFACE ( 'NONE', #12769, 2.599999999741000156, 0.7853981633972997312 ) ;
#40651 = FACE_OUTER_BOUND ( 'NONE', #4002, .T. ) ;
#40652 = CARTESIAN_POINT ( 'NONE',  ( 12.21945847209102354, 2.718477924854734606, -13.62469170119612194 ) ) ;
#40653 = CARTESIAN_POINT ( 'NONE',  ( 9.216140818749000374, -4.008306780893000187, -8.877926425468999128 ) ) ;
#40654 = CARTESIAN_POINT ( 'NONE',  ( 9.050809142811473862, 5.350259454271556692, -7.263208790141661986 ) ) ;
#40655 = VERTEX_POINT ( 'NONE', #54731 ) ;
#40656 = CARTESIAN_POINT ( 'NONE',  ( 24.32158561237937988, 3.683026774043987039, -12.56966788568789894 ) ) ;
#40657 = AXIS2_PLACEMENT_3D ( 'NONE', #48735, #21805, #65138 ) ;
#40658 = DIRECTION ( 'NONE',  ( 0.9999999999999998890, 3.212307467389999644E-09, 9.519590337635998530E-09 ) ) ;
#40659 = CARTESIAN_POINT ( 'NONE',  ( 23.62794487920146835, 13.40242465305992070, 3.894877993122662474 ) ) ;
#40660 = CARTESIAN_POINT ( 'NONE',  ( 16.42341781689399838, -3.643648243171000001, -12.02373124034999918 ) ) ;
#40661 = CARTESIAN_POINT ( 'NONE',  ( 2.842640132544666631, -3.058252359239902685, -1.762666431298148595 ) ) ;
#40662 = CARTESIAN_POINT ( 'NONE',  ( 9.021064158776001207, 4.883347899767999323, -6.417062834774999835 ) ) ;
#40663 = CARTESIAN_POINT ( 'NONE',  ( 8.679055905797000037, 2.899999999999999911, 6.571291218949999902 ) ) ;
#40664 = ORIENTED_EDGE ( 'NONE', *, *, #20597, .F. ) ;
#40665 = CARTESIAN_POINT ( 'NONE',  ( 9.260875088370248420, -3.646744805991136928, -8.814485081663244515 ) ) ;
#40666 = CARTESIAN_POINT ( 'NONE',  ( 18.23401891600712688, 2.774919967966554157, -13.72225625730858667 ) ) ;
#40667 = ORIENTED_EDGE ( 'NONE', *, *, #68106, .T. ) ;
#40668 = ADVANCED_FACE ( 'NONE', ( #60322 ), #14791, .T. ) ;
#40669 = CARTESIAN_POINT ( 'NONE',  ( 8.591232269961365020, 3.293719616469499289, 8.705632950218131327 ) ) ;
#40670 = DIRECTION ( 'NONE',  ( 0.000000000000000000, 1.000000000000000000, 0.000000000000000000 ) ) ;
#40671 = CARTESIAN_POINT ( 'NONE',  ( 8.514954719592999766, 3.207599814920999659, -6.150466394809999571 ) ) ;
#40672 = CARTESIAN_POINT ( 'NONE',  ( 18.28832092577790291, 2.855728055076846683, -11.50255606648410023 ) ) ;
#40673 = CARTESIAN_POINT ( 'NONE',  ( 11.55811496860034815, -2.954409148022000053, -6.964183526617899744 ) ) ;
#40674 = B_SPLINE_CURVE_WITH_KNOTS ( 'NONE', 3,
 ( #12850, #55497, #12501, #50597 ),
 .UNSPECIFIED., .F., .F.,
 ( 4, 4 ),
 ( 0.000000000000000000, 1.000000000000000000 ),
 .UNSPECIFIED. ) ;
#40675 = B_SPLINE_CURVE_WITH_KNOTS ( 'NONE', 3,
 ( #44999, #19449, #50925, #18774 ),
 .UNSPECIFIED., .F., .F.,
 ( 4, 4 ),
 ( 0.000000000000000000, 1.000000000000000000 ),
 .UNSPECIFIED. ) ;
#40676 = LINE ( 'NONE', #57435, #10286 ) ;
#40677 = FACE_OUTER_BOUND ( 'NONE', #40835, .T. ) ;
#40678 = ORIENTED_EDGE ( 'NONE', *, *, #58006, .T. ) ;
#40679 = CARTESIAN_POINT ( 'NONE',  ( 25.60000000000000142, 8.527654132752997995, -7.260537518969999660 ) ) ;
#40680 = CARTESIAN_POINT ( 'NONE',  ( 10.61476354018233259, -2.782534154164604256, 7.827184855449092815 ) ) ;
#40681 = CARTESIAN_POINT ( 'NONE',  ( 9.038304719595000591, 3.867331042029999999, -9.227339949050001877 ) ) ;
#40682 = EDGE_LOOP ( 'NONE', ( #8927, #49104, #38333, #65521 ) ) ;
#40683 = AXIS2_PLACEMENT_3D ( 'NONE', #19740, #51213, #62714 ) ;
#40684 = CARTESIAN_POINT ( 'NONE',  ( 10.68055531501999944, 2.768167480619000198, -6.114404645958000373 ) ) ;
#40685 = VERTEX_POINT ( 'NONE', #12431 ) ;
#40686 = CARTESIAN_POINT ( 'NONE',  ( 9.683304848515998486, 5.038423216181000086, 7.025224608805800131 ) ) ;
#40687 = CARTESIAN_POINT ( 'NONE',  ( 18.09076461395652657, -2.178034604381228867, -12.52076370778329029 ) ) ;
#40688 = CARTESIAN_POINT ( 'NONE',  ( 16.10004050617000004, 3.886235259787000018, 11.90683839252000098 ) ) ;
#40689 = CARTESIAN_POINT ( 'NONE',  ( 24.44917776433500123, -12.41482580133999924, -3.103222239774000357 ) ) ;
#40690 = CARTESIAN_POINT ( 'NONE',  ( 8.551536913492149949, 3.201507455693337612, 5.984856406915247007 ) ) ;
#40691 = ORIENTED_EDGE ( 'NONE', *, *, #58556, .T. ) ;
#40692 = CARTESIAN_POINT ( 'NONE',  ( 9.099999999999999645, 12.35000000006999876, 0.000000000000000000 ) ) ;
#40693 = CARTESIAN_POINT ( 'NONE',  ( 11.14451084122999980, 5.035416949823999566, -8.381520599479999944 ) ) ;
#40694 = CIRCLE ( 'NONE', #13910, 3.200000000000000178 ) ;
#40695 = CYLINDRICAL_SURFACE ( 'NONE', #605, 1.250000000000000222 ) ;
#40696 = CARTESIAN_POINT ( 'NONE',  ( 12.50373643672534030, 3.182160109867286479, -13.63355731004866378 ) ) ;
#40697 = CARTESIAN_POINT ( 'NONE',  ( 8.958265421554999719, -4.240073379563900069, -8.741861511046000288 ) ) ;
#40698 = B_SPLINE_CURVE_WITH_KNOTS ( 'NONE', 3,
 ( #20256, #36687, #36338, #52413, #57652, #67114, #58010, #62218, #4505, #57308, #40549, #10109, #56974, #61877, #30414, #51725, #25158, #67797 ),
 .UNSPECIFIED., .F., .F.,
 ( 4, 2, 2, 2, 2, 2, 2, 2, 4 ),
 ( 0.000000000000000000, 0.1249999999999996669, 0.2499999999999993339, 0.3749999999999990008, 0.4999999999999986677, 0.6249999999999990008, 0.7499999999999993339, 0.8749999999999996669, 1.000000000000000000 ),
 .UNSPECIFIED. ) ;
#40699 = CARTESIAN_POINT ( 'NONE',  ( 17.74252317112528132, 0.7057854747025454900, 13.98219993205038669 ) ) ;
#40700 = CIRCLE ( 'NONE', #12821, 1.000000000000000000 ) ;
#40701 = CARTESIAN_POINT ( 'NONE',  ( 18.12922381500399993, 3.157787539580000136, 11.36563583066999961 ) ) ;
#40702 = CARTESIAN_POINT ( 'NONE',  ( 10.88016425062000003, -2.793121555136000023, -6.864957546339999439 ) ) ;
#40703 = ADVANCED_FACE ( 'NONE', ( #33414 ), #55077, .T. ) ;
#40704 = ORIENTED_EDGE ( 'NONE', *, *, #27085, .T. ) ;
#40705 = ORIENTED_EDGE ( 'NONE', *, *, #57684, .F. ) ;
#40706 = CARTESIAN_POINT ( 'NONE',  ( 10.19741084123000086, 4.262870449202000422, -8.811513791423999820 ) ) ;
#40707 = DIRECTION ( 'NONE',  ( -1.000000000000000000, 0.000000000000000000, 0.000000000000000000 ) ) ;
#40708 = CARTESIAN_POINT ( 'NONE',  ( 7.392379606866390951, -4.680093573814123609, 6.319105353947795933 ) ) ;
#40709 = CARTESIAN_POINT ( 'NONE',  ( 25.52342880444300022, 8.321935307164999074, -8.140383335223001282 ) ) ;
#40710 = CARTESIAN_POINT ( 'NONE',  ( 23.91242621194999884, 9.487396930725999766, -9.248180533506999978 ) ) ;
#40712 = AXIS2_PLACEMENT_3D ( 'NONE', #28115, #49426, #1539 ) ;
#40711 = DIRECTION ( 'NONE',  ( 0.000000000000000000, -0.9916377111174247139, 0.1290528957048031888 ) ) ;
#40714 = CARTESIAN_POINT ( 'NONE',  ( 7.785640454728832260, 3.765028847004302293, 6.163541840524195514 ) ) ;
#40713 = CARTESIAN_POINT ( 'NONE',  ( 10.76492546752099955, -5.139081147506999514, 7.578921399676699089 ) ) ;
#40715 = CARTESIAN_POINT ( 'NONE',  ( 9.091433907306445406, 4.945719512329345591, -8.331756427597948544 ) ) ;
#40716 = ORIENTED_EDGE ( 'NONE', *, *, #21080, .F. ) ;
#40717 = CARTESIAN_POINT ( 'NONE',  ( 21.60000012424471194, 3.970157536060000036E-13, -13.89999856298982372 ) ) ;
#40718 = CARTESIAN_POINT ( 'NONE',  ( 10.99021017617000062, -2.939022385911000068, -5.190637231063000456 ) ) ;
#40719 = CARTESIAN_POINT ( 'NONE',  ( 9.886323620223000930, -4.261100936929000049, -5.979198511086000423 ) ) ;
#40720 = LINE ( 'NONE', #15183, #47024 ) ;
#40721 = CARTESIAN_POINT ( 'NONE',  ( 5.700000000000000178, -1.250000000000000000, 0.000000000000000000 ) ) ;
#40722 = CARTESIAN_POINT ( 'NONE',  ( 11.05000833411999928, -5.233205726482999864, 5.017018830968000387 ) ) ;
#40723 = CARTESIAN_POINT ( 'NONE',  ( 9.839810841229999383, 5.817107086401000160, -6.945352709928000579 ) ) ;
#40724 = EDGE_CURVE ( 'NONE', #24902, #43188, #37146, .T. ) ;
#40725 = EDGE_CURVE ( 'NONE', #11902, #6623, #1902, .T. ) ;
#40726 = LINE ( 'NONE', #68660, #23283 ) ;
#40727 = AXIS2_PLACEMENT_3D ( 'NONE', #29743, #51046, #3147 ) ;
#40728 = EDGE_CURVE ( 'NONE', #34244, #56244, #50181, .T. ) ;
#40729 = CARTESIAN_POINT ( 'NONE',  ( 11.01811411617009817, 2.973039408543999951, 7.174999999999999822 ) ) ;
#40730 = B_SPLINE_SURFACE_WITH_KNOTS ( 'NONE', 3, 3, ( 
 ( #61987, #67559, #23892, #41005 ),
 ( #18309, #50462, #2563, #12719 ),
 ( #19329, #66533, #45573, #34051 ),
 ( #66879, #50124, #61300, #7461 ),
 ( #18653, #34399, #55717, #39986 ),
 ( #9179, #47286, #62328, #31550 ),
 ( #37134, #36101, #35763, #68942 ),
 ( #31216, #9521, #26304, #30519 ) ),
 .UNSPECIFIED., .F., .F., .F.,
 ( 4, 1, 1, 1, 1, 4 ),
 ( 4, 4 ),
 ( 0.7453054410233999061, 0.7647058823529000460, 0.8235294117646999590, 0.8823529411764999830, 0.9411764705882000870, 0.9905827552260000335 ),
 ( -0.1830915166815000050, 1.182948990397000077 ),
 .UNSPECIFIED. ) ;
#40731 = CARTESIAN_POINT ( 'NONE',  ( 25.29986734212600297, -2.258942858049999725, 12.29419282279000036 ) ) ;
#40732 = AXIS2_PLACEMENT_3D ( 'NONE', #5175, #37338, #21257 ) ;
#40733 = CARTESIAN_POINT ( 'NONE',  ( 3.587066914515000260, -2.899936811858999874, -1.487130161374000004 ) ) ;
#40734 = ORIENTED_EDGE ( 'NONE', *, *, #10251, .F. ) ;
#40735 = CARTESIAN_POINT ( 'NONE',  ( 12.36315700431396358, 0.5707228546306866157, -12.58707662888203771 ) ) ;
#40736 = CARTESIAN_POINT ( 'NONE',  ( 12.18001542466667608, -2.493364570470032682, -12.45310825068047045 ) ) ;
#40737 = CARTESIAN_POINT ( 'NONE',  ( 14.00000000000000178, -50.50083396221999976, -44.47484963936999947 ) ) ;
#40738 = CARTESIAN_POINT ( 'NONE',  ( 8.513426658773999733, 5.040787533781999841, 8.522957620707000359 ) ) ;
#40739 = FILL_AREA_STYLE ('',( #14178 ) ) ;
#40740 = ORIENTED_EDGE ( 'NONE', *, *, #26798, .F. ) ;
#40741 = CARTESIAN_POINT ( 'NONE',  ( 6.400593184916999689, -0.6732323296109999911, -0.9643333493903999409 ) ) ;
#40742 = PRODUCT_CONTEXT ( 'NONE', #12359, 'mechanical' ) ;
#40743 = CARTESIAN_POINT ( 'NONE',  ( 17.91195086076331577, 0.5131995812820130398, 12.68604179104477758 ) ) ;
#40744 = CARTESIAN_POINT ( 'NONE',  ( 13.05728973496400336, -11.72286803092000085, -1.966956593348999860 ) ) ;
#40745 = CARTESIAN_POINT ( 'NONE',  ( 7.856851002541000106, 2.832432432432000269, -6.822293592207000934 ) ) ;
#40746 = CARTESIAN_POINT ( 'NONE',  ( 10.59725056272499977, 5.316133253199000208, -7.519505747156228992 ) ) ;
#40747 = ORIENTED_EDGE ( 'NONE', *, *, #52390, .T. ) ;
#40748 = CARTESIAN_POINT ( 'NONE',  ( 10.59303089732000025, -2.436232726560000117, 7.793465286118999913 ) ) ;
#40749 = ORIENTED_EDGE ( 'NONE', *, *, #19624, .F. ) ;
#40750 = EDGE_CURVE ( 'NONE', #28041, #2109, #33065, .T. ) ;
#40751 = CARTESIAN_POINT ( 'NONE',  ( 9.110944094209999733, 5.100000000000000533, -6.571291218949999902 ) ) ;
#40752 = CARTESIAN_POINT ( 'NONE',  ( 7.700043146791999860, -3.346260729029000291, 6.002247316312999459 ) ) ;
#40753 = VECTOR ( 'NONE', #36426, 1000.000000000000114 ) ;
#40754 = CARTESIAN_POINT ( 'NONE',  ( 18.25212991285167519, -0.2010519787742862108, -13.99856097495847607 ) ) ;
#40755 = ORIENTED_EDGE ( 'NONE', *, *, #868, .F. ) ;
#40756 = CARTESIAN_POINT ( 'NONE',  ( 23.62967491266149977, 10.06690055933806782, 9.667224302797498225 ) ) ;
#40757 = DIRECTION ( 'NONE',  ( 1.000000000000000000, 0.000000000000000000, 0.000000000000000000 ) ) ;
#40758 = CARTESIAN_POINT ( 'NONE',  ( 6.745189158770999782, 3.508889101792000087, -8.808374944720000599 ) ) ;
#40759 = CARTESIAN_POINT ( 'NONE',  ( 8.350387243830999395, 3.399999999999999911, 6.632262360512000576 ) ) ;
#40760 = CARTESIAN_POINT ( 'NONE',  ( 24.52306329324777323, 3.339076860759809584, 12.06942449950906138 ) ) ;
#40761 = ORIENTED_EDGE ( 'NONE', *, *, #62774, .T. ) ;
#40762 = CARTESIAN_POINT ( 'NONE',  ( 2.250973465874000379, -3.500000000000000000, 0.000000000000000000 ) ) ;
#40763 = CARTESIAN_POINT ( 'NONE',  ( 12.21224535004423117, -2.300944246481291255, -13.71363154655825767 ) ) ;
#40764 = CARTESIAN_POINT ( 'NONE',  ( 11.33570505509991655, 4.908984911270270146, -7.175001305235313431 ) ) ;
#40765 = CARTESIAN_POINT ( 'NONE',  ( 10.57793869653000129, -4.393380534095000733, -6.024358525186999991 ) ) ;
#40766 = DIRECTION ( 'NONE',  ( 1.000000000000000000, 0.000000000000000000, 0.000000000000000000 ) ) ;
#40767 = ORIENTED_EDGE ( 'NONE', *, *, #62314, .F. ) ;
#40768 = CARTESIAN_POINT ( 'NONE',  ( 17.95596346652836672, 0.4795055876567429487, -13.88886709646117801 ) ) ;
#40769 = FACE_OUTER_BOUND ( 'NONE', #17379, .T. ) ;
#40770 = CARTESIAN_POINT ( 'NONE',  ( 23.95415751879778199, -3.345976127950229806, -12.83253842359969710 ) ) ;
#40771 = DIRECTION ( 'NONE',  ( 0.000000000000000000, -1.000000000000000000, 0.000000000000000000 ) ) ;
#40772 = CARTESIAN_POINT ( 'NONE',  ( 12.20137680394560320, 0.1621987986621312994, -13.89873133405096617 ) ) ;
#40773 = VECTOR ( 'NONE', #62957, 1000.000000000000114 ) ;
#40774 = CARTESIAN_POINT ( 'NONE',  ( 18.09877017944544164, -2.191112624880879878, 12.51823083080035204 ) ) ;
#40775 = VERTEX_POINT ( 'NONE', #18370 ) ;
#40776 = CARTESIAN_POINT ( 'NONE',  ( 10.56591429142999949, -3.980313504646230349, -6.466681092390999197 ) ) ;
#40777 = ORIENTED_EDGE ( 'NONE', *, *, #60224, .T. ) ;
#40778 = CARTESIAN_POINT ( 'NONE',  ( 10.81579666500999970, 5.374569445151000657, 6.698728322222000209 ) ) ;
#40779 = CONICAL_SURFACE ( 'NONE', #10626, 1.699999998954999869, 0.7853981633972997312 ) ;
#40780 = CARTESIAN_POINT ( 'NONE',  ( 24.30000000000000071, 11.85420044612000012, 3.901016762742000488 ) ) ;
#40781 = CARTESIAN_POINT ( 'NONE',  ( 8.789679719592999874, 4.162493982103000256, -5.775210092227999858 ) ) ;
#40782 = CARTESIAN_POINT ( 'NONE',  ( 2.935841626129000126, 1.641030631418000096, -3.325153953193000333 ) ) ;
#40783 = CARTESIAN_POINT ( 'NONE',  ( 10.48414299032999963, -4.098653366703000067, -9.351353705206001621 ) ) ;
#40784 = CARTESIAN_POINT ( 'NONE',  ( 9.231616107288068918, -3.999997736744774546, 6.618420992905502231 ) ) ;
#40785 = FACE_OUTER_BOUND ( 'NONE', #56075, .T. ) ;
#40786 = EDGE_CURVE ( 'NONE', #3413, #57059, #39419, .T. ) ;
#40787 = EDGE_CURVE ( 'NONE', #5467, #63876, #12549, .T. ) ;
#40788 = ORIENTED_EDGE ( 'NONE', *, *, #4327, .F. ) ;
#40789 = EDGE_CURVE ( 'NONE', #36346, #68681, #22562, .T. ) ;
#40790 = CARTESIAN_POINT ( 'NONE',  ( 10.71462282008599942, -3.476853648246800432, 6.656181553372300108 ) ) ;
#40791 = CARTESIAN_POINT ( 'NONE',  ( 10.59536758177122096, 2.228958812539000522, -7.375678105216161740 ) ) ;
#40792 = CARTESIAN_POINT ( 'NONE',  ( 16.08724299200000019, 9.224388201582000235, 8.529033888242999240 ) ) ;
#40793 = CARTESIAN_POINT ( 'NONE',  ( 10.81746213571000048, 5.100000000000000533, 6.571291218949999902 ) ) ;
#40795 = CARTESIAN_POINT ( 'NONE',  ( 24.35365242081700288, -2.582848009905001074, -11.10541636514000174 ) ) ;
#40794 = CARTESIAN_POINT ( 'NONE',  ( 9.228133567168001150, 2.875367362387999837, 8.669940206484001877 ) ) ;
#40796 = CARTESIAN_POINT ( 'NONE',  ( 10.62487750876920067, 3.456442671114800191, -8.343502390669698343 ) ) ;
#40797 = CARTESIAN_POINT ( 'NONE',  ( 24.48566044703800060, -12.12924491941999960, 3.164389501723999576 ) ) ;
#40798 = AXIS2_PLACEMENT_3D ( 'NONE', #61956, #35733, #30488 ) ;
#40799 = CARTESIAN_POINT ( 'NONE',  ( 9.882975701332998852, 4.736880367605800224, -8.182531775206799196 ) ) ;
#40800 = CARTESIAN_POINT ( 'NONE',  ( 18.10839966799241552, 0.4648927885597754495, 12.59142395508373014 ) ) ;
#40801 = B_SPLINE_CURVE_WITH_KNOTS ( 'NONE', 3,
 ( #49489, #64518, #65216, #12091 ),
 .UNSPECIFIED., .F., .F.,
 ( 4, 4 ),
 ( 0.000000000000000000, 1.000000000000000000 ),
 .UNSPECIFIED. ) ;
#40802 = CARTESIAN_POINT ( 'NONE',  ( 24.30000000000000071, 11.76537389984999926, -3.877215761401999750 ) ) ;
#40803 = CARTESIAN_POINT ( 'NONE',  ( 10.68035971519489813, 4.678140486081599825, 8.628134814664999652 ) ) ;
#40804 = CARTESIAN_POINT ( 'NONE',  ( 23.55075185133400240, 10.43333017688000020, 9.388795336593998897 ) ) ;
#40805 = ORIENTED_EDGE ( 'NONE', *, *, #34272, .F. ) ;
#40806 = CARTESIAN_POINT ( 'NONE',  ( 8.604019353210000887, -5.165500668528999917, 8.645534272955000432 ) ) ;
#40807 = CARTESIAN_POINT ( 'NONE',  ( 4.000000000000000000, 0.5625597044909160793, -2.094005558844440618 ) ) ;
#40808 = CARTESIAN_POINT ( 'NONE',  ( 10.40685100253999984, 2.832432432432000269, -6.822293592207000934 ) ) ;
#40809 = CARTESIAN_POINT ( 'NONE',  ( 24.53429010490700080, 8.855930189872001534, 9.286429716155000236 ) ) ;
#40810 = ORIENTED_EDGE ( 'NONE', *, *, #65212, .T. ) ;
#40811 = CARTESIAN_POINT ( 'NONE',  ( 7.743176658771999676, 2.735218126362000124, 6.771983639047999937 ) ) ;
#40813 = CARTESIAN_POINT ( 'NONE',  ( 10.59725056272499977, 5.316133253199000208, 7.480494252843770120 ) ) ;
#40812 = CARTESIAN_POINT ( 'NONE',  ( 9.839304848515999069, -3.211495113978299898, -7.860510733857099197 ) ) ;
#40814 = CARTESIAN_POINT ( 'NONE',  ( 9.991525552923999243, 4.805950298207000593, -8.932431532051998246 ) ) ;
#40815 = ORIENTED_EDGE ( 'NONE', *, *, #57128, .F. ) ;
#40816 = DIRECTION ( 'NONE',  ( 5.812104846703281941E-06, -0.9659358880878460285, -0.2587814909729125312 ) ) ;
#40817 = CARTESIAN_POINT ( 'NONE',  ( 24.67921580188599862, 3.567514645466999923, -12.13750897870000145 ) ) ;
#40818 = CARTESIAN_POINT ( 'NONE',  ( 11.03502897915239878, 4.327133900127000388, 6.264564938179000286 ) ) ;
#40819 = CARTESIAN_POINT ( 'NONE',  ( 20.60000000000000142, -12.34999999999999964, -4.046978686977000011E-05 ) ) ;
#40820 = CARTESIAN_POINT ( 'NONE',  ( 8.221179504219003675, 3.443168248977001245, 6.131664885159996636 ) ) ;
#40821 = ORIENTED_EDGE ( 'NONE', *, *, #51605, .F. ) ;
#40822 = CARTESIAN_POINT ( 'NONE',  ( 11.10000000009000054, -2.699999999911000259, 6.571291220400000022 ) ) ;
#40823 = CYLINDRICAL_SURFACE ( 'NONE', #12797, 2.000000000000000000 ) ;
#40824 = CARTESIAN_POINT ( 'NONE',  ( 8.246323025216810265, -5.454251951018638245, 8.457608258087930153 ) ) ;
#40825 = CIRCLE ( 'NONE', #11778, 13.92493900950999652 ) ;
#40826 = CARTESIAN_POINT ( 'NONE',  ( 10.59725056272499977, -2.683866746800999792, -7.519505747156228992 ) ) ;
#40827 = CARTESIAN_POINT ( 'NONE',  ( 9.068822372493999140, -4.328199826929600036, 6.426348619097999482 ) ) ;
#40828 = VERTEX_POINT ( 'NONE', #66248 ) ;
#40829 = CARTESIAN_POINT ( 'NONE',  ( 10.77808207294999931, -5.296125810246000043, -4.800100549618000478 ) ) ;
#40830 = B_SPLINE_CURVE_WITH_KNOTS ( 'NONE', 3,
 ( #29922, #20095, #2981, #45648, #66954, #19061, #62730, #25337, #61711, #19407, #51560, #3325, #25680, #46675, #35833, #46329, #24657, #51901 ),
 .UNSPECIFIED., .F., .F.,
 ( 4, 2, 2, 2, 2, 2, 2, 2, 4 ),
 ( 0.000000000000000000, 0.1249999999999999722, 0.2499999999999999445, 0.3749999999999998890, 0.4999999999999998890, 0.6249999999999998890, 0.7499999999999998890, 0.8750000000000000000, 1.000000000000000000 ),
 .UNSPECIFIED. ) ;
#40831 = CARTESIAN_POINT ( 'NONE',  ( 11.09195391537400077, -2.942766577210000012, 6.781965272201699868 ) ) ;
#40832 = ORIENTED_EDGE ( 'NONE', *, *, #34750, .F. ) ;
#40833 = EDGE_CURVE ( 'NONE', #28283, #43730, #33475, .T. ) ;
#40834 = CARTESIAN_POINT ( 'NONE',  ( 9.893930206848999376, -5.250000000000000000, 7.500000000000000000 ) ) ;
#40835 = EDGE_LOOP ( 'NONE', ( #5101, #68521, #5938, #53114 ) ) ;
#40836 = CARTESIAN_POINT ( 'NONE',  ( 9.661149330668999724, -3.300107492866999781, -5.762405935562999737 ) ) ;
#40837 = CARTESIAN_POINT ( 'NONE',  ( 10.32322128467999889, -3.399999874579999748, -4.621083553505000552 ) ) ;
#40838 = CARTESIAN_POINT ( 'NONE',  ( 8.174990947233128580, -2.650692654197974729, 7.500004443805800669 ) ) ;
#40839 = CARTESIAN_POINT ( 'NONE',  ( 11.05569598648999907, -2.869047858956000230, 6.826612223887499553 ) ) ;
#40840 = CARTESIAN_POINT ( 'NONE',  ( 12.41357648242114919, 2.012680472106851859, -12.55187634341709213 ) ) ;
#40841 = CARTESIAN_POINT ( 'NONE',  ( 11.31764560330029923, -3.650429500487800460, 8.585859374935999710 ) ) ;
#40842 = CARTESIAN_POINT ( 'NONE',  ( 7.950760841228999176, 2.095715612964000218, 8.056490963156001328 ) ) ;
#40843 = EDGE_LOOP ( 'NONE', ( #25825, #51480, #34031, #63007, #53997, #45795, #52629 ) ) ;
#40844 = B_SPLINE_CURVE_WITH_KNOTS ( 'NONE', 3,
 ( #54585, #49331, #44109, #44462 ),
 .UNSPECIFIED., .F., .F.,
 ( 4, 4 ),
 ( 0.000000000000000000, 1.000000000000000000 ),
 .UNSPECIFIED. ) ;
#40845 = DIRECTION ( 'NONE',  ( 0.000000000000000000, 0.8514543052404082157, -0.5244287998266055073 ) ) ;
#40846 = VECTOR ( 'NONE', #38834, 1000.000000000000000 ) ;
#40847 = CARTESIAN_POINT ( 'NONE',  ( 8.187144353207999714, -4.968144979409999884, 5.971795951526999602 ) ) ;
#40848 = CARTESIAN_POINT ( 'NONE',  ( 7.100000000000000533, 12.35000000006999876, 0.000000000000000000 ) ) ;
#40849 = ORIENTED_EDGE ( 'NONE', *, *, #58026, .T. ) ;
#40850 = CARTESIAN_POINT ( 'NONE',  ( 12.74469048821896955, -1.763307075768893784, -12.47600695802491089 ) ) ;
#40852 = CARTESIAN_POINT ( 'NONE',  ( 11.03502897915239878, 4.327133900127000388, 6.264564938179000286 ) ) ;
#40851 = VECTOR ( 'NONE', #57615, 999.9999999999998863 ) ;
#40853 = CARTESIAN_POINT ( 'NONE',  ( 10.44811814679000150, -5.235603901491000300, -6.609968500665999613 ) ) ;
#40854 = DIRECTION ( 'NONE',  ( 0.000000000000000000, 0.000000000000000000, -1.000000000000000000 ) ) ;
#40855 = CARTESIAN_POINT ( 'NONE',  ( 18.16350100824700320, -3.138009765975000143, -11.88148072165000002 ) ) ;
#40856 = CARTESIAN_POINT ( 'NONE',  ( 9.393930206848999376, -5.250000000000000000, -7.500000000000000000 ) ) ;
#40857 = CARTESIAN_POINT ( 'NONE',  ( 12.57340716663137670, -1.919420395509098931, -13.77954053360031672 ) ) ;
#40858 = CARTESIAN_POINT ( 'NONE',  ( 11.76133460557259980, -3.860150918677800025, -8.354833838171700222 ) ) ;
#40859 = CARTESIAN_POINT ( 'NONE',  ( 10.37041638348499895, -5.241705141469999774, -7.197535585171899619 ) ) ;
#40861 = DIRECTION ( 'NONE',  ( 0.000000000000000000, 0.000000000000000000, -1.000000000000000000 ) ) ;
#40860 = B_SPLINE_CURVE_WITH_KNOTS ( 'NONE', 3,
 ( #68283, #46641, #51530, #35464 ),
 .UNSPECIFIED., .F., .F.,
 ( 4, 4 ),
 ( 0.000000000000000000, 1.000000000000000000 ),
 .UNSPECIFIED. ) ;
#40862 = ORIENTED_EDGE ( 'NONE', *, *, #15141, .T. ) ;
#40863 = ORIENTED_EDGE ( 'NONE', *, *, #47317, .F. ) ;
#40864 = CARTESIAN_POINT ( 'NONE',  ( 7.099999886593999499, 1.243449787579999883E-13, -1.714758320200999846E-13 ) ) ;
#40865 = PRESENTATION_STYLE_ASSIGNMENT (( #25815 ) ) ;
#40866 = DIRECTION ( 'NONE',  ( 0.000000000000000000, -0.8648648648648717963, -0.5020047465136829867 ) ) ;
#40867 = CARTESIAN_POINT ( 'NONE',  ( 18.16281717172225996, 2.646070501177852030, 13.64134067051623411 ) ) ;
#40868 = CARTESIAN_POINT ( 'NONE',  ( 10.61721774768000159, 5.045603402166999985, -6.386910706193999587 ) ) ;
#40869 = DIRECTION ( 'NONE',  ( 1.000000000000000000, 0.000000000000000000, 0.000000000000000000 ) ) ;
#40870 = CARTESIAN_POINT ( 'NONE',  ( 8.893204545428000429, -4.599999999999999645, -6.188268997401999982 ) ) ;
#40871 = CARTESIAN_POINT ( 'NONE',  ( 23.51511290156300404, -13.45754537663000150, 4.321901134974000414 ) ) ;
#40872 = ADVANCED_FACE ( 'NONE', ( #49831 ), #34108, .T. ) ;
#40874 = EDGE_CURVE ( 'NONE', #29433, #27164, #22220, .T. ) ;
#40873 = CARTESIAN_POINT ( 'NONE',  ( 10.96580581817999978, 4.930645553951000792, 6.170542400361000546 ) ) ;
#40875 = CARTESIAN_POINT ( 'NONE',  ( 9.272923981633081070, -3.689545703815816591, 6.685328252913995684 ) ) ;
#40876 = EDGE_CURVE ( 'NONE', #53930, #61548, #55427, .T. ) ;
#40877 = ADVANCED_FACE ( 'NONE', ( #54032 ), #43556, .T. ) ;
#40878 = VERTEX_POINT ( 'NONE', #59629 ) ;
#40879 = CARTESIAN_POINT ( 'NONE',  ( 12.18529561036837983, -2.583342615503333217, 12.43180850209203037 ) ) ;
#40880 = CARTESIAN_POINT ( 'NONE',  ( 9.273063610504998167, -3.644370728184199937, -8.290718512198798962 ) ) ;
#40881 = CARTESIAN_POINT ( 'NONE',  ( 11.18706938844999854, 3.186790175674999670, 6.232702730851999995 ) ) ;
#40882 = CARTESIAN_POINT ( 'NONE',  ( 11.35168717260510007, -4.613789146762799831, 6.498190316041999814 ) ) ;
#40883 = CARTESIAN_POINT ( 'NONE',  ( 7.267555237352232744, -0.6773954909162061000, 0.9416021803066277895 ) ) ;
#40884 = CARTESIAN_POINT ( 'NONE',  ( 10.24733997687999931, 4.272363749081500295, -6.251346978035999591 ) ) ;
#40885 = CARTESIAN_POINT ( 'NONE',  ( 12.18028569061552879, -0.01996654564806360846, 12.69998441237379083 ) ) ;
#40886 = AXIS2_PLACEMENT_3D ( 'NONE', #10220, #47288, #64718 ) ;
#40887 = CARTESIAN_POINT ( 'NONE',  ( 8.610051658774001027, 5.329437560656000272, 6.027391099688998999 ) ) ;
#40888 = CARTESIAN_POINT ( 'NONE',  ( 10.87021720923999979, 2.226038107033000202, 7.782753921296999167 ) ) ;
#40889 = CARTESIAN_POINT ( 'NONE',  ( 8.793536308085935005, -2.899999999999999911, 6.665341197419078156 ) ) ;
#40890 = EDGE_LOOP ( 'NONE', ( #66065, #58345, #31747, #31087 ) ) ;
#40891 = CARTESIAN_POINT ( 'NONE',  ( 8.789679719592999874, 4.162493982103000256, -5.775210092227999858 ) ) ;
#40892 = CARTESIAN_POINT ( 'NONE',  ( 7.193989102394000135, 0.8129426006129999438, -1.245101619383000235 ) ) ;
#40893 = ADVANCED_FACE ( 'NONE', ( #55772 ), #63492, .F. ) ;
#40894 = CARTESIAN_POINT ( 'NONE',  ( 10.92932301586054145, -2.313027949505928493, 7.958417374028298852 ) ) ;
#40896 = CARTESIAN_POINT ( 'NONE',  ( 8.216851002544000693, 2.832432432432000269, 6.822293592207000934 ) ) ;
#40895 = CARTESIAN_POINT ( 'NONE',  ( 7.994581853207999522, -2.263562268490999951, 8.007440964304000985 ) ) ;
#40897 = CARTESIAN_POINT ( 'NONE',  ( 16.39999999379500295, 3.351248059343999941, 11.15756683833000018 ) ) ;
#40898 = CARTESIAN_POINT ( 'NONE',  ( 11.48641235500450009, -4.739919807690899489, -6.822158181405299615 ) ) ;
#40899 = VERTEX_POINT ( 'NONE', #14497 ) ;
#40900 = AXIS2_PLACEMENT_3D ( 'NONE', #48293, #65748, #6320 ) ;
#40901 = CARTESIAN_POINT ( 'NONE',  ( 0.9621534748591999975, 2.512752844666000129, -2.494243791339000094 ) ) ;
#40902 = CARTESIAN_POINT ( 'NONE',  ( 12.11873369409612522, 11.72532246831247349, -3.796278118047919925 ) ) ;
#40904 = CARTESIAN_POINT ( 'NONE',  ( 13.73837349797500096, -9.670565172354999461, -8.019813433522999802 ) ) ;
#40903 = CARTESIAN_POINT ( 'NONE',  ( 9.686609873374599999, 5.723279044498072565, 7.204524705702328724 ) ) ;
#40905 = CARTESIAN_POINT ( 'NONE',  ( 23.66004879239100234, -9.998910854163000295, -9.691527647852998584 ) ) ;
#40906 = CARTESIAN_POINT ( 'NONE',  ( 13.63350196149407267, 9.056970873722406168, 7.433404858428185769 ) ) ;
#40907 = CARTESIAN_POINT ( 'NONE',  ( 12.51458961313714724, -3.187047769811533815, 13.63241538057482494 ) ) ;
#40908 = DIRECTION ( 'NONE',  ( 1.000000000000000000, 0.000000000000000000, 0.000000000000000000 ) ) ;
#40909 = CARTESIAN_POINT ( 'NONE',  ( 9.970944094204998720, 5.100000000000000533, 6.571291218949999902 ) ) ;
#40910 = CARTESIAN_POINT ( 'NONE',  ( 8.913566940379999082, -2.550589632307000088, 8.854674225901000284 ) ) ;
#40911 = VERTEX_POINT ( 'NONE', #19043 ) ;
#40912 = CARTESIAN_POINT ( 'NONE',  ( 9.395323341230000125, 5.146726419831999522, 6.597424767138000412 ) ) ;
#40914 = FACE_OUTER_BOUND ( 'NONE', #24418, .T. ) ;
#40913 = CARTESIAN_POINT ( 'NONE',  ( 5.548748128158000448, 0.07932534654105999339, 1.466367974616999748 ) ) ;
#40915 = CARTESIAN_POINT ( 'NONE',  ( 7.578319455099681967, -4.092892350974873139, 5.763267803938307843 ) ) ;
#40916 = CARTESIAN_POINT ( 'NONE',  ( 7.716851002542999716, -2.832432432432000269, 6.822293592207000934 ) ) ;
#40917 = CARTESIAN_POINT ( 'NONE',  ( 0.9326546106848000450, -3.242811033061999915, 1.104080751309999942 ) ) ;
#40918 = ORIENTED_EDGE ( 'NONE', *, *, #55802, .F. ) ;
#40919 = DIRECTION ( 'NONE',  ( 0.000000000000000000, 1.000000000000000000, 0.000000000000000000 ) ) ;
#40920 = CARTESIAN_POINT ( 'NONE',  ( 10.83364828895399867, -3.239803852721999888, 7.084788038520800413 ) ) ;
#40921 = CARTESIAN_POINT ( 'NONE',  ( 11.58810207955109917, 3.203462856645999945, 7.825000000000000178 ) ) ;
#40922 = CARTESIAN_POINT ( 'NONE',  ( 11.18484176840999922, 2.599663474744000169, 7.740674686800000259 ) ) ;
#40923 = EDGE_CURVE ( 'NONE', #63702, #23202, #35815, .T. ) ;
#40924 = CARTESIAN_POINT ( 'NONE',  ( 11.65456516821461008, 4.802916961510000249, 6.689681884064299311 ) ) ;
#40925 = CARTESIAN_POINT ( 'NONE',  ( 23.77344028463681269, -3.285535634723865339, 13.18386468110849208 ) ) ;
#40926 = EDGE_CURVE ( 'NONE', #41305, #51740, #2631, .T. ) ;
#40927 = CARTESIAN_POINT ( 'NONE',  ( 8.668612063651316646, -4.202134689411700208, 5.871184905936384979 ) ) ;
#40928 = CARTESIAN_POINT ( 'NONE',  ( 12.18936456685733916, -2.391983199617479627, 12.47610573829959435 ) ) ;
#40929 = CARTESIAN_POINT ( 'NONE',  ( 7.586311969103031849, 4.230699495907120244, 5.772666978407863247 ) ) ;
#40930 = ORIENTED_EDGE ( 'NONE', *, *, #20371, .F. ) ;
#40931 = VECTOR ( 'NONE', #47734, 1000.000000000000000 ) ;
#40932 = CARTESIAN_POINT ( 'NONE',  ( 17.55505043854147118, -1.875000000000000000, 13.78631952119025605 ) ) ;
#40933 = FACE_OUTER_BOUND ( 'NONE', #51318, .T. ) ;
#40934 = ORIENTED_EDGE ( 'NONE', *, *, #48529, .T. ) ;
#40935 = CARTESIAN_POINT ( 'NONE',  ( 9.049999337612000261, 3.268496584495999908E-13, 3.612668863294000056E-14 ) ) ;
#40936 = CARTESIAN_POINT ( 'NONE',  ( 13.49998535730550664, -12.08447166622790014, -2.429352492459242896 ) ) ;
#40937 = CYLINDRICAL_SURFACE ( 'NONE', #48334, 1.000000000000000444 ) ;
#40938 = CARTESIAN_POINT ( 'NONE',  ( 11.24441369783139777, 3.956299011112040187, 6.634905315059499209 ) ) ;
#40939 = CIRCLE ( 'NONE', #46535, 12.60000000000000142 ) ;
#40940 = CARTESIAN_POINT ( 'NONE',  ( 9.352253013669001191, 2.817757427878999632, 6.388459691516000127 ) ) ;
#40941 = CARTESIAN_POINT ( 'NONE',  ( 10.81362367151999848, 3.876947539724999725, -9.022206283674000460 ) ) ;
#40942 = CARTESIAN_POINT ( 'NONE',  ( 9.834799664234624927, -3.204277625948437347, -7.863810627050381363 ) ) ;
#40943 = CARTESIAN_POINT ( 'NONE',  ( 11.01776264201000011, -4.914128622650000722, 8.587713430305999651 ) ) ;
#40944 = CARTESIAN_POINT ( 'NONE',  ( 18.21574167892471152, -0.2964030593063894936, -12.59651778044212556 ) ) ;
#40945 = AXIS2_PLACEMENT_3D ( 'NONE', #9953, #50891, #68670 ) ;
#40946 = CARTESIAN_POINT ( 'NONE',  ( 5.500000000000000000, 6.217248937900999058E-14, 3.708144902247999495E-14 ) ) ;
#40947 = CARTESIAN_POINT ( 'NONE',  ( 11.14595257254739913, -4.831736303435800295, -7.741895249827200232 ) ) ;
#40948 = CARTESIAN_POINT ( 'NONE',  ( 8.175760841228999709, 2.599243720295000060, 7.909344432242998657 ) ) ;
#40949 = EDGE_LOOP ( 'NONE', ( #18116, #36360, #1275, #48665 ) ) ;
#40950 =( REPRESENTATION_RELATIONSHIP ('NONE','NONE', #10823, #26842 ) REPRESENTATION_RELATIONSHIP_WITH_TRANSFORMATION ( #27076 )SHAPE_REPRESENTATION_RELATIONSHIP( ) );
#40951 = CIRCLE ( 'NONE', #50981, 10.75000000000000533 ) ;
#40952 = CARTESIAN_POINT ( 'NONE',  ( 11.01817738136000102, -5.556757561671000545, -4.991717353675000801 ) ) ;
#40953 = DIRECTION ( 'NONE',  ( 0.000000000000000000, 0.000000000000000000, -1.000000000000000000 ) ) ;
#40954 = CARTESIAN_POINT ( 'NONE',  ( 10.90000000000000036, -2.399999999999999911, -6.571291218949999902 ) ) ;
#40955 = CARTESIAN_POINT ( 'NONE',  ( 7.608454017953003579, 10.31012780980999999, 5.117594110825002041 ) ) ;
#40956 = CARTESIAN_POINT ( 'NONE',  ( 9.405747021775999528, 3.038503783616799847, -8.343747244947598674 ) ) ;
#40957 = CARTESIAN_POINT ( 'NONE',  ( 12.29798916261918329, 1.995979084551873450, 13.85698889012213186 ) ) ;
#40958 = CARTESIAN_POINT ( 'NONE',  ( 10.91307648679999964, -2.096298111716999646, 7.827187677719999570 ) ) ;
#40959 = EDGE_LOOP ( 'NONE', ( #42913, #9450, #20401, #45209, #44894, #16257, #55310, #52163, #34917, #29191, #51919, #34481, #39634 ) ) ;
#40960 = CARTESIAN_POINT ( 'NONE',  ( 12.70148909168772455, 0.6166679310397558123, -12.67983904305986087 ) ) ;
#40961 = EDGE_CURVE ( 'NONE', #57158, #52029, #58471, .T. ) ;
#40962 = CARTESIAN_POINT ( 'NONE',  ( 12.08616987952487598, -0.09542514088231011937, 13.99967976774382272 ) ) ;
#40963 = EDGE_CURVE ( 'NONE', #20386, #3072, #8109, .T. ) ;
#40964 = ORIENTED_EDGE ( 'NONE', *, *, #60102, .T. ) ;
#40965 = CARTESIAN_POINT ( 'NONE',  ( 25.59994555223599733, 2.024003533649000097, -11.01554633311000053 ) ) ;
#40966 = CARTESIAN_POINT ( 'NONE',  ( 7.100000000000000533, 0.000000000000000000, 0.000000000000000000 ) ) ;
#40967 = CARTESIAN_POINT ( 'NONE',  ( 10.84393020684979980, -5.250000000000000000, -7.500000000000000000 ) ) ;
#40968 = CARTESIAN_POINT ( 'NONE',  ( 11.25210807141120029, -3.959980833595939664, 6.634727177901499573 ) ) ;
#40969 = B_SPLINE_CURVE_WITH_KNOTS ( 'NONE', 3,
 ( #31529, #53542, #63670, #32229 ),
 .UNSPECIFIED., .F., .F.,
 ( 4, 4 ),
 ( 0.000000000000000000, 1.000000000000000000 ),
 .UNSPECIFIED. ) ;
#40970 = CARTESIAN_POINT ( 'NONE',  ( 10.25313817995475674, -2.714785337465082549, 7.027193780659055200 ) ) ;
#40971 = CARTESIAN_POINT ( 'NONE',  ( -0.04643246160058000366, -1.644388561977000007, -3.014063655381999940 ) ) ;
#40972 = CARTESIAN_POINT ( 'NONE',  ( 11.08810207955139937, 3.203462856645999945, -7.174999999999999822 ) ) ;
#40973 = CARTESIAN_POINT ( 'NONE',  ( 10.40769129028899975, -4.889436474118636689, -8.413289387078531689 ) ) ;
#40974 = FACE_OUTER_BOUND ( 'NONE', #26458, .T. ) ;
#40975 = CARTESIAN_POINT ( 'NONE',  ( 10.94487616594229884, 3.696562859151900415, -6.543508100188799581 ) ) ;
#40976 = CYLINDRICAL_SURFACE ( 'NONE', #43685, 12.52500000000000036 ) ;
#40977 = CARTESIAN_POINT ( 'NONE',  ( 10.41838915877000105, 4.531912033713999755, -9.270484952459998595 ) ) ;
#40978 = ADVANCED_FACE ( 'NONE', ( #56454 ), #44032, .F. ) ;
#40979 = CARTESIAN_POINT ( 'NONE',  ( 8.746126402770999064, 5.068373778467000434, -7.097120470443400109 ) ) ;
#40981 = CARTESIAN_POINT ( 'NONE',  ( 9.270072224255999416, -3.906223101245800411, 6.613913699222099041 ) ) ;
#40980 = CARTESIAN_POINT ( 'NONE',  ( 15.59211270977100128, -8.811013545169000594, -7.841491685545999069 ) ) ;
#40982 = CARTESIAN_POINT ( 'NONE',  ( 23.59461952754617897, -13.38743028302391203, 4.020894998903971285 ) ) ;
#40983 = ORIENTED_EDGE ( 'NONE', *, *, #58167, .F. ) ;
#40984 = AXIS2_PLACEMENT_3D ( 'NONE', #62791, #14912, #27737 ) ;
#40985 = CARTESIAN_POINT ( 'NONE',  ( 11.27745123989519982, 4.410212499603100689, 6.707778874960499849 ) ) ;
#40986 = PLANE ( 'NONE',  #48592 ) ;
#40987 = CARTESIAN_POINT ( 'NONE',  ( 10.21225461470299933, 3.026595211686900377, 7.252360304610999897 ) ) ;
#40988 = CARTESIAN_POINT ( 'NONE',  ( 9.024266954400625096, 3.674418004489155010, -6.687886317613946474 ) ) ;
#40989 = CARTESIAN_POINT ( 'NONE',  ( 17.55505043854144276, 0.6250000000000001110, 12.67928921589117586 ) ) ;
#40990 = DIRECTION ( 'NONE',  ( 0.000000000000000000, 0.000000000000000000, -1.000000000000000000 ) ) ;
#40991 = CARTESIAN_POINT ( 'NONE',  ( 8.186600515489956820, 2.905260986775225707, 6.578663288309482660 ) ) ;
#40992 = ORIENTED_EDGE ( 'NONE', *, *, #18028, .F. ) ;
#40993 = B_SPLINE_CURVE_WITH_KNOTS ( 'NONE', 3,
 ( #32563, #10885, #26974, #21373, #53195, #1434, #53876, #16469, #42707, #17157, #43401, #395, #49319, #5295, #54219, #64012 ),
 .UNSPECIFIED., .F., .F.,
 ( 4, 2, 2, 2, 2, 2, 2, 4 ),
 ( 0.000000000000000000, 0.06249999999999916733, 0.1249999999999983347, 0.2499999999999967248, 0.4999999999999966693, 0.7499999999999966693, 0.8749999999999983347, 1.000000000000000000 ),
 .UNSPECIFIED. ) ;
#40994 = CARTESIAN_POINT ( 'NONE',  ( 9.632646554151000018, -3.447209681134600245, -8.499078230848398974 ) ) ;
#40995 = VECTOR ( 'NONE', #44963, 1000.000000000000000 ) ;
#40996 = DIRECTION ( 'NONE',  ( 1.000000000000000000, 0.000000000000000000, 0.000000000000000000 ) ) ;
#40997 = CARTESIAN_POINT ( 'NONE',  ( 11.39835090130999973, -3.121033016283800254, 6.956352367771000189 ) ) ;
#40998 = CARTESIAN_POINT ( 'NONE',  ( 17.68706105916309568, 1.772767334361405656, -12.47466639265151755 ) ) ;
#40999 = FACE_OUTER_BOUND ( 'NONE', #14524, .T. ) ;
#41000 = CARTESIAN_POINT ( 'NONE',  ( 11.09999999999999964, 10.03015638309000046, -5.726993439934999763 ) ) ;
#41001 = B_SPLINE_CURVE_WITH_KNOTS ( 'NONE', 3,
 ( #29551, #2946, #24963, #46981 ),
 .UNSPECIFIED., .F., .F.,
 ( 4, 4 ),
 ( 0.000000000000000000, 0.1254469995254103021 ),
 .UNSPECIFIED. ) ;
#41003 = CIRCLE ( 'NONE', #62267, 3.200000000000000178 ) ;
#41002 = CARTESIAN_POINT ( 'NONE',  ( 12.25852091194881588, 2.803392358698900910, -13.60441894876048252 ) ) ;
#41004 = LINE ( 'NONE', #4970, #52431 ) ;
#41005 = CARTESIAN_POINT ( 'NONE',  ( 25.59037530393599980, 11.08965754835999995, 3.240319064921999725 ) ) ;
#41006 = ADVANCED_FACE ( 'NONE', ( #17859 ), #33246, .F. ) ;
#41007 = DIRECTION ( 'NONE',  ( 1.000000000000000000, -1.659086735363680163E-15, 1.195176146505341979E-14 ) ) ;
#41008 = DIRECTION ( 'NONE',  ( 0.000000000000000000, -1.000000000000000000, 0.000000000000000000 ) ) ;
#41009 = CARTESIAN_POINT ( 'NONE',  ( 23.57056559309938493, 13.35854817469667744, 4.154943855177697820 ) ) ;
#41010 = CARTESIAN_POINT ( 'NONE',  ( 10.31021345716899873, -3.363461959113699606, -8.078719053813800954 ) ) ;
#41011 = CARTESIAN_POINT ( 'NONE',  ( 2.396856900172125382, 0.9112004763889646197, -3.396138185504796070 ) ) ;
#41012 = CARTESIAN_POINT ( 'NONE',  ( 9.369139158774000720, 2.685250982074999904, -7.026194612421999608 ) ) ;
#41013 = CARTESIAN_POINT ( 'NONE',  ( 8.721802827889733933, 2.874603711573444187, 6.749639981083119800 ) ) ;
#41014 = ORIENTED_EDGE ( 'NONE', *, *, #65166, .T. ) ;
#41015 = CARTESIAN_POINT ( 'NONE',  ( 4.000000000000000000, -1.719428477288966750, 1.321180510578594536 ) ) ;
#41016 = CARTESIAN_POINT ( 'NONE',  ( 18.17294214856815060, 2.135913245783947811, -13.83611159055834960 ) ) ;
#41017 = VERTEX_POINT ( 'NONE', #44088 ) ;
#41018 = CARTESIAN_POINT ( 'NONE',  ( 9.832721904869998752, -3.243980311826100138, 7.075568408810499754 ) ) ;
#41019 = CARTESIAN_POINT ( 'NONE',  ( 24.98032478375984766, 2.955846862813865439, 11.57695784767182623 ) ) ;
#41020 = FACE_OUTER_BOUND ( 'NONE', #6196, .T. ) ;
#41021 = CARTESIAN_POINT ( 'NONE',  ( 10.15596191468078224, 2.820845708124703144, -6.216775022417006191 ) ) ;
#41022 = CARTESIAN_POINT ( 'NONE',  ( 11.14256920625030034, -3.957769094421040190, -6.325872106312999676 ) ) ;
#41023 = CARTESIAN_POINT ( 'NONE',  ( 11.60000000000000142, -3.186139913033902538, -6.684405152318921850 ) ) ;
#41024 = CARTESIAN_POINT ( 'NONE',  ( 11.08810207955139937, -4.796537143354000499, -7.174999999999999822 ) ) ;
#41025 = ORIENTED_EDGE ( 'NONE', *, *, #57509, .T. ) ;
#41026 = CARTESIAN_POINT ( 'NONE',  ( 25.30000327618300204, 0.6965695964343684432, -11.50000000000000000 ) ) ;
#41027 = CARTESIAN_POINT ( 'NONE',  ( 24.39664325360668684, -12.03536696638400016, 3.224866859253743279 ) ) ;
#41028 = CARTESIAN_POINT ( 'NONE',  ( 9.585279719593998493, 2.928319778732999978, -8.861178115809998701 ) ) ;
#41029 = ORIENTED_EDGE ( 'NONE', *, *, #60447, .F. ) ;
#41030 = AXIS2_PLACEMENT_3D ( 'NONE', #25257, #35078, #24228 ) ;
#41031 = CARTESIAN_POINT ( 'NONE',  ( 10.04002816746000093, 2.348904337896000172, -7.136750921008999882 ) ) ;
#41032 = ORIENTED_EDGE ( 'NONE', *, *, #44643, .T. ) ;
#41033 = CARTESIAN_POINT ( 'NONE',  ( 10.08655864497999843, 5.007105485494000696, 6.711254117843599154 ) ) ;
#41034 = CARTESIAN_POINT ( 'NONE',  ( 18.15708441975580811, -2.331821618626341852, -12.48915497634519411 ) ) ;
#41035 = COLOUR_RGB ( '', 0.72549020, 0.75294118, 0.79215686) ;
#41036 = DIRECTION ( 'NONE',  ( 1.000000000000000000, 0.000000000000000000, -9.843114642662001530E-13 ) ) ;
#41037 = VECTOR ( 'NONE', #62645, 1000.000000000000000 ) ;
#41038 = CARTESIAN_POINT ( 'NONE',  ( 8.433148997460000018, 5.167567567567999731, 6.822293592207000934 ) ) ;
#41039 = EDGE_CURVE ( 'NONE', #60315, #68087, #3595, .T. ) ;
#41040 = CARTESIAN_POINT ( 'NONE',  ( 9.856463691914767011, 5.100000000000000533, 6.665341197415451724 ) ) ;
#41041 = ADVANCED_FACE ( 'NONE', ( #54210 ), #21704, .F. ) ;
#41042 = EDGE_LOOP ( 'NONE', ( #22973, #39857, #58639, #20566 ) ) ;
#41043 = CARTESIAN_POINT ( 'NONE',  ( 8.972537864292000620, 2.899999999999999911, -6.571291218949999902 ) ) ;
#41044 = CARTESIAN_POINT ( 'NONE',  ( 24.67921430886200085, -8.727631620858000261, -9.158313288899000426 ) ) ;
#41045 = CARTESIAN_POINT ( 'NONE',  ( 8.070721554491710137, -3.646115526505184778, 8.813957122113405873 ) ) ;
#41046 = VECTOR ( 'NONE', #57162, 1000.000000000000000 ) ;
#41047 = CARTESIAN_POINT ( 'NONE',  ( 12.12912605232851604, 2.253778109953301634, -13.81740241363613642 ) ) ;
#41048 = CARTESIAN_POINT ( 'NONE',  ( 9.160535748954998780, 2.900115872948000106, -6.152093930328999427 ) ) ;
#41049 = CARTESIAN_POINT ( 'NONE',  ( 17.65706414889024956, 11.53038916134920555, -4.891395587226483599 ) ) ;
#41050 = CARTESIAN_POINT ( 'NONE',  ( 7.831595309934897386, 4.878214714082836245, 6.417939907564524482 ) ) ;
#41051 = ORIENTED_EDGE ( 'NONE', *, *, #52440, .F. ) ;
#41052 = ORIENTED_EDGE ( 'NONE', *, *, #2832, .T. ) ;
#41053 = AXIS2_PLACEMENT_3D ( 'NONE', #13192, #22621, #44320 ) ;
#41054 = CARTESIAN_POINT ( 'NONE',  ( 9.915635841230999503, 3.210851187372000037, -6.346613542714999667 ) ) ;
#41055 = DIRECTION ( 'NONE',  ( 0.000000000000000000, -0.2461538461537955136, -0.9692307692307821076 ) ) ;
#41056 = DIRECTION ( 'NONE',  ( 1.000000000000000000, 0.000000000000000000, 0.000000000000000000 ) ) ;
#41057 = CARTESIAN_POINT ( 'NONE',  ( 25.08883434079300301, 8.444432640379998745, -8.588577351766998547 ) ) ;
#41058 = CARTESIAN_POINT ( 'NONE',  ( 7.860744422257667452, 4.181951828900120738, 6.138447713083068358 ) ) ;
#41059 = EDGE_CURVE ( 'NONE', #46265, #29696, #10876, .T. ) ;
#41060 = CARTESIAN_POINT ( 'NONE',  ( 17.79421883851900077, -3.253172350820999981, -11.33701189166999868 ) ) ;
#41062 = CYLINDRICAL_SURFACE ( 'NONE', #34011, 1.350000000000000533 ) ;
#41061 = CARTESIAN_POINT ( 'NONE',  ( 10.56229229006299875, -3.012566816337000297, 8.073332500201798823 ) ) ;
#41063 = CARTESIAN_POINT ( 'NONE',  ( 7.800894426331000275, 3.218815461055000160, 6.398977422524000147 ) ) ;
#41064 = ORIENTED_EDGE ( 'NONE', *, *, #31530, .F. ) ;
#41065 = EDGE_CURVE ( 'NONE', #24944, #19063, #32221, .T. ) ;
#41066 = CARTESIAN_POINT ( 'NONE',  ( 25.26999579225652681, -11.52969365347296460, 2.996586438050647949 ) ) ;
#41067 = CARTESIAN_POINT ( 'NONE',  ( 10.48237399227000033, -2.917144342353999775, -4.649494773176000351 ) ) ;
#41068 = CARTESIAN_POINT ( 'NONE',  ( 9.446306596383999832, -5.231133027468000130, -6.569831606205999819 ) ) ;
#41069 = CARTESIAN_POINT ( 'NONE',  ( 10.90000000000000036, 0.2999999999999999889, -4.902439024389999567 ) ) ;
#41070 = CARTESIAN_POINT ( 'NONE',  ( 18.17221331276092755, -2.599179209475691366, -12.42790858714744218 ) ) ;
#41071 = CYLINDRICAL_SURFACE ( 'NONE', #34175, 1.250000000000000222 ) ;
#41072 = CARTESIAN_POINT ( 'NONE',  ( 8.447510841229000533, 4.933589693325000525, -9.154576215408999573 ) ) ;
#41073 = AXIS2_PLACEMENT_3D ( 'NONE', #39835, #23406, #40854 ) ;
#41074 = CARTESIAN_POINT ( 'NONE',  ( 13.99974593105000231, 8.811008772734998828, 7.563940656188999689 ) ) ;
#41075 = B_SPLINE_CURVE_WITH_KNOTS ( 'NONE', 3,
 ( #29771, #2152, #56322, #61224, #3179, #23812, #18229, #39904, #40243, #50042 ),
 .UNSPECIFIED., .F., .F.,
 ( 4, 2, 2, 2, 4 ),
 ( 0.2180895000437835241, 0.4135671250328376569, 0.6090447500218918453, 0.8045223750109458116, 1.000000000000000000 ),
 .UNSPECIFIED. ) ;
#41076 = LINE ( 'NONE', #30934, #32226 ) ;
#41077 = CARTESIAN_POINT ( 'NONE',  ( 10.90000000000000036, -2.778483479159999714, -6.925197956411000000 ) ) ;
#41078 = CIRCLE ( 'NONE', #10936, 13.92493900950999830 ) ;
#41079 = CARTESIAN_POINT ( 'NONE',  ( 0.1625046544502119494, 1.591888665051217622, -2.763666953839243323 ) ) ;
#41080 = DIRECTION ( 'NONE',  ( -1.000000000000000000, 0.000000000000000000, 0.000000000000000000 ) ) ;
#41081 = EDGE_LOOP ( 'NONE', ( #52816, #20842, #20625, #50318 ) ) ;
#41082 = CARTESIAN_POINT ( 'NONE',  ( 12.52850951125299872, -0.5605836838512548992, -12.68334204399185694 ) ) ;
#41084 = CARTESIAN_POINT ( 'NONE',  ( 12.26155906743356461, -2.190709282250366652, -12.51827377312864975 ) ) ;
#41083 = B_SPLINE_CURVE_WITH_KNOTS ( 'NONE', 3,
 ( #56067, #28832, #8177, #17984 ),
 .UNSPECIFIED., .F., .F.,
 ( 4, 4 ),
 ( 0.000000000000000000, 1.000000000000000000 ),
 .UNSPECIFIED. ) ;
#41085 = CARTESIAN_POINT ( 'NONE',  ( 8.703529634540137394, 5.100000000000000533, -6.308756105309840656 ) ) ;
#41087 = FACE_OUTER_BOUND ( 'NONE', #38064, .T. ) ;
#41086 = AXIS2_PLACEMENT_3D ( 'NONE', #13038, #3226, #34368 ) ;
#41088 = ORIENTED_EDGE ( 'NONE', *, *, #1827, .T. ) ;
#41089 = CARTESIAN_POINT ( 'NONE',  ( 9.099999952505998024, -4.000000000000000000, 7.500000000000000000 ) ) ;
#41090 = APPLICATION_PROTOCOL_DEFINITION ( 'draft international standard', 'automotive_design', 1998, #45855 ) ;
#41091 = CARTESIAN_POINT ( 'NONE',  ( 0.5107036710124341905, 3.504666613735739400, 0.4180694620915118564 ) ) ;
#41092 = CARTESIAN_POINT ( 'NONE',  ( 12.99518154839200257, -11.72294562696999876, -1.966205464704999795 ) ) ;
#41093 = CARTESIAN_POINT ( 'NONE',  ( 10.22272469555899832, 4.639546521693399761, 8.606479382885998675 ) ) ;
#41094 = AXIS2_PLACEMENT_3D ( 'NONE', #46420, #61127, #34569 ) ;
#41095 = CARTESIAN_POINT ( 'NONE',  ( 10.97635090131019986, 4.999207052587699707, -8.118017011233499503 ) ) ;
#41096 = ORIENTED_EDGE ( 'NONE', *, *, #14797, .F. ) ;
#41097 = CARTESIAN_POINT ( 'NONE',  ( 11.12914445903999905, -3.083861519183999977, 8.586004431109000024 ) ) ;
#41099 = ORIENTED_EDGE ( 'NONE', *, *, #35907, .T. ) ;
#41098 = B_SPLINE_CURVE_WITH_KNOTS ( 'NONE', 3,
 ( #33, #38471, #11207, #11542, #43026, #58755, #16449, #54196, #16790, #6649, #59791, #48621 ),
 .UNSPECIFIED., .F., .F.,
 ( 4, 2, 2, 2, 2, 4 ),
 ( 0.000000000000000000, 0.2500000000000179856, 0.3750000000000235922, 0.4375000000000248135, 0.5000000000000259792, 1.000000000000000000 ),
 .UNSPECIFIED. ) ;
#41100 = CARTESIAN_POINT ( 'NONE',  ( 7.591111298125107432, -3.321015683491707282, 8.680015853441066298 ) ) ;
#41101 = CARTESIAN_POINT ( 'NONE',  ( 8.111566940377999302, -3.326257819185999942, 8.794522506294001118 ) ) ;
#41102 = CARTESIAN_POINT ( 'NONE',  ( 15.86001156276200064, 8.572187346067000391, 8.239473968622000655 ) ) ;
#41103 = EDGE_CURVE ( 'NONE', #25385, #32603, #48445, .T. ) ;
#41104 = EDGE_CURVE ( 'NONE', #57460, #27251, #5961, .T. ) ;
#41105 = VERTEX_POINT ( 'NONE', #43393 ) ;
#41106 = CARTESIAN_POINT ( 'NONE',  ( -0.000000000000000000, 0.7585797238574916168, -2.824612379753442148 ) ) ;
#41107 = CARTESIAN_POINT ( 'NONE',  ( 0.000000000000000000, 0.000000000000000000, 0.000000000000000000 ) ) ;
#41108 = CARTESIAN_POINT ( 'NONE',  ( 7.970595280405999183, 2.627120679234999923, -8.556648795244999661 ) ) ;
#41109 = CARTESIAN_POINT ( 'NONE',  ( 16.39999999379500295, -3.351248059343999941, -11.15756683833000018 ) ) ;
#41110 = CARTESIAN_POINT ( 'NONE',  ( 17.69835410963201028, -3.108690103393802584, 12.28870081726095087 ) ) ;
#41111 = EDGE_LOOP ( 'NONE', ( #54661, #11781, #34898, #61024 ) ) ;
#41112 = CARTESIAN_POINT ( 'NONE',  ( 11.25041341105000114, -5.730771985297000271, 8.122672103119001008 ) ) ;
#41113 = CARTESIAN_POINT ( 'NONE',  ( 12.18428608238523125, -2.573446268070838983, -13.65756128988527962 ) ) ;
#41114 = CARTESIAN_POINT ( 'NONE',  ( 5.469609839683874597, 0.1963495408493571015, 1.500000000000000444 ) ) ;
#41115 = ORIENTED_EDGE ( 'NONE', *, *, #65162, .T. ) ;
#41116 = CARTESIAN_POINT ( 'NONE',  ( 9.143998948451265818, 2.899999999999999911, 6.465127702479446015 ) ) ;
#41117 = B_SPLINE_CURVE_WITH_KNOTS ( 'NONE', 3,
 ( #68304, #47691, #31609, #58511 ),
 .UNSPECIFIED., .F., .F.,
 ( 4, 4 ),
 ( 0.000000000000000000, 1.000000000000000000 ),
 .UNSPECIFIED. ) ;
#41118 = CARTESIAN_POINT ( 'NONE',  ( 10.76685100253999927, 2.832432432432000269, 6.822293592207000934 ) ) ;
#41119 = VERTEX_POINT ( 'NONE', #27308 ) ;
#41120 = PRODUCT_DEFINITION_SHAPE ( 'NONE', 'NONE',  #39365 ) ;
#41121 = CARTESIAN_POINT ( 'NONE',  ( 10.66153368166920679, 5.571142525177961602, 6.679759109773798720 ) ) ;
#41122 = CARTESIAN_POINT ( 'NONE',  ( 5.282109839684041575, 0.9218200799623742503, -1.199500263597268912 ) ) ;
#41123 = CYLINDRICAL_SURFACE ( 'NONE', #42004, 0.6250000000000005551 ) ;
#41124 = CARTESIAN_POINT ( 'NONE',  ( 8.356851002541000994, 2.832432432432000269, -6.822293592207000934 ) ) ;
#41125 = CARTESIAN_POINT ( 'NONE',  ( 12.34868974583248402, 0.4275223103465176644, -13.89116040406442032 ) ) ;
#41126 = CARTESIAN_POINT ( 'NONE',  ( 18.02645743154362634, -2.910866584900386744, 12.34632125423082449 ) ) ;
#41127 = EDGE_LOOP ( 'NONE', ( #42293, #1031, #58489, #22711 ) ) ;
#41128 = ADVANCED_FACE ( 'NONE', ( #33591 ), #59491, .F. ) ;
#41129 = CARTESIAN_POINT ( 'NONE',  ( 8.493356027204001180, -5.097500218784999149, 6.607661537772998805 ) ) ;
#41131 = EDGE_CURVE ( 'NONE', #45933, #5439, #23089, .T. ) ;
#41130 = B_SPLINE_CURVE_WITH_KNOTS ( 'NONE', 3,
 ( #50922, #3021, #66989, #61748, #13867, #35197, #39057, #60379, #12484, #55133, #7237, #8954, #14892, #63106, #35539, #31319, #57529, #36213, #9287, #57188, #3697, #15233, #67667, #20819, #42157, #67328, #25034, #46366, #63458, #4386, #36558, #19793 ),
 .UNSPECIFIED., .F., .F.,
 ( 4, 2, 2, 2, 2, 2, 2, 2, 1, 2, 2, 2, 1, 1, 1, 2, 2, 4 ),
 ( 0.000000000000000000, 0.2499999999999977796, 0.3749999999999976130, 0.4374999999999985567, 0.4687499999999993339, 0.5000000000000001110, 0.6249999999999926725, 0.6874999999999898970, 0.7187499999999898970, 0.7343749999999898970, 0.7499999999999900080, 0.8124999999999856781, 0.8437499999999835687, 0.8593749999999823475, 0.8671874999999817923, 0.8710937499999804601, 0.8749999999999792388, 1.000000000000000000 ),
 .UNSPECIFIED. ) ;
#41132 = VERTEX_POINT ( 'NONE', #37792 ) ;
#41133 = CARTESIAN_POINT ( 'NONE',  ( 9.569805421428000614, 4.064052243276000453, 8.919241792616000808 ) ) ;
#41134 = CARTESIAN_POINT ( 'NONE',  ( 11.03852705926000155, -5.246732451374000128, 5.026582089102999085 ) ) ;
#41135 = CARTESIAN_POINT ( 'NONE',  ( 8.491329719591000469, 4.851303550474000303, -9.008742670124000540 ) ) ;
#41136 = EDGE_CURVE ( 'NONE', #4104, #6955, #26787, .T. ) ;
#41137 = CARTESIAN_POINT ( 'NONE',  ( 3.103509480039000401, 2.020192966679000168, 3.109413244175000202 ) ) ;
#41138 = B_SPLINE_CURVE_WITH_KNOTS ( 'NONE', 3,
 ( #66671, #60743, #65978, #2024, #67013, #65636, #55504, #7606, #23342, #34189, #28955, #50258, #2704, #45020, #29643, #66325, #19122, #13212 ),
 .UNSPECIFIED., .F., .F.,
 ( 4, 2, 2, 2, 2, 2, 2, 2, 4 ),
 ( 0.1070776897655759813, 0.2026877965917215363, 0.2982979034178671052, 0.3939080102440126185, 0.4895181170701581874, 0.5851282238963034787, 0.6807383307224488256, 0.7763484375485940614, 0.8719585443747394082 ),
 .UNSPECIFIED. ) ;
#41139 = CARTESIAN_POINT ( 'NONE',  ( 11.15192313136999935, -2.359310578948000003, -6.636692315558000210 ) ) ;
#41140 = CARTESIAN_POINT ( 'NONE',  ( 25.30000327618300204, 9.659335867304687184, -6.394377797198702140 ) ) ;
#41141 = CARTESIAN_POINT ( 'NONE',  ( 23.55356904242700367, 13.38988504594999895, 4.198910762617999559 ) ) ;
#41142 = B_SPLINE_CURVE_WITH_KNOTS ( 'NONE', 3,
 ( #39151, #1397, #60474, #38104 ),
 .UNSPECIFIED., .F., .F.,
 ( 4, 4 ),
 ( 0.000000000000000000, 0.1494581667962512628 ),
 .UNSPECIFIED. ) ;
#41143 = VERTEX_POINT ( 'NONE', #22047 ) ;
#41144 = CARTESIAN_POINT ( 'NONE',  ( 11.24379975933729980, -2.921317947059999920, 7.871126858273000515 ) ) ;
#41145 = CARTESIAN_POINT ( 'NONE',  ( 10.54648703831772316, 2.506660384375831718, -8.410204393717869209 ) ) ;
#41146 = CARTESIAN_POINT ( 'NONE',  ( 12.80505043854144276, -0.6250000000000001110, -13.88107975066922428 ) ) ;
#41147 = FACE_OUTER_BOUND ( 'NONE', #60755, .T. ) ;
#41149 = CARTESIAN_POINT ( 'NONE',  ( 5.000000000000000000, -1.199999999999999956, -11.02663029882999801 ) ) ;
#41148 = CARTESIAN_POINT ( 'NONE',  ( 10.12550053024000007, 5.788811067708000024, 7.335561454339999621 ) ) ;
#41150 = VECTOR ( 'NONE', #15213, 1000.000000000000000 ) ;
#41151 = CARTESIAN_POINT ( 'NONE',  ( 10.52641638348499953, 3.025038519517300184, -7.262511127784999410 ) ) ;
#41152 = ADVANCED_FACE ( 'NONE', ( #59456 ), #64693, .F. ) ;
#41153 = CARTESIAN_POINT ( 'NONE',  ( 25.47132200302800342, -11.11905954937000018, 3.299905938470999889 ) ) ;
#41155 = AXIS2_PLACEMENT_3D ( 'NONE', #53323, #59592, #5423 ) ;
#41154 = CARTESIAN_POINT ( 'NONE',  ( 9.933633995697999097, 4.998281561686200192, -7.610798122400000310 ) ) ;
#41156 = B_SPLINE_CURVE_WITH_KNOTS ( 'NONE', 3,
 ( #47774, #58593, #69083, #32040 ),
 .UNSPECIFIED., .F., .F.,
 ( 4, 4 ),
 ( 0.000000000000000000, 1.000000000000000000 ),
 .UNSPECIFIED. ) ;
#41157 = CARTESIAN_POINT ( 'NONE',  ( 18.27977754798707721, 0.02297882141078181478, 12.59998453421652620 ) ) ;
#41158 = CARTESIAN_POINT ( 'NONE',  ( 24.46275371508600216, 3.515554276222999874, 12.28676815851000015 ) ) ;
#41159 = CARTESIAN_POINT ( 'NONE',  ( 11.72433327354039889, 3.016779570871600313, 8.143111181492699302 ) ) ;
#41160 = CARTESIAN_POINT ( 'NONE',  ( 23.62945547067200280, 10.04812290079000014, 9.751475363001999241 ) ) ;
#41161 = ORIENTED_EDGE ( 'NONE', *, *, #63508, .T. ) ;
#41162 = CARTESIAN_POINT ( 'NONE',  ( 7.999933059623999476, -5.198566224659999513, 8.332559954171999905 ) ) ;
#41163 = DIRECTION ( 'NONE',  ( 0.000000000000000000, 1.000000000000000000, 0.000000000000000000 ) ) ;
#41164 = CARTESIAN_POINT ( 'NONE',  ( 4.599999999999999645, 0.000000000000000000, 0.000000000000000000 ) ) ;
#41165 = ORIENTED_EDGE ( 'NONE', *, *, #21319, .F. ) ;
#41166 = CIRCLE ( 'NONE', #59026, 10.75000000000000533 ) ;
#41167 = CARTESIAN_POINT ( 'NONE',  ( 14.80000000000000071, 3.470217030164000072, -11.92928724693999953 ) ) ;
#41168 = CARTESIAN_POINT ( 'NONE',  ( 10.85168717260509830, 3.386210853237200169, 6.498190316041999814 ) ) ;
#41169 = CARTESIAN_POINT ( 'NONE',  ( 10.78888278041000071, 2.675726696512000125, -6.748227692827999391 ) ) ;
#41170 = ORIENTED_EDGE ( 'NONE', *, *, #34831, .F. ) ;
#41171 = LINE ( 'NONE', #29668, #23882 ) ;
#41172 = CARTESIAN_POINT ( 'NONE',  ( 18.00351343198559917, -3.053300080839206121, 12.22464702761727651 ) ) ;
#41173 = CARTESIAN_POINT ( 'NONE',  ( 10.66579975933730040, 5.208485784810999775, 7.915786590091300035 ) ) ;
#41174 = DIRECTION ( 'NONE',  ( -2.859035942644044579E-07, 0.9999999999998158140, 5.353374572246079530E-07 ) ) ;
#41175 = CARTESIAN_POINT ( 'NONE',  ( 15.40000000005200143, 9.187454762873001002, 8.213177997099000649 ) ) ;
#41176 = ORIENTED_EDGE ( 'NONE', *, *, #16251, .T. ) ;
#41177 = CARTESIAN_POINT ( 'NONE',  ( 7.834258984672959336, -4.908978639643027719, 6.449989159278149309 ) ) ;
#41178 = CARTESIAN_POINT ( 'NONE',  ( 7.100000000000000533, -4.000000000000000000, 7.500000000000000000 ) ) ;
#41179 = CARTESIAN_POINT ( 'NONE',  ( 8.269748398527868360, -5.103706565029416886, 8.846130348739302818 ) ) ;
#41180 = CARTESIAN_POINT ( 'NONE',  ( 9.474088727410999056, -5.137817193984000497, 7.404572115919599185 ) ) ;
#41181 = ORIENTED_EDGE ( 'NONE', *, *, #28726, .T. ) ;
#41182 = CARTESIAN_POINT ( 'NONE',  ( 10.48792048572999924, -5.025034920168000241, -4.782290442434000255 ) ) ;
#41183 = CARTESIAN_POINT ( 'NONE',  ( 7.000002934099999408, 1.243449787579999883E-13, -1.714942011622999690E-13 ) ) ;
#41184 = EDGE_LOOP ( 'NONE', ( #69099, #6127, #52332, #44660 ) ) ;
#41185 = CARTESIAN_POINT ( 'NONE',  ( 10.06059687351566723, -3.370476274536376771, 6.407767014557177454 ) ) ;
#41186 = ORIENTED_EDGE ( 'NONE', *, *, #29375, .F. ) ;
#41187 = EDGE_CURVE ( 'NONE', #2494, #7968, #22658, .T. ) ;
#41188 = EDGE_CURVE ( 'NONE', #16959, #12534, #10921, .T. ) ;
#41189 = CARTESIAN_POINT ( 'NONE',  ( 10.06491331857999860, -5.318469253323000245, -7.099528416287999910 ) ) ;
#41190 = CARTESIAN_POINT ( 'NONE',  ( 2.498890132543458709, 2.798833948393634419, -2.150913519912196925 ) ) ;
#41191 = PRESENTATION_LAYER_ASSIGNMENT (  '', '', ( #61256 ) ) ;
#41192 = CARTESIAN_POINT ( 'NONE',  ( 10.93479632507519916, 4.557787252275099732, -8.534037301706000278 ) ) ;
#41193 = CARTESIAN_POINT ( 'NONE',  ( 12.05811496860034993, -2.954409148022000053, 8.035816473382100256 ) ) ;
#41194 = CARTESIAN_POINT ( 'NONE',  ( 12.46375379917804338, 1.976313547018315075, -12.55830662486076577 ) ) ;
#41195 = CARTESIAN_POINT ( 'NONE',  ( 12.10118044953561878, -2.866798846279000390, 6.909094663619399945 ) ) ;
#41196 = CARTESIAN_POINT ( 'NONE',  ( 7.694010841228000608, 5.850290547079999293, 6.784176679236000318 ) ) ;
#41197 = ORIENTED_EDGE ( 'NONE', *, *, #66997, .T. ) ;
#41198 = CARTESIAN_POINT ( 'NONE',  ( 9.510596873516666605, 4.629523725463622341, -8.592232985442825210 ) ) ;
#41199 = CARTESIAN_POINT ( 'NONE',  ( 7.390495559621999888, -2.216884807317999861, 8.370075800106999253 ) ) ;
#41200 = CARTESIAN_POINT ( 'NONE',  ( 15.90018573812399971, -8.493548356068000516, -8.263529029821000904 ) ) ;
#41201 = ORIENTED_EDGE ( 'NONE', *, *, #53455, .F. ) ;
#41202 = CARTESIAN_POINT ( 'NONE',  ( 12.29593341745177781, -2.863102696958912841, -12.35953065740858570 ) ) ;
#41203 = CARTESIAN_POINT ( 'NONE',  ( 11.55194988689359903, 4.580487242693600081, 6.361426117087999543 ) ) ;
#41204 = CARTESIAN_POINT ( 'NONE',  ( 10.25880564679000173, -2.491773655925000330, -7.289938045981000592 ) ) ;
#41205 = CARTESIAN_POINT ( 'NONE',  ( 11.27712163255998412, 9.461969908151001363, -6.800304254993005948 ) ) ;
#41206 = CARTESIAN_POINT ( 'NONE',  ( 17.93733281514800026, -12.03472983398000018, 3.255807327981000032 ) ) ;
#41207 = DIRECTION ( 'NONE',  ( -1.000000000000000000, 0.000000000000000000, 0.000000000000000000 ) ) ;
#41208 = CARTESIAN_POINT ( 'NONE',  ( 12.44718984625871805, -1.987489649616605902, -13.76884489496295139 ) ) ;
#41209 = CARTESIAN_POINT ( 'NONE',  ( 10.77672335273219950, -3.698477709264200275, -8.312023951944400579 ) ) ;
#41210 = CARTESIAN_POINT ( 'NONE',  ( 11.18272066707849888, -2.906477115133000222, -6.838543969064300398 ) ) ;
#41211 = CARTESIAN_POINT ( 'NONE',  ( 17.65081963855161362, -3.193844305817328255, 12.18849311783432654 ) ) ;
#41212 = ORIENTED_EDGE ( 'NONE', *, *, #28727, .T. ) ;
#41213 = VERTEX_POINT ( 'NONE', #29394 ) ;
#41214 = CARTESIAN_POINT ( 'NONE',  ( 12.08019303639704489, 0.1916560648979804826, -13.99999316327169296 ) ) ;
#41215 = CARTESIAN_POINT ( 'NONE',  ( 18.18005043854147118, -2.500000000000000000, -25.00000000000000000 ) ) ;
#41216 = CARTESIAN_POINT ( 'NONE',  ( 18.17052368433065368, 2.609308838564532884, 13.64962199042474289 ) ) ;
#41217 = ADVANCED_FACE ( 'NONE', ( #61533 ), #12607, .T. ) ;
#41218 = CARTESIAN_POINT ( 'NONE',  ( 9.988718791410999387, 2.842026940133999702, -6.504333051298999635 ) ) ;
#41219 = FACE_OUTER_BOUND ( 'NONE', #46304, .T. ) ;
#41220 = CARTESIAN_POINT ( 'NONE',  ( 17.80592519432564913, 3.072462716380374381, 12.29957259991316576 ) ) ;
#41221 = CARTESIAN_POINT ( 'NONE',  ( 5.599999772733899484, -9.503509090790997936E-14, 3.419486915844999993E-14 ) ) ;
#41222 = CARTESIAN_POINT ( 'NONE',  ( 9.124700695083998170, 4.778663323155000420, 8.799742559280000265 ) ) ;
#41223 = CARTESIAN_POINT ( 'NONE',  ( 11.46253286130405691, -3.661005694687299528, -6.691343801417681370 ) ) ;
#41224 = ORIENTED_EDGE ( 'NONE', *, *, #37832, .T. ) ;
#41225 = CARTESIAN_POINT ( 'NONE',  ( 12.46386834215128303, -3.023758766561085665, 12.31399102038137272 ) ) ;
#41226 = CARTESIAN_POINT ( 'NONE',  ( 8.817138961223998095, -3.281636118526699786, -7.985449642667900250 ) ) ;
#41227 = CARTESIAN_POINT ( 'NONE',  ( 9.834151567923001380, 5.173929249342999803, 8.813048229486998508 ) ) ;
#41228 = CARTESIAN_POINT ( 'NONE',  ( 12.14122412107036908, -3.937930136014310190, 8.673243607771999208 ) ) ;
#41229 = CARTESIAN_POINT ( 'NONE',  ( 9.617285841233000454, 5.306366356490000769, -7.996450761531000317 ) ) ;
#41230 = CARTESIAN_POINT ( 'NONE',  ( 10.96416317549000041, 7.893339070327000329, -6.439103628860999962 ) ) ;
#41231 = CARTESIAN_POINT ( 'NONE',  ( 10.96118313518939935, 3.207251432249800249, -8.502430091786999711 ) ) ;
#41232 = EDGE_CURVE ( 'NONE', #10787, #47324, #47231, .T. ) ;
#41233 = CARTESIAN_POINT ( 'NONE',  ( 12.41659929819182118, 0.4896501542853322064, 12.68729270499356510 ) ) ;
#41234 = CARTESIAN_POINT ( 'NONE',  ( 5.630370665534807806, -12.10426712534045990, -3.742487578858010089 ) ) ;
#41235 = CARTESIAN_POINT ( 'NONE',  ( 9.538432183420001209, 5.620896541217999420, 7.423100299691999915 ) ) ;
#41236 = CARTESIAN_POINT ( 'NONE',  ( 11.26444844843000048, -3.604811106221999850, 11.32703155999000089 ) ) ;
#41237 = ORIENTED_EDGE ( 'NONE', *, *, #60971, .F. ) ;
#41238 = CARTESIAN_POINT ( 'NONE',  ( 9.128895280414001334, 3.880154689736000417, -9.060377011187000562 ) ) ;
#41239 = CARTESIAN_POINT ( 'NONE',  ( -2.444943969992999916E-05, -2.899969545325999931, 0.000000000000000000 ) ) ;
#41240 = CARTESIAN_POINT ( 'NONE',  ( 17.96200919170517096, 2.025537500457071260, 13.76266550596355209 ) ) ;
#41241 = CARTESIAN_POINT ( 'NONE',  ( 10.16684687351567007, 4.768183399968648040, 8.499583552997725278 ) ) ;
#41242 = CARTESIAN_POINT ( 'NONE',  ( 12.09999999999999964, -3.133991299512489892, 8.272804384030438385 ) ) ;
#41243 = CARTESIAN_POINT ( 'NONE',  ( 11.26487482311540056, -3.069598554678400149, -7.875904247640098887 ) ) ;
#41244 = ORIENTED_EDGE ( 'NONE', *, *, #17890, .F. ) ;
#41245 = CARTESIAN_POINT ( 'NONE',  ( 1.915792463674000023, 0.7707009544374999743, -3.678912518181000291 ) ) ;
#41246 = CARTESIAN_POINT ( 'NONE',  ( 10.37901637862746895, -2.804465802327228197, 8.962024696469146789 ) ) ;
#41248 = DIRECTION ( 'NONE',  ( 0.000000000000000000, 0.000000000000000000, -1.000000000000000000 ) ) ;
#41247 = CARTESIAN_POINT ( 'NONE',  ( 9.152446624286001864, 2.899999999999999911, -6.169193161299999950 ) ) ;
#41249 = CARTESIAN_POINT ( 'NONE',  ( 0.000000000000000000, -2.899999999999999911, -7.500000000000000000 ) ) ;
#41250 = CARTESIAN_POINT ( 'NONE',  ( 10.38314899745999931, 5.167567567567999731, 6.822293592207000934 ) ) ;
#41251 = CARTESIAN_POINT ( 'NONE',  ( 18.12478797189200463, -2.757742546077707413, -13.61537068597722211 ) ) ;
#41252 = CARTESIAN_POINT ( 'NONE',  ( 11.21979841651039855, 3.695024856201900132, 6.689266534545799558 ) ) ;
#41253 = CARTESIAN_POINT ( 'NONE',  ( 15.90018573812399971, -8.493548356068000516, -8.263529029821000904 ) ) ;
#41254 = CARTESIAN_POINT ( 'NONE',  ( 9.341483607044001047, -4.148132978932999926, 9.337467253566000380 ) ) ;
#41255 = ORIENTED_EDGE ( 'NONE', *, *, #33187, .T. ) ;
#41256 = CARTESIAN_POINT ( 'NONE',  ( 7.764232780408999446, 4.628941086829000184, 5.991667691044999522 ) ) ;
#41258 = CARTESIAN_POINT ( 'NONE',  ( 10.49412055961999890, -2.866949708568999888, -8.960719633954001395 ) ) ;
#41257 = CARTESIAN_POINT ( 'NONE',  ( 5.217721112195000899, -0.1291622704458000037, -1.609550399409999999 ) ) ;
#41259 = VECTOR ( 'NONE', #54670, 1000.000000000000114 ) ;
#41260 = CARTESIAN_POINT ( 'NONE',  ( 7.585160972467329898, -4.237318164244575414, 5.776645283239123074 ) ) ;
#41261 = PLANE ( 'NONE',  #10097 ) ;
#41262 = CARTESIAN_POINT ( 'NONE',  ( 1.748021089240999970, -0.2184777168079999887, 3.585542759708000293 ) ) ;
#41263 = ORIENTED_EDGE ( 'NONE', *, *, #4039, .F. ) ;
#41264 = CARTESIAN_POINT ( 'NONE',  ( 1.143321103043043463, -0.3342943453538773646, -3.285837508824063224 ) ) ;
#41265 = CARTESIAN_POINT ( 'NONE',  ( 11.32595391537419971, -3.283439621430300104, 7.013338090450799811 ) ) ;
#41266 = CARTESIAN_POINT ( 'NONE',  ( 9.595493858556999101, 3.928424745541000185, 5.531312048131000303 ) ) ;
#41267 = CARTESIAN_POINT ( 'NONE',  ( 10.76010575649000067, 4.535386075958999896, 6.001721352166000223 ) ) ;
#41268 = CARTESIAN_POINT ( 'NONE',  ( 11.23610538575739959, 5.109472165990999848, 7.765257665594799796 ) ) ;
#41269 = B_SPLINE_CURVE_WITH_KNOTS ( 'NONE', 3,
 ( #47210, #57007, #35351, #52446, #4540, #14707, #46865, #46523, #19951, #35691, #56674, #8774 ),
 .UNSPECIFIED., .F., .F.,
 ( 4, 2, 2, 2, 2, 4 ),
 ( 0.000000000000000000, 0.2500000000000117129, 0.3750000000000203726, 0.4375000000000172085, 0.5000000000000140998, 1.000000000000000000 ),
 .UNSPECIFIED. ) ;
#41270 = EDGE_CURVE ( 'NONE', #2358, #40685, #27647, .T. ) ;
#41271 = EDGE_CURVE ( 'NONE', #4517, #7244, #52652, .T. ) ;
#41272 = PRODUCT_DEFINITION_SHAPE ( 'NONE', 'NONE',  #69200 ) ;
#41273 = CARTESIAN_POINT ( 'NONE',  ( 23.75090150694354563, -3.269774994020507641, 13.22953792649320448 ) ) ;
#41274 = EDGE_CURVE ( 'NONE', #56214, #5868, #43889, .T. ) ;
#41275 = EDGE_CURVE ( 'NONE', #6365, #53919, #18493, .T. ) ;
#41276 = CARTESIAN_POINT ( 'NONE',  ( 24.30000560035348656, 12.09374145920219767, -3.240508257462953345 ) ) ;
#41277 = CARTESIAN_POINT ( 'NONE',  ( 12.63924565005606304, -1.875000000000000222, 12.57545536278439791 ) ) ;
#41278 = FACE_OUTER_BOUND ( 'NONE', #36541, .T. ) ;
#41279 = CARTESIAN_POINT ( 'NONE',  ( 18.08710802279909657, -2.021458498708258666, 13.85330284862006245 ) ) ;
#41280 = CARTESIAN_POINT ( 'NONE',  ( 17.93700172729746356, 2.995132885295900493, -13.55589876081417522 ) ) ;
#41281 = ORIENTED_EDGE ( 'NONE', *, *, #28984, .F. ) ;
#41282 = CARTESIAN_POINT ( 'NONE',  ( 15.57784398235336631, -9.457709274034865388, -8.211421075710321205 ) ) ;
#41283 = CARTESIAN_POINT ( 'NONE',  ( 9.099999999999999645, -11.84999999999999964, 0.000000000000000000 ) ) ;
#41284 = ORIENTED_EDGE ( 'NONE', *, *, #31889, .T. ) ;
#41285 = CARTESIAN_POINT ( 'NONE',  ( 10.89598863732999945, -5.294083316034999598, 4.900488582003999838 ) ) ;
#41286 = CARTESIAN_POINT ( 'NONE',  ( 15.90018573812067260, 5.468217585226911481, 10.55609518975849248 ) ) ;
#41287 = CARTESIAN_POINT ( 'NONE',  ( 9.414312736919001168, 3.941041961981000430, 5.878350450964999752 ) ) ;
#41288 = CARTESIAN_POINT ( 'NONE',  ( 10.31499646082999888, 5.458376174241999834, -8.355105941236999456 ) ) ;
#41289 = CARTESIAN_POINT ( 'NONE',  ( 20.00000000000000000, 0.000000000000000000, 0.000000000000000000 ) ) ;
#41290 = CARTESIAN_POINT ( 'NONE',  ( 11.24052627608000066, -2.774025043188999895, 6.782107572692000375 ) ) ;
#41291 = B_SPLINE_CURVE_WITH_KNOTS ( 'NONE', 3,
 ( #8231, #39704, #55784, #49493, #22921, #55439, #17693, #39018, #7532, #29223, #12442, #55089, #7196, #49845, #23277, #38186, #44150, #48339, #59519, #16522, #11614, #48689, #64399, #1140, #49369, #21761, #17568, #43793, #59862, #37849, #49032, #60216, #38539, #11968, #33304 ),
 .UNSPECIFIED., .F., .F.,
 ( 4, 1, 1, 1, 1, 1, 1, 1, 1, 1, 1, 1, 1, 1, 1, 1, 1, 1, 1, 1, 1, 1, 1, 1, 1, 1, 1, 1, 1, 1, 1, 1, 4 ),
 ( 0.000000000000000000, 0.02634724210002143546, 0.05799096732718442282, 0.08963469255434740324, 0.1212784177813101688, 0.1529221430084731492, 0.1845658682354359148, 0.2162095934625989091, 0.2478533186897619034, 0.2794970439167246412, 0.3111407691438876633, 0.3427844943710506298, 0.3744282195980133676, 0.4060719448251763897, 0.4377156700521391275, 0.4693593952793021495, 0.5010031205064651161, 0.5326468457334281315, 0.5642905709605910980, 0.5959342961875536693, 0.6275780214147168579, 0.6592217466418798244, 0.6908654718688423957, 0.7225091970960055843, 0.7541529223229681556, 0.7857966475501313441, 0.8174403727772943107, 0.8490840980042568820, 0.8807278232314200705, 0.9123715484585830371, 0.9440152736855456084, 0.9756589989127087970, 1.000000000000000000 ),
 .UNSPECIFIED. ) ;
#41292 = CARTESIAN_POINT ( 'NONE',  ( 18.21544979345815563, 0.2970375428997837353, -12.59650273238872664 ) ) ;
#41293 = LINE ( 'NONE', #14724, #53107 ) ;
#41294 = CARTESIAN_POINT ( 'NONE',  ( 10.48133997687999930, -3.815400206859000054, -6.653701289769800020 ) ) ;
#41295 = CARTESIAN_POINT ( 'NONE',  ( 24.30001685126999789, 8.938702716825000394, -8.938676159935001309 ) ) ;
#41296 = ORIENTED_EDGE ( 'NONE', *, *, #1037, .T. ) ;
#41297 = CARTESIAN_POINT ( 'NONE',  ( 11.02143415462000142, -6.126230856447000050, -5.117104822491000071 ) ) ;
#41298 = PRESENTATION_STYLE_ASSIGNMENT (( #67167 ) ) ;
#41299 = DIRECTION ( 'NONE',  ( -1.000000000000000000, 0.000000000000000000, 0.000000000000000000 ) ) ;
#41300 = DIRECTION ( 'NONE',  ( 1.000000000000000000, 0.000000000000000000, 0.000000000000000000 ) ) ;
#41301 = CARTESIAN_POINT ( 'NONE',  ( 10.19601354018254291, -3.000416447002272058, -6.731816600031361730 ) ) ;
#41302 = CARTESIAN_POINT ( 'NONE',  ( 17.87873473849105110, 1.836456536727118394, 12.46545041361348716 ) ) ;
#41303 = CARTESIAN_POINT ( 'NONE',  ( 12.08015713295724858, 2.543697886577362954, 13.76699599502173399 ) ) ;
#41304 = CARTESIAN_POINT ( 'NONE',  ( 9.966331042021000286, -2.304002513595999613, 6.575636708208000059 ) ) ;
#41305 = VERTEX_POINT ( 'NONE', #68825 ) ;
#41306 = CARTESIAN_POINT ( 'NONE',  ( 12.47604026673111477, 0.5315006616213344692, -12.68502792338267504 ) ) ;
#41307 = DIRECTION ( 'NONE',  ( 1.000000000000000000, 0.000000000000000000, 0.000000000000000000 ) ) ;
#41308 = VERTEX_POINT ( 'NONE', #26540 ) ;
#41309 = CARTESIAN_POINT ( 'NONE',  ( 12.68566995881739601, -1.770266656024991114, 12.47502217142794478 ) ) ;
#41310 = CARTESIAN_POINT ( 'NONE',  ( 18.29995268966800026, 2.861739928647000220, 11.98821236628000086 ) ) ;
#41311 = VECTOR ( 'NONE', #10151, 1000.000000000000000 ) ;
#41312 = FACE_OUTER_BOUND ( 'NONE', #12580, .T. ) ;
#41313 = CARTESIAN_POINT ( 'NONE',  ( 11.52287616594230002, -4.261927842557799551, 8.325646653015098764 ) ) ;
#41314 = B_SPLINE_SURFACE_WITH_KNOTS ( 'NONE', 3, 3, ( 
 ( #65645, #55163, #38389, #43993 ),
 ( #54124, #65299, #22306, #17415 ),
 ( #65986, #49572, #39431, #11815 ),
 ( #38741, #64605, #33504, #48543 ),
 ( #33156, #43646, #17770, #54472 ),
 ( #16711, #21959, #6574, #27914 ),
 ( #2032, #54819, #49919, #1681 ),
 ( #6919, #22997, #49223, #22648 ),
 ( #1331, #44347, #39088, #28251 ),
 ( #23350, #60412, #12518, #648 ),
 ( #33849, #7268, #28607, #60752 ),
 ( #12866, #44692, #38041, #34195 ) ),
 .UNSPECIFIED., .F., .F., .F.,
 ( 4, 1, 1, 1, 1, 1, 1, 1, 1, 4 ),
 ( 4, 4 ),
 ( 0.01095806325966000062, 0.05000000000000000278, 0.1000000000000000056, 0.1499999999999999944, 0.2000000000000000111, 0.2500000000000000000, 0.2999999999999999889, 0.3499999999999999778, 0.4000000000000000222, 0.4461661505078000078 ),
 ( -0.2706701093251999701, 1.270791579988999942 ),
 .UNSPECIFIED. ) ;
#41315 = ADVANCED_FACE ( 'NONE', ( #4851 ), #9756, .T. ) ;
#41316 = CARTESIAN_POINT ( 'NONE',  ( 24.39664233851466690, -12.03536604771145413, -3.224866613121610381 ) ) ;
#41317 = LINE ( 'NONE', #19994, #57738 ) ;
#41318 = CARTESIAN_POINT ( 'NONE',  ( 10.98768472639999949, 2.860903110339000133, 4.945212061661000469 ) ) ;
#41319 = EDGE_CURVE ( 'NONE', #50139, #6099, #39282, .T. ) ;
#41320 = CARTESIAN_POINT ( 'NONE',  ( 12.28024471298226850, 1.983745382141952840, 12.44286253672009579 ) ) ;
#41321 = DIRECTION ( 'NONE',  ( 0.000000000000000000, -0.8648648648648720183, 0.5020047465136825426 ) ) ;
#41322 = CARTESIAN_POINT ( 'NONE',  ( 10.55103166480599874, 2.999015536536000504, -7.570575893572789816 ) ) ;
#41323 = CARTESIAN_POINT ( 'NONE',  ( 5.099999999649000415, -1.199999999999999956, -11.12663029847899843 ) ) ;
#41324 = CARTESIAN_POINT ( 'NONE',  ( 10.24394221959000184, 3.220342255699999878, -6.005413528376000620 ) ) ;
#41325 = CARTESIAN_POINT ( 'NONE',  ( 8.845430433046999497, 2.911395389258000233, -6.828193190755800224 ) ) ;
#41327 = CARTESIAN_POINT ( 'NONE',  ( 9.206426979769998908, -4.358851904410700584, 6.723921629386799381 ) ) ;
#41326 = DIRECTION ( 'NONE',  ( 0.9999999999999682476, 2.518941077746920288E-07, -2.686336010433915230E-09 ) ) ;
#41328 = CARTESIAN_POINT ( 'NONE',  ( 23.59999441188499958, 10.30760541648000128, -9.317696302454001156 ) ) ;
#41329 = ORIENTED_EDGE ( 'NONE', *, *, #12873, .F. ) ;
#41330 = CARTESIAN_POINT ( 'NONE',  ( 12.44983299104790397, -0.5143225250488896449, 12.68597987475963684 ) ) ;
#41331 = CARTESIAN_POINT ( 'NONE',  ( 10.77879632507499785, 4.423544049216699747, 6.714825466131699727 ) ) ;
#41332 = CARTESIAN_POINT ( 'NONE',  ( 9.944325809452999820, -5.443013936195000291, 7.367349259341000156 ) ) ;
#41333 = CARTESIAN_POINT ( 'NONE',  ( 10.05826717315599872, 3.340104753140699767, 8.062357722167599050 ) ) ;
#41334 = CARTESIAN_POINT ( 'NONE',  ( 9.125583543129625497, 3.128114063008116563, -7.573124426811684629 ) ) ;
#41335 = CARTESIAN_POINT ( 'NONE',  ( 5.700000001242999659, -1.249999998757000075, 1.883720477311000285E-09 ) ) ;
#41336 = CARTESIAN_POINT ( 'NONE',  ( 29.91622776601699840, 7.448825475110001390E-09, -6.772075922005999615 ) ) ;
#41337 = CARTESIAN_POINT ( 'NONE',  ( 12.18808187646823882, 2.399650199051974298, 13.69418124938378156 ) ) ;
#41338 = CARTESIAN_POINT ( 'NONE',  ( 8.159770655660624428, 3.206342737484559002, 6.208500430850088847 ) ) ;
#41339 = ORIENTED_EDGE ( 'NONE', *, *, #1484, .T. ) ;
#41340 = CARTESIAN_POINT ( 'NONE',  ( 4.466438209866000264, -0.8917438941569999500, -0.9119035439078000405 ) ) ;
#41341 = CARTESIAN_POINT ( 'NONE',  ( 8.972076168957999087, -4.649151400100800302, -8.602264418015000302 ) ) ;
#41342 = CARTESIAN_POINT ( 'NONE',  ( 10.41258553782401464, -4.805411882504589727, -4.969623107670830819 ) ) ;
#41343 = CARTESIAN_POINT ( 'NONE',  ( 11.10746886766490071, -4.498335456194499926, 8.405426684175299812 ) ) ;
#41344 = VECTOR ( 'NONE', #26006, 1000.000000000000114 ) ;
#41345 = CARTESIAN_POINT ( 'NONE',  ( 17.85753477061698646, 1.826313832178713126, -12.46694048874450900 ) ) ;
#41346 = CARTESIAN_POINT ( 'NONE',  ( 2.584306799209334038, 1.762666431298138825, 3.058252359239908014 ) ) ;
#41347 = CARTESIAN_POINT ( 'NONE',  ( 18.17043869203643425, 2.609785213594550068, 12.42531509794201661 ) ) ;
#41348 = EDGE_CURVE ( 'NONE', #15832, #67676, #48318, .T. ) ;
#41349 = CARTESIAN_POINT ( 'NONE',  ( 12.19167018792746227, 2.619965297409280414, -13.64728369052539847 ) ) ;
#41350 = CARTESIAN_POINT ( 'NONE',  ( 11.05049011050999930, -2.763560161389000402, -5.018746270741000437 ) ) ;
#41351 = CARTESIAN_POINT ( 'NONE',  ( 9.926183059621999760, -4.356410583133000003, -9.313949118577001585 ) ) ;
#41352 = CARTESIAN_POINT ( 'NONE',  ( 9.573148997458000409, 5.167567567567999731, -6.822293592207000934 ) ) ;
#41353 = ADVANCED_FACE ( 'NONE', ( #25844 ), #7049, .F. ) ;
#41354 = CARTESIAN_POINT ( 'NONE',  ( 12.09168665071629256, 0.1308528744652265041, -13.99939340647621222 ) ) ;
#41355 = ADVANCED_FACE ( 'NONE', ( #15359 ), #13745, .T. ) ;
#41356 = CARTESIAN_POINT ( 'NONE',  ( 23.63077126582529175, 13.40261082913402113, 3.886325453134984897 ) ) ;
#41357 = DIRECTION ( 'NONE',  ( -0.000000000000000000, -0.000000000000000000, 1.000000000000000000 ) ) ;
#41358 = PLANE ( 'NONE',  #63831 ) ;
#41359 = VECTOR ( 'NONE', #22822, 1000.000000000000227 ) ;
#41360 = CARTESIAN_POINT ( 'NONE',  ( 18.17737860441360809, -11.15478131644662874, 3.361574628443296575 ) ) ;
#41361 = CARTESIAN_POINT ( 'NONE',  ( 6.799634134627482673, 1.520134557123164365, -0.1051316465493104674 ) ) ;
#41362 = ORIENTED_EDGE ( 'NONE', *, *, #14440, .F. ) ;
#41363 = CARTESIAN_POINT ( 'NONE',  ( 8.445233760363073827, -5.313925467271338299, 7.853812692271767482 ) ) ;
#41364 = CARTESIAN_POINT ( 'NONE',  ( 18.00853468083866460, 1.948185427393965607, -13.86378859567400923 ) ) ;
#41365 = ORIENTED_EDGE ( 'NONE', *, *, #18066, .F. ) ;
#41366 = CARTESIAN_POINT ( 'NONE',  ( 10.84588779216199939, -3.198058499272899979, 7.210800365544999480 ) ) ;
#41367 = CARTESIAN_POINT ( 'NONE',  ( 10.68035971519489813, 4.678140486081599825, 8.628134814664999652 ) ) ;
#41368 = CARTESIAN_POINT ( 'NONE',  ( 18.50007554376852426, 2.772760791841625938, -11.31557096909393323 ) ) ;
#41369 = CARTESIAN_POINT ( 'NONE',  ( 11.43210843320491499, -5.137688304401064165, 6.901605483505058203 ) ) ;
#41370 = CARTESIAN_POINT ( 'NONE',  ( 10.56591429142999949, -3.980313504646230349, -6.466681092390999197 ) ) ;
#41371 = CARTESIAN_POINT ( 'NONE',  ( 11.60000000000000142, -3.579171096429341503, -6.483899970161565385 ) ) ;
#41372 = DIRECTION ( 'NONE',  ( -1.000000000000000000, 0.000000000000000000, 0.000000000000000000 ) ) ;
#41373 = ORIENTED_EDGE ( 'NONE', *, *, #16001, .T. ) ;
#41374 = CARTESIAN_POINT ( 'NONE',  ( 5.000000000000000000, 0.8000000000000000444, -3.149999999999999911 ) ) ;
#41375 = CARTESIAN_POINT ( 'NONE',  ( 9.137754719594999742, 2.319062457810000311, -7.919229449146000022 ) ) ;
#41376 = ORIENTED_EDGE ( 'NONE', *, *, #50407, .T. ) ;
#41377 = EDGE_CURVE ( 'NONE', #60176, #36031, #65139, .T. ) ;
#41378 = CARTESIAN_POINT ( 'NONE',  ( 11.15192953222999961, 2.359300361215999953, -6.636686939130999718 ) ) ;
#41379 = SHAPE_REPRESENTATION_RELATIONSHIP ( 'NONE' , 'NONE' ,  #53976, #23576 ) ;
#41380 = ORIENTED_EDGE ( 'NONE', *, *, #57915, .T. ) ;
#41381 = CARTESIAN_POINT ( 'NONE',  ( 9.149380199233998923, 5.269225938816000543, 7.659530259549099718 ) ) ;
#41382 = CARTESIAN_POINT ( 'NONE',  ( 18.05338926791298704, -2.122656057830398790, -12.53150860927891941 ) ) ;
#41383 = CARTESIAN_POINT ( 'NONE',  ( 11.09999938828999966, -12.24999938819000000, -1.815295647579999972E-09 ) ) ;
#41384 = CARTESIAN_POINT ( 'NONE',  ( 24.66271477989500127, -12.38330044149000031, -2.963253076001000075 ) ) ;
#41385 = CARTESIAN_POINT ( 'NONE',  ( 11.03723142223999965, -8.047823047122999895, -7.049859988296000246 ) ) ;
#41386 = ORIENTED_EDGE ( 'NONE', *, *, #23270, .T. ) ;
#41387 = CARTESIAN_POINT ( 'NONE',  ( 10.22422653164065487, 2.899999999999999911, -6.304440313833538312 ) ) ;
#41388 = B_SPLINE_CURVE_WITH_KNOTS ( 'NONE', 1,
 ( #34317, #7736 ),
 .UNSPECIFIED., .F., .F.,
 ( 2, 2 ),
 ( 0.000000000000000000, 1.000000000000000000 ),
 .UNSPECIFIED. ) ;
#41389 = CARTESIAN_POINT ( 'NONE',  ( 5.500000000000000000, 0.000000000000000000, 0.000000000000000000 ) ) ;
#41390 = DIRECTION ( 'NONE',  ( -1.000000000000000000, 0.000000000000000000, 0.000000000000000000 ) ) ;
#41391 = CARTESIAN_POINT ( 'NONE',  ( 8.969356963619999235, 2.880642974985999860, 7.500000000085178087 ) ) ;
#41392 = B_SPLINE_CURVE_WITH_KNOTS ( 'NONE', 3,
 ( #68353, #51938, #68014, #35870 ),
 .UNSPECIFIED., .F., .F.,
 ( 4, 4 ),
 ( 0.000000000000000000, 1.000000000000000000 ),
 .UNSPECIFIED. ) ;
#41393 = AXIS2_PLACEMENT_3D ( 'NONE', #29119, #11628, #7780 ) ;
#41394 = CARTESIAN_POINT ( 'NONE',  ( 18.05077945915500592, 0.5329747956504938822, 13.98985355243729067 ) ) ;
#41395 = CARTESIAN_POINT ( 'NONE',  ( 17.77447410014400120, 3.189754565392000085, 11.45074580414000032 ) ) ;
#41396 = CARTESIAN_POINT ( 'NONE',  ( 10.61721988130000049, -5.045606037229999785, -6.386907901056999570 ) ) ;
#41397 = ORIENTED_EDGE ( 'NONE', *, *, #45546, .F. ) ;
#41398 = ORIENTED_EDGE ( 'NONE', *, *, #19007, .F. ) ;
#41399 = CONICAL_SURFACE ( 'NONE', #30283, 12.42518894556000042, 0.7854133338342391690 ) ;
#41400 = CARTESIAN_POINT ( 'NONE',  ( 9.178620280414001797, 2.990001567622999623, -8.695425648791999862 ) ) ;
#41401 = EDGE_CURVE ( 'NONE', #44536, #46125, #28262, .T. ) ;
#41402 = CARTESIAN_POINT ( 'NONE',  ( 4.650001657043312697, -2.000000000000000000, -2.821984759847882640E-09 ) ) ;
#41403 = CARTESIAN_POINT ( 'NONE',  ( 12.80505043854146940, -3.125000000000000000, 13.52084414783465860 ) ) ;
#41404 = CARTESIAN_POINT ( 'NONE',  ( 23.67309812202378438, 3.197429271368524173, 13.39122446713678904 ) ) ;
#41405 = CARTESIAN_POINT ( 'NONE',  ( 23.61340685958100138, 10.15619120159999866, -9.483135970162001271 ) ) ;
#41406 = CARTESIAN_POINT ( 'NONE',  ( 9.054101285863998427, 3.441732526340400167, -6.836640842107200022 ) ) ;
#41408 = CARTESIAN_POINT ( 'NONE',  ( 8.852883527364793892, 3.390765634497458159, 9.167735097122442056 ) ) ;
#41407 = CARTESIAN_POINT ( 'NONE',  ( 10.07902593514599943, -4.145841638824199649, 8.493766832166899761 ) ) ;
#41409 = CARTESIAN_POINT ( 'NONE',  ( 11.00000000000000000, 5.200000000000000178, -5.865766984179000332 ) ) ;
#41410 = VERTEX_POINT ( 'NONE', #20947 ) ;
#41411 = CARTESIAN_POINT ( 'NONE',  ( 24.84573432944931426, -12.09401906330531595, 2.924964065930268475 ) ) ;
#41412 = CARTESIAN_POINT ( 'NONE',  ( 7.964385314170995933, -2.867871570892000399, 6.759005350280994584 ) ) ;
#41413 = CARTESIAN_POINT ( 'NONE',  ( 10.26693802597399952, 3.334935831489500124, 8.592736948783000983 ) ) ;
#41414 = DIRECTION ( 'NONE',  ( 1.000000000000000000, 0.000000000000000000, 0.000000000000000000 ) ) ;
#41415 = DIRECTION ( 'NONE',  ( 0.8480635683784329970, -0.3746919961710145075, -0.3746919961710145075 ) ) ;
#41416 = CARTESIAN_POINT ( 'NONE',  ( 0.1499996298882999846, 0.000000000000000000, 0.000000000000000000 ) ) ;
#41417 = CARTESIAN_POINT ( 'NONE',  ( 8.646410841231000788, 2.261390688294000029, -6.733978371730000134 ) ) ;
#41418 = PLANE ( 'NONE',  #58122 ) ;
#41419 = CARTESIAN_POINT ( 'NONE',  ( 7.969586219655325543, 2.977443839350291555, -6.507548348051052756 ) ) ;
#41420 = LINE ( 'NONE', #67631, #35608 ) ;
#41421 = PLANE ( 'NONE',  #47741 ) ;
#41422 = CARTESIAN_POINT ( 'NONE',  ( 25.39991555675432267, -10.74016618265575573, -3.821986234823466777 ) ) ;
#41423 = CARTESIAN_POINT ( 'NONE',  ( 2.728791824580000025, 2.059424881456000112, -2.525877225825000405 ) ) ;
#41424 = VERTEX_POINT ( 'NONE', #15700 ) ;
#41425 = CARTESIAN_POINT ( 'NONE',  ( 12.47502136616923352, -0.5311517451680624058, -12.68505220952107670 ) ) ;
#41426 = CARTESIAN_POINT ( 'NONE',  ( 12.18494477642119378, -2.419331844715135738, -12.47000601354013227 ) ) ;
#41427 = CARTESIAN_POINT ( 'NONE',  ( 8.757697342472001267, 2.899999999999999911, -6.397101765418000241 ) ) ;
#41428 = CARTESIAN_POINT ( 'NONE',  ( 24.60109542677746575, 3.453340786472776092, -12.10341549489917590 ) ) ;
#41429 = CARTESIAN_POINT ( 'NONE',  ( 1.759306799208166350, -3.058252359239909346, 1.762666431298136605 ) ) ;
#41430 = ORIENTED_EDGE ( 'NONE', *, *, #2048, .F. ) ;
#41431 = CARTESIAN_POINT ( 'NONE',  ( 17.55505043854147118, -1.875000000000000000, -25.00000000000000000 ) ) ;
#41432 = AXIS2_PLACEMENT_3D ( 'NONE', #50266, #48975, #59454 ) ;
#41433 = ADVANCED_FACE ( 'NONE', ( #58008 ), #65794, .T. ) ;
#41434 = PRODUCT_CONTEXT ( 'NONE', #37366, 'mechanical' ) ;
#41435 = EDGE_CURVE ( 'NONE', #3245, #5981, #17617, .T. ) ;
#41436 = CARTESIAN_POINT ( 'NONE',  ( 17.82925890460733598, 0.5617199691901461067, 12.68327559333872934 ) ) ;
#41437 = CARTESIAN_POINT ( 'NONE',  ( 10.34393020685000053, -5.250000000000000000, 7.500000000000000000 ) ) ;
#41438 = CARTESIAN_POINT ( 'NONE',  ( 7.790487273278715818, 2.917542662690631339, 6.652519583927194446 ) ) ;
#41439 = CARTESIAN_POINT ( 'NONE',  ( 10.98146005378009882, 4.911671201000399556, -7.013182449205100255 ) ) ;
#41440 = VERTEX_POINT ( 'NONE', #56892 ) ;
#41441 = CARTESIAN_POINT ( 'NONE',  ( 10.09181272066999924, -2.440908155048000516, 7.817368209339999652 ) ) ;
#41442 = EDGE_LOOP ( 'NONE', ( #42200, #3705, #20113, #32768, #17710, #26813, #62885, #54894, #35206, #9569, #63454, #17598 ) ) ;
#41443 = LINE ( 'NONE', #57169, #47346 ) ;
#41444 = CARTESIAN_POINT ( 'NONE',  ( 9.240543146793999796, -4.158911960977000000, 5.873536005760000123 ) ) ;
#41445 = CARTESIAN_POINT ( 'NONE',  ( 15.86242637978999959, 8.523064092628001021, 8.288181269780999116 ) ) ;
#41446 = EDGE_LOOP ( 'NONE', ( #308, #3703, #42781, #14469 ) ) ;
#41447 = CARTESIAN_POINT ( 'NONE',  ( 8.591652855523911114, 2.244927656352591505, -7.464460470874615616 ) ) ;
#41448 = CARTESIAN_POINT ( 'NONE',  ( 9.074999999999999289, 4.417172942406000224, 8.783926296998000538 ) ) ;
#41449 = VECTOR ( 'NONE', #49031, 1000.000000000000000 ) ;
#41450 = CARTESIAN_POINT ( 'NONE',  ( 6.844639158771000709, 2.603491674958000157, -7.446887986542999549 ) ) ;
#41451 = CARTESIAN_POINT ( 'NONE',  ( 11.03443712336079940, 5.057168833716702672, 7.824978679112010838 ) ) ;
#41452 = CARTESIAN_POINT ( 'NONE',  ( 10.17500046684972936, -2.650307855384914202, 7.500001770945068813 ) ) ;
#41453 = ORIENTED_EDGE ( 'NONE', *, *, #7400, .T. ) ;
#41454 = CARTESIAN_POINT ( 'NONE',  ( 2.021806799206416372, 3.408904368339103375, 0.9161175952574877046 ) ) ;
#41455 = CARTESIAN_POINT ( 'NONE',  ( 12.23172337865274706, -2.748896841596946583, -13.61745941693682305 ) ) ;
#41456 = CARTESIAN_POINT ( 'NONE',  ( 11.09999999999999964, -4.000000000000000000, 7.500000000000000000 ) ) ;
#41457 = ORIENTED_EDGE ( 'NONE', *, *, #43653, .F. ) ;
#41458 = EDGE_CURVE ( 'NONE', #55952, #51112, #27122, .T. ) ;
#41459 = CARTESIAN_POINT ( 'NONE',  ( 9.780291077142999612, -3.021588645102999848, -8.450043670922001482 ) ) ;
#41460 = PLANE ( 'NONE',  #58225 ) ;
#41461 = ORIENTED_EDGE ( 'NONE', *, *, #8276, .T. ) ;
#41462 = CARTESIAN_POINT ( 'NONE',  ( 10.98194940877535863, 2.363165821928819188, 6.818563111302845314 ) ) ;
#41463 = ADVANCED_FACE ( 'NONE', ( #14249 ), #57926, .T. ) ;
#41464 = CARTESIAN_POINT ( 'NONE',  ( 11.42394752546313441, 3.297753801639562443, -8.603859202887296220 ) ) ;
#41465 = CARTESIAN_POINT ( 'NONE',  ( 5.115443173016708478, -1.500000000000000222, -0.1963495408493622085 ) ) ;
#41466 = CARTESIAN_POINT ( 'NONE',  ( 10.90000000000000036, -0.2500000000000000000, -4.902439024389999567 ) ) ;
#41467 = CARTESIAN_POINT ( 'NONE',  ( 12.09999999999999964, -4.000000000000000000, 7.500000000000000000 ) ) ;
#41468 = CARTESIAN_POINT ( 'NONE',  ( 9.435596873515667227, -5.092232985442824322, -8.129523725463622341 ) ) ;
#41469 = CARTESIAN_POINT ( 'NONE',  ( 17.62782920531153863, -1.879164230502278210, 12.57477362212319250 ) ) ;
#41470 = ORIENTED_EDGE ( 'NONE', *, *, #12087, .T. ) ;
#41471 = CARTESIAN_POINT ( 'NONE',  ( 8.057193283769001013, -5.122325659685000865, 6.732791538586998747 ) ) ;
#41472 = ORIENTED_EDGE ( 'NONE', *, *, #13109, .F. ) ;
#41473 = CARTESIAN_POINT ( 'NONE',  ( 10.25888757983999966, 4.512388525173999909, 5.993701490107000929 ) ) ;
#41474 = CARTESIAN_POINT ( 'NONE',  ( 11.04384236319999957, 5.374507068257000419, 5.035088906224999938 ) ) ;
#41475 = CARTESIAN_POINT ( 'NONE',  ( 12.78422835261024382, 1.875000554926936402, -13.78631940402569889 ) ) ;
#41476 = CARTESIAN_POINT ( 'NONE',  ( 3.683590334856999604, -3.383589507348999881, 0.007585966762053000974 ) ) ;
#41477 = CARTESIAN_POINT ( 'NONE',  ( 10.39355669675000016, -4.089958462238000081, -9.188182957628999503 ) ) ;
#41478 = CARTESIAN_POINT ( 'NONE',  ( 10.53521345716899837, 4.924890298941200228, -8.340879262988799780 ) ) ;
#41479 = FACE_OUTER_BOUND ( 'NONE', #32936, .T. ) ;
#41480 = EDGE_LOOP ( 'NONE', ( #58963, #40330, #19866, #60690, #16361, #37623, #7924, #30507, #67238, #6094, #58141, #43547, #16248, #34142, #36568, #5772, #18090, #39056, #49659, #42018, #37209, #21326 ) ) ;
#41481 = CARTESIAN_POINT ( 'NONE',  ( 10.70641772631199906, -3.568446272909699957, 6.611684804099500212 ) ) ;
#41482 = CARTESIAN_POINT ( 'NONE',  ( 11.30000000000000071, 0.000000000000000000, -5.373479439185999994E-14 ) ) ;
#41483 = FACE_OUTER_BOUND ( 'NONE', #34212, .T. ) ;
#41484 = CARTESIAN_POINT ( 'NONE',  ( 23.60000000000000142, 2.204728229456999866, -11.99913219504999873 ) ) ;
#41486 = CARTESIAN_POINT ( 'NONE',  ( 24.35365242081699932, -3.253466243142002057, -12.21167519476998464 ) ) ;
#41485 = CARTESIAN_POINT ( 'NONE',  ( 9.215291255903000689, 4.861981595026999337, 8.938817176893000038 ) ) ;
#41487 = CARTESIAN_POINT ( 'NONE',  ( 10.84641504065830020, 4.804462279649600376, -6.900173947321999179 ) ) ;
#41488 = CARTESIAN_POINT ( 'NONE',  ( 12.80505043854146940, -3.149917237299187267, 12.25147871603038219 ) ) ;
#41489 = CARTESIAN_POINT ( 'NONE',  ( 9.830304848515998728, 4.788504886021700102, -7.860510733857099197 ) ) ;
#41490 = CARTESIAN_POINT ( 'NONE',  ( 18.10066919781364803, 0.4738025322793226746, 12.59109159930368627 ) ) ;
#41491 = CARTESIAN_POINT ( 'NONE',  ( 7.006988838338999770, 0.6190876222846001253, -0.9481936368762999834 ) ) ;
#41492 = AXIS2_PLACEMENT_3D ( 'NONE', #34656, #3502, #24840 ) ;
#41493 = CARTESIAN_POINT ( 'NONE',  ( 10.92968717260509948, 3.312350236372100021, 6.377637058250999580 ) ) ;
#41494 = CARTESIAN_POINT ( 'NONE',  ( 23.52015295616099877, 10.38924838980999965, 9.574931041765999851 ) ) ;
#41495 = ORIENTED_EDGE ( 'NONE', *, *, #24564, .T. ) ;
#41496 = CARTESIAN_POINT ( 'NONE',  ( 9.015543146794000151, -4.175914961544999748, 5.699510287082000026 ) ) ;
#41497 = CARTESIAN_POINT ( 'NONE',  ( 17.85637496866990404, 3.182194879603814197, 13.63354919460146064 ) ) ;
#41498 = CARTESIAN_POINT ( 'NONE',  ( 25.60000000000000142, 3.623466631435000362, -13.52296156804999860 ) ) ;
#41499 = VERTEX_POINT ( 'NONE', #35577 ) ;
#41500 = CARTESIAN_POINT ( 'NONE',  ( 0.3621912743483999830, 0.6171034757514999303, 3.149659041885999766 ) ) ;
#41501 = CARTESIAN_POINT ( 'NONE',  ( 11.47500581613029880, 4.988618570924500339, 6.865182626353099948 ) ) ;
#41502 = CIRCLE ( 'NONE', #13677, 2.199999999999999734 ) ;
#41503 = CARTESIAN_POINT ( 'NONE',  ( 10.92546721959000067, 5.641524285727999910, -7.883474821562000301 ) ) ;
#41504 = ORIENTED_EDGE ( 'NONE', *, *, #5813, .T. ) ;
#41505 = CARTESIAN_POINT ( 'NONE',  ( 11.09999999999999964, -4.000000000000000000, 7.500000000000000000 ) ) ;
#41506 = CARTESIAN_POINT ( 'NONE',  ( 17.79118476696444517, -3.162166141421065557, 12.19676423671824494 ) ) ;
#41507 = CARTESIAN_POINT ( 'NONE',  ( 11.23195122972050086, 4.507250159094099651, 8.673036084990000560 ) ) ;
#41508 = CARTESIAN_POINT ( 'NONE',  ( 24.30000000000000071, -12.03537377768999939, 3.224868684338999980 ) ) ;
#41509 = CARTESIAN_POINT ( 'NONE',  ( 7.437260841228000352, 2.216873702600000051, 8.370081218683999680 ) ) ;
#41510 = ORIENTED_EDGE ( 'NONE', *, *, #6525, .T. ) ;
#41511 = CARTESIAN_POINT ( 'NONE',  ( 25.00267152972667972, -11.89262042224634897, -2.924336343934345717 ) ) ;
#41512 = EDGE_CURVE ( 'NONE', #50502, #35889, #67324, .T. ) ;
#41513 = EDGE_CURVE ( 'NONE', #33524, #17499, #46131, .T. ) ;
#41514 = CARTESIAN_POINT ( 'NONE',  ( 8.395639158770999089, 4.988620887051999908, -9.026201633254999024 ) ) ;
#41515 = CARTESIAN_POINT ( 'NONE',  ( 8.259902546588161698, -5.265334245408268998, 8.693842063270954768 ) ) ;
#41516 = CARTESIAN_POINT ( 'NONE',  ( 10.10530484851599908, -2.836617618740000069, 6.968092280137199168 ) ) ;
#41517 = ORIENTED_EDGE ( 'NONE', *, *, #27270, .T. ) ;
#41518 = CARTESIAN_POINT ( 'NONE',  ( 10.59787083401000096, -4.986416387023999697, -5.076332610094000941 ) ) ;
#41519 = CARTESIAN_POINT ( 'NONE',  ( 10.79657053952199952, -4.502253688815499366, 8.675184076076000395 ) ) ;
#41520 = ORIENTED_EDGE ( 'NONE', *, *, #19754, .F. ) ;
#41521 = CARTESIAN_POINT ( 'NONE',  ( 12.80505043854146940, -1.787797342887047947, -13.88538010501570774 ) ) ;
#41522 = EDGE_LOOP ( 'NONE', ( #9886, #19840, #11232, #36122 ) ) ;
#41523 = CARTESIAN_POINT ( 'NONE',  ( 9.976909913808000852, -4.233164088428999605, -6.141918726850000176 ) ) ;
#41524 = CARTESIAN_POINT ( 'NONE',  ( 10.47094409420000005, -5.100000000000000533, 6.571291218949999902 ) ) ;
#41525 = CARTESIAN_POINT ( 'NONE',  ( 11.68788784977535933, 3.014014167207800465, -7.443657794094239222 ) ) ;
#41526 = CARTESIAN_POINT ( 'NONE',  ( 11.55946005378019947, -2.963614890480000152, 8.053412743695298914 ) ) ;
#41527 = CARTESIAN_POINT ( 'NONE',  ( 23.60000000000000142, -11.49391741900999975, 4.090215442373000165 ) ) ;
#41528 = CARTESIAN_POINT ( 'NONE',  ( 11.76072066707849828, -3.023932655881500065, 8.090408888831799317 ) ) ;
#41529 = CARTESIAN_POINT ( 'NONE',  ( 10.86325056272499978, -3.107965259299500183, 7.486779603004729111 ) ) ;
#41530 = ORIENTED_EDGE ( 'NONE', *, *, #31763, .F. ) ;
#41531 = CARTESIAN_POINT ( 'NONE',  ( 9.354346873516664829, 2.749999999999999112, -7.663624617374463099 ) ) ;
#41532 = AXIS2_PLACEMENT_3D ( 'NONE', #40413, #66640, #34841 ) ;
#41533 = CARTESIAN_POINT ( 'NONE',  ( 18.20120694906496084, -0.3761765224146920716, 12.59508068834013983 ) ) ;
#41534 = CARTESIAN_POINT ( 'NONE',  ( 9.927263540182998725, 3.370476274536375438, 6.407767014557179230 ) ) ;
#41535 = VERTEX_POINT ( 'NONE', #31360 ) ;
#41536 = CARTESIAN_POINT ( 'NONE',  ( 12.70862826151954295, -1.767199679044274996, -12.47545624547677434 ) ) ;
#41537 = EDGE_CURVE ( 'NONE', #46470, #55031, #52673, .T. ) ;
#41538 = CARTESIAN_POINT ( 'NONE',  ( 11.50271932425157040, 3.812601581225100400, 6.235801371442999397 ) ) ;
#41539 = CARTESIAN_POINT ( 'NONE',  ( 10.94033064679000233, -5.142732045902000948, -6.493502833853999512 ) ) ;
#41540 = DIRECTION ( 'NONE',  ( 1.000000000000000000, 0.000000000000000000, 0.000000000000000000 ) ) ;
#41541 = CARTESIAN_POINT ( 'NONE',  ( 2.479064736456999540, 3.399126080497508973, -0.9633645835951678560 ) ) ;
#41542 = CARTESIAN_POINT ( 'NONE',  ( 10.82101354018296391, 3.231816600031359510, 8.499583552997727054 ) ) ;
#41543 = CARTESIAN_POINT ( 'NONE',  ( 12.61529649622816507, -3.223097538158948616, -13.62393827815043679 ) ) ;
#41544 = B_SPLINE_CURVE_WITH_KNOTS ( 'NONE', 3,
 ( #39404, #67670, #40102, #66306, #18430, #60724, #61417, #13535, #34854, #56169 ),
 .UNSPECIFIED., .F., .F.,
 ( 4, 2, 2, 2, 4 ),
 ( 0.000000000000000000, 0.2500000000000000000, 0.5000000000000000000, 0.7500000000000000000, 1.000000000000000000 ),
 .UNSPECIFIED. ) ;
#41545 = CARTESIAN_POINT ( 'NONE',  ( 10.57980110216399972, -4.739241740354600552, -7.048535450274799885 ) ) ;
#41546 = B_SPLINE_CURVE_WITH_KNOTS ( 'NONE', 3,
 ( #67143, #50736, #61908, #35350 ),
 .UNSPECIFIED., .F., .F.,
 ( 4, 4 ),
 ( 0.000000000000000000, 1.000000000000000000 ),
 .UNSPECIFIED. ) ;
#41547 = CARTESIAN_POINT ( 'NONE',  ( 11.46253286130405691, 4.338994305312701805, -6.691343801417681370 ) ) ;
#41548 = CARTESIAN_POINT ( 'NONE',  ( 21.54999911806000057, 1.172395514003999961E-13, 13.94999927502997572 ) ) ;
#41549 = EDGE_LOOP ( 'NONE', ( #5156, #29044, #66336, #16958 ) ) ;
#41550 = ORIENTED_EDGE ( 'NONE', *, *, #20598, .F. ) ;
#41551 = FACE_OUTER_BOUND ( 'NONE', #60213, .T. ) ;
#41552 = AXIS2_PLACEMENT_3D ( 'NONE', #10516, #26954, #31856 ) ;
#41553 = CARTESIAN_POINT ( 'NONE',  ( 11.09999999999999964, -0.5000000000000000000, -9.662944685757000940 ) ) ;
#41554 = FACE_OUTER_BOUND ( 'NONE', #60072, .T. ) ;
#41555 = CARTESIAN_POINT ( 'NONE',  ( 10.62924593896999959, 3.609487840896999700, -5.855139066690000504 ) ) ;
#41556 = CARTESIAN_POINT ( 'NONE',  ( 24.60109143485134453, -8.755188789252855486, -9.042389807092181542 ) ) ;
#41557 = CARTESIAN_POINT ( 'NONE',  ( 17.65867742935359175, 3.116692472806303904, 12.28625815163619350 ) ) ;
#41558 = CONICAL_SURFACE ( 'NONE', #20343, 1.700000581162000035, 0.7853984839373144844 ) ;
#41559 = CARTESIAN_POINT ( 'NONE',  ( 23.51705920820199935, -13.43782975258999990, 4.375924611141999598 ) ) ;
#41560 = CARTESIAN_POINT ( 'NONE',  ( 10.74609776273999984, 4.263105564403999459, 9.276980853981999786 ) ) ;
#41561 = ORIENTED_EDGE ( 'NONE', *, *, #28453, .F. ) ;
#41562 = CARTESIAN_POINT ( 'NONE',  ( 9.094793214210151078, 2.227663154009282831, -7.390522279650845405 ) ) ;
#41563 = ORIENTED_EDGE ( 'NONE', *, *, #59258, .T. ) ;
#41564 = CARTESIAN_POINT ( 'NONE',  ( 12.49878241383753519, -3.044913063694495214, 12.30777011605604798 ) ) ;
#41565 = CARTESIAN_POINT ( 'NONE',  ( 9.754317406968999293, -3.838745722419000028, -8.351883209406098629 ) ) ;
#41566 = CARTESIAN_POINT ( 'NONE',  ( 10.30047009227000032, 4.027768540959000276, 9.431354536774000152 ) ) ;
#41567 = CARTESIAN_POINT ( 'NONE',  ( 12.09966954483535773, -3.361010663344000005, 8.485927942460499196 ) ) ;
#41568 = DIRECTION ( 'NONE',  ( 0.000000000000000000, 0.000000000000000000, -1.000000000000000000 ) ) ;
#41569 = CARTESIAN_POINT ( 'NONE',  ( 11.01765929220000118, 7.436533042258000492, -6.255518063588999311 ) ) ;
#41570 = CARTESIAN_POINT ( 'NONE',  ( 24.59232956327399933, 8.769507425530997935, 9.082531692484000274 ) ) ;
#41571 = CARTESIAN_POINT ( 'NONE',  ( 12.50079267818768614, -0.5460377805369048820, 12.68419612078310621 ) ) ;
#41572 = EDGE_CURVE ( 'NONE', #57358, #23058, #8991, .T. ) ;
#41573 = ADVANCED_FACE ( 'NONE', ( #30331 ), #51639, .F. ) ;
#41574 = FACE_OUTER_BOUND ( 'NONE', #51236, .T. ) ;
#41575 = CARTESIAN_POINT ( 'NONE',  ( 10.37873747135000002, 4.882725050998000249, 6.350806206758999650 ) ) ;
#41576 = CARTESIAN_POINT ( 'NONE',  ( 11.55275411606000269, -3.402594452619000176, 11.19752650018000040 ) ) ;
#41577 = ORIENTED_EDGE ( 'NONE', *, *, #16966, .T. ) ;
#41578 = CARTESIAN_POINT ( 'NONE',  ( 8.541054719591000932, 3.807713920470999991, -9.221758713517999695 ) ) ;
#41579 = CARTESIAN_POINT ( 'NONE',  ( -0.000000000000000000, -1.460960874861672476, 2.533832635912068643 ) ) ;
#41580 = DIRECTION ( 'NONE',  ( -1.000000000000000000, 0.000000000000000000, 0.000000000000000000 ) ) ;
#41581 = CARTESIAN_POINT ( 'NONE',  ( 9.167308658909917085, 5.079249101950133571, -8.329436424852559639 ) ) ;
#41582 = DIRECTION ( 'NONE',  ( -1.000000000000000000, 0.000000000000000000, 0.000000000000000000 ) ) ;
#41583 = CARTESIAN_POINT ( 'NONE',  ( 10.32949413291699869, -3.087070836781100169, -7.083453279150199400 ) ) ;
#41584 = ORIENTED_EDGE ( 'NONE', *, *, #23704, .T. ) ;
#41585 = VECTOR ( 'NONE', #60664, 1000.000000000000000 ) ;
#41586 = CARTESIAN_POINT ( 'NONE',  ( 1.534336868148000077, 3.729267013836000011, 0.4700476753697999666 ) ) ;
#41587 = CARTESIAN_POINT ( 'NONE',  ( 7.629823341228000544, 4.763536573491999881, 5.668879554882000349 ) ) ;
#41590 = LINE ( 'NONE', #15367, #58857 ) ;
#41589 = CARTESIAN_POINT ( 'NONE',  ( 9.792620004638278530, 4.710589479228226573, 9.124905218709104204 ) ) ;
#41588 = PRODUCT_DEFINITION_CONTEXT ( 'detailed design', #45855, 'design' ) ;
#41591 = CARTESIAN_POINT ( 'NONE',  ( 18.16751419062931205, -2.624553509083156211, 13.64625295323315513 ) ) ;
#41592 = VERTEX_POINT ( 'NONE', #16298 ) ;
#41593 = FACE_OUTER_BOUND ( 'NONE', #26824, .T. ) ;
#41594 = CARTESIAN_POINT ( 'NONE',  ( 18.16363222863429172, -2.642680409073418168, -13.64211442534931784 ) ) ;
#41595 = CARTESIAN_POINT ( 'NONE',  ( 11.24441369783139777, 3.956299011112040187, 6.634905315059499209 ) ) ;
#41596 = CARTESIAN_POINT ( 'NONE',  ( 11.09999999999999964, -2.685305999535000154, 6.664030027596000494 ) ) ;
#41597 = CARTESIAN_POINT ( 'NONE',  ( 8.181105646794000208, -5.485781663882000281, 8.532068390166999805 ) ) ;
#41598 = ORIENTED_EDGE ( 'NONE', *, *, #18707, .T. ) ;
#41599 = CARTESIAN_POINT ( 'NONE',  ( 8.443892219592001425, 2.905861847853000057, 8.940690431604000565 ) ) ;
#41600 = ADVANCED_FACE ( 'NONE', ( #54396 ), #5888, .T. ) ;
#41602 = CARTESIAN_POINT ( 'NONE',  ( 10.68343305961999867, -3.810133104029999718, -5.661126601970999594 ) ) ;
#41601 = CARTESIAN_POINT ( 'NONE',  ( 10.31652245563454073, 4.682420780414363826, -8.028218637173727856 ) ) ;
#41603 = CARTESIAN_POINT ( 'NONE',  ( 7.575399445029316503, -4.029967771855843317, 5.761070296328433038 ) ) ;
#41604 = CIRCLE ( 'NONE', #5859, 2.000000000000001332 ) ;
#41605 = CARTESIAN_POINT ( 'NONE',  ( 7.930984152288867328, -5.149131075244117284, 6.790530796032830274 ) ) ;
#41606 = DIRECTION ( 'NONE',  ( -1.000000000000000000, 0.000000000000000000, 0.000000000000000000 ) ) ;
#41607 = ORIENTED_EDGE ( 'NONE', *, *, #61029, .T. ) ;
#41608 = DIRECTION ( 'NONE',  ( 0.000000000000000000, 1.000000000000000000, 0.000000000000000000 ) ) ;
#41609 = EDGE_CURVE ( 'NONE', #18530, #16538, #10707, .T. ) ;
#41610 = CARTESIAN_POINT ( 'NONE',  ( 10.78441772631200024, -3.627481539113199815, 6.733203680593099705 ) ) ;
#41611 = CARTESIAN_POINT ( 'NONE',  ( 9.533434135307000901, 2.564753581125000181, 6.150586364588000343 ) ) ;
#41612 = CARTESIAN_POINT ( 'NONE',  ( 10.57892463485000079, 4.649960478797999563, 5.681084732956000138 ) ) ;
#41613 = CARTESIAN_POINT ( 'NONE',  ( 11.70379573085659786, 5.106255642043000087, 7.308581953418300081 ) ) ;
#41614 = CARTESIAN_POINT ( 'NONE',  ( 17.33333333127366771, -3.351260669886449772, -11.15757822838323499 ) ) ;
#41615 = CARTESIAN_POINT ( 'NONE',  ( 18.36021383542241736, 3.331512994329992150, -12.07398673550631329 ) ) ;
#41616 = CARTESIAN_POINT ( 'NONE',  ( 12.21202437720818601, -2.301604982168444558, 12.49562318899339708 ) ) ;
#41617 = CARTESIAN_POINT ( 'NONE',  ( 11.00270877634999955, 2.832878561424999830, -4.969257129766999626 ) ) ;
#41618 = CARTESIAN_POINT ( 'NONE',  ( 17.87817017025377098, -1.864246049947076100, 13.87532391830906597 ) ) ;
#41619 = DIRECTION ( 'NONE',  ( 0.000000000000000000, 0.000000000000000000, -1.000000000000000000 ) ) ;
#41620 = ORIENTED_EDGE ( 'NONE', *, *, #13887, .F. ) ;
#41621 = CARTESIAN_POINT ( 'NONE',  ( 1.700000000000000178, -2.149999999999999911, 0.000000000000000000 ) ) ;
#41622 = CARTESIAN_POINT ( 'NONE',  ( 13.49994651945300284, -12.07042783918999795, -2.492331243371999960 ) ) ;
#41623 = ORIENTED_EDGE ( 'NONE', *, *, #15075, .F. ) ;
#41624 = CARTESIAN_POINT ( 'NONE',  ( 8.214872450534432602, 2.885034184131826329, 6.708591157435166430 ) ) ;
#41625 = ADVANCED_FACE ( 'NONE', ( #27845 ), #42876, .F. ) ;
#41626 = CARTESIAN_POINT ( 'NONE',  ( 10.57980110216399972, 3.260758259645400337, 7.951464549725199227 ) ) ;
#41627 = CARTESIAN_POINT ( 'NONE',  ( 10.34520858566999912, 2.724123081339000052, 6.497325124886000225 ) ) ;
#41628 = CARTESIAN_POINT ( 'NONE',  ( 10.78637067803999905, 5.666041748529999644, -7.787005432561999285 ) ) ;
#41629 = CARTESIAN_POINT ( 'NONE',  ( 9.581508192411627434, -4.779998216922380472, -7.103597363128174358 ) ) ;
#41630 = CARTESIAN_POINT ( 'NONE',  ( 10.83659005484000026, -5.133183563847000030, 8.848364935581999546 ) ) ;
#41631 = CARTESIAN_POINT ( 'NONE',  ( 18.02418542278644509, 0.5485298171726687988, -12.58805670501782359 ) ) ;
#41632 = CARTESIAN_POINT ( 'NONE',  ( 10.90000000000000036, -0.2999999999999999889, 4.902439024389999567 ) ) ;
#41633 = CARTESIAN_POINT ( 'NONE',  ( 11.58071932425156980, -4.167269912168199753, -8.628410767520000135 ) ) ;
#41634 = CARTESIAN_POINT ( 'NONE',  ( 10.90000000346999975, -5.100000000044000892, -5.157071296039999808 ) ) ;
#41635 = ORIENTED_EDGE ( 'NONE', *, *, #16275, .T. ) ;
#41636 = AXIS2_PLACEMENT_3D ( 'NONE', #24794, #14313, #18868 ) ;
#41637 =( NAMED_UNIT ( * ) SI_UNIT ( $, .STERADIAN. ) SOLID_ANGLE_UNIT ( ) );
#41638 = CARTESIAN_POINT ( 'NONE',  ( 25.22250851510596448, -2.724056651873135060, 11.39870813624705370 ) ) ;
#41639 = DIRECTION ( 'NONE',  ( 0.000000000000000000, 2.692747184616903860E-07, -0.9999999999999636957 ) ) ;
#41640 = CARTESIAN_POINT ( 'NONE',  ( 11.79999999471800010, -11.69117318561000118, -1.923227876431999883 ) ) ;
#41641 = CARTESIAN_POINT ( 'NONE',  ( 8.857252140395999618, 8.766943526461002278, 6.126566717276006102 ) ) ;
#41642 = CARTESIAN_POINT ( 'NONE',  ( 12.48178274919584752, 3.171647819517038336, 13.63600670097293843 ) ) ;
#41643 = CARTESIAN_POINT ( 'NONE',  ( 9.854949224988001077, -2.800315695760000168, 9.013807298610000629 ) ) ;
#41644 = CARTESIAN_POINT ( 'NONE',  ( 21.72233714749290101, 0.000000000000000000, 0.000000000000000000 ) ) ;
#41645 = CARTESIAN_POINT ( 'NONE',  ( 12.09897931881621425, -0.1662062226620466543, 13.99901824074930978 ) ) ;
#41646 = ORIENTED_EDGE ( 'NONE', *, *, #27187, .T. ) ;
#41647 = CARTESIAN_POINT ( 'NONE',  ( 12.37951367597797159, -1.897619119404206467, 12.45628731554757351 ) ) ;
#41648 = CARTESIAN_POINT ( 'NONE',  ( 12.80505043854143388, 1.787816316115912185, -13.88537766212463254 ) ) ;
#41649 = CARTESIAN_POINT ( 'NONE',  ( 11.18051369187999988, -5.340070732632000272, 8.416150632189001612 ) ) ;
#41650 = CARTESIAN_POINT ( 'NONE',  ( 15.75060268748879366, 9.413968701426712826, 8.261605506250123909 ) ) ;
#41651 = CARTESIAN_POINT ( 'NONE',  ( 10.90749413291699987, -3.211956830789300277, 7.859564368461399830 ) ) ;
#41652 = VECTOR ( 'NONE', #19779, 999.9999999999998863 ) ;
#41653 = CARTESIAN_POINT ( 'NONE',  ( 12.13082219998073974, 0.2646961475753737414, 12.59722401988189411 ) ) ;
#41654 = EDGE_CURVE ( 'NONE', #35162, #37966, #59642, .T. ) ;
#41655 = EDGE_CURVE ( 'NONE', #68830, #49271, #43919, .T. ) ;
#41656 = CARTESIAN_POINT ( 'NONE',  ( 0.6474295521082999993, 2.420060471650000267, -2.350339292168000416 ) ) ;
#41657 = CARTESIAN_POINT ( 'NONE',  ( 7.945608795480783471, 5.314576234847344871, 7.853946780411420470 ) ) ;
#41658 = CARTESIAN_POINT ( 'NONE',  ( 12.37879419969803685, 1.897860824706880889, 12.45625557883629853 ) ) ;
#41659 = CARTESIAN_POINT ( 'NONE',  ( 9.191972128127998687, -4.867164667115999599, -6.095483598963999938 ) ) ;
#41660 = ADVANCED_FACE ( 'NONE', ( #54050 ), #69097, .F. ) ;
#41661 = CARTESIAN_POINT ( 'NONE',  ( 11.14179841651039915, 3.646693590264900031, -8.439215328713499886 ) ) ;
#41662 = DIRECTION ( 'NONE',  ( -0.7071068341558115478, 0.000000000000000000, -0.7071067282172794899 ) ) ;
#41663 = CARTESIAN_POINT ( 'NONE',  ( 10.34266415877000078, 5.750490533313000086, -8.094415907623000450 ) ) ;
#41664 = CARTESIAN_POINT ( 'NONE',  ( 8.820101285864000218, 3.176316400316700150, -6.521261160937499746 ) ) ;
#41666 = CYLINDRICAL_SURFACE ( 'NONE', #66328, 1.500000000000000000 ) ;
#41665 = CARTESIAN_POINT ( 'NONE',  ( 5.500000000000000000, -6.661338147750999827E-14, -1.931788062847999572E-14 ) ) ;
#41667 = CARTESIAN_POINT ( 'NONE',  ( 11.11486084871780022, -2.792989229543000107, -7.174999999999999822 ) ) ;
#41668 = ORIENTED_EDGE ( 'NONE', *, *, #49386, .T. ) ;
#41669 = CARTESIAN_POINT ( 'NONE',  ( 12.64392860550861819, -0.6042188441982559999, 12.68064732209123946 ) ) ;
#41670 = CARTESIAN_POINT ( 'NONE',  ( 10.38351354018329253, 2.750000000000000000, 7.663624617374469317 ) ) ;
#41671 = CARTESIAN_POINT ( 'NONE',  ( 9.261668853699999815, -2.944250413017999612, 6.507387951280999339 ) ) ;
#41672 = CARTESIAN_POINT ( 'NONE',  ( 8.869809814040998219, 4.614409247670200109, 6.705428891605899722 ) ) ;
#41673 = CARTESIAN_POINT ( 'NONE',  ( 11.29998658800000122, 3.824194713071000340, -11.71675648045999907 ) ) ;
#41674 = CARTESIAN_POINT ( 'NONE',  ( 12.33243540359738866, -2.090896859126742502, 13.75176201293517408 ) ) ;
#41675 = CARTESIAN_POINT ( 'NONE',  ( 12.47652830181506012, 1.943388387788944405, 13.77651117150486115 ) ) ;
#41676 = CARTESIAN_POINT ( 'NONE',  ( 23.81907629691099970, 3.247310101920000136, -13.04146647203000065 ) ) ;
#41677 = ORIENTED_EDGE ( 'NONE', *, *, #4774, .T. ) ;
#41678 = AXIS2_PLACEMENT_3D ( 'NONE', #17290, #37240, #16934 ) ;
#41679 = CARTESIAN_POINT ( 'NONE',  ( 4.729580014212999117, -0.4240496150661999808, 1.052182387563999955 ) ) ;
#41680 = CARTESIAN_POINT ( 'NONE',  ( 8.617468108405999416, -2.769196120524999749, -7.848577323721800170 ) ) ;
#41681 = AXIS2_PLACEMENT_3D ( 'NONE', #62637, #52152, #8227 ) ;
#41682 = CARTESIAN_POINT ( 'NONE',  ( 10.90454231406000041, -5.099691312770999296, -5.130383474399000221 ) ) ;
#41683 = CARTESIAN_POINT ( 'NONE',  ( 10.85814141025499957, -3.516507310755200066, 6.638851159159999682 ) ) ;
#41684 = CARTESIAN_POINT ( 'NONE',  ( 17.84275129854000852, 3.054939169952809230, -12.30480372676524858 ) ) ;
#41685 = CARTESIAN_POINT ( 'NONE',  ( 10.95904654087999930, -2.844192924580000170, 5.123817848908000627 ) ) ;
#41686 = CARTESIAN_POINT ( 'NONE',  ( 18.18003600477297610, 2.504879791473498596, 12.45042248975033061 ) ) ;
#41687 = CARTESIAN_POINT ( 'NONE',  ( 18.20500217920490016, 2.141655701468109019, 13.83591107702473266 ) ) ;
#41688 = CARTESIAN_POINT ( 'NONE',  ( 11.50000000000000000, -5.058572498595999889, 7.174999999999999822 ) ) ;
#41689 = CARTESIAN_POINT ( 'NONE',  ( 11.19050685320999960, -2.516759970060999940, -6.840363309917000478 ) ) ;
#41690 = CARTESIAN_POINT ( 'NONE',  ( 9.028474612548734513, -4.352782978231400257, 8.850949115404409540 ) ) ;
#41691 = CARTESIAN_POINT ( 'NONE',  ( 12.10478902330476281, 0.1895042076700467759, -13.99872220539657519 ) ) ;
#41692 = CARTESIAN_POINT ( 'NONE',  ( 23.56684398259831781, 13.33616302248389118, 4.226923696159335719 ) ) ;
#41693 = DIRECTION ( 'NONE',  ( -0.7071060218675399023, 0.7071075405047398954, -8.464089693328477533E-10 ) ) ;
#41694 = CARTESIAN_POINT ( 'NONE',  ( 2.427569202129625126, 2.124261041935756378, -2.802062795322278532 ) ) ;
#41695 = ORIENTED_EDGE ( 'NONE', *, *, #1566, .T. ) ;
#41696 = CARTESIAN_POINT ( 'NONE',  ( 9.012204719595001023, 3.161445734422999809, -6.178649910536000434 ) ) ;
#41698 = AXIS2_PLACEMENT_3D ( 'NONE', #16342, #32095, #58998 ) ;
#41697 = CARTESIAN_POINT ( 'NONE',  ( 11.12903166480609940, -4.864052766304100217, 7.439078678739090122 ) ) ;
#41699 = VERTEX_POINT ( 'NONE', #47788 ) ;
#41700 = FACE_OUTER_BOUND ( 'NONE', #9643, .T. ) ;
#41702 = CARTESIAN_POINT ( 'NONE',  ( 18.21576355877873965, 2.818661318639662294, -13.71332454644887555 ) ) ;
#41701 = B_SPLINE_CURVE_WITH_KNOTS ( 'NONE', 3,
 ( #69181, #17071, #58695, #32144 ),
 .UNSPECIFIED., .F., .F.,
 ( 4, 4 ),
 ( 0.000000000000000000, 1.000000000000000000 ),
 .UNSPECIFIED. ) ;
#41704 = ORIENTED_EDGE ( 'NONE', *, *, #16995, .T. ) ;
#41703 = B_SPLINE_CURVE_WITH_KNOTS ( 'NONE', 3,
 ( #38489, #55267, #54217, #65743, #28705, #48982 ),
 .UNSPECIFIED., .F., .F.,
 ( 4, 2, 4 ),
 ( 0.000000000000000000, 0.5000000000000000000, 1.000000000000000000 ),
 .UNSPECIFIED. ) ;
#41705 = CARTESIAN_POINT ( 'NONE',  ( 11.47500581613029880, 4.988618570924500339, 6.865182626353099948 ) ) ;
#41706 = EDGE_CURVE ( 'NONE', #63863, #31118, #15930, .T. ) ;
#41708 = CARTESIAN_POINT ( 'NONE',  ( 9.243110841233001196, 4.112741311853999271, -5.603466076760000192 ) ) ;
#41707 = AXIS2_PLACEMENT_3D ( 'NONE', #68448, #41895, #14982 ) ;
#41709 = CARTESIAN_POINT ( 'NONE',  ( 9.709999999999999076, 4.496968146123999865, -8.755198255949000696 ) ) ;
#41710 = FACE_OUTER_BOUND ( 'NONE', #14760, .T. ) ;
#41711 = DIRECTION ( 'NONE',  ( 1.000000000000000000, 0.000000000000000000, 2.662749306050999794E-14 ) ) ;
#41712 = EDGE_CURVE ( 'NONE', #54437, #59964, #17067, .T. ) ;
#41713 = CARTESIAN_POINT ( 'NONE',  ( 11.09999999999999964, -7.940796613052000019, 6.945951997396999644 ) ) ;
#41714 = ORIENTED_EDGE ( 'NONE', *, *, #20144, .F. ) ;
#41715 = FACE_OUTER_BOUND ( 'NONE', #41127, .T. ) ;
#41716 = CARTESIAN_POINT ( 'NONE',  ( 9.535554719593998030, 3.927090956378999742, -9.230892435423001530 ) ) ;
#41717 = ORIENTED_EDGE ( 'NONE', *, *, #6943, .F. ) ;
#41718 = CARTESIAN_POINT ( 'NONE',  ( 9.922184613163000932, 3.489926301007000298, -9.111807643819000546 ) ) ;
#41719 = VERTEX_POINT ( 'NONE', #48467 ) ;
#41720 = CARTESIAN_POINT ( 'NONE',  ( 9.883925467520999320, 2.723846966067000164, 7.588418444866789514 ) ) ;
#41721 = CARTESIAN_POINT ( 'NONE',  ( 17.80610932905897315, -1.927548246225502249, -12.56666212246289405 ) ) ;
#41722 = CARTESIAN_POINT ( 'NONE',  ( 11.53970701685000222, -11.52114570934000071, -1.450082077858000140 ) ) ;
#41723 = CARTESIAN_POINT ( 'NONE',  ( 18.15926133227551631, -2.338854968149422842, -12.48766092793498217 ) ) ;
#41724 = CARTESIAN_POINT ( 'NONE',  ( 10.40583502355000078, -8.253917379314000158, -6.947659401770000187 ) ) ;
#41725 = VERTEX_POINT ( 'NONE', #64870 ) ;
#41726 = CARTESIAN_POINT ( 'NONE',  ( 11.91753023736700179, 11.77475711121000224, -4.379243463657999769 ) ) ;
#41727 = CARTESIAN_POINT ( 'NONE',  ( 8.716308103597052437, 4.026268495047269802, -5.729473523615199682 ) ) ;
#41728 = CARTESIAN_POINT ( 'NONE',  ( 17.79999999998900151, -3.595165934733000057, 11.99793354950999991 ) ) ;
#41729 = DIRECTION ( 'NONE',  ( -1.000000000000000000, 0.000000000000000000, 0.000000000000000000 ) ) ;
#41730 = AXIS2_PLACEMENT_3D ( 'NONE', #11802, #10768, #64588 ) ;
#41731 = CARTESIAN_POINT ( 'NONE',  ( 18.27544000105304534, -0.08309727575450792658, 13.99975851644561864 ) ) ;
#41732 = CARTESIAN_POINT ( 'NONE',  ( 18.31802873821099809, 2.927761598026000112, 11.42873208727000112 ) ) ;
#41733 = CARTESIAN_POINT ( 'NONE',  ( 10.25166529434999951, -3.418639857622999934, -8.733652610425998830 ) ) ;
#41734 = B_SPLINE_CURVE_WITH_KNOTS ( 'NONE', 3,
 ( #68947, #21060, #46608, #52876 ),
 .UNSPECIFIED., .F., .F.,
 ( 4, 4 ),
 ( 0.000000000000000000, 1.000000000000000000 ),
 .UNSPECIFIED. ) ;
#41735 = ADVANCED_FACE ( 'NONE', ( #22233 ), #53903, .T. ) ;
#41736 = ORIENTED_EDGE ( 'NONE', *, *, #44866, .T. ) ;
#41737 = ORIENTED_EDGE ( 'NONE', *, *, #51225, .F. ) ;
#41738 = CARTESIAN_POINT ( 'NONE',  ( 9.626145280412998773, 3.934138271021000222, -9.063586117809000697 ) ) ;
#41739 = CARTESIAN_POINT ( 'NONE',  ( 10.66052890781999984, 2.899999999999999911, -6.152188490330000370 ) ) ;
#41740 = ADVANCED_FACE ( 'NONE', ( #32053 ), #6147, .T. ) ;
#41741 = ADVANCED_FACE ( 'NONE', ( #63841 ), #15955, .T. ) ;
#41742 = CARTESIAN_POINT ( 'NONE',  ( 12.35418469966212562, -2.932966736140843800, 13.57204261866825235 ) ) ;
#41743 = CARTESIAN_POINT ( 'NONE',  ( 24.74066795589899925, 8.629132841860998937, -8.723415954201001909 ) ) ;
#41744 = CARTESIAN_POINT ( 'NONE',  ( 11.05851190073833301, 5.258511900738333189, 6.537362761296000357 ) ) ;
#41745 = CARTESIAN_POINT ( 'NONE',  ( 10.14325461470300027, 3.159754091322399816, -7.713763321667399531 ) ) ;
#41747 = FACE_OUTER_BOUND ( 'NONE', #97, .T. ) ;
#41746 = CARTESIAN_POINT ( 'NONE',  ( 9.380265421555000316, -4.214287043487900064, 6.391527115138999626 ) ) ;
#41748 = VECTOR ( 'NONE', #62140, 999.9999999999998863 ) ;
#41749 = CARTESIAN_POINT ( 'NONE',  ( 4.752943173016667799, 1.199500263597271577, -0.9218200799623702535 ) ) ;
#41750 = ORIENTED_EDGE ( 'NONE', *, *, #27138, .T. ) ;
#41751 = CARTESIAN_POINT ( 'NONE',  ( 25.29995734509200034, 8.533537492639000632, -7.925519463018001254 ) ) ;
#41752 = AXIS2_PLACEMENT_3D ( 'NONE', #8379, #51025, #18870 ) ;
#41753 = CARTESIAN_POINT ( 'NONE',  ( 7.782404085375001834, -2.843788791114000958, 6.809963588862000705 ) ) ;
#41754 = CARTESIAN_POINT ( 'NONE',  ( 10.31759632033899976, 2.815618218644000414, 7.983346856269500691 ) ) ;
#41755 = CARTESIAN_POINT ( 'NONE',  ( 7.945227163831277473, 5.100007011413144831, 6.648088212574772449 ) ) ;
#41756 = CARTESIAN_POINT ( 'NONE',  ( 10.65050275296000137, -5.200029647236999786, 5.937716681140000397 ) ) ;
#41757 = LINE ( 'NONE', #15185, #57558 ) ;
#41758 = CARTESIAN_POINT ( 'NONE',  ( 15.95436146409600120, -3.609635682399999546, -11.22945631340000006 ) ) ;
#41759 = EDGE_CURVE ( 'NONE', #60364, #33864, #66024, .T. ) ;
#41760 = CARTESIAN_POINT ( 'NONE',  ( 13.55436146409600262, 9.071829816454000550, 7.538704307477999578 ) ) ;
#41761 = CARTESIAN_POINT ( 'NONE',  ( 7.965310626361219448, 2.964115357972241238, -6.528796737864926314 ) ) ;
#41762 = CARTESIAN_POINT ( 'NONE',  ( 6.362045118933999710, -1.113463867511000238, -0.3786539577593999728 ) ) ;
#41763 = CARTESIAN_POINT ( 'NONE',  ( 18.49996808500599954, 1.807259460122252470, -11.54438823565103789 ) ) ;
#41764 = CARTESIAN_POINT ( 'NONE',  ( 23.60000000000000142, -11.85420044612000012, 3.901016762742000488 ) ) ;
#41765 = CARTESIAN_POINT ( 'NONE',  ( 3.019656859288000206, -2.470837861336999897, -2.372715509949999912 ) ) ;
#41766 = ORIENTED_EDGE ( 'NONE', *, *, #17050, .F. ) ;
#41767 = CARTESIAN_POINT ( 'NONE',  ( 12.57501510860068272, 0.5812174491462186454, -12.68209204657794231 ) ) ;
#41768 = CARTESIAN_POINT ( 'NONE',  ( 12.19254223304418083, -2.624341220734839109, -12.42172529697063865 ) ) ;
#41769 = DIRECTION ( 'NONE',  ( 1.000000000000000000, 0.000000000000000000, 0.000000000000000000 ) ) ;
#41770 = CARTESIAN_POINT ( 'NONE',  ( 3.500000000000000000, 1.113524292603000010, -3.231029921506000324 ) ) ;
#41771 = CARTESIAN_POINT ( 'NONE',  ( 10.29214449041363366, 3.170483834885991836, -8.579383242754643035 ) ) ;
#41772 = ORIENTED_EDGE ( 'NONE', *, *, #40314, .F. ) ;
#41773 = CARTESIAN_POINT ( 'NONE',  ( 5.442721112194999655, -0.09407552946282000950, -1.172318398388999983 ) ) ;
#41774 = CARTESIAN_POINT ( 'NONE',  ( 0.6675864513507200337, -1.750409042682265159, 3.065373999385508252 ) ) ;
#41775 = CARTESIAN_POINT ( 'NONE',  ( 13.46001156276200028, -11.65487838447000080, -2.352687191044000148 ) ) ;
#41776 = CARTESIAN_POINT ( 'NONE',  ( 7.698725635631044284, 3.848229261580326188, -8.856856640736939568 ) ) ;
#41777 = CARTESIAN_POINT ( 'NONE',  ( 11.30878751119029957, 2.958974835389999836, -8.044634158732998586 ) ) ;
#41778 = ORIENTED_EDGE ( 'NONE', *, *, #42234, .F. ) ;
#41779 = VECTOR ( 'NONE', #57135, 1000.000000000000000 ) ;
#41780 = CARTESIAN_POINT ( 'NONE',  ( 10.66951732929000052, -4.592671928130000580, 5.841406818427000047 ) ) ;
#41781 = EDGE_LOOP ( 'NONE', ( #25982, #64120, #47473, #15910 ) ) ;
#41782 = CARTESIAN_POINT ( 'NONE',  ( 8.501777870119797242, -3.152918059059234945, 6.042693032664300468 ) ) ;
#41783 = CARTESIAN_POINT ( 'NONE',  ( 9.475897313459000770, -4.122021308488999836, 9.013573548576999883 ) ) ;
#41784 = EDGE_CURVE ( 'NONE', #26661, #13504, #23772, .T. ) ;
#41785 = CARTESIAN_POINT ( 'NONE',  ( 15.67439970770000102, 8.782357275181000844, 8.013525452821999906 ) ) ;
#41786 = EDGE_LOOP ( 'NONE', ( #23476, #44720, #53736, #42066 ) ) ;
#41787 = CARTESIAN_POINT ( 'NONE',  ( 23.57822756410993748, 10.24958405627187119, 9.515671483802911723 ) ) ;
#41788 = CARTESIAN_POINT ( 'NONE',  ( 7.976241301082664492, 3.766713024421330047, -6.157346639817824041 ) ) ;
#41789 = CARTESIAN_POINT ( 'NONE',  ( 6.935229719590999764, 2.436157974829999961, -7.440523950196999969 ) ) ;
#41790 = EDGE_CURVE ( 'NONE', #53272, #67920, #21885, .T. ) ;
#41791 = CARTESIAN_POINT ( 'NONE',  ( 9.521013540183334456, -3.231816600031356845, -8.499583552997725278 ) ) ;
#41792 = CARTESIAN_POINT ( 'NONE',  ( 24.44496351116800170, 3.224881296174999967, 12.03535797436000010 ) ) ;
#41793 = VERTEX_POINT ( 'NONE', #38314 ) ;
#41794 = CARTESIAN_POINT ( 'NONE',  ( 10.93227479887999998, -2.539880901735999785, 6.453614191797999666 ) ) ;
#41795 = CARTESIAN_POINT ( 'NONE',  ( 12.47652830184861372, -1.943388387755060398, -13.77651117150767668 ) ) ;
#41796 = CARTESIAN_POINT ( 'NONE',  ( 9.405196823546312146, -3.391797362091467427, 6.627513167511573045 ) ) ;
#41797 = ORIENTED_EDGE ( 'NONE', *, *, #18365, .F. ) ;
#41798 = CARTESIAN_POINT ( 'NONE',  ( 9.051550650638001017, 2.899999999999999911, 6.227445478845999638 ) ) ;
#41799 = VECTOR ( 'NONE', #42846, 1000.000000000000000 ) ;
#41800 = DIRECTION ( 'NONE',  ( -0.9999999999988525845, -7.523236327271644932E-07, 1.314847452163938853E-06 ) ) ;
#41801 = ORIENTED_EDGE ( 'NONE', *, *, #3768, .T. ) ;
#41802 = LINE ( 'NONE', #16258, #42078 ) ;
#41803 = CARTESIAN_POINT ( 'NONE',  ( 17.86532676353943572, 0.5429298016611214805, -13.88573085157339726 ) ) ;
#41804 = CARTESIAN_POINT ( 'NONE',  ( 5.171704601181000172, -0.2775142444059999769, -1.532592734373000143 ) ) ;
#41805 = AXIS2_PLACEMENT_3D ( 'NONE', #22173, #32676, #5062 ) ;
#41806 = CARTESIAN_POINT ( 'NONE',  ( 11.59999999999999964, -2.750000000000000000, -7.500000000000000000 ) ) ;
#41807 = DIRECTION ( 'NONE',  ( 1.000000000000000000, 0.000000000000000000, 0.000000000000000000 ) ) ;
#41808 = CARTESIAN_POINT ( 'NONE',  ( 12.80505043854143388, 3.199751711897557804, -12.18694338143115630 ) ) ;
#41809 = CARTESIAN_POINT ( 'NONE',  ( 10.34947173981000113, -4.457565973839000328, 6.154866550070000386 ) ) ;
#41810 = ORIENTED_EDGE ( 'NONE', *, *, #39670, .F. ) ;
#41811 = CARTESIAN_POINT ( 'NONE',  ( 7.913666363270997373, -4.616745235331003450, 6.306613118563004328 ) ) ;
#41812 = EDGE_LOOP ( 'NONE', ( #43522, #63440, #27528, #38663, #23394 ) ) ;
#41813 = CARTESIAN_POINT ( 'NONE',  ( 11.09647882763000126, 3.099775370665000196, 6.097099813297999660 ) ) ;
#41814 = CARTESIAN_POINT ( 'NONE',  ( 7.000000000000000000, 0.8000000000000000444, 3.149999999999999911 ) ) ;
#41815 = CARTESIAN_POINT ( 'NONE',  ( 9.120035841232999374, 5.288433695693000480, -8.041290150997999930 ) ) ;
#41816 = CARTESIAN_POINT ( 'NONE',  ( 2.684339845264999802, -1.577989888572000066, 3.355529501073999832 ) ) ;
#41817 = CARTESIAN_POINT ( 'NONE',  ( 25.57779276387900325, 2.768488786735999962, 11.23374265755999879 ) ) ;
#41818 = LINE ( 'NONE', #25051, #23871 ) ;
#41819 = CARTESIAN_POINT ( 'NONE',  ( 13.70003001321900449, -12.06139972930709447, -3.524828382075537725 ) ) ;
#41820 = ORIENTED_EDGE ( 'NONE', *, *, #64544, .F. ) ;
#41821 = CARTESIAN_POINT ( 'NONE',  ( 12.50370260266017830, 0.5476489826676945727, 13.88547809940294719 ) ) ;
#41822 = CARTESIAN_POINT ( 'NONE',  ( 10.96887750876899936, -4.692271380433699512, 6.425720373262999274 ) ) ;
#41823 = CARTESIAN_POINT ( 'NONE',  ( 11.09999987043000047, 10.03015713885000082, 5.726993666320999488 ) ) ;
#41824 = EDGE_CURVE ( 'NONE', #15838, #47311, #11739, .T. ) ;
#41825 = DIRECTION ( 'NONE',  ( -1.000000000000000000, 0.000000000000000000, 0.000000000000000000 ) ) ;
#41826 = CARTESIAN_POINT ( 'NONE',  ( 7.384456853207000293, -3.346260729029000291, 6.002247316312999459 ) ) ;
#41828 = CARTESIAN_POINT ( 'NONE',  ( 0.1500001264883999708, 2.724999873498000103, 2.408241100083999765E-10 ) ) ;
#41827 = CARTESIAN_POINT ( 'NONE',  ( 10.34520858566999912, 2.724123081339000052, 6.497325124886000225 ) ) ;
#41829 = VECTOR ( 'NONE', #13993, 1000.000000000000000 ) ;
#41830 = CARTESIAN_POINT ( 'NONE',  ( 11.28118179236249929, 3.732952383914999839, -6.250199235344999771 ) ) ;
#41831 = CARTESIAN_POINT ( 'NONE',  ( 25.57799114520100048, -11.11256384368000205, 3.219680944509000220 ) ) ;
#41832 = CARTESIAN_POINT ( 'NONE',  ( 9.982279731608999285, 4.077800926195140008, -6.636486849903699969 ) ) ;
#41833 = CARTESIAN_POINT ( 'NONE',  ( 18.24182894713846892, 0.2307628456012671414, 12.59789151516662997 ) ) ;
#41834 = CARTESIAN_POINT ( 'NONE',  ( 6.840948176613999898, -1.130182777988000042, -0.07094392349790000496 ) ) ;
#41835 = CARTESIAN_POINT ( 'NONE',  ( 11.22056920625029974, 4.047312782235129802, 8.815417147437999645 ) ) ;
#41836 = CARTESIAN_POINT ( 'NONE',  ( 9.286046699800502680, -3.154588942369298099, 7.038404655459764570 ) ) ;
#41837 = ORIENTED_EDGE ( 'NONE', *, *, #15796, .F. ) ;
#41838 = CARTESIAN_POINT ( 'NONE',  ( 7.486433059621999675, -5.321924421352999701, 8.118250081378000971 ) ) ;
#41839 = DIRECTION ( 'NONE',  ( 0.000000000000000000, -1.000000000000000000, 0.000000000000000000 ) ) ;
#41840 = EDGE_CURVE ( 'NONE', #57343, #23533, #31861, .T. ) ;
#41841 = CARTESIAN_POINT ( 'NONE',  ( 5.000030787343001215, -2.045306479342562156, -0.5496608443529855670 ) ) ;
#41842 = B_SPLINE_CURVE_WITH_KNOTS ( 'NONE', 3,
 ( #40355, #2944, #62697, #14482 ),
 .UNSPECIFIED., .F., .F.,
 ( 4, 4 ),
 ( 0.000000000000000000, 1.000000000000000000 ),
 .UNSPECIFIED. ) ;
#41843 = EDGE_LOOP ( 'NONE', ( #53129, #45669, #33133, #16006 ) ) ;
#41844 = PLANE ( 'NONE',  #21076 ) ;
#41845 = VECTOR ( 'NONE', #28050, 1000.000000000000000 ) ;
#41846 = CARTESIAN_POINT ( 'NONE',  ( 11.68788784977535933, 3.014014167207800465, 7.556342205905759890 ) ) ;
#41847 = CARTESIAN_POINT ( 'NONE',  ( 10.94033278040999946, 5.142729166069000435, -6.493505370358000128 ) ) ;
#41848 = ORIENTED_EDGE ( 'NONE', *, *, #14099, .T. ) ;
#41849 = CARTESIAN_POINT ( 'NONE',  ( 9.164757945270768147, 5.217425660116048469, -7.172825509854747317 ) ) ;
#41850 = CARTESIAN_POINT ( 'NONE',  ( 8.610875063856999745, 4.757997781751000410, 5.934102420827000124 ) ) ;
#41851 = CARTESIAN_POINT ( 'NONE',  ( 10.93656785386839836, 2.939720539848000413, 6.786470850652599474 ) ) ;
#41852 = FACE_OUTER_BOUND ( 'NONE', #41522, .T. ) ;
#41853 = CARTESIAN_POINT ( 'NONE',  ( 8.592635841230999105, 3.856772556595000179, 5.521246073317000125 ) ) ;
#41854 = ORIENTED_EDGE ( 'NONE', *, *, #51321, .F. ) ;
#41855 = CARTESIAN_POINT ( 'NONE',  ( 11.50001496185000249, 12.52500000000000036, 0.000000000000000000 ) ) ;
#41856 = CARTESIAN_POINT ( 'NONE',  ( 25.29995873461299993, 11.13046969959000165, 3.427501705020000067 ) ) ;
#41857 = CIRCLE ( 'NONE', #15066, 1.249999999999999778 ) ;
#41858 = CARTESIAN_POINT ( 'NONE',  ( 8.177847774682394544, -5.688938049909738837, 7.046656128444472422 ) ) ;
#41859 = CARTESIAN_POINT ( 'NONE',  ( 9.347442991499999465, -4.071878040089889517, 8.639547276484998761 ) ) ;
#41860 = ORIENTED_EDGE ( 'NONE', *, *, #34550, .T. ) ;
#41861 = CARTESIAN_POINT ( 'NONE',  ( 16.32966272177200295, -3.529531741950000079, -11.96032165934999902 ) ) ;
#41862 = FACE_OUTER_BOUND ( 'NONE', #60193, .T. ) ;
#41863 = EDGE_LOOP ( 'NONE', ( #18039, #18874, #33828, #5270 ) ) ;
#41864 = CARTESIAN_POINT ( 'NONE',  ( 10.98768472639999949, 0.3876847264043000174, 4.945212061661000469 ) ) ;
#41865 = DIRECTION ( 'NONE',  ( 0.000000000000000000, -0.9659258262890756397, -0.2588190451024934280 ) ) ;
#41866 = EDGE_LOOP ( 'NONE', ( #265, #10615, #30544, #53337, #62812 ) ) ;
#41867 = CARTESIAN_POINT ( 'NONE',  ( 18.11117642456258992, 0.2854033456632677490, -13.89606078824646929 ) ) ;
#41868 = CARTESIAN_POINT ( 'NONE',  ( 9.800903104272999045, -2.772050158355999994, -8.125211791007998841 ) ) ;
#41869 = CARTESIAN_POINT ( 'NONE',  ( 11.59999999999999964, 4.000000000000000000, 7.500000000000000000 ) ) ;
#41870 = CARTESIAN_POINT ( 'NONE',  ( 11.55811496860034815, 5.045590851977999947, -6.964183526617899744 ) ) ;
#41871 = EDGE_CURVE ( 'NONE', #2693, #66715, #28526, .T. ) ;
#41872 = DIRECTION ( 'NONE',  ( 0.2392860387991979920, -0.9709491189736919603, -1.580732896240985235E-14 ) ) ;
#41873 = CARTESIAN_POINT ( 'NONE',  ( 8.700696199801130959, -5.750348757284029944, 7.524179667756733636 ) ) ;
#41874 = CARTESIAN_POINT ( 'NONE',  ( 12.05194988689359903, -3.419512757306400363, 6.361426117087999543 ) ) ;
#41875 = CARTESIAN_POINT ( 'NONE',  ( 7.758198341228000672, 5.797099724369999763, 8.340484548805999765 ) ) ;
#41876 = ORIENTED_EDGE ( 'NONE', *, *, #25647, .F. ) ;
#41877 = CARTESIAN_POINT ( 'NONE',  ( 9.385596873516666605, 2.907767014557175678, -8.129523725463620565 ) ) ;
#41878 = CARTESIAN_POINT ( 'NONE',  ( 11.53828694957233658, -3.690393262785353734, -8.735060943529678212 ) ) ;
#41879 = CARTESIAN_POINT ( 'NONE',  ( 4.699998537092440642, 2.033928548242059464E-13, 13.17499999999999893 ) ) ;
#41880 = ORIENTED_EDGE ( 'NONE', *, *, #56145, .F. ) ;
#41881 = B_SPLINE_SURFACE_WITH_KNOTS ( 'NONE', 3, 3, ( 
 ( #27881, #11779, #33120, #32092 ),
 ( #65609, #610, #44314, #65265 ),
 ( #6184, #38354, #16679, #11433 ),
 ( #21923, #17378, #38006, #59681 ),
 ( #37323, #6537, #42915, #5506 ),
 ( #54435, #26846, #38708, #53408 ),
 ( #22615, #64221, #21578, #6882 ),
 ( #37665, #58995, #33467, #54783 ),
 ( #11097, #58646, #43261, #10747 ),
 ( #28219, #27526, #49533, #59331 ) ),
 .UNSPECIFIED., .F., .F., .F.,
 ( 4, 1, 1, 1, 1, 1, 1, 4 ),
 ( 4, 4 ),
 ( 0.07203983506772999867, 0.1428571428570999946, 0.2857142857143000203, 0.4285714285713999594, 0.5714285714286000406, 0.7142857142856999797, 0.8571428571429000609, 0.9589780836993999635 ),
 ( -0.1900620218102000158, 1.190128522698000069 ),
 .UNSPECIFIED. ) ;
#41882 = CARTESIAN_POINT ( 'NONE',  ( 12.42261142450843536, -2.994360094170046338, -12.32252841079977834 ) ) ;
#41883 = COLOUR_RGB ( '', 0.08235294, 0.09019608, 0.10196078) ;
#41884 = CARTESIAN_POINT ( 'NONE',  ( 11.32777510966000634, 9.448502962084004864, -6.821781130533998372 ) ) ;
#41885 = CARTESIAN_POINT ( 'NONE',  ( 23.56666365135700403, -8.694246338465996260, 8.392498551259993889 ) ) ;
#41886 = CARTESIAN_POINT ( 'NONE',  ( 4.599999999999999645, -3.125000000000000000, -13.52078605991414761 ) ) ;
#41887 = CARTESIAN_POINT ( 'NONE',  ( 12.21869931586267732, -2.282676242266354016, -13.71712068105209958 ) ) ;
#41888 = B_SPLINE_CURVE_WITH_KNOTS ( 'NONE', 3,
 ( #36925, #20839, #5097, #42851 ),
 .UNSPECIFIED., .F., .F.,
 ( 4, 4 ),
 ( 0.000000000000000000, 1.000000000000000000 ),
 .UNSPECIFIED. ) ;
#41889 = CARTESIAN_POINT ( 'NONE',  ( 10.50595525820100029, -4.081787880721680750, -6.637672143048099827 ) ) ;
#41890 = CARTESIAN_POINT ( 'NONE',  ( 12.09999999999999964, -4.000000000000000000, 7.500000000000000000 ) ) ;
#41891 = CARTESIAN_POINT ( 'NONE',  ( 18.24165222613601500, -2.712088604378295464, 12.30466175173927290 ) ) ;
#41892 = VERTEX_POINT ( 'NONE', #49847 ) ;
#41893 = VERTEX_POINT ( 'NONE', #41336 ) ;
#41894 = DIRECTION ( 'NONE',  ( 0.000000000000000000, 1.000000000000000000, 0.000000000000000000 ) ) ;
#41895 = DIRECTION ( 'NONE',  ( 0.000000000000000000, -0.8660254037844288266, -0.5000000000000169864 ) ) ;
#41896 = CARTESIAN_POINT ( 'NONE',  ( 9.858847045824999711, 2.668090821818000169, -7.206973500459000093 ) ) ;
#41897 = DIRECTION ( 'NONE',  ( 0.000000000000000000, -1.000000000000000000, 0.000000000000000000 ) ) ;
#41898 = CIRCLE ( 'NONE', #57507, 1.999999999999999556 ) ;
#41899 = CARTESIAN_POINT ( 'NONE',  ( 17.82007478097245112, 3.066051200070172289, 12.30148382826351394 ) ) ;
#41900 = CARTESIAN_POINT ( 'NONE',  ( 16.26904166988085620, 3.216266637185321020, 11.40336119490550004 ) ) ;
#41901 = CARTESIAN_POINT ( 'NONE',  ( 10.68403803949000164, 5.436614310638000269, 8.578436083822998270 ) ) ;
#41902 = ORIENTED_EDGE ( 'NONE', *, *, #13284, .T. ) ;
#41903 = CARTESIAN_POINT ( 'NONE',  ( 8.615014049714954325, -5.084477605260944166, -6.679144390359880390 ) ) ;
#41904 = ADVANCED_FACE ( 'NONE', ( #13145 ), #66609, .T. ) ;
#41905 = ORIENTED_EDGE ( 'NONE', *, *, #9016, .T. ) ;
#41906 = CARTESIAN_POINT ( 'NONE',  ( 12.30770095535952358, -2.879049501765980956, 12.35516346652265263 ) ) ;
#41907 = EDGE_CURVE ( 'NONE', #4028, #20987, #37674, .T. ) ;
#41908 = CARTESIAN_POINT ( 'NONE',  ( 9.323721904869998411, -3.243980311826100138, -7.924431591189499358 ) ) ;
#41909 = CARTESIAN_POINT ( 'NONE',  ( 11.11504246380000005, 3.456610836627000083, 5.970339330302000036 ) ) ;
#41910 = CARTESIAN_POINT ( 'NONE',  ( 11.72567835872029995, -4.993948309075300074, 8.126439557340900066 ) ) ;
#41911 = CARTESIAN_POINT ( 'NONE',  ( 11.35400411985997948, -11.72677417300536362, -1.687001524046906287 ) ) ;
#41912 = CARTESIAN_POINT ( 'NONE',  ( 23.66004879239100234, 0.000000000000000000, 0.000000000000000000 ) ) ;
#41913 = B_SPLINE_CURVE_WITH_KNOTS ( 'NONE', 3,
 ( #49527, #44989, #60369, #40092 ),
 .UNSPECIFIED., .F., .F.,
 ( 4, 4 ),
 ( 0.000000000000000000, 1.000000000000000000 ),
 .UNSPECIFIED. ) ;
#41914 = CARTESIAN_POINT ( 'NONE',  ( 10.86272200990529946, 2.793294545435000220, -7.079074440652799893 ) ) ;
#41915 = CARTESIAN_POINT ( 'NONE',  ( 10.98988709139175945, 3.461087363048998444, -9.181105347514801451 ) ) ;
#41916 = CARTESIAN_POINT ( 'NONE',  ( 5.695281798977684495, -12.04221271193012477, -3.723442287066820899 ) ) ;
#41917 = CARTESIAN_POINT ( 'NONE',  ( 5.200000000000000178, -1.199999999999999956, 9.776630298829998011 ) ) ;
#41918 = CARTESIAN_POINT ( 'NONE',  ( 9.108369332021359455, -3.858817869685470470, 8.849160905739024585 ) ) ;
#41919 = ORIENTED_EDGE ( 'NONE', *, *, #56935, .T. ) ;
#41920 = CARTESIAN_POINT ( 'NONE',  ( 8.681370280410998674, 2.949305648881000330, -8.659807625323999503 ) ) ;
#41921 = CARTESIAN_POINT ( 'NONE',  ( -0.000000000000000000, -2.824745580908275766, 0.7586348975822421181 ) ) ;
#41922 = AXIS2_PLACEMENT_3D ( 'NONE', #35802, #30902, #67597 ) ;
#41923 = CARTESIAN_POINT ( 'NONE',  ( 9.174642513462172744, 2.649442673323004538, 7.499981897072118819 ) ) ;
#41924 = CARTESIAN_POINT ( 'NONE',  ( 3.385862838527417207, 0.4349489234253638981, -3.502725854251790505 ) ) ;
#41925 = ADVANCED_FACE ( 'NONE', ( #44623 ), #57655, .F. ) ;
#41926 = CARTESIAN_POINT ( 'NONE',  ( 12.10000000000000320, -3.812684744683585869, 8.553266857751333774 ) ) ;
#41927 = CARTESIAN_POINT ( 'NONE',  ( 11.43302763632549990, -5.035790660926999784, -7.022058766158599141 ) ) ;
#41928 = ORIENTED_EDGE ( 'NONE', *, *, #22329, .T. ) ;
#41929 = VECTOR ( 'NONE', #18518, 1000.000000000000000 ) ;
#41930 = CARTESIAN_POINT ( 'NONE',  ( 9.099999931440999390, 4.000000000000000000, 7.500000000000000000 ) ) ;
#41931 = ADVANCED_FACE ( 'NONE', ( #60338 ), #39359, .F. ) ;
#41932 = CARTESIAN_POINT ( 'NONE',  ( 8.335885841230000537, 4.310355144869000732, 9.459505265942000918 ) ) ;
#41934 = CARTESIAN_POINT ( 'NONE',  ( 13.89309513285500230, -9.135233488911998379, -8.214486393748998694 ) ) ;
#41933 = CARTESIAN_POINT ( 'NONE',  ( 9.369139158774000720, 2.685250982074999904, -7.026194612421999608 ) ) ;
#41935 = CARTESIAN_POINT ( 'NONE',  ( 4.700001368028300597, 3.375077994860000042E-14, 13.99999975535615171 ) ) ;
#41936 = VERTEX_POINT ( 'NONE', #2639 ) ;
#41937 = CARTESIAN_POINT ( 'NONE',  ( 11.98052502238430073, -2.954316262216015065, 7.175009015034043536 ) ) ;
#41938 = CARTESIAN_POINT ( 'NONE',  ( 18.17997055489867719, -2.522561811188516856, -13.66861645680632620 ) ) ;
#41939 = CARTESIAN_POINT ( 'NONE',  ( 10.35826357027499789, 4.850513154668600002, 7.335909308151700614 ) ) ;
#41940 = DIRECTION ( 'NONE',  ( -1.000000000000000000, 0.000000000000000000, 0.000000000000000000 ) ) ;
#41941 = CARTESIAN_POINT ( 'NONE',  ( 8.347269353210000631, -2.741638482234999952, 6.457327039244000311 ) ) ;
#41942 = ORIENTED_EDGE ( 'NONE', *, *, #50582, .T. ) ;
#41943 = CARTESIAN_POINT ( 'NONE',  ( 8.572267219592999865, 2.606995215518000286, 6.345762205468999717 ) ) ;
#41945 = CARTESIAN_POINT ( 'NONE',  ( 10.07763305961999833, -2.169024213715999849, -7.244986319234999250 ) ) ;
#41944 = CARTESIAN_POINT ( 'NONE',  ( 10.64914416493166449, 3.188141180065802160, -7.823998238890133905 ) ) ;
#41946 = CARTESIAN_POINT ( 'NONE',  ( 7.484057796017113517, -2.418173406717145646, 6.775917929113594695 ) ) ;
#41947 = DIRECTION ( 'NONE',  ( 0.000000000000000000, -0.2461538461537953471, 0.9692307692307821076 ) ) ;
#41949 = FACE_OUTER_BOUND ( 'NONE', #67728, .T. ) ;
#41948 = VECTOR ( 'NONE', #65828, 1000.000000000000000 ) ;
#41950 = EDGE_LOOP ( 'NONE', ( #40930, #67052, #51585, #62374, #15526 ) ) ;
#41951 = CARTESIAN_POINT ( 'NONE',  ( 5.625859839683333696, -1.460959015002473382, -0.3926218265389205819 ) ) ;
#41952 = CARTESIAN_POINT ( 'NONE',  ( 12.20794988689359961, -3.544213289744700290, 6.606015074393400077 ) ) ;
#41953 = CARTESIAN_POINT ( 'NONE',  ( 10.34021053755999908, 4.202028620710000162, 9.459600235481000041 ) ) ;
#41954 = CARTESIAN_POINT ( 'NONE',  ( 10.46754281781999829, 2.318340407652000223, 6.549777679168999001 ) ) ;
#41955 = CIRCLE ( 'NONE', #1728, 12.84999890301999947 ) ;
#41956 = CARTESIAN_POINT ( 'NONE',  ( 10.25564828895399927, 4.880669054351300495, 7.018986873610899124 ) ) ;
#41957 = ORIENTED_EDGE ( 'NONE', *, *, #21180, .F. ) ;
#41958 = B_SPLINE_CURVE_WITH_KNOTS ( 'NONE', 3,
 ( #14460, #35780, #57095, #9194, #3946, #67924 ),
 .UNSPECIFIED., .F., .F.,
 ( 4, 2, 4 ),
 ( 0.000000000000000000, 0.5000000000000000000, 1.000000000000000000 ),
 .UNSPECIFIED. ) ;
#41959 = CARTESIAN_POINT ( 'NONE',  ( 23.59999468372399889, -2.915558691838999739, 13.58549495651999983 ) ) ;
#41960 = CARTESIAN_POINT ( 'NONE',  ( 12.75685216135443945, 1.762044409276926515, -12.47618552084819576 ) ) ;
#41961 = CARTESIAN_POINT ( 'NONE',  ( 3.300973465876999580, -3.500000000000000000, 0.000000000000000000 ) ) ;
#41962 = CARTESIAN_POINT ( 'NONE',  ( 25.31010560212500238, -2.730875805498000020, -11.36013797732000086 ) ) ;
#41963 = CARTESIAN_POINT ( 'NONE',  ( 18.10291081608028918, -2.039210736883937169, 13.85070288166277663 ) ) ;
#41964 = DIRECTION ( 'NONE',  ( 1.000000000000000000, -3.631529569662070274E-15, 1.174496025128702085E-14 ) ) ;
#41965 = ORIENTED_EDGE ( 'NONE', *, *, #15101, .T. ) ;
#41966 = FACE_OUTER_BOUND ( 'NONE', #65854, .T. ) ;
#41967 = LINE ( 'NONE', #53144, #41311 ) ;
#41968 = ORIENTED_EDGE ( 'NONE', *, *, #9375, .T. ) ;
#41969 =( LENGTH_UNIT ( ) NAMED_UNIT ( * ) SI_UNIT ( .MILLI., .METRE. ) );
#41970 = CARTESIAN_POINT ( 'NONE',  ( 11.46595122972049907, 4.343798595649099425, 8.295047870239098842 ) ) ;
#41971 = ADVANCED_FACE ( 'NONE', ( #55441, #55093 ), #23281, .T. ) ;
#41972 = CARTESIAN_POINT ( 'NONE',  ( 10.81315553411000074, 3.756074350075000012, 6.071610008629000355 ) ) ;
#41973 = ADVANCED_FACE ( 'NONE', ( #18725 ), #5207, .T. ) ;
#41974 = CARTESIAN_POINT ( 'NONE',  ( 10.61721774768000159, 5.045603402166999985, -6.386910706193999587 ) ) ;
#41975 = CARTESIAN_POINT ( 'NONE',  ( 9.615109647822677630, 5.349900357012234764, -7.499993490198826329 ) ) ;
#41976 = CARTESIAN_POINT ( 'NONE',  ( 9.388626433405999450, -4.079401915682999480, 9.259353168384000909 ) ) ;
#41977 = CARTESIAN_POINT ( 'NONE',  ( 17.82189142195447928, -0.6689034848678687695, -12.58223305319197571 ) ) ;
#41978 = CARTESIAN_POINT ( 'NONE',  ( 12.33505003431745273, 2.912475392612775327, -12.34587402707887449 ) ) ;
#41979 = CARTESIAN_POINT ( 'NONE',  ( 10.77256919669529900, -3.037654633983899899, -7.784327714719899483 ) ) ;
#41980 = CARTESIAN_POINT ( 'NONE',  ( 9.587885841227999251, 3.762712042852999872, 8.787816121229999666 ) ) ;
#41981 = EDGE_LOOP ( 'NONE', ( #8937, #68346, #66945, #43591 ) ) ;
#41982 = PRODUCT_CONTEXT ( 'NONE', #38704, 'mechanical' ) ;
#41983 = CARTESIAN_POINT ( 'NONE',  ( 7.325000000000000178, 4.000000000000000000, 9.239711431703000244 ) ) ;
#41984 = CARTESIAN_POINT ( 'NONE',  ( 6.999999691988000095, 12.36734761319999798, 2.759114534468000368 ) ) ;
#41985 = DIRECTION ( 'NONE',  ( 0.000000000000000000, 0.4084292560226189250, -0.9127899773906427150 ) ) ;
#41986 = CIRCLE ( 'NONE', #18537, 8.250000000000000000 ) ;
#41987 = CARTESIAN_POINT ( 'NONE',  ( 10.93008194863999449, 9.554106281501004716, 6.653031737998000850 ) ) ;
#41988 = CARTESIAN_POINT ( 'NONE',  ( 12.41959488098031095, 1.899094099299810212, 13.87060288894783255 ) ) ;
#41989 = CARTESIAN_POINT ( 'NONE',  ( 13.69997185827400088, 11.21472423003503494, 3.290649947225259719 ) ) ;
#41990 = CARTESIAN_POINT ( 'NONE',  ( 10.90000000000000036, -0.2999999999999999889, -4.902439024389999567 ) ) ;
#41991 = CARTESIAN_POINT ( 'NONE',  ( 24.84573454058074660, 8.580102523463006392, 9.011245526633942404 ) ) ;
#41992 = ADVANCED_FACE ( 'NONE', ( #9166 ), #36454, .F. ) ;
#41993 = EDGE_LOOP ( 'NONE', ( #42639, #22553, #22941, #55388 ) ) ;
#41994 = CARTESIAN_POINT ( 'NONE',  ( 12.47072553654366267, -1.841758158201590945, 12.46466843114748890 ) ) ;
#41995 = EDGE_CURVE ( 'NONE', #36015, #49775, #21807, .T. ) ;
#41996 = B_SPLINE_CURVE_WITH_KNOTS ( 'NONE', 3,
 ( #41792, #40760, #62082, #14544 ),
 .UNSPECIFIED., .F., .F.,
 ( 4, 4 ),
 ( 0.000000000000000000, 1.000000000000000000 ),
 .UNSPECIFIED. ) ;
#41997 = CARTESIAN_POINT ( 'NONE',  ( 9.809000818239997699, -5.010295986746999830, -8.032011717116800398 ) ) ;
#41998 = CARTESIAN_POINT ( 'NONE',  ( 11.09999999999999964, -2.861044734458999627E-13, 5.200284647344000995E-13 ) ) ;
#41999 = CARTESIAN_POINT ( 'NONE',  ( 10.59344961228999971, -5.297755890367000120, 8.474197994416998725 ) ) ;
#42000 = CARTESIAN_POINT ( 'NONE',  ( 11.71979841651039855, -4.304975143798100312, 6.689266534545799558 ) ) ;
#42001 = AXIS2_PLACEMENT_3D ( 'NONE', #31468, #30778, #62918 ) ;
#42002 = ADVANCED_FACE ( 'NONE', ( #6845 ), #49609, .T. ) ;
#42003 = B_SPLINE_CURVE_WITH_KNOTS ( 'NONE', 3,
 ( #64252, #18447, #3042, #34872 ),
 .UNSPECIFIED., .F., .F.,
 ( 4, 4 ),
 ( 0.000000000000000000, 1.000000000000000000 ),
 .UNSPECIFIED. ) ;
#42004 = AXIS2_PLACEMENT_3D ( 'NONE', #62436, #52989, #9289 ) ;
#42005 = CARTESIAN_POINT ( 'NONE',  ( 12.32690578124262970, 0.5408165383911035518, 12.58839068838662811 ) ) ;
#42006 = B_SPLINE_CURVE_WITH_KNOTS ( 'NONE', 3,
 ( #50923, #17739, #55482, #40100, #39058 ),
 .UNSPECIFIED., .F., .F.,
 ( 4, 1, 4 ),
 ( 0.000000000000000000, 0.2283573561321438072, 1.000000000000000000 ),
 .UNSPECIFIED. ) ;
#42007 = CARTESIAN_POINT ( 'NONE',  ( 7.726448341228000061, 2.630487280353000390, 6.995957894972000268 ) ) ;
#42008 = CARTESIAN_POINT ( 'NONE',  ( 4.652221739856806870, 0.7358276262617508001, 0.9460093964854561222 ) ) ;
#42009 = CARTESIAN_POINT ( 'NONE',  ( 12.08892279761558086, 2.366838896507799550, 12.37571060269619139 ) ) ;
#42010 = CARTESIAN_POINT ( 'NONE',  ( 10.67905590578999941, -2.899999999999999911, 6.571291218949999902 ) ) ;
#42011 = CARTESIAN_POINT ( 'NONE',  ( 10.62487750876920067, 3.456442671114800191, -8.343502390669698343 ) ) ;
#42012 = CARTESIAN_POINT ( 'NONE',  ( 12.36003207187216013, 11.57530800953516703, -4.784147006775551603 ) ) ;
#42013 = CARTESIAN_POINT ( 'NONE',  ( 10.78888278041000071, 2.675726696512000125, -6.748227692827999391 ) ) ;
#42014 = CARTESIAN_POINT ( 'NONE',  ( 9.529317406968999649, 4.237919115995800290, -8.756892549790999070 ) ) ;
#42016 = CARTESIAN_POINT ( 'NONE',  ( 3.999999615355000149, 1.825000384556999977, -7.326396463183999951E-10 ) ) ;
#42015 = CARTESIAN_POINT ( 'NONE',  ( 11.79999999471800010, -11.69117318561000118, -1.923227876431999883 ) ) ;
#42017 = CARTESIAN_POINT ( 'NONE',  ( 8.801820635884373800, 4.060146622106553416, 6.549596649571864937 ) ) ;
#42018 = ORIENTED_EDGE ( 'NONE', *, *, #26756, .T. ) ;
#42019 = CARTESIAN_POINT ( 'NONE',  ( 12.37275785075365597, 0.4515912410345762629, 12.68919663783466234 ) ) ;
#42020 = EDGE_CURVE ( 'NONE', #60415, #56347, #30999, .T. ) ;
#42021 = CARTESIAN_POINT ( 'NONE',  ( 10.14393020684899938, 5.250000000000000000, 7.500000000000000000 ) ) ;
#42022 = CARTESIAN_POINT ( 'NONE',  ( 10.93728138146000006, -5.425439422033999648, 7.240583766112999697 ) ) ;
#42023 = CARTESIAN_POINT ( 'NONE',  ( 9.830304848515998728, 4.788504886021700102, 7.139489266142899915 ) ) ;
#42024 = DIRECTION ( 'NONE',  ( -0.7071068090162534459, 0.000000000000000000, 0.7071067533568404784 ) ) ;
#42025 = CARTESIAN_POINT ( 'NONE',  ( 12.26168426244257326, -2.190490593926008867, 13.73426451135289916 ) ) ;
#42026 = LINE ( 'NONE', #68231, #16337 ) ;
#42027 = DIRECTION ( 'NONE',  ( 0.000000000000000000, -1.000000000000000000, 0.000000000000000000 ) ) ;
#42028 = ORIENTED_EDGE ( 'NONE', *, *, #100, .F. ) ;
#42029 = CARTESIAN_POINT ( 'NONE',  ( 5.140096680883000424, 0.7660746065864000309, 0.8366799443169999906 ) ) ;
#42030 = CARTESIAN_POINT ( 'NONE',  ( 8.693455549952998851, -3.004437130344999929, -6.696732323226999739 ) ) ;
#42031 = CYLINDRICAL_SURFACE ( 'NONE', #17580, 11.84999999999999964 ) ;
#42032 = CARTESIAN_POINT ( 'NONE',  ( 11.73078751119019891, -4.915752892793999962, 7.020904658857499925 ) ) ;
#42033 = CARTESIAN_POINT ( 'NONE',  ( 17.94956985871012733, 2.984774188598619649, -12.32531689504261685 ) ) ;
#42034 = CARTESIAN_POINT ( 'NONE',  ( 10.52052890781999928, -2.899999999999999911, 6.152188490330000370 ) ) ;
#42035 = CARTESIAN_POINT ( 'NONE',  ( 8.599999952505998024, 4.000000000000000000, -7.500000000000000000 ) ) ;
#42036 = CARTESIAN_POINT ( 'NONE',  ( 24.30001697071400457, -8.938702858184001343, 8.938676113071998941 ) ) ;
#42037 = DIRECTION ( 'NONE',  ( 0.000000000000000000, 0.000000000000000000, -1.000000000000000000 ) ) ;
#42038 = CARTESIAN_POINT ( 'NONE',  ( 5.500000000000000000, 12.43893545635000031, -2.828937028792000152 ) ) ;
#42039 = CYLINDRICAL_SURFACE ( 'NONE', #4255, 1.350000000000000089 ) ;
#42040 = CARTESIAN_POINT ( 'NONE',  ( 7.910784822166045949, -5.348998117051901424, 7.262899563230540423 ) ) ;
#42041 = CARTESIAN_POINT ( 'NONE',  ( 24.17809389475516468, 9.100323006451731089, -9.085318127976481861 ) ) ;
#42042 = CARTESIAN_POINT ( 'NONE',  ( 11.59213512191444018, 3.196550831395155168, 7.825049263296810054 ) ) ;
#42043 = CARTESIAN_POINT ( 'NONE',  ( 23.58303149431899826, 13.27303032590999976, -4.267677747246999331 ) ) ;
#42044 = VERTEX_POINT ( 'NONE', #3494 ) ;
#42045 = CARTESIAN_POINT ( 'NONE',  ( 9.161379719595000637, 5.511689883260999956, -7.095113581311000672 ) ) ;
#42046 = CARTESIAN_POINT ( 'NONE',  ( 11.22749279009020107, -4.225282629687599822, 6.663611138821799784 ) ) ;
#42047 = ORIENTED_EDGE ( 'NONE', *, *, #56359, .F. ) ;
#42048 = CIRCLE ( 'NONE', #67726, 13.89999852641999922 ) ;
#42049 = CARTESIAN_POINT ( 'NONE',  ( 12.80505043854144276, -5.963111948670274387E-16, -25.00000000000000000 ) ) ;
#42050 = CARTESIAN_POINT ( 'NONE',  ( 10.17764828895399809, -2.998858038575999974, -8.046814291299300592 ) ) ;
#42051 = ORIENTED_EDGE ( 'NONE', *, *, #32656, .F. ) ;
#42052 = CARTESIAN_POINT ( 'NONE',  ( 11.42834208742529967, 3.293478249981899975, 6.389420067180999752 ) ) ;
#42053 = CARTESIAN_POINT ( 'NONE',  ( 9.541460841232000334, 2.824732249080000202, -8.992748220058999209 ) ) ;
#42054 = ADVANCED_FACE ( 'NONE', ( #3159 ), #45399, .F. ) ;
#42055 = DIRECTION ( 'NONE',  ( 0.8843050081471317547, -0.1786786086946064722, 0.4313682966571153465 ) ) ;
#42056 = EDGE_CURVE ( 'NONE', #51187, #10058, #65009, .T. ) ;
#42057 = CARTESIAN_POINT ( 'NONE',  ( 10.94501463001509833, -3.527519786474400121, -6.743262887067199784 ) ) ;
#42058 = CARTESIAN_POINT ( 'NONE',  ( 12.40292999708903565, 0.4784640316632534640, -13.88891505532827075 ) ) ;
#42059 = CARTESIAN_POINT ( 'NONE',  ( 13.56648734862639216, -12.13584047101458552, -2.505837749223106758 ) ) ;
#42060 = CARTESIAN_POINT ( 'NONE',  ( 12.96427412810700197, 11.57018092489999894, 1.758708699944000031 ) ) ;
#42061 = VERTEX_POINT ( 'NONE', #24141 ) ;
#42062 = CARTESIAN_POINT ( 'NONE',  ( 8.013507625983999461, 4.606065150774999672, -6.249409674000999892 ) ) ;
#42063 = CARTESIAN_POINT ( 'NONE',  ( 9.675870280412999236, 3.031907308384000022, -8.729608011560001657 ) ) ;
#42064 = ORIENTED_EDGE ( 'NONE', *, *, #17526, .F. ) ;
#42065 = CARTESIAN_POINT ( 'NONE',  ( 10.82565186280000091, 5.331165376905000031, -8.542144899688000947 ) ) ;
#42066 = ORIENTED_EDGE ( 'NONE', *, *, #68641, .F. ) ;
#42067 = CARTESIAN_POINT ( 'NONE',  ( 9.731950584426998674, 4.507735863714500191, 8.674133161175999973 ) ) ;
#42068 = CARTESIAN_POINT ( 'NONE',  ( 18.17892392841396187, -2.542707335428990856, -12.44153274845740498 ) ) ;
#42069 = DIRECTION ( 'NONE',  ( -1.000000000000000000, 0.000000000000000000, -2.609704304917999919E-14 ) ) ;
#42070 = CARTESIAN_POINT ( 'NONE',  ( 23.56666365135700403, -9.069641144917994779, -7.556701426681005529 ) ) ;
#42071 = DIRECTION ( 'NONE',  ( 0.000000000000000000, 0.9421243786071880066, 0.3352635608502960718 ) ) ;
#42072 = ORIENTED_EDGE ( 'NONE', *, *, #51607, .T. ) ;
#42073 = CARTESIAN_POINT ( 'NONE',  ( 12.04524561587600040, 11.75582082520000071, -3.881266971570000113 ) ) ;
#42074 = CARTESIAN_POINT ( 'NONE',  ( 9.797024780922274800, -5.515983957001070692, -6.595663371089560911 ) ) ;
#42075 = B_SPLINE_CURVE_WITH_KNOTS ( 'NONE', 3,
 ( #61542, #61885, #40558, #56644 ),
 .UNSPECIFIED., .F., .F.,
 ( 4, 4 ),
 ( 0.000000000000000000, 1.000000000000000000 ),
 .UNSPECIFIED. ) ;
#42076 = DIRECTION ( 'NONE',  ( 0.000000000000000000, 0.000000000000000000, 1.000000000000000000 ) ) ;
#42077 = CARTESIAN_POINT ( 'NONE',  ( 8.936337454063531638, 3.131903168333550536, 8.168216413461584224 ) ) ;
#42078 = VECTOR ( 'NONE', #63457, 1000.000000000000000 ) ;
#42079 = ADVANCED_FACE ( 'NONE', ( #7719 ), #39013, .T. ) ;
#42080 = CARTESIAN_POINT ( 'NONE',  ( 10.03280471959000231, 3.987760651117999711, -9.123263301387000368 ) ) ;
#42081 =( GEOMETRIC_REPRESENTATION_CONTEXT ( 3 ) GLOBAL_UNCERTAINTY_ASSIGNED_CONTEXT ( ( #37373 ) ) GLOBAL_UNIT_ASSIGNED_CONTEXT ( ( #67587, #8875, #35790 ) ) REPRESENTATION_CONTEXT ( 'NONE', 'WORKASPACE' ) );
#42082 = CARTESIAN_POINT ( 'NONE',  ( 17.88705809229600163, -3.642474092890999771, 12.02409483768999898 ) ) ;
#42083 = CARTESIAN_POINT ( 'NONE',  ( 9.780291077142999612, -3.021588645102999848, -8.450043670922001482 ) ) ;
#42084 = EDGE_LOOP ( 'NONE', ( #38641, #41504, #24610, #539, #3066, #35580, #14319, #52282, #31944, #20464, #27159, #68367, #55034, #20831, #36526, #19078, #1375 ) ) ;
#42085 = EDGE_LOOP ( 'NONE', ( #64653, #3759, #55624 ) ) ;
#42086 = B_SPLINE_CURVE_WITH_KNOTS ( 'NONE', 3,
 ( #12149, #27537, #1653, #623, #48862, #64918, #17032, #28227, #49894, #44321 ),
 .UNSPECIFIED., .F., .F.,
 ( 4, 2, 2, 2, 4 ),
 ( 0.000000000000000000, 0.2500000000000000000, 0.5000000000000000000, 0.7500000000000000000, 1.000000000000000000 ),
 .UNSPECIFIED. ) ;
#42087 = CARTESIAN_POINT ( 'NONE',  ( 10.86079988039000099, 5.063207163126000943, -5.172914090247000551 ) ) ;
#42088 = AXIS2_PLACEMENT_3D ( 'NONE', #69021, #52949, #6075 ) ;
#42089 = CARTESIAN_POINT ( 'NONE',  ( 10.09645344438251691, 5.267621374772807563, -8.036571084497403206 ) ) ;
#42090 = CARTESIAN_POINT ( 'NONE',  ( 1.217640132540999787, -1.762666431298159475, 3.058252359239895135 ) ) ;
#42091 = DIRECTION ( 'NONE',  ( 1.000000000000000000, 0.000000000000000000, 0.000000000000000000 ) ) ;
#42092 = CARTESIAN_POINT ( 'NONE',  ( 11.76588784977539781, 2.879134238109999799, -7.435950347916509884 ) ) ;
#42093 = CARTESIAN_POINT ( 'NONE',  ( 9.180747021775998107, 3.348327362764200288, -8.071865996877098937 ) ) ;
#42095 = CARTESIAN_POINT ( 'NONE',  ( 4.399671512406701623, 1.282007644070062957, -0.5110265287773028131 ) ) ;
#42094 = CARTESIAN_POINT ( 'NONE',  ( 9.901721904869999591, -3.124169273628900179, 7.008306153105300140 ) ) ;
#42096 = CARTESIAN_POINT ( 'NONE',  ( 8.437014469680988782, -2.901284097310000920, 6.624005965434003329 ) ) ;
#42097 = VERTEX_POINT ( 'NONE', #61801 ) ;
#42098 = AXIS2_PLACEMENT_3D ( 'NONE', #44278, #22581, #13494 ) ;
#42099 = DIRECTION ( 'NONE',  ( -1.000000000000000000, 0.000000000000000000, -1.275169027325000072E-14 ) ) ;
#42100 = EDGE_CURVE ( 'NONE', #53475, #2231, #52518, .T. ) ;
#42101 = CARTESIAN_POINT ( 'NONE',  ( 10.35162153983000088, -3.367195699800999975, -4.861353673146999732 ) ) ;
#42102 = CARTESIAN_POINT ( 'NONE',  ( 9.507558421712998253, -4.699533657262000119, -6.366989705700999203 ) ) ;
#42103 = CARTESIAN_POINT ( 'NONE',  ( 13.99999999485600277, 9.471999751521998689, 8.194948195317001804 ) ) ;
#42104 = CIRCLE ( 'NONE', #17558, 12.20000000000000284 ) ;
#42105 = CARTESIAN_POINT ( 'NONE',  ( 10.80815535238000002, -2.937528991339000140, 8.948455587554001056 ) ) ;
#42106 = CARTESIAN_POINT ( 'NONE',  ( 18.18005043817894872, 2.519674551049350786, -12.44700836821350620 ) ) ;
#42107 = CARTESIAN_POINT ( 'NONE',  ( 9.819055905797000605, -2.899999999999999911, -6.571291218949999902 ) ) ;
#42108 = CARTESIAN_POINT ( 'NONE',  ( 15.65828218294665675, -9.154335746262512785, -8.252742830647335381 ) ) ;
#42109 = CARTESIAN_POINT ( 'NONE',  ( 7.972192870573465484, 2.986178616227031846, -6.494259741701720046 ) ) ;
#42110 = CARTESIAN_POINT ( 'NONE',  ( 10.19190035061499877, -3.732283713685800031, -8.468075389605498771 ) ) ;
#42111 = DIRECTION ( 'NONE',  ( 1.000000000000000000, 0.000000000000000000, 0.000000000000000000 ) ) ;
#42112 = CARTESIAN_POINT ( 'NONE',  ( 11.19837472757367713, -4.473492782822720670, 6.765225077371590956 ) ) ;
#42113 = CARTESIAN_POINT ( 'NONE',  ( 3.899999503719000060, 0.000000000000000000, -1.725000594299999968 ) ) ;
#42114 = FACE_OUTER_BOUND ( 'NONE', #8173, .T. ) ;
#42115 = ORIENTED_EDGE ( 'NONE', *, *, #22641, .F. ) ;
#42116 = CARTESIAN_POINT ( 'NONE',  ( 12.19008233596125557, -0.1120021961262563370, -12.69934078656688925 ) ) ;
#42117 = CARTESIAN_POINT ( 'NONE',  ( 12.23179573713378510, -2.749250017956391012, -12.38999654619789403 ) ) ;
#42118 = DIRECTION ( 'NONE',  ( 0.000000000000000000, 0.2588190451024927063, -0.9659258262890757507 ) ) ;
#42119 = CARTESIAN_POINT ( 'NONE',  ( 10.88876599830666692, -5.215403687430652191, 6.904706716043305548 ) ) ;
#42120 = CARTESIAN_POINT ( 'NONE',  ( 10.36503728015293646, 2.650011783304074164, -7.500002219258057323 ) ) ;
#42121 = ORIENTED_EDGE ( 'NONE', *, *, #28810, .T. ) ;
#42122 = CARTESIAN_POINT ( 'NONE',  ( 18.30003129332100187, -2.732683818840999646, -11.53064095373000164 ) ) ;
#42123 = PRODUCT_CONTEXT ( 'NONE', #6535, 'mechanical' ) ;
#42124 = CARTESIAN_POINT ( 'NONE',  ( 11.35034208742529849, -4.630634088820300143, -8.491292290686200062 ) ) ;
#42125 = B_SPLINE_CURVE_WITH_KNOTS ( 'NONE', 3,
 ( #65941, #3007, #34840, #43949, #8259, #33459 ),
 .UNSPECIFIED., .F., .F.,
 ( 4, 2, 4 ),
 ( 0.000000000000000000, 0.5000000000000000000, 1.000000000000000000 ),
 .UNSPECIFIED. ) ;
#42126 = CARTESIAN_POINT ( 'NONE',  ( 17.95596512695399127, 0.4795041973588453632, 12.68781427220483771 ) ) ;
#42127 = CARTESIAN_POINT ( 'NONE',  ( 13.64504292973000332, -11.45087266113000091, -2.419799131125000002 ) ) ;
#42128 = CARTESIAN_POINT ( 'NONE',  ( 7.625781557060339999, 4.984822363484057384, -8.445605089947335387 ) ) ;
#42129 = CARTESIAN_POINT ( 'NONE',  ( 10.90346005378009941, 4.786957292481900161, -7.079777642108599167 ) ) ;
#42130 = ORIENTED_EDGE ( 'NONE', *, *, #20431, .F. ) ;
#42131 = CIRCLE ( 'NONE', #68917, 2.250000000000000000 ) ;
#42132 = B_SPLINE_CURVE_WITH_KNOTS ( 'NONE', 3,
 ( #57195, #52299, #19803, #4396, #20485, #63811, #20141, #42165, #47063, #9297 ),
 .UNSPECIFIED., .F., .F.,
 ( 4, 2, 2, 2, 4 ),
 ( 0.000000000000000000, 0.2500000000000001110, 0.5000000000000001110, 0.7500000000000001110, 1.000000000000000000 ),
 .UNSPECIFIED. ) ;
#42133 = CARTESIAN_POINT ( 'NONE',  ( 10.61382642076999971, -3.385081736013999976, 5.849525238167000651 ) ) ;
#42134 = ORIENTED_EDGE ( 'NONE', *, *, #13282, .F. ) ;
#42135 = CARTESIAN_POINT ( 'NONE',  ( 8.439067896944781211, -2.959717315122096348, 6.275320676522057717 ) ) ;
#42136 = CARTESIAN_POINT ( 'NONE',  ( 7.609456853206999938, -3.276313010012999793, 5.841993238691999935 ) ) ;
#42137 = DIRECTION ( 'NONE',  ( 0.000000000000000000, 0.000000000000000000, -1.000000000000000000 ) ) ;
#42138 = EDGE_CURVE ( 'NONE', #58126, #46140, #30011, .T. ) ;
#42139 = ORIENTED_EDGE ( 'NONE', *, *, #15959, .F. ) ;
#42140 = CARTESIAN_POINT ( 'NONE',  ( 8.482014052312178976, 3.633347688910150808, -9.218057214805476463 ) ) ;
#42141 = EDGE_CURVE ( 'NONE', #14432, #15277, #44252, .T. ) ;
#42142 = CARTESIAN_POINT ( 'NONE',  ( 6.596014158771000169, 5.307493345713999666, -7.572367724995999971 ) ) ;
#42143 = VECTOR ( 'NONE', #8969, 1000.000000000000114 ) ;
#42144 = CARTESIAN_POINT ( 'NONE',  ( 11.09999803709000155, -1.407105940352999962, 11.46396214177000061 ) ) ;
#42145 = ADVANCED_FACE ( 'NONE', ( #34214 ), #29669, .T. ) ;
#42146 = CARTESIAN_POINT ( 'NONE',  ( 8.455992358796999397, 2.899999999999999911, -6.571291218954000257 ) ) ;
#42147 = ORIENTED_EDGE ( 'NONE', *, *, #10415, .F. ) ;
#42148 = CARTESIAN_POINT ( 'NONE',  ( 9.256662271119999730, -4.025830307267999508, 9.295859242339000517 ) ) ;
#42149 = EDGE_CURVE ( 'NONE', #42844, #31626, #8324, .T. ) ;
#42150 = CARTESIAN_POINT ( 'NONE',  ( 10.81772273141334750, 5.100000000000000533, -6.253511885790826952 ) ) ;
#42151 = DIRECTION ( 'NONE',  ( -1.000000000000000000, 0.000000000000000000, 0.000000000000000000 ) ) ;
#42152 = ORIENTED_EDGE ( 'NONE', *, *, #57307, .T. ) ;
#42153 = CIRCLE ( 'NONE', #68933, 0.6999999999999992895 ) ;
#42154 = PLANE ( 'NONE',  #23643 ) ;
#42155 = VERTEX_POINT ( 'NONE', #18472 ) ;
#42156 = CARTESIAN_POINT ( 'NONE',  ( 3.500000000000000444, 0.4524638778880175072, 3.273161885834219298 ) ) ;
#42157 = CARTESIAN_POINT ( 'NONE',  ( 24.11583214838473666, 12.52251212749843212, -3.380867675773815417 ) ) ;
#42158 = DIRECTION ( 'NONE',  ( 0.8660254037843856390, 0.000000000000000000, -0.5000000000000918154 ) ) ;
#42159 = CARTESIAN_POINT ( 'NONE',  ( 8.769668397160224060, 4.137335898486747432, -5.812840004581696363 ) ) ;
#42160 = LINE ( 'NONE', #63461, #48688 ) ;
#42161 = CARTESIAN_POINT ( 'NONE',  ( 24.19055549696582119, 12.39716933831719814, 3.330586599044198959 ) ) ;
#42162 = AXIS2_PLACEMENT_3D ( 'NONE', #48087, #36913, #11361 ) ;
#42163 = CARTESIAN_POINT ( 'NONE',  ( 9.643930206848999376, -2.750000000000000000, -7.500000000000000000 ) ) ;
#42164 = VERTEX_POINT ( 'NONE', #34564 ) ;
#42165 = CARTESIAN_POINT ( 'NONE',  ( 3.326208585479333735, -3.365580714188050937, -1.109430098042168744 ) ) ;
#42166 = ORIENTED_EDGE ( 'NONE', *, *, #65361, .T. ) ;
#42167 = CARTESIAN_POINT ( 'NONE',  ( 10.22398792753999963, 5.507894434963000130, 6.589802269404000157 ) ) ;
#42168 = EDGE_CURVE ( 'NONE', #664, #46365, #10050, .T. ) ;
#42169 = CARTESIAN_POINT ( 'NONE',  ( 4.468342168782999835, 0.2293269131957661466, 1.516947103425834831 ) ) ;
#42170 = DIRECTION ( 'NONE',  ( 0.000000000000000000, -1.000000000000000000, 0.000000000000000000 ) ) ;
#42171 = CARTESIAN_POINT ( 'NONE',  ( 12.72203378256778983, 1.880187905311241581, -13.78554362285502677 ) ) ;
#42172 = CARTESIAN_POINT ( 'NONE',  ( 5.000000004241000440, 0.05000000424131000043, -3.149999962200000336 ) ) ;
#42173 = CARTESIAN_POINT ( 'NONE',  ( 7.000000000000000888, 6.725378844700938608, -3.045375366903437797 ) ) ;
#42174 = CARTESIAN_POINT ( 'NONE',  ( 18.17602483311041439, 0.07155107330948734523, 13.89975717292031376 ) ) ;
#42175 = CARTESIAN_POINT ( 'NONE',  ( 13.70003001321900271, -9.668726926528000476, -7.961868161445000425 ) ) ;
#42176 = VERTEX_POINT ( 'NONE', #51649 ) ;
#42177 = CARTESIAN_POINT ( 'NONE',  ( 12.33180813479861904, 0.4082709497317869030, 13.89192968283204088 ) ) ;
#42178 = CARTESIAN_POINT ( 'NONE',  ( 12.12579573085663043, -2.760622544769000264, 7.285547569258399747 ) ) ;
#42179 = CARTESIAN_POINT ( 'NONE',  ( 11.39975833414730033, -3.203462856645999945, -7.174999999999999822 ) ) ;
#42180 = DIRECTION ( 'NONE',  ( 0.000000000000000000, 1.000000000000000000, 0.000000000000000000 ) ) ;
#42181 = CARTESIAN_POINT ( 'NONE',  ( 7.256081853207000165, -2.531197775378000170, 8.216705951490000714 ) ) ;
#42183 = CARTESIAN_POINT ( 'NONE',  ( 23.89320776801300283, -1.894218448865001792, -11.32736289216000536 ) ) ;
#42182 = CARTESIAN_POINT ( 'NONE',  ( 10.75109581085999899, 2.822145500011000063, 6.655897464539000552 ) ) ;
#42184 = CARTESIAN_POINT ( 'NONE',  ( 10.25149413291699929, 5.037815157227999663, -7.026470926762800495 ) ) ;
#42185 = VECTOR ( 'NONE', #66193, 1000.000000000000000 ) ;
#42186 = FACE_OUTER_BOUND ( 'NONE', #953, .T. ) ;
#42187 = EDGE_CURVE ( 'NONE', #47380, #8792, #68063, .T. ) ;
#42188 = CONICAL_SURFACE ( 'NONE', #66877, 12.69999976913000062, 0.7853981453603698926 ) ;
#42189 = CARTESIAN_POINT ( 'NONE',  ( 10.32844474310100047, 4.771257858050099721, -7.874284411628199365 ) ) ;
#42190 = CARTESIAN_POINT ( 'NONE',  ( 17.78855914542205952, 0.6810629908226980556, 12.58158054216573341 ) ) ;
#42191 = CARTESIAN_POINT ( 'NONE',  ( 7.160490346876999368, -0.4460864650370000017, 1.192484047995999941 ) ) ;
#42192 = EDGE_CURVE ( 'NONE', #1871, #67995, #16729, .T. ) ;
#42193 = VECTOR ( 'NONE', #14924, 1000.000000000000114 ) ;
#42194 = CARTESIAN_POINT ( 'NONE',  ( 18.26079396959979206, -3.428468831595210542, 12.04667397462565148 ) ) ;
#42195 = ORIENTED_EDGE ( 'NONE', *, *, #14194, .T. ) ;
#42196 = CARTESIAN_POINT ( 'NONE',  ( 7.518870559622000016, -3.206365290996999740, 5.681739161071000410 ) ) ;
#42197 = CARTESIAN_POINT ( 'NONE',  ( 9.758079719591000512, 4.905765359186999852, -8.776126235875999271 ) ) ;
#42198 = CARTESIAN_POINT ( 'NONE',  ( 17.84552141390803115, 3.187082727966593865, 13.63240720791674576 ) ) ;
#42199 = CARTESIAN_POINT ( 'NONE',  ( 11.09999952335000195, -1.407106647395000021, 11.46396798199000067 ) ) ;
#42200 = ORIENTED_EDGE ( 'NONE', *, *, #3074, .T. ) ;
#42201 = AXIS2_PLACEMENT_3D ( 'NONE', #6338, #762, #10558 ) ;
#42202 = CARTESIAN_POINT ( 'NONE',  ( 18.35168611684299833, 2.962034070680999776, 12.02052262816000017 ) ) ;
#42203 = CARTESIAN_POINT ( 'NONE',  ( 11.56833327354034857, 3.253412192327699959, 7.988332985010599963 ) ) ;
#42204 = CARTESIAN_POINT ( 'NONE',  ( 10.63743278041000018, 3.721476136598000028, -8.997092462634000753 ) ) ;
#42205 = ORIENTED_EDGE ( 'NONE', *, *, #15720, .T. ) ;
#42206 = CARTESIAN_POINT ( 'NONE',  ( 9.310585478579783469, 3.370455731697034718, -6.407725666907083450 ) ) ;
#42207 = AXIS2_PLACEMENT_3D ( 'NONE', #24843, #29764, #13673 ) ;
#42208 = CARTESIAN_POINT ( 'NONE',  ( 8.613182395985113260, 4.653584300239311133, 5.903187239484920745 ) ) ;
#42209 = CARTESIAN_POINT ( 'NONE',  ( 10.44426222744799837, 3.013556901740999994, 6.687444528363699625 ) ) ;
#42210 = CARTESIAN_POINT ( 'NONE',  ( 5.664191326658419179, 12.07183080424314525, 3.732901064425761639 ) ) ;
#42211 = CARTESIAN_POINT ( 'NONE',  ( 8.143323341229999457, 5.061727314042999915, 5.824077473724000420 ) ) ;
#42212 = ORIENTED_EDGE ( 'NONE', *, *, #13415, .F. ) ;
#42213 = CARTESIAN_POINT ( 'NONE',  ( 11.50001496185000605, 12.31773593199343786, -2.620250046340033556 ) ) ;
#42214 = CARTESIAN_POINT ( 'NONE',  ( 6.821014158771999014, 5.777496342847000754, -7.598381660561000395 ) ) ;
#42215 = CARTESIAN_POINT ( 'NONE',  ( 8.220624047935833900, -5.675834487486897117, 7.965153098552243627 ) ) ;
#42216 = CARTESIAN_POINT ( 'NONE',  ( 9.421417874593998931, -5.177249570814000279, 6.999532383170999239 ) ) ;
#42217 = VERTEX_POINT ( 'NONE', #36609 ) ;
#42218 = CARTESIAN_POINT ( 'NONE',  ( 16.27269624719400198, -3.670072847095000146, -12.01573327568000060 ) ) ;
#42219 = LINE ( 'NONE', #53392, #31721 ) ;
#42220 = ORIENTED_EDGE ( 'NONE', *, *, #47235, .F. ) ;
#42221 = CARTESIAN_POINT ( 'NONE',  ( 10.09184687351566723, -3.000416447002275167, 6.731816600031356401 ) ) ;
#42222 = CARTESIAN_POINT ( 'NONE',  ( 24.51107830332481896, -8.765523554282413699, -8.765522532328214211 ) ) ;
#42223 = CARTESIAN_POINT ( 'NONE',  ( 18.06357043707759402, 0.3639325664385109627, -13.89360161040561970 ) ) ;
#42224 = CARTESIAN_POINT ( 'NONE',  ( 10.19691842572999896, -4.268950419651999617, -8.781589108989999559 ) ) ;
#42225 = CARTESIAN_POINT ( 'NONE',  ( 8.596685841231000325, 2.141799395716999843, -7.895788736628000848 ) ) ;
#42226 = B_SPLINE_CURVE_WITH_KNOTS ( 'NONE', 3,
 ( #19035, #13801, #40364, #61685 ),
 .UNSPECIFIED., .F., .F.,
 ( 4, 4 ),
 ( 0.000000000000000000, 1.000000000000000000 ),
 .UNSPECIFIED. ) ;
#42227 = CARTESIAN_POINT ( 'NONE',  ( 11.10101463001529964, 4.622233839778099984, -6.503413421344399481 ) ) ;
#42228 = CARTESIAN_POINT ( 'NONE',  ( 11.64256920625030034, -3.957769094421040190, 8.674127893687000324 ) ) ;
#42229 = CARTESIAN_POINT ( 'NONE',  ( 8.734407071272288547, -5.610846102776929634, 8.247418371894697842 ) ) ;
#42230 = EDGE_CURVE ( 'NONE', #33960, #11762, #42048, .T. ) ;
#42231 = CARTESIAN_POINT ( 'NONE',  ( 11.73610538575739959, -2.890527834009000152, 7.765257665594799796 ) ) ;
#42232 = ORIENTED_EDGE ( 'NONE', *, *, #8050, .F. ) ;
#42233 = CARTESIAN_POINT ( 'NONE',  ( 7.058509992104999853, 4.314040636970999820, 8.819134391732999845 ) ) ;
#42234 = EDGE_CURVE ( 'NONE', #22269, #37337, #50927, .T. ) ;
#42235 = ORIENTED_EDGE ( 'NONE', *, *, #29731, .T. ) ;
#42236 = CARTESIAN_POINT ( 'NONE',  ( 3.500000000000000444, -3.140247483149941399, 0.3442837550748506503 ) ) ;
#42237 = B_SPLINE_CURVE_WITH_KNOTS ( 'NONE', 3,
 ( #53407, #22271, #48852, #33466, #65264, #16678, #1645, #60026, #27880, #10745, #11096, #17021, #11777, #5505, #32772, #26845, #38353, #16336 ),
 .UNSPECIFIED., .F., .F.,
 ( 4, 2, 2, 2, 2, 2, 2, 2, 4 ),
 ( 0.000000000000000000, 0.1250000000000000000, 0.2500000000000000000, 0.3750000000000000000, 0.5000000000000000000, 0.6250000000000000000, 0.7500000000000000000, 0.8750000000000000000, 1.000000000000000000 ),
 .UNSPECIFIED. ) ;
#42238 = CARTESIAN_POINT ( 'NONE',  ( 9.251933059621999078, -5.159251056493999954, 9.109488373271000583 ) ) ;
#42239 = CARTESIAN_POINT ( 'NONE',  ( 17.55505043854144276, -0.6250000000000001110, 12.67928921589117586 ) ) ;
#42240 = ORIENTED_EDGE ( 'NONE', *, *, #29570, .F. ) ;
#42241 = CARTESIAN_POINT ( 'NONE',  ( 12.80505043854146940, -1.760910691117822280, -12.47634535983623216 ) ) ;
#42242 = CARTESIAN_POINT ( 'NONE',  ( 18.11007341752342015, 3.284452655023115231, 11.17744038474791068 ) ) ;
#42243 = CARTESIAN_POINT ( 'NONE',  ( 10.81059687351629961, 3.370476274536378103, 8.592232985442823434 ) ) ;
#42244 = CARTESIAN_POINT ( 'NONE',  ( 12.08015713295728411, -2.543697886577363843, -13.76699599502173044 ) ) ;
#42245 = AXIS2_PLACEMENT_3D ( 'NONE', #61955, #18281, #29819 ) ;
#42246 = CARTESIAN_POINT ( 'NONE',  ( 10.33364828895399867, -3.239803852721999888, -7.915211961479200475 ) ) ;
#42247 = CARTESIAN_POINT ( 'NONE',  ( 7.077542425583873253, -1.465994342824544899E-06, -1.322443989608400816 ) ) ;
#42248 = CARTESIAN_POINT ( 'NONE',  ( 18.27458182272990328, -2.390008000232556107, 12.37125705564431932 ) ) ;
#42249 = ORIENTED_EDGE ( 'NONE', *, *, #3685, .T. ) ;
#42250 = ORIENTED_EDGE ( 'NONE', *, *, #7970, .T. ) ;
#42251 = EDGE_CURVE ( 'NONE', #23464, #68105, #28393, .T. ) ;
#42252 = AXIS2_PLACEMENT_3D ( 'NONE', #7386, #45495, #1455 ) ;
#42253 = DIRECTION ( 'NONE',  ( 1.000000000000000000, 0.000000000000000000, 0.000000000000000000 ) ) ;
#42254 = CYLINDRICAL_SURFACE ( 'NONE', #45660, 11.65000000000000036 ) ;
#42255 = PLANE ( 'NONE',  #41707 ) ;
#42256 = CARTESIAN_POINT ( 'NONE',  ( 10.79839886931999970, 5.269366011605000288, -6.148705891248999578 ) ) ;
#42257 = CARTESIAN_POINT ( 'NONE',  ( 23.56665676678100141, -10.37811504717999966, -9.381458738969000066 ) ) ;
#42258 = CARTESIAN_POINT ( 'NONE',  ( 25.60000000000000142, 0.000000000000000000, 0.000000000000000000 ) ) ;
#42259 = CARTESIAN_POINT ( 'NONE',  ( 7.920378813398999185, 2.912874113511002783, -6.463705393502997332 ) ) ;
#42260 = AXIS2_PLACEMENT_3D ( 'NONE', #14641, #2774, #35958 ) ;
#42261 = CARTESIAN_POINT ( 'NONE',  ( 10.81315553411000074, 3.756074350075000012, 6.071610008629000355 ) ) ;
#42262 = ORIENTED_EDGE ( 'NONE', *, *, #19990, .F. ) ;
#42263 = CARTESIAN_POINT ( 'NONE',  ( 10.12544718489496098, -5.350147103445326735, -7.676667778836361755 ) ) ;
#42264 = ORIENTED_EDGE ( 'NONE', *, *, #11585, .T. ) ;
#42265 = CARTESIAN_POINT ( 'NONE',  ( 12.29572644340314724, -2.862796356722884461, 12.35963739789472626 ) ) ;
#42266 = CARTESIAN_POINT ( 'NONE',  ( 9.019772138681998896, -4.322628849750500102, -6.695252480703800302 ) ) ;
#42267 = CARTESIAN_POINT ( 'NONE',  ( 9.966324641169999055, 2.303991951421000106, 6.575630951545000435 ) ) ;
#42268 = CARTESIAN_POINT ( 'NONE',  ( 11.48656920625009903, -3.967932847735990531, 8.391549386185598536 ) ) ;
#42269 = CARTESIAN_POINT ( 'NONE',  ( 7.201087902152560005, 0.7854182645431827536, 0.9439803561485179406 ) ) ;
#42270 = CARTESIAN_POINT ( 'NONE',  ( 11.63825819896753977, 3.148796120250299868, -7.660469764776300039 ) ) ;
#42271 = CARTESIAN_POINT ( 'NONE',  ( 10.17349413291699811, 5.162701151235999930, -6.969488574374499201 ) ) ;
#42272 = CARTESIAN_POINT ( 'NONE',  ( 12.52804317529070133, -0.5603556898929450414, 12.68335562943300232 ) ) ;
#42273 = CARTESIAN_POINT ( 'NONE',  ( 8.303477656456466960, 3.015375792701138646, -8.459897655016847651 ) ) ;
#42274 = CARTESIAN_POINT ( 'NONE',  ( 12.80505043854144276, 0.6249999999999994449, -13.88107975066922428 ) ) ;
#42275 = CARTESIAN_POINT ( 'NONE',  ( 9.218006583692512024, -2.655300810998681982, 7.619131915109693232 ) ) ;
#42276 = ADVANCED_FACE ( 'NONE', ( #25427 ), #14261, .T. ) ;
#42277 = ORIENTED_EDGE ( 'NONE', *, *, #9596, .T. ) ;
#42278 = CARTESIAN_POINT ( 'NONE',  ( 5.700000000000000178, 12.50865771883999855, -2.924687089724999911 ) ) ;
#42279 = CARTESIAN_POINT ( 'NONE',  ( 7.127955114086000243, 0.8827681146003000245, 0.7092679259177999684 ) ) ;
#42280 = CARTESIAN_POINT ( 'NONE',  ( 8.924662153698969647, 5.350575487761837223, 7.500021879703680838 ) ) ;
#42281 = DIRECTION ( 'NONE',  ( 1.000000000000000000, 0.000000000000000000, 0.000000000000000000 ) ) ;
#42282 = APPLICATION_CONTEXT ( 'automotive_design' ) ;
#42283 = CARTESIAN_POINT ( 'NONE',  ( 24.61098151538899970, 8.751788807388999558, -9.056922189400999912 ) ) ;
#42284 = CARTESIAN_POINT ( 'NONE',  ( 10.84226088462129844, -3.997572771977982775, -6.359261544073000039 ) ) ;
#42285 = ORIENTED_EDGE ( 'NONE', *, *, #54256, .T. ) ;
#42286 = CARTESIAN_POINT ( 'NONE',  ( 5.630600923344347919, -12.10404814139707419, 3.742416328825248328 ) ) ;
#42287 = CARTESIAN_POINT ( 'NONE',  ( 13.70009528508592211, 8.955766972928957514, 7.451364690503321953 ) ) ;
#42288 = CONICAL_SURFACE ( 'NONE', #12140, 3.249989426617000188, 0.7853950157668545540 ) ;
#42291 = CARTESIAN_POINT ( 'NONE',  ( 11.44437913529000106, 3.868861692926000462, -11.85573592760000139 ) ) ;
#42290 = CARTESIAN_POINT ( 'NONE',  ( 9.857857008493319029, 3.288333712785679541, 9.125423578030003924 ) ) ;
#42289 = UNCERTAINTY_MEASURE_WITH_UNIT (LENGTH_MEASURE( 1.000000000000000082E-05 ), #24874, 'distance_accuracy_value', 'NONE');
#42292 = CARTESIAN_POINT ( 'NONE',  ( 11.09999999999999964, -4.000000000000000000, 7.500000000000000000 ) ) ;
#42293 = ORIENTED_EDGE ( 'NONE', *, *, #68898, .F. ) ;
#42294 = B_SPLINE_CURVE_WITH_KNOTS ( 'NONE', 3,
 ( #6901, #43978, #2015, #55148 ),
 .UNSPECIFIED., .F., .F.,
 ( 4, 4 ),
 ( 0.000000000000000000, 1.000000000000000000 ),
 .UNSPECIFIED. ) ;
#42295 = CARTESIAN_POINT ( 'NONE',  ( 9.590596677641999079, 2.445964682955000136, 7.841184989245001624 ) ) ;
#42297 = CARTESIAN_POINT ( 'NONE',  ( 18.15864108120893050, -2.662504769557529904, -13.63760133890561121 ) ) ;
#42296 = AXIS2_PLACEMENT_3D ( 'NONE', #17156, #65395, #44445 ) ;
#42298 = CARTESIAN_POINT ( 'NONE',  ( 10.50595525820100029, 3.918212119278319694, 8.362327856951900173 ) ) ;
#42299 = CARTESIAN_POINT ( 'NONE',  ( 10.97843137008999825, -5.235400103863000254, 6.782920672145000829 ) ) ;
#42300 = CARTESIAN_POINT ( 'NONE',  ( 7.058516392956000196, -4.314043295739000250, 8.819145559946001356 ) ) ;
#42301 = ORIENTED_EDGE ( 'NONE', *, *, #68357, .F. ) ;
#42302 = CARTESIAN_POINT ( 'NONE',  ( 8.700642219592999993, 5.212261578733999201, 6.157186134061999994 ) ) ;
#42304 = CARTESIAN_POINT ( 'NONE',  ( 10.15335805961999860, -3.144986649008000068, -5.860958514434000399 ) ) ;
#42303 = CARTESIAN_POINT ( 'NONE',  ( 10.99375810342578141, 4.001859925960030928, -6.625879789168364731 ) ) ;
#42305 = CARTESIAN_POINT ( 'NONE',  ( 7.466089535749324213, -2.297169363456695201, 7.143273799371222310 ) ) ;
#42306 = CYLINDRICAL_SURFACE ( 'NONE', #38139, 1.500000000000001110 ) ;
#42307 = CARTESIAN_POINT ( 'NONE',  ( 1.595428564794000081, -2.727979478513999911, -1.783091295463999915 ) ) ;
#42308 = ORIENTED_EDGE ( 'NONE', *, *, #50321, .F. ) ;
#42309 = CARTESIAN_POINT ( 'NONE',  ( 5.740443173016667622, 0.1963495408493638184, -1.499999999999999778 ) ) ;
#42310 = CARTESIAN_POINT ( 'NONE',  ( 10.90333997687999990, -3.786145554879500441, 8.480416814141699788 ) ) ;
#42311 = CARTESIAN_POINT ( 'NONE',  ( 11.05935155529000014, 2.480238120735000162, 6.610075178640000715 ) ) ;
#42312 = CARTESIAN_POINT ( 'NONE',  ( 11.48225819896749833, 2.879005208331999910, 7.288668995979000087 ) ) ;
#42313 = ORIENTED_EDGE ( 'NONE', *, *, #41059, .F. ) ;
#42314 = B_SPLINE_SURFACE_WITH_KNOTS ( 'NONE', 1, 3, ( 
 ( #58984, #45830, #48148, #37309, #26830, #42903, #47120, #10049, #37652, #64208, #29773, #68769, #26138, #67142, #51078, #20887, #19253, #31386, #40580, #3512, #42223, #68421, #47464, #41867, #15642, #20543, #63174, #15302, #36628, #57951, #49871, #28559, #64897, #17010, #12469, #11085, #44646, #43946, #49178, #22259, #22947, #33802, #1289, #48494, #54769, #33454, #64553, #16668, #946, #17722, #59320, #55119, #12125, #38694, #65250, #6523, #49520, #6870, #28206, #1634, #17366, #21908, #22602, #44303, #18064, #60015, #43599, #1984, #23306, #65598, #39045, #32761, #65938, #39383, #598, #60361, #32420, #7222, #53735, #43246, #5833, #27171, #27868, #37993, #11419, #54075 ),
 ( #6171, #27513, #48838, #38339, #59669, #11765, #33109, #54423, #29947, #34501, #23991, #23644, #44981, #55814, #2323, #19430, #61731, #66636, #7916, #13852, #45326, #30279, #13516, #29254, #24681, #28916, #56148, #60704, #55466, #34837, #8256, #19082, #56842, #8940, #66974, #34147, #7562, #40409, #51584, #35180, #46001, #51250, #67652, #3677, #66286, #29604, #12822, #50221, #56492, #18411, #40754, #25019, #46351, #8597, #39736, #3345, #61054, #13173, #50906, #2663, #19776, #18754, #40086, #14193, #50563, #61395, #67312, #62076, #3004, #24336, #45668, #35520, #5413, #58208, #5065, #47383, #57172, #30610, #47035, #57508, #58547, #15898, #36540, #68688, #63090, #25359 ) ),
 .UNSPECIFIED., .F., .F., .F.,
 ( 2, 2 ),
 ( 4, 2, 2, 2, 2, 2, 2, 2, 2, 2, 2, 2, 2, 2, 2, 2, 2, 2, 2, 2, 2, 2, 2, 2, 2, 2, 2, 2, 2, 2, 2, 2, 2, 2, 2, 2, 2, 2, 2, 2, 2, 2, 4 ),
 ( 0.000000000000000000, 1.000000000000000000 ),
 ( 0.000000000000000000, 7.083094307561129462E-05, 0.0001416618861512225892, 0.0002124928292268338974, 0.0002833237723024451785, 0.0003541547153780564595, 0.0004249856584536677948, 0.0004958166015292791301, 0.0005666475446048903570, 0.0006374784876805015838, 0.0007083094307561129191, 0.0007791403738317242544, 0.0008145558453695299220, 0.0008499713169073355896, 0.0008853867884451412573, 0.0009208022599829469249, 0.0009916332030585582602, 0.001027048674596363819, 0.001062464146134169379, 0.001097879617671975155, 0.001133295089209780714, 0.001204126032285392049, 0.001239541503823197608, 0.001274956975361003168, 0.001310372446898808944, 0.001345787918436614503, 0.001416618861512225838, 0.001487449804587837173, 0.001522865276125642733, 0.001558280747663448509, 0.001629111690739059844, 0.001699942633814671179, 0.001735358105352476955, 0.001770773576890282515, 0.001806189048428088074, 0.001841604519965893850, 0.001912435463041505185, 0.001983266406117116520, 0.002018681877654922296, 0.002054097349192727639, 0.002124928292268338757, 0.002195759235343950309, 0.002266590178419561428 ),
 .UNSPECIFIED. ) ;
#42315 = CARTESIAN_POINT ( 'NONE',  ( 23.98813733208841015, -3.345690714576619040, 12.76941329706537331 ) ) ;
#42316 = CARTESIAN_POINT ( 'NONE',  ( 12.29727795756345365, 1.966522083383872799, -12.44559612467660514 ) ) ;
#42317 = EDGE_CURVE ( 'NONE', #34701, #1963, #9682, .T. ) ;
#42318 = CARTESIAN_POINT ( 'NONE',  ( 11.84523293495530005, -5.315205473512000012, 7.552870914315270134 ) ) ;
#42319 = ADVANCED_FACE ( 'NONE', ( #9000 ), #10031, .T. ) ;
#42320 = CARTESIAN_POINT ( 'NONE',  ( 25.40241773096400024, -3.096370345990000494, -11.38623249034000118 ) ) ;
#42321 = CARTESIAN_POINT ( 'NONE',  ( 18.27991844657871212, -2.543687620403382255, 13.76699789025506071 ) ) ;
#42322 = CARTESIAN_POINT ( 'NONE',  ( 7.100000000000000533, 13.94845324556000143, 4.312847325879000770 ) ) ;
#42323 = ORIENTED_EDGE ( 'NONE', *, *, #41136, .T. ) ;
#42324 = CARTESIAN_POINT ( 'NONE',  ( 15.61911349846912067, -9.449623925635307842, -8.220739594291174512 ) ) ;
#42325 = CARTESIAN_POINT ( 'NONE',  ( 23.56664675778400309, 10.37811020278999941, -9.381454169592000625 ) ) ;
#42326 = ORIENTED_EDGE ( 'NONE', *, *, #29687, .F. ) ;
#42327 = CARTESIAN_POINT ( 'NONE',  ( 11.75718044953559804, 4.889766368533900120, 7.036033215662999218 ) ) ;
#42328 = DIRECTION ( 'NONE',  ( -1.000000000000000000, 6.086974017450460374E-15, -6.313390726318450536E-15 ) ) ;
#42329 = CARTESIAN_POINT ( 'NONE',  ( 10.02799997617999850, 3.452028386838999818, -6.074524158096999749 ) ) ;
#42330 = CARTESIAN_POINT ( 'NONE',  ( 7.927339924271998406, 4.618926574321004175, 6.298803404070997480 ) ) ;
#42331 = CARTESIAN_POINT ( 'NONE',  ( 10.16829915263999951, -4.567213659083999566, 5.832528837986999726 ) ) ;
#42332 = CARTESIAN_POINT ( 'NONE',  ( 17.84068610406497868, 0.5560043133243454117, -12.68361349193355103 ) ) ;
#42333 = CARTESIAN_POINT ( 'NONE',  ( 9.008372914924125396, 5.237369076955197045, 8.039691865988411124 ) ) ;
#42334 = CARTESIAN_POINT ( 'NONE',  ( 10.40333997687999990, -3.786145554879500441, -6.519583185858300212 ) ) ;
#42335 = CARTESIAN_POINT ( 'NONE',  ( 7.416892219589999335, 3.448180532882000104, 9.222462917385000125 ) ) ;
#42336 = ORIENTED_EDGE ( 'NONE', *, *, #40041, .F. ) ;
#42337 = EDGE_CURVE ( 'NONE', #5820, #58325, #35084, .T. ) ;
#42338 = FILL_AREA_STYLE ('',( #17 ) ) ;
#42339 = CARTESIAN_POINT ( 'NONE',  ( 11.09999999999999964, 2.700000000000000178, -6.461133846875999787 ) ) ;
#42340 = CARTESIAN_POINT ( 'NONE',  ( 11.87299956498129916, -5.207010770456999893, 7.825000000000000178 ) ) ;
#42341 = CARTESIAN_POINT ( 'NONE',  ( 10.34184687351645771, -4.999583552997724389, -6.731816600031354625 ) ) ;
#42342 = EDGE_CURVE ( 'NONE', #65237, #61230, #18361, .T. ) ;
#42343 = CARTESIAN_POINT ( 'NONE',  ( 11.86854277327999085, 9.759924522331001384, 5.704691307148000767 ) ) ;
#42344 = CARTESIAN_POINT ( 'NONE',  ( 7.717918984469999799, -2.852331559125000027, 6.784354950350999225 ) ) ;
#42345 = CARTESIAN_POINT ( 'NONE',  ( 11.14445611883999909, 10.08446449122000033, 5.720378117617999969 ) ) ;
#42346 = AXIS2_PLACEMENT_3D ( 'NONE', #57224, #29659, #63149 ) ;
#42347 = DIRECTION ( 'NONE',  ( 0.000000000000000000, -0.2461538461537955136, 0.9692307692307821076 ) ) ;
#42348 = CARTESIAN_POINT ( 'NONE',  ( 9.217397846562217723, -4.245312990446880264, 6.659228100213050006 ) ) ;
#42349 = VERTEX_POINT ( 'NONE', #57578 ) ;
#42350 = CARTESIAN_POINT ( 'NONE',  ( 12.56405804856029995, -1.801709437036785433, 12.47051912880706226 ) ) ;
#42351 = CARTESIAN_POINT ( 'NONE',  ( 9.760355082327999199, -4.572497688003699601, -6.356045986629998978 ) ) ;
#42352 = CARTESIAN_POINT ( 'NONE',  ( 11.50001258332000020, 11.56502147876000031, 1.404302031979000054 ) ) ;
#42353 = DIRECTION ( 'NONE',  ( -1.000000000000000000, 0.000000000000000000, 0.000000000000000000 ) ) ;
#42354 = CARTESIAN_POINT ( 'NONE',  ( 12.21210404293059959, -4.381818659177399766, 6.722495590581700320 ) ) ;
#42355 = CARTESIAN_POINT ( 'NONE',  ( 8.698396402458998367, 3.630894432589700127, 6.701746336527099501 ) ) ;
#42356 = CARTESIAN_POINT ( 'NONE',  ( 0.6557558238970999653, -0.7435038563603999506, -3.122230671987999973 ) ) ;
#42357 = CARTESIAN_POINT ( 'NONE',  ( 4.813605073191808970, -1.173669780889472936, 0.2426414077541297898 ) ) ;
#42358 = CARTESIAN_POINT ( 'NONE',  ( 12.10480575880360909, 2.667436721895840801, 12.31441907085212151 ) ) ;
#42359 = CARTESIAN_POINT ( 'NONE',  ( 8.949822372493999367, 3.632306086542600010, -8.702849744394999476 ) ) ;
#42360 = CARTESIAN_POINT ( 'NONE',  ( 11.51102763632551884, 3.088851714329700293, -7.079572058049399708 ) ) ;
#42361 = CARTESIAN_POINT ( 'NONE',  ( 8.224593659958996383, 3.074059020428998146, -6.140725432342995838 ) ) ;
#42362 = CARTESIAN_POINT ( 'NONE',  ( 10.73615471958999912, 3.078044734341000233, -6.088740491863000592 ) ) ;
#42363 = CARTESIAN_POINT ( 'NONE',  ( 9.985242056249999720, 3.541248877825399877, -8.694123841252999085 ) ) ;
#42365 = CARTESIAN_POINT ( 'NONE',  ( 12.22117151670427226, 2.723004125123300589, 12.39680780184485975 ) ) ;
#42364 = LINE ( 'NONE', #42015, #36358 ) ;
#42366 = CARTESIAN_POINT ( 'NONE',  ( 8.973567925431344960, 5.349887660206418261, 7.470588186270433972 ) ) ;
#42367 = ORIENTED_EDGE ( 'NONE', *, *, #41275, .T. ) ;
#42368 = CARTESIAN_POINT ( 'NONE',  ( 12.60523857549420690, 0.5937411427826001509, 12.68132466675082348 ) ) ;
#42369 = CARTESIAN_POINT ( 'NONE',  ( 9.457462135716001583, -5.100000000000000533, -6.571291218949999902 ) ) ;
#42370 = CARTESIAN_POINT ( 'NONE',  ( 9.696086916451999826, -2.554404004330999900, 7.600685922079000179 ) ) ;
#42371 = CARTESIAN_POINT ( 'NONE',  ( 9.325734463322998380, 4.104624583183299258, 6.501052555474699624 ) ) ;
#42372 = CARTESIAN_POINT ( 'NONE',  ( 23.56681659734730871, -2.990540295753150613, -13.66657933901271349 ) ) ;
#42373 = CARTESIAN_POINT ( 'NONE',  ( 12.25820678327527347, -2.802802780256933080, 13.60456178155848406 ) ) ;
#42374 = CARTESIAN_POINT ( 'NONE',  ( 12.17999101424761577, 2.480063841773443301, 13.67763837793895298 ) ) ;
#42375 = CARTESIAN_POINT ( 'NONE',  ( 8.199995020667000034, 2.894508905068999827, 6.645190348705000360 ) ) ;
#42376 = ORIENTED_EDGE ( 'NONE', *, *, #44054, .T. ) ;
#42377 = CARTESIAN_POINT ( 'NONE',  ( 4.705906265422999724, 1.004282239496999907, 0.7862521424935998704 ) ) ;
#42378 = CARTESIAN_POINT ( 'NONE',  ( 8.490822372493999737, -4.367693913457399546, -8.702849744394999476 ) ) ;
#42379 = CARTESIAN_POINT ( 'NONE',  ( 24.84554641417578225, 3.513976416300454542, 11.93643034843086070 ) ) ;
#42380 = CARTESIAN_POINT ( 'NONE',  ( 10.93769853197999886, 5.063116524846000388, -4.920828787216999345 ) ) ;
#42381 = CARTESIAN_POINT ( 'NONE',  ( 18.14833460798322307, 2.303170370814867862, -12.49527837666172125 ) ) ;
#42382 = CARTESIAN_POINT ( 'NONE',  ( 9.732128830620874638, -4.207195853723359136, 8.743003876391233220 ) ) ;
#42383 = CARTESIAN_POINT ( 'NONE',  ( 18.17924748727732620, 2.534358940238659486, 12.44349985642685041 ) ) ;
#42384 = LINE ( 'NONE', #5311, #47996 ) ;
#42385 = CARTESIAN_POINT ( 'NONE',  ( 10.75915805961999894, -5.387268372866000021, -6.278119777966000292 ) ) ;
#42386 = CARTESIAN_POINT ( 'NONE',  ( 12.61333915116789051, 3.228660600395449887, 13.62267210748412616 ) ) ;
#42387 = CARTESIAN_POINT ( 'NONE',  ( 11.49999035076000276, -3.886252136122000156, 11.90689009355000039 ) ) ;
#42388 = CARTESIAN_POINT ( 'NONE',  ( 24.72544608131600086, 12.30754379070000049, 2.942921080080999729 ) ) ;
#42389 = EDGE_CURVE ( 'NONE', #65308, #3801, #57707, .T. ) ;
#42390 = CARTESIAN_POINT ( 'NONE',  ( 11.09999987043000047, 10.03015713885000082, 5.726993666320999488 ) ) ;
#42391 = EDGE_CURVE ( 'NONE', #52849, #46074, #5816, .T. ) ;
#42392 = CARTESIAN_POINT ( 'NONE',  ( 5.000000000000000000, -11.29999999999999893, 0.000000000000000000 ) ) ;
#42393 = EDGE_LOOP ( 'NONE', ( #14501, #49803, #49254, #25700, #15215, #34799, #29576, #66382, #15636, #15223, #53258, #17691 ) ) ;
#42394 = CARTESIAN_POINT ( 'NONE',  ( 8.555820280412000045, 2.414630869937000046, -6.801495146585999407 ) ) ;
#42395 = CARTESIAN_POINT ( 'NONE',  ( 11.47364560330029981, -3.734560974198899874, 8.324524538096799375 ) ) ;
#42396 = ORIENTED_EDGE ( 'NONE', *, *, #38346, .T. ) ;
#42397 = CARTESIAN_POINT ( 'NONE',  ( 7.900104261408000816, 3.351183067932000270, -6.316134894229000096 ) ) ;
#42398 = CARTESIAN_POINT ( 'NONE',  ( 10.42380110216399913, -4.973546009874400653, -6.905442784147899360 ) ) ;
#42399 = VERTEX_POINT ( 'NONE', #58965 ) ;
#42400 = DIRECTION ( 'NONE',  ( 1.000000000000000000, 0.000000000000000000, 0.000000000000000000 ) ) ;
#42401 = CARTESIAN_POINT ( 'NONE',  ( 9.093935841232999806, 2.156584729807999867, -7.959751745006000689 ) ) ;
#42402 = CARTESIAN_POINT ( 'NONE',  ( 18.23887202961200060, -3.252214874110999965, 11.14733497513999971 ) ) ;
#42403 = CARTESIAN_POINT ( 'NONE',  ( 13.99999999485600277, -9.471999751521998689, -8.194948195317001804 ) ) ;
#42404 = CARTESIAN_POINT ( 'NONE',  ( 12.42592716733844860, 0.4969868315108272316, -13.88804154506775923 ) ) ;
#42405 = DIRECTION ( 'NONE',  ( 0.000000000000000000, 1.000000000000000000, 0.000000000000000000 ) ) ;
#42406 = LINE ( 'NONE', #15826, #47441 ) ;
#42407 = ORIENTED_EDGE ( 'NONE', *, *, #8748, .F. ) ;
#42408 = CARTESIAN_POINT ( 'NONE',  ( 10.16426084122999995, 4.808846957865000604, -8.639578604182998944 ) ) ;
#42409 = ORIENTED_EDGE ( 'NONE', *, *, #25570, .F. ) ;
#42410 = VECTOR ( 'NONE', #52869, 1000.000000000000114 ) ;
#42411 = CARTESIAN_POINT ( 'NONE',  ( 10.84184687351628540, 3.000416447002276943, -6.731816600031354625 ) ) ;
#42412 = ORIENTED_EDGE ( 'NONE', *, *, #20514, .F. ) ;
#42413 = CARTESIAN_POINT ( 'NONE',  ( 8.896088727410999653, 2.725263018055000153, 7.393088754863899936 ) ) ;
#42414 = CARTESIAN_POINT ( 'NONE',  ( 17.65867742935362728, -3.116692472806303904, -12.28625815163619883 ) ) ;
#42415 = ADVANCED_FACE ( 'NONE', ( #65233 ), #11895, .T. ) ;
#42416 = CARTESIAN_POINT ( 'NONE',  ( 18.02663564786298522, 11.82897200926889347, -3.432444815763982415 ) ) ;
#42417 = CARTESIAN_POINT ( 'NONE',  ( 18.17241432537605306, -2.400344151260349168, -12.47423995686379072 ) ) ;
#42418 = CARTESIAN_POINT ( 'NONE',  ( 12.54664124763763944, 0.5694488842926255234, 13.88429844810378277 ) ) ;
#42419 = VERTEX_POINT ( 'NONE', #1616 ) ;
#42420 = CARTESIAN_POINT ( 'NONE',  ( 12.65912070212100105, 11.49976653515000002, -4.814127980893999847 ) ) ;
#42421 = CARTESIAN_POINT ( 'NONE',  ( 18.21444431150800014, 11.56145208044000050, -4.416819796118000241 ) ) ;
#42422 = LINE ( 'NONE', #42761, #2852 ) ;
#42423 = LINE ( 'NONE', #36836, #66254 ) ;
#42424 = CARTESIAN_POINT ( 'NONE',  ( 8.848264158775000610, 5.751585344281000545, -8.235867044345999588 ) ) ;
#42425 = CARTESIAN_POINT ( 'NONE',  ( 18.31587707750999883, -3.089759977613000252, 11.98885651319999823 ) ) ;
#42426 = CARTESIAN_POINT ( 'NONE',  ( 10.46009514222999925, -2.565650894080999667, -6.975682682930000489 ) ) ;
#42427 = VERTEX_POINT ( 'NONE', #22932 ) ;
#42428 = ORIENTED_EDGE ( 'NONE', *, *, #47046, .T. ) ;
#42429 = CARTESIAN_POINT ( 'NONE',  ( 10.95289953139000083, 5.154333551509999722, -5.174586382582000432 ) ) ;
#42430 = CARTESIAN_POINT ( 'NONE',  ( 10.12812406805898036, 4.965061169224918025, -8.480932067564513233 ) ) ;
#42431 = CARTESIAN_POINT ( 'NONE',  ( 8.279780176894341537, -3.802829724692906588, 6.095677100425044515 ) ) ;
#42432 = CARTESIAN_POINT ( 'NONE',  ( 0.1499942179680000265, 0.3599680999394012093, -2.749953718116143531 ) ) ;
#42433 = CARTESIAN_POINT ( 'NONE',  ( 11.59456039236534330, 5.314711678001000195, -7.563984187103470092 ) ) ;
#42434 = CARTESIAN_POINT ( 'NONE',  ( 9.636671671056999955, 3.144964309357700216, -7.643603315539799326 ) ) ;
#42436 = CARTESIAN_POINT ( 'NONE',  ( 10.27121258196999953, -3.420947237194000401, 4.846519661431999637 ) ) ;
#42435 = CARTESIAN_POINT ( 'NONE',  ( 10.91488779216199845, -3.070969952137800441, 7.164969140522200242 ) ) ;
#42437 = CARTESIAN_POINT ( 'NONE',  ( 4.627943173016668688, -0.9218200799623714747, -1.199500263597270466 ) ) ;
#42438 = ORIENTED_EDGE ( 'NONE', *, *, #52353, .T. ) ;
#42439 = PLANE ( 'NONE',  #24685 ) ;
#42440 = CARTESIAN_POINT ( 'NONE',  ( 8.325003570449004187, -2.868532950405002779, 6.316175323229005656 ) ) ;
#42441 = EDGE_CURVE ( 'NONE', #40590, #26260, #6705, .T. ) ;
#42442 = EDGE_CURVE ( 'NONE', #13783, #45966, #43193, .T. ) ;
#42443 = CARTESIAN_POINT ( 'NONE',  ( 9.811013376692999444, 2.859607053196999704, 8.079558723821699928 ) ) ;
#42444 = LINE ( 'NONE', #48030, #50375 ) ;
#42445 = CARTESIAN_POINT ( 'NONE',  ( 9.533427734455999669, -2.564762519363000148, 6.150594768287000136 ) ) ;
#42446 = CARTESIAN_POINT ( 'NONE',  ( 17.55505043854143565, 1.875000000000000000, -12.57545641911172751 ) ) ;
#42447 = CARTESIAN_POINT ( 'NONE',  ( 44.24148000000000280, -2.258942858049999725, 12.29419282279000036 ) ) ;
#42448 = CARTESIAN_POINT ( 'NONE',  ( 14.03176826122700227, 8.820984799833000878, 7.691098505213000536 ) ) ;
#42449 = B_SPLINE_CURVE_WITH_KNOTS ( 'NONE', 3,
 ( #9388, #639, #32799, #22297 ),
 .UNSPECIFIED., .F., .F.,
 ( 4, 4 ),
 ( 0.000000000000000000, 1.000000000000000000 ),
 .UNSPECIFIED. ) ;
#42450 = DIRECTION ( 'NONE',  ( 0.000000000000000000, 1.000000000000000000, 0.000000000000000000 ) ) ;
#42451 = CARTESIAN_POINT ( 'NONE',  ( 9.307392757686999474, -3.414780058706799792, -8.139707405630899117 ) ) ;
#42452 = CARTESIAN_POINT ( 'NONE',  ( 6.031018102971001049, 1.262548346495000029, 0.3929982786279000440 ) ) ;
#42453 = B_SPLINE_SURFACE_WITH_KNOTS ( 'NONE', 3, 3, ( 
 ( #25783, #58282, #31724, #47114 ),
 ( #26131, #37647, #48143, #36968 ),
 ( #69116, #10727, #53390, #57945 ),
 ( #53729, #48487, #593, #58626 ),
 ( #5828, #20882, #27165, #68414 ),
 ( #42218, #42553, #16662, #10041 ),
 ( #20536, #41861, #31380, #52692 ),
 ( #63523, #15976, #10385, #6518 ),
 ( #40660, #1628, #17005, #33101 ) ),
 .UNSPECIFIED., .F., .F., .F.,
 ( 4, 1, 1, 1, 1, 1, 4 ),
 ( 4, 4 ),
 ( 0.05214259105101000380, 0.1666666666667000196, 0.3333333333333000081, 0.5000000000000000000, 0.6666666666667000474, 0.8333333333333000637, 0.9777068595523999983 ),
 ( -0.1900882580235000174, 1.190231865545000156 ),
 .UNSPECIFIED. ) ;
#42454 = CARTESIAN_POINT ( 'NONE',  ( 6.999999999999999112, 9.045785485369089329, -4.691862879246641249 ) ) ;
#42455 = CARTESIAN_POINT ( 'NONE',  ( 17.55505043854143565, 3.199698446519375850, 12.18695736643652694 ) ) ;
#42456 = FACE_OUTER_BOUND ( 'NONE', #9668, .T. ) ;
#42457 = EDGE_LOOP ( 'NONE', ( #370, #33110, #5894, #2666 ) ) ;
#42458 = CARTESIAN_POINT ( 'NONE',  ( 12.37008254743958169, 0.4489258298041860495, -12.68932177688765606 ) ) ;
#42459 = CARTESIAN_POINT ( 'NONE',  ( 23.59999176271200128, 13.22318677037999812, 4.267778497637999102 ) ) ;
#42460 = LINE ( 'NONE', #10635, #6337 ) ;
#42461 = DIRECTION ( 'NONE',  ( 0.000000000000000000, 1.000000000000000000, 0.000000000000000000 ) ) ;
#42462 = CARTESIAN_POINT ( 'NONE',  ( 3.500000000000000444, 0.1535256407529738132, 3.288177470438649053 ) ) ;
#42463 = ORIENTED_EDGE ( 'NONE', *, *, #14550, .F. ) ;
#42464 = CARTESIAN_POINT ( 'NONE',  ( 5.291478153344000290, -1.078708783361999934, 0.4686457328678000356 ) ) ;
#42465 = ITEM_DEFINED_TRANSFORMATION ( 'NONE', 'NONE', #67527,  #9676 ) ;
#42466 = CARTESIAN_POINT ( 'NONE',  ( 11.59603632436369125, -4.842640371965599932, -7.303218851299499548 ) ) ;
#42467 = EDGE_CURVE ( 'NONE', #4, #47991, #1874, .T. ) ;
#42468 = CARTESIAN_POINT ( 'NONE',  ( 24.69898681705700128, -8.733955352176000275, -9.243040794412999972 ) ) ;
#42469 = CARTESIAN_POINT ( 'NONE',  ( 10.52101354018262391, -3.231816600031356845, 6.500416447002272946 ) ) ;
#42470 = CARTESIAN_POINT ( 'NONE',  ( 7.662253596345666828, 4.464690838466052192, -8.784472088508959331 ) ) ;
#42471 = CARTESIAN_POINT ( 'NONE',  ( 12.99403162610500040, 12.11619719077999946, 2.031914795679000019 ) ) ;
#42472 = VERTEX_POINT ( 'NONE', #17348 ) ;
#42473 = EDGE_CURVE ( 'NONE', #9350, #11696, #44313, .T. ) ;
#42474 = CARTESIAN_POINT ( 'NONE',  ( 9.409421956854998825, -2.113407700033000047, 7.914197133433000353 ) ) ;
#42475 = CARTESIAN_POINT ( 'NONE',  ( 17.83374359992749447, 3.059519611938945172, -13.53873550554769345 ) ) ;
#42476 = ORIENTED_EDGE ( 'NONE', *, *, #38255, .F. ) ;
#42477 = CARTESIAN_POINT ( 'NONE',  ( 13.61451884198527829, 11.47057857663811653, 2.038550092597725794 ) ) ;
#42478 = CARTESIAN_POINT ( 'NONE',  ( 7.583058059622000080, -4.763531818439999732, 5.668890958491999754 ) ) ;
#42479 = DIRECTION ( 'NONE',  ( 1.000000000000000000, 0.000000000000000000, 0.000000000000000000 ) ) ;
#42480 = ORIENTED_EDGE ( 'NONE', *, *, #7092, .F. ) ;
#42481 = CARTESIAN_POINT ( 'NONE',  ( 4.074968078372999791, 0.000000000000000000, 0.000000000000000000 ) ) ;
#42482 = CARTESIAN_POINT ( 'NONE',  ( 7.315310841225000082, 5.563598295091999546, -6.420781807775999717 ) ) ;
#42483 = CARTESIAN_POINT ( 'NONE',  ( 9.489763540183334456, -3.672815144550900524, -8.717465845835395299 ) ) ;
#42484 = CARTESIAN_POINT ( 'NONE',  ( 7.292138728207834930, 3.170712126231089112, -8.579042257717643949 ) ) ;
#42485 = ORIENTED_EDGE ( 'NONE', *, *, #1093, .T. ) ;
#42486 = CARTESIAN_POINT ( 'NONE',  ( 10.87021507563000000, -2.226042145532000305, 7.782753277595999997 ) ) ;
#42487 = CARTESIAN_POINT ( 'NONE',  ( 24.95780622180999941, 12.04100287684999948, -2.875622496761999880 ) ) ;
#42488 = CARTESIAN_POINT ( 'NONE',  ( 21.72233714749290101, -1.140832415794000035E-13, 6.000000000000000000 ) ) ;
#42489 = VERTEX_POINT ( 'NONE', #37631 ) ;
#42490 = CARTESIAN_POINT ( 'NONE',  ( 6.138359839683334762, -0.7554284705563483193, -1.310679582531387721 ) ) ;
#42491 = B_SPLINE_CURVE_WITH_KNOTS ( 'NONE', 3,
 ( #14043, #35372, #3874, #57357 ),
 .UNSPECIFIED., .F., .F.,
 ( 4, 4 ),
 ( 0.000000000000000000, 1.000000000000000000 ),
 .UNSPECIFIED. ) ;
#42492 = ORIENTED_EDGE ( 'NONE', *, *, #62120, .T. ) ;
#42493 = CARTESIAN_POINT ( 'NONE',  ( 23.57704543710643463, -10.25518402361791814, 9.510250455292135641 ) ) ;
#42494 = CARTESIAN_POINT ( 'NONE',  ( 17.94097423839755479, -1.871151600930998748, -12.46029012432409466 ) ) ;
#42495 = DIRECTION ( 'NONE',  ( 0.000000000000000000, 0.3118250626419980520, -0.9501395320205942019 ) ) ;
#42496 = EDGE_CURVE ( 'NONE', #56231, #47849, #898, .T. ) ;
#42497 = AXIS2_PLACEMENT_3D ( 'NONE', #17490, #22377, #5950 ) ;
#42498 = CARTESIAN_POINT ( 'NONE',  ( 11.60000000000000320, 3.359735910920770063, -6.808168915892151674 ) ) ;
#42499 = DIRECTION ( 'NONE',  ( -1.000000000000000000, 0.000000000000000000, 0.000000000000000000 ) ) ;
#42500 = DIRECTION ( 'NONE',  ( -1.000000000000000000, 0.000000000000000000, 0.000000000000000000 ) ) ;
#42501 = FACE_OUTER_BOUND ( 'NONE', #32746, .T. ) ;
#42502 = ORIENTED_EDGE ( 'NONE', *, *, #12479, .T. ) ;
#42503 = CARTESIAN_POINT ( 'NONE',  ( 10.86190547754509872, -3.108323067758099967, -7.528299448264639260 ) ) ;
#42504 = EDGE_LOOP ( 'NONE', ( #17245, #21562, #25095, #19504, #66287 ) ) ;
#42505 = CARTESIAN_POINT ( 'NONE',  ( 9.576488281553999116, 4.593976206186999534, 5.662041230125000268 ) ) ;
#42506 = CARTESIAN_POINT ( 'NONE',  ( 10.49411415877000131, 2.866942652264999669, -8.960728730887002058 ) ) ;
#42507 = AXIS2_PLACEMENT_3D ( 'NONE', #45470, #34987, #39532 ) ;
#42508 = CYLINDRICAL_SURFACE ( 'NONE', #34494, 1.999999999999999556 ) ;
#42509 = CARTESIAN_POINT ( 'NONE',  ( 12.20884949286983279, 2.312191565065523147, -13.71150332431687247 ) ) ;
#42510 = CARTESIAN_POINT ( 'NONE',  ( 1.775000508673000077, 0.000000000000000000, 0.000000000000000000 ) ) ;
#42511 = CARTESIAN_POINT ( 'NONE',  ( 25.59994555223599733, -8.527741194213000142, -7.260611644044000279 ) ) ;
#42512 = CARTESIAN_POINT ( 'NONE',  ( 18.05145975767274535, -0.3802875570022093421, 13.89301034115782940 ) ) ;
#42513 = CARTESIAN_POINT ( 'NONE',  ( 13.69992376746900042, -12.26631831379999937, -2.532779022035999805 ) ) ;
#42514 = ORIENTED_EDGE ( 'NONE', *, *, #24951, .F. ) ;
#42515 = CARTESIAN_POINT ( 'NONE',  ( 17.10000426004115326, 12.52500000000000036, 2.429202523439327966E-10 ) ) ;
#42516 = CARTESIAN_POINT ( 'NONE',  ( 12.00271932425157040, -4.187398418774900044, 6.235801371442999397 ) ) ;
#42517 = CARTESIAN_POINT ( 'NONE',  ( 18.11689869015255994, -0.2739455837727965970, -13.89636968673228878 ) ) ;
#42518 = CARTESIAN_POINT ( 'NONE',  ( 8.592629440379999650, -3.856773448568000084, 5.521258396339000285 ) ) ;
#42520 = DIRECTION ( 'NONE',  ( 0.000000000000000000, 1.000000000000000000, 0.000000000000000000 ) ) ;
#42519 = CARTESIAN_POINT ( 'NONE',  ( 10.06843885510000014, 4.148608506723999945, 8.941445591976998841 ) ) ;
#42521 = CARTESIAN_POINT ( 'NONE',  ( 11.13349010443639919, 5.274453806861999716, -7.595309363461700158 ) ) ;
#42522 = DIRECTION ( 'NONE',  ( -1.000000000000000000, 1.157371756800000045E-14, 1.736057635198999949E-14 ) ) ;
#42523 = CARTESIAN_POINT ( 'NONE',  ( 9.728988259786000015, 3.886559292927400211, -8.359557531806398600 ) ) ;
#42524 = EDGE_CURVE ( 'NONE', #7379, #8238, #2503, .T. ) ;
#42525 = EDGE_CURVE ( 'NONE', #44634, #22260, #68362, .T. ) ;
#42526 = CARTESIAN_POINT ( 'NONE',  ( 17.88507951091365911, -0.5311517451680607405, 12.68505220952105184 ) ) ;
#42527 = CARTESIAN_POINT ( 'NONE',  ( 6.874156308958999873, -1.004440062237000220, -0.5229138879281000074 ) ) ;
#42528 = CARTESIAN_POINT ( 'NONE',  ( 10.90000000000000036, -0.2500000000000000000, 9.776630298829998011 ) ) ;
#42529 = VERTEX_POINT ( 'NONE', #53379 ) ;
#42530 = CARTESIAN_POINT ( 'NONE',  ( 8.341918146793998901, -5.601799093797000140, 7.176147756900999930 ) ) ;
#42531 = CARTESIAN_POINT ( 'NONE',  ( 8.623264158775000965, 5.288433695693000480, -8.041290150997999930 ) ) ;
#42532 = EDGE_CURVE ( 'NONE', #2041, #52805, #40951, .T. ) ;
#42533 = VECTOR ( 'NONE', #20333, 1000.000000000000000 ) ;
#42534 = DIRECTION ( 'NONE',  ( 0.000000000000000000, 0.000000000000000000, -1.000000000000000000 ) ) ;
#42535 = CARTESIAN_POINT ( 'NONE',  ( 10.99284065376417452, 6.341348534417104332, 5.182868225897757419 ) ) ;
#42536 = EDGE_LOOP ( 'NONE', ( #21559, #27922, #41880, #36253 ) ) ;
#42537 = CARTESIAN_POINT ( 'NONE',  ( 0.1565305517722999917, 1.141789477572999978, -2.999605631121999849 ) ) ;
#42538 = CARTESIAN_POINT ( 'NONE',  ( 17.55505043854143565, 3.248147246781390329, 13.61798588129781074 ) ) ;
#42539 = CARTESIAN_POINT ( 'NONE',  ( 2.838475737650000053, -2.711141585093999939, -2.603476249589999458 ) ) ;
#42540 = VERTEX_POINT ( 'NONE', #26815 ) ;
#42541 = CARTESIAN_POINT ( 'NONE',  ( 12.64055030734118645, -0.7009231686363676106, -12.58048995873114073 ) ) ;
#42542 = CARTESIAN_POINT ( 'NONE',  ( 9.136057238048000073, -5.084840204920000772, -6.477689566282000655 ) ) ;
#42543 = CARTESIAN_POINT ( 'NONE',  ( 18.22954180134188817, 2.744780546098122720, -12.29741030561552861 ) ) ;
#42544 = CARTESIAN_POINT ( 'NONE',  ( 10.31021345716899873, 4.636538040886300394, 6.921280946186199934 ) ) ;
#42545 = DIRECTION ( 'NONE',  ( 0.000000000000000000, -1.000000000000000000, 0.000000000000000000 ) ) ;
#42546 = EDGE_LOOP ( 'NONE', ( #42195, #48354, #53383, #57572 ) ) ;
#42547 = CARTESIAN_POINT ( 'NONE',  ( 11.50001496185000249, 11.50879548940379493, -5.112724829163610707 ) ) ;
#42548 = B_SPLINE_CURVE_WITH_KNOTS ( 'NONE', 3,
 ( #19297, #2876, #57046, #61953 ),
 .UNSPECIFIED., .F., .F.,
 ( 4, 4 ),
 ( 0.000000000000000000, 1.000000000000000000 ),
 .UNSPECIFIED. ) ;
#42549 = CARTESIAN_POINT ( 'NONE',  ( 8.204454719587999989, 2.564091104321999826, -6.530737592441999695 ) ) ;
#42550 = CARTESIAN_POINT ( 'NONE',  ( 8.403769448316676716, -2.537713777690222994, 8.442983533627888448 ) ) ;
#42551 = CARTESIAN_POINT ( 'NONE',  ( 9.041480666858999982, -3.573487373903700082, 6.293984733123999753 ) ) ;
#42552 = ORIENTED_EDGE ( 'NONE', *, *, #13301, .F. ) ;
#42553 = CARTESIAN_POINT ( 'NONE',  ( 16.22798078375900133, -3.564332247067999671, -11.94996243427999971 ) ) ;
#42554 = CARTESIAN_POINT ( 'NONE',  ( 6.302943173016666734, 1.199500263597271799, -0.9218200799623701425 ) ) ;
#42555 = VERTEX_POINT ( 'NONE', #43579 ) ;
#42556 = CARTESIAN_POINT ( 'NONE',  ( 12.35703415364444346, 3.053811614356524373, -12.22452321716938251 ) ) ;
#42557 = CARTESIAN_POINT ( 'NONE',  ( 24.69609434945602544, -8.660954285513374984, -8.619379122962911310 ) ) ;
#42558 = CIRCLE ( 'NONE', #10214, 1.249999999999999778 ) ;
#42559 = CARTESIAN_POINT ( 'NONE',  ( 7.974113208588001100, 4.561154361229000642, -6.272154006859000930 ) ) ;
#42560 = ORIENTED_EDGE ( 'NONE', *, *, #62365, .T. ) ;
#42561 = CARTESIAN_POINT ( 'NONE',  ( 11.09999999999999964, -4.000000000000000000, 7.500000000000000000 ) ) ;
#42562 = CARTESIAN_POINT ( 'NONE',  ( 9.961715168003999921, 7.673027129248000122, 5.716196767530000500 ) ) ;
#42563 = CARTESIAN_POINT ( 'NONE',  ( 11.18412378248529926, 3.450971646934100079, -6.461285588983000316 ) ) ;
#42564 = CARTESIAN_POINT ( 'NONE',  ( 12.72186720215634459, 3.119790641632218087, -12.28533200497074063 ) ) ;
#42565 = CARTESIAN_POINT ( 'NONE',  ( 11.31349144726329925, -4.738947899111299655, 8.542723541016000510 ) ) ;
#42566 = ORIENTED_EDGE ( 'NONE', *, *, #25754, .T. ) ;
#42567 = CARTESIAN_POINT ( 'NONE',  ( 8.373670280412000011, 2.202812441249000219, 7.706988150133999405 ) ) ;
#42568 = ORIENTED_EDGE ( 'NONE', *, *, #48924, .F. ) ;
#42569 = CARTESIAN_POINT ( 'NONE',  ( 7.768029383457135673, 2.842467889454252994, 6.805004285200667802 ) ) ;
#42570 = CARTESIAN_POINT ( 'NONE',  ( 11.44571737393082600, -5.011200127299592744, -8.273761053885760219 ) ) ;
#42571 = CARTESIAN_POINT ( 'NONE',  ( 10.96871661479000082, 5.813363305173999684, -4.931850597599000352 ) ) ;
#42572 = ORIENTED_EDGE ( 'NONE', *, *, #50357, .F. ) ;
#42573 = CARTESIAN_POINT ( 'NONE',  ( 12.78420607872188342, -1.875260891907202243, -12.57537395219491749 ) ) ;
#42574 = EDGE_CURVE ( 'NONE', #49213, #1541, #11649, .T. ) ;
#42575 = CARTESIAN_POINT ( 'NONE',  ( 6.343015658241001553, 8.380865186898988739, -3.925761800723999606 ) ) ;
#42576 = CARTESIAN_POINT ( 'NONE',  ( 9.599999931441001166, -2.750000000000000000, 7.500000000000000000 ) ) ;
#42577 = FACE_OUTER_BOUND ( 'NONE', #67839, .T. ) ;
#42578 = CARTESIAN_POINT ( 'NONE',  ( 12.53635786351538606, -1.839692799137185641, -13.87860051966028152 ) ) ;
#42579 = EDGE_CURVE ( 'NONE', #16924, #65047, #39863, .T. ) ;
#42580 = CARTESIAN_POINT ( 'NONE',  ( 11.38795122972049967, -3.601717549869600354, -6.578956058177199751 ) ) ;
#42581 = CYLINDRICAL_SURFACE ( 'NONE', #16323, 1.250000000000000222 ) ;
#42582 = CARTESIAN_POINT ( 'NONE',  ( 18.26113864896150218, -2.644667523736221604, 12.31932909903656181 ) ) ;
#42583 = ORIENTED_EDGE ( 'NONE', *, *, #16186, .T. ) ;
#42584 = CARTESIAN_POINT ( 'NONE',  ( 11.07071167063000061, -6.643645819897000315, -5.582924995379999977 ) ) ;
#42585 = ORIENTED_EDGE ( 'NONE', *, *, #45620, .T. ) ;
#42586 = B_SPLINE_CURVE_WITH_KNOTS ( 'NONE', 3,
 ( #20074, #63742, #26357, #15852 ),
 .UNSPECIFIED., .F., .F.,
 ( 4, 4 ),
 ( 0.000000000000000000, 1.000000000000000000 ),
 .UNSPECIFIED. ) ;
#42587 = DIRECTION ( 'NONE',  ( 1.000000000000000000, 0.000000000000000000, 0.000000000000000000 ) ) ;
#42588 = CARTESIAN_POINT ( 'NONE',  ( 8.099999999999999645, 0.000000000000000000, 0.000000000000000000 ) ) ;
#42589 = CARTESIAN_POINT ( 'NONE',  ( 4.900006121741999010, 0.5234957687185628483, 1.947945353336630436 ) ) ;
#42590 = CARTESIAN_POINT ( 'NONE',  ( 9.856715971886000460, 4.814120192353000149, -8.929574926876000518 ) ) ;
#42591 = DIRECTION ( 'NONE',  ( -0.000000000000000000, -0.000000000000000000, 1.000000000000000000 ) ) ;
#42592 = CARTESIAN_POINT ( 'NONE',  ( 18.17483763482896109, 2.416937413673594381, -12.47057468851364348 ) ) ;
#42593 = CARTESIAN_POINT ( 'NONE',  ( 23.73965757102299889, -13.16312038164999976, 3.763220966169999571 ) ) ;
#42594 = CARTESIAN_POINT ( 'NONE',  ( 8.783078676347997771, 3.752732269140699906, -8.446684196061099215 ) ) ;
#42595 = CIRCLE ( 'NONE', #60469, 0.7499999936418002555 ) ;
#42596 = ORIENTED_EDGE ( 'NONE', *, *, #9101, .T. ) ;
#42597 = CARTESIAN_POINT ( 'NONE',  ( 9.028931733733378096, 2.726262640825360961, -8.739372639417585020 ) ) ;
#42598 = CARTESIAN_POINT ( 'NONE',  ( 9.719613305057999142, 5.967773797872000685, 7.406643507784999692 ) ) ;
#42599 = B_SPLINE_CURVE_WITH_KNOTS ( 'NONE', 3,
 ( #40227, #1436, #55271, #39535 ),
 .UNSPECIFIED., .F., .F.,
 ( 4, 4 ),
 ( 0.1836163425310814723, 1.000000000000000000 ),
 .UNSPECIFIED. ) ;
#42600 = CARTESIAN_POINT ( 'NONE',  ( 2.280140132542667342, -3.408904368339108260, 0.9161175952574674985 ) ) ;
#42601 = CARTESIAN_POINT ( 'NONE',  ( 11.65278751119019951, -4.790480620979200133, 7.086443476450299706 ) ) ;
#42602 = CARTESIAN_POINT ( 'NONE',  ( 5.477523075960999854, 12.82224764859999766, -2.276049205301000189 ) ) ;
#42603 = CARTESIAN_POINT ( 'NONE',  ( 11.13257108636000048, 9.198727620182998166, -6.595251064759999338 ) ) ;
#42604 = CARTESIAN_POINT ( 'NONE',  ( 12.72277096606028834, -0.6196453797482989190, 12.67964297675817598 ) ) ;
#42605 = VECTOR ( 'NONE', #41800, 1000.000000000000114 ) ;
#42606 = DIRECTION ( 'NONE',  ( -1.000000000000000000, 0.000000000000000000, 0.000000000000000000 ) ) ;
#42607 = ADVANCED_FACE ( 'NONE', ( #32403 ), #43229, .T. ) ;
#42608 = DIRECTION ( 'NONE',  ( -1.000000000000000000, 0.000000000000000000, 0.000000000000000000 ) ) ;
#42609 = CARTESIAN_POINT ( 'NONE',  ( 11.44795901272999927, -3.583381594953999549, 11.14153199795000049 ) ) ;
#42610 = ORIENTED_EDGE ( 'NONE', *, *, #59704, .T. ) ;
#42611 = CARTESIAN_POINT ( 'NONE',  ( 9.418385841233000377, 3.251172436837000301, -6.320036569851000152 ) ) ;
#42612 = CARTESIAN_POINT ( 'NONE',  ( 6.773735035739000487, -0.8949653936606000171, 0.6576296519798999762 ) ) ;
#42613 = EDGE_CURVE ( 'NONE', #13775, #33561, #24, .T. ) ;
#42614 = EDGE_CURVE ( 'NONE', #16254, #28416, #37598, .T. ) ;
#42615 = CARTESIAN_POINT ( 'NONE',  ( 17.86935674558754528, 3.040604463256959100, 13.54376658945627909 ) ) ;
#42616 = CARTESIAN_POINT ( 'NONE',  ( 9.115118560745049336, 5.349923934101355805, -7.499992884230159973 ) ) ;
#42617 = CARTESIAN_POINT ( 'NONE',  ( 5.000000000000000000, 0.2500000000000000000, -9.776630298829998011 ) ) ;
#42618 = CARTESIAN_POINT ( 'NONE',  ( 10.25564828895399927, -3.119330945648699949, -7.981013126389099099 ) ) ;
#42619 = VERTEX_POINT ( 'NONE', #61380 ) ;
#42620 = CARTESIAN_POINT ( 'NONE',  ( 11.20596535229475776, 3.091087823720314987, -7.824984935920127782 ) ) ;
#42621 = CARTESIAN_POINT ( 'NONE',  ( 12.40000000000000213, -11.60847947989999973, -1.809983899806999919 ) ) ;
#42623 = CARTESIAN_POINT ( 'NONE',  ( 11.08482133862618468, -3.057020944820409092, -8.373613860257945518 ) ) ;
#42622 = CARTESIAN_POINT ( 'NONE',  ( 8.316054719590999511, 3.826300099041999747, -9.055335252254000267 ) ) ;
#42624 = CARTESIAN_POINT ( 'NONE',  ( 25.55276892244668474, -11.13096414089930164, 3.116574921624185368 ) ) ;
#42625 = ORIENTED_EDGE ( 'NONE', *, *, #60838, .F. ) ;
#42626 = CARTESIAN_POINT ( 'NONE',  ( 9.479214860607999782, 4.071727169861000029, 9.089299483126000112 ) ) ;
#42627 = CARTESIAN_POINT ( 'NONE',  ( 18.16587897468629009, -2.632730956727242333, -13.64436436691515731 ) ) ;
#42628 = CARTESIAN_POINT ( 'NONE',  ( 11.73671932425159881, 3.872987101045399783, 6.643164954553199664 ) ) ;
#42629 = CARTESIAN_POINT ( 'NONE',  ( 11.01776264201000011, -4.914128622650000722, 8.587713430305999651 ) ) ;
#42630 = CARTESIAN_POINT ( 'NONE',  ( 8.064120559623999540, -4.228293421747000735, 8.941387937291999322 ) ) ;
#42631 = EDGE_LOOP ( 'NONE', ( #60399, #47207, #53580, #64806 ) ) ;
#42632 = CARTESIAN_POINT ( 'NONE',  ( 9.678448551390218313, -4.965577467693124802, -8.481121822464514182 ) ) ;
#42633 = EDGE_CURVE ( 'NONE', #10274, #29557, #13414, .T. ) ;
#42635 = CARTESIAN_POINT ( 'NONE',  ( 11.09178064679000109, -4.578543110806999827, -8.908602356389000221 ) ) ;
#42634 = CARTESIAN_POINT ( 'NONE',  ( 10.40299135172147693, 4.795252583382552558, -7.137146156348714854 ) ) ;
#42636 = CARTESIAN_POINT ( 'NONE',  ( 7.744874159809953085, -5.467231327630983628, 8.434612347329016657 ) ) ;
#42637 = CARTESIAN_POINT ( 'NONE',  ( 18.04064113778062861, -0.3934955819137399557, 13.89250369607185398 ) ) ;
#42638 = CARTESIAN_POINT ( 'NONE',  ( 2.247081873818999931, 2.483819732826999971, -1.905290611529000033 ) ) ;
#42639 = ORIENTED_EDGE ( 'NONE', *, *, #36441, .T. ) ;
#42641 = CARTESIAN_POINT ( 'NONE',  ( 5.657109839683332808, -1.199500263597270022, -0.9218200799623730290 ) ) ;
#42640 = AXIS2_PLACEMENT_3D ( 'NONE', #55371, #12026, #65149 ) ;
#42642 = CARTESIAN_POINT ( 'NONE',  ( 11.48995257254740032, -5.095356924909000718, 7.181435527216799564 ) ) ;
#42643 = CARTESIAN_POINT ( 'NONE',  ( 10.49349279008999858, 3.667611644732699627, 6.265968249244999733 ) ) ;
#42644 = EDGE_LOOP ( 'NONE', ( #32082, #30231, #60084, #30358 ) ) ;
#42645 = CARTESIAN_POINT ( 'NONE',  ( 9.021064158776001207, 4.883347899767999323, -6.417062834774999835 ) ) ;
#42646 = CARTESIAN_POINT ( 'NONE',  ( 12.56977253056424004, 1.799738463188376825, -12.47080370841241503 ) ) ;
#42647 = CARTESIAN_POINT ( 'NONE',  ( 11.26857802013510046, -5.174568897094999897, 7.527343341769989316 ) ) ;
#42648 = CARTESIAN_POINT ( 'NONE',  ( 24.74075890553500301, -3.240096724082000001, -11.83467285805000024 ) ) ;
#42649 = CIRCLE ( 'NONE', #228, 0.9500000000000007327 ) ;
#42650 = CARTESIAN_POINT ( 'NONE',  ( 17.99250848602325803, 2.946479007099335412, -13.56856542436401369 ) ) ;
#42651 = ORIENTED_EDGE ( 'NONE', *, *, #21995, .F. ) ;
#42652 = CARTESIAN_POINT ( 'NONE',  ( 11.07299956498199833, 5.207010770456999893, 7.174999999999999822 ) ) ;
#42653 = CARTESIAN_POINT ( 'NONE',  ( 10.67905590578999941, -2.899999999999999911, 6.571291218949999902 ) ) ;
#42654 = ORIENTED_EDGE ( 'NONE', *, *, #63905, .T. ) ;
#42655 = PRESENTATION_STYLE_ASSIGNMENT (( #25199 ) ) ;
#42656 = CARTESIAN_POINT ( 'NONE',  ( 10.82179975933729921, 4.948878321068100661, 7.826467126457498757 ) ) ;
#42657 = CIRCLE ( 'NONE', #61672, 12.39999890530000037 ) ;
#42658 = LINE ( 'NONE', #37411, #21957 ) ;
#42659 = CARTESIAN_POINT ( 'NONE',  ( 10.38153063908000107, 2.772139908660999907, -8.408082511401000048 ) ) ;
#42660 = DIRECTION ( 'NONE',  ( -1.000000000000000000, 0.000000000000000000, 0.000000000000000000 ) ) ;
#42661 = CARTESIAN_POINT ( 'NONE',  ( 10.44675369521999997, -2.885048926231000177, 8.863479194807000638 ) ) ;
#42662 = CARTESIAN_POINT ( 'NONE',  ( 17.83159136582989035, 0.5605836838512537890, -12.68334204399185694 ) ) ;
#42663 = ADVANCED_FACE ( 'NONE', ( #7208 ), #56569, .F. ) ;
#42664 = CARTESIAN_POINT ( 'NONE',  ( 12.34817707643961526, 2.926896462515248487, -12.34181790736438522 ) ) ;
#42665 = CARTESIAN_POINT ( 'NONE',  ( 10.96949144726329806, -4.580206776679999869, -6.681274802424499448 ) ) ;
#42666 = CARTESIAN_POINT ( 'NONE',  ( 7.764232780408999446, 4.628941086829000184, 5.991667691044999522 ) ) ;
#42667 = ORIENTED_EDGE ( 'NONE', *, *, #56185, .F. ) ;
#42668 =( NAMED_UNIT ( * ) PLANE_ANGLE_UNIT ( ) SI_UNIT ( $, .RADIAN. ) );
#42669 = CARTESIAN_POINT ( 'NONE',  ( 24.69607615698642533, -3.134132996396517434, 11.81031189595167952 ) ) ;
#42670 = CARTESIAN_POINT ( 'NONE',  ( 24.62620337042029206, -8.774568047083310063, -9.205177742587718370 ) ) ;
#42671 = CARTESIAN_POINT ( 'NONE',  ( 8.617856957858560207, 2.961633343650540873, -6.199064870269592298 ) ) ;
#42672 = CARTESIAN_POINT ( 'NONE',  ( 18.02641336659266003, 3.027085105403482412, 12.23097768044556055 ) ) ;
#42673 = CARTESIAN_POINT ( 'NONE',  ( 10.97046361309999973, 6.148683856984000329, 5.033387594187999525 ) ) ;
#42674 = DIRECTION ( 'NONE',  ( -1.000000000000000000, 0.000000000000000000, 0.000000000000000000 ) ) ;
#42675 = CARTESIAN_POINT ( 'NONE',  ( 12.55586324466750270, -0.5732756865038156624, -12.68257855878029439 ) ) ;
#42676 = B_SPLINE_CURVE_WITH_KNOTS ( 'NONE', 3,
 ( #59420, #26931, #52810, #16426 ),
 .UNSPECIFIED., .F., .F.,
 ( 4, 4 ),
 ( 0.000000000000000000, 0.5000000000000298650 ),
 .UNSPECIFIED. ) ;
#42677 = CARTESIAN_POINT ( 'NONE',  ( 12.80505043854144276, 0.6249999999999994449, -12.67928921589118652 ) ) ;
#42678 = ORIENTED_EDGE ( 'NONE', *, *, #9605, .T. ) ;
#42679 = CARTESIAN_POINT ( 'NONE',  ( 12.44978597066681836, -1.852986171447666974, 12.46300423074626451 ) ) ;
#42680 = CARTESIAN_POINT ( 'NONE',  ( 10.33890035061499901, -3.732283713685800031, -8.468075389605498771 ) ) ;
#42681 = CARTESIAN_POINT ( 'NONE',  ( 23.59999192078999997, 10.30759737717999869, 9.317725909430999209 ) ) ;
#42682 = CARTESIAN_POINT ( 'NONE',  ( 17.55505043854147118, -1.875000000000000000, -13.78627172894481667 ) ) ;
#42683 = CARTESIAN_POINT ( 'NONE',  ( 11.71564426047340035, -3.460037133261700149, 6.654192128557399499 ) ) ;
#42684 = VECTOR ( 'NONE', #59277, 1000.000000000000000 ) ;
#42685 = CARTESIAN_POINT ( 'NONE',  ( 11.70379573085659786, 5.106255642043000087, -7.691418046581699919 ) ) ;
#42686 = CARTESIAN_POINT ( 'NONE',  ( 12.15475987602171770, 0.3182341284860636388, 12.59598505207571861 ) ) ;
#42687 = CARTESIAN_POINT ( 'NONE',  ( 0.04415809921860000542, -1.568133397559999809, -2.874292603119999789 ) ) ;
#42688 = ADVANCED_BREP_SHAPE_REPRESENTATION ( '', ( #29488, #9676 ), #16178 ) ;
#42689 = CARTESIAN_POINT ( 'NONE',  ( 4.706016184301807570, -0.01789162623760187643, 1.198355196476257545 ) ) ;
#42690 = CARTESIAN_POINT ( 'NONE',  ( 12.08977223171467763, 2.598917558143519102, 12.32906181315049210 ) ) ;
#42692 = CARTESIAN_POINT ( 'NONE',  ( 8.175760841228999709, 2.599243720295000060, 7.909344432242998657 ) ) ;
#42691 = CARTESIAN_POINT ( 'NONE',  ( 9.606367640780998585, 4.538247246588100303, -6.493012239633999982 ) ) ;
#42693 = CARTESIAN_POINT ( 'NONE',  ( 10.89149144726329865, 3.340422662105400065, -6.569275630703699242 ) ) ;
#42694 = CARTESIAN_POINT ( 'NONE',  ( 7.612465007326000510, 3.179383379803001564, -6.407107007521996245 ) ) ;
#42695 = EDGE_CURVE ( 'NONE', #51578, #28388, #5834, .T. ) ;
#42696 = EDGE_CURVE ( 'NONE', #24788, #5489, #63237, .T. ) ;
#42697 = CARTESIAN_POINT ( 'NONE',  ( 10.66042971959000063, 2.315663237570999566, -7.431702255173999738 ) ) ;
#42698 = CARTESIAN_POINT ( 'NONE',  ( 8.896088727410999653, 2.725263018055000153, -7.606911245136100064 ) ) ;
#42700 = CARTESIAN_POINT ( 'NONE',  ( 18.12515139794508912, -0.2563289266217783635, 12.69652241465665732 ) ) ;
#42699 = DIRECTION ( 'NONE',  ( 0.7071067811865459074, -0.08614499000932547557, 0.7018397542860447258 ) ) ;
#42701 = CARTESIAN_POINT ( 'NONE',  ( 8.757697342472001267, 2.899999999999999911, -6.397101765418000241 ) ) ;
#42702 = VERTEX_POINT ( 'NONE', #56476 ) ;
#42703 = AXIS2_PLACEMENT_3D ( 'NONE', #52093, #67827, #25877 ) ;
#42704 = CARTESIAN_POINT ( 'NONE',  ( 1.071837387928000096, -2.100966486736999705, -2.491430570518000209 ) ) ;
#42705 = CARTESIAN_POINT ( 'NONE',  ( 9.020964430773000586, 2.907392932634000005, 6.146188468825999784 ) ) ;
#42706 = VECTOR ( 'NONE', #8297, 1000.000000000000227 ) ;
#42707 = CARTESIAN_POINT ( 'NONE',  ( 18.27990737420740786, 0.1887961029076866970, -12.59999260960568712 ) ) ;
#42708 = CARTESIAN_POINT ( 'NONE',  ( 8.895138961223999274, 4.832207374954999857, 6.937618199889199033 ) ) ;
#42709 = CARTESIAN_POINT ( 'NONE',  ( 12.47325605351262290, -3.030051207268857461, 13.54664584463135135 ) ) ;
#42710 = CARTESIAN_POINT ( 'NONE',  ( 12.18133850337987134, 2.541372565827187735, 13.66455005694026603 ) ) ;
#42711 = CARTESIAN_POINT ( 'NONE',  ( 8.995772571291157149, -5.001491341851800776, -8.076234199639099387 ) ) ;
#42712 = ORIENTED_EDGE ( 'NONE', *, *, #17205, .T. ) ;
#42713 = EDGE_CURVE ( 'NONE', #11605, #49203, #55874, .T. ) ;
#42714 = CARTESIAN_POINT ( 'NONE',  ( 4.934838347548000215, -0.2021279076763000115, -1.116266169982000234 ) ) ;
#42715 = CARTESIAN_POINT ( 'NONE',  ( 9.200038493598999167, -3.074215132699300135, -6.617216466537199970 ) ) ;
#42716 = DIRECTION ( 'NONE',  ( 0.000000000000000000, 0.8648648648648720183, 0.5020047465136825426 ) ) ;
#42717 = CARTESIAN_POINT ( 'NONE',  ( 17.84632887397102863, -3.351233551899249985, 11.15758637348127458 ) ) ;
#42718 = EDGE_CURVE ( 'NONE', #66385, #61133, #33786, .T. ) ;
#42719 = CARTESIAN_POINT ( 'NONE',  ( 17.75769270374269482, 3.091259753241552666, -12.29395838111494754 ) ) ;
#42720 = CARTESIAN_POINT ( 'NONE',  ( 9.654341692891298621, -2.749999283195044164, 7.663628708442520754 ) ) ;
#42721 = CARTESIAN_POINT ( 'NONE',  ( 17.96110074834104253, 2.975239710473370103, 12.32804434199381483 ) ) ;
#42722 = LINE ( 'NONE', #21726, #24545 ) ;
#42723 = CARTESIAN_POINT ( 'NONE',  ( 10.86460564679000029, -3.843601288168000174, -5.985268170611000471 ) ) ;
#42724 = CARTESIAN_POINT ( 'NONE',  ( 11.14975833414749928, 3.203462856645999945, -7.825000000000000178 ) ) ;
#42725 = B_SPLINE_SURFACE_WITH_KNOTS ( 'NONE', 3, 3, ( 
 ( #42838, #64148, #49113, #38980 ),
 ( #54706, #59948, #28492, #33738 ),
 ( #6805, #189, #21505, #28142 ),
 ( #16262, #11022, #1564, #37586 ),
 ( #58919, #22886, #44237, #32359 ),
 ( #48427, #53675, #22198, #5769 ),
 ( #17657, #27111, #60298, #1225 ),
 ( #43534, #12407, #535, #21847 ),
 ( #22538, #43182, #64486, #32696 ) ),
 .UNSPECIFIED., .F., .F., .F.,
 ( 4, 1, 1, 1, 1, 1, 4 ),
 ( 4, 4 ),
 ( 0.05214259105100000485, 0.1666666666667000196, 0.3333333333333000081, 0.5000000000000000000, 0.6666666666667000474, 0.8333333333333000637, 0.9777068595523999983 ),
 ( -0.1900882580235000174, 1.190231865545000156 ),
 .UNSPECIFIED. ) ;
#42726 = DIRECTION ( 'NONE',  ( 1.000000000000000000, 0.000000000000000000, 0.000000000000000000 ) ) ;
#42727 = CARTESIAN_POINT ( 'NONE',  ( 23.61456325407660017, 10.17980770879276697, -9.423256655973792917 ) ) ;
#42728 = CARTESIAN_POINT ( 'NONE',  ( 8.761230081853241813, -3.478588282862478120, -8.281074114623761417 ) ) ;
#42729 = ORIENTED_EDGE ( 'NONE', *, *, #12478, .F. ) ;
#42730 = CARTESIAN_POINT ( 'NONE',  ( 8.804445280412998898, 5.597201461420000967, -8.171008079894999554 ) ) ;
#42731 = CARTESIAN_POINT ( 'NONE',  ( 11.76902897915239876, -3.778278678798900447, 6.662660017635100296 ) ) ;
#42732 = VERTEX_POINT ( 'NONE', #7898 ) ;
#42733 = AXIS2_PLACEMENT_3D ( 'NONE', #20515, #10366, #41839 ) ;
#42734 = CARTESIAN_POINT ( 'NONE',  ( 7.924773910468002391, 3.741844367409119521, -6.158492087791373137 ) ) ;
#42735 = CARTESIAN_POINT ( 'NONE',  ( 10.79303032197930001, -3.336467919271199900, -6.572090902022299730 ) ) ;
#42736 = VERTEX_POINT ( 'NONE', #2646 ) ;
#42737 = CARTESIAN_POINT ( 'NONE',  ( 10.92968717260509948, 3.312350236372100021, 6.377637058250999580 ) ) ;
#42738 = CARTESIAN_POINT ( 'NONE',  ( 4.699999740790709701, 13.17499974068000057, -1.948182422444000466E-09 ) ) ;
#42739 = B_SPLINE_CURVE_WITH_KNOTS ( 'NONE', 3,
 ( #3793, #19198, #61167, #46117 ),
 .UNSPECIFIED., .F., .F.,
 ( 4, 4 ),
 ( 0.5000023781865966521, 1.000000000000000000 ),
 .UNSPECIFIED. ) ;
#42740 = CARTESIAN_POINT ( 'NONE',  ( 17.89159592529800236, -3.376698609984999599, 11.11057657535000054 ) ) ;
#42741 = CARTESIAN_POINT ( 'NONE',  ( 11.56833327354034857, -4.746587807672299597, -7.011667014989399149 ) ) ;
#42742 = CARTESIAN_POINT ( 'NONE',  ( 12.72381130742976474, 0.6210784669310237538, -13.88131957737374300 ) ) ;
#42743 = CARTESIAN_POINT ( 'NONE',  ( 6.999999999999999112, -6.725428974790256476, -3.045254342161083816 ) ) ;
#42744 = CARTESIAN_POINT ( 'NONE',  ( 13.51802873821100270, 11.59174185862000073, 2.195273509308000026 ) ) ;
#42745 = ORIENTED_EDGE ( 'NONE', *, *, #7961, .F. ) ;
#42746 = CARTESIAN_POINT ( 'NONE',  ( 9.468110841233000841, 4.082930418187999955, -6.104944817728999773 ) ) ;
#42747 = ORIENTED_EDGE ( 'NONE', *, *, #55505, .T. ) ;
#42748 = AXIS2_PLACEMENT_3D ( 'NONE', #1466, #11950, #11256 ) ;
#42749 = CARTESIAN_POINT ( 'NONE',  ( 10.85226354018294792, 2.907767014557178342, -6.870476274536370553 ) ) ;
#42750 = SURFACE_STYLE_FILL_AREA ( #27361 ) ;
#42751 = VERTEX_POINT ( 'NONE', #29235 ) ;
#42752 = CARTESIAN_POINT ( 'NONE',  ( 9.655963142879999239, 5.251703735191999733, 7.763860089407599752 ) ) ;
#42753 = CARTESIAN_POINT ( 'NONE',  ( 18.18011893007464153, -2.482032845566130241, -12.45575022786950647 ) ) ;
#42754 = CARTESIAN_POINT ( 'NONE',  ( 24.97036873516232092, -8.550788777872098123, 8.359011271273349308 ) ) ;
#42755 = CARTESIAN_POINT ( 'NONE',  ( 10.24809687351608289, 4.327184855449106138, -6.282534154164607365 ) ) ;
#42756 = CARTESIAN_POINT ( 'NONE',  ( 23.89320776801300283, -8.862674798131001452, -7.304122743059000555 ) ) ;
#42757 = CARTESIAN_POINT ( 'NONE',  ( 12.27431752107754015, -0.3302328523437085273, 13.89472426752322853 ) ) ;
#42758 = EDGE_LOOP ( 'NONE', ( #11643, #46811, #40015, #66829 ) ) ;
#42759 = CARTESIAN_POINT ( 'NONE',  ( 12.18592533278400047, 11.71489335541000010, -3.703722432179000101 ) ) ;
#42760 = CARTESIAN_POINT ( 'NONE',  ( 18.44593829204400137, 11.84685177148000079, -3.896686237526999719 ) ) ;
#42761 = CARTESIAN_POINT ( 'NONE',  ( 11.09999999999999964, 2.700688487044999864, -5.124965750789000296 ) ) ;
#42762 = CARTESIAN_POINT ( 'NONE',  ( 4.765942101178999302, -0.7564391385043001126, 0.9147881139243999593 ) ) ;
#42763 = ADVANCED_BREP_SHAPE_REPRESENTATION ( '', ( #8079, #9676 ), #57795 ) ;
#42764 = CARTESIAN_POINT ( 'NONE',  ( 9.734454719592999794, 3.021734963141999852, -6.070209284876999511 ) ) ;
#42765 = FACE_OUTER_BOUND ( 'NONE', #65302, .T. ) ;
#42766 = CARTESIAN_POINT ( 'NONE',  ( 10.77434462036999818, -4.612888200890999713, -8.898797372219998891 ) ) ;
#42767 = ORIENTED_EDGE ( 'NONE', *, *, #3527, .T. ) ;
#42768 = EDGE_LOOP ( 'NONE', ( #8077, #17969, #64744, #64247 ) ) ;
#42769 = CARTESIAN_POINT ( 'NONE',  ( 11.09999999999999964, 5.299999999999999822, 6.469505845987999493 ) ) ;
#42770 = CARTESIAN_POINT ( 'NONE',  ( 10.91441078833591405, -5.114410788335912450, -6.482042798774522829 ) ) ;
#42771 = CYLINDRICAL_SURFACE ( 'NONE', #31878, 12.52500000000000036 ) ;
#42772 = CARTESIAN_POINT ( 'NONE',  ( 9.266851002542999538, -2.832432432432000269, 6.822293592207000934 ) ) ;
#42773 = CARTESIAN_POINT ( 'NONE',  ( 7.000000000000000000, -0.2897247358851999799, 3.000000000000000000 ) ) ;
#42774 = EDGE_CURVE ( 'NONE', #23094, #58951, #62544, .T. ) ;
#42775 = EDGE_CURVE ( 'NONE', #15559, #22723, #24173, .T. ) ;
#42776 = CARTESIAN_POINT ( 'NONE',  ( 10.92968717260509948, 3.312350236372100021, -8.622362941748999532 ) ) ;
#42777 = CARTESIAN_POINT ( 'NONE',  ( 9.510025935145998588, 3.874109063559000088, -6.642177514500700042 ) ) ;
#42779 = CARTESIAN_POINT ( 'NONE',  ( 8.348093183609000434, 4.599999999999999645, -6.056236567608999977 ) ) ;
#42778 = CARTESIAN_POINT ( 'NONE',  ( 10.20567167105699902, -4.990538396979200542, 7.333638993632098924 ) ) ;
#42780 = CARTESIAN_POINT ( 'NONE',  ( 8.332046967449000974, -2.867486995832002616, 6.314275746166007508 ) ) ;
#42781 = ORIENTED_EDGE ( 'NONE', *, *, #64174, .T. ) ;
#42782 = CONICAL_SURFACE ( 'NONE', #12644, 2.050045943449999797, 0.7853981633972997312 ) ;
#42783 = PRODUCT_DEFINITION_SHAPE ( 'NONE', 'NONE',  #69209 ) ;
#42784 = CARTESIAN_POINT ( 'NONE',  ( 9.409308287954999628, -2.634700736117999931, 8.920302460802998823 ) ) ;
#42785 = CARTESIAN_POINT ( 'NONE',  ( 9.659038493598998798, 4.925784867300699865, 8.382783533462799141 ) ) ;
#42786 = CARTESIAN_POINT ( 'NONE',  ( 10.89393020684959978, -5.250000000000000000, -7.500000000000000000 ) ) ;
#42787 = CARTESIAN_POINT ( 'NONE',  ( 10.27814441345999974, -5.521593622715999850, 8.751220666652999469 ) ) ;
#42788 = CARTESIAN_POINT ( 'NONE',  ( 9.883148997457000817, -5.167567567567999731, 6.822293592207000934 ) ) ;
#42789 = CARTESIAN_POINT ( 'NONE',  ( 25.46373329105799854, 11.23406619596999967, -3.161081784610999978 ) ) ;
#42790 = CARTESIAN_POINT ( 'NONE',  ( 13.05446786537200232, -12.11615129267999968, -2.032410325197000045 ) ) ;
#42791 = EDGE_CURVE ( 'NONE', #48042, #10703, #30860, .T. ) ;
#42792 = CARTESIAN_POINT ( 'NONE',  ( 6.816501042874381078, 2.788803157567000035, -8.345558963038001821 ) ) ;
#42793 = AXIS2_PLACEMENT_3D ( 'NONE', #43531, #32016, #48423 ) ;
#42794 = CARTESIAN_POINT ( 'NONE',  ( 9.459367640780998343, -3.591293244209800228, -6.735364967924099666 ) ) ;
#42795 = CARTESIAN_POINT ( 'NONE',  ( 6.383918340290000160, 0.03180299129942999736, -1.321917036380999999 ) ) ;
#42796 = EDGE_CURVE ( 'NONE', #12955, #1683, #32597, .T. ) ;
#42797 = CARTESIAN_POINT ( 'NONE',  ( 11.51837338474677708, -4.264324089837040255, 8.333200082717626245 ) ) ;
#42798 = CONICAL_SURFACE ( 'NONE', #50646, 2.824973347946000413, 0.7853886971611369061 ) ;
#42799 = LINE ( 'NONE', #47705, #31734 ) ;
#42800 = VERTEX_POINT ( 'NONE', #15546 ) ;
#42801 = CARTESIAN_POINT ( 'NONE',  ( 12.42410782380136425, 0.4959072410923918706, -12.68697406334525546 ) ) ;
#42802 = CARTESIAN_POINT ( 'NONE',  ( 11.58902763632552002, 3.213494089586499847, -7.137085349939700230 ) ) ;
#42803 = CARTESIAN_POINT ( 'NONE',  ( 7.100000000000000533, 4.000000000000000000, 8.849999999999999645 ) ) ;
#42804 = CARTESIAN_POINT ( 'NONE',  ( 10.89438299915333275, -5.254480013706496422, 6.992200716271752547 ) ) ;
#42805 = LINE ( 'NONE', #9955, #48287 ) ;
#42806 = VERTEX_POINT ( 'NONE', #37545 ) ;
#42807 = CARTESIAN_POINT ( 'NONE',  ( 25.20346112680899964, -11.20001863952999877, -3.404198054529000039 ) ) ;
#42808 = CARTESIAN_POINT ( 'NONE',  ( 10.64902344389989963, -4.883530143601199747, -6.963800219468099684 ) ) ;
#42809 = CARTESIAN_POINT ( 'NONE',  ( 18.16417820191648858, 0.1413121814401153697, 12.69896133444684949 ) ) ;
#42810 = CARTESIAN_POINT ( 'NONE',  ( 10.42726354018300050, -4.629523725463626782, 6.407767014557179230 ) ) ;
#42811 = CARTESIAN_POINT ( 'NONE',  ( 11.49999672495000169, -4.789193247147717436, 10.68959786790916588 ) ) ;
#42812 = CARTESIAN_POINT ( 'NONE',  ( 10.65413259636999932, 3.216622244594500302, -7.926858177843299380 ) ) ;
#42813 = ORIENTED_EDGE ( 'NONE', *, *, #21703, .T. ) ;
#42814 = CARTESIAN_POINT ( 'NONE',  ( 9.298040139821001304, -4.087076480742000584, 9.429402848390999736 ) ) ;
#42815 = CARTESIAN_POINT ( 'NONE',  ( 18.09702113181629457, 2.811936484508641865, -13.60234957393456945 ) ) ;
#42816 = EDGE_LOOP ( 'NONE', ( #20951, #68756, #1620, #27592 ) ) ;
#42817 = CARTESIAN_POINT ( 'NONE',  ( 10.99874143819000061, -2.710832050839000029, 4.962905352413001125 ) ) ;
#42818 = CARTESIAN_POINT ( 'NONE',  ( 7.802019353206999241, -5.638700495537999124, 8.266402903491000487 ) ) ;
#42819 = CARTESIAN_POINT ( 'NONE',  ( 8.623264158775000965, 5.288433695693000480, -8.041290150997999930 ) ) ;
#42820 = ORIENTED_EDGE ( 'NONE', *, *, #56798, .T. ) ;
#42821 = CARTESIAN_POINT ( 'NONE',  ( 23.57776935471744650, -2.928921454179648887, -13.64745658425302643 ) ) ;
#42822 = B_SPLINE_CURVE_WITH_KNOTS ( 'NONE', 3,
 ( #20040, #57432, #30882, #26322, #65074, #17194, #64732, #43437, #10920, #59156 ),
 .UNSPECIFIED., .F., .F.,
 ( 4, 2, 2, 2, 4 ),
 ( 0.1253969396550571880, 0.3126920919075452110, 0.4999872441600332618, 0.6872823964125207574, 0.8745775486650082531 ),
 .UNSPECIFIED. ) ;
#42823 = CARTESIAN_POINT ( 'NONE',  ( 6.917510841229000285, 5.477119873501999692, -8.694708770948999188 ) ) ;
#42824 = CARTESIAN_POINT ( 'NONE',  ( 11.09999999999999964, -6.593648102827000201, 5.598803487171999826 ) ) ;
#42825 = CARTESIAN_POINT ( 'NONE',  ( 7.344182448917417005, 2.650014028440602409, -7.853118540549031579 ) ) ;
#42826 = ORIENTED_EDGE ( 'NONE', *, *, #59507, .T. ) ;
#42827 = CARTESIAN_POINT ( 'NONE',  ( 10.55991645936999923, -5.094263939633999705, 6.075409946530999861 ) ) ;
#42828 = LINE ( 'NONE', #58557, #32870 ) ;
#42829 = CARTESIAN_POINT ( 'NONE',  ( 8.350387243830999395, 5.100000000000000533, -6.632262360512000576 ) ) ;
#42830 = ORIENTED_EDGE ( 'NONE', *, *, #16560, .F. ) ;
#42831 = CARTESIAN_POINT ( 'NONE',  ( 8.856495485442710702, 4.349453410998743941, -8.453238005838597857 ) ) ;
#42832 = CARTESIAN_POINT ( 'NONE',  ( 10.99305444037999990, -4.495427106425000652, -6.233607450113000326 ) ) ;
#42833 = ORIENTED_EDGE ( 'NONE', *, *, #29564, .T. ) ;
#42834 = CYLINDRICAL_SURFACE ( 'NONE', #49915, 0.6999999999999992895 ) ;
#42835 = CARTESIAN_POINT ( 'NONE',  ( 17.55505043854147118, -1.760910691117821836, -12.47634535983622861 ) ) ;
#42836 = CARTESIAN_POINT ( 'NONE',  ( 4.819071405523000173, 0.6499247483229999567, 1.258579622759999905 ) ) ;
#42837 = CARTESIAN_POINT ( 'NONE',  ( 11.59999999999999964, 4.072982449166801189, -6.447388989144585913 ) ) ;
#42838 = CARTESIAN_POINT ( 'NONE',  ( 16.13899430609699692, 3.920333201250000066, 11.93553532998999955 ) ) ;
#42839 = CARTESIAN_POINT ( 'NONE',  ( 7.108747422739984501, 5.156822660709760697, -8.212378574850216495 ) ) ;
#42840 = CARTESIAN_POINT ( 'NONE',  ( 24.14319150313052731, 12.47686771584972831, 3.361582803975455835 ) ) ;
#42841 = EDGE_CURVE ( 'NONE', #36843, #33549, #25907, .T. ) ;
#42842 = VERTEX_POINT ( 'NONE', #54316 ) ;
#42843 = CARTESIAN_POINT ( 'NONE',  ( 13.69992376746900042, -12.26631831379999937, -2.532779022035999805 ) ) ;
#42844 = VERTEX_POINT ( 'NONE', #11318 ) ;
#42845 = CARTESIAN_POINT ( 'NONE',  ( 10.02201554968999986, 3.298015135926000152, 5.700522662207000657 ) ) ;
#42846 = DIRECTION ( 'NONE',  ( -1.000000000000000000, 0.000000000000000000, 9.258974054462001038E-14 ) ) ;
#42847 = CIRCLE ( 'NONE', #57359, 11.84999999999999964 ) ;
#42848 = CARTESIAN_POINT ( 'NONE',  ( 21.59999987243000064, -13.89999852641999922, 0.000000000000000000 ) ) ;
#42849 = CARTESIAN_POINT ( 'NONE',  ( 12.35317296531419551, 2.068098628661974470, -13.75563068618459184 ) ) ;
#42850 = DIRECTION ( 'NONE',  ( 1.000000000000000000, 0.000000000000000000, 0.000000000000000000 ) ) ;
#42851 = CARTESIAN_POINT ( 'NONE',  ( 8.379867906096000851, 2.923743482149999906, 6.439439799146000176 ) ) ;
#42852 = CARTESIAN_POINT ( 'NONE',  ( 17.96752346481819984, -0.4700078255514594794, 13.88931146942756634 ) ) ;
#42853 = AXIS2_PLACEMENT_3D ( 'NONE', #38173, #1126, #43781 ) ;
#42854 = CARTESIAN_POINT ( 'NONE',  ( 9.392078467011812037, -5.386183347138083555, -8.566888829028510344 ) ) ;
#42855 = ORIENTED_EDGE ( 'NONE', *, *, #38570, .T. ) ;
#42856 = CARTESIAN_POINT ( 'NONE',  ( 12.41269542049148455, 0.4865081001878581168, 13.88853895923280746 ) ) ;
#42857 = CARTESIAN_POINT ( 'NONE',  ( 10.82533997688000049, -3.756890902898200046, 8.614534918052999757 ) ) ;
#42858 = CARTESIAN_POINT ( 'NONE',  ( 18.14887598841489691, -0.1995645668690017027, -13.89814765003239216 ) ) ;
#42859 = ADVANCED_FACE ( 'NONE', ( #22154 ), #6610, .F. ) ;
#42860 = ADVANCED_FACE ( 'NONE', ( #9747 ), #68126, .F. ) ;
#42861 = CARTESIAN_POINT ( 'NONE',  ( 8.309480646794000336, -2.905864338704999827, 8.940687151810998046 ) ) ;
#42863 = CARTESIAN_POINT ( 'NONE',  ( 18.29058462260969975, 11.07487261139536194, -3.615341608537649964 ) ) ;
#42862 = CARTESIAN_POINT ( 'NONE',  ( 9.034110134264999203, 4.695345051283999815, 8.660667941667000491 ) ) ;
#42864 = CARTESIAN_POINT ( 'NONE',  ( 10.42380110216399913, 3.026453990125600235, -6.905442784147899360 ) ) ;
#42865 = ADVANCED_FACE ( 'NONE', ( #30403 ), #64059, .F. ) ;
#42866 = CARTESIAN_POINT ( 'NONE',  ( 12.09999999999999609, -4.292035002842707669, 6.463642954493290738 ) ) ;
#42867 = B_SPLINE_CURVE_WITH_KNOTS ( 'NONE', 3,
 ( #13102, #14730, #44918, #66222 ),
 .UNSPECIFIED., .F., .F.,
 ( 4, 4 ),
 ( 0.000000000000000000, 1.000000000000000000 ),
 .UNSPECIFIED. ) ;
#42868 = CARTESIAN_POINT ( 'NONE',  ( 9.931621437244999129, 4.575883738927100097, -6.851875117168399143 ) ) ;
#42869 = CARTESIAN_POINT ( 'NONE',  ( 17.77532606275349991, -0.5849872192492382439, 12.68185863724641216 ) ) ;
#42870 = B_SPLINE_SURFACE_WITH_KNOTS ( 'NONE', 3, 3, ( 
 ( #62324, #30857, #51825, #3923 ),
 ( #20021, #68239, #9515, #62658 ),
 ( #25609, #24579, #41685, #8155 ),
 ( #18986, #29501, #2900, #24230 ),
 ( #66874, #40312, #61633, #13749 ) ),
 .UNSPECIFIED., .F., .F., .F.,
 ( 4, 1, 4 ),
 ( 4, 4 ),
 ( -0.007897885364823000257, 0.000000000000000000, 0.04616514892271000176 ),
 ( -0.1721959722423999917, 1.172195972106000017 ),
 .UNSPECIFIED. ) ;
#42871 = CARTESIAN_POINT ( 'NONE',  ( 6.940572573649000709, -0.2869491282519000541, -1.095445449434000018 ) ) ;
#42872 = CARTESIAN_POINT ( 'NONE',  ( 24.22080089608900266, 8.983041208896999308, 8.867674127912000159 ) ) ;
#42873 = ORIENTED_EDGE ( 'NONE', *, *, #28058, .F. ) ;
#42874 = CARTESIAN_POINT ( 'NONE',  ( 8.598668146794999245, -2.376522687267000222, 7.686981355459999499 ) ) ;
#42875 = CARTESIAN_POINT ( 'NONE',  ( 9.468589158772999781, 4.034680274230000308, -6.102912434217000026 ) ) ;
#42876 = CYLINDRICAL_SURFACE ( 'NONE', #60599, 1.000000000000000000 ) ;
#42877 = CARTESIAN_POINT ( 'NONE',  ( 0.9681103717476999826, 3.205765437135000173, -1.404659375816999844 ) ) ;
#42878 = ORIENTED_EDGE ( 'NONE', *, *, #43256, .T. ) ;
#42879 = VECTOR ( 'NONE', #22049, 1000.000000000000114 ) ;
#42880 = CARTESIAN_POINT ( 'NONE',  ( 0.6995747022588000297, -0.7815069638253000495, -3.281818906455000295 ) ) ;
#42881 = ADVANCED_FACE ( 'NONE', ( #60156 ), #36720, .T. ) ;
#42882 = CARTESIAN_POINT ( 'NONE',  ( 10.94501463001509833, 4.472480213525599879, 8.256737112932800216 ) ) ;
#42883 = CARTESIAN_POINT ( 'NONE',  ( 10.08211611373999972, 4.728047954991999369, -8.793974144431000894 ) ) ;
#42884 = ORIENTED_EDGE ( 'NONE', *, *, #44761, .F. ) ;
#42885 = CARTESIAN_POINT ( 'NONE',  ( 9.216839207166820813, 4.768179003839034813, -6.500433908363888236 ) ) ;
#42886 = CARTESIAN_POINT ( 'NONE',  ( 9.629471092178999214, -5.100000000000000533, 6.152188490330000370 ) ) ;
#42887 = CARTESIAN_POINT ( 'NONE',  ( 10.24733997687999931, 4.272363749081500295, 8.748653021963999521 ) ) ;
#42888 = CARTESIAN_POINT ( 'NONE',  ( 5.700000000000000178, 12.03770622561999915, 3.722046322334000124 ) ) ;
#42889 = CARTESIAN_POINT ( 'NONE',  ( 7.731795280408999993, 4.580608786027000612, 9.213365309690999538 ) ) ;
#42890 = ORIENTED_EDGE ( 'NONE', *, *, #386, .F. ) ;
#42891 = CARTESIAN_POINT ( 'NONE',  ( 6.608918340290000693, 0.03531958898060999497, -1.468087261088999895 ) ) ;
#42892 = CARTESIAN_POINT ( 'NONE',  ( 7.359129719585999929, 5.425783499582999880, -6.515903575897000088 ) ) ;
#42893 = CARTESIAN_POINT ( 'NONE',  ( 8.549219542760198465, -3.460297557318590567, 5.846195167334228948 ) ) ;
#42894 = VECTOR ( 'NONE', #40340, 1000.000000000000000 ) ;
#42895 = CARTESIAN_POINT ( 'NONE',  ( 11.01837338474678063, -4.264324089837040255, -6.666799917282374643 ) ) ;
#42896 = ORIENTED_EDGE ( 'NONE', *, *, #17203, .F. ) ;
#42897 = CARTESIAN_POINT ( 'NONE',  ( 2.990556799210291938, 3.500000000000001776, -0.4581489286485044832 ) ) ;
#42898 = CARTESIAN_POINT ( 'NONE',  ( 6.209193173016666734, -0.3926218265389190276, -1.460959015002473826 ) ) ;
#42899 = ORIENTED_EDGE ( 'NONE', *, *, #12273, .T. ) ;
#42900 = CARTESIAN_POINT ( 'NONE',  ( 8.158337970077000990E-06, -2.999989272562999965, 0.000000000000000000 ) ) ;
#42901 = CARTESIAN_POINT ( 'NONE',  ( 9.944763587296000296, 10.12538011034999919, -5.137399309246999834 ) ) ;
#42902 = VECTOR ( 'NONE', #37911, 1000.000000000000114 ) ;
#42903 = CARTESIAN_POINT ( 'NONE',  ( 17.69771933245237605, 0.6088408278571637577, -13.88204686096231733 ) ) ;
#42904 = ORIENTED_EDGE ( 'NONE', *, *, #46488, .T. ) ;
#42905 = CARTESIAN_POINT ( 'NONE',  ( 10.79353630809283437, -2.899999999999999911, 6.665341197380430849 ) ) ;
#42906 =( NAMED_UNIT ( * ) SI_UNIT ( $, .STERADIAN. ) SOLID_ANGLE_UNIT ( ) );
#42907 = CARTESIAN_POINT ( 'NONE',  ( 10.16684687351666661, -3.231816600031351516, 8.499583552997723501 ) ) ;
#42908 = AXIS2_PLACEMENT_3D ( 'NONE', #67556, #14439, #18987 ) ;
#42909 = CARTESIAN_POINT ( 'NONE',  ( 12.64121575286206323, 3.103492734220864691, -12.29027329182863149 ) ) ;
#42910 = CARTESIAN_POINT ( 'NONE',  ( 10.89503166480599994, -5.274847857784000560, 7.410114961806599787 ) ) ;
#42911 = ORIENTED_EDGE ( 'NONE', *, *, #29067, .F. ) ;
#42912 = CARTESIAN_POINT ( 'NONE',  ( 8.758795280412000395, 3.977267228909999730, 9.308925224542001331 ) ) ;
#42913 = ORIENTED_EDGE ( 'NONE', *, *, #28951, .F. ) ;
#42914 = CARTESIAN_POINT ( 'NONE',  ( 10.07314899745999881, 5.167567567567999731, -6.822293592207000934 ) ) ;
#42915 = CARTESIAN_POINT ( 'NONE',  ( 15.72310803393400036, -9.201544169428000686, -8.280720087647999605 ) ) ;
#42916 = CARTESIAN_POINT ( 'NONE',  ( 11.01665240710999960, 6.699956017084000237, -5.516881093594999896 ) ) ;
#42917 = ORIENTED_EDGE ( 'NONE', *, *, #24656, .F. ) ;
#42918 = CARTESIAN_POINT ( 'NONE',  ( 12.66096866354273409, -1.891485216129972446, -12.57270334283925806 ) ) ;
#42919 = LINE ( 'NONE', #65268, #45529 ) ;
#42920 = DIRECTION ( 'NONE',  ( 0.000000000000000000, 1.000000000000000000, 0.000000000000000000 ) ) ;
#42921 = EDGE_CURVE ( 'NONE', #5748, #58625, #46548, .T. ) ;
#42922 = CARTESIAN_POINT ( 'NONE',  ( 10.85226354018294792, 2.907767014557178342, 8.129523725463624118 ) ) ;
#42923 = CARTESIAN_POINT ( 'NONE',  ( 12.12491761308583449, -2.264077311857971342, -13.81573193591466442 ) ) ;
#42924 = ADVANCED_FACE ( 'NONE', ( #48546 ), #20836, .T. ) ;
#42925 = CARTESIAN_POINT ( 'NONE',  ( 10.69872335273220010, -3.650693637952500126, -8.440710326446700051 ) ) ;
#42926 = CARTESIAN_POINT ( 'NONE',  ( 11.59999999999999964, 4.000000000000000000, -7.500000000000000000 ) ) ;
#42927 = CARTESIAN_POINT ( 'NONE',  ( 18.26836321268588392, -2.610382005543646855, 12.32663954618810997 ) ) ;
#42928 = ORIENTED_EDGE ( 'NONE', *, *, #42473, .T. ) ;
#42929 = CARTESIAN_POINT ( 'NONE',  ( 10.84657802013509986, -5.315911219205999849, -7.469366283838649423 ) ) ;
#42930 = VERTEX_POINT ( 'NONE', #16032 ) ;
#42931 = CONICAL_SURFACE ( 'NONE', #11675, 12.42518024156999878, 0.7854126340177727261 ) ;
#42932 = CARTESIAN_POINT ( 'NONE',  ( 11.56599877858000092, -12.45298756855999933, -1.663864064400000009 ) ) ;
#42933 = CARTESIAN_POINT ( 'NONE',  ( 9.643930206848999376, 5.250000000000000000, -7.500000000000000000 ) ) ;
#42934 = CARTESIAN_POINT ( 'NONE',  ( 10.40558702164999971, 5.599341344818000721, -8.437759619346000051 ) ) ;
#42935 = CARTESIAN_POINT ( 'NONE',  ( 3.800000448357999883, 0.000000000000000000, 0.000000000000000000 ) ) ;
#42936 = FACE_OUTER_BOUND ( 'NONE', #50627, .T. ) ;
#42937 = CARTESIAN_POINT ( 'NONE',  ( 8.200215151753006637, 2.889589711576002085, -6.692116421364998402 ) ) ;
#42938 = CARTESIAN_POINT ( 'NONE',  ( 9.820199962102000413, 3.883325513302000154, 6.055618835924000187 ) ) ;
#42939 = ORIENTED_EDGE ( 'NONE', *, *, #49559, .F. ) ;
#42940 = CARTESIAN_POINT ( 'NONE',  ( 1.800973465875000068, -3.500000000000000000, 0.000000000000000000 ) ) ;
#42941 = CARTESIAN_POINT ( 'NONE',  ( 9.228133567168001150, 2.875367362387999837, 8.669940206484001877 ) ) ;
#42942 = CARTESIAN_POINT ( 'NONE',  ( 2.217640132542666453, -1.762666431298159475, 3.058252359239895135 ) ) ;
#42943 = CARTESIAN_POINT ( 'NONE',  ( 11.90211496860029960, -3.206052520092899982, 7.906860999147899527 ) ) ;
#42944 = CARTESIAN_POINT ( 'NONE',  ( 5.399998535875000449, 12.98068687585000092, -1.765643277144999912 ) ) ;
#42945 = VECTOR ( 'NONE', #40617, 1000.000000000000000 ) ;
#42946 = CARTESIAN_POINT ( 'NONE',  ( 11.05748560607000108, 9.481327459506999844, -6.305849355301000436 ) ) ;
#42947 = EDGE_CURVE ( 'NONE', #58024, #426, #34276, .T. ) ;
#42948 = CARTESIAN_POINT ( 'NONE',  ( 11.09999999999999964, 2.274006712557999688, -7.281956340829000673 ) ) ;
#42949 = AXIS2_PLACEMENT_3D ( 'NONE', #43442, #4639, #47990 ) ;
#42950 = CARTESIAN_POINT ( 'NONE',  ( 23.58303273028899838, -10.33244704280000015, -9.360922793932001440 ) ) ;
#42951 = CARTESIAN_POINT ( 'NONE',  ( 10.56491664109999995, 4.212242527248999835, 8.933458498617000032 ) ) ;
#42952 = CARTESIAN_POINT ( 'NONE',  ( 23.59999172348799945, -10.30759808834999980, 9.317726582648999667 ) ) ;
#42953 = EDGE_LOOP ( 'NONE', ( #44818, #50374, #46835, #40749 ) ) ;
#42954 = DIRECTION ( 'NONE',  ( 0.000000000000000000, -1.000000000000000000, 0.000000000000000000 ) ) ;
#42955 = CARTESIAN_POINT ( 'NONE',  ( 7.161035820969999577, 1.208716259960000095, 0.3209503551946999989 ) ) ;
#42956 = CARTESIAN_POINT ( 'NONE',  ( 18.15591411656198773, 2.672312740310635260, 13.63535347231577077 ) ) ;
#42957 = CARTESIAN_POINT ( 'NONE',  ( 10.83581759971949587, 5.012714476637088801, 4.871130536448504245 ) ) ;
#42958 = AXIS2_PLACEMENT_3D ( 'NONE', #46866, #58044, #62924 ) ;
#42959 = CARTESIAN_POINT ( 'NONE',  ( 10.69456919669529960, -2.906008650422999828, -7.823222900359999343 ) ) ;
#42960 = ORIENTED_EDGE ( 'NONE', *, *, #7970, .F. ) ;
#42961 = CARTESIAN_POINT ( 'NONE',  ( 5.641095281751840496, -12.09393047400899412, 3.739612655151788978 ) ) ;
#42962 = CARTESIAN_POINT ( 'NONE',  ( 7.795982780410000146, 3.164805384346000228, 9.104735843897000080 ) ) ;
#42963 = ADVANCED_FACE ( 'NONE', ( #5543 ), #26538, .F. ) ;
#42965 = CARTESIAN_POINT ( 'NONE',  ( 11.02755399909320566, -3.866653594937912608, -8.778526265510098625 ) ) ;
#42964 = CARTESIAN_POINT ( 'NONE',  ( 8.903895280414001689, 3.867331042029999999, -9.227339949050001877 ) ) ;
#42966 = CARTESIAN_POINT ( 'NONE',  ( 24.84571236082737045, 12.09404552098319918, -2.924969662484652844 ) ) ;
#42967 = ORIENTED_EDGE ( 'NONE', *, *, #8134, .T. ) ;
#42968 = CARTESIAN_POINT ( 'NONE',  ( 9.388624299788999039, 4.079402096444999515, 9.259357173634999327 ) ) ;
#42969 = CARTESIAN_POINT ( 'NONE',  ( 18.14726809210094416, -2.096144380837183352, -13.84220294531915307 ) ) ;
#42970 = CARTESIAN_POINT ( 'NONE',  ( 11.28949010443639978, 5.000675062740000065, 7.425165037173959703 ) ) ;
#42971 = CARTESIAN_POINT ( 'NONE',  ( 10.40516264833000015, -5.216401621862000404, 6.765753642936999768 ) ) ;
#42972 = CARTESIAN_POINT ( 'NONE',  ( 8.539831853209999935, -5.633481712366999794, 7.451234046297000368 ) ) ;
#42973 = EDGE_LOOP ( 'NONE', ( #54391, #20454, #62872, #12526 ) ) ;
#42974 = CARTESIAN_POINT ( 'NONE',  ( 7.968176658772001097, 2.280568568659000483, 6.510284508622999233 ) ) ;
#42976 = CARTESIAN_POINT ( 'NONE',  ( 10.67529314679000052, -3.066674550532999977, -8.703235919197002346 ) ) ;
#42975 = CARTESIAN_POINT ( 'NONE',  ( 11.36486084871759950, -5.207010770456999893, -7.825000000000000178 ) ) ;
#42977 = CARTESIAN_POINT ( 'NONE',  ( 7.798838663971441321, -4.555560098518249390, 9.151540452632529465 ) ) ;
#42978 = CARTESIAN_POINT ( 'NONE',  ( 10.71256247620999957, -5.951803124515000043, 7.233045248871000865 ) ) ;
#42979 = CARTESIAN_POINT ( 'NONE',  ( 1.166291019826000142, -0.3298644081521999727, -3.242294882329999961 ) ) ;
#42980 = EDGE_LOOP ( 'NONE', ( #27856, #52262, #21538, #58281, #9298, #29630, #17004, #24304, #3400, #64428, #53371, #918, #62848, #44599 ) ) ;
#42981 = CARTESIAN_POINT ( 'NONE',  ( 25.02476335228798376, -11.45589514262583464, -3.243232877822501248 ) ) ;
#42982 = CARTESIAN_POINT ( 'NONE',  ( 10.95257053952200010, -4.394359323863099576, 8.422730500489899796 ) ) ;
#42983 = CARTESIAN_POINT ( 'NONE',  ( 10.93656785386839836, 2.939720539848000413, 6.786470850652599474 ) ) ;
#42984 = PRESENTATION_LAYER_ASSIGNMENT (  '', '', ( #45245 ) ) ;
#42985 = ORIENTED_EDGE ( 'NONE', *, *, #53924, .T. ) ;
#42986 = CARTESIAN_POINT ( 'NONE',  ( 8.175739158770999992, 4.686731264770999772, -8.717075579553000608 ) ) ;
#42987 = CARTESIAN_POINT ( 'NONE',  ( 12.25647171456040319, 2.009180677272484949, -12.43879158508227611 ) ) ;
#42988 = CARTESIAN_POINT ( 'NONE',  ( 11.26346886766499900, -4.634677072395899877, 8.653146038559000885 ) ) ;
#42989 = CARTESIAN_POINT ( 'NONE',  ( 9.116868839903307986, 5.079248981113716255, -8.329446991275979428 ) ) ;
#42990 = CARTESIAN_POINT ( 'NONE',  ( 18.16751419051670879, 2.624553509637494564, -13.64625295310859165 ) ) ;
#42991 = ORIENTED_EDGE ( 'NONE', *, *, #7004, .F. ) ;
#42992 = CARTESIAN_POINT ( 'NONE',  ( 8.175754440378000254, -2.599231861044000169, 7.909347897884000389 ) ) ;
#42993 = DIRECTION ( 'NONE',  ( 0.000000000000000000, 0.000000000000000000, -1.000000000000000000 ) ) ;
#42994 = ORIENTED_EDGE ( 'NONE', *, *, #58227, .T. ) ;
#42995 = CARTESIAN_POINT ( 'NONE',  ( 12.36135608140801345, -3.049327969019417051, -12.22544940668144697 ) ) ;
#42997 = CARTESIAN_POINT ( 'NONE',  ( 10.55518582084299872, 3.433275964779900047, 8.155074391384399490 ) ) ;
#42996 = VECTOR ( 'NONE', #32615, 1000.000000000000000 ) ;
#42998 = CARTESIAN_POINT ( 'NONE',  ( 9.323722176100000425, 3.947350570199999797, 6.051869652381999920 ) ) ;
#42999 = CARTESIAN_POINT ( 'NONE',  ( 10.90760153359000029, 2.969978076949999934, -4.934359432739999995 ) ) ;
#43000 = CARTESIAN_POINT ( 'NONE',  ( 8.335548698406999080, 5.102342278510997531, 6.653323484791000553 ) ) ;
#43001 = EDGE_CURVE ( 'NONE', #16743, #66793, #27565, .T. ) ;
#43002 = CARTESIAN_POINT ( 'NONE',  ( 9.353731048338000065, -2.823575173856999410, 9.032043499493001448 ) ) ;
#43003 = ADVANCED_FACE ( 'NONE', ( #300 ), #21963, .T. ) ;
#43004 = CARTESIAN_POINT ( 'NONE',  ( 17.71666921258853478, 0.6040886362899379192, -12.68065483099175417 ) ) ;
#43005 = DIRECTION ( 'NONE',  ( 0.6684585169941805738, -0.6684585169941805738, 0.3260773253629903334 ) ) ;
#43006 = CARTESIAN_POINT ( 'NONE',  ( 10.35410941423799791, -3.257202320419700037, -6.825313060354999628 ) ) ;
#43007 = EDGE_CURVE ( 'NONE', #59855, #44325, #6225, .T. ) ;
#43008 = EDGE_CURVE ( 'NONE', #7987, #31711, #57545, .T. ) ;
#43009 = CARTESIAN_POINT ( 'NONE',  ( 9.010198341230998054, 5.040787533781999841, 8.522957620707000359 ) ) ;
#43010 = ORIENTED_EDGE ( 'NONE', *, *, #11180, .T. ) ;
#43011 = CARTESIAN_POINT ( 'NONE',  ( 25.10985785448133356, -2.855902626858047633, 11.47560089494121094 ) ) ;
#43012 = CARTESIAN_POINT ( 'NONE',  ( 24.66708179568188442, -8.738412506716594308, -9.169048261100254393 ) ) ;
#43013 = CARTESIAN_POINT ( 'NONE',  ( 11.48381255716000027, 12.35454260995000020, 1.695649549036999826 ) ) ;
#43014 = CARTESIAN_POINT ( 'NONE',  ( 18.19141764354314716, 2.135256814392525460, 12.41776106013548464 ) ) ;
#43015 = CARTESIAN_POINT ( 'NONE',  ( 10.96255546505999945, 6.761651470398000185, 5.456355616689999799 ) ) ;
#43017 = CARTESIAN_POINT ( 'NONE',  ( 11.13997082032999941, 9.835715680716001330, 6.100895928452999328 ) ) ;
#43016 = B_SPLINE_CURVE_WITH_KNOTS ( 'NONE', 3,
 ( #57470, #52577, #36499, #9232, #40714, #51546, #9577, #14499 ),
 .UNSPECIFIED., .F., .F.,
 ( 4, 2, 2, 4 ),
 ( 0.000000000000000000, 0.2500000000000000000, 0.5000000000000000000, 1.000000000000000000 ),
 .UNSPECIFIED. ) ;
#43018 = CARTESIAN_POINT ( 'NONE',  ( 12.54858945020884065, -0.5700410258314839718, -12.68277524907877130 ) ) ;
#43019 = CARTESIAN_POINT ( 'NONE',  ( -15.86200481174999943, 2.399999999999999911, -6.571291218949999902 ) ) ;
#43020 = AXIS2_PLACEMENT_3D ( 'NONE', #45614, #7164, #39676 ) ;
#43021 = ORIENTED_EDGE ( 'NONE', *, *, #5998, .F. ) ;
#43022 = CARTESIAN_POINT ( 'NONE',  ( 12.16862919417109268, -2.135222488495310600, 12.41776696322756735 ) ) ;
#43023 = CARTESIAN_POINT ( 'NONE',  ( 10.06027973160899869, -3.909869487835140323, -6.499640669006000238 ) ) ;
#43024 = CARTESIAN_POINT ( 'NONE',  ( 21.70000133425200062, 14.00000000000000000, 0.000000000000000000 ) ) ;
#43025 = EDGE_CURVE ( 'NONE', #52126, #64582, #46594, .T. ) ;
#43026 = CARTESIAN_POINT ( 'NONE',  ( 8.300444773060121406, 2.921714170698993751, -6.487055555563432385 ) ) ;
#43027 = CARTESIAN_POINT ( 'NONE',  ( 11.17410807141120088, -3.953638752893899877, 6.497602131078999754 ) ) ;
#43028 = B_SPLINE_SURFACE_WITH_KNOTS ( 'NONE', 1, 3, ( 
 ( #66743, #56944, #30381, #41211, #14976, #34946, #9374, #61843, #18861, #61504, #36300, #56260, #59007, #59343, #58312, #5855, #47487, #64232, #68444, #26505, #58657, #10758, #36652, #21589, #32102, #27196, #48515, #37333, #64579, #53419, #52723, #37677, #5516, #15325, #26857, #57974, #275, #10072, #20564, #52377, #48170, #41891, #11108, #25811, #624, #42582, #21933, #42927, #43271, #63197, #31409, #4820, #26162, #68793, #16349, #32443, #20911, #4473, #42248, #16689, #53758, #38017, #63553, #31071, #47143, #15668, #36997, #10413, #31755, #53073, #5172, #69145, #47836, #21253, #63890, #16005, #49543, #54447, #27890, #22284, #59691, #43625, #55488, #23327, #39758, #44667, #22972, #7243, #64919, #33478, #54793, #49202, #17033, #34169, #972, #7588, #28938, #65274, #38366, #11792, #1655, #12490, #39407, #33825, #2004, #6548, #28228, #60038 ),
 ( #65961, #17388, #33132, #6195, #6892, #50241, #48863, #28581, #12842, #27538, #2345, #1309, #60727, #44322, #23665, #65619, #39065, #17745, #60385, #22624, #11444, #55140, #49895, #32785, #12150, #43969, #54100, #45002, #18085, #66309, #18433, #38718, #41126, #3702, #35205, #50929, #30636, #13196, #7938, #18777, #35545, #46025, #25041, #56514, #62098, #34524, #3028, #13874, #55834, #8621, #29969, #14560, #56863, #68023, #29274, #61755, #8960, #30300, #8282, #67333, #51606, #51272, #19107, #19801, #40107, #19453, #46720, #3366, #24703, #66996, #13538, #40774, #61420, #20139, #46373, #50588, #61077, #29625, #66658, #34857, #2688, #4045, #56172, #24014, #14216, #67673, #62439, #51946, #45348, #24358, #35878, #57193, #25382, #45690, #40429, #9294, #27368, #11971, #28062, #49372, #48341, #54626, #41469, #52297, #16866, #1144, #22454, #64750 ) ),
 .UNSPECIFIED., .F., .F., .F.,
 ( 2, 2 ),
 ( 4, 2, 2, 2, 2, 2, 2, 2, 2, 2, 2, 2, 2, 2, 2, 2, 2, 2, 2, 2, 2, 2, 2, 2, 2, 2, 2, 2, 2, 2, 2, 2, 2, 2, 2, 2, 2, 2, 2, 2, 2, 2, 2, 2, 2, 2, 2, 2, 2, 2, 2, 2, 2, 4 ),
 ( 0.000000000000000000, 1.000000000000000000 ),
 ( 0.000000000000000000, 7.157214214794704388E-05, 0.0001431442842958940878, 0.0001789303553698675894, 0.0002147164264438411181, 0.0002326094619808278825, 0.0002505024975178146468, 0.0002862885685917881755, 0.0003220746396657616500, 0.0003578607107397351788, 0.0003936467818137087075, 0.0004294328528876822362, 0.0004652189239616557649, 0.0004831119594986425293, 0.0005010049950356292936, 0.0005725771371835763511, 0.0006441492793315233001, 0.0007157214214794703575, 0.0007872935636274174150, 0.0008588657057753644724, 0.0008946517768493380011, 0.0009304378479233115298, 0.0009662239189972850585, 0.001002009990071258587, 0.001037796061145232224, 0.001073582132219205645, 0.001145154274367152702, 0.001180940345441126339, 0.001216726416515099760, 0.001252512487589073180, 0.001288298558663046600, 0.001359870700810993658, 0.001395656771884967295, 0.001431442842958940715, 0.001467228914032914135, 0.001503014985106887772, 0.001574587127254834830, 0.001646159269402781887, 0.001681945340476755524, 0.001717731411550728945, 0.001753517482624702365, 0.001789303553698676002, 0.001860875695846623060, 0.001896661766920596480, 0.001932447837994570117, 0.001968233909068543754, 0.002004019980142517175, 0.002039806051216491029, 0.002075592122290464449, 0.002147164264438411289, 0.002182950335512384710, 0.002218736406586358130, 0.002254522477660331550, 0.002290308548734305404 ),
 .UNSPECIFIED. ) ;
#43029 = CARTESIAN_POINT ( 'NONE',  ( 10.74795391537419853, 4.830118059977199785, -8.063786182297898009 ) ) ;
#43030 = CARTESIAN_POINT ( 'NONE',  ( 8.726787239609997471, 3.780467314030099946, 6.659501631675699862 ) ) ;
#43031 = CARTESIAN_POINT ( 'NONE',  ( 0.3678308122907000266, 2.092960143115000005, 2.433246087927000367 ) ) ;
#43032 = CARTESIAN_POINT ( 'NONE',  ( 8.745593092018999926, 5.100000000000000533, 6.404090157675000228 ) ) ;
#43033 = CARTESIAN_POINT ( 'NONE',  ( 12.22009801487423175, 2.720357631080353666, 12.39749406087476302 ) ) ;
#43035 = CARTESIAN_POINT ( 'NONE',  ( 18.49993212792200126, -2.908182645667999999, -12.18276646858999968 ) ) ;
#43034 = CARTESIAN_POINT ( 'NONE',  ( 9.707684229509998985, 3.195116560491999991, -6.690125258578699885 ) ) ;
#43036 = CARTESIAN_POINT ( 'NONE',  ( 10.71918447801630059, 5.140463864104999558, -7.474854604063350116 ) ) ;
#43037 = CARTESIAN_POINT ( 'NONE',  ( 7.572352458090005456, 3.472372354340000911, -6.527657354165006254 ) ) ;
#43038 = CARTESIAN_POINT ( 'NONE',  ( 17.60000000064766823, 12.03387897622311797, -3.206083669095133981 ) ) ;
#43039 = CARTESIAN_POINT ( 'NONE',  ( 0.07500022993665000914, 0.000000000000000000, -2.325000277643999969 ) ) ;
#43041 = CARTESIAN_POINT ( 'NONE',  ( 9.934999999999998721, -4.640430492595999823, -9.117542781427999898 ) ) ;
#43040 = CARTESIAN_POINT ( 'NONE',  ( 12.80000000000000071, 10.78295181803999903, -4.410266442048000002 ) ) ;
#43042 = CARTESIAN_POINT ( 'NONE',  ( 16.39999999231800132, 3.216285993016000155, 11.40340220863999932 ) ) ;
#43043 = ORIENTED_EDGE ( 'NONE', *, *, #10951, .F. ) ;
#43044 = CARTESIAN_POINT ( 'NONE',  ( 12.21982330445614195, 0.2196444115568565170, 12.69744877134261429 ) ) ;
#43045 = CARTESIAN_POINT ( 'NONE',  ( 7.773264469372000107, 2.859518616742000141, 6.768376720750000075 ) ) ;
#43046 = EDGE_CURVE ( 'NONE', #10323, #54361, #26652, .T. ) ;
#43047 = CARTESIAN_POINT ( 'NONE',  ( 11.09999999999999964, 4.000000000000000000, -7.500000000000000000 ) ) ;
#43048 = CARTESIAN_POINT ( 'NONE',  ( 17.92259505138787290, 3.107618780086595311, -12.21081961728242504 ) ) ;
#43049 = ADVANCED_FACE ( 'NONE', ( #998 ), #52904, .T. ) ;
#43050 = CARTESIAN_POINT ( 'NONE',  ( 12.54721708147389059, -1.835134883933975392, 13.87920628830545411 ) ) ;
#43051 = CARTESIAN_POINT ( 'NONE',  ( 11.13228700200999910, 2.679094735942999961, 4.957687805034000306 ) ) ;
#43052 = CARTESIAN_POINT ( 'NONE',  ( 12.80505043854143388, 1.845932447629014872, 13.81930785430178155 ) ) ;
#43053 = ORIENTED_EDGE ( 'NONE', *, *, #1099, .T. ) ;
#43054 = PLANE ( 'NONE',  #30417 ) ;
#43055 = CARTESIAN_POINT ( 'NONE',  ( 8.571413182547999554, 4.599999999999999645, 5.927302706106000407 ) ) ;
#43056 = FACE_OUTER_BOUND ( 'NONE', #3369, .T. ) ;
#43057 = CARTESIAN_POINT ( 'NONE',  ( 11.19568717260499824, -4.466067913030199676, 6.739296831621899742 ) ) ;
#43058 = CARTESIAN_POINT ( 'NONE',  ( 17.88706890093970259, 3.029615921040858861, -12.31227368058699767 ) ) ;
#43059 = CARTESIAN_POINT ( 'NONE',  ( 21.00000000000000000, 11.79499999999999993, 0.000000000000000000 ) ) ;
#43060 = FACE_OUTER_BOUND ( 'NONE', #12030, .T. ) ;
#43061 = CARTESIAN_POINT ( 'NONE',  ( 11.79999999771000141, -3.595163221087000149, 11.99793848941000007 ) ) ;
#43062 = CARTESIAN_POINT ( 'NONE',  ( 10.08211398012999993, -4.728049789772000189, -8.793977405422999993 ) ) ;
#43063 = CARTESIAN_POINT ( 'NONE',  ( 12.15646016996021217, 2.140061664406224917, 13.83614491990443085 ) ) ;
#43064 = CARTESIAN_POINT ( 'NONE',  ( 25.29986325275000070, 2.078227429405999693, 11.31065739696999906 ) ) ;
#43065 = CARTESIAN_POINT ( 'NONE',  ( 24.46729256464000457, 12.16659091368999945, 3.168154674931000336 ) ) ;
#43066 = DIRECTION ( 'NONE',  ( -4.331025598861020273E-21, -3.276905820014099985E-06, 0.9999999999946310725 ) ) ;
#43067 = ORIENTED_EDGE ( 'NONE', *, *, #31067, .F. ) ;
#43068 = CARTESIAN_POINT ( 'NONE',  ( 7.349539055719287006, 3.476414806253772749, 9.161239507722385156 ) ) ;
#43069 = CARTESIAN_POINT ( 'NONE',  ( 11.67056785386840012, -4.718624889240500053, 7.016391833292499491 ) ) ;
#43070 = ORIENTED_EDGE ( 'NONE', *, *, #7179, .F. ) ;
#43071 = AXIS2_PLACEMENT_3D ( 'NONE', #13359, #23834, #55999 ) ;
#43072 = CARTESIAN_POINT ( 'NONE',  ( 24.63332964936066816, 10.83443035059421433, -3.855530959300003335 ) ) ;
#43073 = CARTESIAN_POINT ( 'NONE',  ( 10.86687616594229944, -4.344946439135400240, -6.412662853391999818 ) ) ;
#43074 = ORIENTED_EDGE ( 'NONE', *, *, #32405, .T. ) ;
#43075 = CARTESIAN_POINT ( 'NONE',  ( 10.93990547754509812, 5.032986398992000510, 7.467215766047949899 ) ) ;
#43076 = CARTESIAN_POINT ( 'NONE',  ( 6.326199169711658854, -1.131438764395593655, 0.04874608710810101470 ) ) ;
#43077 = CARTESIAN_POINT ( 'NONE',  ( 23.74395678421098310, 3.264333397773110157, -13.24373423702363617 ) ) ;
#43078 = CONICAL_SURFACE ( 'NONE', #31914, 1.200857723089999940, 0.7853979760808852406 ) ;
#43079 = CARTESIAN_POINT ( 'NONE',  ( 1.700000000000000178, -1.500000000000000000, 0.000000000000000000 ) ) ;
#43080 = CARTESIAN_POINT ( 'NONE',  ( 11.19434208742519843, -4.478858766422799675, -8.252717006421999457 ) ) ;
#43081 = CARTESIAN_POINT ( 'NONE',  ( 12.18002302684027960, -0.03981422837198456133, -13.90000146831368255 ) ) ;
#43082 = CARTESIAN_POINT ( 'NONE',  ( 6.868195110880497722, -1.013868087716280009, -0.5278221404403410366 ) ) ;
#43083 = B_SPLINE_CURVE_WITH_KNOTS ( 'NONE', 3,
 ( #24285, #2274, #23592, #34450 ),
 .UNSPECIFIED., .F., .F.,
 ( 4, 4 ),
 ( 0.000000000000000000, 1.000000000000000000 ),
 .UNSPECIFIED. ) ;
#43084 = CARTESIAN_POINT ( 'NONE',  ( 9.675541251098000117, -4.656741678598999457, -8.653222148251000334 ) ) ;
#43085 = CARTESIAN_POINT ( 'NONE',  ( 12.99421883851900184, 11.64667883987999986, 1.861676925984000031 ) ) ;
#43086 = ORIENTED_EDGE ( 'NONE', *, *, #37092, .F. ) ;
#43087 = EDGE_CURVE ( 'NONE', #17344, #26163, #39157, .T. ) ;
#43088 = ADVANCED_FACE ( 'NONE', ( #48810 ), #6346, .T. ) ;
#43089 = CARTESIAN_POINT ( 'NONE',  ( 8.621524209948821849, 3.647212272540921951, 8.851469415033248467 ) ) ;
#43090 = ORIENTED_EDGE ( 'NONE', *, *, #52164, .F. ) ;
#43091 = AXIS2_PLACEMENT_3D ( 'NONE', #64344, #23090, #37449 ) ;
#43092 = CARTESIAN_POINT ( 'NONE',  ( 10.69601354018300832, 4.999583552997727054, -6.731816600031361730 ) ) ;
#43093 = PRESENTATION_STYLE_ASSIGNMENT (( #59858 ) ) ;
#43094 = ORIENTED_EDGE ( 'NONE', *, *, #45146, .F. ) ;
#43095 = CARTESIAN_POINT ( 'NONE',  ( 11.50029455687000102, -11.56505190006999939, -1.404305717648999918 ) ) ;
#43096 = CARTESIAN_POINT ( 'NONE',  ( 17.93780763597379391, -2.994506166037827821, -12.32249531978309065 ) ) ;
#43097 = AXIS2_PLACEMENT_3D ( 'NONE', #19878, #41207, #67413 ) ;
#43098 = CARTESIAN_POINT ( 'NONE',  ( 10.55661746422400959, -2.989346313686768397, 5.028522878686708886 ) ) ;
#43099 = CARTESIAN_POINT ( 'NONE',  ( 13.49994651945300284, 12.07042783918999795, 2.492331243371999960 ) ) ;
#43100 = CARTESIAN_POINT ( 'NONE',  ( 11.18483536755999808, -2.599651619047000040, 7.740676724427999922 ) ) ;
#43101 = CARTESIAN_POINT ( 'NONE',  ( 18.05693606625744252, -2.118559450820218792, -12.53247283883959007 ) ) ;
#43102 = CARTESIAN_POINT ( 'NONE',  ( 12.30864111941012951, 0.3802875570022034579, 13.89301034115782940 ) ) ;
#43103 = ORIENTED_EDGE ( 'NONE', *, *, #18280, .F. ) ;
#43104 = CARTESIAN_POINT ( 'NONE',  ( 12.79484580939900162, 11.81466332729999991, -3.323431527667999763 ) ) ;
#43105 = CARTESIAN_POINT ( 'NONE',  ( 18.15988268186300303, 12.12177778538999995, -3.303327906654999868 ) ) ;
#43106 = ADVANCED_FACE ( 'NONE', ( #43569 ), #53480, .T. ) ;
#43107 = CARTESIAN_POINT ( 'NONE',  ( 9.125583543129625497, 3.128114063008116563, 7.426875573188317148 ) ) ;
#43108 = CARTESIAN_POINT ( 'NONE',  ( 5.063547794415999448, 1.011671888745000025, 0.8705125097731000183 ) ) ;
#43109 = CARTESIAN_POINT ( 'NONE',  ( 9.047164158776000775, 2.156584729807999867, -7.959751745006000689 ) ) ;
#43110 = CARTESIAN_POINT ( 'NONE',  ( 17.60000001947600268, -11.86186880240999919, 3.298627760718999991 ) ) ;
#43111 = CARTESIAN_POINT ( 'NONE',  ( 10.20917469696999902, -3.334764780022000163, -5.769478358936999562 ) ) ;
#43112 = ORIENTED_EDGE ( 'NONE', *, *, #24106, .F. ) ;
#43113 = VERTEX_POINT ( 'NONE', #24306 ) ;
#43114 = CARTESIAN_POINT ( 'NONE',  ( 10.87371169224999967, 5.064035864983999602, -5.107130734103000336 ) ) ;
#43115 = CARTESIAN_POINT ( 'NONE',  ( 17.92254446318295535, -3.154612309593181507, 13.64000973912208003 ) ) ;
#43116 = FACE_OUTER_BOUND ( 'NONE', #23353, .T. ) ;
#43117 = CARTESIAN_POINT ( 'NONE',  ( 6.000859839683335473, -0.3926218265389255779, 1.460959015002472494 ) ) ;
#43118 = B_SPLINE_CURVE_WITH_KNOTS ( 'NONE', 3,
 ( #9688, #25778, #68406, #37637 ),
 .UNSPECIFIED., .F., .F.,
 ( 4, 4 ),
 ( 0.000000000000000000, 1.000000000000000000 ),
 .UNSPECIFIED. ) ;
#43119 = CARTESIAN_POINT ( 'NONE',  ( 11.05435090131019926, 5.119447121461000449, -8.192386390235398608 ) ) ;
#43120 = CARTESIAN_POINT ( 'NONE',  ( 9.659988259785999176, 3.868581654116200141, -8.495776841814999258 ) ) ;
#43122 = CARTESIAN_POINT ( 'NONE',  ( 4.399769195526705978, -0.2610650747889547429, -1.154523729464906001 ) ) ;
#43121 = CARTESIAN_POINT ( 'NONE',  ( 10.10234252387499865, -4.857027829858100887, 7.631191628371899682 ) ) ;
#43123 = CARTESIAN_POINT ( 'NONE',  ( 8.212419626809003503, -3.104180672527999896, 6.104185052591001082 ) ) ;
#43124 = EDGE_LOOP ( 'NONE', ( #52352, #25761, #63464, #67243 ) ) ;
#43125 = DIRECTION ( 'NONE',  ( -1.000000000000000000, 0.000000000000000000, 0.000000000000000000 ) ) ;
#43126 = VECTOR ( 'NONE', #59141, 1000.000000000000227 ) ;
#43127 = CARTESIAN_POINT ( 'NONE',  ( 10.83668192271000130, -4.288535286065000562, 9.448729895547000268 ) ) ;
#43128 = CARTESIAN_POINT ( 'NONE',  ( 9.530380199233999150, 5.132898093246000215, 7.642395078236999595 ) ) ;
#43129 = CARTESIAN_POINT ( 'NONE',  ( 4.605026506348999682, -1.500000000000000000, 0.000000000000000000 ) ) ;
#43130 = CARTESIAN_POINT ( 'NONE',  ( 10.58844302970999962, -3.754658547780000521, 5.545362468768000319 ) ) ;
#43131 = ADVANCED_FACE ( 'NONE', ( #35493 ), #9587, .F. ) ;
#43132 = CARTESIAN_POINT ( 'NONE',  ( 18.05168367658140838, 2.879595443362037432, -12.35500515152453538 ) ) ;
#43133 = CARTESIAN_POINT ( 'NONE',  ( 16.20679720086500097, -3.450734216086000394, -11.08786462205999968 ) ) ;
#43134 = CARTESIAN_POINT ( 'NONE',  ( 8.824126402770998467, -3.060189502158800146, -7.145601175474399547 ) ) ;
#43135 = VECTOR ( 'NONE', #62230, 1000.000000000000114 ) ;
#43136 = CARTESIAN_POINT ( 'NONE',  ( 5.219320540948999998, -0.1144865814785000074, 1.118427654993999987 ) ) ;
#43137 = CARTESIAN_POINT ( 'NONE',  ( 23.60000000000000142, 2.258942858049999725, -12.29419282279000036 ) ) ;
#43138 = FACE_OUTER_BOUND ( 'NONE', #2163, .T. ) ;
#43139 = EDGE_LOOP ( 'NONE', ( #5333, #10501, #6905, #20748, #17202 ) ) ;
#43140 = CARTESIAN_POINT ( 'NONE',  ( 12.23574065127464827, -0.2580991232524066925, -12.69647497719791573 ) ) ;
#43141 = B_SPLINE_CURVE_WITH_KNOTS ( 'NONE', 3,
 ( #41478, #9998, #8970, #51281 ),
 .UNSPECIFIED., .F., .F.,
 ( 4, 4 ),
 ( 0.000000000000000000, 1.000000000000000000 ),
 .UNSPECIFIED. ) ;
#43142 = B_SPLINE_CURVE_WITH_KNOTS ( 'NONE', 3,
 ( #38105, #63292, #59431, #31166 ),
 .UNSPECIFIED., .F., .F.,
 ( 4, 4 ),
 ( 0.000000000000000000, 1.000000000000000000 ),
 .UNSPECIFIED. ) ;
#43143 = CARTESIAN_POINT ( 'NONE',  ( 10.80133863405319872, 4.534404523786000674, -8.181696703306599261 ) ) ;
#43144 = CARTESIAN_POINT ( 'NONE',  ( 17.80000000001300009, -3.351264566333000072, -11.15757590352999884 ) ) ;
#43145 = FACE_OUTER_BOUND ( 'NONE', #54183, .T. ) ;
#43146 = CARTESIAN_POINT ( 'NONE',  ( 10.76537527815838580, 5.100000000000000533, 6.445686799303629755 ) ) ;
#43147 = VERTEX_POINT ( 'NONE', #51555 ) ;
#43148 = CARTESIAN_POINT ( 'NONE',  ( 7.486137746321728237, -5.349333099367949096, 7.677008113425388025 ) ) ;
#43149 = CARTESIAN_POINT ( 'NONE',  ( 11.19434208742519843, -4.478858766422799675, -8.252717006421999457 ) ) ;
#43150 = FACE_OUTER_BOUND ( 'NONE', #13541, .T. ) ;
#43151 = CARTESIAN_POINT ( 'NONE',  ( 12.79999999914999975, -12.11987927271999865, 3.159802730921999814 ) ) ;
#43152 = CARTESIAN_POINT ( 'NONE',  ( 10.91301932002725650, 2.749999999999998224, -7.799851088612626882 ) ) ;
#43153 = CARTESIAN_POINT ( 'NONE',  ( 11.27745123989519982, 4.410212499603100689, -8.292221125039500151 ) ) ;
#43154 = EDGE_LOOP ( 'NONE', ( #18253, #42064, #61348, #1714 ) ) ;
#43155 = CARTESIAN_POINT ( 'NONE',  ( 10.55813551225999980, -2.466564559586000183, 6.633531786299999844 ) ) ;
#43156 = CARTESIAN_POINT ( 'NONE',  ( 18.12467946932835616, 2.757395321821673129, -13.61549383066601138 ) ) ;
#43157 = VERTEX_POINT ( 'NONE', #46669 ) ;
#43158 = CARTESIAN_POINT ( 'NONE',  ( 7.307500000000000107, 0.2999999999999999889, -3.149999999999999911 ) ) ;
#43159 = CARTESIAN_POINT ( 'NONE',  ( 25.12927996638910955, 8.519456805637897645, -8.174607305189095285 ) ) ;
#43160 = CARTESIAN_POINT ( 'NONE',  ( 8.474089158773999486, 4.131080973160000447, -6.108642999115999395 ) ) ;
#43161 = ORIENTED_EDGE ( 'NONE', *, *, #6209, .T. ) ;
#43162 = DIRECTION ( 'NONE',  ( -1.000000000000000000, 3.552713679099000216E-14, -7.105427358198000432E-14 ) ) ;
#43163 = CARTESIAN_POINT ( 'NONE',  ( 7.563935841224999734, 2.455281733534999677, -8.606072783617999988 ) ) ;
#43164 = CARTESIAN_POINT ( 'NONE',  ( 10.33351354018233259, -5.249999999999999112, -7.336375382625531572 ) ) ;
#43165 = CARTESIAN_POINT ( 'NONE',  ( 9.424850063658244181, 5.349972463430670899, 7.500009360578276052 ) ) ;
#43166 = ORIENTED_EDGE ( 'NONE', *, *, #62529, .F. ) ;
#43167 = CARTESIAN_POINT ( 'NONE',  ( 10.03491210303999992, -5.615910465798999773, 7.351455544018000943 ) ) ;
#43168 = EDGE_CURVE ( 'NONE', #27228, #16591, #34956, .T. ) ;
#43169 = ADVANCED_FACE ( 'NONE', ( #67285 ), #35827, .F. ) ;
#43170 = CARTESIAN_POINT ( 'NONE',  ( 24.85113676206800193, 11.95314342760000059, -2.993325325037999640 ) ) ;
#43171 = PLANE ( 'NONE',  #41678 ) ;
#43172 = ORIENTED_EDGE ( 'NONE', *, *, #4827, .T. ) ;
#43173 = AXIS2_PLACEMENT_3D ( 'NONE', #37999, #33114, #64902 ) ;
#43174 = CARTESIAN_POINT ( 'NONE',  ( 6.294609839683335650, 1.500000000000001110, -0.1963495408493590721 ) ) ;
#43175 = LINE ( 'NONE', #16602, #7443 ) ;
#43176 = ORIENTED_EDGE ( 'NONE', *, *, #9597, .F. ) ;
#43177 = CARTESIAN_POINT ( 'NONE',  ( 6.553816671982000130, -1.199981415667000118, 0.9000247785775999931 ) ) ;
#43178 = CARTESIAN_POINT ( 'NONE',  ( 18.16417894366983177, 0.1413088920345111354, -13.89905105385967943 ) ) ;
#43179 = CARTESIAN_POINT ( 'NONE',  ( 4.317328812926999326, 0.6646734451123000875, 1.217994223230000062 ) ) ;
#43180 = AXIS2_PLACEMENT_3D ( 'NONE', #11259, #16848, #21406 ) ;
#43181 = CARTESIAN_POINT ( 'NONE',  ( 8.229591223330004368, 5.116109178766001797, -6.360512773592004621 ) ) ;
#43182 = CARTESIAN_POINT ( 'NONE',  ( 16.43164332880499856, 3.528999066054999467, 11.96046905204000055 ) ) ;
#43183 = CARTESIAN_POINT ( 'NONE',  ( 7.189449102910221434, 4.002238097908506376, -8.883099350742211797 ) ) ;
#43184 = CARTESIAN_POINT ( 'NONE',  ( 24.15455527622187049, 12.45781941376721136, 3.353847473082901764 ) ) ;
#43185 = CIRCLE ( 'NONE', #16375, 3.200000000000000178 ) ;
#43186 = ORIENTED_EDGE ( 'NONE', *, *, #6209, .F. ) ;
#43187 = CARTESIAN_POINT ( 'NONE',  ( 8.741252916288999586, 4.092558584984410608, -8.374574604871998673 ) ) ;
#43188 = VERTEX_POINT ( 'NONE', #3653 ) ;
#43189 = CARTESIAN_POINT ( 'NONE',  ( 9.889842476439000052, 4.052276433608000161, 9.260531940735001299 ) ) ;
#43190 = CARTESIAN_POINT ( 'NONE',  ( 10.83253786428999987, 2.899999999999999911, 6.571291218949999902 ) ) ;
#43191 = EDGE_CURVE ( 'NONE', #55845, #12182, #758, .T. ) ;
#43192 = LINE ( 'NONE', #38284, #37428 ) ;
#43193 = CIRCLE ( 'NONE', #35374, 12.50000000000000000 ) ;
#43194 = CARTESIAN_POINT ( 'NONE',  ( 12.58320380180958509, 3.084393765090617467, -13.53199207997350584 ) ) ;
#43195 = CARTESIAN_POINT ( 'NONE',  ( 9.216851002545999094, 2.832432432432000269, 6.822293592207000934 ) ) ;
#43196 = ADVANCED_FACE ( 'NONE', ( #8571 ), #29917, .F. ) ;
#43197 = CARTESIAN_POINT ( 'NONE',  ( 4.600000127571202135, -13.89999852641999922, 0.000000000000000000 ) ) ;
#43198 = CARTESIAN_POINT ( 'NONE',  ( 18.13658220607009142, -0.2292390942789229447, 13.89746050377130793 ) ) ;
#43199 = CARTESIAN_POINT ( 'NONE',  ( 24.59232786471100241, -3.480949894194999672, 12.13588334916000022 ) ) ;
#43200 = VERTEX_POINT ( 'NONE', #48375 ) ;
#43201 = VECTOR ( 'NONE', #58803, 1000.000000000000000 ) ;
#43202 = CARTESIAN_POINT ( 'NONE',  ( 12.64393528606200334, -11.55448221446000012, 4.935476321030999536 ) ) ;
#43203 = CARTESIAN_POINT ( 'NONE',  ( 11.19041504065829962, -2.975441626403999784, 8.263934892306599167 ) ) ;
#43204 = DIRECTION ( 'NONE',  ( 0.000000000000000000, 0.000000000000000000, 1.000000000000000000 ) ) ;
#43205 = DIRECTION ( 'NONE',  ( 1.000000000000000000, 0.000000000000000000, 0.000000000000000000 ) ) ;
#43206 = CARTESIAN_POINT ( 'NONE',  ( 9.170316940378999249, -5.558929022707999046, 6.272984818914999927 ) ) ;
#43208 = CARTESIAN_POINT ( 'NONE',  ( 10.98768472639999949, 0.3876847264043000174, 4.945212061661000469 ) ) ;
#43207 = CARTESIAN_POINT ( 'NONE',  ( 10.40726830891999910, 3.797905842462999892, 5.889914049998000500 ) ) ;
#43209 = CARTESIAN_POINT ( 'NONE',  ( 10.94072200990529886, 2.922907051630999842, -7.124286150322599376 ) ) ;
#43210 = CARTESIAN_POINT ( 'NONE',  ( 24.60170725920900026, -8.811863727701000570, -9.296544040758000449 ) ) ;
#43211 = LINE ( 'NONE', #28525, #55287 ) ;
#43212 = CARTESIAN_POINT ( 'NONE',  ( 18.15872281507842345, -0.1622035078961262533, 12.69861136640059129 ) ) ;
#43213 = DIRECTION ( 'NONE',  ( -1.000000000000000000, 0.000000000000000000, 0.000000000000000000 ) ) ;
#43214 = CARTESIAN_POINT ( 'NONE',  ( 17.79999999998900151, -3.595165934733000057, 11.99793354950999991 ) ) ;
#43215 = ORIENTED_EDGE ( 'NONE', *, *, #21237, .T. ) ;
#43216 = CARTESIAN_POINT ( 'NONE',  ( 9.021581853209999835, -2.193670085072000120, 7.400591740205000768 ) ) ;
#43217 = CARTESIAN_POINT ( 'NONE',  ( 9.179055905797000037, -2.899999999999999911, 6.571291218949999902 ) ) ;
#43218 = CARTESIAN_POINT ( 'NONE',  ( 17.55505043854143565, 1.760910691117812954, 12.47634535983622861 ) ) ;
#43219 = DIRECTION ( 'NONE',  ( 1.000000000000000000, 0.000000000000000000, 0.000000000000000000 ) ) ;
#43220 = AXIS2_PLACEMENT_3D ( 'NONE', #32972, #54284, #7087 ) ;
#43221 = B_SPLINE_CURVE_WITH_KNOTS ( 'NONE', 3,
 ( #42403, #89, #10234, #5329 ),
 .UNSPECIFIED., .F., .F.,
 ( 4, 4 ),
 ( 0.000000000000000000, 1.000000000000000000 ),
 .UNSPECIFIED. ) ;
#43222 = CARTESIAN_POINT ( 'NONE',  ( 0.6256366850171000138, -2.634961698279000064, 2.360490016663000290 ) ) ;
#43223 = CARTESIAN_POINT ( 'NONE',  ( 10.73213259636989925, 3.092475607087700418, 7.005495010505599751 ) ) ;
#43224 = CARTESIAN_POINT ( 'NONE',  ( 10.19794834123000093, 4.262170647947000290, -8.834315641189999013 ) ) ;
#43225 = PRODUCT_DEFINITION ( 'UNKNOWN', '', #22913, #44184 ) ;
#43226 = VERTEX_POINT ( 'NONE', #37536 ) ;
#43227 = EDGE_CURVE ( 'NONE', #14826, #38133, #60826, .T. ) ;
#43228 = CARTESIAN_POINT ( 'NONE',  ( 12.57206729000417056, -0.6812425322175689191, -12.58157083403807164 ) ) ;
#43229 = CYLINDRICAL_SURFACE ( 'NONE', #28687, 1.250000000000000222 ) ;
#43230 = CARTESIAN_POINT ( 'NONE',  ( 18.00816351061646969, 3.042045466722131941, -12.22726353680069344 ) ) ;
#43231 = CARTESIAN_POINT ( 'NONE',  ( 5.614176421965364483, 12.11993299477459551, 3.746642824816280637 ) ) ;
#43233 = CARTESIAN_POINT ( 'NONE',  ( 8.218892219592001780, 3.011620138462000273, 8.801434747080000065 ) ) ;
#43232 = PRESENTATION_LAYER_ASSIGNMENT (  '', '', ( #19781 ) ) ;
#43234 = ORIENTED_EDGE ( 'NONE', *, *, #4718, .F. ) ;
#43235 = CARTESIAN_POINT ( 'NONE',  ( 6.536630799317000751, -1.539848055637000002, 0.4860074956841999860 ) ) ;
#43236 = CARTESIAN_POINT ( 'NONE',  ( 8.576820280409998887, 4.814347755891000169, -8.757164289523000633 ) ) ;
#43237 = CARTESIAN_POINT ( 'NONE',  ( 8.449083656217606375, -2.260425563746147670, 7.515772993398566193 ) ) ;
#43238 = CONICAL_SURFACE ( 'NONE', #3018, 1.900023899775999947, 0.7853981633972997312 ) ;
#43239 = CARTESIAN_POINT ( 'NONE',  ( 9.294772138681999252, -4.476015718025199597, 8.687347221188998603 ) ) ;
#43240 = ORIENTED_EDGE ( 'NONE', *, *, #27478, .T. ) ;
#43241 = CARTESIAN_POINT ( 'NONE',  ( 11.30000285318000230, 11.76356368987999979, 1.428410073821000159 ) ) ;
#43242 = CARTESIAN_POINT ( 'NONE',  ( 11.35619132127000164, 11.69822877698999974, 1.509327410273999970 ) ) ;
#43243 = ORIENTED_EDGE ( 'NONE', *, *, #46571, .F. ) ;
#43244 = CARTESIAN_POINT ( 'NONE',  ( 12.80505043854143388, 3.199751711897557804, -12.18694338143115630 ) ) ;
#43245 = CARTESIAN_POINT ( 'NONE',  ( 6.983162019845000401, 12.13278763737000077, 3.076796177952999756 ) ) ;
#43246 = CARTESIAN_POINT ( 'NONE',  ( 17.71666486338982338, -0.6040897852209337060, -13.88232707694115398 ) ) ;
#43247 = ORIENTED_EDGE ( 'NONE', *, *, #52838, .T. ) ;
#43248 = CARTESIAN_POINT ( 'NONE',  ( 10.62788468813516474, -2.420134780600908364, -6.689474005288416514 ) ) ;
#43249 = FACE_OUTER_BOUND ( 'NONE', #1491, .T. ) ;
#43250 = AXIS2_PLACEMENT_3D ( 'NONE', #63348, #36448, #4624 ) ;
#43251 = DIRECTION ( 'NONE',  ( 0.000000000000000000, -1.000000000000000000, 0.000000000000000000 ) ) ;
#43252 = DIRECTION ( 'NONE',  ( -1.000000000000000000, 0.000000000000000000, 0.000000000000000000 ) ) ;
#43253 = CARTESIAN_POINT ( 'NONE',  ( 11.36272200990529946, -5.206705454565000224, 7.920925559347199219 ) ) ;
#43254 = ORIENTED_EDGE ( 'NONE', *, *, #48466, .T. ) ;
#43255 = CARTESIAN_POINT ( 'NONE',  ( 7.705392219590000202, 3.245534453799999941, 8.949623695221001540 ) ) ;
#43256 = EDGE_CURVE ( 'NONE', #28703, #68545, #39912, .T. ) ;
#43257 = EDGE_CURVE ( 'NONE', #10372, #15717, #19790, .T. ) ;
#43258 = ORIENTED_EDGE ( 'NONE', *, *, #13887, .T. ) ;
#43259 = LINE ( 'NONE', #49531, #10565 ) ;
#43260 = EDGE_CURVE ( 'NONE', #32830, #37266, #45845, .T. ) ;
#43261 = CARTESIAN_POINT ( 'NONE',  ( 15.95500032369699994, -8.890098389148999303, -8.614471248541999415 ) ) ;
#43262 = CARTESIAN_POINT ( 'NONE',  ( 11.07243245105999918, 6.098035042109999360, -5.197348905474999725 ) ) ;
#43263 = ORIENTED_EDGE ( 'NONE', *, *, #20204, .F. ) ;
#43264 = CARTESIAN_POINT ( 'NONE',  ( 12.22973370829438622, -2.255582799352161327, -12.50515469879591812 ) ) ;
#43265 = DIRECTION ( 'NONE',  ( 0.000000000000000000, 0.9905022095861402143, 0.1374968101629056305 ) ) ;
#43266 = CARTESIAN_POINT ( 'NONE',  ( 23.59999999999999787, -0.9826074631703644036, 13.89481016226972798 ) ) ;
#43267 = CARTESIAN_POINT ( 'NONE',  ( 24.26287167771109310, -3.288955327281299024, -12.27454490589861358 ) ) ;
#43268 = CARTESIAN_POINT ( 'NONE',  ( 12.25061842917687827, -2.988573241473616360, -13.67729937646034344 ) ) ;
#43269 = CARTESIAN_POINT ( 'NONE',  ( 11.48225819896749833, -5.120994791668000090, -7.711331004020999913 ) ) ;
#43270 = CARTESIAN_POINT ( 'NONE',  ( 12.56879673637879691, -1.798456840550200830, 12.47100214317080358 ) ) ;
#43271 = CARTESIAN_POINT ( 'NONE',  ( 18.27038927661327961, -2.598921547761774420, 12.32906097307313686 ) ) ;
#43272 = ORIENTED_EDGE ( 'NONE', *, *, #60389, .T. ) ;
#43273 = CARTESIAN_POINT ( 'NONE',  ( 10.88813259637009878, -5.155817667926999803, -8.129798612793599943 ) ) ;
#43274 = ORIENTED_EDGE ( 'NONE', *, *, #27557, .T. ) ;
#43275 = VECTOR ( 'NONE', #3579, 1000.000000000000114 ) ;
#43276 = DIRECTION ( 'NONE',  ( -1.000000000000000000, 0.000000000000000000, 0.000000000000000000 ) ) ;
#43277 = CARTESIAN_POINT ( 'NONE',  ( 9.925639158771000226, 4.357364160690000432, -9.282962013144999247 ) ) ;
#43278 = CARTESIAN_POINT ( 'NONE',  ( 10.52343057594999998, 3.209665745824000105, -9.177097971982000502 ) ) ;
#43279 = EDGE_CURVE ( 'NONE', #51438, #51664, #47526, .T. ) ;
#43280 = CARTESIAN_POINT ( 'NONE',  ( 8.924662153698969647, 5.350575487761837223, 7.500021879703680838 ) ) ;
#43281 = PRESENTATION_LAYER_ASSIGNMENT (  '', '', ( #18731 ) ) ;
#43282 = CARTESIAN_POINT ( 'NONE',  ( 9.068197172117432814, 5.125396288428779812, -6.749639981086953178 ) ) ;
#43283 = CARTESIAN_POINT ( 'NONE',  ( 24.22080405609500176, -12.17114551901999953, 3.345703174095000065 ) ) ;
#43284 = CARTESIAN_POINT ( 'NONE',  ( 11.02452225494999993, -2.775477745048999800, -6.571291218949999902 ) ) ;
#43285 = B_SPLINE_CURVE_WITH_KNOTS ( 'NONE', 3,
 ( #37371, #69178, #48554, #37713 ),
 .UNSPECIFIED., .F., .F.,
 ( 4, 4 ),
 ( 0.000000000000000000, 1.000000000000000000 ),
 .UNSPECIFIED. ) ;
#43286 = EDGE_LOOP ( 'NONE', ( #61308, #2603, #20060, #18835 ) ) ;
#43287 = CONICAL_SURFACE ( 'NONE', #60055, 1.249999322936999890, 0.7853979760808852406 ) ;
#43288 = PLANE ( 'NONE',  #30225 ) ;
#43289 = CARTESIAN_POINT ( 'NONE',  ( 11.18051582549000145, 5.340073783367000892, 8.416152717850000187 ) ) ;
#43290 = CARTESIAN_POINT ( 'NONE',  ( 2.248890132542666898, -2.798833948393641080, 2.150913519912190708 ) ) ;
#43291 = CARTESIAN_POINT ( 'NONE',  ( 11.43990547754509990, -2.967013601007999934, 7.467215766047949899 ) ) ;
#43292 = CARTESIAN_POINT ( 'NONE',  ( 5.500000000000000000, 2.451372438371999805E-13, 6.461498003317998333E-14 ) ) ;
#43293 = AXIS2_PLACEMENT_3D ( 'NONE', #60352, #12461, #44638 ) ;
#43294 = CARTESIAN_POINT ( 'NONE',  ( 10.99074018437999989, 9.115166694568001660, -6.428052138438000718 ) ) ;
#43295 = CARTESIAN_POINT ( 'NONE',  ( 10.78327292636594237, 5.333380840314849713, -6.342316951424320060 ) ) ;
#43296 = CARTESIAN_POINT ( 'NONE',  ( 23.62003649549700057, -10.21603048626000110, -9.339736802856998921 ) ) ;
#43297 = DIRECTION ( 'NONE',  ( 1.000000000000000000, 0.000000000000000000, 0.000000000000000000 ) ) ;
#43298 = CIRCLE ( 'NONE', #63342, 12.39999890530000037 ) ;
#43299 = LINE ( 'NONE', #64607, #7602 ) ;
#43300 = B_SPLINE_SURFACE_WITH_KNOTS ( 'NONE', 1, 3, ( 
 ( #36571, #41475, #37260, #42171, #52646, #48096, #4053, #69071, #26084, #62783, #47412, #30994, #10682, #53343, #68717, #16273, #37599, #198, #20837, #42849, #63470, #14905, #15593, #36228, #36923, #11033, #57543, #58238, #4400, #9647, #52303, #47068, #21177, #58581, #42509, #21859, #1929, #59957, #59613, #1235, #60309, #33400, #38285, #48785, #12068, #54716, #44592, #55063, #54365, #65542, #892, #6120, #22205, #6815, #39330, #44245, #12416, #43542, #11710, #28151, #5778, #27121, #49463, #23249, #1576, #17665, #22894, #60650, #65885, #32371, #38989, #18013, #53686, #33748, #64842, #48437, #43194, #7165, #546, #64497, #16617, #28504, #49817, #33049, #43888, #11367 ),
 ( #37942, #59264, #32705, #54018, #27458, #22546, #6469, #38635, #16954, #27816, #49121, #65191, #17310, #2270, #45271, #51200, #45948, #34783, #12765, #34092, #44930, #18355, #66577, #56791, #55412, #61680, #45615, #28859, #40358, #40030, #35127, #41047, #51532, #13796, #34445, #35468, #62025, #67258, #23588, #50507, #55759, #24281, #8202, #50168, #56441, #7861, #67598, #8889, #46298, #61342, #8544, #29552, #13460, #19374, #24964, #3628, #7505, #23938, #18697, #29893, #13117, #2607, #66234, #30224, #39677, #19723, #3293, #50853, #56092, #19031, #60996, #24628, #29195, #40696, #2947, #66920, #14139, #31592, #26345, #15161, #62368, #14485, #25305, #67950, #25652, #37174 ) ),
 .UNSPECIFIED., .F., .F., .F.,
 ( 2, 2 ),
 ( 4, 2, 2, 2, 2, 2, 2, 2, 2, 2, 2, 2, 2, 2, 2, 2, 2, 2, 2, 2, 2, 2, 2, 2, 2, 2, 2, 2, 2, 2, 2, 2, 2, 2, 2, 2, 2, 2, 2, 2, 2, 2, 4 ),
 ( 0.000000000000000000, 1.000000000000000000 ),
 ( 0.000000000000000000, 7.142430198406409696E-05, 0.0001428486039681281939, 0.0002142729059521922773, 0.0002856972079362563879, 0.0003571215099203204442, 0.0004285458119043845547, 0.0004999701138884486652, 0.0005356822648804807204, 0.0005713944158725127757, 0.0006071065668645447225, 0.0006428187178565767778, 0.0007142430198406408883, 0.0007856673218247049988, 0.0008213794728167370541, 0.0008570916238087691093, 0.0008928037748008011646, 0.0009285159257928332199, 0.0009999402277768973304, 0.001071364529760961441, 0.001142788831745025551, 0.001214213133729089445, 0.001285637435713153556, 0.001321349586705185611, 0.001357061737697217666, 0.001428486039681281777, 0.001499910341665345887, 0.001535622492657377942, 0.001571334643649409998, 0.001607046794641442053, 0.001642758945633474108, 0.001714183247617538219, 0.001785607549601602329, 0.001821319700593634384, 0.001857031851585666440, 0.001928456153569730550, 0.001964168304561762605, 0.001999880455553794661, 0.002035592606545826716, 0.002071304757537858771, 0.002142729059521922882, 0.002214153361505986992, 0.002285577663490051103 ),
 .UNSPECIFIED. ) ;
#43301 = VERTEX_POINT ( 'NONE', #53622 ) ;
#43302 = CARTESIAN_POINT ( 'NONE',  ( 11.00000000000000000, 5.200000000000000178, 5.865766984179000332 ) ) ;
#43303 = CARTESIAN_POINT ( 'NONE',  ( 7.349215237593000438, -1.066568762865999886, 0.6056346772294000091 ) ) ;
#43304 = CARTESIAN_POINT ( 'NONE',  ( 18.05358084703146559, 2.122495591609770305, 13.74627451715323012 ) ) ;
#43305 = LINE ( 'NONE', #17064, #64622 ) ;
#43306 = CARTESIAN_POINT ( 'NONE',  ( 10.12841772631199966, -3.509411006705700053, -8.509834072393999804 ) ) ;
#43307 = ORIENTED_EDGE ( 'NONE', *, *, #15328, .F. ) ;
#43308 = B_SPLINE_CURVE_WITH_KNOTS ( 'NONE', 3,
 ( #26299, #27329, #26987, #31546, #21050, #63337, #15465, #36791, #58112, #48303, #47966, #59136 ),
 .UNSPECIFIED., .F., .F.,
 ( 4, 2, 2, 2, 2, 4 ),
 ( 0.000000000000000000, 0.2499999999999965583, 0.3749999999999968914, 0.4374999999999996669, 0.5000000000000025535, 1.000000000000000000 ),
 .UNSPECIFIED. ) ;
#43309 = B_SPLINE_CURVE_WITH_KNOTS ( 'NONE', 3,
 ( #15365, #57657, #16041, #37372, #42287, #5210 ),
 .UNSPECIFIED., .F., .F.,
 ( 4, 2, 4 ),
 ( 0.000000000000000000, 0.5000000000000000000, 1.000000000000000000 ),
 .UNSPECIFIED. ) ;
#43310 = DIRECTION ( 'NONE',  ( 0.000000000000000000, -1.000000000000000000, 0.000000000000000000 ) ) ;
#43311 = CARTESIAN_POINT ( 'NONE',  ( 7.218295280410000458, 4.773081973066999772, 8.927402469597002010 ) ) ;
#43313 = FACE_OUTER_BOUND ( 'NONE', #51911, .T. ) ;
#43312 = CARTESIAN_POINT ( 'NONE',  ( 9.459729719592999686, 2.527713920559999661, -6.969421869128999525 ) ) ;
#43314 = CARTESIAN_POINT ( 'NONE',  ( 2.520034936199110120, -3.248084742043254813, 0.2529824396494559924 ) ) ;
#43315 = ADVANCED_FACE ( 'NONE', ( #31965 ), #61112, .T. ) ;
#43316 = VERTEX_POINT ( 'NONE', #52587 ) ;
#43317 = ADVANCED_FACE ( 'NONE', ( #15536 ), #27838, .F. ) ;
#43318 = CARTESIAN_POINT ( 'NONE',  ( 9.722769750889000306, 5.493785011855999656, 6.566826815556000341 ) ) ;
#43319 = CARTESIAN_POINT ( 'NONE',  ( 18.24660850951287472, -2.298559566806798404, -13.81002375772540702 ) ) ;
#43320 = CARTESIAN_POINT ( 'NONE',  ( 10.40333997687999990, 4.213854445120500003, 8.480416814141699788 ) ) ;
#43321 = CARTESIAN_POINT ( 'NONE',  ( 9.569799020577001158, -4.064052785562999759, 8.919253808370999792 ) ) ;
#43322 = CARTESIAN_POINT ( 'NONE',  ( 8.090519353209000286, -5.342173944271999986, 8.432314172168000610 ) ) ;
#43323 = ORIENTED_EDGE ( 'NONE', *, *, #55318, .F. ) ;
#43324 = CARTESIAN_POINT ( 'NONE',  ( 24.43232361759900328, 11.98245802077999933, -3.250304477315999918 ) ) ;
#43325 = VECTOR ( 'NONE', #36644, 1000.000000000000000 ) ;
#43327 = CARTESIAN_POINT ( 'NONE',  ( 10.47111935320999976, -5.170637620872999385, -8.712950754783999940 ) ) ;
#43326 = CARTESIAN_POINT ( 'NONE',  ( 11.93277786803400176, -12.01216300861999997, 3.678628708156000293 ) ) ;
#43328 = B_SPLINE_CURVE_WITH_KNOTS ( 'NONE', 3,
 ( #24799, #7690, #46469, #55933, #23765, #45100, #29032, #18872, #51028 ),
 .UNSPECIFIED., .F., .F.,
 ( 4, 1, 1, 1, 1, 1, 4 ),
 ( 0.000000000000000000, 0.1176715969261405564, 0.3173201826739889819, 0.5169687684225861002, 0.7166173541704345951, 0.9162659399182834230, 1.000000000000000000 ),
 .UNSPECIFIED. ) ;
#43329 = CARTESIAN_POINT ( 'NONE',  ( 7.806648733296884579, -4.393915723649380212, 9.194460218222584302 ) ) ;
#43330 = CARTESIAN_POINT ( 'NONE',  ( 24.67921321864300310, 12.29514728640000065, 2.979192498689000157 ) ) ;
#43331 = FACE_OUTER_BOUND ( 'NONE', #16103, .T. ) ;
#43332 = VERTEX_POINT ( 'NONE', #22148 ) ;
#43333 = CARTESIAN_POINT ( 'NONE',  ( 25.26126434830474565, -11.18200453048727283, -3.383907761729669339 ) ) ;
#43334 = CARTESIAN_POINT ( 'NONE',  ( 12.05610404293055993, -4.502836909561000134, 6.476063885290000322 ) ) ;
#43335 = CARTESIAN_POINT ( 'NONE',  ( 8.162581873609997984, 3.457979189883997329, 6.166988478103001547 ) ) ;
#43336 = VECTOR ( 'NONE', #23102, 1000.000000000000000 ) ;
#43337 = CARTESIAN_POINT ( 'NONE',  ( 10.32533997688000049, 4.243109097101799954, 8.614534918052999757 ) ) ;
#43338 = EDGE_LOOP ( 'NONE', ( #19788, #65891, #33546, #40376 ) ) ;
#43339 = CARTESIAN_POINT ( 'NONE',  ( 9.658629719592001450, 5.496789211521000418, -7.043125396300999874 ) ) ;
#43340 = AXIS2_PLACEMENT_3D ( 'NONE', #54821, #6920, #7269 ) ;
#43341 = CARTESIAN_POINT ( 'NONE',  ( 12.12470607006057399, 2.231004149372982415, -12.40091715157283936 ) ) ;
#43342 = CARTESIAN_POINT ( 'NONE',  ( 11.13880513895979973, -2.849548954067000039, 8.139542779846600240 ) ) ;
#43343 = B_SPLINE_CURVE_WITH_KNOTS ( 'NONE', 3,
 ( #6378, #6727, #28068, #2526 ),
 .UNSPECIFIED., .F., .F.,
 ( 4, 4 ),
 ( 0.000000000000000000, 1.000000000000000000 ),
 .UNSPECIFIED. ) ;
#43344 = EDGE_CURVE ( 'NONE', #14597, #32433, #40557, .T. ) ;
#43345 = VERTEX_POINT ( 'NONE', #54660 ) ;
#43346 = CARTESIAN_POINT ( 'NONE',  ( 7.948155326409716892, 4.903496817485942572, -6.391515375827595768 ) ) ;
#43347 = AXIS2_PLACEMENT_3D ( 'NONE', #31037, #58277, #69111 ) ;
#43349 = EDGE_CURVE ( 'NONE', #51331, #11010, #38227, .T. ) ;
#43348 = CARTESIAN_POINT ( 'NONE',  ( 10.40685100253999984, -2.832432432432000269, -6.822293592207000934 ) ) ;
#43350 = EDGE_LOOP ( 'NONE', ( #66534, #58234, #39997, #10744 ) ) ;
#43351 = CARTESIAN_POINT ( 'NONE',  ( 9.010191940380000375, -5.040796345420999636, 8.522966281393001609 ) ) ;
#43352 = CARTESIAN_POINT ( 'NONE',  ( 23.75091569058821861, 9.822198688071051009, 9.446472845318485412 ) ) ;
#43353 = ORIENTED_EDGE ( 'NONE', *, *, #44290, .F. ) ;
#43354 = CARTESIAN_POINT ( 'NONE',  ( 12.27385967125950650, -2.970546648634963649, -12.24484150081280553 ) ) ;
#43355 = CARTESIAN_POINT ( 'NONE',  ( 10.28441772631199846, 4.372518460886800185, 6.733203680593099705 ) ) ;
#43356 = CARTESIAN_POINT ( 'NONE',  ( 9.447841622600000377, 5.447457912891000120, 7.431328695644999982 ) ) ;
#43357 = CARTESIAN_POINT ( 'NONE',  ( 10.96087378956999991, 2.844615129876999937, -5.099797510035999792 ) ) ;
#43358 = CARTESIAN_POINT ( 'NONE',  ( 7.969753415490000492, 5.131577060784002775, 6.757500301899002970 ) ) ;
#43359 = CARTESIAN_POINT ( 'NONE',  ( 11.09999999999999964, 5.350000000000000533, 7.500000000000000000 ) ) ;
#43360 = DIRECTION ( 'NONE',  ( -1.000000000000000000, 0.000000000000000000, 0.000000000000000000 ) ) ;
#43361 = CARTESIAN_POINT ( 'NONE',  ( 18.01141060613105793, 0.4275228316712895160, -12.69032453495386648 ) ) ;
#43362 = AXIS2_PLACEMENT_3D ( 'NONE', #46427, #35257, #67053 ) ;
#43363 = CARTESIAN_POINT ( 'NONE',  ( 12.22895615647772516, 2.742396662204058977, -12.39180484752808020 ) ) ;
#43364 = CARTESIAN_POINT ( 'NONE',  ( 10.96533729122639933, -5.140346530769000388, -7.470001566214039990 ) ) ;
#43365 = CARTESIAN_POINT ( 'NONE',  ( 8.983795280412000039, 3.979464555644999901, 9.134076336209998814 ) ) ;
#43366 = VERTEX_POINT ( 'NONE', #30091 ) ;
#43367 = AXIS2_PLACEMENT_3D ( 'NONE', #6392, #55690, #1161 ) ;
#43368 = CARTESIAN_POINT ( 'NONE',  ( 8.767881343006999728, -4.605543323398999966, -6.293427432547999523 ) ) ;
#43369 = CARTESIAN_POINT ( 'NONE',  ( 11.48052502238429895, 5.045683737783986267, 7.175009015034043536 ) ) ;
#43370 = CARTESIAN_POINT ( 'NONE',  ( 11.26395919764000197, 12.20155262497000059, 1.453968487665999954 ) ) ;
#43371 = EDGE_CURVE ( 'NONE', #33656, #14617, #64151, .T. ) ;
#43372 = CARTESIAN_POINT ( 'NONE',  ( 18.18564075751665143, 2.124969003714952898, 12.41952547471440482 ) ) ;
#43373 = CARTESIAN_POINT ( 'NONE',  ( 11.01665246377999985, 6.699949187588000399, 5.516876281257999892 ) ) ;
#43374 = CARTESIAN_POINT ( 'NONE',  ( 11.14285950365999867, 10.00557278198999889, 5.861225909637999720 ) ) ;
#43375 = CARTESIAN_POINT ( 'NONE',  ( 10.56276198887462847, -4.665935521472182934, 8.067505198359821605 ) ) ;
#43376 = FACE_OUTER_BOUND ( 'NONE', #16854, .T. ) ;
#43377 = ORIENTED_EDGE ( 'NONE', *, *, #17117, .T. ) ;
#43378 = CARTESIAN_POINT ( 'NONE',  ( 12.08118961495429744, -2.529460273524984704, 12.34351656561901223 ) ) ;
#43379 = CARTESIAN_POINT ( 'NONE',  ( 9.707684229509998985, -4.804883439508000897, -6.690125258578699885 ) ) ;
#43380 = CARTESIAN_POINT ( 'NONE',  ( 10.07102359808000003, 4.042170458878000083, 8.920189456109998360 ) ) ;
#43381 = CARTESIAN_POINT ( 'NONE',  ( 9.199609130449999839, -2.551382302226000487, 7.536606162076999738 ) ) ;
#43382 = CARTESIAN_POINT ( 'NONE',  ( 11.08841369783139896, 3.942447888101379583, -8.639288317626999003 ) ) ;
#43383 = CARTESIAN_POINT ( 'NONE',  ( 12.09168743772587362, 0.1288995356414812388, 12.59934597632939735 ) ) ;
#43384 = AXIS2_PLACEMENT_3D ( 'NONE', #7689, #40199, #6642 ) ;
#43385 = CARTESIAN_POINT ( 'NONE',  ( 9.112170280412000167, 2.368264398678999516, 7.410200237937000445 ) ) ;
#43386 = DIRECTION ( 'NONE',  ( 0.000000000000000000, -0.9553735099700839672, 0.2954005017724949389 ) ) ;
#43387 = CONICAL_SURFACE ( 'NONE', #47880, 11.45000314237999994, 0.7853984362573629419 ) ;
#43388 = CARTESIAN_POINT ( 'NONE',  ( 12.19649458927090357, 2.642789655208612754, 12.41715525233005479 ) ) ;
#43389 = CARTESIAN_POINT ( 'NONE',  ( 18.43044927002210898, -3.211191212929379368, -12.10643352320191291 ) ) ;
#43390 = CARTESIAN_POINT ( 'NONE',  ( 10.94072200990529886, 2.922907051630999842, -7.124286150322599376 ) ) ;
#43391 = CARTESIAN_POINT ( 'NONE',  ( 8.231600168468999001, 3.072304018142998139, -6.138007231110007567 ) ) ;
#43392 = CARTESIAN_POINT ( 'NONE',  ( 10.99306084123000105, 4.495422912016000083, -6.233618171705999522 ) ) ;
#43393 = CARTESIAN_POINT ( 'NONE',  ( 5.500000000000000000, -0.2500000000000000000, 9.776630298829998011 ) ) ;
#43395 = CARTESIAN_POINT ( 'NONE',  ( 12.20626853909072906, 2.679149498294548071, 12.40801937966798008 ) ) ;
#43394 = CARTESIAN_POINT ( 'NONE',  ( 7.927339924271998406, 4.618926574321004175, 6.298803404070997480 ) ) ;
#43396 = DIRECTION ( 'NONE',  ( 0.000000000000000000, 0.2714570858282905341, 0.9624505444715651947 ) ) ;
#43397 = ORIENTED_EDGE ( 'NONE', *, *, #23182, .T. ) ;
#43398 = VECTOR ( 'NONE', #23814, 1000.000000000000227 ) ;
#43399 = CARTESIAN_POINT ( 'NONE',  ( 12.20071720273219462, 0.1607023182928339899, 12.69865132254282436 ) ) ;
#43400 = CARTESIAN_POINT ( 'NONE',  ( 9.660601868375998436, -2.901236202253999696, -6.151180522693000086 ) ) ;
#43401 = CARTESIAN_POINT ( 'NONE',  ( 18.20247741961644650, -0.3746922849188884519, -12.59513687152069572 ) ) ;
#43402 = FACE_OUTER_BOUND ( 'NONE', #32714, .T. ) ;
#43403 = VECTOR ( 'NONE', #29713, 1000.000000000000000 ) ;
#43404 = EDGE_CURVE ( 'NONE', #16060, #33283, #19163, .T. ) ;
#43405 = EDGE_CURVE ( 'NONE', #60537, #59934, #6754, .T. ) ;
#43406 = CARTESIAN_POINT ( 'NONE',  ( 12.12630585043898535, -2.775512167237639716, 13.72213635400578013 ) ) ;
#43407 = CARTESIAN_POINT ( 'NONE',  ( 11.29996849689000271, 12.23272706294999956, 1.505586356912999912 ) ) ;
#43408 = DIRECTION ( 'NONE',  ( 0.000000000000000000, -1.000000000000000000, 0.000000000000000000 ) ) ;
#43409 = ORIENTED_EDGE ( 'NONE', *, *, #54696, .T. ) ;
#43410 = ADVANCED_FACE ( 'NONE', ( #17956 ), #49035, .F. ) ;
#43411 = EDGE_CURVE ( 'NONE', #7557, #15849, #29842, .T. ) ;
#43412 = CARTESIAN_POINT ( 'NONE',  ( 17.55505043854147118, -1.787797342887044172, -13.88538010501570774 ) ) ;
#43413 = CIRCLE ( 'NONE', #33383, 0.7499999999999998890 ) ;
#43414 = DIRECTION ( 'NONE',  ( 0.000000000000000000, 0.000000000000000000, 1.000000000000000000 ) ) ;
#43415 = CARTESIAN_POINT ( 'NONE',  ( 10.61503919148293740, 5.349978903665603802, -7.499997722305280945 ) ) ;
#43416 = CARTESIAN_POINT ( 'NONE',  ( 19.99999987597299977, 0.000000000000000000, -12.42499880353994790 ) ) ;
#43417 = CARTESIAN_POINT ( 'NONE',  ( 18.29999039390560611, -11.60794187010165679, 4.146723114213013872 ) ) ;
#43418 = CARTESIAN_POINT ( 'NONE',  ( 10.90000000000000036, 0.2500000000000000000, 4.902439024389999567 ) ) ;
#43419 = CARTESIAN_POINT ( 'NONE',  ( 10.89979975933730039, 4.819074589197400726, 7.781807394638899922 ) ) ;
#43420 = CARTESIAN_POINT ( 'NONE',  ( 15.89998535262536805, 8.893549080881223645, 8.534693534631724532 ) ) ;
#43421 = CARTESIAN_POINT ( 'NONE',  ( 11.00119435320999983, -4.640445114785999969, -9.059317673956000405 ) ) ;
#43422 = CARTESIAN_POINT ( 'NONE',  ( 4.657109839682542329, -1.199500263597270022, -0.9218200799623730290 ) ) ;
#43423 = B_SPLINE_CURVE_WITH_KNOTS ( 'NONE', 3,
 ( #67185, #29816, #51798, #40621 ),
 .UNSPECIFIED., .F., .F.,
 ( 4, 4 ),
 ( 0.000000000000000000, 1.000000000000000000 ),
 .UNSPECIFIED. ) ;
#43424 = CARTESIAN_POINT ( 'NONE',  ( 9.793536308085231568, 2.899999999999999911, 6.665341197415458829 ) ) ;
#43425 = CARTESIAN_POINT ( 'NONE',  ( 23.85842739849388039, 9.609046041819039985, -9.387911839951371462 ) ) ;
#43426 = PLANE ( 'NONE',  #21977 ) ;
#43427 = VERTEX_POINT ( 'NONE', #47532 ) ;
#43428 = CARTESIAN_POINT ( 'NONE',  ( 7.407491200529044306, 2.500879239676554011, 8.383868204678638136 ) ) ;
#43429 = CARTESIAN_POINT ( 'NONE',  ( 11.07564694612699974, -4.931992688388300294, 7.128058497017000228 ) ) ;
#43430 = ORIENTED_EDGE ( 'NONE', *, *, #68658, .F. ) ;
#43431 = CARTESIAN_POINT ( 'NONE',  ( 18.02738429465122039, -2.090191673117356874, 13.75189211025434233 ) ) ;
#43432 = CARTESIAN_POINT ( 'NONE',  ( 10.66995391537419913, -3.056324258617099776, -8.140910455049299443 ) ) ;
#43433 = ORIENTED_EDGE ( 'NONE', *, *, #26589, .F. ) ;
#43434 = CARTESIAN_POINT ( 'NONE',  ( 11.01790547754519878, 5.174295865741999734, 7.462730980357120458 ) ) ;
#43435 = CARTESIAN_POINT ( 'NONE',  ( 5.744489815226755169, -0.5444585885964672300, 0.9942383223988339180 ) ) ;
#43436 = CARTESIAN_POINT ( 'NONE',  ( 24.30000560072254956, -3.240508257516428348, 12.09374145940176781 ) ) ;
#43437 = CARTESIAN_POINT ( 'NONE',  ( 8.684028039623166606, -2.794631556210835033, 8.206409581471101333 ) ) ;
#43438 = CARTESIAN_POINT ( 'NONE',  ( 12.80505043854146763, -3.248147246781390329, -13.61798588129781074 ) ) ;
#43439 = CARTESIAN_POINT ( 'NONE',  ( 12.18006436421865679, 0.02054912266423991260, -13.89999925486820231 ) ) ;
#43440 = CARTESIAN_POINT ( 'NONE',  ( 7.000000000000000000, -6.255435840762999966, -3.000000000000000000 ) ) ;
#43441 = CARTESIAN_POINT ( 'NONE',  ( 10.34225158793000077, -3.348983461003999906, -8.881464249475000017 ) ) ;
#43442 = CARTESIAN_POINT ( 'NONE',  ( 11.09999999999999964, 4.000000000000000000, 7.500000000000000000 ) ) ;
#43443 = ORIENTED_EDGE ( 'NONE', *, *, #23622, .F. ) ;
#43444 = CARTESIAN_POINT ( 'NONE',  ( 9.219485841232998524, 3.892978337449999771, -8.893414073324001023 ) ) ;
#43445 = ORIENTED_EDGE ( 'NONE', *, *, #61008, .T. ) ;
#43446 = CARTESIAN_POINT ( 'NONE',  ( 24.57788509330325866, -12.41755320267419016, 3.012067450276798120 ) ) ;
#43447 =( NAMED_UNIT ( * ) PLANE_ANGLE_UNIT ( ) SI_UNIT ( $, .RADIAN. ) );
#43448 = ORIENTED_EDGE ( 'NONE', *, *, #11730, .T. ) ;
#43449 = CARTESIAN_POINT ( 'NONE',  ( 4.599999999999999645, 3.199698446519374073, 12.18695736643652694 ) ) ;
#43450 = CARTESIAN_POINT ( 'NONE',  ( 18.15889616939342233, -2.662482328103963791, -12.41224410776443321 ) ) ;
#43451 = EDGE_CURVE ( 'NONE', #52427, #28311, #7504, .T. ) ;
#43452 = CARTESIAN_POINT ( 'NONE',  ( 24.73255479474749663, -8.642945031846046788, 8.588131473315229414 ) ) ;
#43453 = CARTESIAN_POINT ( 'NONE',  ( 10.18559687351583243, 5.092232985442825210, -6.870476274536379435 ) ) ;
#43454 = LINE ( 'NONE', #68022, #40607 ) ;
#43455 = B_SPLINE_SURFACE_WITH_KNOTS ( 'NONE', 3, 3, ( 
 ( #22437, #43778, #27007, #48325 ),
 ( #64384, #11257, #23134, #56337 ),
 ( #50747, #55302, #44822, #44485 ),
 ( #7397, #65776, #40257, #13353 ) ),
 .UNSPECIFIED., .F., .F., .F.,
 ( 4, 4 ),
 ( 4, 4 ),
 ( -0.01349945606786999951, 0.08053609420915000539 ),
 ( -0.0005287450254680999126, 0.02696599629895000266 ),
 .UNSPECIFIED. ) ;
#43456 = FACE_OUTER_BOUND ( 'NONE', #5774, .T. ) ;
#43457 = EDGE_CURVE ( 'NONE', #8013, #22744, #41590, .T. ) ;
#43458 = CARTESIAN_POINT ( 'NONE',  ( 7.849215480312374815, 2.936390630773842769, -6.610087627805777188 ) ) ;
#43459 = CARTESIAN_POINT ( 'NONE',  ( 12.37737328439355444, 0.4562271229319652677, 13.88993195058941410 ) ) ;
#43460 = VERTEX_POINT ( 'NONE', #25165 ) ;
#43461 = CARTESIAN_POINT ( 'NONE',  ( 12.78642148534500045, 11.38816520531000087, -4.576060180783999343 ) ) ;
#43462 = CARTESIAN_POINT ( 'NONE',  ( 17.90267118914800193, 12.03818693049999844, -3.242368311117000079 ) ) ;
#43463 = CARTESIAN_POINT ( 'NONE',  ( 10.06276198887462847, 3.334064478527818842, 8.067505198359821605 ) ) ;
#43464 = FACE_OUTER_BOUND ( 'NONE', #46112, .T. ) ;
#43465 = CARTESIAN_POINT ( 'NONE',  ( 9.925639158771000226, 4.357364160690000432, -9.282962013144999247 ) ) ;
#43466 = CARTESIAN_POINT ( 'NONE',  ( 18.35309808591700076, -2.844562563850999926, 12.04738788559999918 ) ) ;
#43467 = CARTESIAN_POINT ( 'NONE',  ( 11.17811058788999823, -2.762459764047000110, -6.187206491620000470 ) ) ;
#43468 = ORIENTED_EDGE ( 'NONE', *, *, #7820, .F. ) ;
#43469 = CARTESIAN_POINT ( 'NONE',  ( 7.871384613761001070, -5.129340912189999990, 6.740051747100999968 ) ) ;
#43470 = CARTESIAN_POINT ( 'NONE',  ( 23.60000000000000142, 0.000000000000000000, 0.000000000000000000 ) ) ;
#43471 = CARTESIAN_POINT ( 'NONE',  ( 10.85502524286000003, -2.899999999999999911, 6.518873296399666728 ) ) ;
#43472 = CARTESIAN_POINT ( 'NONE',  ( 11.04782425406999913, -5.235403588978999601, 5.041461677707999911 ) ) ;
#43473 = CARTESIAN_POINT ( 'NONE',  ( 13.46376629110800138, 9.221173139870998625, 7.505113150216000228 ) ) ;
#43474 = CARTESIAN_POINT ( 'NONE',  ( 6.105026506350000659, -1.500000000000000000, 0.000000000000000000 ) ) ;
#43475 = CARTESIAN_POINT ( 'NONE',  ( 11.22567835872029995, 3.006051690924700370, -6.873560442659099046 ) ) ;
#43476 = CARTESIAN_POINT ( 'NONE',  ( 9.229392757687000071, 4.677963304775400566, -8.241085728986799808 ) ) ;
#43478 = CARTESIAN_POINT ( 'NONE',  ( 8.450126246929182017, 5.099734361584643771, -6.554153617478260863 ) ) ;
#43477 = CARTESIAN_POINT ( 'NONE',  ( 9.420468108405998464, -3.033597967472499768, 7.226304214866999587 ) ) ;
#43479 = CARTESIAN_POINT ( 'NONE',  ( 9.140753410162000492, -5.100000000000000533, 6.175944241622000064 ) ) ;
#43480 = ORIENTED_EDGE ( 'NONE', *, *, #12236, .T. ) ;
#43481 = CARTESIAN_POINT ( 'NONE',  ( 11.14767835872009982, 3.125658946326500320, 8.051056647135798272 ) ) ;
#43482 = CARTESIAN_POINT ( 'NONE',  ( 9.285188841453999586, -5.269672295101000437, 8.747824102203999530 ) ) ;
#43483 = CARTESIAN_POINT ( 'NONE',  ( 9.505051052051998184, 5.120555153167999585, 7.280704316743199733 ) ) ;
#43484 = CARTESIAN_POINT ( 'NONE',  ( 11.98513281071060632, -5.084573083995119980, 7.175000865651856685 ) ) ;
#43485 = ADVANCED_FACE ( 'NONE', ( #46840 ), #65215, .F. ) ;
#43486 = CARTESIAN_POINT ( 'NONE',  ( 10.28315099603999982, -2.387772357283999725, 7.684266429524000408 ) ) ;
#43487 = CARTESIAN_POINT ( 'NONE',  ( 9.661532504241865382, -5.554291940393154547, 6.696210084226174253 ) ) ;
#43488 = CARTESIAN_POINT ( 'NONE',  ( 10.43559687351661758, 2.907767014557176566, 6.870476274536375882 ) ) ;
#43489 = ADVANCED_FACE ( 'NONE', ( #3826 ), #35415, .T. ) ;
#43490 = ADVANCED_FACE ( 'NONE', ( #30760 ), #38752, .F. ) ;
#43491 = CARTESIAN_POINT ( 'NONE',  ( 10.11390035061499937, -3.695660922043800145, -8.600505223349999895 ) ) ;
#43492 = CARTESIAN_POINT ( 'NONE',  ( 6.333504020672999779, -0.7569293636342000475, -1.084220404132000048 ) ) ;
#43493 = DIRECTION ( 'NONE',  ( 0.000000000000000000, 0.000000000000000000, -1.000000000000000000 ) ) ;
#43494 = DIRECTION ( 'NONE',  ( 0.000000000000000000, 1.000000000000000000, 0.000000000000000000 ) ) ;
#43495 = CARTESIAN_POINT ( 'NONE',  ( 12.70247988648370452, 0.6166112555940446160, -12.67984200623736513 ) ) ;
#43496 = CARTESIAN_POINT ( 'NONE',  ( 11.85159063708299954, 4.825025306051200502, -7.731961446576300467 ) ) ;
#43497 = CARTESIAN_POINT ( 'NONE',  ( 21.54999911806000057, 1.172395514003999961E-13, -2.486899575159999765E-14 ) ) ;
#43498 = DIRECTION ( 'NONE',  ( 0.000000000000000000, 0.000000000000000000, -1.000000000000000000 ) ) ;
#43499 = CARTESIAN_POINT ( 'NONE',  ( 0.9676401325417666177, 1.762666431298152148, -3.058252359239900908 ) ) ;
#43500 = ORIENTED_EDGE ( 'NONE', *, *, #53066, .T. ) ;
#43501 = CARTESIAN_POINT ( 'NONE',  ( 7.325000000000000178, -4.000000000000000000, 9.239711431703000244 ) ) ;
#43502 = SHAPE_DEFINITION_REPRESENTATION ( #2556, #27655 ) ;
#43503 = CARTESIAN_POINT ( 'NONE',  ( 10.94501463001509833, -3.527519786474400121, -6.743262887067199784 ) ) ;
#43504 = CARTESIAN_POINT ( 'NONE',  ( 11.09999999999999964, -5.449702613288000208, -5.124965750789000296 ) ) ;
#43505 = EDGE_CURVE ( 'NONE', #53670, #67173, #66713, .T. ) ;
#43506 = CIRCLE ( 'NONE', #25638, 1.000000000000000444 ) ;
#43507 = DIRECTION ( 'NONE',  ( -1.000000000000000000, 0.000000000000000000, 0.000000000000000000 ) ) ;
#43508 = DIRECTION ( 'NONE',  ( 0.000000000000000000, -1.000000000000000000, 0.000000000000000000 ) ) ;
#43509 = CARTESIAN_POINT ( 'NONE',  ( 11.41486084871699802, 2.792989229543000107, -7.825000000000000178 ) ) ;
#43510 = ORIENTED_EDGE ( 'NONE', *, *, #41871, .T. ) ;
#43511 = CARTESIAN_POINT ( 'NONE',  ( 17.59665311020856393, 3.123961325934789812, -13.52113166927136589 ) ) ;
#43512 = EDGE_LOOP ( 'NONE', ( #37390, #2821, #27609, #30087, #58588 ) ) ;
#43513 = CARTESIAN_POINT ( 'NONE',  ( 17.60000001287599858, 11.53033693765999779, -4.891431908114999949 ) ) ;
#43514 = CARTESIAN_POINT ( 'NONE',  ( 24.89166245840957359, 8.575309574094205800, -8.440744490289855406 ) ) ;
#43515 = CARTESIAN_POINT ( 'NONE',  ( 9.468589158772999781, 4.034680274230000308, -6.102912434217000026 ) ) ;
#43516 = ORIENTED_EDGE ( 'NONE', *, *, #48296, .F. ) ;
#43517 = CARTESIAN_POINT ( 'NONE',  ( 23.71153097368373253, -13.14506149773556665, 3.853782021005720093 ) ) ;
#43518 = CARTESIAN_POINT ( 'NONE',  ( 11.71922412107039868, -3.930460928605089777, -6.185573549454999487 ) ) ;
#43519 = CARTESIAN_POINT ( 'NONE',  ( 8.309810841226997979, 5.485324155719999872, -6.315380258366999122 ) ) ;
#43520 = CARTESIAN_POINT ( 'NONE',  ( 10.51835931249056699, -5.126777126180352084, -6.752018918863353925 ) ) ;
#43521 = CARTESIAN_POINT ( 'NONE',  ( 7.250503751640505534, 3.823235083025295467, -8.849529909115084081 ) ) ;
#43522 = ORIENTED_EDGE ( 'NONE', *, *, #1654, .F. ) ;
#43523 = CARTESIAN_POINT ( 'NONE',  ( 10.99934110471000004, -5.081022574063999819, 8.239050178861999640 ) ) ;
#43524 = CARTESIAN_POINT ( 'NONE',  ( 25.25799237449400181, 11.13203901161000076, -3.460366607564000496 ) ) ;
#43525 = LINE ( 'NONE', #42829, #43934 ) ;
#43526 = ORIENTED_EDGE ( 'NONE', *, *, #11139, .T. ) ;
#43527 = CARTESIAN_POINT ( 'NONE',  ( 11.29998636608000062, -3.695122995756999984, 11.25914041192000070 ) ) ;
#43528 = CARTESIAN_POINT ( 'NONE',  ( 7.100000000000000533, 0.000000000000000000, 0.000000000000000000 ) ) ;
#43529 = ORIENTED_EDGE ( 'NONE', *, *, #39936, .F. ) ;
#43530 = CARTESIAN_POINT ( 'NONE',  ( 10.03791290906799993, 3.277531639390499851, 6.615820196229499572 ) ) ;
#43531 = CARTESIAN_POINT ( 'NONE',  ( 7.000000000000000000, 0.000000000000000000, 0.000000000000000000 ) ) ;
#43532 = CARTESIAN_POINT ( 'NONE',  ( 5.161168627748000226, 0.8913906144712999691, -1.100839504782000100 ) ) ;
#43533 = CARTESIAN_POINT ( 'NONE',  ( 8.115647571493003198, 4.568121236579997024, -6.191716341584998951 ) ) ;
#43534 = CARTESIAN_POINT ( 'NONE',  ( 16.39967273502900014, 3.641490841173999904, 12.02437761214999945 ) ) ;
#43535 = CARTESIAN_POINT ( 'NONE',  ( 11.19955063476130164, 4.976598135215295038, 8.326430086672804265 ) ) ;
#43536 = ADVANCED_FACE ( 'NONE', ( #54137 ), #43238, .T. ) ;
#43537 = CARTESIAN_POINT ( 'NONE',  ( 9.327456490741958817, -3.944521858995455599, 9.238771218640099647 ) ) ;
#43538 = VERTEX_POINT ( 'NONE', #48207 ) ;
#43539 = CARTESIAN_POINT ( 'NONE',  ( 10.80168826891999956, 3.998196217194999846, 9.431555066626000183 ) ) ;
#43540 = CARTESIAN_POINT ( 'NONE',  ( 4.605026506348999682, -1.500000000000000000, 0.000000000000000000 ) ) ;
#43541 = CARTESIAN_POINT ( 'NONE',  ( 13.25828219467840086, 12.15323025559004222, 2.051492516881130879 ) ) ;
#43542 = CARTESIAN_POINT ( 'NONE',  ( 12.29043182814382007, 2.854820394136931672, -13.59177665069740293 ) ) ;
#43543 = CARTESIAN_POINT ( 'NONE',  ( 24.54223752884296061, -12.46060277342660783, -3.023618805801078224 ) ) ;
#43544 = CARTESIAN_POINT ( 'NONE',  ( 24.48513953661800358, 3.324320571727000129, 12.08694663984000073 ) ) ;
#43545 = CARTESIAN_POINT ( 'NONE',  ( 17.63737865760588974, -0.6198980793944591783, 13.88138779565240100 ) ) ;
#43546 = CARTESIAN_POINT ( 'NONE',  ( 24.46225083065800376, -3.149516733939000002, 11.96334735801000093 ) ) ;
#43547 = ORIENTED_EDGE ( 'NONE', *, *, #9160, .T. ) ;
#43548 = ORIENTED_EDGE ( 'NONE', *, *, #6309, .T. ) ;
#43549 = CARTESIAN_POINT ( 'NONE',  ( 10.91307008594999850, 2.096286256021000050, 7.827189715349000210 ) ) ;
#43550 = CARTESIAN_POINT ( 'NONE',  ( 12.21931057678297528, 0.2190559830119534757, 13.89769592719668445 ) ) ;
#43551 = B_SPLINE_CURVE_WITH_KNOTS ( 'NONE', 3,
 ( #39059, #55136, #7583, #17383 ),
 .UNSPECIFIED., .F., .F.,
 ( 4, 4 ),
 ( 0.000000000000000000, 1.000000000000000000 ),
 .UNSPECIFIED. ) ;
#43552 = CARTESIAN_POINT ( 'NONE',  ( 10.64887885159599890, -2.730985436695000157, 7.651388779553199626 ) ) ;
#43553 = CARTESIAN_POINT ( 'NONE',  ( 9.571967469951999874, -4.084684048989999816, 8.946621592834999248 ) ) ;
#43554 = CARTESIAN_POINT ( 'NONE',  ( 17.69618303672615056, -0.6091729397527337886, -13.88202727520719648 ) ) ;
#43555 = CARTESIAN_POINT ( 'NONE',  ( 8.449245559625000013, -5.458705123429999695, 7.456451825584000659 ) ) ;
#43557 = AXIS2_PLACEMENT_3D ( 'NONE', #48147, #58983, #47814 ) ;
#43556 = CYLINDRICAL_SURFACE ( 'NONE', #50526, 0.5000000000000002220 ) ;
#43559 = CARTESIAN_POINT ( 'NONE',  ( 7.882275234989998935, -4.670605665485999758, 6.328280003999000591 ) ) ;
#43558 = CARTESIAN_POINT ( 'NONE',  ( 11.02022949779800065, -3.290320231472799950, 6.435697190503999465 ) ) ;
#43560 = CARTESIAN_POINT ( 'NONE',  ( 10.44426222744799837, 3.013556901740999994, -8.312555471636301263 ) ) ;
#43561 = CARTESIAN_POINT ( 'NONE',  ( 12.09999999999999787, -4.813068503488582728, 6.962391415777370973 ) ) ;
#43562 = CARTESIAN_POINT ( 'NONE',  ( 23.63944133423405347, 10.04331723767212914, -9.682724240561979556 ) ) ;
#43563 = CARTESIAN_POINT ( 'NONE',  ( 17.80382244274732528, -0.5734477787136644800, 12.68256797703445038 ) ) ;
#43564 = CARTESIAN_POINT ( 'NONE',  ( 0.1103081484368000076, -1.521127753326000143, -2.712944034833999929 ) ) ;
#43565 = ADVANCED_BREP_SHAPE_REPRESENTATION ( '', ( #50398, #9676 ), #806 ) ;
#43566 = DIRECTION ( 'NONE',  ( 0.000000000000000000, -0.9867381147929490393, -0.1623203401144079905 ) ) ;
#43567 = EDGE_LOOP ( 'NONE', ( #17106, #68979, #54243, #46040 ) ) ;
#43568 = DIRECTION ( 'NONE',  ( 0.000000000000000000, 1.000000000000000000, 0.000000000000000000 ) ) ;
#43569 = FACE_OUTER_BOUND ( 'NONE', #10063, .T. ) ;
#43570 = EDGE_CURVE ( 'NONE', #3005, #49517, #29215, .T. ) ;
#43571 = EDGE_CURVE ( 'NONE', #67640, #56058, #53273, .T. ) ;
#43572 = CARTESIAN_POINT ( 'NONE',  ( 0.000000000000000000, -5.100000000000000533, 7.500000000000000000 ) ) ;
#43573 = CARTESIAN_POINT ( 'NONE',  ( 10.99335825054266103, 5.917683583687179727, 4.994028698803151478 ) ) ;
#43574 = CARTESIAN_POINT ( 'NONE',  ( 0.5928308122907000044, 2.413895893032000028, 2.806361486493000434 ) ) ;
#43575 = CARTESIAN_POINT ( 'NONE',  ( 10.89835090130999973, 4.878966983716200190, 6.956352367771000189 ) ) ;
#43576 = CARTESIAN_POINT ( 'NONE',  ( 10.65229834123000074, 4.944334466443999432, -8.478467788338001299 ) ) ;
#43577 = VERTEX_POINT ( 'NONE', #6235 ) ;
#43578 = CARTESIAN_POINT ( 'NONE',  ( 12.36386718854188160, -0.5708113556792973053, -12.58706429964239071 ) ) ;
#43579 = CARTESIAN_POINT ( 'NONE',  ( 8.615121458427411838, 5.349954800205006578, -7.499992720895565235 ) ) ;
#43580 = CARTESIAN_POINT ( 'NONE',  ( 17.72109462663381052, 3.180738073285645839, -12.19192004217519099 ) ) ;
#43581 = CARTESIAN_POINT ( 'NONE',  ( 7.173532264820161153, -2.920499069053410057, 8.329439769247674263 ) ) ;
#43582 = CARTESIAN_POINT ( 'NONE',  ( 9.079732780410999737, 5.421534627450999899, 6.381126373995999579 ) ) ;
#43583 = ORIENTED_EDGE ( 'NONE', *, *, #49706, .T. ) ;
#43584 = CARTESIAN_POINT ( 'NONE',  ( 6.155189463736999933, 0.8358542970315000487, -1.207425004536999857 ) ) ;
#43585 = CARTESIAN_POINT ( 'NONE',  ( 7.011054719589999706, 4.455038580940000159, -9.171635993214000138 ) ) ;
#43586 = EDGE_CURVE ( 'NONE', #17921, #36772, #5213, .T. ) ;
#43587 = B_SPLINE_CURVE_WITH_KNOTS ( 'NONE', 3,
 ( #40138, #24045, #25072, #62131 ),
 .UNSPECIFIED., .F., .F.,
 ( 4, 4 ),
 ( 0.000000000000000000, 1.000000000000000000 ),
 .UNSPECIFIED. ) ;
#43589 = CARTESIAN_POINT ( 'NONE',  ( 10.72520610419000064, 5.521650664120000940, 6.612990918765000004 ) ) ;
#43588 = CARTESIAN_POINT ( 'NONE',  ( 8.449824646308410792, -2.260412847700007610, 7.499181798588557157 ) ) ;
#43590 = CARTESIAN_POINT ( 'NONE',  ( 9.522734463322999332, -3.866750753272200303, 6.227746477418000026 ) ) ;
#43591 = ORIENTED_EDGE ( 'NONE', *, *, #43652, .T. ) ;
#43592 = CARTESIAN_POINT ( 'NONE',  ( 18.14117786275458855, -2.282023444416175995, -13.71724589037892983 ) ) ;
#43593 = FACE_BOUND ( 'NONE', #29661, .T. ) ;
#43594 = ORIENTED_EDGE ( 'NONE', *, *, #68027, .T. ) ;
#43595 = EDGE_CURVE ( 'NONE', #26293, #60334, #32481, .T. ) ;
#43596 = CARTESIAN_POINT ( 'NONE',  ( 11.10000000000000142, 2.718803219220815137, -8.524899190229213275 ) ) ;
#43598 = CARTESIAN_POINT ( 'NONE',  ( 16.39974593105000267, 3.376006003137999922, 11.11079012987999981 ) ) ;
#43597 = VECTOR ( 'NONE', #13789, 1000.000000000000227 ) ;
#43599 = CARTESIAN_POINT ( 'NONE',  ( 17.95947766544255231, -0.4766231184928892417, -13.88900205690511136 ) ) ;
#43600 = VERTEX_POINT ( 'NONE', #26894 ) ;
#43601 = CARTESIAN_POINT ( 'NONE',  ( 10.76685100253999927, -2.832432432432000269, 6.822293592207000934 ) ) ;
#43602 = SURFACE_STYLE_USAGE ( .BOTH. , #59672 ) ;
#43603 = CARTESIAN_POINT ( 'NONE',  ( 10.40480513895999870, 4.779740423663599636, -7.066537524675499782 ) ) ;
#43604 = DIRECTION ( 'NONE',  ( -1.000000000000000000, 0.000000000000000000, 0.000000000000000000 ) ) ;
#43605 = CARTESIAN_POINT ( 'NONE',  ( 10.57503300763299947, -3.118110956362800223, 6.575021251017499679 ) ) ;
#43606 = ORIENTED_EDGE ( 'NONE', *, *, #4010, .T. ) ;
#43607 = CARTESIAN_POINT ( 'NONE',  ( 8.309482780410998970, 2.905861847853000057, 8.940690431604000565 ) ) ;
#43608 = B_SPLINE_CURVE_WITH_KNOTS ( 'NONE', 3,
 ( #30342, #35244, #30677, #51648, #31030, #13579, #56215, #67715, #19841, #8325, #50971, #3067, #45730, #48130, #37630, #63850, #26814, #5128 ),
 .UNSPECIFIED., .F., .F.,
 ( 4, 2, 2, 2, 2, 2, 2, 2, 4 ),
 ( 0.000000000000000000, 0.1250000000000000000, 0.2500000000000000000, 0.3750000000000000000, 0.5000000000000000000, 0.6250000000000000000, 0.7500000000000000000, 0.8750000000000000000, 1.000000000000000000 ),
 .UNSPECIFIED. ) ;
#43609 = CARTESIAN_POINT ( 'NONE',  ( 18.20740272079784816, -2.198619098391816795, 13.82629845589066520 ) ) ;
#43611 = ORIENTED_EDGE ( 'NONE', *, *, #55681, .F. ) ;
#43610 = APPLICATION_CONTEXT ( 'automotive_design' ) ;
#43612 = AXIS2_PLACEMENT_3D ( 'NONE', #4850, #30750, #36684 ) ;
#43613 = CARTESIAN_POINT ( 'NONE',  ( 9.289752973821547855, -4.327172861449232855, -6.282573595533348154 ) ) ;
#43614 = DIRECTION ( 'NONE',  ( 0.000000000000000000, 1.000000000000000000, 0.000000000000000000 ) ) ;
#43615 = CARTESIAN_POINT ( 'NONE',  ( 11.01654511052000096, 5.423852610492999382, -4.991940169492999679 ) ) ;
#43616 = ORIENTED_EDGE ( 'NONE', *, *, #44643, .F. ) ;
#43617 = B_SPLINE_SURFACE_WITH_KNOTS ( 'NONE', 3, 3, ( 
 ( #3592, #56757, #45580, #29516, #20031, #57085, #66886, #13077, #41012, #62334, #51166, #35431, #61646, #56407, #50469, #40662, #67225, #51839, #14451, #8509, #67915, #9185, #19691, #55724, #50819, #61994, #30191, #7824, #24592, #29161, #8854, #56056, #19338, #61306, #23900 ),
 ( #51497, #30525, #39992, #45236, #13427, #3936, #25274, #66541, #24243, #18660, #18998, #29858, #45913, #15131, #42045, #20373, #57423, #41696, #63351, #52185, #15479, #52879, #26999, #52530, #5320, #10225, #63002, #25621, #37479, #26662, #21737, #47978, #4978, #58460, #4285 ),
 ( #20718, #21397, #36451, #47640, #48315, #31559, #26311, #68597, #57770, #21063, #9881, #420, #80, #30871, #62669, #31223, #68253, #4627, #36107, #5658, #25965, #14788, #15813, #42730, #36804, #53563, #10567, #31905, #42394, #37143, #58124, #68950, #47294, #9528, #63700 ),
 ( #53219, #64034, #16155, #58805, #10910, #32254, #46948, #28382, #22083, #11249, #37824, #6696, #17544, #1807, #2159, #1116, #17895, #59488, #7047, #32587, #38516, #1459, #22774, #48663, #33630, #44125, #39212, #60538, #49345, #7390, #54598, #6343, #49698, #43771, #65423 ) ),
 .UNSPECIFIED., .F., .F., .F.,
 ( 4, 4 ),
 ( 4, 1, 1, 1, 1, 1, 1, 1, 1, 1, 1, 1, 1, 1, 1, 1, 1, 1, 1, 1, 1, 1, 1, 1, 1, 1, 1, 1, 1, 1, 1, 1, 4 ),
 ( -0.1039370721279000015, 1.103937072127999963 ),
 ( -0.02000000000000000042, 0.01250000000000000069, 0.04499999999999999833, 0.07749999999999999944, 0.1100000000000000006, 0.1424999999999999878, 0.1749999999999999889, 0.2074999999999999900, 0.2399999999999999911, 0.2725000000000000200, 0.3049999999999999933, 0.3375000000000000222, 0.3699999999999999956, 0.4025000000000000244, 0.4349999999999999978, 0.4675000000000000266, 0.5000000000000000000, 0.5324999999999999734, 0.5649999999999999467, 0.5975000000000000311, 0.6300000000000000044, 0.6624999999999999778, 0.6949999999999999512, 0.7275000000000000355, 0.7600000000000000089, 0.7924999999999999822, 0.8249999999999999556, 0.8575000000000000400, 0.8900000000000000133, 0.9224999999999999867, 0.9549999999999999600, 0.9875000000000000444, 1.020000000000000018 ),
 .UNSPECIFIED. ) ;
#43618 = CARTESIAN_POINT ( 'NONE',  ( 12.39760546513567263, -2.025954772141364213, -12.54945441499613423 ) ) ;
#43619 = CARTESIAN_POINT ( 'NONE',  ( 10.82309687351639660, 2.782534154164606921, -7.172815144550894750 ) ) ;
#43620 = CARTESIAN_POINT ( 'NONE',  ( 11.40221299665285670, 4.908904393308908709, -7.824988380119695996 ) ) ;
#43621 = CARTESIAN_POINT ( 'NONE',  ( 7.307500000000000107, -0.2500000000000000000, 3.149999999999999911 ) ) ;
#43622 = CARTESIAN_POINT ( 'NONE',  ( 12.19349437040520634, -2.125667349631288339, -13.83768917864515302 ) ) ;
#43623 = CARTESIAN_POINT ( 'NONE',  ( 11.53148876160955005, -4.790673964186999534, -8.322268080792200706 ) ) ;
#43624 = CARTESIAN_POINT ( 'NONE',  ( 5.971693173017000866, -0.7554284705563540925, 1.310679582531384391 ) ) ;
#43625 = CARTESIAN_POINT ( 'NONE',  ( 18.03677854873450670, -1.942400312675104157, 12.44938339399087290 ) ) ;
#43626 = ORIENTED_EDGE ( 'NONE', *, *, #38600, .F. ) ;
#43627 = CARTESIAN_POINT ( 'NONE',  ( 10.52799293566599914, -3.193321847920899792, -8.489570425681801424 ) ) ;
#43628 = VERTEX_POINT ( 'NONE', #27576 ) ;
#43629 = CARTESIAN_POINT ( 'NONE',  ( 5.200000002192999737, 0.6646153561348999705, 2.616923086418999844 ) ) ;
#43630 = CARTESIAN_POINT ( 'NONE',  ( 9.196339158776000389, 4.112741311853999271, -5.603466076760000192 ) ) ;
#43631 = CARTESIAN_POINT ( 'NONE',  ( 10.01277517397999972, 3.440623091551000101, -9.267603345544999982 ) ) ;
#43632 = CARTESIAN_POINT ( 'NONE',  ( 9.858853446676000942, -2.668079545448999834, -7.206971019603000350 ) ) ;
#43633 = CARTESIAN_POINT ( 'NONE',  ( 5.599969214251100169, -11.06886219213000011, -1.536526853569999851 ) ) ;
#43634 = CARTESIAN_POINT ( 'NONE',  ( 23.99052667663800165, 13.00930538603000031, 3.385156461033000053 ) ) ;
#43635 = CYLINDRICAL_SURFACE ( 'NONE', #57901, 1.600000000000000089 ) ;
#43636 = ORIENTED_EDGE ( 'NONE', *, *, #33542, .T. ) ;
#43637 = DIRECTION ( 'NONE',  ( 0.000000000000000000, 1.000000000000000000, 0.000000000000000000 ) ) ;
#43638 = CARTESIAN_POINT ( 'NONE',  ( 10.46432998405999903, 2.042755206296999582, 7.723699495214000343 ) ) ;
#43639 = CARTESIAN_POINT ( 'NONE',  ( 10.90000000000000036, 2.832432432432000269, -6.822293592207000934 ) ) ;
#43640 = CARTESIAN_POINT ( 'NONE',  ( 10.94125056272499918, -2.966599088466999934, 7.484684486284700178 ) ) ;
#43641 = CARTESIAN_POINT ( 'NONE',  ( 11.09999999999999964, -2.700469802787999640, -5.124965750789000296 ) ) ;
#43642 = CARTESIAN_POINT ( 'NONE',  ( 10.45672469555900008, 4.433465011431599656, -6.750062220519700062 ) ) ;
#43643 = CIRCLE ( 'NONE', #32512, 1.099999999999999867 ) ;
#43644 = CARTESIAN_POINT ( 'NONE',  ( 10.47213937496879232, 2.299779464567346388, 7.025414528928831892 ) ) ;
#43645 = CARTESIAN_POINT ( 'NONE',  ( 23.55075815555500185, -10.43336509543999924, -9.388742684132997951 ) ) ;
#43646 = CARTESIAN_POINT ( 'NONE',  ( 23.95108089639600379, -9.462566780697001079, 9.411396329312999853 ) ) ;
#43647 = VECTOR ( 'NONE', #10616, 1000.000000000000000 ) ;
#43648 = CARTESIAN_POINT ( 'NONE',  ( 24.54174074856994636, 3.611931245565921156, -12.30360799778222969 ) ) ;
#43649 = EDGE_LOOP ( 'NONE', ( #21012, #49965, #51029, #13571 ) ) ;
#43650 = CARTESIAN_POINT ( 'NONE',  ( 9.269210841233000764, 3.098073081301000009, -8.567513114264999174 ) ) ;
#43651 = CARTESIAN_POINT ( 'NONE',  ( 7.127827688624999602, 1.235070164474999954, -0.1964835531513000055 ) ) ;
#43652 = EDGE_CURVE ( 'NONE', #23202, #18749, #9745, .T. ) ;
#43653 = EDGE_CURVE ( 'NONE', #51187, #42164, #41701, .T. ) ;
#43654 = CARTESIAN_POINT ( 'NONE',  ( 18.10189407302235409, 2.802802817710309924, 13.60450747121971204 ) ) ;
#43655 = DIRECTION ( 'NONE',  ( 0.000000000000000000, 0.5000000000000169864, 0.8660254037844288266 ) ) ;
#43656 = CARTESIAN_POINT ( 'NONE',  ( 11.01041369783139956, -4.064477673403060543, -8.776385133971000840 ) ) ;
#43657 = ORIENTED_EDGE ( 'NONE', *, *, #40439, .F. ) ;
#43658 = CARTESIAN_POINT ( 'NONE',  ( 24.98632622962700012, 3.086021350299999799, -11.61344612987000069 ) ) ;
#43659 = CARTESIAN_POINT ( 'NONE',  ( 7.346670280409000497, 2.374037589774999901, 8.293392681990997772 ) ) ;
#43661 = DIRECTION ( 'NONE',  ( 1.000000000000000000, -1.157371756808000041E-14, 1.157371756808000041E-14 ) ) ;
#43660 = CARTESIAN_POINT ( 'NONE',  ( 8.713854719593998155, 5.442817578555000146, -8.106149115450000053 ) ) ;
#43662 = CARTESIAN_POINT ( 'NONE',  ( 25.30000327618300204, -10.83443035398000021, 3.855530949778000149 ) ) ;
#43663 = ORIENTED_EDGE ( 'NONE', *, *, #18233, .F. ) ;
#43664 = CARTESIAN_POINT ( 'NONE',  ( 10.46085995768999943, 5.403395036974999677, 7.721808039505000387 ) ) ;
#43665 = CARTESIAN_POINT ( 'NONE',  ( 18.06232794982562595, -1.996188719851625715, -13.85695876210811228 ) ) ;
#43666 = CARTESIAN_POINT ( 'NONE',  ( 11.26487482311540056, 4.930401445321599851, 7.124095752359899336 ) ) ;
#43667 = CARTESIAN_POINT ( 'NONE',  ( 11.12914445903999905, -3.083861519183999977, 8.586004431109000024 ) ) ;
#43668 = CARTESIAN_POINT ( 'NONE',  ( 8.705995559625000269, -2.542850487891999745, 7.419808283050000064 ) ) ;
#43669 = ORIENTED_EDGE ( 'NONE', *, *, #3228, .F. ) ;
#43670 = FACE_OUTER_BOUND ( 'NONE', #5472, .T. ) ;
#43672 = CARTESIAN_POINT ( 'NONE',  ( 10.94033064679000233, -5.142732045902000948, -6.493502833853999512 ) ) ;
#43671 = CARTESIAN_POINT ( 'NONE',  ( 12.04524561587600040, -11.75582082520000071, 3.881266971570999758 ) ) ;
#43673 = CARTESIAN_POINT ( 'NONE',  ( 7.807018160663298012, -4.386125006573436735, 9.196209433013514456 ) ) ;
#43674 = CARTESIAN_POINT ( 'NONE',  ( 9.719606904206999687, -5.967761543230999166, 7.406644089178000101 ) ) ;
#43675 = CARTESIAN_POINT ( 'NONE',  ( 23.58549486637999948, 3.200144626573000028, 13.61915301421999835 ) ) ;
#43676 = ORIENTED_EDGE ( 'NONE', *, *, #45625, .T. ) ;
#43677 = FACE_OUTER_BOUND ( 'NONE', #49805, .T. ) ;
#43678 = CARTESIAN_POINT ( 'NONE',  ( 10.80487885159599948, -3.003595720052600448, 7.618867373350600047 ) ) ;
#43679 = EDGE_CURVE ( 'NONE', #44093, #24800, #21973, .T. ) ;
#43680 = CARTESIAN_POINT ( 'NONE',  ( 8.493443684196000376, 2.902502839086001263, 6.607649189245996091 ) ) ;
#43681 = CARTESIAN_POINT ( 'NONE',  ( 10.86272200990529946, 2.793294545435000220, 7.920925559347199219 ) ) ;
#43682 = VERTEX_POINT ( 'NONE', #21293 ) ;
#43683 = CARTESIAN_POINT ( 'NONE',  ( 9.170239158775000732, 4.769103072373000352, -8.666849124598000387 ) ) ;
#43684 = CARTESIAN_POINT ( 'NONE',  ( 23.74333464321300013, 13.04438545414000039, -3.827011755022000195 ) ) ;
#43685 = AXIS2_PLACEMENT_3D ( 'NONE', #25236, #46912, #35056 ) ;
#43686 = CARTESIAN_POINT ( 'NONE',  ( 12.64184255386818201, 1.896331190223614405, -12.57194050387412076 ) ) ;
#43687 = CARTESIAN_POINT ( 'NONE',  ( 11.89189666366029918, -4.052152326617509459, 6.326270943800999191 ) ) ;
#43688 = ORIENTED_EDGE ( 'NONE', *, *, #44538, .T. ) ;
#43690 = CYLINDRICAL_SURFACE ( 'NONE', #36269, 0.5000000000000002220 ) ;
#43689 = B_SPLINE_CURVE_WITH_KNOTS ( 'NONE', 3,
 ( #50926, #35542, #56861, #24355 ),
 .UNSPECIFIED., .F., .F.,
 ( 4, 4 ),
 ( 0.000000000000000000, 1.000000000000000000 ),
 .UNSPECIFIED. ) ;
#43691 = CARTESIAN_POINT ( 'NONE',  ( 8.817462135714999150, -5.100000000000000533, 6.571291218949999902 ) ) ;
#43692 = ORIENTED_EDGE ( 'NONE', *, *, #16134, .T. ) ;
#43693 = CARTESIAN_POINT ( 'NONE',  ( 9.523691940378000709, -4.852736108563000528, 8.683927195503999386 ) ) ;
#43694 = CARTESIAN_POINT ( 'NONE',  ( 23.89493791382834331, 9.543146308824796975, 9.361218189416669944 ) ) ;
#43695 = ORIENTED_EDGE ( 'NONE', *, *, #56990, .F. ) ;
#43696 = CARTESIAN_POINT ( 'NONE',  ( 7.000000000000000000, 10.80467228076000019, -3.475853456584999890 ) ) ;
#43697 = CARTESIAN_POINT ( 'NONE',  ( 11.77359063708300013, 4.955772084214699724, 7.231278212164300001 ) ) ;
#43698 = CARTESIAN_POINT ( 'NONE',  ( 23.60205915885299888, 2.489696159912998752, -12.09604418629000122 ) ) ;
#43699 = CARTESIAN_POINT ( 'NONE',  ( 10.60434687351569494, 5.250000000000001776, 7.663624617374461323 ) ) ;
#43700 = DIRECTION ( 'NONE',  ( 1.000000000000000000, 0.000000000000000000, 0.000000000000000000 ) ) ;
#43701 = CARTESIAN_POINT ( 'NONE',  ( 9.171146261768624797, 4.712741083356099203, -6.460774852777244170 ) ) ;
#43702 = CARTESIAN_POINT ( 'NONE',  ( 13.99932787941000178, 9.131694343880999654, 8.218494815692999111 ) ) ;
#43703 = CARTESIAN_POINT ( 'NONE',  ( 18.17902769456078360, 0.04114048977874683322, -12.69993211551499535 ) ) ;
#43704 = AXIS2_PLACEMENT_3D ( 'NONE', #46408, #3399, #66340 ) ;
#43705 = CARTESIAN_POINT ( 'NONE',  ( 12.18526316313925406, 2.581188759499452701, -12.43231204083059005 ) ) ;
#43706 = CARTESIAN_POINT ( 'NONE',  ( 10.27610941423800028, -3.155589807313900153, -6.733017893878099791 ) ) ;
#43707 = CARTESIAN_POINT ( 'NONE',  ( 7.518864158771000561, 3.206360348473000332, 5.681727837477000165 ) ) ;
#43708 = EDGE_LOOP ( 'NONE', ( #54613, #15785, #36177, #3716 ) ) ;
#43709 = SURFACE_SIDE_STYLE ('',( #27629 ) ) ;
#43710 = CARTESIAN_POINT ( 'NONE',  ( 23.56666365135700403, -11.16210620489000327, 3.571147223011999827 ) ) ;
#43711 = CARTESIAN_POINT ( 'NONE',  ( 0.7509734658760000015, -3.500000000000000000, 0.000000000000000000 ) ) ;
#43712 = CARTESIAN_POINT ( 'NONE',  ( 11.25951067610000145, 12.19482939020999979, 1.501993453007000046 ) ) ;
#43713 = CARTESIAN_POINT ( 'NONE',  ( 18.10980516112008942, 2.943705546998117484, 12.25131356140272310 ) ) ;
#43714 = EDGE_CURVE ( 'NONE', #8437, #24854, #30009, .T. ) ;
#43715 = CARTESIAN_POINT ( 'NONE',  ( 11.07071174448999962, 5.425085858506999870, 5.078388370519999917 ) ) ;
#43716 = ADVANCED_FACE ( 'NONE', ( #43313 ), #22319, .F. ) ;
#43717 = CARTESIAN_POINT ( 'NONE',  ( 11.07143661373999954, 7.542210745176000763, 6.453318764178000322 ) ) ;
#43718 = CARTESIAN_POINT ( 'NONE',  ( 10.51210369451062832, -4.198138975488563851, 8.352216648108843344 ) ) ;
#43719 = DIRECTION ( 'NONE',  ( 0.000000000000000000, 0.000000000000000000, -1.000000000000000000 ) ) ;
#43720 = ORIENTED_EDGE ( 'NONE', *, *, #63025, .F. ) ;
#43721 = CARTESIAN_POINT ( 'NONE',  ( 12.48129647765401451, -3.124180215534335225, 12.20653620603298073 ) ) ;
#43722 = CARTESIAN_POINT ( 'NONE',  ( 9.631696787963999640, -3.803923679411099990, -6.375149554610999303 ) ) ;
#43723 = LINE ( 'NONE', #28329, #57165 ) ;
#43724 = FACE_OUTER_BOUND ( 'NONE', #38051, .T. ) ;
#43725 = CARTESIAN_POINT ( 'NONE',  ( 11.28533594839949750, 4.750012929834699804, -6.640482273977399430 ) ) ;
#43726 = CARTESIAN_POINT ( 'NONE',  ( 12.42151672539423934, -0.6105138165312035126, 12.58520200551375545 ) ) ;
#43727 = CARTESIAN_POINT ( 'NONE',  ( 9.523698341228998387, 4.852728889087999598, 8.683917172082999514 ) ) ;
#43728 = LINE ( 'NONE', #50352, #24912 ) ;
#43729 = CARTESIAN_POINT ( 'NONE',  ( 12.72061467711774974, 1.765703846569725011, 12.47566797393135651 ) ) ;
#43730 = VERTEX_POINT ( 'NONE', #11829 ) ;
#43731 = CARTESIAN_POINT ( 'NONE',  ( 9.073148997461000675, 5.167567567567999731, -6.822293592207000934 ) ) ;
#43732 = CARTESIAN_POINT ( 'NONE',  ( 11.03918313518939875, 3.292400735470800033, -8.394758848575399668 ) ) ;
#43733 = CARTESIAN_POINT ( 'NONE',  ( 18.23353331006402200, -0.2537702651956276201, 12.59744904646397679 ) ) ;
#43735 = EDGE_CURVE ( 'NONE', #12913, #6746, #35036, .T. ) ;
#43734 = B_SPLINE_CURVE_WITH_KNOTS ( 'NONE', 3,
 ( #27174, #33112, #27871, #6174, #48497 ),
 .UNSPECIFIED., .F., .F.,
 ( 4, 1, 4 ),
 ( 0.000000000000000000, 0.5000000000000000000, 1.000000000000000000 ),
 .UNSPECIFIED. ) ;
#43736 = CARTESIAN_POINT ( 'NONE',  ( 11.27531844363630320, 4.339035105373933554, 6.691304915923900865 ) ) ;
#43738 = CARTESIAN_POINT ( 'NONE',  ( 17.92176999521577230, -0.5062894561356391376, 12.68641719396355860 ) ) ;
#43737 = CARTESIAN_POINT ( 'NONE',  ( 7.800985831153996131, 4.602212482482000766, 6.372454311207003563 ) ) ;
#43739 = CARTESIAN_POINT ( 'NONE',  ( 10.92441504065829960, -3.305585767322499979, -6.982228367137699898 ) ) ;
#43740 = CARTESIAN_POINT ( 'NONE',  ( 11.00008140503725329, 5.084125838812211917, 7.632269737612043414 ) ) ;
#43741 = EDGE_LOOP ( 'NONE', ( #54522, #55647, #26573, #25620 ) ) ;
#43742 = ADVANCED_FACE ( 'NONE', ( #16726 ), #34000, .F. ) ;
#43743 = CARTESIAN_POINT ( 'NONE',  ( 0.8763362521023999596, 3.132555770593000055, 1.386468609675000074 ) ) ;
#43744 = FACE_OUTER_BOUND ( 'NONE', #46409, .T. ) ;
#43745 = CARTESIAN_POINT ( 'NONE',  ( 8.241912900173000267, 4.599999999999999645, 6.117539782833000928 ) ) ;
#43747 = B_SPLINE_CURVE_WITH_KNOTS ( 'NONE', 3,
 ( #13868, #19102, #35198, #56510, #66304, #8616, #29965, #61070, #13189, #51266, #28575, #49890, #7933, #3362 ),
 .UNSPECIFIED., .F., .F.,
 ( 4, 2, 2, 1, 1, 2, 2, 4 ),
 ( 0.000000000000000000, 0.2499999999999955036, 0.3749999999999888978, 0.4374999999999855116, 0.4687499999999806821, 0.4843749999999786282, 0.4999999999999765743, 1.000000000000000000 ),
 .UNSPECIFIED. ) ;
#43746 = DIRECTION ( 'NONE',  ( 1.000000000000000000, 0.000000000000000000, 0.000000000000000000 ) ) ;
#43748 = VECTOR ( 'NONE', #35681, 1000.000000000000000 ) ;
#43749 = CARTESIAN_POINT ( 'NONE',  ( 12.22896558337872897, -2.961354171198312457, 13.68321881638708604 ) ) ;
#43750 = CARTESIAN_POINT ( 'NONE',  ( 11.00333291544899872, -3.468906853242413657, 6.341063066638221279 ) ) ;
#43751 = LINE ( 'NONE', #17521, #16521 ) ;
#43752 = ORIENTED_EDGE ( 'NONE', *, *, #46571, .T. ) ;
#43753 = DIRECTION ( 'NONE',  ( 1.000000000000000000, 0.000000000000000000, 0.000000000000000000 ) ) ;
#43754 = CARTESIAN_POINT ( 'NONE',  ( 10.84999882987999875, -12.50000000000000000, 0.000000000000000000 ) ) ;
#43755 = CARTESIAN_POINT ( 'NONE',  ( 9.709204462303732797, 2.899999999999999911, 6.662590550607019324 ) ) ;
#43756 = CARTESIAN_POINT ( 'NONE',  ( 1.032791847629000115, 1.715249283262000102, -3.156226979448999881 ) ) ;
#43757 = CARTESIAN_POINT ( 'NONE',  ( 11.36190547754509872, -3.108323067758099967, 7.471700551735359852 ) ) ;
#43758 = EDGE_CURVE ( 'NONE', #35905, #46383, #55871, .T. ) ;
#43759 = CARTESIAN_POINT ( 'NONE',  ( 18.08840168032788398, 2.173540213500963159, -12.52169971385178115 ) ) ;
#43760 = CARTESIAN_POINT ( 'NONE',  ( 11.07345995138000028, 3.998673170817999889, 8.920816085870999501 ) ) ;
#43761 = CARTESIAN_POINT ( 'NONE',  ( 10.48133997687999930, 4.184599793140999502, 8.346298710230199092 ) ) ;
#43762 = AXIS2_PLACEMENT_3D ( 'NONE', #27360, #49028, #1135 ) ;
#43763 = B_SPLINE_CURVE_WITH_KNOTS ( 'NONE', 3,
 ( #51404, #50723, #55626, #66446 ),
 .UNSPECIFIED., .F., .F.,
 ( 4, 4 ),
 ( 0.000000000000000000, 1.000000000000000000 ),
 .UNSPECIFIED. ) ;
#43764 = CARTESIAN_POINT ( 'NONE',  ( 11.59213512191444018, -4.803449168604846164, -7.174950736703190834 ) ) ;
#43765 = CARTESIAN_POINT ( 'NONE',  ( 11.28109314679000086, -2.660122028910999692, -6.904120269057000492 ) ) ;
#43766 = DIRECTION ( 'NONE',  ( 1.000000000000000000, 0.000000000000000000, 0.000000000000000000 ) ) ;
#43767 = CARTESIAN_POINT ( 'NONE',  ( 9.529144223516999190, -2.330665094450000030, -8.349943402163999551 ) ) ;
#43768 = CARTESIAN_POINT ( 'NONE',  ( 12.73341336112467559, -10.78295181804177894, 4.410266442042688695 ) ) ;
#43769 = CARTESIAN_POINT ( 'NONE',  ( 9.411508750485571895, 5.333019778067357386, 7.282918306495822947 ) ) ;
#43770 = ORIENTED_EDGE ( 'NONE', *, *, #58517, .T. ) ;
#43771 = CARTESIAN_POINT ( 'NONE',  ( 8.414360841228999632, 5.461114003844000031, -8.582501063019000398 ) ) ;
#43772 = ORIENTED_EDGE ( 'NONE', *, *, #47854, .F. ) ;
#43773 = CARTESIAN_POINT ( 'NONE',  ( 17.98387256218937225, -2.954798081836346846, 13.56641578797404790 ) ) ;
#43774 = CARTESIAN_POINT ( 'NONE',  ( 10.07503300763299947, -3.118110956362800223, -8.424978748982498544 ) ) ;
#43775 = ORIENTED_EDGE ( 'NONE', *, *, #49105, .F. ) ;
#43776 = CARTESIAN_POINT ( 'NONE',  ( 11.59603632436369125, 3.157359628034400068, 7.696781148700499564 ) ) ;
#43777 = CARTESIAN_POINT ( 'NONE',  ( 5.647538256146063418, 0.7451564378516357667, 0.8540504721569680546 ) ) ;
#43778 = CARTESIAN_POINT ( 'NONE',  ( 8.741072744221000335, -4.062652182992059657, -8.366433385397499478 ) ) ;
#43779 = CARTESIAN_POINT ( 'NONE',  ( 9.861802827889732725, -2.874603711573434417, -6.749639981083136675 ) ) ;
#43780 = DIRECTION ( 'NONE',  ( -1.000000000000000000, 0.000000000000000000, 0.000000000000000000 ) ) ;
#43781 = DIRECTION ( 'NONE',  ( 0.000000000000000000, -1.000000000000000000, 0.000000000000000000 ) ) ;
#43782 = CARTESIAN_POINT ( 'NONE',  ( 11.59999999999999964, -4.304783012932057673, -6.544326332797709256 ) ) ;
#43783 = CARTESIAN_POINT ( 'NONE',  ( 10.26368921839999970, -4.794141574281000295, -8.804455889106000299 ) ) ;
#43784 = CARTESIAN_POINT ( 'NONE',  ( 11.09999999999999964, 4.000000000000000000, -7.500000000000000000 ) ) ;
#43785 = EDGE_LOOP ( 'NONE', ( #59060, #47242, #68502, #8372, #50659, #20528, #49174 ) ) ;
#43786 = CARTESIAN_POINT ( 'NONE',  ( 10.19741084123000086, 4.262870449202000422, -8.811513791423999820 ) ) ;
#43787 = EDGE_LOOP ( 'NONE', ( #50270, #21768, #11420, #5973 ) ) ;
#43788 = CARTESIAN_POINT ( 'NONE',  ( 10.82101354018296391, 3.231816600031359510, -6.500416447002272946 ) ) ;
#43789 = AXIS2_PLACEMENT_3D ( 'NONE', #56768, #56418, #68263 ) ;
#43790 = EDGE_LOOP ( 'NONE', ( #20393, #32189 ) ) ;
#43791 = DIRECTION ( 'NONE',  ( 0.000000000000000000, 1.000000000000000000, 0.000000000000000000 ) ) ;
#43792 = FACE_OUTER_BOUND ( 'NONE', #57843, .T. ) ;
#43793 = CARTESIAN_POINT ( 'NONE',  ( 10.45222191436347714, 4.437430566769827500, 8.256798586434323184 ) ) ;
#43794 = CARTESIAN_POINT ( 'NONE',  ( 23.58885762929001473, 13.25331360343164278, -4.277525096992856213 ) ) ;
#43795 = ADVANCED_FACE ( 'NONE', ( #45041 ), #61117, .T. ) ;
#43796 = CARTESIAN_POINT ( 'NONE',  ( 9.466846873515667227, -4.768183399968645375, -8.499583552997723501 ) ) ;
#43797 = EDGE_CURVE ( 'NONE', #44976, #14053, #19964, .T. ) ;
#43798 = CARTESIAN_POINT ( 'NONE',  ( 10.57223537388000167, -4.020426196685999543, 8.920680607665000039 ) ) ;
#43799 = CARTESIAN_POINT ( 'NONE',  ( 7.848633776075367940, 2.977326305471488244, -6.549596320077490041 ) ) ;
#43800 = ADVANCED_FACE ( 'NONE', ( #61457 ), #15503, .F. ) ;
#43801 = CARTESIAN_POINT ( 'NONE',  ( 12.18829585510503577, 0.1017048024283954966, 13.89950429703524826 ) ) ;
#43802 = VERTEX_POINT ( 'NONE', #5475 ) ;
#43803 = CARTESIAN_POINT ( 'NONE',  ( 10.94535373587000038, 2.924507478818999751, 4.924562996314999275 ) ) ;
#43804 = CARTESIAN_POINT ( 'NONE',  ( 10.65445404527255135, 4.823605068675146157, -4.782660509889021583 ) ) ;
#43805 = CARTESIAN_POINT ( 'NONE',  ( 9.404204162135625822, 4.790364090350968773, 7.875309037467246753 ) ) ;
#43806 = CARTESIAN_POINT ( 'NONE',  ( 4.525603349966000444, 1.298316671829000013, 0.3090933427313000137 ) ) ;
#43807 = VECTOR ( 'NONE', #13717, 1000.000000000000000 ) ;
#43808 = CARTESIAN_POINT ( 'NONE',  ( 8.532195280408998883, 5.331510020787000315, -8.114341808290998159 ) ) ;
#43809 = CARTESIAN_POINT ( 'NONE',  ( 4.149992563292000725, -2.000000000000000000, 0.000000000000000000 ) ) ;
#43810 = AXIS2_PLACEMENT_3D ( 'NONE', #6121, #37600, #27459 ) ;
#43811 = CARTESIAN_POINT ( 'NONE',  ( 9.882901294779998125, -4.314558311729999929, -9.161035779983999205 ) ) ;
#43812 = ORIENTED_EDGE ( 'NONE', *, *, #16966, .F. ) ;
#43813 = CARTESIAN_POINT ( 'NONE',  ( 9.523148997461001741, -5.167567567567999731, -6.822293592207000934 ) ) ;
#43814 = CARTESIAN_POINT ( 'NONE',  ( 18.30003129334700063, 2.732683817159999862, -11.53064095410000078 ) ) ;
#43815 = CARTESIAN_POINT ( 'NONE',  ( 4.400000000000000355, 0.5526513453421999511, 1.394480724316999876 ) ) ;
#43816 = DIRECTION ( 'NONE',  ( 1.267684221833849905E-20, -0.9999999999999997780, -2.657887425080999156E-08 ) ) ;
#43817 = CARTESIAN_POINT ( 'NONE',  ( 8.549163638619971195, -3.170442981555772199, 5.998973939403969169 ) ) ;
#43818 = CARTESIAN_POINT ( 'NONE',  ( 1.042640132542499654, 3.058252359239899132, 1.762666431298154146 ) ) ;
#43819 = CARTESIAN_POINT ( 'NONE',  ( 10.89324174884020024, 3.967693531726030010, -8.674442868902998427 ) ) ;
#43820 = CARTESIAN_POINT ( 'NONE',  ( 9.432025935145999185, 3.854158361175799907, -6.506233167833100239 ) ) ;
#43822 = CARTESIAN_POINT ( 'NONE',  ( 10.55944656072999877, -2.874072957412999951, 4.818572726091000291 ) ) ;
#43821 = CARTESIAN_POINT ( 'NONE',  ( 10.33030484851599873, -3.211495113978299898, 7.139489266142899915 ) ) ;
#43823 = CARTESIAN_POINT ( 'NONE',  ( 11.18559687351634935, -2.907767014557174790, 8.129523725463618788 ) ) ;
#43824 = EDGE_LOOP ( 'NONE', ( #53487, #47804, #5066, #3734 ) ) ;
#43825 = CARTESIAN_POINT ( 'NONE',  ( 10.77368717260499942, 3.460071470104900015, 6.618743573831199711 ) ) ;
#43826 = CARTESIAN_POINT ( 'NONE',  ( 10.27814441345999974, -5.521593622715999850, 8.751220666652999469 ) ) ;
#43827 = CARTESIAN_POINT ( 'NONE',  ( 10.49288779216199785, 5.056118594996999782, 7.119137915499500480 ) ) ;
#43828 = CARTESIAN_POINT ( 'NONE',  ( 11.29998770065200731, -3.699024161916728115, 11.75540420325642543 ) ) ;
#43829 = B_SPLINE_CURVE_WITH_KNOTS ( 'NONE', 3,
 ( #2887, #8483, #24901, #61965, #30495, #35740, #51808, #46231, #13047, #3906, #44864, #61616, #57058, #34376, #55696, #2542, #7792, #40982, #56380, #24562, #30166, #29132, #45885, #50440, #67195, #8823, #14078, #23869, #45208, #66511, #51469, #18633, #39962, #67538, #8139, #61280 ),
 .UNSPECIFIED., .F., .F.,
 ( 4, 2, 2, 1, 2, 2, 2, 1, 1, 1, 2, 2, 2, 2, 2, 2, 2, 2, 2, 4 ),
 ( 0.000000000000000000, 0.1249999999992055799, 0.1874999999988075372, 0.2187499999986079191, 0.2343749999985092758, 0.2499999999984106325, 0.3749999999976186826, 0.4374999999972214448, 0.4687499999970250464, 0.4843749999969280129, 0.4921874999968802733, 0.4999999999968325337, 0.5624999999972273290, 0.5937499999974238385, 0.6093749999975215381, 0.6249999999976191267, 0.6874999999980111465, 0.7187499999982103205, 0.7499999999984094945, 1.000000000000000000 ),
 .UNSPECIFIED. ) ;
#43830 = CARTESIAN_POINT ( 'NONE',  ( 10.71756905878999966, -3.040221764047000175, 8.808455607108001573 ) ) ;
#43831 = CARTESIAN_POINT ( 'NONE',  ( 9.954831044986722333, -2.229402479047418950, 7.375981937142048750 ) ) ;
#43832 = CARTESIAN_POINT ( 'NONE',  ( 10.39393020684999946, 2.750000000000000000, 7.500000000000000000 ) ) ;
#43833 = CARTESIAN_POINT ( 'NONE',  ( 9.887950584426999256, -3.601336184534900120, -6.578094656394299911 ) ) ;
#43834 = VECTOR ( 'NONE', #42158, 1000.000000000000000 ) ;
#43835 = CARTESIAN_POINT ( 'NONE',  ( 6.456205881263000101, 1.377540824270000019, 0.5088348457508999889 ) ) ;
#43836 = EDGE_CURVE ( 'NONE', #65244, #1839, #15960, .T. ) ;
#43837 = CARTESIAN_POINT ( 'NONE',  ( 10.40987047770899920, -5.250000000000000888, 7.249610810850631637 ) ) ;
#43838 = DIRECTION ( 'NONE',  ( 0.7071067617951957152, 0.000000000000000000, -0.7071068005778986532 ) ) ;
#43839 = CARTESIAN_POINT ( 'NONE',  ( 11.54749144726329924, -4.500836215462999945, 8.206726025856399431 ) ) ;
#43840 = CARTESIAN_POINT ( 'NONE',  ( 11.85979573085659844, 4.840012015667699785, -7.645349278262099979 ) ) ;
#43841 = ADVANCED_FACE ( 'NONE', ( #36954 ), #23128, .T. ) ;
#43842 = CARTESIAN_POINT ( 'NONE',  ( 12.30534114219160635, 2.122480415404790932, -13.74636906787548263 ) ) ;
#43843 = CARTESIAN_POINT ( 'NONE',  ( 24.45999032648100169, -8.787256713296999422, 8.710686399493999588 ) ) ;
#43844 = CARTESIAN_POINT ( 'NONE',  ( 8.266851002545999805, -2.832432432432000269, 6.822293592207000934 ) ) ;
#43845 = ORIENTED_EDGE ( 'NONE', *, *, #29818, .T. ) ;
#43846 = CARTESIAN_POINT ( 'NONE',  ( 11.36656731458420033, -12.29889127619872724, -1.513729328724678469 ) ) ;
#43847 = LINE ( 'NONE', #52956, #25404 ) ;
#43848 = CARTESIAN_POINT ( 'NONE',  ( 25.36464211350600451, -8.490054962244000691, -7.944963175427000479 ) ) ;
#43849 = CARTESIAN_POINT ( 'NONE',  ( 7.947784805529094498, -5.286778829772836197, 7.027374276529119612 ) ) ;
#43850 = CARTESIAN_POINT ( 'NONE',  ( 7.000000000000000888, 9.166793235311024191, 4.705382354989500193 ) ) ;
#43851 = CARTESIAN_POINT ( 'NONE',  ( 13.55309301929700005, 12.11670754034000019, 2.533073449765999907 ) ) ;
#43852 = ORIENTED_EDGE ( 'NONE', *, *, #5533, .T. ) ;
#43853 = CARTESIAN_POINT ( 'NONE',  ( 5.000000000000000000, 0.2999999999999999889, 2.733587386567000177 ) ) ;
#43854 = CARTESIAN_POINT ( 'NONE',  ( 18.02642401515173631, 2.910531091912870405, -13.57777274349195906 ) ) ;
#43855 = VERTEX_POINT ( 'NONE', #32736 ) ;
#43856 = CARTESIAN_POINT ( 'NONE',  ( 25.00274840847853142, -8.478821250423088429, -8.837051340891205697 ) ) ;
#43857 = CARTESIAN_POINT ( 'NONE',  ( 25.09891544561744681, 8.522828975275432484, -8.212590430020295429 ) ) ;
#43858 = CARTESIAN_POINT ( 'NONE',  ( 8.971339158776000744, 4.082930418187999955, -6.104944817728999773 ) ) ;
#43859 = CARTESIAN_POINT ( 'NONE',  ( 6.537250824846000619, -1.012620940260093416, 1.149827999411389357 ) ) ;
#43860 = CARTESIAN_POINT ( 'NONE',  ( 8.793536308084599185, 2.899999999999999911, 6.665341197421785324 ) ) ;
#43861 = CARTESIAN_POINT ( 'NONE',  ( 8.160635841226000053, 2.425297598239999797, -6.437049665397999831 ) ) ;
#43862 = CARTESIAN_POINT ( 'NONE',  ( 15.89979320885400327, -3.824231472901999496, -11.71686814605000038 ) ) ;
#43863 = CARTESIAN_POINT ( 'NONE',  ( 10.31059687351566545, -4.629523725463621453, 8.592232985442823434 ) ) ;
#43864 = VERTEX_POINT ( 'NONE', #69102 ) ;
#43865 = CARTESIAN_POINT ( 'NONE',  ( 9.013429960698999821, -4.933961117404000341, 8.417889755737999025 ) ) ;
#43866 = CARTESIAN_POINT ( 'NONE',  ( 27.09999999999999787, 0.000000000000000000, 0.000000000000000000 ) ) ;
#43867 = DIRECTION ( 'NONE',  ( 0.000000000000000000, 0.7158784314710769925, -0.6982249432342777506 ) ) ;
#43868 = EDGE_LOOP ( 'NONE', ( #625, #16421, #13346, #46426, #50943, #14374, #1458, #62523, #24145, #56604, #44026, #67966, #24584, #50254, #4980 ) ) ;
#43869 = FACE_OUTER_BOUND ( 'NONE', #15406, .T. ) ;
#43870 = DIRECTION ( 'NONE',  ( 0.000000000000000000, -1.000000000000000000, 0.000000000000000000 ) ) ;
#43871 = ORIENTED_EDGE ( 'NONE', *, *, #17313, .F. ) ;
#43872 = CARTESIAN_POINT ( 'NONE',  ( 9.204063610504999104, 4.411988005505000032, 6.583971515917899531 ) ) ;
#43873 = CARTESIAN_POINT ( 'NONE',  ( 17.84632148815561692, -1.821395309707484422, -12.46765979085770937 ) ) ;
#43874 = CARTESIAN_POINT ( 'NONE',  ( 4.419090712286999789, 0.3277123218568999685, 1.522640465285999944 ) ) ;
#43875 = CARTESIAN_POINT ( 'NONE',  ( 11.60000000000000320, 4.866008700487510552, -6.727195615969563391 ) ) ;
#43876 = CARTESIAN_POINT ( 'NONE',  ( 24.71765909950762108, 11.77379917328191183, -3.190796897422294887 ) ) ;
#43877 = DIRECTION ( 'NONE',  ( -1.000000000000000000, 0.000000000000000000, 0.000000000000000000 ) ) ;
#43878 = EDGE_CURVE ( 'NONE', #38751, #31059, #6650, .T. ) ;
#43879 = EDGE_CURVE ( 'NONE', #59129, #68689, #36502, .T. ) ;
#43880 = CARTESIAN_POINT ( 'NONE',  ( 9.839304848515999069, 4.788504886021700102, 7.139489266142899915 ) ) ;
#43881 = EDGE_CURVE ( 'NONE', #67865, #47885, #67501, .T. ) ;
#43882 = EDGE_CURVE ( 'NONE', #63961, #46988, #28892, .T. ) ;
#43883 = CARTESIAN_POINT ( 'NONE',  ( 8.164397154371004106, -4.665396042252996978, 6.167056685642003266 ) ) ;
#43884 = VERTEX_POINT ( 'NONE', #50202 ) ;
#43885 = DIRECTION ( 'NONE',  ( -0.000000000000000000, -0.000000000000000000, 1.000000000000000000 ) ) ;
#43886 = CARTESIAN_POINT ( 'NONE',  ( 10.24394221959000184, 3.220342255699999878, -6.005413528376000620 ) ) ;
#43887 = CARTESIAN_POINT ( 'NONE',  ( 11.09999999999999964, 7.281355457699000056, 6.286510842043999681 ) ) ;
#43888 = CARTESIAN_POINT ( 'NONE',  ( 12.78422499708364768, 3.124999410541264400, -13.52084427634423314 ) ) ;
#43889 = CIRCLE ( 'NONE', #3645, 0.6999999999999992895 ) ;
#43890 = CARTESIAN_POINT ( 'NONE',  ( 10.14029229006299992, -2.893743561734000380, -6.857675253263499471 ) ) ;
#43891 = CARTESIAN_POINT ( 'NONE',  ( 10.34020413671000149, -4.202027362542999356, 9.459588031742001135 ) ) ;
#43892 = CARTESIAN_POINT ( 'NONE',  ( 17.78863088638135537, -0.6916885356984026068, 13.98290438115173373 ) ) ;
#43893 = CARTESIAN_POINT ( 'NONE',  ( 25.09299735342200321, -3.211993599267000121, 11.60337401171999971 ) ) ;
#43894 = B_SPLINE_CURVE_WITH_KNOTS ( 'NONE', 3,
 ( #59197, #16204, #48364, #26710, #21444, #21788 ),
 .UNSPECIFIED., .F., .F.,
 ( 4, 2, 4 ),
 ( 0.000000000000000000, 0.5000000000000000000, 1.000000000000000000 ),
 .UNSPECIFIED. ) ;
#43895 = EDGE_LOOP ( 'NONE', ( #11445, #23307, #66411, #1167 ) ) ;
#43896 = ORIENTED_EDGE ( 'NONE', *, *, #2298, .F. ) ;
#43897 = CARTESIAN_POINT ( 'NONE',  ( 9.942214158770999788, 3.986577607995999806, -9.280166295424001177 ) ) ;
#43898 = CARTESIAN_POINT ( 'NONE',  ( 12.34379246237138261, -0.4226248004909251010, 13.89137006862893209 ) ) ;
#43899 = CARTESIAN_POINT ( 'NONE',  ( 12.78475456307759828, -0.6250000000000008882, -13.88107975066922783 ) ) ;
#43900 = CARTESIAN_POINT ( 'NONE',  ( 9.323728576950999880, -3.947350124452999598, 6.051857392047999440 ) ) ;
#43901 = LINE ( 'NONE', #54729, #29479 ) ;
#43902 = EDGE_CURVE ( 'NONE', #43682, #21925, #33781, .T. ) ;
#43903 = CARTESIAN_POINT ( 'NONE',  ( 8.064120559623999540, -4.228293421747000735, 8.941387937291999322 ) ) ;
#43904 = CARTESIAN_POINT ( 'NONE',  ( -0.2999999999999999889, 0.5773502691895999739, 1.000000000000000000 ) ) ;
#43906 = CYLINDRICAL_SURFACE ( 'NONE', #52962, 1.250000000000000222 ) ;
#43905 = CARTESIAN_POINT ( 'NONE',  ( 10.89358376188600097, -5.078750111091999919, 6.812480849273599759 ) ) ;
#43907 = CIRCLE ( 'NONE', #11494, 1.000000000000000000 ) ;
#43908 = CARTESIAN_POINT ( 'NONE',  ( 17.60000000000000142, 48.67241131317999958, -16.56944037379999912 ) ) ;
#43909 = CARTESIAN_POINT ( 'NONE',  ( 12.09999999999999964, -4.862088370180454255, 7.087473780876516471 ) ) ;
#43910 = AXIS2_PLACEMENT_3D ( 'NONE', #66223, #34084, #7495 ) ;
#43911 = CARTESIAN_POINT ( 'NONE',  ( 23.56664675778400309, 10.37811020278999941, -9.381454169592000625 ) ) ;
#43912 = CARTESIAN_POINT ( 'NONE',  ( 18.12436022580822836, -0.2580991232524050272, 12.69647497719789975 ) ) ;
#43913 = CARTESIAN_POINT ( 'NONE',  ( 6.637290055325000715, -1.379059567415999998, -0.7179416942773999555 ) ) ;
#43914 = CARTESIAN_POINT ( 'NONE',  ( 18.16560600438747386, -2.633677674594984808, -12.41941284408005153 ) ) ;
#43915 = ORIENTED_EDGE ( 'NONE', *, *, #29605, .T. ) ;
#43917 = CYLINDRICAL_SURFACE ( 'NONE', #54104, 11.84999999999999964 ) ;
#43916 = CARTESIAN_POINT ( 'NONE',  ( 8.224933059623998233, -5.629389383493999865, 8.631822608164000599 ) ) ;
#43918 = CARTESIAN_POINT ( 'NONE',  ( 8.456370280410999030, 2.836879604150999601, -8.783908972046001296 ) ) ;
#43919 = LINE ( 'NONE', #32733, #32706 ) ;
#43920 = CARTESIAN_POINT ( 'NONE',  ( 24.35365242081700288, 8.355077740100997019, -8.511587483919999642 ) ) ;
#43921 = CARTESIAN_POINT ( 'NONE',  ( 1.004152257442999963, 3.426971461775999650, -0.8894074146212000986 ) ) ;
#43922 = ADVANCED_FACE ( 'NONE', ( #8236 ), #39714, .T. ) ;
#43923 = CARTESIAN_POINT ( 'NONE',  ( 9.392382111846503179, 2.695375482096328490, 8.670063079933681749 ) ) ;
#43924 = CARTESIAN_POINT ( 'NONE',  ( 11.29596084123000210, 2.828872990872000059, -8.191118698770999629 ) ) ;
#43925 = ORIENTED_EDGE ( 'NONE', *, *, #44196, .F. ) ;
#43926 = CARTESIAN_POINT ( 'NONE',  ( 12.11859257910637844, -0.2316996085786171000, -12.59787430930301433 ) ) ;
#43927 = CARTESIAN_POINT ( 'NONE',  ( 10.84393020684979980, -5.250000000000000000, -7.500000000000000000 ) ) ;
#43928 = CARTESIAN_POINT ( 'NONE',  ( 17.94028104512295485, 3.089952709746675463, -12.21524586714253147 ) ) ;
#43929 = EDGE_CURVE ( 'NONE', #5573, #54836, #48305, .T. ) ;
#43930 = FACE_OUTER_BOUND ( 'NONE', #16018, .T. ) ;
#43931 = CARTESIAN_POINT ( 'NONE',  ( 9.250899447075999760, 4.135077451221000011, 9.175524215473998879 ) ) ;
#43932 = ORIENTED_EDGE ( 'NONE', *, *, #15720, .F. ) ;
#43933 = CARTESIAN_POINT ( 'NONE',  ( 6.256018102970999806, 1.402153912072999997, 0.4364538398439999911 ) ) ;
#43934 = VECTOR ( 'NONE', #28132, 1000.000000000000114 ) ;
#43935 = CARTESIAN_POINT ( 'NONE',  ( 7.499445280409000603, 5.564636229952000690, -7.532446618777999703 ) ) ;
#43937 = CARTESIAN_POINT ( 'NONE',  ( 11.11504246380000005, 3.456610836627000083, 5.970339330302000036 ) ) ;
#43936 = CARTESIAN_POINT ( 'NONE',  ( 8.446461008496655154, -2.261511969888099660, 7.573099163943432188 ) ) ;
#43938 = CARTESIAN_POINT ( 'NONE',  ( 12.80505043854143388, 1.760910691117811844, 12.47634535983622861 ) ) ;
#43939 = ORIENTED_EDGE ( 'NONE', *, *, #51000, .F. ) ;
#43941 = CARTESIAN_POINT ( 'NONE',  ( 11.10000000009000054, 2.699999999911000259, 6.571291220400000022 ) ) ;
#43940 = CONICAL_SURFACE ( 'NONE', #28313, 1.150090567076000214, 0.7854665416972951286 ) ;
#43942 = CARTESIAN_POINT ( 'NONE',  ( 10.23808992278000041, -2.752437370156000540, 6.820045513931999537 ) ) ;
#43943 = ORIENTED_EDGE ( 'NONE', *, *, #39009, .F. ) ;
#43944 = CARTESIAN_POINT ( 'NONE',  ( 10.90000000296000060, 2.899999999990999999, 5.160242730682999657 ) ) ;
#43945 = CARTESIAN_POINT ( 'NONE',  ( 16.13869549901199818, 3.415897281711999689, 11.19349503352999875 ) ) ;
#43946 = CARTESIAN_POINT ( 'NONE',  ( 18.17808105194527002, 0.05063168410658663854, -13.89988098555964946 ) ) ;
#43947 = ORIENTED_EDGE ( 'NONE', *, *, #40122, .T. ) ;
#43948 = CARTESIAN_POINT ( 'NONE',  ( 15.82968830470041866, -8.721231603649751918, -7.724200095968971169 ) ) ;
#43949 = CARTESIAN_POINT ( 'NONE',  ( 24.14471467316711539, -9.246855113160467710, -9.586736432819547460 ) ) ;
#43950 = CARTESIAN_POINT ( 'NONE',  ( 10.90346005378009941, 4.786957292481900161, -7.079777642108599167 ) ) ;
#43951 = CARTESIAN_POINT ( 'NONE',  ( 8.216851002544000693, 2.832432432432000269, 6.822293592207000934 ) ) ;
#43952 = CARTESIAN_POINT ( 'NONE',  ( 9.470944094206000585, -5.100000000000000533, 6.571291218949999902 ) ) ;
#43953 = ORIENTED_EDGE ( 'NONE', *, *, #23439, .T. ) ;
#43954 = CARTESIAN_POINT ( 'NONE',  ( 7.743176658771999676, 2.735218126362000124, 6.771983639047999937 ) ) ;
#43955 = CARTESIAN_POINT ( 'NONE',  ( 23.63066792764499979, -13.46837681827999944, -3.823564519506999826 ) ) ;
#43956 = DIRECTION ( 'NONE',  ( 1.000000000000000000, 0.000000000000000000, 0.000000000000000000 ) ) ;
#43957 = PRESENTATION_LAYER_ASSIGNMENT (  '', '', ( #68480 ) ) ;
#43958 = DIRECTION ( 'NONE',  ( 0.000000000000000000, -1.000000000000000000, 0.000000000000000000 ) ) ;
#43959 = ORIENTED_EDGE ( 'NONE', *, *, #27755, .T. ) ;
#43960 = CARTESIAN_POINT ( 'NONE',  ( 12.36723811880913892, -2.053846804184053632, -12.54438404081591507 ) ) ;
#43961 = VECTOR ( 'NONE', #17754, 999.9999999999998863 ) ;
#43962 = DIRECTION ( 'NONE',  ( 1.000000000000000000, 0.000000000000000000, 0.000000000000000000 ) ) ;
#43963 = CARTESIAN_POINT ( 'NONE',  ( 7.789447165042808763, 5.491073919830230743, -6.392873027944447450 ) ) ;
#43964 = CARTESIAN_POINT ( 'NONE',  ( 9.129428851719998406, 5.099284414202999827, 6.151604790022999758 ) ) ;
#43965 = DIRECTION ( 'NONE',  ( -1.000000000000000000, 0.000000000000000000, 0.000000000000000000 ) ) ;
#43966 = CARTESIAN_POINT ( 'NONE',  ( 10.23103300763299828, -3.307558760216100069, -8.226274395107198600 ) ) ;
#43967 = CARTESIAN_POINT ( 'NONE',  ( 12.61298032308283190, -3.180483649554697312, 12.19204447432963612 ) ) ;
#43968 = ADVANCED_FACE ( 'NONE', ( #23623 ), #24227, .T. ) ;
#43970 = EDGE_CURVE ( 'NONE', #10927, #35290, #13293, .T. ) ;
#43969 = CARTESIAN_POINT ( 'NONE',  ( 17.93339585188542529, -2.997500062648085883, 12.32163866699053578 ) ) ;
#43971 = ORIENTED_EDGE ( 'NONE', *, *, #12313, .T. ) ;
#43972 = CARTESIAN_POINT ( 'NONE',  ( 11.59456039236534330, -2.685288321999000249, -7.563984187103470092 ) ) ;
#43973 = VERTEX_POINT ( 'NONE', #12103 ) ;
#43974 = CARTESIAN_POINT ( 'NONE',  ( 11.60578299225600141, -12.22760809526000081, -1.919009911369000010 ) ) ;
#43975 = CARTESIAN_POINT ( 'NONE',  ( 8.500189158773000742, 2.724453559418999582, -8.908010318766001134 ) ) ;
#43976 = CARTESIAN_POINT ( 'NONE',  ( 2.265629263920999836, 1.834942145265999969, -2.713944450215000082 ) ) ;
#43977 = CARTESIAN_POINT ( 'NONE',  ( 10.13382174003999836, -5.176455793257000337, -8.189804425074999727 ) ) ;
#43978 = CARTESIAN_POINT ( 'NONE',  ( 10.77706886429733402, 2.899999999999999911, -6.444141223373583749 ) ) ;
#43979 = CARTESIAN_POINT ( 'NONE',  ( 24.32734093809899889, 12.60105586225999907, 3.144288050074000029 ) ) ;
#43980 = CARTESIAN_POINT ( 'NONE',  ( 10.40537527825904007, -5.100000000000000533, -6.445686799541589629 ) ) ;
#43981 = ORIENTED_EDGE ( 'NONE', *, *, #9919, .T. ) ;
#43982 = CARTESIAN_POINT ( 'NONE',  ( 1.839363843321667691, -3.114462284487641508, -1.632227178342313012 ) ) ;
#43983 = VECTOR ( 'NONE', #36495, 1000.000000000000114 ) ;
#43984 = CARTESIAN_POINT ( 'NONE',  ( 10.37373942323999998, 2.215265813302000009, 7.703982730183001060 ) ) ;
#43985 = CARTESIAN_POINT ( 'NONE',  ( 1.850000260467999924, 1.625000260409000141, -4.909918316425000356E-10 ) ) ;
#43986 = EDGE_CURVE ( 'NONE', #19784, #1839, #33433, .T. ) ;
#43987 = CARTESIAN_POINT ( 'NONE',  ( 4.500000000000000000, 13.10000000000000142, -1.604287306883032847E-15 ) ) ;
#43988 = CARTESIAN_POINT ( 'NONE',  ( 5.399998535875000449, 12.99045401563999924, -1.690592933733000125 ) ) ;
#43989 = CIRCLE ( 'NONE', #67422, 1.800000000000000044 ) ;
#43990 = CARTESIAN_POINT ( 'NONE',  ( 10.82595391537419971, 4.716560378569699452, -7.986661909549199301 ) ) ;
#43991 = CARTESIAN_POINT ( 'NONE',  ( 10.45582195740702325, 2.255160618932426697, 7.383274727460120701 ) ) ;
#43992 = CARTESIAN_POINT ( 'NONE',  ( 24.03156049766399960, -9.408031995601998432, -9.735591824543000428 ) ) ;
#43993 = CARTESIAN_POINT ( 'NONE',  ( 24.63625278502800242, -8.802584369108002349, 9.348454315309000506 ) ) ;
#43994 = CARTESIAN_POINT ( 'NONE',  ( 23.60000000000000497, -12.92119876218218977, 5.203224594798002478 ) ) ;
#43995 = EDGE_LOOP ( 'NONE', ( #5185, #963, #7659, #9026 ) ) ;
#43996 = CARTESIAN_POINT ( 'NONE',  ( 7.822379440378000481, -4.636725880537000855, 9.378965771357000492 ) ) ;
#43997 = CARTESIAN_POINT ( 'NONE',  ( 9.619730517102000888, -2.477793449086000077, -8.275032865112999403 ) ) ;
#43998 = CARTESIAN_POINT ( 'NONE',  ( 17.92067731499815864, 3.006998531728875435, 13.55270476886629716 ) ) ;
#43999 = DIRECTION ( 'NONE',  ( 1.000000000000000000, 0.000000000000000000, 0.000000000000000000 ) ) ;
#44000 = CARTESIAN_POINT ( 'NONE',  ( 10.71503032197929883, -3.256621462143499901, -6.460430507351999196 ) ) ;
#44001 = ORIENTED_EDGE ( 'NONE', *, *, #18479, .F. ) ;
#44002 = STYLED_ITEM ( 'NONE', ( #13169 ), #31875 ) ;
#44003 = CARTESIAN_POINT ( 'NONE',  ( 24.87965708725800340, 2.960048322974000001, -11.62351559612999807 ) ) ;
#44004 = CARTESIAN_POINT ( 'NONE',  ( 7.256079719589999755, 2.531201476950000195, 8.216704145297999418 ) ) ;
#44005 = AXIS2_PLACEMENT_3D ( 'NONE', #45324, #8254, #61051 ) ;
#44007 = CARTESIAN_POINT ( 'NONE',  ( 9.793536308083167441, -2.899999999999999911, 6.665341197420959318 ) ) ;
#44006 = CARTESIAN_POINT ( 'NONE',  ( 9.939260841229000221, 5.099602161831000124, -9.049221499261999924 ) ) ;
#44008 = CARTESIAN_POINT ( 'NONE',  ( 3.023038497928110413, -3.255317685661237803, 0.1302360752436395042 ) ) ;
#44009 = ORIENTED_EDGE ( 'NONE', *, *, #22248, .T. ) ;
#44010 = CARTESIAN_POINT ( 'NONE',  ( 10.96876099447000108, 2.333339469804000199, 6.524055942683999021 ) ) ;
#44011 = CARTESIAN_POINT ( 'NONE',  ( 17.69797138021026939, -3.108785234939712261, -13.52525919603468552 ) ) ;
#44012 = CARTESIAN_POINT ( 'NONE',  ( 10.96949144726329806, 3.419793223320000131, 8.318725197575499664 ) ) ;
#44013 = ADVANCED_FACE ( 'NONE', ( #49500 ), #55790, .F. ) ;
#44014 = CARTESIAN_POINT ( 'NONE',  ( 9.813358178091998951, -5.349400659402999914, 6.657024270273000255 ) ) ;
#44015 = CARTESIAN_POINT ( 'NONE',  ( 8.205377021103002377, 3.106081841748002059, 6.107037662485001128 ) ) ;
#44017 = ORIENTED_EDGE ( 'NONE', *, *, #56625, .F. ) ;
#44016 = AXIS2_PLACEMENT_3D ( 'NONE', #63435, #48397, #20450 ) ;
#44018 = CARTESIAN_POINT ( 'NONE',  ( 9.020964430773000586, -2.907392932634000005, 6.146188468825999784 ) ) ;
#44019 = FACE_OUTER_BOUND ( 'NONE', #400, .T. ) ;
#44021 = CARTESIAN_POINT ( 'NONE',  ( 10.71315564678999976, -2.619204038425999581, -8.142086897834001746 ) ) ;
#44020 = CARTESIAN_POINT ( 'NONE',  ( 12.46470380486700158, -12.15408297959000095, 3.184072412108000183 ) ) ;
#44022 = CARTESIAN_POINT ( 'NONE',  ( 7.801841845076483040, -4.493699489315019946, 9.169207277517051224 ) ) ;
#44023 = CARTESIAN_POINT ( 'NONE',  ( 10.21608469020999976, -5.961703525007000515, 7.319668113368000384 ) ) ;
#44024 = CARTESIAN_POINT ( 'NONE',  ( 11.38678751119029897, -5.166297436425000278, -8.110172976325500827 ) ) ;
#44025 = CARTESIAN_POINT ( 'NONE',  ( 10.28462143724499889, -3.241588663654300095, 8.353549467159899322 ) ) ;
#44026 = ORIENTED_EDGE ( 'NONE', *, *, #63133, .F. ) ;
#44027 = CARTESIAN_POINT ( 'NONE',  ( 25.29987261391899978, -9.517611874540000017, 8.103398312166998352 ) ) ;
#44028 = CARTESIAN_POINT ( 'NONE',  ( 10.92380110216399913, -4.973546009874400653, 8.094557215852098864 ) ) ;
#44029 = DIRECTION ( 'NONE',  ( 0.000000000000000000, -0.9905022095861402143, -0.1374968101629056305 ) ) ;
#44030 = CARTESIAN_POINT ( 'NONE',  ( 10.22687885159599830, 5.132709421626000079, 7.635128076451499268 ) ) ;
#44031 = EDGE_LOOP ( 'NONE', ( #43166, #43636, #48741, #42878, #33992 ) ) ;
#44032 = B_SPLINE_SURFACE_WITH_KNOTS ( 'NONE', 3, 3, ( 
 ( #8559, #66591, #40044, #61355, #36155, #9575, #53268, #30917, #57818, #41745, #5370, #20077, #36497, #68997, #68298, #52230, #37187, #4330, #57467, #5708, #26708, #9927, #25664, #58506, #37526, #48362, #14835, #58852, #10611, #42434, #10962, #31265, #68645, #27049, #42777, #21109, #58169, #63401, #46996, #26360, #10270, #32302, #20763, #20417, #53610, #31603, #31951, #42093, #52575, #52925, #48022, #15857, #41406, #62712, #5021, #63046, #4669, #125, #15522, #15173, #26011, #47340, #47686, #36849, #63745, #21442, #64084 ),
 ( #16202, #54293, #27389, #32637, #469, #27744, #59543, #28082, #12344, #7436, #11638, #22135, #28433, #32979, #28787, #16546, #6395, #64773, #17594, #38921, #21786, #6742, #33677, #49057, #16887, #43120, #23174, #59885, #1856, #22825, #54995, #38562, #1507, #1163, #43820, #44173, #17942, #37876, #59195, #7096, #11297, #38214, #43476, #49747, #64424, #22478, #49396, #48716, #53947, #60242, #6050, #818, #55340, #44523, #65117, #17240, #65818, #39262, #11994, #33331, #60585, #12690, #65469, #34027, #54648, #29482, #57055 ),
 ( #40294, #61962, #14420, #67192, #14075, #56377, #66167, #39605, #56027, #66508, #67535, #24898, #45550, #8480, #2884, #34373, #45882, #3563, #13394, #61613, #18286, #40628, #51466, #29129, #44861, #2539, #34716, #50789, #35398, #13729, #2207, #29824, #3232, #46228, #8136, #7789, #13044, #50098, #24207, #39959, #51129, #23520, #8820, #35061, #24559, #30163, #19659, #61276, #35737, #19304, #18630, #66855, #60932, #9155, #23866, #50437, #56724, #18969, #40979, #55692, #62302, #45203, #25928, #36768, #47946, #31522, #46 ),
 ( #15095, #52844, #58090, #37448, #16122, #20684, #42363, #64005, #47605, #63664, #10193, #46574, #20001, #36419, #46914, #21366, #5286, #47258, #4941, #52496, #14756, #26279, #53188, #62968, #42014, #67882, #21029, #31870, #9493, #25238, #52146, #57733, #9844, #15781, #63315, #51805, #68912, #37111, #26628, #31190, #57388, #62631, #30492, #4592, #20335, #58425, #3903, #10530, #15443, #42698, #58769, #41325, #41664, #36074, #30836, #68217, #68562, #4250, #25588, #53868, #59114, #11907, #6310, #12262, #16460, #27656, #5969 ) ),
 .UNSPECIFIED., .F., .F., .F.,
 ( 4, 4 ),
 ( 4, 1, 1, 1, 1, 1, 1, 1, 1, 1, 1, 1, 1, 1, 1, 1, 1, 1, 1, 1, 1, 1, 1, 1, 1, 1, 1, 1, 1, 1, 1, 1, 1, 1, 1, 1, 1, 1, 1, 1, 1, 1, 1, 1, 1, 1, 1, 1, 1, 1, 1, 1, 1, 1, 1, 1, 1, 1, 1, 1, 1, 1, 1, 1, 4 ),
 ( -0.02000000000000000042, 1.020000000000000018 ),
 ( -0.02000000000000000042, -0.003749999999999999861, 0.01250000000000000069, 0.02875000000000000125, 0.04499999999999999833, 0.06124999999999999889, 0.07749999999999999944, 0.09375000000000000000, 0.1100000000000000006, 0.1262500000000000011, 0.1424999999999999878, 0.1587500000000000022, 0.1749999999999999889, 0.1912500000000000033, 0.2074999999999999900, 0.2237500000000000044, 0.2399999999999999911, 0.2562499999999999778, 0.2725000000000000200, 0.2887500000000000067, 0.3049999999999999933, 0.3212499999999999800, 0.3375000000000000222, 0.3537500000000000089, 0.3699999999999999956, 0.3862499999999999822, 0.4025000000000000244, 0.4187500000000000111, 0.4349999999999999978, 0.4512499999999999845, 0.4675000000000000266, 0.4837500000000000133, 0.5000000000000000000, 0.5162499999999999867, 0.5324999999999999734, 0.5487499999999999600, 0.5649999999999999467, 0.5812500000000000444, 0.5975000000000000311, 0.6137500000000000178, 0.6300000000000000044, 0.6462499999999999911, 0.6624999999999999778, 0.6787499999999999645, 0.6949999999999999512, 0.7112500000000000488, 0.7275000000000000355, 0.7437500000000000222, 0.7600000000000000089, 0.7762499999999999956, 0.7924999999999999822, 0.8087499999999999689, 0.8249999999999999556, 0.8412500000000000533, 0.8575000000000000400, 0.8737500000000000266, 0.8900000000000000133, 0.9062500000000000000, 0.9224999999999999867, 0.9387499999999999734, 0.9549999999999999600, 0.9712499999999999467, 0.9875000000000000444, 1.003749999999999920, 1.020000000000000018 ),
 .UNSPECIFIED. ) ;
#44033 = CARTESIAN_POINT ( 'NONE',  ( 8.962479719595000560, 2.546924812613000189, -6.918870225297999887 ) ) ;
#44034 = LINE ( 'NONE', #42392, #51557 ) ;
#44035 = CARTESIAN_POINT ( 'NONE',  ( 12.27369669298500021, 2.970039040581486045, -12.24495604130072124 ) ) ;
#44036 = CARTESIAN_POINT ( 'NONE',  ( 10.94635971519499940, -3.540377183549800133, 8.264615166761799969 ) ) ;
#44037 = CARTESIAN_POINT ( 'NONE',  ( 8.912651967921339846, -2.899999999999999911, 6.383937126463831824 ) ) ;
#44038 = CARTESIAN_POINT ( 'NONE',  ( 10.44601354018326944, 3.000416447002273834, -8.268183399968640046 ) ) ;
#44039 = ORIENTED_EDGE ( 'NONE', *, *, #9007, .T. ) ;
#44040 = CARTESIAN_POINT ( 'NONE',  ( 24.35365242081699932, 10.79182034090998776, 4.028979491970003934 ) ) ;
#44041 = CARTESIAN_POINT ( 'NONE',  ( 23.59999192078999997, 10.30759737717999869, 9.317725909430999209 ) ) ;
#44042 = VERTEX_POINT ( 'NONE', #17702 ) ;
#44043 = B_SPLINE_SURFACE_WITH_KNOTS ( 'NONE', 3, 3, ( 
 ( #28317, #22373, #38458, #43370 ),
 ( #65364, #5944, #44413, #43712 ),
 ( #27978, #65006, #59779, #49288 ),
 ( #33220, #43013, #58743, #1399 ),
 ( #27286, #32873, #54186, #59091 ),
 ( #26943, #48254, #54542, #64317 ),
 ( #37422, #44062, #48953, #17484 ),
 ( #23064, #38808, #6284, #48607 ),
 ( #16437, #21677, #60132, #711 ) ),
 .UNSPECIFIED., .F., .F., .F.,
 ( 4, 1, 1, 1, 1, 1, 4 ),
 ( 4, 4 ),
 ( 0.02288375853140000096, 0.1666666666667000196, 0.3333333333333000081, 0.5000000000000000000, 0.6666666666667000474, 0.8333333333333000637, 0.9485331614076999429 ),
 ( -0.1900389547208000129, 1.190219847277000031 ),
 .UNSPECIFIED. ) ;
#44044 = CARTESIAN_POINT ( 'NONE',  ( 12.65065493613389513, -3.183300664725537743, -12.19125106909030443 ) ) ;
#44045 = CARTESIAN_POINT ( 'NONE',  ( 11.50687348028854906, 2.996540789803000315, 6.957450711802899868 ) ) ;
#44046 = CARTESIAN_POINT ( 'NONE',  ( 9.900941392955999731, -4.883847137081999357, -9.070879136699002032 ) ) ;
#44047 = CARTESIAN_POINT ( 'NONE',  ( 10.95282897429000002, 2.845676247909999734, -5.175250098289999379 ) ) ;
#44048 = CARTESIAN_POINT ( 'NONE',  ( 17.56118420217200082, -11.55273616383000146, 4.939615522132000613 ) ) ;
#44049 = DIRECTION ( 'NONE',  ( 1.000000000000000000, 0.000000000000000000, 0.000000000000000000 ) ) ;
#44050 = CARTESIAN_POINT ( 'NONE',  ( 8.061933748689000367, 4.603465626214999773, -6.221450782568999749 ) ) ;
#44051 = CARTESIAN_POINT ( 'NONE',  ( 18.14024703743436717, -0.2197131112048710255, -12.69744725510432914 ) ) ;
#44052 = CARTESIAN_POINT ( 'NONE',  ( 12.18517285595358501, 2.419552247719690019, -12.46997200859132704 ) ) ;
#44053 = CARTESIAN_POINT ( 'NONE',  ( 11.47810404293059960, -4.563346034752700398, -8.647151967355000579 ) ) ;
#44054 = EDGE_CURVE ( 'NONE', #47396, #27357, #50798, .T. ) ;
#44056 = ADVANCED_FACE ( 'NONE', ( #44627 ), #18046, .T. ) ;
#44055 = CARTESIAN_POINT ( 'NONE',  ( 9.251926658770999623, 5.159258275969999197, 9.109498396691998678 ) ) ;
#44057 = ORIENTED_EDGE ( 'NONE', *, *, #15355, .F. ) ;
#44058 = AXIS2_PLACEMENT_3D ( 'NONE', #43866, #1908, #65171 ) ;
#44059 = PRESENTATION_STYLE_ASSIGNMENT (( #12581 ) ) ;
#44060 = CYLINDRICAL_SURFACE ( 'NONE', #52562, 0.4999999999999998335 ) ;
#44061 = CARTESIAN_POINT ( 'NONE',  ( 7.303793052280064479, 3.233246055057100943, 6.357929222382162848 ) ) ;
#44062 = CARTESIAN_POINT ( 'NONE',  ( 11.74257329013500240, 12.32813410531000109, 1.877195977750000022 ) ) ;
#44063 = B_SPLINE_CURVE_WITH_KNOTS ( 'NONE', 3,
 ( #47767, #10689, #31340, #4406 ),
 .UNSPECIFIED., .F., .F.,
 ( 4, 4 ),
 ( 0.000000000000000000, 1.000000000000000000 ),
 .UNSPECIFIED. ) ;
#44064 = CONICAL_SURFACE ( 'NONE', #25076, 13.94999927503000059, 0.7853981058017837080 ) ;
#44065 = CARTESIAN_POINT ( 'NONE',  ( 18.05281416665457428, 3.003450933888335950, 12.23680105844127475 ) ) ;
#44066 = CARTESIAN_POINT ( 'NONE',  ( 11.12440625316000009, 5.543025011711000261, 5.163735498011999603 ) ) ;
#44067 = CARTESIAN_POINT ( 'NONE',  ( 11.10328610135029948, 3.121939224269600022, -7.825000000000000178 ) ) ;
#44068 = CARTESIAN_POINT ( 'NONE',  ( 9.980191603681628720, -3.849750744317739670, 8.361949783971203587 ) ) ;
#44069 = CARTESIAN_POINT ( 'NONE',  ( 11.09999999999999964, -5.299524241844999928, -5.124965750789000296 ) ) ;
#44070 = ORIENTED_EDGE ( 'NONE', *, *, #36387, .F. ) ;
#44071 = CARTESIAN_POINT ( 'NONE',  ( 12.47064909367912477, -3.118799700203786607, 12.20791227269315371 ) ) ;
#44072 = CARTESIAN_POINT ( 'NONE',  ( 9.049126402770998112, -2.931626221533000010, -7.097120470443400109 ) ) ;
#44073 = CARTESIAN_POINT ( 'NONE',  ( 24.56500367226799852, -3.482495402162000264, -12.16326672459999791 ) ) ;
#44074 = EDGE_CURVE ( 'NONE', #6099, #46556, #20436, .T. ) ;
#44076 = AXIS2_PLACEMENT_3D ( 'NONE', #55373, #27421, #7468 ) ;
#44075 = B_SPLINE_CURVE_WITH_KNOTS ( 'NONE', 3,
 ( #30321, #8642, #12863, #34877, #56196, #55511, #39777, #35226, #8304, #66677, #34543, #19127, #61097, #46393 ),
 .UNSPECIFIED., .F., .F.,
 ( 4, 2, 2, 1, 1, 2, 2, 4 ),
 ( 0.000000000000000000, 0.2500000000001028067, 0.3750000000001583178, 0.4375000000001811329, 0.4687500000001925127, 0.4843750000001808553, 0.5000000000001691980, 1.000000000000000000 ),
 .UNSPECIFIED. ) ;
#44077 = CARTESIAN_POINT ( 'NONE',  ( 4.149992563292000725, 2.000000000000000000, 0.000000000000000000 ) ) ;
#44078 = EDGE_CURVE ( 'NONE', #57550, #41936, #1928, .T. ) ;
#44079 = CARTESIAN_POINT ( 'NONE',  ( 10.23103300763299828, 4.692441239783899931, -8.226274395107198600 ) ) ;
#44080 = CARTESIAN_POINT ( 'NONE',  ( 12.50535913667519949, -0.6550687562476263937, 12.58296113213902068 ) ) ;
#44081 = CARTESIAN_POINT ( 'NONE',  ( 9.497295280408998508, 3.734279507827999556, 8.942126004519000304 ) ) ;
#44082 = DIRECTION ( 'NONE',  ( -0.5000000000000150990, -0.08222066253632250021, 0.8621135439442261239 ) ) ;
#44083 = CARTESIAN_POINT ( 'NONE',  ( 12.58288255545463130, 3.084271795211692258, 12.29604036100131914 ) ) ;
#44084 = ORIENTED_EDGE ( 'NONE', *, *, #8223, .F. ) ;
#44085 = CARTESIAN_POINT ( 'NONE',  ( 8.047385841228999581, 4.468366666325000125, 8.882140983065999862 ) ) ;
#44086 = CARTESIAN_POINT ( 'NONE',  ( 11.06379841651039797, 3.598362324325699912, -8.567697191971999970 ) ) ;
#44087 = B_SPLINE_CURVE_WITH_KNOTS ( 'NONE', 3,
 ( #58162, #31598, #5364, #117 ),
 .UNSPECIFIED., .F., .F.,
 ( 4, 4 ),
 ( 0.000000000000000000, 1.000000000000000000 ),
 .UNSPECIFIED. ) ;
#44088 = CARTESIAN_POINT ( 'NONE',  ( 9.643927823787143083, -2.750011555256801188, 7.500000155056757656 ) ) ;
#44090 = CARTESIAN_POINT ( 'NONE',  ( 24.76117192814322365, 11.73046401989726029, 3.191744692855882359 ) ) ;
#44089 = CARTESIAN_POINT ( 'NONE',  ( 12.48079089729741398, 10.80976533105202542, -4.345114765769909404 ) ) ;
#44091 = CARTESIAN_POINT ( 'NONE',  ( 11.81056516821459823, -3.390321848206700128, -8.115298063151199059 ) ) ;
#44092 = CARTESIAN_POINT ( 'NONE',  ( 11.00009108335970609, 5.118893581675404647, 7.402342568044064208 ) ) ;
#44093 = VERTEX_POINT ( 'NONE', #31284 ) ;
#44094 = VECTOR ( 'NONE', #39357, 1000.000000000000000 ) ;
#44095 = CARTESIAN_POINT ( 'NONE',  ( 1.114745999307000135, -3.300563260077000294, -0.9171157435373999967 ) ) ;
#44096 = CARTESIAN_POINT ( 'NONE',  ( 6.778816671981999775, -0.8882170986559999593, 0.6661914818925001036 ) ) ;
#44097 =( GEOMETRIC_REPRESENTATION_CONTEXT ( 3 ) GLOBAL_UNCERTAINTY_ASSIGNED_CONTEXT ( ( #19923 ) ) GLOBAL_UNIT_ASSIGNED_CONTEXT ( ( #46116, #19546, #30723 ) ) REPRESENTATION_CONTEXT ( 'NONE', 'WORKASPACE' ) );
#44098 = CARTESIAN_POINT ( 'NONE',  ( 12.79999999914999975, -12.11987927271999865, 3.159802730921999814 ) ) ;
#44099 = DIRECTION ( 'NONE',  ( 0.000000000000000000, 1.000000000000000000, 0.000000000000000000 ) ) ;
#44100 = CARTESIAN_POINT ( 'NONE',  ( 11.11486084871780022, -2.792989229543000107, -7.174999999999999822 ) ) ;
#44101 = CARTESIAN_POINT ( 'NONE',  ( 12.78089888617687109, -1.787816964400932296, 13.88537754411822078 ) ) ;
#44102 = CARTESIAN_POINT ( 'NONE',  ( 10.98417233644999946, 2.893962206862000119, 4.881461471176000266 ) ) ;
#44103 = CARTESIAN_POINT ( 'NONE',  ( 9.022188178962251115, -4.591134893453497234, -8.523911321890818016 ) ) ;
#44104 = CARTESIAN_POINT ( 'NONE',  ( 13.24816728597000193, -12.42904273309000018, -1.833878933190999927 ) ) ;
#44105 = ORIENTED_EDGE ( 'NONE', *, *, #43411, .F. ) ;
#44106 = CARTESIAN_POINT ( 'NONE',  ( 7.604583333330377393, 5.349999999999999645, -7.323285413235573138 ) ) ;
#44107 = CARTESIAN_POINT ( 'NONE',  ( 9.564884880418375701, 5.349923162331274185, -7.500006638304977713 ) ) ;
#44108 = CARTESIAN_POINT ( 'NONE',  ( 18.18005044212792143, 2.500000099754956739, -13.67345740034994250 ) ) ;
#44109 = CARTESIAN_POINT ( 'NONE',  ( 10.51835931249053324, 5.126777126165764642, -6.752018918838221140 ) ) ;
#44110 = CARTESIAN_POINT ( 'NONE',  ( 1.705112477863000020, -2.304706330186000240, 2.969293668968000066 ) ) ;
#44111 = B_SPLINE_CURVE_WITH_KNOTS ( 'NONE', 3,
 ( #4831, #32796, #38027, #47848 ),
 .UNSPECIFIED., .F., .F.,
 ( 4, 4 ),
 ( 0.000000000000000000, 1.000000000000000000 ),
 .UNSPECIFIED. ) ;
#44112 = LINE ( 'NONE', #39899, #5363 ) ;
#44113 = DIRECTION ( 'NONE',  ( 1.000000000000000000, 0.000000000000000000, 0.000000000000000000 ) ) ;
#44114 = CARTESIAN_POINT ( 'NONE',  ( 9.514114512910998300, 4.887632373702999189, 8.462748516415999234 ) ) ;
#44115 = AXIS2_PLACEMENT_3D ( 'NONE', #65907, #59634, #33420 ) ;
#44116 = CARTESIAN_POINT ( 'NONE',  ( 11.76133460557259980, 4.139849081322200419, 6.645166161828299778 ) ) ;
#44117 = EDGE_CURVE ( 'NONE', #57932, #22650, #35757, .T. ) ;
#44118 = EDGE_CURVE ( 'NONE', #68740, #34308, #62490, .T. ) ;
#44119 = LINE ( 'NONE', #64715, #4412 ) ;
#44120 = CARTESIAN_POINT ( 'NONE',  ( 10.82674314678999927, -3.167157901876000103, -6.225148200207000215 ) ) ;
#44121 = CARTESIAN_POINT ( 'NONE',  ( 11.53142628873784226, 3.735369189129102097, -11.95516350776760106 ) ) ;
#44122 = CARTESIAN_POINT ( 'NONE',  ( 12.80000000000000071, -10.78295181803999903, 4.410266442048000002 ) ) ;
#44123 = CARTESIAN_POINT ( 'NONE',  ( 12.28979759249027204, -2.853877291415200634, 12.36206589978998593 ) ) ;
#44124 = VERTEX_POINT ( 'NONE', #9247 ) ;
#44125 = CARTESIAN_POINT ( 'NONE',  ( 8.795585841232000490, 5.251032986819000214, -6.070151079272999795 ) ) ;
#44126 = ORIENTED_EDGE ( 'NONE', *, *, #20011, .T. ) ;
#44127 = CARTESIAN_POINT ( 'NONE',  ( 17.75779383521795296, -3.091556742956585779, 13.53003950643004671 ) ) ;
#44128 = CARTESIAN_POINT ( 'NONE',  ( 11.10887482311539998, -2.815046254222000055, -7.978749413531599721 ) ) ;
#44129 = ORIENTED_EDGE ( 'NONE', *, *, #6464, .T. ) ;
#44130 = CARTESIAN_POINT ( 'NONE',  ( 11.10612378248509913, 3.517039242046199998, 8.413720204863100349 ) ) ;
#44131 = CARTESIAN_POINT ( 'NONE',  ( 6.116137458369862223, 1.019062767528970737, 0.4963261465187597254 ) ) ;
#44132 = CARTESIAN_POINT ( 'NONE',  ( 23.80818434440886833, 3.306688368710591241, -13.11409483359108208 ) ) ;
#44133 = CARTESIAN_POINT ( 'NONE',  ( 11.20904666305999875, 5.937823941418000295, 7.147334722859000067 ) ) ;
#44134 = CARTESIAN_POINT ( 'NONE',  ( 24.30001694391200218, -12.21047201246000036, 3.271805662802000025 ) ) ;
#44135 = CARTESIAN_POINT ( 'NONE',  ( 9.664763540182335078, -2.782534154164604256, -7.172815144550905408 ) ) ;
#44136 = CARTESIAN_POINT ( 'NONE',  ( 17.91761838490639036, 0.6233258800551639833, -12.58457734799054784 ) ) ;
#44137 = CARTESIAN_POINT ( 'NONE',  ( 9.843620110012999191, -5.021680390140000227, -8.761463725090999688 ) ) ;
#44138 = CARTESIAN_POINT ( 'NONE',  ( 11.08380555355736163, 3.999999927305438963, -9.033895164528459532 ) ) ;
#44139 = VERTEX_POINT ( 'NONE', #40386 ) ;
#44140 = ADVANCED_FACE ( 'NONE', ( #67632, #14516 ), #41421, .T. ) ;
#44142 = EDGE_CURVE ( 'NONE', #9965, #57932, #40830, .T. ) ;
#44141 = CARTESIAN_POINT ( 'NONE',  ( 10.61675993195453849, -2.980798815563405757, -5.036430362955847784 ) ) ;
#44143 = ORIENTED_EDGE ( 'NONE', *, *, #26997, .F. ) ;
#44144 = FACE_OUTER_BOUND ( 'NONE', #68955, .T. ) ;
#44145 = SURFACE_SIDE_STYLE ('',( #44833 ) ) ;
#44146 = EDGE_CURVE ( 'NONE', #6099, #27955, #59149, .T. ) ;
#44147 = ORIENTED_EDGE ( 'NONE', *, *, #66482, .F. ) ;
#44148 = CARTESIAN_POINT ( 'NONE',  ( 10.90000000000000036, 2.778483479159999714, -6.925197956411000000 ) ) ;
#44149 = CARTESIAN_POINT ( 'NONE',  ( 11.05166408303000125, -5.150113226472000427, 5.124970633734999836 ) ) ;
#44150 = CARTESIAN_POINT ( 'NONE',  ( 10.72299000889467635, 3.772656371820692911, 6.655959434011009535 ) ) ;
#44151 = DIRECTION ( 'NONE',  ( 0.000000000000000000, 1.000000000000000000, 0.000000000000000000 ) ) ;
#44152 = CARTESIAN_POINT ( 'NONE',  ( 12.76358260308698611, 1.876037923228466298, 13.78611687077048842 ) ) ;
#44153 = CARTESIAN_POINT ( 'NONE',  ( 9.388626433405999450, -4.079401915682999480, 9.259353168384000909 ) ) ;
#44154 = CARTESIAN_POINT ( 'NONE',  ( 7.850354840490529895, 2.911893064861816427, -6.650750720717241826 ) ) ;
#44155 = CARTESIAN_POINT ( 'NONE',  ( 12.44165070291072439, 0.6323113780857038124, 13.98571806661952976 ) ) ;
#44156 = ORIENTED_EDGE ( 'NONE', *, *, #12756, .F. ) ;
#44157 = CARTESIAN_POINT ( 'NONE',  ( 12.78455560662700208, 11.44263450739000021, -4.698119303721000506 ) ) ;
#44158 = CARTESIAN_POINT ( 'NONE',  ( 9.251496707488000126, -3.918323994020610268, 6.643597378104299622 ) ) ;
#44159 = CARTESIAN_POINT ( 'NONE',  ( 8.757986382567201744, 4.151567127026601689, 6.650284907739020035 ) ) ;
#44160 = CARTESIAN_POINT ( 'NONE',  ( 5.117342238861000148, 0.2443688909792999520, 1.311937767346999850 ) ) ;
#44161 = EDGE_CURVE ( 'NONE', #68087, #63300, #62253, .T. ) ;
#44162 = CARTESIAN_POINT ( 'NONE',  ( 9.684729719592999331, 2.370176859044999862, -6.912649125838000508 ) ) ;
#44163 = CIRCLE ( 'NONE', #16241, 2.400000066501999818 ) ;
#44164 = CARTESIAN_POINT ( 'NONE',  ( 9.916846873516377059, 3.231816600031355069, -8.499583552997725278 ) ) ;
#44165 = CARTESIAN_POINT ( 'NONE',  ( 10.04002603384999937, -2.348908096685999869, -7.136751747961000092 ) ) ;
#44166 = CARTESIAN_POINT ( 'NONE',  ( 17.55505043854144276, -0.6250000000000001110, 13.88107975066923316 ) ) ;
#44167 = CYLINDRICAL_SURFACE ( 'NONE', #45994, 0.5000000000000004441 ) ;
#44168 = DIRECTION ( 'NONE',  ( -6.753599194678000463E-10, -6.753597969543999501E-10, -1.000000000000000000 ) ) ;
#44169 = CARTESIAN_POINT ( 'NONE',  ( 8.615663457454523666, -2.873897790767480753, -6.750856197900089839 ) ) ;
#44170 = CARTESIAN_POINT ( 'NONE',  ( 8.566291307401062483, -2.988918445095709142, 6.176011962928662946 ) ) ;
#44171 = DIRECTION ( 'NONE',  ( 1.000000000000000000, 0.000000000000000000, 0.000000000000000000 ) ) ;
#44172 = CARTESIAN_POINT ( 'NONE',  ( 10.44125056272499918, 5.033400911533000510, -7.515315513715298934 ) ) ;
#44173 = CARTESIAN_POINT ( 'NONE',  ( 9.406696787962999906, 4.172481380750499902, -6.510508982544899403 ) ) ;
#44175 = CARTESIAN_POINT ( 'NONE',  ( 10.95339184458999959, -2.662495063361999925, 4.888666547750000646 ) ) ;
#44174 = CARTESIAN_POINT ( 'NONE',  ( 9.925038493598998812, -3.372531419565699906, 8.098323595618600379 ) ) ;
#44176 = CARTESIAN_POINT ( 'NONE',  ( 7.682778389973002220, -3.526905737521000006, 6.475916620580998817 ) ) ;
#44177 = ORIENTED_EDGE ( 'NONE', *, *, #1880, .F. ) ;
#44178 = CARTESIAN_POINT ( 'NONE',  ( 10.73213259636989925, 3.092475607087700418, 7.005495010505599751 ) ) ;
#44179 = CARTESIAN_POINT ( 'NONE',  ( 10.58844302970999962, -3.754658547780000521, 5.545362468768000319 ) ) ;
#44180 = CARTESIAN_POINT ( 'NONE',  ( 10.41690035061499842, 4.304339077956200299, 6.399494776650000105 ) ) ;
#44181 = CARTESIAN_POINT ( 'NONE',  ( 10.88351354018293904, -5.249999999999998224, -7.336375382625530683 ) ) ;
#44182 = CARTESIAN_POINT ( 'NONE',  ( 11.18051369187999988, -5.340070732632000272, 8.416150632189001612 ) ) ;
#44183 = CARTESIAN_POINT ( 'NONE',  ( 9.743004321115734001, -5.518491777742534410, 8.419011746474035718 ) ) ;
#44185 = CARTESIAN_POINT ( 'NONE',  ( 11.48828127163000268, 3.524947629324000076, -11.86450458095000116 ) ) ;
#44184 = PRODUCT_DEFINITION_CONTEXT ( 'detailed design', #49409, 'design' ) ;
#44186 = ORIENTED_EDGE ( 'NONE', *, *, #6524, .T. ) ;
#44187 = VECTOR ( 'NONE', #27012, 1000.000000000000114 ) ;
#44188 = CARTESIAN_POINT ( 'NONE',  ( 9.178734463322998138, -3.895375416816699854, -8.498947444525299488 ) ) ;
#44189 = CARTESIAN_POINT ( 'NONE',  ( 11.30000285318000230, -11.76356368987999979, -1.428410073821000159 ) ) ;
#44190 = CARTESIAN_POINT ( 'NONE',  ( 5.116892472961001026, -1.574491786429000006, -0.3581626104627999574 ) ) ;
#44191 = B_SPLINE_SURFACE_WITH_KNOTS ( 'NONE', 3, 3, ( 
 ( #580, #49155, #11400, #26463, #21889, #53375, #54055, #64529, #16648, #37974, #21547, #58611, #32737, #15961, #1267, #926, #47795, #22583, #48126, #21206, #42539, #22238, #64876, #69103, #10712, #16988, #13495, #40065, #18733, #23286, #34816, #28893, #28186, #44964, #55791 ),
 ( #12104, #44628, #61377, #18047, #55099, #7541, #7895, #17703, #49852, #39364, #59994, #8237, #65230, #29232, #50203, #44279, #23972, #24315, #65920, #56128, #12448, #50543, #33434, #60684, #17343, #54750, #12801, #34129, #23624, #29584, #50887, #2304, #2982, #66268, #39027 ),
 ( #39715, #18390, #38672, #2643, #6849, #1962, #49501, #1613, #55446, #61033, #22929, #65579, #60342, #33783, #13152, #45306, #7205, #34480, #28541, #66613, #41765, #3658, #35499, #20438, #9248, #14172, #56820, #9594, #8920, #67290, #29923, #9949, #45980, #62057, #15194 ),
 ( #31286, #14517, #19408, #30257, #56473, #8575, #20097, #3326, #14854, #4689, #30938, #57152, #41423, #36517, #52594, #25682, #35834, #57842, #24996, #57488, #52254, #63068, #51561, #24658, #51229, #30590, #46676, #4350, #67980, #36176, #40733, #62398, #46331, #47015, #45649 ) ),
 .UNSPECIFIED., .F., .F., .F.,
 ( 4, 4 ),
 ( 4, 1, 1, 1, 1, 1, 1, 1, 1, 1, 1, 1, 1, 1, 1, 1, 1, 1, 1, 1, 1, 1, 1, 1, 1, 1, 1, 1, 1, 1, 1, 1, 4 ),
 ( -0.1039370721279000015, 1.103937072127999963 ),
 ( -0.01999999999998999800, 0.01250000000001000137, 0.04500000000000999728, 0.07750000000001000533, 0.1100000000000000006, 0.1424999999999999878, 0.1749999999999999889, 0.2074999999999999900, 0.2399999999999999911, 0.2725000000000000200, 0.3049999999999999933, 0.3375000000000000222, 0.3699999999999999956, 0.4025000000000000244, 0.4349999999999999978, 0.4675000000000000266, 0.5000000000000000000, 0.5324999999999999734, 0.5649999999999999467, 0.5975000000000000311, 0.6300000000000000044, 0.6624999999999999778, 0.6949999999999999512, 0.7275000000000000355, 0.7600000000000000089, 0.7924999999999000622, 0.8249999999999000355, 0.8574999999999000089, 0.8899999999999000933, 0.9224999999999000666, 0.9549999999999000400, 0.9874999999999000133, 1.020000000000000018 ),
 .UNSPECIFIED. ) ;
#44192 = CARTESIAN_POINT ( 'NONE',  ( 7.000000000000000000, 10.32086050633190766, -4.256250858473547893 ) ) ;
#44193 = VECTOR ( 'NONE', #22400, 1000.000000000000227 ) ;
#44194 = CARTESIAN_POINT ( 'NONE',  ( 11.49999672495000169, 3.632761979779000061, -11.06912554803999882 ) ) ;
#44195 = EDGE_CURVE ( 'NONE', #14147, #18158, #44932, .T. ) ;
#44196 = EDGE_CURVE ( 'NONE', #6623, #41725, #4915, .T. ) ;
#44197 = CARTESIAN_POINT ( 'NONE',  ( 9.406851002546000373, 2.832432432432000269, -6.822293592207000934 ) ) ;
#44198 = CARTESIAN_POINT ( 'NONE',  ( 11.04333729122639873, 2.996877626170000308, -7.473611442402849470 ) ) ;
#44199 = CARTESIAN_POINT ( 'NONE',  ( 7.768029367744567537, -2.842467755650244232, 6.805004515721170044 ) ) ;
#44200 = CARTESIAN_POINT ( 'NONE',  ( 24.48514019804499853, -8.805442486866001062, 8.922418878371999540 ) ) ;
#44201 = CARTESIAN_POINT ( 'NONE',  ( 8.253230575588421658, -2.714951384259771228, 7.027308161653141205 ) ) ;
#44202 = VERTEX_POINT ( 'NONE', #64104 ) ;
#44203 = CARTESIAN_POINT ( 'NONE',  ( 25.60000000000000142, 8.527654132752997995, -7.260537518969999660 ) ) ;
#44204 = CARTESIAN_POINT ( 'NONE',  ( 12.54683519492311738, 0.5695321295966281339, -13.88429381145914299 ) ) ;
#44205 = DIRECTION ( 'NONE',  ( -1.000000000000000000, 0.000000000000000000, 0.000000000000000000 ) ) ;
#44206 = CARTESIAN_POINT ( 'NONE',  ( 2.327754220767750404, -2.003492624900453212, -2.889646723249190696 ) ) ;
#44207 = CARTESIAN_POINT ( 'NONE',  ( 13.67905361531531838, -11.43958844919984585, -2.204572756906674424 ) ) ;
#44208 = CARTESIAN_POINT ( 'NONE',  ( 21.10000109091659937, 0.000000000000000000, 0.000000000000000000 ) ) ;
#44209 = CARTESIAN_POINT ( 'NONE',  ( 13.55168611684300117, 12.14221570691000096, 2.415203473206000151 ) ) ;
#44210 = VERTEX_POINT ( 'NONE', #20781 ) ;
#44211 = VECTOR ( 'NONE', #38226, 1000.000000000000114 ) ;
#44212 = CARTESIAN_POINT ( 'NONE',  ( 23.60205915885299888, 9.377218989177011466, 8.305825996807000067 ) ) ;
#44213 = CARTESIAN_POINT ( 'NONE',  ( 17.80571586434983544, 1.927376100771097223, -13.77836213227538131 ) ) ;
#44214 = VERTEX_POINT ( 'NONE', #21804 ) ;
#44215 = CARTESIAN_POINT ( 'NONE',  ( 7.307500000000000107, 0.2999999999999999889, 3.149999999999999911 ) ) ;
#44216 = CARTESIAN_POINT ( 'NONE',  ( 18.20279897513206180, 3.027817981728711860, 11.45825916391118859 ) ) ;
#44217 = CIRCLE ( 'NONE', #14064, 1.500000000000001110 ) ;
#44218 = FACE_OUTER_BOUND ( 'NONE', #65996, .T. ) ;
#44219 = CARTESIAN_POINT ( 'NONE',  ( 13.99999999347100044, -9.187456302440001110, -8.213201953411001455 ) ) ;
#44220 = CARTESIAN_POINT ( 'NONE',  ( 10.52799293566599914, -3.193321847920899792, -8.489570425681801424 ) ) ;
#44221 = CARTESIAN_POINT ( 'NONE',  ( 18.01482197226484416, 0.4234835433089234047, -12.69049809664633166 ) ) ;
#44222 = CARTESIAN_POINT ( 'NONE',  ( 9.020964430773000586, -2.907392932634000005, 6.146188468825999784 ) ) ;
#44223 = VERTEX_POINT ( 'NONE', #53287 ) ;
#44224 = CARTESIAN_POINT ( 'NONE',  ( 8.299720885770000223, 3.399999999999999911, -6.084164326786999588 ) ) ;
#44225 = B_SPLINE_CURVE_WITH_KNOTS ( 'NONE', 3,
 ( #18615, #8466, #40283, #52133 ),
 .UNSPECIFIED., .F., .F.,
 ( 4, 4 ),
 ( 0.000000000000000000, 1.000000000000000000 ),
 .UNSPECIFIED. ) ;
#44226 = B_SPLINE_CURVE_WITH_KNOTS ( 'NONE', 3,
 ( #65049, #32572, #53884, #38857 ),
 .UNSPECIFIED., .F., .F.,
 ( 4, 4 ),
 ( 0.000000000000000000, 0.1254233535197428473 ),
 .UNSPECIFIED. ) ;
#44227 = CARTESIAN_POINT ( 'NONE',  ( 18.16776742079022000, -2.623333169985007096, -13.64647547701515506 ) ) ;
#44228 = CARTESIAN_POINT ( 'NONE',  ( 18.05387017988397957, -2.121311586850259001, 13.74657283405556285 ) ) ;
#44229 = VERTEX_POINT ( 'NONE', #36870 ) ;
#44230 = CARTESIAN_POINT ( 'NONE',  ( 10.44806481732999792, 3.684980864017000091, -6.173120265414000052 ) ) ;
#44231 = DIRECTION ( 'NONE',  ( 0.000000000000000000, 0.000000000000000000, -1.000000000000000000 ) ) ;
#44232 = EDGE_CURVE ( 'NONE', #37319, #24248, #61166, .T. ) ;
#44233 = ORIENTED_EDGE ( 'NONE', *, *, #64871, .T. ) ;
#44234 = CARTESIAN_POINT ( 'NONE',  ( 9.862621437244998290, 4.667147537636399335, 8.250837174995698575 ) ) ;
#44235 = CARTESIAN_POINT ( 'NONE',  ( 17.92067275948981475, -3.101661042832208004, -12.21227817455808129 ) ) ;
#44236 = CARTESIAN_POINT ( 'NONE',  ( 8.266851002545999805, 2.832432432432000269, 6.822293592207000934 ) ) ;
#44237 = CARTESIAN_POINT ( 'NONE',  ( 16.07057712374000147, 3.541973289920000045, 11.85942491664999920 ) ) ;
#44238 = CARTESIAN_POINT ( 'NONE',  ( 23.56666365135700403, 2.963314674624001999, 12.23574966054999358 ) ) ;
#44239 = CARTESIAN_POINT ( 'NONE',  ( 9.611342523874998989, 3.142972170141900001, 7.631191628371899682 ) ) ;
#44240 = CARTESIAN_POINT ( 'NONE',  ( 4.700001368028300597, -14.00000000000000000, 0.000000000000000000 ) ) ;
#44241 = ORIENTED_EDGE ( 'NONE', *, *, #25050, .T. ) ;
#44242 = FACE_OUTER_BOUND ( 'NONE', #25180, .T. ) ;
#44243 = CARTESIAN_POINT ( 'NONE',  ( 10.71315778041000044, 2.619207518211999819, -8.142085279690999045 ) ) ;
#44244 = CARTESIAN_POINT ( 'NONE',  ( 18.14395184984607567, -12.07230981080912890, 3.337076190873973225 ) ) ;
#44245 = CARTESIAN_POINT ( 'NONE',  ( 12.27362767355643136, 2.829117748835542123, -13.59812893905842479 ) ) ;
#44246 = CARTESIAN_POINT ( 'NONE',  ( 9.836342523874998633, -5.264483068122999931, -7.306436165809000016 ) ) ;
#44247 = CARTESIAN_POINT ( 'NONE',  ( 24.56665315110400272, 3.304344730019999954, 12.00442456974999850 ) ) ;
#44248 = EDGE_CURVE ( 'NONE', #51109, #46470, #9796, .T. ) ;
#44249 = CARTESIAN_POINT ( 'NONE',  ( 17.93540541742265404, 0.4960449563116372529, 13.88808666890938248 ) ) ;
#44250 = AXIS2_PLACEMENT_3D ( 'NONE', #33111, #27515, #32763 ) ;
#44251 = CARTESIAN_POINT ( 'NONE',  ( 17.78593649203479643, 0.5808626952944924149, 13.88365973251299401 ) ) ;
#44252 = B_SPLINE_CURVE_WITH_KNOTS ( 'NONE', 3,
 ( #40817, #8326, #7286, #2050, #18129, #60770 ),
 .UNSPECIFIED., .F., .F.,
 ( 4, 2, 4 ),
 ( 0.000000000000000000, 0.5000000000000000000, 1.000000000000000000 ),
 .UNSPECIFIED. ) ;
#44253 = ORIENTED_EDGE ( 'NONE', *, *, #35615, .F. ) ;
#44254 = ORIENTED_EDGE ( 'NONE', *, *, #42389, .T. ) ;
#44255 = CARTESIAN_POINT ( 'NONE',  ( 8.748814158775001459, 5.251032986819000214, -6.070151079272999795 ) ) ;
#44256 = CARTESIAN_POINT ( 'NONE',  ( 12.23477845768578831, 0.2559490221015915390, 13.89683205629558316 ) ) ;
#44257 = CARTESIAN_POINT ( 'NONE',  ( 12.33489288317253418, -0.4118289862746280505, -13.89178842664826519 ) ) ;
#44258 = CARTESIAN_POINT ( 'NONE',  ( 9.509907746701999898, -5.077451867123000007, 8.469011304701000498 ) ) ;
#44259 = LINE ( 'NONE', #17678, #65170 ) ;
#44260 = CARTESIAN_POINT ( 'NONE',  ( 7.678995559621999867, -2.599231861044000169, 7.909347897884000389 ) ) ;
#44261 = CARTESIAN_POINT ( 'NONE',  ( 11.58810207955139937, -4.796537143354000499, 7.825000000000000178 ) ) ;
#44263 = CARTESIAN_POINT ( 'NONE',  ( 25.30000327618300204, -6.604245036507551141E-15, -11.49994408209238017 ) ) ;
#44262 = CARTESIAN_POINT ( 'NONE',  ( 10.56430484851600049, -2.836617618740000069, 6.968092280137199168 ) ) ;
#44264 = CARTESIAN_POINT ( 'NONE',  ( 10.07503300763299947, 4.881889043637199777, -8.424978748982498544 ) ) ;
#44265 = CIRCLE ( 'NONE', #4052, 3.200000000000000178 ) ;
#44266 = CARTESIAN_POINT ( 'NONE',  ( 11.09999999999999964, -4.000000000000000000, 7.500000000000000000 ) ) ;
#44267 = CARTESIAN_POINT ( 'NONE',  ( 8.741151519676998660, 4.018750234858180725, -8.366807394121199337 ) ) ;
#44268 = CARTESIAN_POINT ( 'NONE',  ( 18.10875687686965918, 0.2899325138666226653, 12.69554708236671914 ) ) ;
#44269 = FACE_OUTER_BOUND ( 'NONE', #24971, .T. ) ;
#44270 = CARTESIAN_POINT ( 'NONE',  ( 4.149992563291998948, -1.599290730647371594, 1.229060429538527011 ) ) ;
#44271 = VERTEX_POINT ( 'NONE', #11658 ) ;
#44273 = CARTESIAN_POINT ( 'NONE',  ( 9.897084615057014645, 5.285910559402416276, 7.026781793019058142 ) ) ;
#44272 = CARTESIAN_POINT ( 'NONE',  ( 10.89419229449708659, 5.254378413735692810, 6.992145683900290898 ) ) ;
#44274 = CARTESIAN_POINT ( 'NONE',  ( 9.749220280410998640, 5.656948148960999845, -6.994239053114000626 ) ) ;
#44275 = CARTESIAN_POINT ( 'NONE',  ( 12.64132288496830547, -1.896477787946246440, 13.78309086827115770 ) ) ;
#44276 = CARTESIAN_POINT ( 'NONE',  ( 7.070925607327942508, -0.1731109087963655924, -1.329073895981641495 ) ) ;
#44277 = CARTESIAN_POINT ( 'NONE',  ( 0.5516986677755000290, 3.485378829570000114, 1.246872170512999922 ) ) ;
#44278 = CARTESIAN_POINT ( 'NONE',  ( 8.849999778957998942, -4.000000000000000000, -7.500000000000000000 ) ) ;
#44279 = CARTESIAN_POINT ( 'NONE',  ( 2.690656551265000029, 2.202451855867999964, 2.837790456605000067 ) ) ;
#44280 = ORIENTED_EDGE ( 'NONE', *, *, #59386, .F. ) ;
#44281 = ADVANCED_FACE ( 'NONE', ( #58186 ), #25419, .F. ) ;
#44282 = EDGE_CURVE ( 'NONE', #63154, #17632, #10978, .T. ) ;
#44283 = CARTESIAN_POINT ( 'NONE',  ( 12.25981900110941325, -0.4746736627229765637, -12.59106879393900691 ) ) ;
#44284 = CARTESIAN_POINT ( 'NONE',  ( 6.950054030189999565, -13.87069231928999891, 4.225386915259999654 ) ) ;
#44285 = DIRECTION ( 'NONE',  ( -1.000000000000000000, 0.000000000000000000, 0.000000000000000000 ) ) ;
#44286 = CARTESIAN_POINT ( 'NONE',  ( 7.293864158771000028, 3.416213390569000197, 6.162512717529000206 ) ) ;
#44287 = ORIENTED_EDGE ( 'NONE', *, *, #27623, .F. ) ;
#44288 = CARTESIAN_POINT ( 'NONE',  ( 5.830830324679999954, 1.564645433990000001, 0.3990237390554000063 ) ) ;
#44289 = EDGE_CURVE ( 'NONE', #64753, #30347, #14091, .T. ) ;
#44290 = EDGE_CURVE ( 'NONE', #26079, #35697, #4035, .T. ) ;
#44291 = CARTESIAN_POINT ( 'NONE',  ( 10.92585229548211423, 9.545762865684249476, 6.039706820605043269 ) ) ;
#44293 = CARTESIAN_POINT ( 'NONE',  ( 23.56664678325900297, -13.31363270032999857, -4.296980171176000063 ) ) ;
#44292 = CARTESIAN_POINT ( 'NONE',  ( 8.581139754955028565, -4.140793541034012648, 5.766079433607869120 ) ) ;
#44294 = CARTESIAN_POINT ( 'NONE',  ( 11.05435090131019926, 5.119447121461000449, -8.192386390235398608 ) ) ;
#44295 = ORIENTED_EDGE ( 'NONE', *, *, #20131, .F. ) ;
#44296 = CYLINDRICAL_SURFACE ( 'NONE', #36665, 0.5000000000000000000 ) ;
#44297 = AXIS2_PLACEMENT_3D ( 'NONE', #65256, #16673, #951 ) ;
#44298 = CARTESIAN_POINT ( 'NONE',  ( 10.03687746070841058, 5.286620459901869573, -7.027007559937229253 ) ) ;
#44299 = EDGE_LOOP ( 'NONE', ( #24163, #14697, #23787, #61493, #33058 ) ) ;
#44300 = CARTESIAN_POINT ( 'NONE',  ( 0.09997256829956273350, 2.799974420760032334, 1.315025725132122498E-09 ) ) ;
#44301 = CARTESIAN_POINT ( 'NONE',  ( 24.91842629950604149, -8.566757067395633030, -8.413190967713612523 ) ) ;
#44302 = AXIS2_PLACEMENT_3D ( 'NONE', #11352, #22531, #43870 ) ;
#44303 = CARTESIAN_POINT ( 'NONE',  ( 17.98979471028674126, -0.4491394412341178088, -13.89023495843588840 ) ) ;
#44304 = VERTEX_POINT ( 'NONE', #60260 ) ;
#44305 = LINE ( 'NONE', #10737, #10734 ) ;
#44306 = DIRECTION ( 'NONE',  ( -0.7071067811865086039, -0.6115519423577077118, 0.3549707337212042457 ) ) ;
#44307 = CARTESIAN_POINT ( 'NONE',  ( 10.14601354018333090, -3.000416447002271170, 8.268183399968638270 ) ) ;
#44308 = CARTESIAN_POINT ( 'NONE',  ( 8.936672300099200328, -2.275486823213108245, 7.787304321185041012 ) ) ;
#44309 = CARTESIAN_POINT ( 'NONE',  ( 18.18005043799237086, -2.500000011518549670, 12.45159158845318359 ) ) ;
#44310 = ORIENTED_EDGE ( 'NONE', *, *, #39639, .F. ) ;
#44311 = CARTESIAN_POINT ( 'NONE',  ( 7.935739158771999868, 5.430400319332999715, 7.210801214872999410 ) ) ;
#44312 = CARTESIAN_POINT ( 'NONE',  ( 24.23232874665299974, -12.46722082417999999, -3.269194826637000340 ) ) ;
#44313 = CIRCLE ( 'NONE', #18603, 10.75000000000000533 ) ;
#44314 = CARTESIAN_POINT ( 'NONE',  ( 15.39284288850700122, -9.264553731144999915, -8.207894312349999666 ) ) ;
#44315 = ORIENTED_EDGE ( 'NONE', *, *, #53449, .F. ) ;
#44316 = DIRECTION ( 'NONE',  ( 0.000000000000000000, -1.000000000000000000, 0.000000000000000000 ) ) ;
#44317 = CARTESIAN_POINT ( 'NONE',  ( 16.10004050617000004, -4.849232186851411441, -11.59252887645439678 ) ) ;
#44318 = PLANE ( 'NONE',  #46047 ) ;
#44319 = CARTESIAN_POINT ( 'NONE',  ( 5.000030787342999439, 0.5496608443529871213, 2.045306479342561268 ) ) ;
#44320 = DIRECTION ( 'NONE',  ( 0.000000000000000000, 0.9905022095861402143, 0.1374968101629056305 ) ) ;
#44321 = CARTESIAN_POINT ( 'NONE',  ( 10.53521345716899837, 4.924890298941200228, 6.659120737011199331 ) ) ;
#44322 = CARTESIAN_POINT ( 'NONE',  ( 17.77721830936824077, -3.084271799839129358, 12.29605728393572228 ) ) ;
#44323 = ORIENTED_EDGE ( 'NONE', *, *, #48657, .T. ) ;
#44324 = CARTESIAN_POINT ( 'NONE',  ( 10.72191429142990060, -3.974927396630719922, -6.183971186511000084 ) ) ;
#44325 = VERTEX_POINT ( 'NONE', #66184 ) ;
#44326 = CARTESIAN_POINT ( 'NONE',  ( 11.64585080655600002, -12.33238363550000116, -1.848877788567000024 ) ) ;
#44327 = CARTESIAN_POINT ( 'NONE',  ( 9.395239158775000377, 5.045571591548999812, -9.086294919530001124 ) ) ;
#44328 = CARTESIAN_POINT ( 'NONE',  ( 3.383414956651999983, 2.956519816798000022, 1.636834048316999857 ) ) ;
#44329 = CARTESIAN_POINT ( 'NONE',  ( 10.93146935944000120, -2.472881306517999978, -7.514158774805000718 ) ) ;
#44330 = EDGE_CURVE ( 'NONE', #53410, #26903, #32123, .T. ) ;
#44331 = CARTESIAN_POINT ( 'NONE',  ( 3.500000000000000000, 1.140396268832999827, -3.309002319436000317 ) ) ;
#44332 = DIRECTION ( 'NONE',  ( 0.9999999999999967804, 7.921521013571943306E-08, -3.389355116421979744E-10 ) ) ;
#44333 = LINE ( 'NONE', #38377, #4294 ) ;
#44334 = ORIENTED_EDGE ( 'NONE', *, *, #39328, .T. ) ;
#44335 = EDGE_CURVE ( 'NONE', #866, #67604, #54949, .T. ) ;
#44336 = DIRECTION ( 'NONE',  ( -1.000000000000000000, 3.552713679026999935E-14, -3.552713679026999935E-14 ) ) ;
#44337 = CARTESIAN_POINT ( 'NONE',  ( 10.80903300763299946, -3.402282662142699809, 6.873077781830399857 ) ) ;
#44338 = CARTESIAN_POINT ( 'NONE',  ( 9.939321360490000146, 2.638097915594000309, 6.328629954376999933 ) ) ;
#44339 = DIRECTION ( 'NONE',  ( 0.000000000000000000, 1.000000000000000000, 0.000000000000000000 ) ) ;
#44340 = CARTESIAN_POINT ( 'NONE',  ( 10.42363156114900136, 3.315688435009791935, -8.575598637068461372 ) ) ;
#44341 = B_SPLINE_CURVE_WITH_KNOTS ( 'NONE', 3,
 ( #49118, #28501, #34089, #44926 ),
 .UNSPECIFIED., .F., .F.,
 ( 4, 4 ),
 ( 0.000000000000000000, 1.000000000000000000 ),
 .UNSPECIFIED. ) ;
#44342 = CARTESIAN_POINT ( 'NONE',  ( 9.208681878221188555, 2.678902866167812924, 7.777850098883442698 ) ) ;
#44343 = CARTESIAN_POINT ( 'NONE',  ( 11.26487482311540056, 4.930401445321599851, -7.875904247640098887 ) ) ;
#44344 = CARTESIAN_POINT ( 'NONE',  ( 7.100000000000176392, 3.045734354883735229, -8.506847764030522896 ) ) ;
#44345 = CARTESIAN_POINT ( 'NONE',  ( 10.23959632033899858, 2.942832934044000037, -7.068569539041399175 ) ) ;
#44346 = CARTESIAN_POINT ( 'NONE',  ( 7.100000000000000533, -2.649999999999999911, 7.500000000000000000 ) ) ;
#44347 = CARTESIAN_POINT ( 'NONE',  ( 23.61266196672000106, -10.15867583602999957, 9.482229976157999118 ) ) ;
#44348 = DIRECTION ( 'NONE',  ( 0.000000000000000000, -0.001239076634196937133, 0.9999992323442525866 ) ) ;
#44349 = ORIENTED_EDGE ( 'NONE', *, *, #16472, .F. ) ;
#44350 = CARTESIAN_POINT ( 'NONE',  ( 8.309480646794000336, -2.905864338704999827, 8.940687151810998046 ) ) ;
#44351 = CARTESIAN_POINT ( 'NONE',  ( 9.974327024990000012, -5.476443305113000370, -7.051545409824000465 ) ) ;
#44352 = CARTESIAN_POINT ( 'NONE',  ( 18.20725128760094691, 2.198916822427670947, 13.82623906782133005 ) ) ;
#44353 = CARTESIAN_POINT ( 'NONE',  ( 23.63989407724920255, 3.364481845875844090, 13.53838179598365876 ) ) ;
#44354 = CARTESIAN_POINT ( 'NONE',  ( 10.86272200990529946, -5.206705454565000224, -7.079074440652799893 ) ) ;
#44355 = VERTEX_POINT ( 'NONE', #49414 ) ;
#44356 = VECTOR ( 'NONE', #43661, 1000.000000000000000 ) ;
#44357 = CARTESIAN_POINT ( 'NONE',  ( 10.61705858902340971, -5.079493225104016574, -8.329679463145376772 ) ) ;
#44358 = CARTESIAN_POINT ( 'NONE',  ( 7.239691113742999562, 4.389299166881000858, 9.135259451319999613 ) ) ;
#44360 = CARTESIAN_POINT ( 'NONE',  ( 11.26212378248529866, 3.384904051819500381, 8.663708617168998316 ) ) ;
#44359 = CARTESIAN_POINT ( 'NONE',  ( 8.845310841232000953, 5.851083642416999631, -7.072167224702999633 ) ) ;
#44361 = CARTESIAN_POINT ( 'NONE',  ( 10.98632665877000036, 3.015084670878999784, -9.064442106213000727 ) ) ;
#44362 = EDGE_LOOP ( 'NONE', ( #45944, #58430, #48603, #13664, #64739 ) ) ;
#44363 = CARTESIAN_POINT ( 'NONE',  ( 10.46754281781999829, 2.318340407652000223, 6.549777679168999001 ) ) ;
#44364 = AXIS2_PLACEMENT_3D ( 'NONE', #33280, #765, #5317 ) ;
#44365 = CARTESIAN_POINT ( 'NONE',  ( 17.55505043854147118, -1.787797342887048391, -13.88538010501571129 ) ) ;
#44366 = CARTESIAN_POINT ( 'NONE',  ( 11.06795257254739973, 3.036453385827900142, 7.219770138693499817 ) ) ;
#44367 = CARTESIAN_POINT ( 'NONE',  ( 9.910640133503999749, -2.107273866476999657, 7.885282692430999774 ) ) ;
#44368 = DIRECTION ( 'NONE',  ( 1.000000000000000000, 0.000000000000000000, 0.000000000000000000 ) ) ;
#44369 = ORIENTED_EDGE ( 'NONE', *, *, #63221, .F. ) ;
#44370 = CARTESIAN_POINT ( 'NONE',  ( 24.72545694048200104, 12.30753067676000079, -2.942917560469000104 ) ) ;
#44371 = EDGE_CURVE ( 'NONE', #36055, #39994, #60762, .T. ) ;
#44372 = EDGE_CURVE ( 'NONE', #23807, #58927, #10728, .T. ) ;
#44374 = CARTESIAN_POINT ( 'NONE',  ( 11.14450444037999866, -5.035425715994000129, -8.381528062715000615 ) ) ;
#44373 = CARTESIAN_POINT ( 'NONE',  ( 12.20391894010200140, -11.86124369401000145, 3.532130569927999897 ) ) ;
#44375 = CARTESIAN_POINT ( 'NONE',  ( 8.093318583063375371, -4.415994369059405678, 5.811304729630019317 ) ) ;
#44376 = CARTESIAN_POINT ( 'NONE',  ( 11.25041341105000114, -5.730771985297000271, 8.122672103119001008 ) ) ;
#44377 = CARTESIAN_POINT ( 'NONE',  ( 23.61806549638300012, 2.886582507844000389, 13.53859147826000076 ) ) ;
#44378 = CARTESIAN_POINT ( 'NONE',  ( 9.653405316140000636, -4.213249376011100722, 6.518487389810699639 ) ) ;
#44379 = ORIENTED_EDGE ( 'NONE', *, *, #64235, .T. ) ;
#44380 = CARTESIAN_POINT ( 'NONE',  ( 24.83134064321769330, -11.65949623918286093, -3.197451102845753290 ) ) ;
#44381 = CARTESIAN_POINT ( 'NONE',  ( 10.70226357027499908, -2.879914860223000250, 7.283900408233900059 ) ) ;
#44382 = ORIENTED_EDGE ( 'NONE', *, *, #45315, .F. ) ;
#44383 = DIRECTION ( 'NONE',  ( 0.000000000000000000, -0.9916377111174248249, -0.1290528957048031888 ) ) ;
#44384 = ORIENTED_EDGE ( 'NONE', *, *, #31262, .F. ) ;
#44385 = CARTESIAN_POINT ( 'NONE',  ( 9.699495280410998177, 5.048004622677000341, -6.120508709481000231 ) ) ;
#44386 = CARTESIAN_POINT ( 'NONE',  ( 23.52038098767900109, 13.48733383052000079, -4.207157608410000194 ) ) ;
#44387 = CARTESIAN_POINT ( 'NONE',  ( 8.262341161841696646, 5.029723662799696626, 6.384309865549246510 ) ) ;
#44388 = CARTESIAN_POINT ( 'NONE',  ( 12.61707675448779398, 1.903914349653179627, -12.57067604690442764 ) ) ;
#44389 = CARTESIAN_POINT ( 'NONE',  ( 10.89969598649000027, -3.111999510220800236, 6.971269690999399415 ) ) ;
#44390 = EDGE_CURVE ( 'NONE', #64636, #61687, #24116, .T. ) ;
#44391 = DIRECTION ( 'NONE',  ( 1.000000000000000000, 0.000000000000000000, 0.000000000000000000 ) ) ;
#44392 = AXIS2_PLACEMENT_3D ( 'NONE', #13074, #44205, #54675 ) ;
#44393 = EDGE_LOOP ( 'NONE', ( #36272, #58232, #49265, #53939 ) ) ;
#44394 = CARTESIAN_POINT ( 'NONE',  ( 7.854816940377000734, -4.561648098548999997, 6.153050355516999304 ) ) ;
#44395 = CARTESIAN_POINT ( 'NONE',  ( 18.00086112087972268, -0.5837697426893185826, 13.98798827748170481 ) ) ;
#44396 = EDGE_LOOP ( 'NONE', ( #29309, #62198 ) ) ;
#44397 = CARTESIAN_POINT ( 'NONE',  ( 12.54729787553185716, -3.152819052640251307, -12.19917003430776958 ) ) ;
#44398 = CARTESIAN_POINT ( 'NONE',  ( 11.33456651104149948, 4.112542507956200133, 8.635175889530000148 ) ) ;
#44399 = CARTESIAN_POINT ( 'NONE',  ( 9.115000000004000569, -5.349999999999999645, -7.500000000000000000 ) ) ;
#44400 = CARTESIAN_POINT ( 'NONE',  ( 11.13224000329999974, 2.679518535232000342, -4.955559702528000265 ) ) ;
#44401 = CARTESIAN_POINT ( 'NONE',  ( 17.86987531604100354, -11.45991251204999983, 4.658960512821999522 ) ) ;
#44402 = CARTESIAN_POINT ( 'NONE',  ( 8.225195096046189036, -2.649880853682571313, 7.500010424662522546 ) ) ;
#44403 = CARTESIAN_POINT ( 'NONE',  ( 12.51718303290435763, -3.054853725429545808, -13.53993614671057166 ) ) ;
#44404 = CARTESIAN_POINT ( 'NONE',  ( 18.16600380262988423, 0.1321628250398309556, -12.69908003149456377 ) ) ;
#44405 = AXIS2_PLACEMENT_3D ( 'NONE', #47494, #20572, #41897 ) ;
#44406 = CARTESIAN_POINT ( 'NONE',  ( 12.18432844470346232, 2.573800461449739618, -12.43409912879210566 ) ) ;
#44407 = CARTESIAN_POINT ( 'NONE',  ( 11.61759063708296047, -2.782734359457999851, -7.842242470354300110 ) ) ;
#44408 = CARTESIAN_POINT ( 'NONE',  ( 8.096551658772000337, 5.061727314042999915, 5.824077473724000420 ) ) ;
#44409 = ORIENTED_EDGE ( 'NONE', *, *, #47998, .T. ) ;
#44410 = AXIS2_PLACEMENT_3D ( 'NONE', #64689, #31866, #53183 ) ;
#44411 = CARTESIAN_POINT ( 'NONE',  ( 21.59999953993000332, -1.509903313490000218E-14, 4.329869796037999436E-14 ) ) ;
#44412 = DIRECTION ( 'NONE',  ( 0.000000000000000000, 1.000000000000000000, 0.000000000000000000 ) ) ;
#44413 = CARTESIAN_POINT ( 'NONE',  ( 11.35194613850999978, 12.28618680900000015, 1.513058913260000082 ) ) ;
#44414 = CARTESIAN_POINT ( 'NONE',  ( 23.83662517011200066, -3.384089299514999816, 13.10251501914999928 ) ) ;
#44415 = CARTESIAN_POINT ( 'NONE',  ( 17.83404768640021487, 1.940633243441993283, 12.56443520114847345 ) ) ;
#44416 = LINE ( 'NONE', #33222, #19394 ) ;
#44417 = CARTESIAN_POINT ( 'NONE',  ( 11.25041981190000051, 5.730782764036999488, 8.122675980938000251 ) ) ;
#44418 = AXIS2_PLACEMENT_3D ( 'NONE', #44454, #7371, #54926 ) ;
#44419 = ADVANCED_FACE ( 'NONE', ( #27762 ), #65489, .T. ) ;
#44420 = LINE ( 'NONE', #49996, #20173 ) ;
#44421 = CARTESIAN_POINT ( 'NONE',  ( 2.202983345419999850, 2.610295513370000098, -1.876847361837999939 ) ) ;
#44422 = ORIENTED_EDGE ( 'NONE', *, *, #33393, .T. ) ;
#44423 = CARTESIAN_POINT ( 'NONE',  ( 12.12470607006060597, -2.231004149372987744, 12.40091715157283936 ) ) ;
#44424 = CARTESIAN_POINT ( 'NONE',  ( 9.604355082327998616, -4.449513475323099598, -6.601790705997299114 ) ) ;
#44425 = DIRECTION ( 'NONE',  ( 1.000000000000000000, 0.000000000000000000, 0.000000000000000000 ) ) ;
#44426 = DIRECTION ( 'NONE',  ( 1.000000000000000000, 0.000000000000000000, 0.000000000000000000 ) ) ;
#44427 = CARTESIAN_POINT ( 'NONE',  ( 11.10887482311539998, 5.184953745778000389, -7.978749413531599721 ) ) ;
#44428 = ORIENTED_EDGE ( 'NONE', *, *, #31509, .F. ) ;
#44429 = CARTESIAN_POINT ( 'NONE',  ( 12.08032332909581186, -0.02297882141078348359, 12.59998453421652798 ) ) ;
#44430 = CARTESIAN_POINT ( 'NONE',  ( 9.459510841229999301, 5.445214367171999470, 7.703373622193999459 ) ) ;
#44431 = CARTESIAN_POINT ( 'NONE',  ( 8.674830025576062198, 2.649890579813255709, 7.499988935010339475 ) ) ;
#44432 = CARTESIAN_POINT ( 'NONE',  ( 12.46441593768242839, 3.024116347931779636, 12.31386760464157781 ) ) ;
#44433 = ORIENTED_EDGE ( 'NONE', *, *, #16746, .T. ) ;
#44434 = CARTESIAN_POINT ( 'NONE',  ( 25.20466183898900070, 8.548377718155000693, 7.995577011338999007 ) ) ;
#44435 = B_SPLINE_CURVE_WITH_KNOTS ( 'NONE', 3,
 ( #49878, #60709, #34153, #33461 ),
 .UNSPECIFIED., .F., .F.,
 ( 4, 4 ),
 ( 0.000000000000000000, 0.1494581667962518179 ),
 .UNSPECIFIED. ) ;
#44436 = CARTESIAN_POINT ( 'NONE',  ( 10.24733997687999931, 4.272363749081500295, -6.251346978035999591 ) ) ;
#44437 = CIRCLE ( 'NONE', #25448, 0.7499999936418002555 ) ;
#44438 = CARTESIAN_POINT ( 'NONE',  ( 9.537173706499306292, 4.215401811041960656, 8.849618031277225683 ) ) ;
#44440 = CARTESIAN_POINT ( 'NONE',  ( 9.050000000000000711, -7.679126935408000065, 5.093340497782000043 ) ) ;
#44439 = CARTESIAN_POINT ( 'NONE',  ( 12.17041751256825144, 10.92137764454934690, -4.055351144145800113 ) ) ;
#44441 = CARTESIAN_POINT ( 'NONE',  ( 10.15998825978599918, -4.131418345883800747, 6.504223158184999853 ) ) ;
#44442 = CARTESIAN_POINT ( 'NONE',  ( 10.87518447801629939, -3.134012688501500055, -7.480906371072489236 ) ) ;
#44443 = EDGE_LOOP ( 'NONE', ( #62399, #1321, #48668, #18155 ) ) ;
#44444 = CARTESIAN_POINT ( 'NONE',  ( 1.405611034014000227, -1.124102084663000101, 3.059032707631999859 ) ) ;
#44445 = DIRECTION ( 'NONE',  ( 0.000000000000000000, 0.000000000000000000, -1.000000000000000000 ) ) ;
#44446 = AXIS2_PLACEMENT_3D ( 'NONE', #14005, #12622, #24491 ) ;
#44447 = CARTESIAN_POINT ( 'NONE',  ( 11.05478570706233299, -2.868293641868291388, 6.886599490775120458 ) ) ;
#44448 = CARTESIAN_POINT ( 'NONE',  ( 17.96066850196192632, -2.975608638376130877, 13.56100830561149095 ) ) ;
#44449 = CARTESIAN_POINT ( 'NONE',  ( 10.02314899745999988, 5.167567567567999731, -6.822293592207000934 ) ) ;
#44451 = CARTESIAN_POINT ( 'NONE',  ( 12.08961158949552228, -2.638129719752023927, 13.74921199938403937 ) ) ;
#44450 = AXIS2_PLACEMENT_3D ( 'NONE', #14234, #20157, #45706 ) ;
#44452 = CARTESIAN_POINT ( 'NONE',  ( 10.98148522610999933, 2.884794181589999784, 4.906648103019000118 ) ) ;
#44453 = CARTESIAN_POINT ( 'NONE',  ( 9.307788144226000426, -3.909067355573210278, 6.546538158064899804 ) ) ;
#44454 = CARTESIAN_POINT ( 'NONE',  ( -15.86200481174999943, 2.399999999999999911, -6.571291218949999902 ) ) ;
#44455 = ORIENTED_EDGE ( 'NONE', *, *, #37605, .T. ) ;
#44456 = DIRECTION ( 'NONE',  ( 1.000000000000000000, 0.000000000000000000, 0.000000000000000000 ) ) ;
#44457 = ADVANCED_FACE ( 'NONE', ( #50118 ), #13777, .F. ) ;
#44458 = EDGE_CURVE ( 'NONE', #55115, #69034, #48255, .T. ) ;
#44459 = FACE_OUTER_BOUND ( 'NONE', #53603, .T. ) ;
#44460 = CARTESIAN_POINT ( 'NONE',  ( 18.18005043857343139, 2.459498578984884443, -13.68200151021915545 ) ) ;
#44461 = AXIS2_PLACEMENT_3D ( 'NONE', #41431, #20792, #10298 ) ;
#44462 = CARTESIAN_POINT ( 'NONE',  ( 10.52314899745999988, 5.167567567567999731, -6.822293592207000934 ) ) ;
#44463 = CARTESIAN_POINT ( 'NONE',  ( 18.18005043854143565, 2.500000000000000000, -25.00000000000000000 ) ) ;
#44464 = ORIENTED_EDGE ( 'NONE', *, *, #48297, .T. ) ;
#44465 = CARTESIAN_POINT ( 'NONE',  ( 1.855140132539666586, -0.9161175952574772685, -3.408904368339104707 ) ) ;
#44466 = CARTESIAN_POINT ( 'NONE',  ( 18.05401280175960110, 2.123066371663036023, -12.53147770072749267 ) ) ;
#44467 = CARTESIAN_POINT ( 'NONE',  ( 5.855026506350000659, 1.500000000000000000, 0.000000000000000000 ) ) ;
#44468 = CARTESIAN_POINT ( 'NONE',  ( 11.81056516821459823, 4.609678151793300316, 6.884701936848800052 ) ) ;
#44469 = CONICAL_SURFACE ( 'NONE', #64533, 2.824973347946000413, 0.7853886971611369061 ) ;
#44470 = CARTESIAN_POINT ( 'NONE',  ( 11.08810207955139937, 3.203462856645999945, -7.174999999999999822 ) ) ;
#44471 = CARTESIAN_POINT ( 'NONE',  ( 10.76587944038000089, -3.166536971515000243, -8.574494061818999313 ) ) ;
#44472 = CARTESIAN_POINT ( 'NONE',  ( 17.64997652425314811, -0.7254930141145078393, -13.98119259374181311 ) ) ;
#44473 = CARTESIAN_POINT ( 'NONE',  ( 10.98768472633000037, -5.449702618601000026, 4.945212061625999134 ) ) ;
#44474 = CARTESIAN_POINT ( 'NONE',  ( 12.49090498479077560, -3.040702594595472874, 12.30901830445581346 ) ) ;
#44475 = EDGE_CURVE ( 'NONE', #10719, #33864, #42153, .T. ) ;
#44476 = VERTEX_POINT ( 'NONE', #67555 ) ;
#44477 = CARTESIAN_POINT ( 'NONE',  ( 7.366448187504803791, 3.134553601932692946, 9.009082482539499281 ) ) ;
#44478 = ORIENTED_EDGE ( 'NONE', *, *, #35907, .F. ) ;
#44479 = CARTESIAN_POINT ( 'NONE',  ( 18.10320344748336652, -2.199570933858661537, 13.73260621368703482 ) ) ;
#44480 = CARTESIAN_POINT ( 'NONE',  ( 7.793464139059000040, 3.207866775510000323, 6.406745604615000644 ) ) ;
#44481 = ORIENTED_EDGE ( 'NONE', *, *, #58887, .T. ) ;
#44482 = ADVANCED_FACE ( 'NONE', ( #40999 ), #42870, .F. ) ;
#44483 = CARTESIAN_POINT ( 'NONE',  ( 11.68788784977535933, 3.014014167207800465, 7.556342205905759890 ) ) ;
#44484 = CARTESIAN_POINT ( 'NONE',  ( 6.083820272009583974, 1.131309771130457609, 0.05987387093659040510 ) ) ;
#44485 = CARTESIAN_POINT ( 'NONE',  ( 8.698396402458998367, -4.369105567410300317, -8.298253663472900499 ) ) ;
#44486 = CARTESIAN_POINT ( 'NONE',  ( 10.89874804681000064, 2.834828962328999502, 9.088465460431999432 ) ) ;
#44487 = DIRECTION ( 'NONE',  ( 0.000000000000000000, 0.000000000000000000, 1.000000000000000000 ) ) ;
#44488 = CARTESIAN_POINT ( 'NONE',  ( 10.66476354018241501, -2.782534154164604256, 7.827184855449094592 ) ) ;
#44489 = CARTESIAN_POINT ( 'NONE',  ( 11.80756411264299999, 3.251511910489000012, -11.33753290789000090 ) ) ;
#44490 = CARTESIAN_POINT ( 'NONE',  ( 9.961463664312999455, -2.787129471086000176, -8.677705025472000955 ) ) ;
#44491 = CARTESIAN_POINT ( 'NONE',  ( 5.000000000000000000, -1.800000000000000044, 0.000000000000000000 ) ) ;
#44492 = CARTESIAN_POINT ( 'NONE',  ( 5.537956561560666735, -1.500000000000001332, 0.3217608788839214085 ) ) ;
#44493 = EDGE_LOOP ( 'NONE', ( #25223, #57331, #23474, #19579 ) ) ;
#44494 = CARTESIAN_POINT ( 'NONE',  ( 10.00551210286899995, 3.782771630962269871, 6.243812680477911492 ) ) ;
#44495 = ORIENTED_EDGE ( 'NONE', *, *, #42056, .T. ) ;
#44496 = CARTESIAN_POINT ( 'NONE',  ( 10.68942872663553523, 3.124652943151730700, -4.799721330066085478 ) ) ;
#44497 = CARTESIAN_POINT ( 'NONE',  ( 10.26948980103999887, -4.629959721010000528, 4.845921682315999846 ) ) ;
#44498 = FACE_OUTER_BOUND ( 'NONE', #66274, .T. ) ;
#44499 = CARTESIAN_POINT ( 'NONE',  ( 9.962988259787000089, 3.832626376493700082, -8.768215461831999846 ) ) ;
#44500 = CARTESIAN_POINT ( 'NONE',  ( 12.37528356179625710, 2.046093867836325852, 13.75926687192407094 ) ) ;
#44501 = CARTESIAN_POINT ( 'NONE',  ( 10.27968096967000022, -5.739708848514999850, 7.774962785835000112 ) ) ;
#44502 = ORIENTED_EDGE ( 'NONE', *, *, #30476, .T. ) ;
#44503 = DIRECTION ( 'NONE',  ( -7.209535665603963368E-10, -0.7071067809378975833, -0.7071067814351975622 ) ) ;
#44504 = CARTESIAN_POINT ( 'NONE',  ( 12.44118158293134613, -0.5082612142235585218, 13.88749228919890122 ) ) ;
#44505 = ORIENTED_EDGE ( 'NONE', *, *, #56275, .T. ) ;
#44506 = CARTESIAN_POINT ( 'NONE',  ( 6.794909439180999655, 5.172411450403999744, -8.246583185469999577 ) ) ;
#44507 = DIRECTION ( 'NONE',  ( 1.000000000000000000, 0.000000000000000000, 0.000000000000000000 ) ) ;
#44508 = CARTESIAN_POINT ( 'NONE',  ( 8.872292071306626227, 4.874163933583397501, 7.537009346329285542 ) ) ;
#44509 = AXIS2_PLACEMENT_3D ( 'NONE', #67286, #15188, #36512 ) ;
#44510 = CARTESIAN_POINT ( 'NONE',  ( 4.152514736428999598, -1.182555397712999889, -0.9394135237491000323 ) ) ;
#44511 = CARTESIAN_POINT ( 'NONE',  ( 9.825045280412000537, 3.116293075258000478, -6.208411413796000033 ) ) ;
#44512 = LINE ( 'NONE', #18618, #14654 ) ;
#44513 = CARTESIAN_POINT ( 'NONE',  ( 10.78636854442000192, -5.666037955714999796, -7.787004779180999314 ) ) ;
#44514 = PRODUCT_DEFINITION ( 'UNKNOWN', '', #54158, #15707 ) ;
#44515 =( GEOMETRIC_REPRESENTATION_CONTEXT ( 3 ) GLOBAL_UNCERTAINTY_ASSIGNED_CONTEXT ( ( #3827 ) ) GLOBAL_UNIT_ASSIGNED_CONTEXT ( ( #61246, #28753, #29100 ) ) REPRESENTATION_CONTEXT ( 'NONE', 'WORKASPACE' ) );
#44516 = CARTESIAN_POINT ( 'NONE',  ( 8.294122261300687526, 2.649609490281852331, -7.853149655434442877 ) ) ;
#44517 = DIRECTION ( 'NONE',  ( 1.000000000000000000, 0.000000000000000000, 0.000000000000000000 ) ) ;
#44518 = CARTESIAN_POINT ( 'NONE',  ( 10.90000668870999867, -1.199999999999999956, -9.776630298829998011 ) ) ;
#44519 = CARTESIAN_POINT ( 'NONE',  ( 9.130720302798000176, -5.231133027468000130, -6.569831606205999819 ) ) ;
#44520 = CARTESIAN_POINT ( 'NONE',  ( 11.19518313518939934, 3.462699341914400097, -8.179416362154199760 ) ) ;
#44521 = CARTESIAN_POINT ( 'NONE',  ( 1.000973465875999890, 3.500000000000000000, 0.000000000000000000 ) ) ;
#44522 = CARTESIAN_POINT ( 'NONE',  ( 10.93990547754509812, 5.032986398992000510, -7.532784233952049213 ) ) ;
#44523 = CARTESIAN_POINT ( 'NONE',  ( 8.950772138681999834, 3.626242194157900389, -6.567719246739500250 ) ) ;
#44525 = CARTESIAN_POINT ( 'NONE',  ( 11.00012419157999943, -2.844226485624000045, 5.106573563347000189 ) ) ;
#44524 = CARTESIAN_POINT ( 'NONE',  ( 9.521784697134998865, -3.454948069423500190, 8.343659109631099469 ) ) ;
#44526 = VECTOR ( 'NONE', #51951, 1000.000000000000114 ) ;
#44527 = DIRECTION ( 'NONE',  ( 1.000000000000000000, 0.000000000000000000, 0.000000000000000000 ) ) ;
#44528 = ORIENTED_EDGE ( 'NONE', *, *, #47992, .T. ) ;
#44529 = CARTESIAN_POINT ( 'NONE',  ( 10.64391429142989765, 4.022379549362480766, 8.674673860548999471 ) ) ;
#44530 = CARTESIAN_POINT ( 'NONE',  ( 10.96580795178999956, -4.930647899304999804, 6.170539049947000088 ) ) ;
#44531 = CARTESIAN_POINT ( 'NONE',  ( 9.228442991499999692, 3.919472480837189909, 8.776675254768999679 ) ) ;
#44532 = CARTESIAN_POINT ( 'NONE',  ( 17.60000001072100062, -11.41073498373000028, 4.623967591968000335 ) ) ;
#44533 = CARTESIAN_POINT ( 'NONE',  ( 9.882266086202999844, -4.932716797830999589, 6.390980246320999925 ) ) ;
#44534 = CARTESIAN_POINT ( 'NONE',  ( 9.759298684490481435, -5.294816862906961852, 8.717541015033191343 ) ) ;
#44535 = CARTESIAN_POINT ( 'NONE',  ( 11.80707028823900195, 3.411567914393000223, -11.89801974982000132 ) ) ;
#44536 = VERTEX_POINT ( 'NONE', #56394 ) ;
#44537 = EDGE_CURVE ( 'NONE', #14453, #7391, #2448, .T. ) ;
#44538 = EDGE_CURVE ( 'NONE', #20915, #37115, #61631, .T. ) ;
#44539 =( REPRESENTATION_RELATIONSHIP ('NONE','NONE', #10823, #60856 ) REPRESENTATION_RELATIONSHIP_WITH_TRANSFORMATION ( #5051 )SHAPE_REPRESENTATION_RELATIONSHIP( ) );
#44540 = CARTESIAN_POINT ( 'NONE',  ( 9.533342523874999586, -4.992846242613000030, -7.348017636355000270 ) ) ;
#44541 = B_SPLINE_CURVE_WITH_KNOTS ( 'NONE', 3,
 ( #28204, #29601, #61393, #1631 ),
 .UNSPECIFIED., .F., .F.,
 ( 4, 4 ),
 ( 0.000000000000000000, 1.000000000000000000 ),
 .UNSPECIFIED. ) ;
#44542 = CARTESIAN_POINT ( 'NONE',  ( 9.833513540183334456, -5.249999999999999112, -7.336375382625531572 ) ) ;
#44543 = FACE_OUTER_BOUND ( 'NONE', #57502, .T. ) ;
#44544 = CARTESIAN_POINT ( 'NONE',  ( 8.753494611379007750, -2.844423643914999023, -6.810303980490998832 ) ) ;
#44545 = VECTOR ( 'NONE', #65287, 1000.000000000000114 ) ;
#44546 = DIRECTION ( 'NONE',  ( 1.000000000000000000, 0.000000000000000000, 0.000000000000000000 ) ) ;
#44547 = FACE_OUTER_BOUND ( 'NONE', #54900, .T. ) ;
#44548 = CARTESIAN_POINT ( 'NONE',  ( 11.75718044953559804, 4.889766368533900120, -7.963966784336999005 ) ) ;
#44549 = CARTESIAN_POINT ( 'NONE',  ( 12.63945631780503831, 1.891770379291387361, -13.78384844198478021 ) ) ;
#44551 = CARTESIAN_POINT ( 'NONE',  ( 8.455992358796999397, 5.100000000000000533, 6.571291218954000257 ) ) ;
#44550 = VECTOR ( 'NONE', #29920, 1000.000000000000000 ) ;
#44552 = CARTESIAN_POINT ( 'NONE',  ( 23.56665657345700282, -13.31365812469000076, 4.296923216748999685 ) ) ;
#44553 = VERTEX_POINT ( 'NONE', #755 ) ;
#44554 = CARTESIAN_POINT ( 'NONE',  ( 10.90000000000000036, -1.376649746192999846, 11.21582968292000082 ) ) ;
#44555 = CARTESIAN_POINT ( 'NONE',  ( 12.36315992512968265, -0.5793931417437993003, -13.98801390351337837 ) ) ;
#44556 = CARTESIAN_POINT ( 'NONE',  ( 14.02348875342600110, -8.812421938351000961, -7.562304860556999131 ) ) ;
#44557 = CARTESIAN_POINT ( 'NONE',  ( 11.59999999999999964, 5.064318446328999634, -8.155535082817699788 ) ) ;
#44558 = CARTESIAN_POINT ( 'NONE',  ( 10.40434687351665310, -5.250000000000000888, -7.663624617374465764 ) ) ;
#44559 = CARTESIAN_POINT ( 'NONE',  ( 7.000000000000000888, 10.53694504865381631, 4.009111100864517496 ) ) ;
#44560 = CARTESIAN_POINT ( 'NONE',  ( 5.647168941335773518, 12.08810193142241474, -3.737902345522961856 ) ) ;
#44561 = ORIENTED_EDGE ( 'NONE', *, *, #1932, .F. ) ;
#44562 = FILL_AREA_STYLE_COLOUR ( '', #54066 ) ;
#44563 = CARTESIAN_POINT ( 'NONE',  ( 18.16447345601862651, 2.360953327207878871, -13.70196990072541610 ) ) ;
#44564 = ORIENTED_EDGE ( 'NONE', *, *, #46397, .T. ) ;
#44565 = EDGE_CURVE ( 'NONE', #34321, #64614, #19906, .T. ) ;
#44566 = PLANE ( 'NONE',  #35082 ) ;
#44567 = CARTESIAN_POINT ( 'NONE',  ( 24.92851483856576777, 8.562961969008355823, -8.403401768322540377 ) ) ;
#44568 = CARTESIAN_POINT ( 'NONE',  ( 8.854170280414001226, 4.902869380824999901, -8.978557145469999057 ) ) ;
#44569 = CARTESIAN_POINT ( 'NONE',  ( 8.807788144226000426, 4.090932644426789722, -8.453461841935100196 ) ) ;
#44570 = CARTESIAN_POINT ( 'NONE',  ( 11.17901463001529905, -3.302889347096799710, -6.383488688482000128 ) ) ;
#44571 = CARTESIAN_POINT ( 'NONE',  ( 9.338847651065298905, -5.080747737076881876, -6.285327966759164831 ) ) ;
#44572 = CARTESIAN_POINT ( 'NONE',  ( 10.24809687351566723, -3.672815144550895194, 8.717465845835393523 ) ) ;
#44573 = ORIENTED_EDGE ( 'NONE', *, *, #41824, .T. ) ;
#44574 = CARTESIAN_POINT ( 'NONE',  ( 8.374870900372675564, 4.397654444569530696, -6.040776445627388469 ) ) ;
#44575 = CARTESIAN_POINT ( 'NONE',  ( 18.18005043832647161, -2.519786138815505616, -13.66921024352858538 ) ) ;
#44576 = CARTESIAN_POINT ( 'NONE',  ( 18.14740543753015345, -2.299612738903852982, 13.71393688410694622 ) ) ;
#44577 = ORIENTED_EDGE ( 'NONE', *, *, #955, .F. ) ;
#44578 = CARTESIAN_POINT ( 'NONE',  ( 10.30296826955000000, 4.081263352980999848, -9.025008366823000117 ) ) ;
#44579 = ORIENTED_EDGE ( 'NONE', *, *, #6394, .T. ) ;
#44580 = CARTESIAN_POINT ( 'NONE',  ( 8.874784697134998623, 4.545051930576500254, 8.343659109631099469 ) ) ;
#44581 = CARTESIAN_POINT ( 'NONE',  ( 18.10358258445732815, -2.009225442943083806, -12.43878435193940568 ) ) ;
#44582 = CARTESIAN_POINT ( 'NONE',  ( 10.99338701711599242, 6.091027238782714903, -5.064515391775427311 ) ) ;
#44583 = DIRECTION ( 'NONE',  ( 0.000000000000000000, 1.000000000000000000, 0.000000000000000000 ) ) ;
#44584 = CARTESIAN_POINT ( 'NONE',  ( 11.60581233665799950, -11.65209074823999913, -1.826497490784000144 ) ) ;
#44585 = B_SPLINE_CURVE_WITH_KNOTS ( 'NONE', 3,
 ( #26056, #31647, #58210, #62078, #4023, #41447, #57867, #14197, #9270, #35522, #15568, #56844, #42140, #20459, #57511, #62756, #25706, #8942 ),
 .UNSPECIFIED., .F., .F.,
 ( 4, 2, 2, 2, 2, 2, 2, 2, 4 ),
 ( 0.000000000000000000, 0.1250000000000000000, 0.2500000000000000000, 0.3750000000000000000, 0.5000000000000000000, 0.6250000000000000000, 0.7500000000000000000, 0.8750000000000000000, 1.000000000000000000 ),
 .UNSPECIFIED. ) ;
#44586 = CARTESIAN_POINT ( 'NONE',  ( 9.989267173155999657, 3.235527139800300045, 8.151477970733999712 ) ) ;
#44587 = CARTESIAN_POINT ( 'NONE',  ( 9.354496976570960243, -3.359497858161771600, 9.117191629812770870 ) ) ;
#44588 = ORIENTED_EDGE ( 'NONE', *, *, #54179, .T. ) ;
#44589 = CARTESIAN_POINT ( 'NONE',  ( 8.599999952505998024, -4.000000000000000000, -7.500000000000000000 ) ) ;
#44590 = CARTESIAN_POINT ( 'NONE',  ( 11.16750778041000025, 3.188704589882000118, -8.788663768996000769 ) ) ;
#44591 = CARTESIAN_POINT ( 'NONE',  ( 5.100000000000000533, 0.1499999999999999944, -6.463315149415000072 ) ) ;
#44592 = CARTESIAN_POINT ( 'NONE',  ( 12.19646863228097367, 2.642680340209512924, -13.64216715890480636 ) ) ;
#44593 = CARTESIAN_POINT ( 'NONE',  ( 10.08963399569799790, -2.728594541839999721, -7.641111829547599932 ) ) ;
#44594 = CARTESIAN_POINT ( 'NONE',  ( 11.14698053895999941, -5.129799765052999838, 5.886044098803999702 ) ) ;
#44595 = CARTESIAN_POINT ( 'NONE',  ( 17.94354858665102981, 0.4896942981276218299, 13.88839019180477052 ) ) ;
#44596 = CARTESIAN_POINT ( 'NONE',  ( 25.31135185429100076, -2.728831955372000184, 11.35931141337999861 ) ) ;
#44597 = EDGE_CURVE ( 'NONE', #52918, #55782, #36438, .T. ) ;
#44598 = EDGE_CURVE ( 'NONE', #33287, #66793, #23251, .T. ) ;
#44599 = ORIENTED_EDGE ( 'NONE', *, *, #6692, .T. ) ;
#44600 = ORIENTED_EDGE ( 'NONE', *, *, #5648, .T. ) ;
#44601 = CARTESIAN_POINT ( 'NONE',  ( 8.889129719593999113, 5.687930027805999877, -7.109876198051000351 ) ) ;
#44602 = CARTESIAN_POINT ( 'NONE',  ( 12.18006436421859107, -0.02054912257076008456, 13.89999925486856824 ) ) ;
#44603 = CARTESIAN_POINT ( 'NONE',  ( 12.66331021905145349, -0.6090267839202087030, -13.88203573366523358 ) ) ;
#44604 = CARTESIAN_POINT ( 'NONE',  ( 9.758146639703001668, -2.901368778958000050, 6.555068849476000103 ) ) ;
#44605 = CARTESIAN_POINT ( 'NONE',  ( 5.599999999999999645, -0.4000000000000000222, 6.406472342878999804 ) ) ;
#44606 = CARTESIAN_POINT ( 'NONE',  ( 7.229683059621999419, -2.630475685621000093, 6.995953627589999613 ) ) ;
#44607 = DIRECTION ( 'NONE',  ( -1.000000000000000000, 0.000000000000000000, 0.000000000000000000 ) ) ;
#44609 = CARTESIAN_POINT ( 'NONE',  ( 8.766851002546001581, 2.832432432432000269, 6.822293592207000934 ) ) ;
#44608 = CARTESIAN_POINT ( 'NONE',  ( 9.652455549953000258, -3.004437130344999929, 8.303267676773000261 ) ) ;
#44610 = CYLINDRICAL_SURFACE ( 'NONE', #22966, 0.6999999999999992895 ) ;
#44611 = CARTESIAN_POINT ( 'NONE',  ( 12.80505043854144276, -0.7302158263239078018, 13.98094363220830871 ) ) ;
#44612 = CARTESIAN_POINT ( 'NONE',  ( 8.668369459057998938, 3.037916315484999963, -6.050520490110999461 ) ) ;
#44613 = CARTESIAN_POINT ( 'NONE',  ( 18.08617525414963367, 0.3300695133819673832, 12.69424233780834754 ) ) ;
#44614 = B_SPLINE_SURFACE_WITH_KNOTS ( 'NONE', 3, 3, ( 
 ( #32373, #47071, #47763, #27124 ),
 ( #548, #31680, #9649, #41817 ),
 ( #63124, #57899, #36573, #53001 ),
 ( #28153, #59959, #18015, #22896 ),
 ( #1578, #54367, #11712, #34094 ),
 ( #49467, #65887, #33750, #2272 ),
 ( #23590, #44247, #28506, #55414 ),
 ( #1931, #43544, #44933, #6818 ) ),
 .UNSPECIFIED., .F., .F., .F.,
 ( 4, 1, 1, 1, 1, 4 ),
 ( 4, 4 ),
 ( 0.7453233389708999734, 0.7647058823529000460, 0.8235294117646999590, 0.8823529411764999830, 0.9411764705882000870, 0.9905821372920999845 ),
 ( -0.1830924183985000175, 1.182948959795000032 ),
 .UNSPECIFIED. ) ;
#44615 = CARTESIAN_POINT ( 'NONE',  ( 6.999999691988000095, 11.00717859340000082, -1.432487142323000118 ) ) ;
#44616 = CARTESIAN_POINT ( 'NONE',  ( 4.149992563291999836, 0.2617923565147971532, 1.999946284944288388 ) ) ;
#44617 = ORIENTED_EDGE ( 'NONE', *, *, #24919, .T. ) ;
#44619 = LINE ( 'NONE', #2296, #17275 ) ;
#44618 = CARTESIAN_POINT ( 'NONE',  ( 23.60000000000000142, 0.000000000000000000, 0.000000000000000000 ) ) ;
#44620 = CARTESIAN_POINT ( 'NONE',  ( 8.903895280414001689, 3.867331042029999999, -9.227339949050001877 ) ) ;
#44621 =( BOUNDED_SURFACE ( )  B_SPLINE_SURFACE ( 3, 3, ( 
 ( #39668, #60643, #44238, #34437 ),
 ( #60299, #2940, #50160, #1565 ),
 ( #12755, #40019, #44920, #22887 ),
 ( #1920, #61334, #38628, #59949 ) ),
 .UNSPECIFIED., .F., .F., .T. ) 
 B_SPLINE_SURFACE_WITH_KNOTS ( ( 4, 4 ),
 ( 4, 4 ),
 ( 0.000000000000000000, 1.000000000000000000 ),
 ( 0.000000000000000000, 1.000000000000000000 ),
 .UNSPECIFIED. ) 
 GEOMETRIC_REPRESENTATION_ITEM ( )  RATIONAL_B_SPLINE_SURFACE ( (
 ( 1.512182578520000042, 1.160176301760999840, 1.160176301760999840, 1.512182578520000042),
 ( 1.111288591041000196, 0.8526025270081000196, 0.8526025270081000196, 1.111288591041000196),
 ( 1.111288591041000196, 0.8526025270081000196, 0.8526025270081000196, 1.111288591041000196),
 ( 1.512182578520000042, 1.160176301760999840, 1.160176301760999840, 1.512182578520000042) ) ) 
 REPRESENTATION_ITEM ( '' )  SURFACE ( )  );
#44622 = EDGE_CURVE ( 'NONE', #13468, #59568, #48653, .T. ) ;
#44623 = FACE_OUTER_BOUND ( 'NONE', #58726, .T. ) ;
#44624 = CARTESIAN_POINT ( 'NONE',  ( 10.78887616594230003, 3.613544262574699850, 8.718182393403999697 ) ) ;
#44625 = EDGE_CURVE ( 'NONE', #7311, #63350, #15817, .T. ) ;
#44626 = B_SPLINE_SURFACE_WITH_KNOTS ( 'NONE', 3, 3, ( 
 ( #54806, #37692, #21604, #53773 ),
 ( #6906, #38029, #22638, #33838 ),
 ( #64248, #5870, #27208, #48531 ),
 ( #59357, #9566, #41732, #57119 ),
 ( #67600, #25654, #56793, #68287 ),
 ( #46986, #46645, #40701, #62702 ),
 ( #50255, #12855, #63037, #28952 ),
 ( #62028, #14823, #20407, #15164 ),
 ( #51534, #46301, #52219, #30906 ),
 ( #4319, #67952, #20068, #41395 ) ),
 .UNSPECIFIED., .F., .F., .F.,
 ( 4, 1, 1, 1, 1, 1, 1, 4 ),
 ( 4, 4 ),
 ( 0.04183311431308000400, 0.1428571428570999946, 0.2857142857143000203, 0.4285714285713999594, 0.5714285714286000406, 0.7142857142856999797, 0.8571428571429000609, 0.9292981235707000742 ),
 ( -0.1917799910644999994, 1.191756862851000021 ),
 .UNSPECIFIED. ) ;
#44627 = FACE_OUTER_BOUND ( 'NONE', #20829, .T. ) ;
#44628 = CARTESIAN_POINT ( 'NONE',  ( 2.039003242238999647, 1.871422929480999864, -2.898831499164999936 ) ) ;
#44629 = VERTEX_POINT ( 'NONE', #21724 ) ;
#44630 = CARTESIAN_POINT ( 'NONE',  ( 12.15475987602170882, -0.3182341284860687458, -12.59598505207571506 ) ) ;
#44631 = CARTESIAN_POINT ( 'NONE',  ( 12.41685245973976137, -2.003519757431140302, -12.55365090558318997 ) ) ;
#44632 = CARTESIAN_POINT ( 'NONE',  ( 12.80000000000000071, 50.14170351282000127, -17.06962823869000090 ) ) ;
#44633 = CARTESIAN_POINT ( 'NONE',  ( 9.181704719590001673, 3.734279507827999556, 8.942126004519000304 ) ) ;
#44634 = VERTEX_POINT ( 'NONE', #20706 ) ;
#44635 = CARTESIAN_POINT ( 'NONE',  ( 5.348560349866000152, 0.1454693244516999939, 1.365796648849999961 ) ) ;
#44636 = CARTESIAN_POINT ( 'NONE',  ( 10.94393950981584496, 9.248375527724082446, 6.280586408606567694 ) ) ;
#44638 = DIRECTION ( 'NONE',  ( 1.000000000000000000, 0.000000000000000000, 0.000000000000000000 ) ) ;
#44637 = CARTESIAN_POINT ( 'NONE',  ( 8.567616298378466055, -3.838977648115872388, 5.766192393133341199 ) ) ;
#44639 = CARTESIAN_POINT ( 'NONE',  ( 11.42834208742529967, 3.293478249981899975, -8.610579932818998472 ) ) ;
#44640 = EDGE_LOOP ( 'NONE', ( #57609, #11082, #18679, #16550 ) ) ;
#44641 = CARTESIAN_POINT ( 'NONE',  ( 12.79999998712400178, -11.53033693765999779, 4.891431908114999949 ) ) ;
#44642 = ORIENTED_EDGE ( 'NONE', *, *, #9736, .F. ) ;
#44643 = EDGE_CURVE ( 'NONE', #23998, #26809, #43308, .T. ) ;
#44644 = CARTESIAN_POINT ( 'NONE',  ( 9.477176340467600824, -5.064601050969631757, 8.332457336712117524 ) ) ;
#44645 = CARTESIAN_POINT ( 'NONE',  ( 24.34833280985366954, 12.15210571723978461, -3.256146913270965282 ) ) ;
#44646 = CARTESIAN_POINT ( 'NONE',  ( 18.17607592425854079, 0.07112389991332046524, -13.89976024287834910 ) ) ;
#44647 = ORIENTED_EDGE ( 'NONE', *, *, #15939, .F. ) ;
#44648 = CARTESIAN_POINT ( 'NONE',  ( 10.94661356027324750, 9.196282120471490629, -6.312081210087247207 ) ) ;
#44649 = B_SPLINE_CURVE_WITH_KNOTS ( 'NONE', 3,
 ( #68137, #62891, #20948, #53103 ),
 .UNSPECIFIED., .F., .F.,
 ( 4, 4 ),
 ( 0.000000000000000000, 1.000000000000000000 ),
 .UNSPECIFIED. ) ;
#44650 = B_SPLINE_CURVE_WITH_KNOTS ( 'NONE', 3,
 ( #56817, #8916, #62727, #57482, #67628, #19752 ),
 .UNSPECIFIED., .F., .F.,
 ( 4, 2, 4 ),
 ( 0.000000000000000000, 0.5000000000000000000, 1.000000000000000000 ),
 .UNSPECIFIED. ) ;
#44651 = CARTESIAN_POINT ( 'NONE',  ( 8.378939858970831267, 5.131721239846337212, 6.760536747085705400 ) ) ;
#44652 = FACE_OUTER_BOUND ( 'NONE', #35574, .T. ) ;
#44653 = DIRECTION ( 'NONE',  ( -1.000000000000000000, 0.000000000000000000, 0.000000000000000000 ) ) ;
#44654 = CARTESIAN_POINT ( 'NONE',  ( 5.500000000000000000, -1.315736040608999957, 10.71955403322999878 ) ) ;
#44655 = ORIENTED_EDGE ( 'NONE', *, *, #21131, .F. ) ;
#44656 = CARTESIAN_POINT ( 'NONE',  ( 8.256676658772999389, 2.876288091423999660, 6.568897128359000526 ) ) ;
#44657 = CARTESIAN_POINT ( 'NONE',  ( 23.58549534400300018, -13.39460428332999875, -4.038169368742999588 ) ) ;
#44658 = CARTESIAN_POINT ( 'NONE',  ( 11.02644139764960229, 5.226441397652185294, 6.590108525923451310 ) ) ;
#44659 = CARTESIAN_POINT ( 'NONE',  ( 8.379867906096000851, 2.923743482149999906, 6.439439799146000176 ) ) ;
#44660 = ORIENTED_EDGE ( 'NONE', *, *, #38220, .T. ) ;
#44661 = CARTESIAN_POINT ( 'NONE',  ( 25.39409943791158142, 11.19591960080123805, 3.259891097492937817 ) ) ;
#44662 = CARTESIAN_POINT ( 'NONE',  ( 8.956149159797568871, -5.077028306801780744, -7.209669135134798346 ) ) ;
#44663 = FACE_OUTER_BOUND ( 'NONE', #59403, .T. ) ;
#44664 = CARTESIAN_POINT ( 'NONE',  ( 5.000030787343002103, -1.834918991542628941, 1.057581170753189248 ) ) ;
#44665 = CARTESIAN_POINT ( 'NONE',  ( 21.10000000000000142, 0.000000000000000000, 0.000000000000000000 ) ) ;
#44666 = CARTESIAN_POINT ( 'NONE',  ( 5.805026506351000037, 1.500000000000000000, 0.000000000000000000 ) ) ;
#44667 = CARTESIAN_POINT ( 'NONE',  ( 17.95182328287553375, -1.877974217481241714, 12.45926392518878068 ) ) ;
#44668 = VERTEX_POINT ( 'NONE', #52865 ) ;
#44669 = CARTESIAN_POINT ( 'NONE',  ( 11.10612378248509913, -4.482960757953799558, -6.586279795136899651 ) ) ;
#44670 = VERTEX_POINT ( 'NONE', #43059 ) ;
#44671 = CIRCLE ( 'NONE', #29051, 2.000000000000000888 ) ;
#44672 = CARTESIAN_POINT ( 'NONE',  ( 1.700000811628999964, 1.775000326287000219, 0.000000000000000000 ) ) ;
#44673 = FACE_OUTER_BOUND ( 'NONE', #16655, .T. ) ;
#44674 = CARTESIAN_POINT ( 'NONE',  ( 2.503158723626000004, -1.438123771530000150, 3.058110052863999950 ) ) ;
#44675 = CARTESIAN_POINT ( 'NONE',  ( 10.61721988130000049, -5.045606037229999785, -6.386907901056999570 ) ) ;
#44676 = CARTESIAN_POINT ( 'NONE',  ( 6.813937712952314207, 1.320991801770956098, -0.7472670741277307460 ) ) ;
#44677 = CARTESIAN_POINT ( 'NONE',  ( 8.163776391448005043, 3.396249911995000481, -6.162465440825001473 ) ) ;
#44678 = EDGE_CURVE ( 'NONE', #18715, #23593, #409, .T. ) ;
#44680 = EDGE_CURVE ( 'NONE', #41017, #4376, #65835, .T. ) ;
#44679 = CARTESIAN_POINT ( 'NONE',  ( 23.56665676678700194, 0.01733454660186801305, -13.98987989644267671 ) ) ;
#44681 = ORIENTED_EDGE ( 'NONE', *, *, #39063, .F. ) ;
#44682 = CARTESIAN_POINT ( 'NONE',  ( 10.09654241571003119, -5.267280400567660337, -8.036449566519722865 ) ) ;
#44683 = EDGE_CURVE ( 'NONE', #67010, #19021, #34311, .T. ) ;
#44684 = CARTESIAN_POINT ( 'NONE',  ( 11.34641504065830020, -3.195537720350400068, 8.099826052678000821 ) ) ;
#44685 = CARTESIAN_POINT ( 'NONE',  ( 10.34520858566999912, 2.724123081339000052, 6.497325124886000225 ) ) ;
#44686 = CARTESIAN_POINT ( 'NONE',  ( 25.30000327618300204, -8.756202924575998026, -7.455126447192999883 ) ) ;
#44687 = DIRECTION ( 'NONE',  ( -0.9999999999995587974, 4.522743910255808775E-07, 8.233165790437657900E-07 ) ) ;
#44688 = CARTESIAN_POINT ( 'NONE',  ( 10.99166666666766723, 4.098468854244242010, 8.958105619230160244 ) ) ;
#44689 = CARTESIAN_POINT ( 'NONE',  ( 11.24025954179439957, 4.771812902496799680, -8.141292208271599051 ) ) ;
#44690 = CARTESIAN_POINT ( 'NONE',  ( 24.30001683613300045, -12.21047198529999989, -3.271805531187999883 ) ) ;
#44691 = CARTESIAN_POINT ( 'NONE',  ( 10.08762143724499794, 4.758411336345700349, -6.646450532840099790 ) ) ;
#44692 = CARTESIAN_POINT ( 'NONE',  ( 23.58437014357399875, -10.35669085107999976, 9.329830741018000140 ) ) ;
#44693 = CARTESIAN_POINT ( 'NONE',  ( 0.7509734658760000015, -3.500000000000000000, 0.000000000000000000 ) ) ;
#44694 = CARTESIAN_POINT ( 'NONE',  ( 10.56170778040999991, 5.057487376164999660, -8.595710652231000282 ) ) ;
#44695 = ORIENTED_EDGE ( 'NONE', *, *, #23795, .F. ) ;
#44696 = CARTESIAN_POINT ( 'NONE',  ( 7.860168146793000687, -2.263562268490999951, 8.007440964304000985 ) ) ;
#44697 = CARTESIAN_POINT ( 'NONE',  ( 18.27869735329872114, 2.567871808702999914, 13.76250717860552264 ) ) ;
#44698 = CARTESIAN_POINT ( 'NONE',  ( 7.000000000000000000, 0.3230303992915000144, 3.000000000000000000 ) ) ;
#44699 = CARTESIAN_POINT ( 'NONE',  ( 11.13349010443639919, -2.725546193138000284, -7.595309363461700158 ) ) ;
#44700 = B_SPLINE_CURVE_WITH_KNOTS ( 'NONE', 3,
 ( #10624, #20432, #67976, #52939 ),
 .UNSPECIFIED., .F., .F.,
 ( 4, 4 ),
 ( 0.000000000000000000, 1.000000000000000000 ),
 .UNSPECIFIED. ) ;
#44701 = EDGE_LOOP ( 'NONE', ( #12238, #68037, #49953, #4895, #50305 ) ) ;
#44702 = CARTESIAN_POINT ( 'NONE',  ( 24.67559728077000258, 3.457949410299000270, -12.04093993320999978 ) ) ;
#44703 = CARTESIAN_POINT ( 'NONE',  ( 7.999926658772999133, 5.198556077301000222, 8.332552905512999430 ) ) ;
#44705 = CARTESIAN_POINT ( 'NONE',  ( 9.205629240798000268, -4.228941919214900480, 6.623477632995699693 ) ) ;
#44704 = CARTESIAN_POINT ( 'NONE',  ( 10.26990035061499817, -3.768906505327899836, -8.335645555860798694 ) ) ;
#44706 = CARTESIAN_POINT ( 'NONE',  ( 10.87273915876999908, 5.407616985330000681, -8.698399706473999515 ) ) ;
#44707 = ORIENTED_EDGE ( 'NONE', *, *, #21910, .F. ) ;
#44708 = CARTESIAN_POINT ( 'NONE',  ( 10.35616100078999935, 2.777276096020000029, 8.995275123087999702 ) ) ;
#44709 = CARTESIAN_POINT ( 'NONE',  ( 17.93991242251033924, -3.137220474326288588, -13.64397427468588120 ) ) ;
#44710 = CARTESIAN_POINT ( 'NONE',  ( 11.06379841651039797, 3.598362324325699912, 6.432302808027999141 ) ) ;
#44711 = CARTESIAN_POINT ( 'NONE',  ( 10.61382642076999971, -3.385081736013999976, 5.849525238167000651 ) ) ;
#44712 = CARTESIAN_POINT ( 'NONE',  ( 8.962745559623000347, -5.445226602819000838, 7.703375344019999460 ) ) ;
#44713 = VERTEX_POINT ( 'NONE', #43418 ) ;
#44714 = CARTESIAN_POINT ( 'NONE',  ( 11.09999999999999964, 5.299769311822999818, 5.136744346970999686 ) ) ;
#44715 = CARTESIAN_POINT ( 'NONE',  ( 10.72801694037999987, -3.751276547904999870, -8.836912395451999913 ) ) ;
#44716 = CARTESIAN_POINT ( 'NONE',  ( 7.921590741316500761, -2.367433491553081915, 8.106647180208147674 ) ) ;
#44717 = CARTESIAN_POINT ( 'NONE',  ( 10.15903154954000165, -4.166415630773999901, 9.114167874391000623 ) ) ;
#44718 = DIRECTION ( 'NONE',  ( 1.000000000000000000, 0.000000000000000000, 0.000000000000000000 ) ) ;
#44719 = CARTESIAN_POINT ( 'NONE',  ( 9.754721904869999349, -3.124169273628900179, 7.008306153105300140 ) ) ;
#44720 = ORIENTED_EDGE ( 'NONE', *, *, #32078, .F. ) ;
#44721 = CARTESIAN_POINT ( 'NONE',  ( 11.03776785110999903, -5.237767851104999650, 6.571291218949999902 ) ) ;
#44722 = CARTESIAN_POINT ( 'NONE',  ( 11.34226088462130022, -3.997572771977982775, 8.640738455926999961 ) ) ;
#44723 = VERTEX_POINT ( 'NONE', #44467 ) ;
#44724 = ADVANCED_FACE ( 'NONE', ( #49336 ), #38503, .T. ) ;
#44725 = CARTESIAN_POINT ( 'NONE',  ( 4.574515983791000080E-07, -2.400000066501999818, 0.000000000000000000 ) ) ;
#44726 = ORIENTED_EDGE ( 'NONE', *, *, #40963, .F. ) ;
#44727 = CARTESIAN_POINT ( 'NONE',  ( 9.053070280414001303, 2.391443348526999912, -6.856688371964000162 ) ) ;
#44728 = ADVANCED_FACE ( 'NONE', ( #17533 ), #12989, .T. ) ;
#44729 = CARTESIAN_POINT ( 'NONE',  ( 11.46989666366029859, 3.941571897678119996, -8.814970315645998866 ) ) ;
#44730 = CARTESIAN_POINT ( 'NONE',  ( 1.700000000000000178, 0.000000000000000000, 0.000000000000000000 ) ) ;
#44731 = CARTESIAN_POINT ( 'NONE',  ( 12.59734647783783856, 1.910499211092021365, -12.56957462197894060 ) ) ;
#44732 = CARTESIAN_POINT ( 'NONE',  ( 12.10533460557258323, -3.815825449682300086, 6.374224726731999802 ) ) ;
#44733 = CARTESIAN_POINT ( 'NONE',  ( 11.23213259636990102, -4.907524392912299582, 7.005495010505599751 ) ) ;
#44734 = EDGE_LOOP ( 'NONE', ( #19427, #26413, #51654, #47755 ) ) ;
#44735 = CARTESIAN_POINT ( 'NONE',  ( 9.833513540183332680, 2.750000000000000000, 7.663624617374469317 ) ) ;
#44736 = VERTEX_POINT ( 'NONE', #6684 ) ;
#44737 = CARTESIAN_POINT ( 'NONE',  ( 7.507480646791999668, -3.501517589953999643, 9.055975309745999624 ) ) ;
#44738 = FACE_OUTER_BOUND ( 'NONE', #14275, .T. ) ;
#44739 = ORIENTED_EDGE ( 'NONE', *, *, #59479, .T. ) ;
#44740 = CARTESIAN_POINT ( 'NONE',  ( 12.51357205051175114, -1.821485253447858055, -12.46764665430163710 ) ) ;
#44741 = CARTESIAN_POINT ( 'NONE',  ( 10.59610807141099897, 4.052703327804870526, 6.360477084256999980 ) ) ;
#44742 = CARTESIAN_POINT ( 'NONE',  ( 23.89320776801300283, 1.894218448783000941, -11.32736289219000270 ) ) ;
#44743 = CARTESIAN_POINT ( 'NONE',  ( 10.83351354018309820, 2.750000000000000000, 7.663624617374469317 ) ) ;
#44744 = CARTESIAN_POINT ( 'NONE',  ( 8.457129882803000598, 5.100036551512999949, -6.571411952062999440 ) ) ;
#44745 = CARTESIAN_POINT ( 'NONE',  ( 9.201637546194751494, 4.272535203994794806, -6.269669426086102781 ) ) ;
#44746 = CARTESIAN_POINT ( 'NONE',  ( 12.21968270649331245, -2.719953125373908875, -13.62430835208222923 ) ) ;
#44747 = CARTESIAN_POINT ( 'NONE',  ( 18.08024441302280039, 0.3389720875425278890, -12.69391532355469110 ) ) ;
#44748 = CARTESIAN_POINT ( 'NONE',  ( 12.30233513030038317, 2.119611855453280569, -12.53231127769398690 ) ) ;
#44749 = CARTESIAN_POINT ( 'NONE',  ( 11.38379707368349969, -4.566644629509899467, -6.509947486183500054 ) ) ;
#44750 = CARTESIAN_POINT ( 'NONE',  ( 9.085767219592000288, 2.821863697211000055, 6.127145479358000024 ) ) ;
#44751 = ORIENTED_EDGE ( 'NONE', *, *, #8369, .F. ) ;
#44752 = CARTESIAN_POINT ( 'NONE',  ( 11.59999999999999964, -4.862088370180456032, -7.912526219123482640 ) ) ;
#44753 = DIRECTION ( 'NONE',  ( -1.000000000000000000, 0.000000000000000000, 0.000000000000000000 ) ) ;
#44754 = CARTESIAN_POINT ( 'NONE',  ( 10.48734600210000067, 4.351287276768000645, -6.182257940481999725 ) ) ;
#44755 = AXIS2_PLACEMENT_3D ( 'NONE', #50341, #30064, #8035 ) ;
#44756 = CARTESIAN_POINT ( 'NONE',  ( 18.01423850902969903, 2.075512308681780382, 12.54039470262457634 ) ) ;
#44757 = CARTESIAN_POINT ( 'NONE',  ( 10.96255537160999971, 5.431623798070999598, 4.905442062451000673 ) ) ;
#44759 = ADVANCED_FACE ( 'NONE', ( #59828 ), #28410, .F. ) ;
#44758 = CARTESIAN_POINT ( 'NONE',  ( 10.52638970730999901, 2.451081172664000274, 6.282749363171999946 ) ) ;
#44760 = CARTESIAN_POINT ( 'NONE',  ( 11.09999999999999964, -0.5000000000000000000, 5.124965750789000296 ) ) ;
#44761 = EDGE_CURVE ( 'NONE', #51740, #58690, #14949, .T. ) ;
#44762 = CARTESIAN_POINT ( 'NONE',  ( 12.75651925146921606, -0.7192569394295693641, -12.57945425907935544 ) ) ;
#44763 = EDGE_CURVE ( 'NONE', #41410, #55747, #27460, .T. ) ;
#44764 = ORIENTED_EDGE ( 'NONE', *, *, #24948, .F. ) ;
#44765 = CARTESIAN_POINT ( 'NONE',  ( 12.19628620791409723, -2.642962752853494912, 12.41715721841834785 ) ) ;
#44766 = CARTESIAN_POINT ( 'NONE',  ( 9.579025935145997650, -4.145841638824199649, -6.506233167833100239 ) ) ;
#44767 = CARTESIAN_POINT ( 'NONE',  ( 9.681187238460999822, 2.612249048987000055, 7.804677627401999551 ) ) ;
#44768 = AXIS2_PLACEMENT_3D ( 'NONE', #1102, #60180, #23109 ) ;
#44769 = CYLINDRICAL_SURFACE ( 'NONE', #49922, 1.000000000000000000 ) ;
#44770 = CARTESIAN_POINT ( 'NONE',  ( 10.66995391537419913, 4.943675741382899780, -8.140910455049299443 ) ) ;
#44771 = CARTESIAN_POINT ( 'NONE',  ( 12.17677020551147393, -0.3597103837128051707, 12.59488153751295769 ) ) ;
#44772 = CARTESIAN_POINT ( 'NONE',  ( 8.149357780409999918, 2.583668273793999770, 6.684750595573999199 ) ) ;
#44773 = CARTESIAN_POINT ( 'NONE',  ( 11.20904666305999875, 5.937823941418000295, 7.147334722859000067 ) ) ;
#44774 = CARTESIAN_POINT ( 'NONE',  ( 12.22973370829435069, 2.255582799352162660, 12.50515469879591102 ) ) ;
#44775 = VERTEX_POINT ( 'NONE', #11757 ) ;
#44776 = CARTESIAN_POINT ( 'NONE',  ( 8.897989158775001073, 4.990139824845000405, -9.121472988377998803 ) ) ;
#44777 = CARTESIAN_POINT ( 'NONE',  ( 10.22272469555899832, 4.639546521693399761, -6.393520617113999549 ) ) ;
#44778 = EDGE_CURVE ( 'NONE', #58012, #55873, #11591, .T. ) ;
#44779 = DIRECTION ( 'NONE',  ( 0.000000000000000000, -0.9835354258236025382, -0.1807154286440004198 ) ) ;
#44781 = DIRECTION ( 'NONE',  ( 1.000000000000000000, 0.000000000000000000, 0.000000000000000000 ) ) ;
#44780 = CARTESIAN_POINT ( 'NONE',  ( 8.560879440379000727, -4.228293421747000735, 8.941387937291999322 ) ) ;
#44782 = CARTESIAN_POINT ( 'NONE',  ( 10.71722949779699974, -3.442773960835399993, 6.664331202173499946 ) ) ;
#44783 = CARTESIAN_POINT ( 'NONE',  ( 10.60441638348510018, -4.841589649988700117, -7.294998899090099798 ) ) ;
#44784 = ORIENTED_EDGE ( 'NONE', *, *, #44118, .T. ) ;
#44785 = CARTESIAN_POINT ( 'NONE',  ( 1.453292983455000131, -2.653487697479000040, 1.892165331686999963 ) ) ;
#44786 = CARTESIAN_POINT ( 'NONE',  ( 23.61437290050061577, -10.18035114601963897, -9.423216756301032504 ) ) ;
#44787 = CARTESIAN_POINT ( 'NONE',  ( 11.09049432275999969, -2.710637143123000303, -5.109752498865000270 ) ) ;
#44788 = CARTESIAN_POINT ( 'NONE',  ( 17.86939907854621978, -3.040585884638498992, 13.54383026114072130 ) ) ;
#44789 = DIRECTION ( 'NONE',  ( 1.000000000000000000, 0.000000000000000000, 0.000000000000000000 ) ) ;
#44790 = CARTESIAN_POINT ( 'NONE',  ( 15.86547101025934126, 8.701845401024112192, 7.746061882573283874 ) ) ;
#44791 = LINE ( 'NONE', #40229, #65441 ) ;
#44792 = CARTESIAN_POINT ( 'NONE',  ( 9.421210490158761885, -5.348867133177450661, 7.442204040579022184 ) ) ;
#44793 = CARTESIAN_POINT ( 'NONE',  ( 10.46029575260939026, 4.828733415692241238, 6.746534734305132730 ) ) ;
#44794 = ORIENTED_EDGE ( 'NONE', *, *, #33625, .T. ) ;
#44795 = CARTESIAN_POINT ( 'NONE',  ( 21.70000133425200062, 3.970157536060000036E-13, -13.99999976176021299 ) ) ;
#44796 = CARTESIAN_POINT ( 'NONE',  ( 11.04798050665000098, 5.246683672049000435, 5.092742987927000975 ) ) ;
#44797 = CARTESIAN_POINT ( 'NONE',  ( 7.420699437778675467, -2.375962897128845785, 8.123829696352604657 ) ) ;
#44798 = CARTESIAN_POINT ( 'NONE',  ( 9.564884880418375701, 5.349923162331274185, -7.500006638304977713 ) ) ;
#44799 = CARTESIAN_POINT ( 'NONE',  ( 1.975310191361000056, 2.864690124100000013, -2.197449004149000462 ) ) ;
#44800 = ORIENTED_EDGE ( 'NONE', *, *, #39187, .T. ) ;
#44801 = CARTESIAN_POINT ( 'NONE',  ( 1.750973465873000068, -3.500000000000000000, 0.000000000000000000 ) ) ;
#44802 = AXIS2_PLACEMENT_3D ( 'NONE', #51696, #56606, #7683 ) ;
#44803 = CARTESIAN_POINT ( 'NONE',  ( 17.87083331331561098, 1.960545027353535863, -12.56104967893682200 ) ) ;
#44804 = CARTESIAN_POINT ( 'NONE',  ( 10.40516904918000129, 5.216391323504000255, 6.765759859247999941 ) ) ;
#44805 = CARTESIAN_POINT ( 'NONE',  ( 10.69872335273220010, 4.349306362047499874, 6.559289673553299060 ) ) ;
#44807 = CARTESIAN_POINT ( 'NONE',  ( 11.59610237318921477, -4.810409949404850671, -7.174950768514437804 ) ) ;
#44806 = VECTOR ( 'NONE', #42099, 1000.000000000000000 ) ;
#44808 = CARTESIAN_POINT ( 'NONE',  ( 6.999999691988000095, 1.243449787579999883E-13, -1.714942017578999994E-13 ) ) ;
#44809 = EDGE_CURVE ( 'NONE', #31174, #26452, #51597, .T. ) ;
#44810 = CARTESIAN_POINT ( 'NONE',  ( 17.60357723836707322, -0.7301778992647969257, -13.98094561311457618 ) ) ;
#44811 = CARTESIAN_POINT ( 'NONE',  ( 12.22262912555220993, -10.88886164594843109, 4.142707164971341172 ) ) ;
#44812 = CARTESIAN_POINT ( 'NONE',  ( 12.39197104280896511, -2.969147788937597010, 12.32981191671119348 ) ) ;
#44813 = ORIENTED_EDGE ( 'NONE', *, *, #41188, .F. ) ;
#44814 = CARTESIAN_POINT ( 'NONE',  ( 7.916096965541012942, 2.414406326178271112, 8.226579130988907806 ) ) ;
#44815 = ORIENTED_EDGE ( 'NONE', *, *, #29333, .T. ) ;
#44816 = CARTESIAN_POINT ( 'NONE',  ( 18.06505946208164559, -2.138585121884149398, 13.74350169411782829 ) ) ;
#44817 = CARTESIAN_POINT ( 'NONE',  ( 10.51810807141099779, -3.940954591493389891, -8.776647962565998995 ) ) ;
#44818 = ORIENTED_EDGE ( 'NONE', *, *, #34689, .T. ) ;
#44819 = VERTEX_POINT ( 'NONE', #31137 ) ;
#44820 = CARTESIAN_POINT ( 'NONE',  ( 10.82035090130999855, 4.758726914843000699, 7.030721746772699454 ) ) ;
#44821 = CARTESIAN_POINT ( 'NONE',  ( 24.52306328733310892, -3.339076862689864811, -12.06942450666826616 ) ) ;
#44822 = CARTESIAN_POINT ( 'NONE',  ( 8.712681907068999365, -4.225805508133200661, -8.364514367444298770 ) ) ;
#44823 = CLOSED_SHELL ( 'NONE', ( #1879, #30895, #21262, #60448, #40668, #32970, #27322, #25614, #48997, #42145, #186, #2076, #785, #48576, #39852, #3603, #2165, #57566, #12618, #15217, #6652, #67487, #8450, #2523 ) ) ;
#44824 = CARTESIAN_POINT ( 'NONE',  ( 9.595493858556999101, 3.928424745541000185, 5.531312048131000303 ) ) ;
#44825 = CARTESIAN_POINT ( 'NONE',  ( 12.75598089126020618, -1.787835849362730434, -13.88537514715539878 ) ) ;
#44826 = CARTESIAN_POINT ( 'NONE',  ( 25.60000000000000142, 9.517611874540000017, 8.103398312166998352 ) ) ;
#44827 = CARTESIAN_POINT ( 'NONE',  ( 11.48394322905000031, 3.487217528443000258, -11.17162453992000160 ) ) ;
#44828 = CARTESIAN_POINT ( 'NONE',  ( 9.910158555493998378, -2.531067292016000003, -7.917737669614999696 ) ) ;
#44829 = LINE ( 'NONE', #28751, #41845 ) ;
#44830 = DIRECTION ( 'NONE',  ( 0.000000000000000000, -0.9421243786071880066, -0.3352635608502960163 ) ) ;
#44831 = VERTEX_POINT ( 'NONE', #24327 ) ;
#44832 = CARTESIAN_POINT ( 'NONE',  ( 0.7106019637973529646, 2.186897047493125523, -2.353682317170576965 ) ) ;
#44833 = SURFACE_STYLE_FILL_AREA ( #51102 ) ;
#44834 = DIRECTION ( 'NONE',  ( 1.000000000000000000, 0.000000000000000000, 0.000000000000000000 ) ) ;
#44835 = CARTESIAN_POINT ( 'NONE',  ( 10.27507144281000073, -4.625210729382000174, 5.003494133775000741 ) ) ;
#44836 = CARTESIAN_POINT ( 'NONE',  ( 5.000030787343000327, 1.290525307673961120, -1.679270695423620952 ) ) ;
#44837 = FACE_OUTER_BOUND ( 'NONE', #18021, .T. ) ;
#44838 = CARTESIAN_POINT ( 'NONE',  ( 12.70233692021770011, 1.883156082608297366, 13.78505115204620068 ) ) ;
#44839 = CARTESIAN_POINT ( 'NONE',  ( 9.980430903642000473, -4.047223565251000466, 9.090364706348999846 ) ) ;
#44840 = ORIENTED_EDGE ( 'NONE', *, *, #68920, .F. ) ;
#44841 = CARTESIAN_POINT ( 'NONE',  ( 10.12947109217999930, 5.100000000000000533, 6.152188490330000370 ) ) ;
#44842 = CARTESIAN_POINT ( 'NONE',  ( 12.22921562908471316, 0.4443071882833232178, 13.99296005428181822 ) ) ;
#44843 = EDGE_CURVE ( 'NONE', #46708, #44139, #36622, .T. ) ;
#44844 = VERTEX_POINT ( 'NONE', #50898 ) ;
#44845 = DIRECTION ( 'NONE',  ( 0.000000000000000000, -1.000000000000000000, 0.000000000000000000 ) ) ;
#44846 = CARTESIAN_POINT ( 'NONE',  ( 10.42914842315198243, -5.349767025452218938, 7.570572966693990047 ) ) ;
#44847 = CARTESIAN_POINT ( 'NONE',  ( 23.73387382971900195, -3.552757729846999890, -13.41925964844999974 ) ) ;
#44848 = CARTESIAN_POINT ( 'NONE',  ( 16.09992084546400193, 8.991497430826001391, 8.719551690569000257 ) ) ;
#44849 = CARTESIAN_POINT ( 'NONE',  ( 8.739954719592999410, 3.122811675949999977, -6.006064052396999919 ) ) ;
#44850 = CARTESIAN_POINT ( 'NONE',  ( 9.948096873516250938, 3.672815144550898303, -8.717465845835395299 ) ) ;
#44851 = CARTESIAN_POINT ( 'NONE',  ( 10.96581858901999951, 7.643649345463000344, -6.313571852796998840 ) ) ;
#44852 = DIRECTION ( 'NONE',  ( 1.000000000000000000, 0.000000000000000000, 0.000000000000000000 ) ) ;
#44853 = VECTOR ( 'NONE', #12663, 1000.000000000000000 ) ;
#44854 = CARTESIAN_POINT ( 'NONE',  ( 24.14469707708988011, 3.678927588120181280, 12.80140320797930187 ) ) ;
#44855 = DIRECTION ( 'NONE',  ( 0.000000000000000000, 1.000000000000000000, 0.000000000000000000 ) ) ;
#44856 = CARTESIAN_POINT ( 'NONE',  ( 9.394730517101999467, -2.624921803719999946, -8.200122328058998988 ) ) ;
#44857 = CARTESIAN_POINT ( 'NONE',  ( 10.33364828895399867, 4.760196147278000112, -7.915211961479200475 ) ) ;
#44858 = CARTESIAN_POINT ( 'NONE',  ( 12.35913603387738036, 0.5748214922496756030, 12.58705572532742600 ) ) ;
#44859 = CARTESIAN_POINT ( 'NONE',  ( 11.35545123989519922, 4.475221369382300196, -8.417769225118700405 ) ) ;
#44860 = ADVANCED_FACE ( 'NONE', ( #23636 ), #13165, .F. ) ;
#44861 = CARTESIAN_POINT ( 'NONE',  ( 9.607317406968999052, 4.212364169857599983, -8.621889436328999068 ) ) ;
#44863 = CARTESIAN_POINT ( 'NONE',  ( 10.28158534179000050, -3.278999312060000282, 4.850220352478999963 ) ) ;
#44862 = CARTESIAN_POINT ( 'NONE',  ( 15.91386961183700244, -8.663061527162000175, -7.870519177131000355 ) ) ;
#44864 = CARTESIAN_POINT ( 'NONE',  ( 23.57687597998769036, -13.36283493320904547, 4.129073899263432601 ) ) ;
#44865 = ORIENTED_EDGE ( 'NONE', *, *, #55982, .T. ) ;
#44866 = EDGE_CURVE ( 'NONE', #48780, #26681, #64090, .T. ) ;
#44867 = CARTESIAN_POINT ( 'NONE',  ( 11.55811496860034815, 5.045590851977999947, 8.035816473382100256 ) ) ;
#44868 = VECTOR ( 'NONE', #30817, 1000.000000000000000 ) ;
#44869 = CARTESIAN_POINT ( 'NONE',  ( 11.18051369187999988, -5.340070732632000272, 8.416150632189001612 ) ) ;
#44870 = CARTESIAN_POINT ( 'NONE',  ( 10.41488779216199845, 4.929030047862200448, 7.164969140522200242 ) ) ;
#44871 = CARTESIAN_POINT ( 'NONE',  ( 10.28877584378239796, 4.466001735846803378, -8.236827240972795394 ) ) ;
#44872 = CARTESIAN_POINT ( 'NONE',  ( 10.40727044253999978, -3.797905333157999941, 5.889909992361999969 ) ) ;
#44873 = CARTESIAN_POINT ( 'NONE',  ( 10.90000000536000080, -2.899999999941999640, -5.157071284930999866 ) ) ;
#44874 = UNCERTAINTY_MEASURE_WITH_UNIT (LENGTH_MEASURE( 1.000000000000000082E-05 ), #66138, 'distance_accuracy_value', 'NONE');
#44875 = EDGE_LOOP ( 'NONE', ( #27494, #23566, #34590, #40308, #68117 ) ) ;
#44876 = CARTESIAN_POINT ( 'NONE',  ( 9.835279731608999043, -3.897539901865500145, -6.362794488108000301 ) ) ;
#44877 = CARTESIAN_POINT ( 'NONE',  ( 23.50387503050299998, 0.000000000000000000, 0.000000000000000000 ) ) ;
#44878 = CARTESIAN_POINT ( 'NONE',  ( 6.175593184917000045, -0.9243234316805000184, -1.323994513613999890 ) ) ;
#44879 = CARTESIAN_POINT ( 'NONE',  ( 7.000000000000000000, 10.55012386388540335, -4.027521431284991849 ) ) ;
#44880 = DIRECTION ( 'NONE',  ( 0.7071067617951957152, 0.000000000000000000, -0.7071068005778986532 ) ) ;
#44881 = CARTESIAN_POINT ( 'NONE',  ( 10.65364694612719809, 3.195501139158400061, -7.821061011719899980 ) ) ;
#44882 = LINE ( 'NONE', #33699, #49877 ) ;
#44883 = CARTESIAN_POINT ( 'NONE',  ( 9.617321917839001699, -3.361793157411000266, -5.915550373431999631 ) ) ;
#44884 = CARTESIAN_POINT ( 'NONE',  ( 17.55505043854147118, -1.875000000000000000, -25.00000000000000000 ) ) ;
#44885 = EDGE_CURVE ( 'NONE', #62603, #14127, #13842, .T. ) ;
#44886 = ORIENTED_EDGE ( 'NONE', *, *, #58310, .F. ) ;
#44887 = DIRECTION ( 'NONE',  ( 1.000000000000000000, 0.000000000000000000, 0.000000000000000000 ) ) ;
#44888 = CARTESIAN_POINT ( 'NONE',  ( 12.09857429938280582, -0.1657344298535316507, -13.99903850390423798 ) ) ;
#44889 = LINE ( 'NONE', #18315, #55560 ) ;
#44890 = CARTESIAN_POINT ( 'NONE',  ( 24.98633618363800224, -8.514521811727000511, -8.479283273084000427 ) ) ;
#44891 = CARTESIAN_POINT ( 'NONE',  ( 10.59184687351642751, -3.000416447002275167, -8.268183399968643599 ) ) ;
#44892 = DIRECTION ( 'NONE',  ( 1.000000000000000000, 0.000000000000000000, 0.000000000000000000 ) ) ;
#44893 = CARTESIAN_POINT ( 'NONE',  ( 13.64718133169100156, 12.21462133634999958, 2.516296819814999974 ) ) ;
#44894 = ORIENTED_EDGE ( 'NONE', *, *, #30497, .T. ) ;
#44895 = VECTOR ( 'NONE', #45330, 1000.000000000000000 ) ;
#44896 = CARTESIAN_POINT ( 'NONE',  ( 23.56666365135700403, 9.114812703021994977, 8.684180617873007435 ) ) ;
#44897 = CARTESIAN_POINT ( 'NONE',  ( 18.17537916830624312, 2.421093501972792605, -13.68989611939600159 ) ) ;
#44898 = ORIENTED_EDGE ( 'NONE', *, *, #15398, .T. ) ;
#44899 = CARTESIAN_POINT ( 'NONE',  ( 25.37957587859375508, -8.342525504610193821, -8.311485206920414370 ) ) ;
#44900 = CARTESIAN_POINT ( 'NONE',  ( 2.561390132543708287, 3.499999999999999112, 0.4581489286485193602 ) ) ;
#44901 = CARTESIAN_POINT ( 'NONE',  ( 9.972410841228999345, 4.357364160690000432, -9.282962013144999247 ) ) ;
#44902 = CARTESIAN_POINT ( 'NONE',  ( 11.09999999999999787, -3.333452946750000478, -8.929141463601279582 ) ) ;
#44903 = CARTESIAN_POINT ( 'NONE',  ( 10.84657802013509986, -5.315911219205999849, -7.469366283838649423 ) ) ;
#44904 = CARTESIAN_POINT ( 'NONE',  ( 17.81145623651324428, 0.5702806495112531238, -12.68276204030717125 ) ) ;
#44905 = B_SPLINE_CURVE_WITH_KNOTS ( 'NONE', 3,
 ( #4200, #41276, #30114, #36369 ),
 .UNSPECIFIED., .F., .F.,
 ( 4, 4 ),
 ( 0.000000000000000000, 1.000000000000000000 ),
 .UNSPECIFIED. ) ;
#44906 = CARTESIAN_POINT ( 'NONE',  ( 10.90833333333529609, -5.360760283596206932, 7.292330520109904235 ) ) ;
#44907 = VERTEX_POINT ( 'NONE', #39037 ) ;
#44908 = CARTESIAN_POINT ( 'NONE',  ( 9.323728576950999880, -3.947350124452999598, 6.051857392047999440 ) ) ;
#44909 = CARTESIAN_POINT ( 'NONE',  ( 18.13614788755254636, -2.730255577220590979, -13.62187136675007082 ) ) ;
#44910 = CARTESIAN_POINT ( 'NONE',  ( 7.100000000000000533, 5.221516520829000640, -8.074802043613001246 ) ) ;
#44911 = VERTEX_POINT ( 'NONE', #54760 ) ;
#44912 = AXIS2_PLACEMENT_3D ( 'NONE', #23167, #28780, #66502 ) ;
#44913 = CARTESIAN_POINT ( 'NONE',  ( 9.949437606643998677, 2.508497579857000392, -7.171862210735000076 ) ) ;
#44914 = DIRECTION ( 'NONE',  ( 1.000000000000000000, 0.000000000000000000, 7.522916419415000070E-14 ) ) ;
#44915 = ORIENTED_EDGE ( 'NONE', *, *, #67347, .T. ) ;
#44916 = CARTESIAN_POINT ( 'NONE',  ( 9.506000818238998562, 2.989704013253000614, 6.967988282883199602 ) ) ;
#44917 = CARTESIAN_POINT ( 'NONE',  ( 18.06277981064212668, -1.966570380498759540, -12.44558849270348944 ) ) ;
#44918 = CARTESIAN_POINT ( 'NONE',  ( 11.75740844561608789, -2.954218652640771214, 7.824999626888802240 ) ) ;
#44919 = FACE_OUTER_BOUND ( 'NONE', #59736, .T. ) ;
#44920 = CARTESIAN_POINT ( 'NONE',  ( 23.56666365135700403, 2.488348886737001386, 11.45224114470000565 ) ) ;
#44921 = CARTESIAN_POINT ( 'NONE',  ( 8.927455549952998837, 4.674761969675400586, 8.044430187461498960 ) ) ;
#44922 = EDGE_CURVE ( 'NONE', #6210, #63228, #63220, .T. ) ;
#44923 = CARTESIAN_POINT ( 'NONE',  ( 7.602384083408999516, -9.083445339000999041, -5.683146030659999681 ) ) ;
#44924 = ADVANCED_FACE ( 'NONE', ( #49511 ), #29245, .F. ) ;
#44925 = ORIENTED_EDGE ( 'NONE', *, *, #68001, .F. ) ;
#44926 = CARTESIAN_POINT ( 'NONE',  ( 9.433148997456999751, 5.167567567567999731, 6.822293592207000934 ) ) ;
#44927 = CARTESIAN_POINT ( 'NONE',  ( 10.50897971959000010, 4.485029564998000318, -9.114435267298000909 ) ) ;
#44928 = CARTESIAN_POINT ( 'NONE',  ( 10.87222337084000046, -5.065783434862999535, -5.123851454306000086 ) ) ;
#44929 = ADVANCED_FACE ( 'NONE', ( #50555 ), #22064, .F. ) ;
#44930 = CARTESIAN_POINT ( 'NONE',  ( 12.27274079034939902, 2.022162746929204058, -13.85319239000171265 ) ) ;
#44931 = CARTESIAN_POINT ( 'NONE',  ( 11.19809687351600047, -3.672815144550895639, 8.717465845835397076 ) ) ;
#44932 = B_SPLINE_CURVE_WITH_KNOTS ( 'NONE', 3,
 ( #56819, #30256, #57151, #30936, #47013, #52252 ),
 .UNSPECIFIED., .F., .F.,
 ( 4, 2, 4 ),
 ( 0.000000000000000000, 0.5000000000000000000, 1.000000000000000000 ),
 .UNSPECIFIED. ) ;
#44933 = CARTESIAN_POINT ( 'NONE',  ( 24.59180944708200300, 3.481108335742999937, 12.13646551132999996 ) ) ;
#44934 = CARTESIAN_POINT ( 'NONE',  ( 17.81092223849609368, -0.6836428945794228440, 13.98330131869062321 ) ) ;
#44935 = DIRECTION ( 'NONE',  ( 0.000000000000000000, -1.000000000000000000, 0.000000000000000000 ) ) ;
#44936 = VERTEX_POINT ( 'NONE', #2314 ) ;
#44937 = VERTEX_POINT ( 'NONE', #44293 ) ;
#44938 = CARTESIAN_POINT ( 'NONE',  ( 9.196339158776000389, 4.112741311853999271, -5.603466076760000192 ) ) ;
#44939 = CARTESIAN_POINT ( 'NONE',  ( 12.47664075725316479, -0.5322329922416514369, 13.88628950328731548 ) ) ;
#44940 = CARTESIAN_POINT ( 'NONE',  ( 12.23612747310287041, -2.758947143698455395, 13.61512400665175981 ) ) ;
#44941 = CARTESIAN_POINT ( 'NONE',  ( 9.199823022402380701, -5.768932760263438375, 7.515113865975768803 ) ) ;
#44942 = CARTESIAN_POINT ( 'NONE',  ( 8.770183059623999355, -3.049610585291000042, 6.392533570808999421 ) ) ;
#44943 = EDGE_CURVE ( 'NONE', #61230, #25637, #31544, .T. ) ;
#44944 = CARTESIAN_POINT ( 'NONE',  ( 19.39373726536100051, -11.26964301940000013, -9.703002290528998444E-14 ) ) ;
#44946 = CARTESIAN_POINT ( 'NONE',  ( 11.12372457444999974, -6.328645827022000070, 5.418228406735999592 ) ) ;
#44945 = CARTESIAN_POINT ( 'NONE',  ( 10.41031740696899810, -3.787635830142400462, 6.378110563671000044 ) ) ;
#44947 = DIRECTION ( 'NONE',  ( 0.000000000000000000, -1.000000000000000000, 0.000000000000000000 ) ) ;
#44948 = ORIENTED_EDGE ( 'NONE', *, *, #28726, .F. ) ;
#44949 = ADVANCED_FACE ( 'NONE', ( #40077 ), #28552, .F. ) ;
#44950 = CARTESIAN_POINT ( 'NONE',  ( 12.80505043854146940, -3.125000000000000000, -12.28373071562070074 ) ) ;
#44951 = CARTESIAN_POINT ( 'NONE',  ( 10.94683815890999945, -2.933330690924000006, -5.178000042639999911 ) ) ;
#44952 = CARTESIAN_POINT ( 'NONE',  ( 11.10000000000000142, 5.421946730020413163, 6.652676983765400287 ) ) ;
#44953 = CARTESIAN_POINT ( 'NONE',  ( 12.41269347227960118, -0.4865065285064677503, 12.68745508179905457 ) ) ;
#44954 = CARTESIAN_POINT ( 'NONE',  ( 18.08677744228779005, -2.828625537410247581, -12.36890451986435124 ) ) ;
#44955 = EDGE_LOOP ( 'NONE', ( #63648, #15516, #11086, #21645, #9018 ) ) ;
#44957 = CARTESIAN_POINT ( 'NONE',  ( 8.856793857978997764, 5.100000000000000533, -6.339888365514000590 ) ) ;
#44956 = DIRECTION ( 'NONE',  ( 0.000000000000000000, 0.000000000000000000, -1.000000000000000000 ) ) ;
#44958 = CARTESIAN_POINT ( 'NONE',  ( 9.649770280412001355, 4.042991257420999851, -5.768106221333000327 ) ) ;
#44959 = CARTESIAN_POINT ( 'NONE',  ( 12.36772010770948249, -2.053374490018978538, 13.75810180220398671 ) ) ;
#44960 = CARTESIAN_POINT ( 'NONE',  ( 10.66579975933730040, 5.208485784810999775, 7.915786590091300035 ) ) ;
#44961 = AXIS2_PLACEMENT_3D ( 'NONE', #46254, #67218, #55366 ) ;
#44962 = CARTESIAN_POINT ( 'NONE',  ( 8.599999986286999132, 4.750000013710600655, -7.500000000038047787 ) ) ;
#44963 = DIRECTION ( 'NONE',  ( -1.000000000000000000, 0.000000000000000000, 0.000000000000000000 ) ) ;
#44964 = CARTESIAN_POINT ( 'NONE',  ( 3.442447097232000264, 1.741959211826000109, -3.162405688284999794 ) ) ;
#44965 = ORIENTED_EDGE ( 'NONE', *, *, #53541, .F. ) ;
#44966 = CARTESIAN_POINT ( 'NONE',  ( 12.17677020551147038, 0.3597103837127930692, -12.59488153751296657 ) ) ;
#44967 = CARTESIAN_POINT ( 'NONE',  ( 7.809516811409829451, -3.056020742931339296, 6.488504755083804199 ) ) ;
#44968 = CARTESIAN_POINT ( 'NONE',  ( 11.06697824069853375, -2.733021759301466069, 6.467485083839107141 ) ) ;
#44969 = CARTESIAN_POINT ( 'NONE',  ( 10.88314899746000108, -5.167567567567999731, 6.822293592207000934 ) ) ;
#44970 = ORIENTED_EDGE ( 'NONE', *, *, #1973, .F. ) ;
#44971 = CARTESIAN_POINT ( 'NONE',  ( 5.672919488924000220, 1.281289678559000000, 0.3267609307802000207 ) ) ;
#44972 = CARTESIAN_POINT ( 'NONE',  ( 8.385635841226999787, 2.841678116489999795, -6.718113446527000931 ) ) ;
#44974 = CARTESIAN_POINT ( 'NONE',  ( 10.60664092702282346, 5.179495029648225390, -8.179803431736248243 ) ) ;
#44973 = CARTESIAN_POINT ( 'NONE',  ( 8.576023037351861333, -4.025143239269920237, 5.760539197808133061 ) ) ;
#44975 = CARTESIAN_POINT ( 'NONE',  ( 10.62452888361057113, -4.871957554394390044, -7.561478660064198110 ) ) ;
#44976 = VERTEX_POINT ( 'NONE', #49862 ) ;
#44977 = CARTESIAN_POINT ( 'NONE',  ( 9.736871746126999128, -2.742172332680000046, 6.839224809731999422 ) ) ;
#44978 = VERTEX_POINT ( 'NONE', #18058 ) ;
#44979 = DIRECTION ( 'NONE',  ( -1.000000000000000000, 0.000000000000000000, 0.000000000000000000 ) ) ;
#44980 = CARTESIAN_POINT ( 'NONE',  ( 24.87152730243871446, -8.583156850595695886, -8.460088049133823063 ) ) ;
#44981 = CARTESIAN_POINT ( 'NONE',  ( 17.93874521385978937, 0.6200266137005103761, -13.98626978124057629 ) ) ;
#44982 = EDGE_CURVE ( 'NONE', #5301, #52724, #14183, .T. ) ;
#44983 = EDGE_CURVE ( 'NONE', #15150, #7244, #25718, .T. ) ;
#44984 = ORIENTED_EDGE ( 'NONE', *, *, #41712, .T. ) ;
#44985 = CARTESIAN_POINT ( 'NONE',  ( 10.94064497426557558, 9.306490196098094358, -6.239143843092519681 ) ) ;
#44986 = PLANE ( 'NONE',  #28279 ) ;
#44987 = CARTESIAN_POINT ( 'NONE',  ( 7.292164158769000259, 2.863733890340999899, -8.313606627241000524 ) ) ;
#44988 = CARTESIAN_POINT ( 'NONE',  ( 20.10000000000000142, -11.84999999999999964, 0.000000000000000000 ) ) ;
#44989 = CARTESIAN_POINT ( 'NONE',  ( 11.52319144466311052, -2.880026002252477291, 7.175010281093781472 ) ) ;
#44990 = ORIENTED_EDGE ( 'NONE', *, *, #63113, .F. ) ;
#44991 = CARTESIAN_POINT ( 'NONE',  ( 9.587288403116620117, 2.899999999999999911, -6.305985889556955826 ) ) ;
#44992 = CARTESIAN_POINT ( 'NONE',  ( 12.39223264510079758, -2.969378069107369456, -13.56257646889492285 ) ) ;
#44993 = CARTESIAN_POINT ( 'NONE',  ( 9.893930206848997599, 2.750000000000000000, 7.500000000000000000 ) ) ;
#44994 = CYLINDRICAL_SURFACE ( 'NONE', #28140, 1.250000000000000222 ) ;
#44995 = ORIENTED_EDGE ( 'NONE', *, *, #13444, .T. ) ;
#44996 = DIRECTION ( 'NONE',  ( 0.000000000000000000, 0.000000000000000000, -1.000000000000000000 ) ) ;
#44997 = CARTESIAN_POINT ( 'NONE',  ( 8.216851002544000693, -2.832432432432000269, 6.822293592207000934 ) ) ;
#44998 = DIRECTION ( 'NONE',  ( 0.000000000000000000, 1.000000000000000000, 0.000000000000000000 ) ) ;
#44999 = CARTESIAN_POINT ( 'NONE',  ( 25.29986325275000070, 2.078227429405999693, 11.31065739696999906 ) ) ;
#45000 = CARTESIAN_POINT ( 'NONE',  ( 12.78089695109148494, -1.787798027819077040, -13.88537998392834893 ) ) ;
#45001 = CARTESIAN_POINT ( 'NONE',  ( 12.64263601961789085, -0.6038715862870278617, -13.88233985103438251 ) ) ;
#45002 = CARTESIAN_POINT ( 'NONE',  ( 17.94557471909619295, -2.987998163485180214, 12.32438680867657332 ) ) ;
#45003 = ORIENTED_EDGE ( 'NONE', *, *, #3608, .F. ) ;
#45004 = ADVANCED_FACE ( 'NONE', ( #20796 ), #11055, .F. ) ;
#45005 = CARTESIAN_POINT ( 'NONE',  ( 10.51925056272499859, -2.825232917634000085, -7.517410630436119234 ) ) ;
#45006 = EDGE_CURVE ( 'NONE', #43226, #16623, #19420, .T. ) ;
#45007 = ORIENTED_EDGE ( 'NONE', *, *, #32740, .T. ) ;
#45008 = CIRCLE ( 'NONE', #8169, 0.5000000000000004441 ) ;
#45009 = FACE_OUTER_BOUND ( 'NONE', #17183, .T. ) ;
#45010 = CARTESIAN_POINT ( 'NONE',  ( 9.825045280412000537, 3.116293075258000478, -6.208411413796000033 ) ) ;
#45011 = EDGE_CURVE ( 'NONE', #60701, #44355, #66579, .T. ) ;
#45012 = CARTESIAN_POINT ( 'NONE',  ( 2.412568162807000149, -1.368190713007999992, 2.909400328758999787 ) ) ;
#45013 = CARTESIAN_POINT ( 'NONE',  ( 10.10656447933000024, -4.887648864398999926, -6.257283015674000026 ) ) ;
#45014 = CARTESIAN_POINT ( 'NONE',  ( 6.875386523732225363, 1.468717224916136654, 0.3829316497910061345 ) ) ;
#45015 = CARTESIAN_POINT ( 'NONE',  ( 7.798085185677998687, 3.459333709783000366, -6.382131374430003667 ) ) ;
#45016 = CARTESIAN_POINT ( 'NONE',  ( 3.999999855301999752, 0.000000000000000000, 0.000000000000000000 ) ) ;
#45017 = ORIENTED_EDGE ( 'NONE', *, *, #37583, .T. ) ;
#45018 = CARTESIAN_POINT ( 'NONE',  ( 10.78441772631200024, -3.627481539113199815, 6.733203680593099705 ) ) ;
#45019 = CARTESIAN_POINT ( 'NONE',  ( 10.15293113568789352, 5.100000000000000533, -6.444141223401127938 ) ) ;
#45020 = CARTESIAN_POINT ( 'NONE',  ( 10.66714959198803570, -5.079709024443942234, -8.329714913667055853 ) ) ;
#45021 = CARTESIAN_POINT ( 'NONE',  ( 8.883148997460001084, -5.167567567567999731, 6.822293592207000934 ) ) ;
#45022 = CARTESIAN_POINT ( 'NONE',  ( 9.218008530890955399, 2.655297806746307554, 7.619097669105685533 ) ) ;
#45023 = CARTESIAN_POINT ( 'NONE',  ( 10.53057053952199951, 3.659587858614300249, -6.703496287302799672 ) ) ;
#45024 = EDGE_CURVE ( 'NONE', #49108, #33013, #59891, .T. ) ;
#45025 = CARTESIAN_POINT ( 'NONE',  ( 24.85114900759599976, -11.95312945982000130, 2.993324385169999768 ) ) ;
#45026 = CARTESIAN_POINT ( 'NONE',  ( 8.880265421554998539, 3.785712956512099936, -8.608472884860999486 ) ) ;
#45027 = CARTESIAN_POINT ( 'NONE',  ( 18.02418542278644153, -0.5485298171726814553, 12.58805670501782181 ) ) ;
#45028 = CARTESIAN_POINT ( 'NONE',  ( 24.60320129348500018, 3.644628662557000354, 12.27776523668999786 ) ) ;
#45029 = CARTESIAN_POINT ( 'NONE',  ( 0.8685892898898377457, -0.3281013245661921207, -3.507234403409725587 ) ) ;
#45030 = CARTESIAN_POINT ( 'NONE',  ( 10.23581084123000018, 3.621841509808999771, -8.806208131805998818 ) ) ;
#45031 = ORIENTED_EDGE ( 'NONE', *, *, #303, .T. ) ;
#45032 = CARTESIAN_POINT ( 'NONE',  ( 7.330275273710999961, -4.426925773067000414, 9.293310812901001583 ) ) ;
#45033 = AXIS2_PLACEMENT_3D ( 'NONE', #14206, #9978, #20128 ) ;
#45034 = CARTESIAN_POINT ( 'NONE',  ( 17.87892170566133032, 1.864264957476230222, 13.87532524069350082 ) ) ;
#45035 = FACE_OUTER_BOUND ( 'NONE', #25431, .T. ) ;
#45036 = CARTESIAN_POINT ( 'NONE',  ( 10.05041772631199848, -3.450375740502100275, -8.631352948887998977 ) ) ;
#45037 = ORIENTED_EDGE ( 'NONE', *, *, #25253, .F. ) ;
#45038 = VECTOR ( 'NONE', #44082, 1000.000000000000114 ) ;
#45039 = CARTESIAN_POINT ( 'NONE',  ( 8.513426658773999733, 5.040787533781999841, 8.522957620707000359 ) ) ;
#45041 = FACE_OUTER_BOUND ( 'NONE', #63501, .T. ) ;
#45040 = CARTESIAN_POINT ( 'NONE',  ( 18.90826270587400160, 0.000000000000000000, 0.000000000000000000 ) ) ;
#45042 = CARTESIAN_POINT ( 'NONE',  ( 10.94846415877000112, 3.841064079579000090, -9.341816855317999213 ) ) ;
#45043 = VERTEX_POINT ( 'NONE', #20108 ) ;
#45044 = CARTESIAN_POINT ( 'NONE',  ( 9.298033738970000073, 4.087077023028999001, 9.429414864145000408 ) ) ;
#45045 = CARTESIAN_POINT ( 'NONE',  ( 17.55505043854147118, -3.248147246781389885, -13.61798588129780896 ) ) ;
#45046 = CARTESIAN_POINT ( 'NONE',  ( 11.55610404293055993, 3.497163090439000310, 6.476063885290000322 ) ) ;
#45047 = CARTESIAN_POINT ( 'NONE',  ( 11.09648096125000016, -3.099777420064000033, 6.097103007060000301 ) ) ;
#45048 = CARTESIAN_POINT ( 'NONE',  ( 7.453125355210004521, 3.231590054310000237, 6.459270056246999125 ) ) ;
#45049 = VERTEX_POINT ( 'NONE', #3337 ) ;
#45050 = CARTESIAN_POINT ( 'NONE',  ( 11.83124374198900064, -3.528976724670999765, 11.96046730081999954 ) ) ;
#45051 = CARTESIAN_POINT ( 'NONE',  ( 17.55505043854143565, 3.248147246781390329, 13.61798588129781074 ) ) ;
#45052 = CARTESIAN_POINT ( 'NONE',  ( 7.914911323226687223, -2.423414753718124093, 8.235095959117245457 ) ) ;
#45053 = CONICAL_SURFACE ( 'NONE', #46149, 0.4377388725247000623, 0.7853981633972997312 ) ;
#45054 = CARTESIAN_POINT ( 'NONE',  ( 10.96580795178999956, -4.930647899304999804, 6.170539049947000088 ) ) ;
#45055 = CARTESIAN_POINT ( 'NONE',  ( 11.75203632436369894, -5.109717061557999429, -7.240848640331599917 ) ) ;
#45056 = CARTESIAN_POINT ( 'NONE',  ( 10.58857120343300018, -4.055348968344419269, 6.359530327585999565 ) ) ;
#45057 = ORIENTED_EDGE ( 'NONE', *, *, #46095, .F. ) ;
#45058 = CARTESIAN_POINT ( 'NONE',  ( 21.49999863197000138, 0.000000000000000000, 0.000000000000000000 ) ) ;
#45059 = CARTESIAN_POINT ( 'NONE',  ( 10.84995525820099971, -4.107710726525199973, 8.635644537520001052 ) ) ;
#45060 = ORIENTED_EDGE ( 'NONE', *, *, #24000, .F. ) ;
#45061 = CARTESIAN_POINT ( 'NONE',  ( 9.120226521874423398, -5.092799636466279090, -6.532201274827058590 ) ) ;
#45062 = AXIS2_PLACEMENT_3D ( 'NONE', #23927, #19978, #46889 ) ;
#45063 = ORIENTED_EDGE ( 'NONE', *, *, #67214, .F. ) ;
#45064 = EDGE_CURVE ( 'NONE', #13467, #57524, #57410, .T. ) ;
#45065 = EDGE_CURVE ( 'NONE', #14617, #3072, #59225, .T. ) ;
#45066 = CARTESIAN_POINT ( 'NONE',  ( 9.974327024990000012, -5.476443305113000370, -7.051545409824000465 ) ) ;
#45067 = CARTESIAN_POINT ( 'NONE',  ( 8.456370280410999030, 2.836879604150999601, -8.783908972046001296 ) ) ;
#45068 = CARTESIAN_POINT ( 'NONE',  ( 9.433536308084699229, -2.899999999999999911, -6.665341197421564168 ) ) ;
#45069 = CARTESIAN_POINT ( 'NONE',  ( 8.237102957402385073, 4.936199535989180376, 6.266989881494448689 ) ) ;
#45070 = CARTESIAN_POINT ( 'NONE',  ( 12.51690604397273887, 1.945290150052898515, -12.56367745121460011 ) ) ;
#45071 = CARTESIAN_POINT ( 'NONE',  ( 11.00180110216400031, -4.856393875115199599, 8.023010882787499298 ) ) ;
#45072 = CARTESIAN_POINT ( 'NONE',  ( 12.06833327354034857, -4.746587807672299597, 7.988332985010599963 ) ) ;
#45073 = ORIENTED_EDGE ( 'NONE', *, *, #46900, .T. ) ;
#45074 = B_SPLINE_CURVE_WITH_KNOTS ( 'NONE', 3,
 ( #40916, #67475, #29070, #23805 ),
 .UNSPECIFIED., .F., .F.,
 ( 4, 4 ),
 ( 0.000000000000000000, 0.2509294615239107684 ),
 .UNSPECIFIED. ) ;
#45075 = CARTESIAN_POINT ( 'NONE',  ( 9.226510893196484986, 2.899999999999999911, -6.310481362401603178 ) ) ;
#45076 = ORIENTED_EDGE ( 'NONE', *, *, #13767, .F. ) ;
#45077 = CARTESIAN_POINT ( 'NONE',  ( 8.277730646792999636, -4.874569256861000177, 6.119503992241999590 ) ) ;
#45078 = CARTESIAN_POINT ( 'NONE',  ( 18.27990784067583618, 0.1916560647487305369, 13.99999316327169119 ) ) ;
#45079 = ORIENTED_EDGE ( 'NONE', *, *, #58109, .F. ) ;
#45080 = CARTESIAN_POINT ( 'NONE',  ( 12.29711362085067528, -1.966768764679983184, -12.44555721978030860 ) ) ;
#45081 = CARTESIAN_POINT ( 'NONE',  ( 11.28533594839949750, 4.750012929834699804, 8.359517726022600570 ) ) ;
#45082 = CARTESIAN_POINT ( 'NONE',  ( 23.60205915885299888, 2.504446818059999469, -12.27382285987999211 ) ) ;
#45083 = DIRECTION ( 'NONE',  ( 0.8843050080896639464, -0.1786785916254929885, 0.4313683038451824325 ) ) ;
#45084 = CARTESIAN_POINT ( 'NONE',  ( 7.621422090919002912, 4.588776658069999570, 6.481258258681996232 ) ) ;
#45085 = CARTESIAN_POINT ( 'NONE',  ( 9.262620115046999558, 3.343122245339613663, -6.424592926396654136 ) ) ;
#45086 = CARTESIAN_POINT ( 'NONE',  ( 12.18011073905427111, -2.522020058064991410, -13.66873259811635677 ) ) ;
#45087 = CARTESIAN_POINT ( 'NONE',  ( 18.10141690196193309, 0.3036663359794742334, -12.69511825016613749 ) ) ;
#45088 = CARTESIAN_POINT ( 'NONE',  ( 8.716851002545999094, 2.832432432432000269, 6.822293592207000934 ) ) ;
#45089 = CARTESIAN_POINT ( 'NONE',  ( 11.30579707368350029, -4.634832087857400751, -6.390809033205999690 ) ) ;
#45090 = CARTESIAN_POINT ( 'NONE',  ( 7.839801658770999992, 3.084076314893000159, 9.259847992573000397 ) ) ;
#45091 = ORIENTED_EDGE ( 'NONE', *, *, #17843, .F. ) ;
#45092 = VECTOR ( 'NONE', #15760, 1000.000000000000114 ) ;
#45093 = CARTESIAN_POINT ( 'NONE',  ( 12.10000669845703847, -11.02846243759423039, 3.754394857303111621 ) ) ;
#45094 = CARTESIAN_POINT ( 'NONE',  ( 7.413218301918568010, 4.974493527912905222, 6.530297539223000491 ) ) ;
#45095 = EDGE_CURVE ( 'NONE', #21396, #59370, #57805, .T. ) ;
#45096 = CARTESIAN_POINT ( 'NONE',  ( 10.17309652395999997, 4.709165316578000748, -8.664874001714000684 ) ) ;
#45097 = CARTESIAN_POINT ( 'NONE',  ( 17.59659105803583756, 1.876041592512284195, 12.57524627323323330 ) ) ;
#45098 = CARTESIAN_POINT ( 'NONE',  ( 18.26281727343199890, 2.856883730594999893, -11.95041273044000008 ) ) ;
#45099 = CARTESIAN_POINT ( 'NONE',  ( 10.71256887705999894, 5.951815279772000089, 7.233043586354999555 ) ) ;
#45100 = CARTESIAN_POINT ( 'NONE',  ( 11.42394752546313441, -4.702246198360438889, -8.603859202887296220 ) ) ;
#45101 = CARTESIAN_POINT ( 'NONE',  ( 12.15889392793075530, -0.3761765223121792956, -12.59508068834428052 ) ) ;
#45102 = ORIENTED_EDGE ( 'NONE', *, *, #35996, .F. ) ;
#45103 = CARTESIAN_POINT ( 'NONE',  ( 12.59734647783787409, -1.910499211092022476, 12.56957462197894415 ) ) ;
#45104 = CARTESIAN_POINT ( 'NONE',  ( 9.931621437244999129, -3.424116261072899903, -6.851875117168399143 ) ) ;
#45105 = CARTESIAN_POINT ( 'NONE',  ( 10.20319667131999886, 3.421760346951000287, 6.017732782098999422 ) ) ;
#45106 = FACE_OUTER_BOUND ( 'NONE', #39455, .T. ) ;
#45107 = CARTESIAN_POINT ( 'NONE',  ( 10.42380110216399913, 3.026453990125600235, -6.905442784147899360 ) ) ;
#45108 = EDGE_CURVE ( 'NONE', #51664, #23524, #13231, .T. ) ;
#45109 = CARTESIAN_POINT ( 'NONE',  ( 12.41256632787946756, 0.4864235087029698534, 12.68745975172790530 ) ) ;
#45110 = VECTOR ( 'NONE', #18958, 1000.000000000000000 ) ;
#45111 = CARTESIAN_POINT ( 'NONE',  ( 8.545864158774001851, 3.856772556595000179, 5.521246073317000125 ) ) ;
#45112 = CARTESIAN_POINT ( 'NONE',  ( 9.566963020987998334, 5.215925787220999865, 6.177726425586999248 ) ) ;
#45113 = CARTESIAN_POINT ( 'NONE',  ( 12.32534826942432282, 2.099231811413890814, 12.53595023114330331 ) ) ;
#45114 = EDGE_LOOP ( 'NONE', ( #48336, #62043, #12897, #62834 ) ) ;
#45115 = AXIS2_PLACEMENT_3D ( 'NONE', #49769, #59213, #44546 ) ;
#45116 = CARTESIAN_POINT ( 'NONE',  ( 25.47132167539000136, 8.417332019620999972, 7.979435755108000627 ) ) ;
#45117 = CARTESIAN_POINT ( 'NONE',  ( 11.18272066707849888, 5.093522884867000222, -6.838543969064300398 ) ) ;
#45118 = CARTESIAN_POINT ( 'NONE',  ( 5.452606837613999780, -0.4199405305951999789, 1.440017343911000003 ) ) ;
#45120 = CARTESIAN_POINT ( 'NONE',  ( 17.94293909943462850, -0.4900986450237151959, 12.68726951834787897 ) ) ;
#45119 = CARTESIAN_POINT ( 'NONE',  ( 7.662254440376999653, -2.688354259407999880, 8.140021027181001401 ) ) ;
#45121 = CARTESIAN_POINT ( 'NONE',  ( 10.13465911260399999, -4.436443689698799986, 6.595367916746299741 ) ) ;
#45122 = CARTESIAN_POINT ( 'NONE',  ( 11.73671932425159881, -4.127012898954600217, -8.356835045446798560 ) ) ;
#45123 = ORIENTED_EDGE ( 'NONE', *, *, #48052, .F. ) ;
#45124 = CARTESIAN_POINT ( 'NONE',  ( 0.8715629140400000807, 2.401393137604999950, -2.383704365015999915 ) ) ;
#45125 = CARTESIAN_POINT ( 'NONE',  ( 18.04536347370801508, -0.3876168848819628310, -12.69203885981792368 ) ) ;
#45126 = CARTESIAN_POINT ( 'NONE',  ( 11.05503063675000064, -2.753313764949999687, -5.052995050064000182 ) ) ;
#45127 = CARTESIAN_POINT ( 'NONE',  ( 17.88876225152345611, -3.028809290952733324, 13.54697662062045005 ) ) ;
#45128 = CARTESIAN_POINT ( 'NONE',  ( 24.25374608244400321, -12.19813778996000053, 3.308085337617999944 ) ) ;
#45129 = CARTESIAN_POINT ( 'NONE',  ( 4.900006121742000786, -2.000000000000001332, -0.2617993877991417473 ) ) ;
#45130 = CARTESIAN_POINT ( 'NONE',  ( 6.999999691988000095, -1.865174681369999698E-13, 1.040631529540999901E-13 ) ) ;
#45131 = LINE ( 'NONE', #60513, #13205 ) ;
#45132 = CARTESIAN_POINT ( 'NONE',  ( 13.37677363193000168, -12.31133347089000019, -1.988942882797000156 ) ) ;
#45133 = VERTEX_POINT ( 'NONE', #53300 ) ;
#45134 = CARTESIAN_POINT ( 'NONE',  ( 9.459510841229999301, 5.445214367171999470, 7.703373622193999459 ) ) ;
#45135 = CARTESIAN_POINT ( 'NONE',  ( 8.970944094206998898, -5.100000000000000533, 6.571291218949999902 ) ) ;
#45136 = CARTESIAN_POINT ( 'NONE',  ( 7.432865048533964014, -2.297794684850921421, 7.857475797735035350 ) ) ;
#45137 = VECTOR ( 'NONE', #55507, 1000.000000000000000 ) ;
#45138 = CARTESIAN_POINT ( 'NONE',  ( 10.71480780573668312, -2.649489222497538599, 7.676606295960795912 ) ) ;
#45139 = CARTESIAN_POINT ( 'NONE',  ( 0.8420640498653999551, -3.400502393318999950, 1.157769971473999959 ) ) ;
#45140 = ORIENTED_EDGE ( 'NONE', *, *, #3629, .T. ) ;
#45141 = CARTESIAN_POINT ( 'NONE',  ( 10.65673534980369119, 5.179482957638356311, -8.179835726794676631 ) ) ;
#45142 = CARTESIAN_POINT ( 'NONE',  ( 11.79999999684100054, -12.15995044155999949, -2.000340912084999978 ) ) ;
#45143 = CARTESIAN_POINT ( 'NONE',  ( 9.444315208305999576, 2.927258006877999641, 8.897018628538001295 ) ) ;
#45144 = CARTESIAN_POINT ( 'NONE',  ( 10.57564694612699974, 3.068007311611700150, 7.128058497017000228 ) ) ;
#45145 = EDGE_CURVE ( 'NONE', #52892, #49685, #9866, .T. ) ;
#45146 = EDGE_CURVE ( 'NONE', #11513, #57880, #27282, .T. ) ;
#45147 = DIRECTION ( 'NONE',  ( 0.000000000000000000, -0.3352635608502960163, -0.9421243786071880066 ) ) ;
#45148 = CARTESIAN_POINT ( 'NONE',  ( 10.16007944038000055, -4.812966563646999596, -8.526591612524001107 ) ) ;
#45149 = CYLINDRICAL_SURFACE ( 'NONE', #42252, 11.84999999999999964 ) ;
#45150 = EDGE_CURVE ( 'NONE', #68281, #68269, #33971, .T. ) ;
#45151 = EDGE_CURVE ( 'NONE', #16325, #68200, #3131, .T. ) ;
#45152 = LINE ( 'NONE', #33279, #8694 ) ;
#45153 = CARTESIAN_POINT ( 'NONE',  ( 12.31573549172491866, -2.888971355233717286, 12.35241121500909856 ) ) ;
#45154 = CARTESIAN_POINT ( 'NONE',  ( 7.938548115121596638, 2.267677432809916294, 7.755639217155871457 ) ) ;
#45155 = AXIS2_PLACEMENT_3D ( 'NONE', #43853, #2917, #2575 ) ;
#45156 = ORIENTED_EDGE ( 'NONE', *, *, #55635, .F. ) ;
#45157 = CARTESIAN_POINT ( 'NONE',  ( 17.96192083627962788, -2.025460433975771579, 13.76272661095429228 ) ) ;
#45158 = CARTESIAN_POINT ( 'NONE',  ( 10.86272200990529946, -5.206705454565000224, -7.079074440652799893 ) ) ;
#45159 = ORIENTED_EDGE ( 'NONE', *, *, #24656, .T. ) ;
#45160 = VERTEX_POINT ( 'NONE', #16232 ) ;
#45161 = CARTESIAN_POINT ( 'NONE',  ( 10.90346005378009941, 4.786957292481900161, 7.920222357891399945 ) ) ;
#45162 = CARTESIAN_POINT ( 'NONE',  ( 9.604346873516666605, 5.250000000000001776, -7.336375382625535124 ) ) ;
#45164 = CARTESIAN_POINT ( 'NONE',  ( 12.80505043854143388, 3.149917237299187267, -12.25147871603038219 ) ) ;
#45163 = AXIS2_PLACEMENT_3D ( 'NONE', #37307, #58982, #27866 ) ;
#45165 = DIRECTION ( 'NONE',  ( 1.000000000000000000, 0.000000000000000000, 0.000000000000000000 ) ) ;
#45166 = CARTESIAN_POINT ( 'NONE',  ( 10.25165889348999926, 3.418644779562000302, -8.733642166016998942 ) ) ;
#45167 = CARTESIAN_POINT ( 'NONE',  ( 16.26901036074197648, -3.345264657739864589, -11.86070554647184316 ) ) ;
#45168 = CARTESIAN_POINT ( 'NONE',  ( 9.660528907822998335, 2.899999999999999911, -6.152188490330000370 ) ) ;
#45169 = CARTESIAN_POINT ( 'NONE',  ( 17.64985999057966026, 0.7135009822675021374, -12.57978225961209162 ) ) ;
#45170 = CARTESIAN_POINT ( 'NONE',  ( 10.48414299032999963, -4.098653366703000067, -9.351353705206001621 ) ) ;
#45171 = CARTESIAN_POINT ( 'NONE',  ( 11.71210404293059959, -4.381818659177399766, -8.277504409418298792 ) ) ;
#45172 = FILL_AREA_STYLE_COLOUR ( '', #17705 ) ;
#45173 = ORIENTED_EDGE ( 'NONE', *, *, #41512, .T. ) ;
#45174 = ADVANCED_FACE ( 'NONE', ( #64456 ), #7555, .F. ) ;
#45175 = B_SPLINE_CURVE_WITH_KNOTS ( 'NONE', 3,
 ( #49094, #49434, #19699, #2246, #66203, #7833, #23559, #14458, #13084, #56065, #57092, #51173, #39648, #56414, #51504, #35778, #44900, #14114 ),
 .UNSPECIFIED., .F., .F.,
 ( 4, 2, 2, 2, 2, 2, 2, 2, 4 ),
 ( 0.000000000000000000, 0.1250000000000000278, 0.2500000000000000000, 0.3749999999999999445, 0.4999999999999999445, 0.6249999999999998890, 0.7499999999999998890, 0.8750000000000000000, 1.000000000000000000 ),
 .UNSPECIFIED. ) ;
#45176 = DIRECTION ( 'NONE',  ( 0.000000000000000000, 1.000000000000000000, 0.000000000000000000 ) ) ;
#45177 = PLANE ( 'NONE',  #4603 ) ;
#45178 = DIRECTION ( 'NONE',  ( -0.000000000000000000, 0.7270098363383213913, 0.6866270442294909460 ) ) ;
#45179 = CARTESIAN_POINT ( 'NONE',  ( 10.46957120343300041, 3.937990586507050139, -8.777708647662999297 ) ) ;
#45180 = CARTESIAN_POINT ( 'NONE',  ( 12.61529649622812954, 3.223097538158945952, 13.62393827815043501 ) ) ;
#45181 = CARTESIAN_POINT ( 'NONE',  ( 11.18706725482999964, -3.186788126275999833, 6.232699537089999353 ) ) ;
#45182 = VERTEX_POINT ( 'NONE', #11327 ) ;
#45183 = CARTESIAN_POINT ( 'NONE',  ( 12.66329582868160131, 0.6090237436409963179, -12.68033599931248290 ) ) ;
#45184 = CARTESIAN_POINT ( 'NONE',  ( 12.42469545966024214, -0.4960449563116401950, 13.88808666890938248 ) ) ;
#45185 = ORIENTED_EDGE ( 'NONE', *, *, #44142, .T. ) ;
#45186 = CARTESIAN_POINT ( 'NONE',  ( 11.04384236319999957, 7.001054304361000291, 5.879104636179000032 ) ) ;
#45187 = DIRECTION ( 'NONE',  ( 1.000000000000000000, 0.000000000000000000, 0.000000000000000000 ) ) ;
#45188 = CARTESIAN_POINT ( 'NONE',  ( 8.796304629759626792, 4.535214477905362251, 6.807845768027799060 ) ) ;
#45189 = CARTESIAN_POINT ( 'NONE',  ( 12.80505043854143388, 1.875000000000000000, -25.00000000000000000 ) ) ;
#45190 = B_SPLINE_CURVE_WITH_KNOTS ( 'NONE', 3,
 ( #31355, #21881, #37965, #5115 ),
 .UNSPECIFIED., .F., .F.,
 ( 4, 4 ),
 ( 0.000000000000000000, 1.000000000000000000 ),
 .UNSPECIFIED. ) ;
#45191 = B_SPLINE_SURFACE_WITH_KNOTS ( 'NONE', 3, 3, ( 
 ( #58171, #47688, #10272, #52927 ),
 ( #5023, #42436, #5372, #37189 ),
 ( #58508, #60587, #13396, #2541 ),
 ( #34718, #44863, #34375, #17596 ),
 ( #29131, #33333, #23176, #1509 ),
 ( #34029, #45205, #28789, #66510 ),
 ( #50100, #17944, #43822, #12692 ),
 ( #66169, #55694, #23868, #22827 ),
 ( #7791, #65820, #39264, #44175 ),
 ( #65119, #44525, #27746, #22480 ),
 ( #55342, #7438, #18632, #39961 ) ),
 .UNSPECIFIED., .F., .F., .F.,
 ( 4, 1, 1, 1, 1, 1, 1, 1, 4 ),
 ( 4, 4 ),
 ( -0.01601554030910999973, 0.000000000000000000, 0.06250000000000000000, 0.1250000000000000000, 0.1875000000000000000, 0.2500000000000000000, 0.3125000000000000000, 0.3750000000000000000, 0.4240941240803000056 ),
 ( -0.1689889244683999980, 1.168921279219000020 ),
 .UNSPECIFIED. ) ;
#45192 = ADVANCED_FACE ( 'NONE', ( #37219 ), #158, .T. ) ;
#45193 = DIRECTION ( 'NONE',  ( 1.000000000000000000, 0.000000000000000000, 0.000000000000000000 ) ) ;
#45194 = CARTESIAN_POINT ( 'NONE',  ( 10.90000000346999975, -5.100000000044000892, -5.157071296039999808 ) ) ;
#45195 = CARTESIAN_POINT ( 'NONE',  ( 0.5842604209659999492, 3.128647331775999962, -1.414269894618000123 ) ) ;
#45196 = DIRECTION ( 'NONE',  ( 1.000000000000000000, 0.000000000000000000, 0.000000000000000000 ) ) ;
#45197 = EDGE_CURVE ( 'NONE', #60567, #10372, #39964, .T. ) ;
#45198 = CARTESIAN_POINT ( 'NONE',  ( 12.70928935905665291, 3.193791526923301927, 12.18850694772984333 ) ) ;
#45199 = CARTESIAN_POINT ( 'NONE',  ( 9.817462135711998883, 5.100000000000000533, 6.571291218949999902 ) ) ;
#45200 = CARTESIAN_POINT ( 'NONE',  ( 10.67826222744820086, 3.331419131587999960, -8.050725169876500331 ) ) ;
#45201 = FACE_OUTER_BOUND ( 'NONE', #61247, .T. ) ;
#45202 = CARTESIAN_POINT ( 'NONE',  ( 11.09991415876999987, 2.373387781209999936, -6.776601845694000481 ) ) ;
#45203 = CARTESIAN_POINT ( 'NONE',  ( 8.670138961223999630, 4.946050868436800307, -8.139313957553699908 ) ) ;
#45205 = CARTESIAN_POINT ( 'NONE',  ( 10.42020212696999870, -3.045227368876000096, 4.899674683287999599 ) ) ;
#45204 = CARTESIAN_POINT ( 'NONE',  ( 0.1500002361980000143, 0.000000000000000000, -2.724999730217442906 ) ) ;
#45206 = B_SPLINE_CURVE_WITH_KNOTS ( 'NONE', 3,
 ( #38195, #43803, #65098, #38547, #67177 ),
 .UNSPECIFIED., .F., .F.,
 ( 4, 1, 4 ),
 ( 0.000000000000000000, 0.5000000000000000000, 1.000000000000000000 ),
 .UNSPECIFIED. ) ;
#45207 = CONICAL_SURFACE ( 'NONE', #54118, 1.725000594299999968, 0.7853984795078434722 ) ;
#45208 = CARTESIAN_POINT ( 'NONE',  ( 23.61450813208451649, -13.39969347648717068, 3.938932084374531684 ) ) ;
#45209 = ORIENTED_EDGE ( 'NONE', *, *, #29333, .F. ) ;
#45210 = CARTESIAN_POINT ( 'NONE',  ( 8.856793857978997764, 5.100000000000000533, -6.339888365514000590 ) ) ;
#45211 = AXIS2_PLACEMENT_3D ( 'NONE', #58552, #11009, #21834 ) ;
#45212 = CARTESIAN_POINT ( 'NONE',  ( 10.59344961228999971, -5.297755890367000120, 8.474197994416998725 ) ) ;
#45213 = CARTESIAN_POINT ( 'NONE',  ( 9.579025935145997650, 3.854158361175799907, 8.493766832166899761 ) ) ;
#45214 = CARTESIAN_POINT ( 'NONE',  ( 10.26539516633362759, 4.233208782175254647, -8.343294540545050708 ) ) ;
#45215 = DIRECTION ( 'NONE',  ( -1.000000000000000000, 0.000000000000000000, 0.000000000000000000 ) ) ;
#45216 = CARTESIAN_POINT ( 'NONE',  ( 12.36816014207664161, 2.947033975320460630, 13.56836638442238296 ) ) ;
#45217 = ORIENTED_EDGE ( 'NONE', *, *, #58109, .T. ) ;
#45218 = AXIS2_PLACEMENT_3D ( 'NONE', #47561, #9795, #20290 ) ;
#45219 = CARTESIAN_POINT ( 'NONE',  ( 9.252709346416999381, -2.968569381205999669, -7.010219103474399915 ) ) ;
#45220 = CARTESIAN_POINT ( 'NONE',  ( 5.399998535875000449, 6.217248937900999058E-14, -13.10000000000360210 ) ) ;
#45221 = CARTESIAN_POINT ( 'NONE',  ( 18.17388115328630960, 2.104502522679955856, -12.42302150255121340 ) ) ;
#45222 = CARTESIAN_POINT ( 'NONE',  ( 7.000000000000000888, 7.162101251533245616, 3.226271710805416415 ) ) ;
#45223 = DIRECTION ( 'NONE',  ( -1.000000000000000000, 0.000000000000000000, 0.000000000000000000 ) ) ;
#45224 = CARTESIAN_POINT ( 'NONE',  ( 11.63410404293056999, 3.557672215630899970, -8.400720262063998689 ) ) ;
#45225 = DIRECTION ( 'NONE',  ( -1.000000000000000000, 0.000000000000000000, 0.000000000000000000 ) ) ;
#45226 = CARTESIAN_POINT ( 'NONE',  ( 9.526735624254000001, -3.423478821957000040, -6.068694811299999436 ) ) ;
#45227 = FACE_OUTER_BOUND ( 'NONE', #57850, .T. ) ;
#45228 = ORIENTED_EDGE ( 'NONE', *, *, #66632, .T. ) ;
#45229 = CARTESIAN_POINT ( 'NONE',  ( 17.65355681324606252, 3.248032782086212489, -13.61801318301548491 ) ) ;
#45230 = ADVANCED_FACE ( 'NONE', ( #32668 ), #23179, .F. ) ;
#45231 = CARTESIAN_POINT ( 'NONE',  ( 12.80505043854144098, -0.7302158263239267866, -13.98094363220830871 ) ) ;
#45232 = EDGE_CURVE ( 'NONE', #65709, #10513, #26392, .T. ) ;
#45233 = CARTESIAN_POINT ( 'NONE',  ( 25.60000000000000142, -11.77655473258999841, -4.190794510628000680 ) ) ;
#45234 = CARTESIAN_POINT ( 'NONE',  ( 9.933148997456999751, -5.167567567567999731, 6.822293592207000934 ) ) ;
#45235 = CARTESIAN_POINT ( 'NONE',  ( 4.900006121741999898, 1.947945353336630436, -0.5234957687185638475 ) ) ;
#45236 = CARTESIAN_POINT ( 'NONE',  ( 9.708354719591000048, 5.481267232667000222, -8.005061172455999241 ) ) ;
#45237 = CARTESIAN_POINT ( 'NONE',  ( 6.885860368544080679, 0.8047703218898319966, 1.294940731405771706 ) ) ;
#45238 = ORIENTED_EDGE ( 'NONE', *, *, #55793, .T. ) ;
#45239 = CARTESIAN_POINT ( 'NONE',  ( 4.000000000000000000, 1.878608423871360289, 1.082950885222729420 ) ) ;
#45240 = CARTESIAN_POINT ( 'NONE',  ( 18.17895306041983972, 2.542296241241985832, -13.66441818551904674 ) ) ;
#45241 = EDGE_LOOP ( 'NONE', ( #15578, #6363, #38950, #57960 ) ) ;
#45242 = CARTESIAN_POINT ( 'NONE',  ( 18.18005043854144276, 0.000000000000000000, -25.00000000000000000 ) ) ;
#45243 = CARTESIAN_POINT ( 'NONE',  ( 7.100000000000000533, -11.84999999999999964, 0.000000000000000000 ) ) ;
#45244 = CARTESIAN_POINT ( 'NONE',  ( 9.310554719594000161, 3.934138271021000222, -9.063586117809000697 ) ) ;
#45245 = STYLED_ITEM ( 'NONE', ( #40865 ), #42688 ) ;
#45246 = CARTESIAN_POINT ( 'NONE',  ( 24.09354147538195434, -12.55951106403002093, 3.397315377048726770 ) ) ;
#45247 = CARTESIAN_POINT ( 'NONE',  ( 11.43856039236529831, -2.967715280237000375, -7.550239075043479353 ) ) ;
#45248 = CARTESIAN_POINT ( 'NONE',  ( 9.381451725828847898, -5.100000000000000533, -6.394648509984842022 ) ) ;
#45249 = CARTESIAN_POINT ( 'NONE',  ( 10.16476354018233508, -2.782534154164604256, 7.827184855449094592 ) ) ;
#45250 = ORIENTED_EDGE ( 'NONE', *, *, #26406, .F. ) ;
#45251 = CARTESIAN_POINT ( 'NONE',  ( 9.957691290288998687, 3.110563525881361535, -8.413289387078533466 ) ) ;
#45252 = CARTESIAN_POINT ( 'NONE',  ( 17.88831561177691398, -3.029094439784365544, -13.54684341222245436 ) ) ;
#45253 = CARTESIAN_POINT ( 'NONE',  ( 8.599639158772999892, 2.261390688294000029, -6.733978371730000134 ) ) ;
#45254 = ORIENTED_EDGE ( 'NONE', *, *, #40439, .T. ) ;
#45255 = EDGE_CURVE ( 'NONE', #33910, #21413, #47338, .T. ) ;
#45256 = CARTESIAN_POINT ( 'NONE',  ( 10.56590837162999996, 5.293226105229999590, -7.067087619452999903 ) ) ;
#45257 = CARTESIAN_POINT ( 'NONE',  ( 7.000000000000000000, 0.5415384615382999867, -2.132307692307999769 ) ) ;
#45258 = ORIENTED_EDGE ( 'NONE', *, *, #25484, .F. ) ;
#45259 = CARTESIAN_POINT ( 'NONE',  ( 8.771455549952998254, 4.888629236328500660, 8.216988513669100769 ) ) ;
#45260 = CARTESIAN_POINT ( 'NONE',  ( 18.28023629128827565, -2.459623831379296632, -12.35762167929922839 ) ) ;
#45261 = CIRCLE ( 'NONE', #32967, 12.49999909016000110 ) ;
#45262 = CARTESIAN_POINT ( 'NONE',  ( 8.239310352252500635, 2.650829846289728842, 7.263894687833489350 ) ) ;
#45263 = CARTESIAN_POINT ( 'NONE',  ( 25.29987931604000195, 11.13052921044000065, -3.427478701325000099 ) ) ;
#45264 = CARTESIAN_POINT ( 'NONE',  ( 11.56631965465000178, -11.51200727500000021, -1.523108403756999962 ) ) ;
#45265 = CARTESIAN_POINT ( 'NONE',  ( 8.851468108405999402, 4.834201109053600121, 7.263744984161399465 ) ) ;
#45266 = CYLINDRICAL_SURFACE ( 'NONE', #56033, 0.5000000000000004441 ) ;
#45267 = VERTEX_POINT ( 'NONE', #12727 ) ;
#45268 = CARTESIAN_POINT ( 'NONE',  ( 17.55505043854147118, -1.787816316115923954, 13.88537766212463254 ) ) ;
#45269 = CARTESIAN_POINT ( 'NONE',  ( 10.82674528040999995, 3.167160000746000126, -6.225151413000000744 ) ) ;
#45270 = CARTESIAN_POINT ( 'NONE',  ( 24.30000000000000071, 8.810505093353000916, -8.810505093353000916 ) ) ;
#45271 = CARTESIAN_POINT ( 'NONE',  ( 12.36046591005674777, 1.940744226335691103, -13.86483863263027416 ) ) ;
#45272 = B_SPLINE_CURVE_WITH_KNOTS ( 'NONE', 3,
 ( #21558, #10383, #69114, #26129, #52690 ),
 .UNSPECIFIED., .F., .F.,
 ( 4, 1, 4 ),
 ( 0.000000000000000000, 0.5000000000000000000, 1.000000000000000000 ),
 .UNSPECIFIED. ) ;
#45273 = CARTESIAN_POINT ( 'NONE',  ( 17.79999999998900151, -3.595165934733000057, -11.99793354950999991 ) ) ;
#45274 = CARTESIAN_POINT ( 'NONE',  ( 9.013429960698999821, -4.933961117404000341, 8.417889755737999025 ) ) ;
#45275 = CARTESIAN_POINT ( 'NONE',  ( 18.20015658150181892, -0.3334496638227529841, 13.99603244703262739 ) ) ;
#45276 = CARTESIAN_POINT ( 'NONE',  ( 18.18005043799237086, -2.500000011518549670, 12.45159158845318359 ) ) ;
#45277 = ORIENTED_EDGE ( 'NONE', *, *, #69169, .T. ) ;
#45278 = ORIENTED_EDGE ( 'NONE', *, *, #61833, .T. ) ;
#45279 = CARTESIAN_POINT ( 'NONE',  ( 8.640504719592000171, 2.305580295895999665, -7.860904109308999743 ) ) ;
#45280 = EDGE_CURVE ( 'NONE', #53432, #36464, #20582, .T. ) ;
#45281 = CARTESIAN_POINT ( 'NONE',  ( 10.73912476064303156, -2.651371201321786941, 7.263709536581201220 ) ) ;
#45282 = CIRCLE ( 'NONE', #15125, 1.249999999999999778 ) ;
#45283 = CARTESIAN_POINT ( 'NONE',  ( 12.19334556251213186, -2.628630844604569194, 13.64533835530551009 ) ) ;
#45284 = DIRECTION ( 'NONE',  ( 1.000000000000000000, 0.000000000000000000, 0.000000000000000000 ) ) ;
#45285 = CARTESIAN_POINT ( 'NONE',  ( 24.02092319654100194, 9.294262032018000497, -9.129398518842998911 ) ) ;
#45286 = DIRECTION ( 'NONE',  ( 1.000000000000000000, 0.000000000000000000, 0.000000000000000000 ) ) ;
#45288 = CARTESIAN_POINT ( 'NONE',  ( 11.12486991174999851, -6.581659117425999739, 5.643192323797999954 ) ) ;
#45287 = CARTESIAN_POINT ( 'NONE',  ( 9.827747021775998348, -4.858221690000700477, 6.746879837742599584 ) ) ;
#45289 = CARTESIAN_POINT ( 'NONE',  ( 12.80505043854143388, 3.199698446519374517, 12.18695736643652694 ) ) ;
#45290 = ORIENTED_EDGE ( 'NONE', *, *, #58779, .F. ) ;
#45291 = CARTESIAN_POINT ( 'NONE',  ( 10.97725418964999911, -2.701085748494000072, 4.940122434141000163 ) ) ;
#45292 = CARTESIAN_POINT ( 'NONE',  ( 7.931011803055000975, 3.387313518888000363, -6.297038610257000180 ) ) ;
#45293 = CARTESIAN_POINT ( 'NONE',  ( 17.62710295837867847, 0.6209187240130098484, 12.67955909024709094 ) ) ;
#45294 = CARTESIAN_POINT ( 'NONE',  ( 12.30788008590002391, -0.3788802694180442021, 12.69239629738001973 ) ) ;
#45295 = CARTESIAN_POINT ( 'NONE',  ( 4.149992563291998948, 0.5234817089163672499, 1.947893036340042849 ) ) ;
#45296 = ORIENTED_EDGE ( 'NONE', *, *, #21218, .T. ) ;
#45298 = CARTESIAN_POINT ( 'NONE',  ( 24.44496482743900145, 12.03536723905999928, -3.224852005146999989 ) ) ;
#45297 = CARTESIAN_POINT ( 'NONE',  ( 11.09999999999999964, 5.299311513382999550, 5.124965750789000296 ) ) ;
#45299 = CARTESIAN_POINT ( 'NONE',  ( 8.655270280412999284, 4.162493982103000256, -5.775210092227999858 ) ) ;
#45300 = B_SPLINE_CURVE_WITH_KNOTS ( 'NONE', 3,
 ( #43862, #21833, #33376, #18936, #45167, #1211 ),
 .UNSPECIFIED., .F., .F.,
 ( 4, 2, 4 ),
 ( 0.000000000000000000, 0.5000000000000000000, 1.000000000000000000 ),
 .UNSPECIFIED. ) ;
#45301 = CARTESIAN_POINT ( 'NONE',  ( 9.271640687503564848, 2.873222873816658307, 6.752018918868503583 ) ) ;
#45302 = CARTESIAN_POINT ( 'NONE',  ( 10.14887885159599890, 5.269014563305000287, 7.651388779553199626 ) ) ;
#45303 = AXIS2_PLACEMENT_3D ( 'NONE', #30837, #52497, #36420 ) ;
#45304 =( NAMED_UNIT ( * ) SI_UNIT ( $, .STERADIAN. ) SOLID_ANGLE_UNIT ( ) );
#45305 = CARTESIAN_POINT ( 'NONE',  ( 1.700000000000000178, 0.000000000000000000, 0.000000000000000000 ) ) ;
#45306 = CARTESIAN_POINT ( 'NONE',  ( 2.781247112084000328, 2.100317644827999874, 2.706193714288000152 ) ) ;
#45307 = ORIENTED_EDGE ( 'NONE', *, *, #60579, .F. ) ;
#45308 = CARTESIAN_POINT ( 'NONE',  ( 12.57519818727761951, -0.5812897767837165164, -12.68208758371478595 ) ) ;
#45310 = CARTESIAN_POINT ( 'NONE',  ( 12.05670819615735923, -4.620649663933218854, 8.119355997108678835 ) ) ;
#45309 = B_SPLINE_CURVE_WITH_KNOTS ( 'NONE', 3,
 ( #58053, #31833, #10156, #64657 ),
 .UNSPECIFIED., .F., .F.,
 ( 4, 4 ),
 ( 0.000000000000000000, 1.000000000000000000 ),
 .UNSPECIFIED. ) ;
#45311 = LINE ( 'NONE', #65924, #33157 ) ;
#45312 = CARTESIAN_POINT ( 'NONE',  ( 24.51228084553499897, 3.325039717427999975, -12.06631758408999922 ) ) ;
#45313 = EDGE_LOOP ( 'NONE', ( #51939, #53548, #60275, #27707, #6033, #5361, #48579, #67254, #5529, #54159 ) ) ;
#45314 = CARTESIAN_POINT ( 'NONE',  ( 6.803907741853000957, -1.064812127159999955, 0.2760466167989999997 ) ) ;
#45315 = EDGE_CURVE ( 'NONE', #10058, #13432, #24803, .T. ) ;
#45316 = EDGE_CURVE ( 'NONE', #47095, #28041, #11409, .T. ) ;
#45317 = CARTESIAN_POINT ( 'NONE',  ( 8.087285841226000471, 5.397384434738000003, -7.480682713844000631 ) ) ;
#45319 = CARTESIAN_POINT ( 'NONE',  ( 24.62769666408257052, -8.773247285887615377, 9.203857927720639154 ) ) ;
#45318 = CARTESIAN_POINT ( 'NONE',  ( 24.30000000000000071, 9.517611874540000017, 8.103398312166000039 ) ) ;
#45320 = DIRECTION ( 'NONE',  ( 0.000000000000000000, 0.7071067811865474617, 0.7071067811865474617 ) ) ;
#45321 = CARTESIAN_POINT ( 'NONE',  ( 10.72299000889467635, -4.227343628179307977, -8.344040565988990465 ) ) ;
#45322 = EDGE_LOOP ( 'NONE', ( #13048, #43067, #61586, #41284, #38177 ) ) ;
#45323 = ORIENTED_EDGE ( 'NONE', *, *, #50671, .T. ) ;
#45324 = CARTESIAN_POINT ( 'NONE',  ( 0.000000000000000000, 0.000000000000000000, 0.000000000000000000 ) ) ;
#45325 = CARTESIAN_POINT ( 'NONE',  ( 8.406105646793999853, -5.342173944271999986, 8.432314172168000610 ) ) ;
#45326 = CARTESIAN_POINT ( 'NONE',  ( 18.14493363608989540, 0.4251989115648961426, -13.99355557726514299 ) ) ;
#45327 = EDGE_LOOP ( 'NONE', ( #65097, #33297, #9169, #31526, #55132, #34632, #58195, #68794, #32159, #35134, #14549 ) ) ;
#45328 = CARTESIAN_POINT ( 'NONE',  ( 10.44668246007000079, -8.240391359595998111, 6.962948453051999387 ) ) ;
#45329 = CARTESIAN_POINT ( 'NONE',  ( 18.30017264560541079, 0.9191760165933146043, 11.85014035445314740 ) ) ;
#45330 = DIRECTION ( 'NONE',  ( 1.000000000000000000, 0.000000000000000000, 0.000000000000000000 ) ) ;
#45331 = FACE_OUTER_BOUND ( 'NONE', #49179, .T. ) ;
#45332 = CARTESIAN_POINT ( 'NONE',  ( 25.39940350028005156, 8.416042725244727407, 8.072285808956092268 ) ) ;
#45333 = ORIENTED_EDGE ( 'NONE', *, *, #36440, .F. ) ;
#45334 = CARTESIAN_POINT ( 'NONE',  ( 9.471368011205999693, -2.030678448189000118, 7.549764202121000523 ) ) ;
#45335 = CARTESIAN_POINT ( 'NONE',  ( 23.86947894555299854, -13.28527095192000118, -3.447687139233999609 ) ) ;
#45336 = CARTESIAN_POINT ( 'NONE',  ( 5.605026506349999771, -1.500000000000000000, 0.000000000000000000 ) ) ;
#45337 = ADVANCED_FACE ( 'NONE', ( #33363 ), #10894, .T. ) ;
#45338 = CARTESIAN_POINT ( 'NONE',  ( 9.727263540182331525, 4.629523725463627670, 8.592232985442818105 ) ) ;
#45339 = CARTESIAN_POINT ( 'NONE',  ( 12.15832103307001155, -2.898357473903109494, 13.69738840704686389 ) ) ;
#45340 = ORIENTED_EDGE ( 'NONE', *, *, #11126, .T. ) ;
#45341 = FACE_OUTER_BOUND ( 'NONE', #45322, .T. ) ;
#45342 = EDGE_CURVE ( 'NONE', #53037, #5820, #22856, .T. ) ;
#45343 = DIRECTION ( 'NONE',  ( 1.000000000000000000, 0.000000000000000000, 0.000000000000000000 ) ) ;
#45344 = CARTESIAN_POINT ( 'NONE',  ( 3.500000000000000888, 2.793279419286928356, 1.985771234201202606 ) ) ;
#45345 = CARTESIAN_POINT ( 'NONE',  ( 23.81728226941260118, -3.309408472638277310, -13.09637078731351778 ) ) ;
#45346 = PLANE ( 'NONE',  #57759 ) ;
#45347 = CARTESIAN_POINT ( 'NONE',  ( 12.23550883753394025, 0.2581888431706758635, -13.89679013629344517 ) ) ;
#45348 = CARTESIAN_POINT ( 'NONE',  ( 17.86190681601109631, -1.955416883085901558, 12.56193573862144852 ) ) ;
#45349 = VERTEX_POINT ( 'NONE', #1079 ) ;
#45350 = CARTESIAN_POINT ( 'NONE',  ( 11.36056039236529891, -3.108928759355700233, -7.543366519014379712 ) ) ;
#45351 = ORIENTED_EDGE ( 'NONE', *, *, #38305, .F. ) ;
#45352 = DIRECTION ( 'NONE',  ( 0.000000000000000000, -1.000000000000000000, 0.000000000000000000 ) ) ;
#45353 = AXIS2_PLACEMENT_3D ( 'NONE', #8832, #9167, #46588 ) ;
#45354 = CARTESIAN_POINT ( 'NONE',  ( 8.532195280408998883, 5.331510020787000315, -8.114341808290998159 ) ) ;
#45355 = CARTESIAN_POINT ( 'NONE',  ( 2.580236016716999981, -1.802165296364000024, -2.662471851299000214 ) ) ;
#45356 = CARTESIAN_POINT ( 'NONE',  ( 10.55068143582000140, -2.412180768165999911, -6.919582641217999708 ) ) ;
#45357 = AXIS2_PLACEMENT_3D ( 'NONE', #64915, #6191, #33473 ) ;
#45358 = CARTESIAN_POINT ( 'NONE',  ( 17.79999999998900151, 3.595165934733000057, -11.99793354950999991 ) ) ;
#45359 = CARTESIAN_POINT ( 'NONE',  ( 9.074999999999999289, -4.417172942406000224, 8.783926296998000538 ) ) ;
#45360 = ORIENTED_EDGE ( 'NONE', *, *, #38262, .T. ) ;
#45361 = CARTESIAN_POINT ( 'NONE',  ( 12.08071932425156980, -4.167269912168199753, 6.371589232479998977 ) ) ;
#45362 = CARTESIAN_POINT ( 'NONE',  ( 10.40726830891999910, 3.797905842462999892, 5.889914049998000500 ) ) ;
#45363 = CARTESIAN_POINT ( 'NONE',  ( 25.29986734212600297, -2.596989636639000398, 11.35306351421000137 ) ) ;
#45364 = CARTESIAN_POINT ( 'NONE',  ( 10.99999218979999860, 0.000000000000000000, -2.784439345760000141E-13 ) ) ;
#45366 = CARTESIAN_POINT ( 'NONE',  ( 9.074999999999999289, 4.417172942406000224, 8.783926296998000538 ) ) ;
#45365 = CARTESIAN_POINT ( 'NONE',  ( 10.68403803949000164, 5.436614310638000269, 8.578436083822998270 ) ) ;
#45367 = CARTESIAN_POINT ( 'NONE',  ( 11.28533594839949750, 4.750012929834699804, -6.640482273977399430 ) ) ;
#45368 = CARTESIAN_POINT ( 'NONE',  ( 25.59997774154300032, -2.856411620672000051, -11.13959722905999961 ) ) ;
#45369 = ADVANCED_FACE ( 'NONE', ( #27303, #11215 ), #383, .F. ) ;
#45370 = CARTESIAN_POINT ( 'NONE',  ( 10.13626717315599990, 3.235527139800300045, -6.848522029265999400 ) ) ;
#45371 = B_SPLINE_CURVE_WITH_KNOTS ( 'NONE', 3,
 ( #59206, #37886, #33688, #831 ),
 .UNSPECIFIED., .F., .F.,
 ( 4, 4 ),
 ( 0.000000000000000000, 1.000000000000000000 ),
 .UNSPECIFIED. ) ;
#45372 = CARTESIAN_POINT ( 'NONE',  ( 11.83810207955129989, -3.203462856645999945, 7.174999999999999822 ) ) ;
#45373 = CARTESIAN_POINT ( 'NONE',  ( 24.56500367226799852, 3.482495402162000264, 12.16326672459999791 ) ) ;
#45374 = CARTESIAN_POINT ( 'NONE',  ( 8.093108454043214550, 5.099642902067280659, -6.624168013080805828 ) ) ;
#45375 = FACE_OUTER_BOUND ( 'NONE', #68712, .T. ) ;
#45376 = VERTEX_POINT ( 'NONE', #37788 ) ;
#45377 = CARTESIAN_POINT ( 'NONE',  ( 9.234504440379000201, -5.964711531933999389, 7.776478361891000723 ) ) ;
#45378 = CARTESIAN_POINT ( 'NONE',  ( 18.08737871041808987, 2.022152854634007291, 13.85319383421289530 ) ) ;
#45379 = LINE ( 'NONE', #44698, #33407 ) ;
#45380 = CARTESIAN_POINT ( 'NONE',  ( 10.14887885159599890, -2.730985436695000157, -7.348611220446799486 ) ) ;
#45381 = ORIENTED_EDGE ( 'NONE', *, *, #27078, .F. ) ;
#45382 = CARTESIAN_POINT ( 'NONE',  ( 7.422239158771000156, 5.361039412362000434, 6.973453640356000349 ) ) ;
#45384 = CARTESIAN_POINT ( 'NONE',  ( 0.7532955584366096691, -2.936936850608698801, 1.972122296016285858 ) ) ;
#45383 = CARTESIAN_POINT ( 'NONE',  ( 9.690635841230999858, 2.927176851028000293, -5.932007155957999878 ) ) ;
#45385 = CARTESIAN_POINT ( 'NONE',  ( 10.19121415877000203, 3.990707652596999555, -5.651362387566000400 ) ) ;
#45386 = VERTEX_POINT ( 'NONE', #59452 ) ;
#45387 = CYLINDRICAL_SURFACE ( 'NONE', #20533, 1.350000000000000089 ) ;
#45388 = CARTESIAN_POINT ( 'NONE',  ( 9.258050732556000639, -4.895927245463000510, -6.008721945297999412 ) ) ;
#45389 = CARTESIAN_POINT ( 'NONE',  ( 11.50687348028854906, 2.996540789803000315, 6.957450711802899868 ) ) ;
#45390 = CARTESIAN_POINT ( 'NONE',  ( 10.33537187819000103, -5.153689638257000105, 8.830861236101000600 ) ) ;
#45391 = CARTESIAN_POINT ( 'NONE',  ( 11.09999999999999964, -2.685305999535000154, 6.664030027596000494 ) ) ;
#45392 = EDGE_LOOP ( 'NONE', ( #59683, #29221, #38291, #6755 ) ) ;
#45393 = FACE_BOUND ( 'NONE', #52992, .T. ) ;
#45394 = ADVANCED_FACE ( 'NONE', ( #6305 ), #29892, .T. ) ;
#45395 = EDGE_CURVE ( 'NONE', #51926, #14947, #22042, .T. ) ;
#45396 = CARTESIAN_POINT ( 'NONE',  ( 10.61442944038000036, -5.287639274524000399, -7.937245019889999753 ) ) ;
#45397 = CARTESIAN_POINT ( 'NONE',  ( 7.966961417027972558, -2.304181943332437754, 7.113926501787253720 ) ) ;
#45398 = CARTESIAN_POINT ( 'NONE',  ( 9.290195424034999760, -2.377814350880000038, 7.540992175424999999 ) ) ;
#45400 = CARTESIAN_POINT ( 'NONE',  ( 11.67403632436368888, -4.976178716761900489, -7.272033745815799755 ) ) ;
#45399 = CONICAL_SURFACE ( 'NONE', #9693, 1.449999999967999553, 0.7853981633972997312 ) ;
#45401 = CARTESIAN_POINT ( 'NONE',  ( 10.38593802597399929, -4.593629475532499562, 8.475365825607600101 ) ) ;
#45402 = ORIENTED_EDGE ( 'NONE', *, *, #49303, .T. ) ;
#45403 = CARTESIAN_POINT ( 'NONE',  ( 10.60972883830999969, -5.134198870706001117, -4.837030643953000641 ) ) ;
#45404 = EDGE_CURVE ( 'NONE', #22584, #51958, #8656, .T. ) ;
#45405 = B_SPLINE_CURVE_WITH_KNOTS ( 'NONE', 3,
 ( #60788, #66717, #12902, #45746 ),
 .UNSPECIFIED., .F., .F.,
 ( 4, 4 ),
 ( 0.000000000000000000, 1.000000000000000000 ),
 .UNSPECIFIED. ) ;
#45406 = CARTESIAN_POINT ( 'NONE',  ( 12.11759063708296047, -2.782734359457999851, 7.157757529645699890 ) ) ;
#45407 = VERTEX_POINT ( 'NONE', #10526 ) ;
#45408 = CARTESIAN_POINT ( 'NONE',  ( 8.995772571291155373, 2.998508658148200556, 6.923765800360898837 ) ) ;
#45409 = ORIENTED_EDGE ( 'NONE', *, *, #65365, .F. ) ;
#45410 = CARTESIAN_POINT ( 'NONE',  ( 9.883740731405000091, -5.634417356902000407, -7.003562403358999156 ) ) ;
#45411 = CARTESIAN_POINT ( 'NONE',  ( 8.704995280412999747, 5.140767546012999567, -6.196177269779999719 ) ) ;
#45412 = FACE_OUTER_BOUND ( 'NONE', #45241, .T. ) ;
#45413 = DIRECTION ( 'NONE',  ( 0.000000000000000000, 0.000000000000000000, 1.000000000000000000 ) ) ;
#45414 = CARTESIAN_POINT ( 'NONE',  ( 12.36494524851998023, 2.943800415886788091, -12.33703218264929902 ) ) ;
#45415 = CARTESIAN_POINT ( 'NONE',  ( 11.29718447801629999, -2.996774412198000448, 7.522119512433738997 ) ) ;
#45416 = CARTESIAN_POINT ( 'NONE',  ( 11.85545123989520100, -3.524778630617700248, 6.582230774881299595 ) ) ;
#45417 = EDGE_LOOP ( 'NONE', ( #53192, #5351, #17561, #22104 ) ) ;
#45418 = CARTESIAN_POINT ( 'NONE',  ( 9.802263540183334456, 2.907767014557178786, 8.129523725463625894 ) ) ;
#45419 = CARTESIAN_POINT ( 'NONE',  ( 7.737831853206999178, -5.687202994508999687, 6.847270485579000088 ) ) ;
#45420 = PLANE ( 'NONE',  #60323 ) ;
#45421 = ORIENTED_EDGE ( 'NONE', *, *, #12672, .F. ) ;
#45422 = CARTESIAN_POINT ( 'NONE',  ( 12.08418858410078300, -2.401692437127227464, -12.36899414651120921 ) ) ;
#45423 = EDGE_CURVE ( 'NONE', #55971, #11176, #35467, .T. ) ;
#45424 = CARTESIAN_POINT ( 'NONE',  ( 10.94072200990529886, 2.922907051630999842, 7.875713849677398848 ) ) ;
#45425 = CARTESIAN_POINT ( 'NONE',  ( 10.31966935320999923, -4.764591648058999596, -5.997654637741999473 ) ) ;
#45426 = CARTESIAN_POINT ( 'NONE',  ( 10.72934687351609639, 3.836375382625535124, 8.750000000000000000 ) ) ;
#45427 = CARTESIAN_POINT ( 'NONE',  ( 17.70961302874500021, -11.81369488050999905, 3.327702596852999850 ) ) ;
#45428 = CARTESIAN_POINT ( 'NONE',  ( 24.51327040722500072, -8.786342692851000891, 8.911852834696000869 ) ) ;
#45429 = CARTESIAN_POINT ( 'NONE',  ( 12.39133745138803810, -2.968584063660574479, -13.56278128057737398 ) ) ;
#45430 = CARTESIAN_POINT ( 'NONE',  ( 5.468188860442999122, -0.6025205152629000693, 1.401692221310999908 ) ) ;
#45431 = CARTESIAN_POINT ( 'NONE',  ( 11.40425819896749893, -5.255890247626999745, -7.736761623643599428 ) ) ;
#45432 = CARTESIAN_POINT ( 'NONE',  ( 8.564063803065426583, -5.052895881395312649, 6.264019472755840923 ) ) ;
#45433 = ORIENTED_EDGE ( 'NONE', *, *, #36636, .T. ) ;
#45434 =( LENGTH_UNIT ( ) NAMED_UNIT ( * ) SI_UNIT ( .MILLI., .METRE. ) );
#45435 = CARTESIAN_POINT ( 'NONE',  ( 12.17041389150293185, -11.12724490998814453, 3.450620877153329324 ) ) ;
#45436 = CARTESIAN_POINT ( 'NONE',  ( 4.599999999999999645, 0.7302158263239085789, 13.98094363220830871 ) ) ;
#45437 = CARTESIAN_POINT ( 'NONE',  ( 10.80159548023000049, 2.805082485475999476, -8.157276499959001725 ) ) ;
#45438 = CARTESIAN_POINT ( 'NONE',  ( 8.717034166355354330, 5.096433331277959056, 6.336971952315185064 ) ) ;
#45439 = AXIS2_PLACEMENT_3D ( 'NONE', #7151, #66562, #35115 ) ;
#45440 = CARTESIAN_POINT ( 'NONE',  ( 17.69826591161632834, 1.891282299241872522, 12.57273691359006129 ) ) ;
#45441 = CARTESIAN_POINT ( 'NONE',  ( 17.85449583315300259, 3.297641659324999974, -11.83458394846000061 ) ) ;
#45442 = CARTESIAN_POINT ( 'NONE',  ( 11.27110638630999873, 5.469603964121000139, 8.504707115835000053 ) ) ;
#45443 = AXIS2_PLACEMENT_3D ( 'NONE', #13501, #61037, #1273 ) ;
#45444 = CARTESIAN_POINT ( 'NONE',  ( 11.12299956498149811, 5.207010770456999893, 7.174999999999999822 ) ) ;
#45445 = EDGE_LOOP ( 'NONE', ( #12966, #34410, #13270, #28670 ) ) ;
#45446 = CARTESIAN_POINT ( 'NONE',  ( 12.21868246241199962, -2.283434118842408100, 12.49941978418538646 ) ) ;
#45447 = CARTESIAN_POINT ( 'NONE',  ( 8.945797255587999430, -2.996487526130999779, -7.457514444071220439 ) ) ;
#45448 = CARTESIAN_POINT ( 'NONE',  ( 9.722769750889000306, 5.493785011855999656, 6.566826815556000341 ) ) ;
#45449 = CARTESIAN_POINT ( 'NONE',  ( 12.09456039236534330, -2.685288321999000249, 7.436015812896529020 ) ) ;
#45450 = AXIS2_PLACEMENT_3D ( 'NONE', #27151, #21888, #47794 ) ;
#45451 = CARTESIAN_POINT ( 'NONE',  ( 10.22687885159599830, 5.132709421626000079, -7.364871923548499844 ) ) ;
#45452 = CARTESIAN_POINT ( 'NONE',  ( 12.18004360525213414, -0.009762034906140630575, 12.70000045436730751 ) ) ;
#45453 = EDGE_CURVE ( 'NONE', #27484, #45997, #1396, .T. ) ;
#45454 = EDGE_CURVE ( 'NONE', #26293, #12504, #22311, .T. ) ;
#45455 = CARTESIAN_POINT ( 'NONE',  ( 7.866204719590000671, 4.580608786027000612, 9.213365309690999538 ) ) ;
#45456 = CARTESIAN_POINT ( 'NONE',  ( 9.075483283097998566, 4.020836891789999257, 8.948690653012000951 ) ) ;
#45457 = CARTESIAN_POINT ( 'NONE',  ( 12.52557666887732957, 1.940868768839140390, 12.56439497327412624 ) ) ;
#45458 = ORIENTED_EDGE ( 'NONE', *, *, #53039, .T. ) ;
#45459 = CARTESIAN_POINT ( 'NONE',  ( 8.450464158772000189, 3.789127741898000057, -9.388182174781999123 ) ) ;
#45460 = CARTESIAN_POINT ( 'NONE',  ( 11.60118044953561878, 5.133201153721000054, -8.090905336380599167 ) ) ;
#45461 = CARTESIAN_POINT ( 'NONE',  ( 10.74016332886163383, -5.523909096309798095, 8.356370520113504341 ) ) ;
#45463 = CARTESIAN_POINT ( 'NONE',  ( 10.23976354018233259, 3.672815144550903632, 8.717465845835395299 ) ) ;
#45462 = CARTESIAN_POINT ( 'NONE',  ( 25.29987667925500361, 10.83443035398000021, 3.855530949778000149 ) ) ;
#45464 = CARTESIAN_POINT ( 'NONE',  ( 9.604759580228998672, -4.843256805554699618, 7.701558687214699717 ) ) ;
#45465 = CARTESIAN_POINT ( 'NONE',  ( 10.94487616594229884, -4.303437140848100029, -6.543508100188799581 ) ) ;
#45466 = ORIENTED_EDGE ( 'NONE', *, *, #48217, .F. ) ;
#45467 = CARTESIAN_POINT ( 'NONE',  ( 1.057517373740999966, 3.437215509016000148, 1.521310954037999874 ) ) ;
#45468 = CARTESIAN_POINT ( 'NONE',  ( 17.95596512699729885, -0.4795041973233179489, -12.68781427220655011 ) ) ;
#45469 = CARTESIAN_POINT ( 'NONE',  ( 9.436337454063533414, -4.868096831666449908, 8.168216413461584224 ) ) ;
#45470 = CARTESIAN_POINT ( 'NONE',  ( 11.04384236319999957, -1.500344243307999870, 5.035088906224999938 ) ) ;
#45471 = DIRECTION ( 'NONE',  ( 0.000000000000000000, 0.2461538461537955413, 0.9692307692307821076 ) ) ;
#45472 = CARTESIAN_POINT ( 'NONE',  ( 17.69888641710121746, -1.891428316105117746, -13.78380564104365291 ) ) ;
#45473 = CARTESIAN_POINT ( 'NONE',  ( 11.64975833414749928, -4.796537143354000499, 7.174999999999999822 ) ) ;
#45474 = CARTESIAN_POINT ( 'NONE',  ( 9.408235422789894997, -5.323194378891031420, 7.228731909742346140 ) ) ;
#45475 = CARTESIAN_POINT ( 'NONE',  ( 8.656816940379998826, -5.329429281359999493, 6.027400270608000099 ) ) ;
#45476 = ORIENTED_EDGE ( 'NONE', *, *, #38711, .F. ) ;
#45477 = CARTESIAN_POINT ( 'NONE',  ( 9.331135841230999262, 4.141907758973999876, 6.047574021139999978 ) ) ;
#45479 = EDGE_CURVE ( 'NONE', #23870, #56039, #10545, .T. ) ;
#45478 = B_SPLINE_CURVE_WITH_KNOTS ( 'NONE', 3,
 ( #54078, #10394, #36978, #26834 ),
 .UNSPECIFIED., .F., .F.,
 ( 4, 4 ),
 ( 0.000000000000000000, 1.000000000000000000 ),
 .UNSPECIFIED. ) ;
#45480 = CARTESIAN_POINT ( 'NONE',  ( 10.25000000000000000, 0.000000000000000000, 0.000000000000000000 ) ) ;
#45481 = CARTESIAN_POINT ( 'NONE',  ( 7.450637537771028995, -2.261141324514762907, 7.466197568434639109 ) ) ;
#45482 = VECTOR ( 'NONE', #62960, 1000.000000000000000 ) ;
#45483 = CARTESIAN_POINT ( 'NONE',  ( 17.82923902994810916, -0.5617296174771665429, 13.88472048964353611 ) ) ;
#45484 = CARTESIAN_POINT ( 'NONE',  ( 1.843384988122999779, -3.419251011552999930, 1.101167613520000144 ) ) ;
#45485 = ORIENTED_EDGE ( 'NONE', *, *, #60477, .T. ) ;
#45486 = CARTESIAN_POINT ( 'NONE',  ( 1.896806799206333327, 0.9161175952574848180, -3.408904368339103819 ) ) ;
#45487 = ADVANCED_FACE ( 'NONE', ( #65384 ), #22227, .F. ) ;
#45488 = CARTESIAN_POINT ( 'NONE',  ( 11.04482279157316604, -2.508505527921017553, -8.445267545976777868 ) ) ;
#45489 = CARTESIAN_POINT ( 'NONE',  ( 10.22398792753999963, 5.507894434963000130, 6.589802269404000157 ) ) ;
#45490 = CARTESIAN_POINT ( 'NONE',  ( 10.35826357027499789, 4.850513154668600002, 7.335909308151700614 ) ) ;
#45491 = B_SPLINE_CURVE_WITH_KNOTS ( 'NONE', 3,
 ( #3951, #19706, #45597, #40679 ),
 .UNSPECIFIED., .F., .F.,
 ( 4, 4 ),
 ( 0.000000000000000000, 1.000000000000000000 ),
 .UNSPECIFIED. ) ;
#45492 = CYLINDRICAL_SURFACE ( 'NONE', #18956, 2.750000000000000000 ) ;
#45493 = CARTESIAN_POINT ( 'NONE',  ( 11.03091694037999915, -5.020463882420000523, -6.601194361798000010 ) ) ;
#45494 = AXIS2_PLACEMENT_3D ( 'NONE', #37433, #10861, #26955 ) ;
#45495 = DIRECTION ( 'NONE',  ( -1.000000000000000000, 0.000000000000000000, 0.000000000000000000 ) ) ;
#45496 = CARTESIAN_POINT ( 'NONE',  ( 25.44993977744900349, -9.517611874540000017, -8.103398312166000039 ) ) ;
#45497 = CARTESIAN_POINT ( 'NONE',  ( 12.18822406275262438, -2.601257609840999407, 12.42743042555770572 ) ) ;
#45498 = CARTESIAN_POINT ( 'NONE',  ( 8.068768932173844277, 3.857044016492371163, 5.763189706540536861 ) ) ;
#45499 = ORIENTED_EDGE ( 'NONE', *, *, #11200, .F. ) ;
#45500 = VECTOR ( 'NONE', #47718, 1000.000000000000114 ) ;
#45501 = CARTESIAN_POINT ( 'NONE',  ( 17.80571586434987097, -1.927376100771097223, 13.77836213227538487 ) ) ;
#45502 = DIRECTION ( 'NONE',  ( 0.000000000000000000, -0.9999808993455937545, -0.006180691221632959691 ) ) ;
#45503 = ORIENTED_EDGE ( 'NONE', *, *, #33277, .F. ) ;
#45504 = CARTESIAN_POINT ( 'NONE',  ( 0.1500002361980000143, 2.725000000000000089, 0.000000000000000000 ) ) ;
#45505 = CARTESIAN_POINT ( 'NONE',  ( 25.09890362839945510, -2.850910023355439638, -11.48729055544455413 ) ) ;
#45506 = PLANE ( 'NONE',  #29400 ) ;
#45507 = EDGE_CURVE ( 'NONE', #2520, #50721, #58971, .T. ) ;
#45508 = DIRECTION ( 'NONE',  ( 1.000000000000000000, 0.000000000000000000, 0.000000000000000000 ) ) ;
#45509 = CYLINDRICAL_SURFACE ( 'NONE', #13053, 1.350000000000000533 ) ;
#45510 = DIRECTION ( 'NONE',  ( 0.000000000000000000, 0.000000000000000000, -1.000000000000000000 ) ) ;
#45511 = CARTESIAN_POINT ( 'NONE',  ( 18.36682228790370530, 2.717338739979867412, -11.46589211741044778 ) ) ;
#45512 = CARTESIAN_POINT ( 'NONE',  ( 11.27765354842000001, -3.273798832483999721, 6.368296067120999382 ) ) ;
#45513 = B_SPLINE_CURVE_WITH_KNOTS ( 'NONE', 3,
 ( #23091, #22399, #60161, #66080 ),
 .UNSPECIFIED., .F., .F.,
 ( 4, 4 ),
 ( 0.000000000000000000, 1.000000000000000000 ),
 .UNSPECIFIED. ) ;
#45514 = CARTESIAN_POINT ( 'NONE',  ( 17.77668021070434889, 0.6849607937330790541, -12.58136878870645248 ) ) ;
#45515 = AXIS2_PLACEMENT_3D ( 'NONE', #29272, #13536, #1306 ) ;
#45516 = CARTESIAN_POINT ( 'NONE',  ( 25.46373185538400463, 11.23406899464000119, 3.161078463958999496 ) ) ;
#45517 = CARTESIAN_POINT ( 'NONE',  ( 11.46179707368349909, -4.498457171163099844, -6.629085939160999530 ) ) ;
#45518 = FILL_AREA_STYLE ('',( #45172 ) ) ;
#45519 = ORIENTED_EDGE ( 'NONE', *, *, #63473, .F. ) ;
#45520 = CARTESIAN_POINT ( 'NONE',  ( 8.969356963619999235, 2.880642974985999860, -7.499999999914821025 ) ) ;
#45521 =( NAMED_UNIT ( * ) SI_UNIT ( $, .STERADIAN. ) SOLID_ANGLE_UNIT ( ) );
#45522 = CARTESIAN_POINT ( 'NONE',  ( 5.700000000000000178, -0.2999999999999999889, -9.662944685757000940 ) ) ;
#45523 = CARTESIAN_POINT ( 'NONE',  ( 6.865208375034998589, 8.291377142895010266, 4.196513763680004061 ) ) ;
#45524 = CARTESIAN_POINT ( 'NONE',  ( 9.861671671056999600, 2.738456190347000163, -7.711876388024100137 ) ) ;
#45525 = CARTESIAN_POINT ( 'NONE',  ( 12.18114782263372753, 2.542296328577541953, 13.66436634302260167 ) ) ;
#45526 = CARTESIAN_POINT ( 'NONE',  ( 9.534903635507999908, -3.030945724184999968, 8.761987396837000119 ) ) ;
#45527 = EDGE_LOOP ( 'NONE', ( #58354, #54538, #6921, #34671, #31000 ) ) ;
#45528 = CARTESIAN_POINT ( 'NONE',  ( 12.20071720274720661, -0.1607023183492722884, -12.69865132254261120 ) ) ;
#45529 = VECTOR ( 'NONE', #64913, 1000.000000000000000 ) ;
#45530 = CARTESIAN_POINT ( 'NONE',  ( 12.37030616679613892, -0.4491394412341195297, 13.89023495843590261 ) ) ;
#45531 = EDGE_LOOP ( 'NONE', ( #29142, #6444, #51196, #41677, #11017 ) ) ;
#45532 = LINE ( 'NONE', #56361, #66676 ) ;
#45533 = CARTESIAN_POINT ( 'NONE',  ( 18.43317799840264115, 2.892723637958514171, 12.11800683821377156 ) ) ;
#45534 = CARTESIAN_POINT ( 'NONE',  ( 23.86791715242600276, -3.655973686719000249, -13.23133700220999920 ) ) ;
#45535 = DIRECTION ( 'NONE',  ( 0.000000000000000000, 1.000000000000000000, 0.000000000000000000 ) ) ;
#45536 = CONICAL_SURFACE ( 'NONE', #41030, 2.074968475931999734, 0.7853828752794411727 ) ;
#45537 = VECTOR ( 'NONE', #32036, 1000.000000000000000 ) ;
#45538 = CARTESIAN_POINT ( 'NONE',  ( 8.823496488120920134, 2.820676299976329293, -8.179574529512112946 ) ) ;
#45539 = EDGE_CURVE ( 'NONE', #59750, #12624, #9816, .T. ) ;
#45540 = EDGE_CURVE ( 'NONE', #9263, #34148, #23374, .T. ) ;
#45541 = CARTESIAN_POINT ( 'NONE',  ( 0.3428519969243999932, -2.525007632204000263, -2.706826389191999915 ) ) ;
#45542 = CARTESIAN_POINT ( 'NONE',  ( 18.50013789939208664, 2.065999734462983189E-14, -11.64999999999999325 ) ) ;
#45543 = CONICAL_SURFACE ( 'NONE', #54461, 1.449999999967999553, 0.7853981633972997312 ) ;
#45544 = CARTESIAN_POINT ( 'NONE',  ( 12.30701392268162309, 3.003682976637727986, 12.23675526868967367 ) ) ;
#45545 = CARTESIAN_POINT ( 'NONE',  ( 9.529318513071000751, -2.297586052318000061, -7.360088033824999876 ) ) ;
#45546 = EDGE_CURVE ( 'NONE', #2158, #65247, #51419, .T. ) ;
#45547 = CARTESIAN_POINT ( 'NONE',  ( 11.31825954179440075, 4.666231193203100425, -8.053565341712399572 ) ) ;
#45548 = CARTESIAN_POINT ( 'NONE',  ( 23.50387503050299998, -0.02080343500003916865, 13.99998454345904442 ) ) ;
#45549 = CARTESIAN_POINT ( 'NONE',  ( 11.36056039236529891, 4.891071240644300211, -7.543366519014379712 ) ) ;
#45550 = CARTESIAN_POINT ( 'NONE',  ( 9.911267173156000254, 3.130949526459800403, -6.759401780699699103 ) ) ;
#45552 = CARTESIAN_POINT ( 'NONE',  ( 9.297364180957998769, -4.070567455836420656, 6.524104241236299728 ) ) ;
#45551 = CARTESIAN_POINT ( 'NONE',  ( 15.95192027319500205, -8.515023616297000331, -8.165096030563999463 ) ) ;
#45553 = CARTESIAN_POINT ( 'NONE',  ( 30.60000000000000142, 0.000000000000000000, 0.000000000000000000 ) ) ;
#45554 = ORIENTED_EDGE ( 'NONE', *, *, #9945, .F. ) ;
#45555 = CIRCLE ( 'NONE', #51134, 1.900000000000001021 ) ;
#45556 = DIRECTION ( 'NONE',  ( 0.000000000000000000, -1.000000000000000000, 0.000000000000000000 ) ) ;
#45557 = CARTESIAN_POINT ( 'NONE',  ( 10.15903154954000165, -4.166415630773999901, 9.114167874391000623 ) ) ;
#45558 = CARTESIAN_POINT ( 'NONE',  ( 10.28824205624999877, 3.639798001706899822, 6.562398383267799673 ) ) ;
#45559 = CARTESIAN_POINT ( 'NONE',  ( 17.60000004896734893, -11.45068297995442386, 4.713086259421401358 ) ) ;
#45560 = VECTOR ( 'NONE', #4964, 1000.000000000000000 ) ;
#45561 = PLANE ( 'NONE',  #39952 ) ;
#45562 = DIRECTION ( 'NONE',  ( -0.000000000000000000, -0.000000000000000000, 1.000000000000000000 ) ) ;
#45563 = CARTESIAN_POINT ( 'NONE',  ( 7.064321704349473485, -0.3488121830932555678, -1.301244489718812236 ) ) ;
#45564 = ORIENTED_EDGE ( 'NONE', *, *, #1041, .T. ) ;
#45565 = CARTESIAN_POINT ( 'NONE',  ( 9.430013376692999216, -5.017903082085999777, -6.982691809975100306 ) ) ;
#45566 = CARTESIAN_POINT ( 'NONE',  ( 24.53429014662800256, -8.855930250654999725, 9.286429702500999639 ) ) ;
#45567 = PRODUCT_DEFINITION_SHAPE ( 'NONE', 'NONE',  #2199 ) ;
#45568 = CARTESIAN_POINT ( 'NONE',  ( 18.18591139755467623, 2.124730565513604841, -12.41957995629783973 ) ) ;
#45569 = CARTESIAN_POINT ( 'NONE',  ( 2.521806799209333150, 3.408904368339103375, 0.9161175952574877046 ) ) ;
#45570 = CARTESIAN_POINT ( 'NONE',  ( 5.407309473667999633, 12.95251760905999916, 1.915207572621000054 ) ) ;
#45571 = CARTESIAN_POINT ( 'NONE',  ( 12.27416439412415450, 2.829982835813917408, -13.59791655271627064 ) ) ;
#45572 = CARTESIAN_POINT ( 'NONE',  ( 9.795911616191999016, -5.239375073306999475, -6.095351682555999240 ) ) ;
#45573 = CARTESIAN_POINT ( 'NONE',  ( 25.41677650706899882, 11.20716069352000055, 3.225949357593000055 ) ) ;
#45574 = VERTEX_POINT ( 'NONE', #38414 ) ;
#45575 = LINE ( 'NONE', #68245, #36656 ) ;
#45576 = CARTESIAN_POINT ( 'NONE',  ( 12.15994429558105239, -0.3334496638227552046, -13.99603244703262739 ) ) ;
#45577 = CARTESIAN_POINT ( 'NONE',  ( 44.24148000000000280, -11.77655473258999841, -4.190794510628000680 ) ) ;
#45578 = CARTESIAN_POINT ( 'NONE',  ( 18.17481653531215358, -2.416771143973758029, -13.69072451366435672 ) ) ;
#45579 = CARTESIAN_POINT ( 'NONE',  ( 3.040556799211332706, 3.500000000000000888, -0.4581489286485045387 ) ) ;
#45580 = CARTESIAN_POINT ( 'NONE',  ( 9.667489158770999680, 4.808846957865000604, -8.639578604182998944 ) ) ;
#45581 = CARTESIAN_POINT ( 'NONE',  ( 12.21210404293059959, -4.381818659177399766, 6.722495590581700320 ) ) ;
#45582 = ORIENTED_EDGE ( 'NONE', *, *, #27470, .T. ) ;
#45583 = CARTESIAN_POINT ( 'NONE',  ( 5.000000000000000000, 0.6769230769231000533, -2.665384615385000266 ) ) ;
#45584 = CARTESIAN_POINT ( 'NONE',  ( 18.08228063350337678, 2.164202898012135723, -13.73897034938254968 ) ) ;
#45585 = ORIENTED_EDGE ( 'NONE', *, *, #156, .T. ) ;
#45586 = CARTESIAN_POINT ( 'NONE',  ( 10.13667167105699995, -4.855035690642299784, 7.356396684460199786 ) ) ;
#45587 = CARTESIAN_POINT ( 'NONE',  ( 11.09999999999999964, -4.000000000000000000, -7.500000000000000000 ) ) ;
#45588 = EDGE_CURVE ( 'NONE', #50903, #48489, #23059, .T. ) ;
#45589 = CARTESIAN_POINT ( 'NONE',  ( 8.754720280412998434, 5.687930027805999877, -7.109876198051000351 ) ) ;
#45590 = CARTESIAN_POINT ( 'NONE',  ( 24.07543054079696532, -12.58937790781994792, 3.411500176492500369 ) ) ;
#45591 = CARTESIAN_POINT ( 'NONE',  ( 10.85168717260509830, -4.613789146762799831, -8.501809683958001074 ) ) ;
#45592 = CARTESIAN_POINT ( 'NONE',  ( 17.94293909947463561, 0.4900986449918856569, -12.68726951834973349 ) ) ;
#45593 = ADVANCED_FACE ( 'NONE', ( #43670 ), #54625, .F. ) ;
#45594 = CIRCLE ( 'NONE', #43340, 11.50000000000000533 ) ;
#45595 = FACE_OUTER_BOUND ( 'NONE', #31662, .T. ) ;
#45596 = ORIENTED_EDGE ( 'NONE', *, *, #23269, .F. ) ;
#45597 = CARTESIAN_POINT ( 'NONE',  ( 25.49995753756342864, 8.603837101912144902, -7.325400450398672270 ) ) ;
#45598 = CARTESIAN_POINT ( 'NONE',  ( 10.83351354018233259, -5.249999999999999112, 7.663624617374471093 ) ) ;
#45599 = CARTESIAN_POINT ( 'NONE',  ( 6.649999999999999467, 5.221516520829000640, -8.074802043613001246 ) ) ;
#45600 = ORIENTED_EDGE ( 'NONE', *, *, #28113, .F. ) ;
#45601 = CARTESIAN_POINT ( 'NONE',  ( 10.69578011722000177, 5.505003832924999507, -7.759263776825999770 ) ) ;
#45602 = EDGE_LOOP ( 'NONE', ( #41362, #11270, #51082, #17464, #12903, #42249, #2035 ) ) ;
#45603 = CARTESIAN_POINT ( 'NONE',  ( 8.695468108405998819, 5.098602956001000663, 7.188863445572599709 ) ) ;
#45604 = CARTESIAN_POINT ( 'NONE',  ( 18.05281416665461336, -3.003450933888336838, -12.23680105844127652 ) ) ;
#45605 = DIRECTION ( 'NONE',  ( 1.000000000000000000, 0.000000000000000000, 0.000000000000000000 ) ) ;
#45606 = CARTESIAN_POINT ( 'NONE',  ( 11.04230989607018643, 2.757690103929812064, 6.361542621410388065 ) ) ;
#45607 = AXIS2_PLACEMENT_3D ( 'NONE', #38334, #48833, #6864 ) ;
#45608 = CARTESIAN_POINT ( 'NONE',  ( 8.428197172116266955, 5.125396288426561142, 6.749639981083130458 ) ) ;
#45609 = CARTESIAN_POINT ( 'NONE',  ( 9.409377086007973290, -2.477133334551472110, 8.340513213184692631 ) ) ;
#45610 = ORIENTED_EDGE ( 'NONE', *, *, #15055, .T. ) ;
#45611 = CARTESIAN_POINT ( 'NONE',  ( 24.62620337095130907, -3.584633747652771429, 12.20158770660386161 ) ) ;
#45612 = B_SPLINE_CURVE_WITH_KNOTS ( 'NONE', 3,
 ( #68674, #15884, #36527, #42122 ),
 .UNSPECIFIED., .F., .F.,
 ( 4, 4 ),
 ( 0.4999999998439638160, 1.000000000000000000 ),
 .UNSPECIFIED. ) ;
#45613 = FACE_OUTER_BOUND ( 'NONE', #66322, .T. ) ;
#45614 = CARTESIAN_POINT ( 'NONE',  ( 8.455992358769000461, 4.599999999999999645, 6.571291218974000259 ) ) ;
#45615 = CARTESIAN_POINT ( 'NONE',  ( 12.17479962224109435, 2.156383435693109529, -13.83294862407085901 ) ) ;
#45616 = CARTESIAN_POINT ( 'NONE',  ( 9.355088727410999283, -5.274736981944999847, -7.606911245136100064 ) ) ;
#45617 = CARTESIAN_POINT ( 'NONE',  ( 9.352255147285999826, -2.817754448466000206, 6.388456890282999900 ) ) ;
#45618 = CARTESIAN_POINT ( 'NONE',  ( 18.24178265820143352, 0.2353130933619127785, 13.99804086085458721 ) ) ;
#45619 = DIRECTION ( 'NONE',  ( 1.000000000000000000, 0.000000000000000000, 0.000000000000000000 ) ) ;
#45620 = EDGE_CURVE ( 'NONE', #8503, #45133, #59054, .T. ) ;
#45621 = ORIENTED_EDGE ( 'NONE', *, *, #10584, .T. ) ;
#45622 = ORIENTED_EDGE ( 'NONE', *, *, #66755, .F. ) ;
#45623 = CARTESIAN_POINT ( 'NONE',  ( 8.491329719591000469, 4.851303550474000303, -9.008742670124000540 ) ) ;
#45624 = DIRECTION ( 'NONE',  ( 0.7071067811866525998, 0.000000000000000000, -0.7071067811864425456 ) ) ;
#45625 = EDGE_CURVE ( 'NONE', #48149, #52223, #50691, .T. ) ;
#45626 = EDGE_CURVE ( 'NONE', #59620, #7868, #21440, .T. ) ;
#45627 = CARTESIAN_POINT ( 'NONE',  ( 12.18501279890337052, -2.418803504714349017, 13.69036126159378775 ) ) ;
#45628 = CARTESIAN_POINT ( 'NONE',  ( 24.30001683570900184, 3.271769286791000209, 12.21048169671000139 ) ) ;
#45629 = CARTESIAN_POINT ( 'NONE',  ( 23.64132359913000059, 10.11790787233000088, -9.385294766974999092 ) ) ;
#45630 = CARTESIAN_POINT ( 'NONE',  ( 18.31802873821099809, -2.927761598026000112, -11.42873208727000112 ) ) ;
#45632 = CARTESIAN_POINT ( 'NONE',  ( 11.01655351471000088, -5.424347081247000268, 4.991940595874999609 ) ) ;
#45631 = CARTESIAN_POINT ( 'NONE',  ( 10.35965911260399963, -4.496147888241900148, 6.471616938597000157 ) ) ;
#45633 = DIRECTION ( 'NONE',  ( -0.7071058580588949205, -0.7071077043129949669, 4.007446525297969874E-09 ) ) ;
#45634 = ORIENTED_EDGE ( 'NONE', *, *, #56523, .T. ) ;
#45635 = CARTESIAN_POINT ( 'NONE',  ( 10.32998539982999908, -3.095235127366999794, 4.624383164039000071 ) ) ;
#45636 = VECTOR ( 'NONE', #64123, 1000.000000000000114 ) ;
#45637 = CARTESIAN_POINT ( 'NONE',  ( 23.89320776801300283, -10.75689324692999804, -4.023240149044999825 ) ) ;
#45638 = CARTESIAN_POINT ( 'NONE',  ( 10.00107860442999907, -4.626219091573998909, -9.027249334595000008 ) ) ;
#45639 = CARTESIAN_POINT ( 'NONE',  ( 17.80401300531091024, 0.5733651658914310500, 12.68257300503909590 ) ) ;
#45640 = CARTESIAN_POINT ( 'NONE',  ( 12.40964703146719650, -0.4840289222540395397, 12.68758247551644125 ) ) ;
#45641 = CARTESIAN_POINT ( 'NONE',  ( 5.500000000000000000, -12.65263727151999795, 3.063503113339999917 ) ) ;
#45642 = ORIENTED_EDGE ( 'NONE', *, *, #26125, .T. ) ;
#45643 = DIRECTION ( 'NONE',  ( 1.000000000000000000, 0.000000000000000000, 0.000000000000000000 ) ) ;
#45644 = CARTESIAN_POINT ( 'NONE',  ( 9.342560841233000346, 5.835196551504000517, -7.008466539623000813 ) ) ;
#45645 = EDGE_CURVE ( 'NONE', #47743, #65548, #17792, .T. ) ;
#45646 = CARTESIAN_POINT ( 'NONE',  ( 25.46372779695100164, -11.23407511953000082, -3.161075425950000017 ) ) ;
#45647 = FILL_AREA_STYLE_COLOUR ( '', #60153 ) ;
#45648 = CARTESIAN_POINT ( 'NONE',  ( 0.3474143384075761842, -2.924575863667731035, 1.686609425636008908 ) ) ;
#45649 = CARTESIAN_POINT ( 'NONE',  ( 3.730112762836999885, 1.979060574517999882, -2.346675849479999965 ) ) ;
#45650 = ORIENTED_EDGE ( 'NONE', *, *, #41065, .T. ) ;
#45651 = CARTESIAN_POINT ( 'NONE',  ( 12.42151672539423579, 0.6105138165312113951, -12.58520200551375545 ) ) ;
#45652 = CARTESIAN_POINT ( 'NONE',  ( 12.80505043854146940, -1.875000000000000444, -12.57541666120756396 ) ) ;
#45653 = DIRECTION ( 'NONE',  ( 0.000000000000000000, 0.000000000000000000, 1.000000000000000000 ) ) ;
#45654 = CARTESIAN_POINT ( 'NONE',  ( 8.064114158772998309, 4.228291488957999888, 8.941375734143997889 ) ) ;
#45655 = CARTESIAN_POINT ( 'NONE',  ( 5.200000002332999749, 0.2500000023327000331, -3.149999979209999967 ) ) ;
#45656 = ORIENTED_EDGE ( 'NONE', *, *, #59342, .T. ) ;
#45657 = CARTESIAN_POINT ( 'NONE',  ( 5.398974669483000532, -0.7389799844016000652, 1.268943043503000023 ) ) ;
#45658 = CARTESIAN_POINT ( 'NONE',  ( 10.90570892106003065, 9.799753219705101159, 5.723325390456533768 ) ) ;
#45659 = CARTESIAN_POINT ( 'NONE',  ( 10.76290585702710523, 2.920651757519677538, -8.329491109684418859 ) ) ;
#45660 = AXIS2_PLACEMENT_3D ( 'NONE', #68447, #63202, #36306 ) ;
#45661 = CARTESIAN_POINT ( 'NONE',  ( 1.521806799207250149, 3.408904368339103375, 0.9161175952574877046 ) ) ;
#45662 = CARTESIAN_POINT ( 'NONE',  ( 11.10101463001529964, 4.622233839778099984, -6.503413421344399481 ) ) ;
#45663 = ORIENTED_EDGE ( 'NONE', *, *, #12563, .F. ) ;
#45664 = CARTESIAN_POINT ( 'NONE',  ( 10.90638082498000117, -5.227498618488000126, 6.784459667733999666 ) ) ;
#45665 = ORIENTED_EDGE ( 'NONE', *, *, #57375, .T. ) ;
#45666 = LINE ( 'NONE', #55117, #62991 ) ;
#45667 = CARTESIAN_POINT ( 'NONE',  ( 8.213543146793000460, -3.608524635952000459, 5.913372239166000632 ) ) ;
#45668 = CARTESIAN_POINT ( 'NONE',  ( 17.96742444759811974, -0.6007076874295256275, -13.98710814480368114 ) ) ;
#45669 = ORIENTED_EDGE ( 'NONE', *, *, #24919, .F. ) ;
#45670 = CARTESIAN_POINT ( 'NONE',  ( 10.90000053908999966, 9.856474340180000127, -5.627824942316999923 ) ) ;
#45671 = CARTESIAN_POINT ( 'NONE',  ( 9.299999999999998934, 4.537600397704999899, 9.154563893594000135 ) ) ;
#45672 = DIRECTION ( 'NONE',  ( 0.000000000000000000, -1.000000000000000000, 0.000000000000000000 ) ) ;
#45673 = ADVANCED_FACE ( 'NONE', ( #38065, #59390 ), #22673, .F. ) ;
#45674 = CARTESIAN_POINT ( 'NONE',  ( 9.101497196731600070, -2.899999999999999911, 6.350512455778112297 ) ) ;
#45675 = CARTESIAN_POINT ( 'NONE',  ( 17.83355475040677973, -3.059894173690222541, 12.30333952404826370 ) ) ;
#45676 = VERTEX_POINT ( 'NONE', #35594 ) ;
#45677 = CARTESIAN_POINT ( 'NONE',  ( 10.65050275296000137, -5.200029647236999786, 5.937716681140000397 ) ) ;
#45678 = CARTESIAN_POINT ( 'NONE',  ( 12.18524893065073655, -2.418966797217242171, -13.69026124204716588 ) ) ;
#45679 = CARTESIAN_POINT ( 'NONE',  ( 10.57101354018312023, 4.768183399968643599, -8.499583552997725278 ) ) ;
#45680 = CARTESIAN_POINT ( 'NONE',  ( 9.852263540182327972, 2.907767014557178342, 8.129523725463624118 ) ) ;
#45681 = DIRECTION ( 'NONE',  ( -1.000000000000000000, 0.000000000000000000, 0.000000000000000000 ) ) ;
#45682 = ORIENTED_EDGE ( 'NONE', *, *, #59925, .T. ) ;
#45683 = CYLINDRICAL_SURFACE ( 'NONE', #26082, 1.350000000000000533 ) ;
#45684 = CARTESIAN_POINT ( 'NONE',  ( 8.824071121570657539, -3.025928824985223198, -7.248446557932072487 ) ) ;
#45685 = CARTESIAN_POINT ( 'NONE',  ( 10.71685100253999856, 2.832432432432000269, 6.822293592207000934 ) ) ;
#45686 = CARTESIAN_POINT ( 'NONE',  ( 9.073148997461000675, -5.167567567567999731, -6.822293592207000934 ) ) ;
#45687 = DIRECTION ( 'NONE',  ( 0.000000000000000000, 0.8514547570628039352, -0.5244280662542016858 ) ) ;
#45688 = AXIS2_PLACEMENT_3D ( 'NONE', #3975, #34791, #18705 ) ;
#45689 = CARTESIAN_POINT ( 'NONE',  ( 12.18832812670980914, 0.1018973686818595847, -13.89950237059084870 ) ) ;
#45690 = CARTESIAN_POINT ( 'NONE',  ( 17.78721996965305507, -1.919630126996079600, 12.56804012644223079 ) ) ;
#45691 = ORIENTED_EDGE ( 'NONE', *, *, #25332, .T. ) ;
#45692 = CARTESIAN_POINT ( 'NONE',  ( 11.64633327354034797, -4.864904118400500188, -6.934277916748599502 ) ) ;
#45693 = ORIENTED_EDGE ( 'NONE', *, *, #66910, .T. ) ;
#45694 = CARTESIAN_POINT ( 'NONE',  ( 10.20319667131999886, 3.421760346951000287, 6.017732782098999422 ) ) ;
#45695 = LINE ( 'NONE', #19113, #66858 ) ;
#45696 = CARTESIAN_POINT ( 'NONE',  ( 10.01508584123000034, 4.845406482350000488, -6.387189183984999907 ) ) ;
#45697 = CARTESIAN_POINT ( 'NONE',  ( 3.138669809652000264, -2.989695960142000342, 1.902536878218999972 ) ) ;
#45698 = CARTESIAN_POINT ( 'NONE',  ( 10.31499432720999998, -5.458372854186999135, -8.355103994551999591 ) ) ;
#45699 = CARTESIAN_POINT ( 'NONE',  ( 10.20000030442999872, 12.49999969551000056, -3.568568717444000015E-10 ) ) ;
#45700 = CARTESIAN_POINT ( 'NONE',  ( 9.626866900951128514, -2.437244704642051119, -6.713792515457897458 ) ) ;
#45701 = EDGE_LOOP ( 'NONE', ( #33975, #53565, #47690, #3788 ) ) ;
#45702 = CARTESIAN_POINT ( 'NONE',  ( 11.51456785386839954, -4.946394603182100447, 6.863111178199799767 ) ) ;
#45703 = CARTESIAN_POINT ( 'NONE',  ( 10.62697636434999993, 3.142921793056999924, 8.668445734229999644 ) ) ;
#45704 = ADVANCED_FACE ( 'NONE', ( #19505 ), #30016, .T. ) ;
#45705 = CARTESIAN_POINT ( 'NONE',  ( 15.40000000001299973, 8.815237407733999220, 7.616696375847999967 ) ) ;
#45706 = DIRECTION ( 'NONE',  ( 0.000000000000000000, 0.9549051095264925459, -0.2969111513570973915 ) ) ;
#45708 = CARTESIAN_POINT ( 'NONE',  ( 23.59999176271200128, 13.22318677037999812, 4.267778497637999102 ) ) ;
#45707 = CARTESIAN_POINT ( 'NONE',  ( 10.37373942323999998, 2.215265813302000009, 7.703982730183001060 ) ) ;
#45709 = CARTESIAN_POINT ( 'NONE',  ( 10.30487885159599770, 4.996404279947399552, -7.381132626649399064 ) ) ;
#45710 = B_SPLINE_CURVE_WITH_KNOTS ( 'NONE', 3,
 ( #23211, #11672, #22166, #53981, #44559, #33011, #28822, #48746, #2238, #65503, #23552, #12378, #66196, #54326, #27777, #49087, #1199, #43850, #38956, #17975, #59919, #39294, #18318, #12028, #60962, #33364, #6777 ),
 .UNSPECIFIED., .F., .F.,
 ( 4, 2, 2, 2, 2, 2, 2, 2, 2, 2, 1, 2, 2, 4 ),
 ( 0.000000000000000000, 0.1249999999999979183, 0.1874999999999976963, 0.2499999999999975020, 0.3124999999999972800, 0.3749999999999970579, 0.4374999999999968914, 0.4999999999999966693, 0.6249999999999976685, 0.7499999999999986677, 0.8124999999999992228, 0.8437499999999992228, 0.8749999999999993339, 1.000000000000000000 ),
 .UNSPECIFIED. ) ;
#45711 = CARTESIAN_POINT ( 'NONE',  ( 10.90000000000000036, -0.2999999999999999889, -4.902439024389999567 ) ) ;
#45712 = CARTESIAN_POINT ( 'NONE',  ( 9.908304848515998131, 4.913464051101100516, -7.917643062525700159 ) ) ;
#45713 = CARTESIAN_POINT ( 'NONE',  ( 17.64985999057966026, -0.7135009822674878155, 12.57978225961208807 ) ) ;
#45714 = CARTESIAN_POINT ( 'NONE',  ( 11.07299956498199833, 5.207010770456999893, -7.825000000000000178 ) ) ;
#45715 = CARTESIAN_POINT ( 'NONE',  ( 5.000015393671500163, -2.571712834666313134E-16, -2.099962892531002545 ) ) ;
#45716 = CARTESIAN_POINT ( 'NONE',  ( 9.248821772879615821, -3.697635112905263366, 6.625936606111492821 ) ) ;
#45717 = ORIENTED_EDGE ( 'NONE', *, *, #22654, .F. ) ;
#45718 = CARTESIAN_POINT ( 'NONE',  ( 8.411456853209999807, -3.882020254083999866, 5.870054788755000530 ) ) ;
#45719 = CARTESIAN_POINT ( 'NONE',  ( 18.18935690068781241, 2.871730747427965191, 13.70230915895854018 ) ) ;
#45720 = ADVANCED_FACE ( 'NONE', ( #19155 ), #18477, .T. ) ;
#45721 = DIRECTION ( 'NONE',  ( 1.000000000000000000, 0.000000000000000000, 3.552713678820000309E-14 ) ) ;
#45722 = CARTESIAN_POINT ( 'NONE',  ( 10.31746213571000048, 5.100000000000000533, 6.571291218949999902 ) ) ;
#45723 = ORIENTED_EDGE ( 'NONE', *, *, #40069, .F. ) ;
#45724 = EDGE_CURVE ( 'NONE', #52017, #31558, #40477, .T. ) ;
#45725 = CARTESIAN_POINT ( 'NONE',  ( 8.347267219593000220, 2.741641653469999884, 6.457329666915000210 ) ) ;
#45727 = CARTESIAN_POINT ( 'NONE',  ( 11.51145123989532948, 4.605239108938600445, 6.331134574721999364 ) ) ;
#45726 = CARTESIAN_POINT ( 'NONE',  ( 9.104759580228998672, -4.843256805554699618, -7.298441312785299395 ) ) ;
#45728 = CARTESIAN_POINT ( 'NONE',  ( 10.49411415877000131, 2.866942652264999669, -8.960728730887002058 ) ) ;
#45729 = ORIENTED_EDGE ( 'NONE', *, *, #58981, .T. ) ;
#45730 = CARTESIAN_POINT ( 'NONE',  ( 5.232109839683333874, 0.9218200799623741393, -1.199500263597268690 ) ) ;
#45731 = CARTESIAN_POINT ( 'NONE',  ( 18.21591247723855034, -2.819087736749462003, -13.71325046847544193 ) ) ;
#45732 = CARTESIAN_POINT ( 'NONE',  ( 10.57149279008999798, 3.703313553258400059, 6.398515879103999993 ) ) ;
#45733 = CARTESIAN_POINT ( 'NONE',  ( 11.00366278039000001, -2.264082614160999984, 7.798350693290999835 ) ) ;
#45734 = FACE_OUTER_BOUND ( 'NONE', #57273, .T. ) ;
#45735 = ORIENTED_EDGE ( 'NONE', *, *, #701, .F. ) ;
#45736 = CARTESIAN_POINT ( 'NONE',  ( 11.71260115691700143, -3.298410940261000235, 11.83433202606999934 ) ) ;
#45737 = CARTESIAN_POINT ( 'NONE',  ( 10.34939194037999854, -2.653148377029999949, -7.312413909354000374 ) ) ;
#45738 = CARTESIAN_POINT ( 'NONE',  ( 7.931404649784815852, -2.307123594424923319, 7.902069134632180081 ) ) ;
#45739 = CARTESIAN_POINT ( 'NONE',  ( 9.352255147285999826, -2.817754448466000206, 6.388456890282999900 ) ) ;
#45740 = CARTESIAN_POINT ( 'NONE',  ( 11.10101463001529964, -3.377766160221900016, -6.503413421344399481 ) ) ;
#45741 = CARTESIAN_POINT ( 'NONE',  ( 10.56122949779699915, -3.290320231472799950, 6.435697190503999465 ) ) ;
#45742 = ORIENTED_EDGE ( 'NONE', *, *, #31710, .F. ) ;
#45743 = CARTESIAN_POINT ( 'NONE',  ( 2.750973465876000557, -3.500000000000000000, 0.000000000000000000 ) ) ;
#45744 = DIRECTION ( 'NONE',  ( -1.000000000000000000, 0.000000000000000000, 0.000000000000000000 ) ) ;
#45745 = EDGE_LOOP ( 'NONE', ( #3856, #28991, #10416 ) ) ;
#45746 = CARTESIAN_POINT ( 'NONE',  ( 18.29995268966800026, -2.861739928647000220, -11.98821236628000086 ) ) ;
#45747 = ORIENTED_EDGE ( 'NONE', *, *, #68687, .F. ) ;
#45748 = CARTESIAN_POINT ( 'NONE',  ( 9.795737326637999232, -4.289037785427000316, -5.816478295321999781 ) ) ;
#45749 = CARTESIAN_POINT ( 'NONE',  ( 9.798945280410000791, 5.639765292528999829, -8.059103558718000215 ) ) ;
#45750 = DIRECTION ( 'NONE',  ( 0.000000000000000000, -1.000000000000000000, 0.000000000000000000 ) ) ;
#45751 = DIRECTION ( 'NONE',  ( -1.000000000000000000, 0.000000000000000000, 0.000000000000000000 ) ) ;
#45752 = CARTESIAN_POINT ( 'NONE',  ( 12.31295406811161719, 2.114551508724274775, -12.53308940647968761 ) ) ;
#45753 = CARTESIAN_POINT ( 'NONE',  ( 11.10026222744819790, -4.774534945026900346, 6.861998062869400172 ) ) ;
#45754 = CARTESIAN_POINT ( 'NONE',  ( 7.988545280410000338, 3.566637212418000136, 5.743604853744000316 ) ) ;
#45755 = EDGE_LOOP ( 'NONE', ( #45956, #58807, #26164, #28296, #24932, #29255, #34290, #45063, #52450, #6294 ) ) ;
#45756 = AXIS2_PLACEMENT_3D ( 'NONE', #60186, #47970, #38506 ) ;
#45757 = CARTESIAN_POINT ( 'NONE',  ( 9.729346873516670158, 3.836375382625535124, 8.750000000000000000 ) ) ;
#45758 = CARTESIAN_POINT ( 'NONE',  ( 7.802019353206999241, -5.638700495537999124, 8.266402903491000487 ) ) ;
#45759 = CARTESIAN_POINT ( 'NONE',  ( 17.60357723839708299, 0.7301778992647629529, 13.98094561311457618 ) ) ;
#45760 = ORIENTED_EDGE ( 'NONE', *, *, #35769, .T. ) ;
#45761 = B_SPLINE_SURFACE_WITH_KNOTS ( 'NONE', 3, 3, ( 
 ( #25733, #9644, #41133, #3370, #51950, #62443, #30640, #65712, #13878, #46377, #9299, #36226, #17834, #14564, #24708, #67677, #51611, #62781, #57540, #39153, #30992, #60476, #35882, #46724, #52301, #25045, #12584, #35549, #14902, #46030, #4398, #33914, #55231, #57197, #56867 ),
 ( #4049, #29973, #25386, #24362, #8286, #68029, #67337, #8625, #14222, #8964, #40433, #35209, #29631, #50933, #20143, #45694, #41473, #3032, #67002, #30304, #19111, #61759, #56520, #51276, #3706, #19458, #40778, #62102, #19805, #21855, #31673, #4736, #9993, #31331, #47065 ),
 ( #52644, #54014, #15590, #26080, #47409, #57893, #26427, #58576, #68713, #48091, #64494, #43189, #542, #5091, #16614, #10679, #20832, #42167, #53340, #63467, #37594, #16269, #20487, #58928, #36919, #195, #36569, #5442, #48433, #64157, #47758, #6116, #58235, #41813, #52995 ),
 ( #26779, #69068, #63120, #10338, #21174, #11029, #15246, #42505, #68368, #63813, #15924, #37257, #21512, #37939, #59261, #42845, #11364, #32368, #32027, #53682, #32702, #5775, #27118, #59954, #1925, #22543, #888, #33745, #65538, #43539, #6812, #50165, #49460, #17307, #38986 ) ),
 .UNSPECIFIED., .F., .F., .F.,
 ( 4, 4 ),
 ( 4, 1, 1, 1, 1, 1, 1, 1, 1, 1, 1, 1, 1, 1, 1, 1, 1, 1, 1, 1, 1, 1, 1, 1, 1, 1, 1, 1, 1, 1, 1, 1, 4 ),
 ( -0.1039370721279000015, 1.103937072127999963 ),
 ( -0.01735257130020999988, 0.01084535706264999969, 0.03904328542550000031, 0.06724121378835999641, 0.09543914215121999944, 0.1236370705141000004, 0.1518349988768999959, 0.1800329272397999947, 0.2082308556026999935, 0.2364287839655000167, 0.2646267123283999601, 0.2928246406912000110, 0.3210225690540999821, 0.3492204974169000331, 0.3774184257798000042, 0.4056163541427000307, 0.4338142825054999707, 0.4620122108683999973, 0.4902101392311999928, 0.5184080675940999638, 0.5466059959569999904, 0.5748039243197999859, 0.6030018526827000125, 0.6311997810455000080, 0.6593977094084000345, 0.6875956377712000300, 0.7157935661340999456, 0.7439914944969999722, 0.7721894228597999676, 0.8003873512226999942, 0.8285852795854999897, 0.8567832079484000163, 0.8849811363112999318 ),
 .UNSPECIFIED. ) ;
#45762 = CARTESIAN_POINT ( 'NONE',  ( 12.10312773382969453, -2.298350437047144812, -12.38862788998081754 ) ) ;
#45763 = CARTESIAN_POINT ( 'NONE',  ( 11.62579573085663043, 5.239377455231000624, 7.285547569258399747 ) ) ;
#45764 = CARTESIAN_POINT ( 'NONE',  ( 10.63743064679000128, -3.721475434679999861, -8.997096235511000017 ) ) ;
#45765 = CARTESIAN_POINT ( 'NONE',  ( 6.502943173016666911, -1.199500263597274241, 0.9218200799623669228 ) ) ;
#45766 = CARTESIAN_POINT ( 'NONE',  ( 17.56043577778200060, -12.16710011284000181, 3.134847618462999641 ) ) ;
#45767 = CARTESIAN_POINT ( 'NONE',  ( 9.015584277044482064, 3.283082709547154643, -8.431467892494236338 ) ) ;
#45768 = CARTESIAN_POINT ( 'NONE',  ( 12.19623795424366897, -2.642762699020543060, -13.64211084970869692 ) ) ;
#45769 = CARTESIAN_POINT ( 'NONE',  ( 17.55505043854144631, -0.6250000000000001110, -12.67928921589118652 ) ) ;
#45770 = DIRECTION ( 'NONE',  ( 1.000000000000000000, 0.000000000000000000, 0.000000000000000000 ) ) ;
#45771 = CARTESIAN_POINT ( 'NONE',  ( 10.71503032197929883, -3.256621462143499901, -6.460430507351999196 ) ) ;
#45772 = CARTESIAN_POINT ( 'NONE',  ( 8.474485200571999499, -5.100000000000000533, 6.560614371780999043 ) ) ;
#45773 = EDGE_LOOP ( 'NONE', ( #50998, #19728, #47619, #50688, #3519 ) ) ;
#45774 = VERTEX_POINT ( 'NONE', #29321 ) ;
#45775 = CARTESIAN_POINT ( 'NONE',  ( 12.65360965127988813, -11.23193385081858331, 3.094113056522455718 ) ) ;
#45776 = CARTESIAN_POINT ( 'NONE',  ( 17.86920599199770265, 3.040695425030093713, 13.54374392800313132 ) ) ;
#45777 = CARTESIAN_POINT ( 'NONE',  ( 23.91260411953700071, -3.265466992718999872, 12.84004109222999901 ) ) ;
#45778 = DIRECTION ( 'NONE',  ( 0.000000000000000000, -0.9565994702956989171, 0.2914059941558995170 ) ) ;
#45779 = CARTESIAN_POINT ( 'NONE',  ( 17.94652436847575672, 2.012680451140230531, 12.55183781965936696 ) ) ;
#45780 = FACE_OUTER_BOUND ( 'NONE', #47812, .T. ) ;
#45781 = CARTESIAN_POINT ( 'NONE',  ( 10.22108913916999917, 2.983268757921999637, 8.764704075288999974 ) ) ;
#45782 = CARTESIAN_POINT ( 'NONE',  ( 10.25047016403776823, -3.823336794438516151, -8.849920973562444004 ) ) ;
#45783 = ADVANCED_FACE ( 'NONE', ( #56221 ), #24406, .T. ) ;
#45784 = ORIENTED_EDGE ( 'NONE', *, *, #69045, .F. ) ;
#45785 = CARTESIAN_POINT ( 'NONE',  ( 12.61707675448782773, -1.903914349653180516, 12.57067604690442586 ) ) ;
#45786 = ADVANCED_FACE ( 'NONE', ( #45393, #39803 ), #12890, .T. ) ;
#45787 = CARTESIAN_POINT ( 'NONE',  ( 9.528367640780999182, -3.526522998810799781, -6.614188603779100006 ) ) ;
#45788 = CARTESIAN_POINT ( 'NONE',  ( 11.07345995138000028, 3.998673170817999889, 8.920816085870999501 ) ) ;
#45789 = CARTESIAN_POINT ( 'NONE',  ( 11.02799293566599914, -3.193321847920899792, 6.510429574318199464 ) ) ;
#45790 = CARTESIAN_POINT ( 'NONE',  ( 10.15303300763299887, 4.787165141710600480, -8.325626572044798834 ) ) ;
#45791 = CARTESIAN_POINT ( 'NONE',  ( 12.18201988759300036, -0.05063260980701941860, 12.69986973508908079 ) ) ;
#45792 = CARTESIAN_POINT ( 'NONE',  ( 8.481676658773000810, 2.472348777564000066, 6.234194744024999402 ) ) ;
#45793 = CARTESIAN_POINT ( 'NONE',  ( 10.34520858566999912, 2.724123081339000052, 6.497325124886000225 ) ) ;
#45794 = CARTESIAN_POINT ( 'NONE',  ( 12.60184172746868114, 1.908867898185655054, 12.56980895172865687 ) ) ;
#45795 = ORIENTED_EDGE ( 'NONE', *, *, #59514, .T. ) ;
#45796 = CARTESIAN_POINT ( 'NONE',  ( 25.36465253276900000, 8.490056772567001531, 7.944948624166999984 ) ) ;
#45797 = CARTESIAN_POINT ( 'NONE',  ( 10.41964694612699915, 2.813019656517000477, -7.973702485506099613 ) ) ;
#45798 = CARTESIAN_POINT ( 'NONE',  ( 10.65216644777291854, -5.457257952748706842, 6.517891258330301696 ) ) ;
#45800 = CARTESIAN_POINT ( 'NONE',  ( 10.17726354018233437, 4.629523725463628558, 8.592232985442819881 ) ) ;
#45799 = CARTESIAN_POINT ( 'NONE',  ( 25.30000327618300204, 8.756202924575998026, 7.455126447192999883 ) ) ;
#45801 = CARTESIAN_POINT ( 'NONE',  ( 10.38795058442699926, -3.601336184534900120, 8.421905343605699201 ) ) ;
#45802 = AXIS2_PLACEMENT_3D ( 'NONE', #21404, #42400, #53226 ) ;
#45803 = CARTESIAN_POINT ( 'NONE',  ( 10.60026222744819790, -4.774534945026900346, -8.138001937130599828 ) ) ;
#45804 = ORIENTED_EDGE ( 'NONE', *, *, #1932, .T. ) ;
#45805 = CARTESIAN_POINT ( 'NONE',  ( 2.154202210879000212, -0.2286091751511999948, 3.751814989407999956 ) ) ;
#45806 = EDGE_CURVE ( 'NONE', #43188, #10178, #45555, .T. ) ;
#45807 = CARTESIAN_POINT ( 'NONE',  ( 17.75512362481055106, -0.5924617913105076905, -12.68139389763045521 ) ) ;
#45809 = CARTESIAN_POINT ( 'NONE',  ( 11.56599877858000092, 3.774257655232999831, -11.98333518513999962 ) ) ;
#45808 = CARTESIAN_POINT ( 'NONE',  ( 11.04677151279999947, -2.764386413791999786, -5.039776830043000366 ) ) ;
#45810 = CARTESIAN_POINT ( 'NONE',  ( 11.03776785110999903, 5.237767851104999650, 6.571291218949999902 ) ) ;
#45811 = CARTESIAN_POINT ( 'NONE',  ( 10.07102359808000003, 4.042170458878000083, 8.920189456109998360 ) ) ;
#45812 = CARTESIAN_POINT ( 'NONE',  ( 12.61614725291588890, -3.223296771745977285, 13.62389115065821699 ) ) ;
#45813 = DIRECTION ( 'NONE',  ( 1.000000000000000000, 0.000000000000000000, 9.841108777351999576E-13 ) ) ;
#45814 = CARTESIAN_POINT ( 'NONE',  ( 21.10000109091659937, 12.52500000000000036, 0.000000000000000000 ) ) ;
#45815 = CARTESIAN_POINT ( 'NONE',  ( 8.271691940379001906, -5.629389383493999865, 8.631822608164000599 ) ) ;
#45816 = ORIENTED_EDGE ( 'NONE', *, *, #13106, .T. ) ;
#45817 = CARTESIAN_POINT ( 'NONE',  ( 7.464691113743000095, 4.351669901925999895, 8.977196921526999773 ) ) ;
#45818 = CYLINDRICAL_SURFACE ( 'NONE', #66380, 11.84999999999999964 ) ;
#45819 = CARTESIAN_POINT ( 'NONE',  ( 7.412945637235106133, -2.444942208937388894, 8.282280356623708428 ) ) ;
#45820 = DIRECTION ( 'NONE',  ( 0.4384236320213996119, 0.6355252626312996034, 0.6355252626312996034 ) ) ;
#45821 = CARTESIAN_POINT ( 'NONE',  ( 0.7419268129216000096, 3.132555770593000055, 1.386468609675000074 ) ) ;
#45822 = ORIENTED_EDGE ( 'NONE', *, *, #36724, .T. ) ;
#45823 = DIRECTION ( 'NONE',  ( 1.000000000000000000, 0.000000000000000000, 0.000000000000000000 ) ) ;
#45824 = CARTESIAN_POINT ( 'NONE',  ( 12.33518044953559922, -3.231951024059400268, 7.099502491684900107 ) ) ;
#45825 = DIRECTION ( 'NONE',  ( 0.000000000000000000, -0.9421243786071872295, 0.3352635608502975151 ) ) ;
#45826 = CARTESIAN_POINT ( 'NONE',  ( 10.98286939055999945, 3.998514186275999638, 9.091062412789998604 ) ) ;
#45827 = CARTESIAN_POINT ( 'NONE',  ( 11.04333729122639873, 2.996877626170000308, 7.526388557597149642 ) ) ;
#45828 = FACE_OUTER_BOUND ( 'NONE', #38369, .T. ) ;
#45829 = CARTESIAN_POINT ( 'NONE',  ( 11.14450444037999866, -5.035425715994000129, -8.381528062715000615 ) ) ;
#45830 = CARTESIAN_POINT ( 'NONE',  ( 17.57569743819256658, 0.6249994633519876386, -13.88107975068472300 ) ) ;
#45831 = CARTESIAN_POINT ( 'NONE',  ( 8.751496707488000126, -3.918323994020610268, -8.356402621895700378 ) ) ;
#45832 = CARTESIAN_POINT ( 'NONE',  ( 12.25748074642598695, -2.187380181826345193, 12.51928400914606954 ) ) ;
#45833 = CARTESIAN_POINT ( 'NONE',  ( 7.925081587919548198, 2.341303385547595983, 8.036180917343964225 ) ) ;
#45834 = ORIENTED_EDGE ( 'NONE', *, *, #28946, .F. ) ;
#45835 = CARTESIAN_POINT ( 'NONE',  ( 18.10946311474936721, -2.988545908040631804, 13.67730534870324277 ) ) ;
#45836 = CARTESIAN_POINT ( 'NONE',  ( 11.09999999999999964, 2.685305999535000154, 6.664030027596000494 ) ) ;
#45837 = EDGE_LOOP ( 'NONE', ( #12204, #65037, #11610, #23818, #50049 ) ) ;
#45838 = VERTEX_POINT ( 'NONE', #61806 ) ;
#45839 = DIRECTION ( 'NONE',  ( 1.000000000000000000, 0.000000000000000000, 0.000000000000000000 ) ) ;
#45840 = CARTESIAN_POINT ( 'NONE',  ( 24.60115016800667220, -3.453285475674932048, -12.10347685339371893 ) ) ;
#45841 = CIRCLE ( 'NONE', #33568, 1.949999999999999956 ) ;
#45842 = DIRECTION ( 'NONE',  ( 0.000000000000000000, -0.2098318009950989882, 0.9777374981512947372 ) ) ;
#45843 = ADVANCED_FACE ( 'NONE', ( #51319 ), #65639, .F. ) ;
#45844 = CARTESIAN_POINT ( 'NONE',  ( 9.815201913989998417, 2.813632032385000148, 8.848857341496000117 ) ) ;
#45846 = ADVANCED_FACE ( 'NONE', ( #7988 ), #17806, .F. ) ;
#45845 = B_SPLINE_CURVE_WITH_KNOTS ( 'NONE', 3,
 ( #11311, #16213, #484, #42107 ),
 .UNSPECIFIED., .F., .F.,
 ( 4, 4 ),
 ( 0.000000000000000000, 1.000000000000000000 ),
 .UNSPECIFIED. ) ;
#45847 = CARTESIAN_POINT ( 'NONE',  ( 7.102406491832000235, -0.2966009291953999871, -3.049954386258999950 ) ) ;
#45848 = CARTESIAN_POINT ( 'NONE',  ( 9.454862456499625978, -3.587552194319129750, -6.728365969834097626 ) ) ;
#45849 = CARTESIAN_POINT ( 'NONE',  ( 10.59303089732000025, -2.436232726560000117, 7.793465286118999913 ) ) ;
#45850 = CARTESIAN_POINT ( 'NONE',  ( 18.14493211602550105, -0.4188397444781337686, -12.59305179380755213 ) ) ;
#45851 = CARTESIAN_POINT ( 'NONE',  ( 10.91623602276999883, -5.459825388708999583, -8.642870457474998602 ) ) ;
#45852 = CARTESIAN_POINT ( 'NONE',  ( 11.77359063708300013, -3.044227915785300276, -7.768721787835699999 ) ) ;
#45853 = CARTESIAN_POINT ( 'NONE',  ( 7.257235050943683596, -0.9062970480449128452, 0.7219501443736217050 ) ) ;
#45854 = ORIENTED_EDGE ( 'NONE', *, *, #4016, .T. ) ;
#45855 = APPLICATION_CONTEXT ( 'automotive_design' ) ;
#45856 = AXIS2_PLACEMENT_3D ( 'NONE', #32976, #17237, #12341 ) ;
#45857 = CARTESIAN_POINT ( 'NONE',  ( 10.97044361512000066, -6.159047241444000065, -5.038256385253999881 ) ) ;
#45858 =( NAMED_UNIT ( * ) SI_UNIT ( $, .STERADIAN. ) SOLID_ANGLE_UNIT ( ) );
#45859 = LINE ( 'NONE', #2178, #25824 ) ;
#45860 = DIRECTION ( 'NONE',  ( -1.000000000000000000, 0.000000000000000000, 0.000000000000000000 ) ) ;
#45861 = CARTESIAN_POINT ( 'NONE',  ( 9.735025935145998233, 3.814256956409300070, -6.234344474498000110 ) ) ;
#45862 = CARTESIAN_POINT ( 'NONE',  ( 12.15267534726961607, 2.198616041048513381, 13.82629894333309295 ) ) ;
#45863 = CARTESIAN_POINT ( 'NONE',  ( 9.910640133503999749, -2.107273866476999657, 7.885282692430999774 ) ) ;
#45864 = ORIENTED_EDGE ( 'NONE', *, *, #59514, .F. ) ;
#45865 = CARTESIAN_POINT ( 'NONE',  ( 12.20062903853931147, 0.1603600964535310536, -12.69865684038602360 ) ) ;
#45866 = CARTESIAN_POINT ( 'NONE',  ( 12.12629894760563509, -0.2577288767859198249, 13.99764474128114600 ) ) ;
#45867 = ORIENTED_EDGE ( 'NONE', *, *, #12169, .F. ) ;
#45868 = CARTESIAN_POINT ( 'NONE',  ( 11.33810207955129812, -3.203462856645999945, -7.825000000000000178 ) ) ;
#45869 = EDGE_CURVE ( 'NONE', #93, #44093, #23933, .T. ) ;
#45870 = CARTESIAN_POINT ( 'NONE',  ( 24.60109517054022987, -3.453341049831690324, 12.10341519414737199 ) ) ;
#45871 = CARTESIAN_POINT ( 'NONE',  ( 15.82725884711995512, 9.380130419263576158, 8.300201155565265054 ) ) ;
#45872 = PLANE ( 'NONE',  #23887 ) ;
#45873 = ADVANCED_FACE ( 'NONE', ( #63515 ), #32068, .F. ) ;
#45874 = CARTESIAN_POINT ( 'NONE',  ( 8.656893636725156327, 5.180000428241942068, -8.180009313714272423 ) ) ;
#45875 = CARTESIAN_POINT ( 'NONE',  ( 0.5568389912892000027, 2.537743131474000435, -2.464631551651000230 ) ) ;
#45876 = CARTESIAN_POINT ( 'NONE',  ( 11.09999999999999964, 2.700683852703999577, 5.124965750789000296 ) ) ;
#45877 = CARTESIAN_POINT ( 'NONE',  ( 12.61585440497580990, 3.174879747171424960, 12.19344691178322471 ) ) ;
#45878 = CARTESIAN_POINT ( 'NONE',  ( 18.30000000000000071, 2.775703640144308260, 11.68316444257406772 ) ) ;
#45879 = CARTESIAN_POINT ( 'NONE',  ( 10.80133863405319872, 4.534404523786000674, -8.181696703306599261 ) ) ;
#45880 = DIRECTION ( 'NONE',  ( 0.000000000000000000, 1.000000000000000000, 0.000000000000000000 ) ) ;
#45881 = CARTESIAN_POINT ( 'NONE',  ( 11.48522412107029922, 4.047131449166419870, -6.609122077774299164 ) ) ;
#45882 = CARTESIAN_POINT ( 'NONE',  ( 9.809950584426999853, 4.453199839589800035, -6.451980747609000311 ) ) ;
#45884 = CARTESIAN_POINT ( 'NONE',  ( 12.63917144495449207, 1.891830949853918975, 12.57269938248749064 ) ) ;
#45883 = CARTESIAN_POINT ( 'NONE',  ( 15.67439970770000102, -8.782357275181000844, -8.013525452821999906 ) ) ;
#45885 = CARTESIAN_POINT ( 'NONE',  ( 23.60093109724832772, -13.39265514436702098, 3.991923406020022824 ) ) ;
#45886 = ORIENTED_EDGE ( 'NONE', *, *, #38919, .T. ) ;
#45887 = EDGE_CURVE ( 'NONE', #3039, #37419, #26123, .T. ) ;
#45888 = CARTESIAN_POINT ( 'NONE',  ( 11.06967835872019812, 3.245266201729799960, 7.975673736933100777 ) ) ;
#45889 = CARTESIAN_POINT ( 'NONE',  ( 10.99433452212999818, -3.697619272994999928, 5.729306330972000261 ) ) ;
#45890 = CARTESIAN_POINT ( 'NONE',  ( 10.36422949779699820, 4.557226039164599563, 6.664331202173499946 ) ) ;
#45891 = CARTESIAN_POINT ( 'NONE',  ( 25.60000000000000142, -2.258942858049999725, 12.29419282279000036 ) ) ;
#45892 = CIRCLE ( 'NONE', #53678, 1.000000000000000444 ) ;
#45893 = CARTESIAN_POINT ( 'NONE',  ( 5.700000000000000178, 0.5292307692307999245, -2.083846153846000249 ) ) ;
#45894 = CARTESIAN_POINT ( 'NONE',  ( 6.999999691988000095, -12.49999909016000110, 4.774434232535999529E-10 ) ) ;
#45895 = DIRECTION ( 'NONE',  ( 0.000000000000000000, 0.8514547570628037132, -0.5244280662542021298 ) ) ;
#45896 = B_SPLINE_CURVE_WITH_KNOTS ( 'NONE', 3,
 ( #63131, #67691, #57907, #48708, #52656, #31002, #36581, #31686, #27381, #68726, #52316, #30650, #14575, #19814, #35891, #63482, #4060, #57206 ),
 .UNSPECIFIED., .F., .F.,
 ( 4, 2, 2, 2, 2, 2, 2, 2, 4 ),
 ( 0.000000000000000000, 0.1250000000000000278, 0.2500000000000000000, 0.3749999999999999445, 0.4999999999999999445, 0.6249999999999998890, 0.7499999999999998890, 0.8750000000000000000, 1.000000000000000000 ),
 .UNSPECIFIED. ) ;
#45897 = ORIENTED_EDGE ( 'NONE', *, *, #65734, .F. ) ;
#45898 = CARTESIAN_POINT ( 'NONE',  ( 8.948759580228999866, -5.110528875107000601, -7.234556850645999404 ) ) ;
#45899 = CARTESIAN_POINT ( 'NONE',  ( 11.00000000000000000, 2.941427501403999667, -7.825000000000000178 ) ) ;
#45900 = CARTESIAN_POINT ( 'NONE',  ( 11.64767835872009982, -4.874341053673500568, 8.051056647135798272 ) ) ;
#45901 = CARTESIAN_POINT ( 'NONE',  ( 18.22257245894167710, 2.198943951577544631, -12.40664208059732587 ) ) ;
#45902 = CARTESIAN_POINT ( 'NONE',  ( 8.363820752062002484, -3.209969472227002463, -6.508691878251005924 ) ) ;
#45903 = CARTESIAN_POINT ( 'NONE',  ( 17.55505043854143565, 3.125000000000000000, 12.28373071562070074 ) ) ;
#45904 = CARTESIAN_POINT ( 'NONE',  ( 12.22115613568263903, 2.722964197629289984, -13.62363865701805210 ) ) ;
#45905 = CARTESIAN_POINT ( 'NONE',  ( 9.128137413980999426, -5.235394649229000663, -8.110359502241001550 ) ) ;
#45906 = DIRECTION ( 'NONE',  ( 1.000000000000000000, 0.000000000000000000, 0.000000000000000000 ) ) ;
#45907 = VERTEX_POINT ( 'NONE', #63162 ) ;
#45908 = CARTESIAN_POINT ( 'NONE',  ( -0.000000000000000000, -2.824612379753681513, -0.7585797238568994239 ) ) ;
#45909 = CARTESIAN_POINT ( 'NONE',  ( 12.22983020848963065, 0.4451122480341365151, -13.99293440828418511 ) ) ;
#45910 = CARTESIAN_POINT ( 'NONE',  ( 13.67488484168399943, -8.948943314763999624, -7.542122959438999352 ) ) ;
#45911 = CARTESIAN_POINT ( 'NONE',  ( 18.15909587492906496, -2.338249772828220774, -13.70640098171541155 ) ) ;
#45912 = CARTESIAN_POINT ( 'NONE',  ( 18.17974523563204414, 2.479825770664845663, 12.45623811633683431 ) ) ;
#45913 = CARTESIAN_POINT ( 'NONE',  ( 9.260829719593999698, 4.861259245430999520, -8.806664389576001284 ) ) ;
#45914 = CARTESIAN_POINT ( 'NONE',  ( 6.871489329557980419, 1.027917644197982705, 1.125047304260232917 ) ) ;
#45915 = EDGE_LOOP ( 'NONE', ( #37559, #44898, #17266, #37517 ) ) ;
#45916 = CARTESIAN_POINT ( 'NONE',  ( 27.09999999999999787, 0.000000000000000000, 9.250000000000000000 ) ) ;
#45917 = CARTESIAN_POINT ( 'NONE',  ( 18.26447107791328861, 2.367226376531800458, -13.79841952404521166 ) ) ;
#45918 = EDGE_LOOP ( 'NONE', ( #47796, #66981, #19671, #3614, #1301, #12392 ) ) ;
#45919 = CARTESIAN_POINT ( 'NONE',  ( 5.700000000000000178, 12.50865771883999855, 2.924687089724999911 ) ) ;
#45920 = CARTESIAN_POINT ( 'NONE',  ( 20.60000000000000142, 0.000000000000000000, 0.000000000000000000 ) ) ;
#45921 = CARTESIAN_POINT ( 'NONE',  ( 8.953620280414000376, 2.881930053949999682, -8.823338183322999129 ) ) ;
#45922 = EDGE_CURVE ( 'NONE', #60348, #23570, #57857, .T. ) ;
#45923 = CARTESIAN_POINT ( 'NONE',  ( 10.13819615328233503, 2.541217446078312570, -6.488444088169603496 ) ) ;
#45924 = EDGE_CURVE ( 'NONE', #50708, #21198, #5485, .T. ) ;
#45925 = CARTESIAN_POINT ( 'NONE',  ( 11.18923293495519822, -5.032672437899000428, -7.458486839450950256 ) ) ;
#45926 = LINE ( 'NONE', #63012, #16972 ) ;
#45927 = EDGE_CURVE ( 'NONE', #46284, #41305, #56503, .T. ) ;
#45928 = CARTESIAN_POINT ( 'NONE',  ( 4.919609839683332986, 0.1963495408493571848, 1.500000000000000666 ) ) ;
#45929 = EDGE_LOOP ( 'NONE', ( #10263, #34527, #32010, #24394 ) ) ;
#45930 = CARTESIAN_POINT ( 'NONE',  ( 10.02145237372899800, 4.043732047787757189, -8.774080944853649200 ) ) ;
#45931 = CYLINDRICAL_SURFACE ( 'NONE', #12763, 1.250000000000000222 ) ;
#45932 = CARTESIAN_POINT ( 'NONE',  ( 8.979720280412999855, 5.524776413195999325, -7.147585171405999915 ) ) ;
#45933 = VERTEX_POINT ( 'NONE', #10036 ) ;
#45934 = CARTESIAN_POINT ( 'NONE',  ( 10.15787172175999942, 4.213497149090000171, -5.822953133183999874 ) ) ;
#45935 =( NAMED_UNIT ( * ) SI_UNIT ( $, .STERADIAN. ) SOLID_ANGLE_UNIT ( ) );
#45936 = EDGE_LOOP ( 'NONE', ( #63445, #57461, #3423, #6128 ) ) ;
#45937 = CARTESIAN_POINT ( 'NONE',  ( 9.733963142879998642, 5.117257953482000410, 7.735518817439499983 ) ) ;
#45938 = CARTESIAN_POINT ( 'NONE',  ( 17.86124198984734690, -1.955044089803213536, -12.56196094884553638 ) ) ;
#45939 = CARTESIAN_POINT ( 'NONE',  ( 11.44794916906000104, -11.60968724315999978, -1.479704744065999833 ) ) ;
#45940 = AXIS2_PLACEMENT_3D ( 'NONE', #27812, #1232, #45945 ) ;
#45941 = FACE_OUTER_BOUND ( 'NONE', #21567, .T. ) ;
#45942 = DIRECTION ( 'NONE',  ( 1.000000000000000000, 0.000000000000000000, 0.000000000000000000 ) ) ;
#45943 = B_SPLINE_CURVE_WITH_KNOTS ( 'NONE', 3,
 ( #26763, #42150, #15574, #59936 ),
 .UNSPECIFIED., .F., .F.,
 ( 4, 4 ),
 ( 0.000000000000000000, 1.000000000000000000 ),
 .UNSPECIFIED. ) ;
#45944 = ORIENTED_EDGE ( 'NONE', *, *, #19083, .T. ) ;
#45945 = DIRECTION ( 'NONE',  ( 0.000000000000000000, 0.000000000000000000, 1.000000000000000000 ) ) ;
#45946 = CARTESIAN_POINT ( 'NONE',  ( 10.50084834123000022, 4.616783736607999344, -6.288082254674000282 ) ) ;
#45947 = DIRECTION ( 'NONE',  ( 1.000000000000000000, 0.000000000000000000, 0.000000000000000000 ) ) ;
#45948 = CARTESIAN_POINT ( 'NONE',  ( 12.32403884885180645, 1.971565993173698850, -13.86048321094706637 ) ) ;
#45949 = CARTESIAN_POINT ( 'NONE',  ( 9.101797255588000013, -2.721932483203000075, -7.445890648716809501 ) ) ;
#45950 = CARTESIAN_POINT ( 'NONE',  ( 18.03319344185665329, 0.5490318484135021659, 13.98923259457976087 ) ) ;
#45951 = FACE_OUTER_BOUND ( 'NONE', #26869, .T. ) ;
#45952 = AXIS2_PLACEMENT_3D ( 'NONE', #50070, #1826, #45176 ) ;
#45953 = CARTESIAN_POINT ( 'NONE',  ( 7.836901522150861332, 4.790146211336424820, 6.377682021994305117 ) ) ;
#45954 = B_SPLINE_CURVE_WITH_KNOTS ( 'NONE', 3,
 ( #31466, #43333, #26568, #21990, #21646, #38072, #42981, #37735, #11163, #27252, #64637, #59399, #44380, #34576, #39464, #22338, #12898, #33880, #1365, #50300, #50642, #34227, #66018 ),
 .UNSPECIFIED., .F., .F.,
 ( 4, 2, 2, 1, 2, 2, 2, 2, 1, 1, 2, 2, 4 ),
 ( 0.000000000000000000, 0.2500000000000023315, 0.3750000000000046629, 0.4375000000000032196, 0.4687500000000038858, 0.5000000000000044409, 0.6250000000000305311, 0.6875000000000408562, 0.7187500000000447420, 0.7343750000000456302, 0.7421875000000482947, 0.7500000000000510703, 1.000000000000000000 ),
 .UNSPECIFIED. ) ;
#45955 = ORIENTED_EDGE ( 'NONE', *, *, #17203, .T. ) ;
#45956 = ORIENTED_EDGE ( 'NONE', *, *, #58167, .T. ) ;
#45957 = CARTESIAN_POINT ( 'NONE',  ( 10.10682028041000002, 4.294368353031000396, -8.968663198664000191 ) ) ;
#45958 = CARTESIAN_POINT ( 'NONE',  ( 21.60000000000000142, 0.000000000000000000, 0.000000000000000000 ) ) ;
#45959 = CARTESIAN_POINT ( 'NONE',  ( 10.40685100253999984, 2.832432432432000269, -6.822293592207000934 ) ) ;
#45960 = CARTESIAN_POINT ( 'NONE',  ( 24.14075185647167032, 3.327828376135185451, 12.49053418803123705 ) ) ;
#45961 = CARTESIAN_POINT ( 'NONE',  ( 23.55757338048400129, 10.23275786013000044, -9.678818376535998524 ) ) ;
#45962 = CARTESIAN_POINT ( 'NONE',  ( 18.12922381500399993, -3.157787539580000136, -11.36563583066999961 ) ) ;
#45964 = CARTESIAN_POINT ( 'NONE',  ( 8.651157662976507012, 5.422415455645571036, 6.482274542572600495 ) ) ;
#45963 = CARTESIAN_POINT ( 'NONE',  ( 9.525809814041000578, -3.217492037304399588, 6.488038963273999649 ) ) ;
#45965 = CARTESIAN_POINT ( 'NONE',  ( 8.987059360767002403, -5.121592602089997115, -6.365116772834005232 ) ) ;
#45966 = VERTEX_POINT ( 'NONE', #58621 ) ;
#45967 = B_SPLINE_CURVE_WITH_KNOTS ( 'NONE', 3,
 ( #16071, #50918, #1378, #64985, #11858, #45679, #59758, #29615, #13528, #22695, #33199, #46015, #61742, #44038, #67322, #66984, #19097, #7927 ),
 .UNSPECIFIED., .F., .F.,
 ( 4, 2, 2, 2, 2, 2, 2, 2, 4 ),
 ( 0.000000000000000000, 0.1250000000000000000, 0.2500000000000000000, 0.3750000000000000000, 0.5000000000000000000, 0.6250000000000000000, 0.7500000000000000000, 0.8750000000000000000, 1.000000000000000000 ),
 .UNSPECIFIED. ) ;
#45968 = CARTESIAN_POINT ( 'NONE',  ( 10.26195629121000152, -3.399999734730999812, 4.591198190832999515 ) ) ;
#45969 = EDGE_CURVE ( 'NONE', #47655, #22693, #53158, .T. ) ;
#45970 = CARTESIAN_POINT ( 'NONE',  ( 23.60205915885299888, -11.88166580726000454, -3.967996863081999948 ) ) ;
#45971 = CARTESIAN_POINT ( 'NONE',  ( 9.309135711596999485, -5.864995026133001055, -7.324074232821000230 ) ) ;
#45972 = DIRECTION ( 'NONE',  ( 0.000000000000000000, 1.000000000000000000, 0.000000000000000000 ) ) ;
#45973 = CARTESIAN_POINT ( 'NONE',  ( 9.870828026683421186, -2.650036842959835770, -7.402527408165655132 ) ) ;
#45974 = CARTESIAN_POINT ( 'NONE',  ( 4.599999999999999645, -3.248147246781390329, -13.61798588129781251 ) ) ;
#45975 = CARTESIAN_POINT ( 'NONE',  ( 11.09999999999999964, 0.000000000000000000, 0.000000000000000000 ) ) ;
#45976 = CARTESIAN_POINT ( 'NONE',  ( 7.634919074141999218, -4.860412626018001170, 6.427891721055999597 ) ) ;
#45977 = AXIS2_PLACEMENT_3D ( 'NONE', #51255, #13521, #3008 ) ;
#45978 =( NAMED_UNIT ( * ) PLANE_ANGLE_UNIT ( ) SI_UNIT ( $, .RADIAN. ) );
#45979 = DIRECTION ( 'NONE',  ( 1.000000000000000000, 0.000000000000000000, 0.000000000000000000 ) ) ;
#45980 = CARTESIAN_POINT ( 'NONE',  ( 3.591840252576999681, 0.3470336765304000148, -3.407861879647000158 ) ) ;
#45981 = EDGE_LOOP ( 'NONE', ( #59389, #17430, #25860, #53562 ) ) ;
#45982 = CARTESIAN_POINT ( 'NONE',  ( 12.54694134722857513, -0.5693054069933395356, -12.68281928773557787 ) ) ;
#45983 = CARTESIAN_POINT ( 'NONE',  ( 12.19038559394824972, -2.613250548335406265, -12.42445786901186722 ) ) ;
#45984 = CARTESIAN_POINT ( 'NONE',  ( 13.63315305048522319, 12.20113081363246543, 2.519319003639657328 ) ) ;
#45985 = CARTESIAN_POINT ( 'NONE',  ( 24.60170725920900026, 3.645111442846999950, -12.27956986324999988 ) ) ;
#45986 = CARTESIAN_POINT ( 'NONE',  ( 9.970944094204998720, -5.100000000000000533, 6.571291218949999902 ) ) ;
#45987 = ORIENTED_EDGE ( 'NONE', *, *, #28497, .T. ) ;
#45988 = CARTESIAN_POINT ( 'NONE',  ( 5.622505169306999839, 1.226089021931999978, -0.4951583500558000006 ) ) ;
#45989 = SHAPE_DEFINITION_REPRESENTATION ( #45567, #26842 ) ;
#45990 = CARTESIAN_POINT ( 'NONE',  ( 0.5525390791026434378, 2.818854795173400429, 2.124449897083314553 ) ) ;
#45991 = CARTESIAN_POINT ( 'NONE',  ( 13.22410434383600197, -11.56587205782000005, -1.788415454164999918 ) ) ;
#45992 = CARTESIAN_POINT ( 'NONE',  ( 1.698890132539874642, -2.798833948393640192, 2.150913519912191152 ) ) ;
#45994 = AXIS2_PLACEMENT_3D ( 'NONE', #7431, #55334, #55686 ) ;
#45993 = CARTESIAN_POINT ( 'NONE',  ( 10.77368717260499942, 3.460071470104900015, -8.381256426168800289 ) ) ;
#45995 = ORIENTED_EDGE ( 'NONE', *, *, #9550, .F. ) ;
#45996 = CARTESIAN_POINT ( 'NONE',  ( 9.924739995124999936, -5.060461104229999840, 8.686133300732999274 ) ) ;
#45997 = VERTEX_POINT ( 'NONE', #4439 ) ;
#45998 = CARTESIAN_POINT ( 'NONE',  ( 8.486008579191000933, -3.399999999999999911, 5.976611076844000614 ) ) ;
#45999 = CARTESIAN_POINT ( 'NONE',  ( 8.047379440378000126, -4.468370631666999770, 8.882152684713000568 ) ) ;
#46000 = AXIS2_PLACEMENT_3D ( 'NONE', #28680, #39160, #38815 ) ;
#46001 = CARTESIAN_POINT ( 'NONE',  ( 18.28005834358923920, 0.01140630886273286473, -14.00000041621361291 ) ) ;
#46002 = EDGE_CURVE ( 'NONE', #60711, #8263, #62318, .T. ) ;
#46003 = ORIENTED_EDGE ( 'NONE', *, *, #14074, .F. ) ;
#46004 = CARTESIAN_POINT ( 'NONE',  ( 10.94429324618039523, 9.240129021172709400, -6.284308437708901351 ) ) ;
#46005 = EDGE_CURVE ( 'NONE', #39090, #24276, #43118, .T. ) ;
#46006 = CARTESIAN_POINT ( 'NONE',  ( 11.03977792510109701, -5.161925716696966759, -8.467638888452240664 ) ) ;
#46007 = CARTESIAN_POINT ( 'NONE',  ( 6.794914158771000245, 2.836301549691000012, -8.273864296493000481 ) ) ;
#46008 = CARTESIAN_POINT ( 'NONE',  ( 10.20217841747468945, 2.710350078041137145, 7.038638062422410080 ) ) ;
#46009 = ADVANCED_FACE ( 'NONE', ( #57583 ), #38426, .F. ) ;
#46010 = DIRECTION ( 'NONE',  ( 0.000000000000000000, -0.9466492601157000530, 0.3222656952305000266 ) ) ;
#46011 = VERTEX_POINT ( 'NONE', #19764 ) ;
#46012 = CARTESIAN_POINT ( 'NONE',  ( 9.719606904206999687, -5.967761543230999166, 7.406644089178000101 ) ) ;
#46013 = ADVANCED_FACE ( 'NONE', ( #52953 ), #68325, .F. ) ;
#46014 = CARTESIAN_POINT ( 'NONE',  ( 12.19290954905150315, -2.626136292398727701, -13.64584403834836479 ) ) ;
#46015 = CARTESIAN_POINT ( 'NONE',  ( 10.47726354018323214, 3.370476274536374106, -8.592232985442821658 ) ) ;
#46016 = CARTESIAN_POINT ( 'NONE',  ( 10.64447714202000128, -5.073836261934999925, -8.340686666652999293 ) ) ;
#46017 = DIRECTION ( 'NONE',  ( -1.000000000000000000, 0.000000000000000000, 0.000000000000000000 ) ) ;
#46018 = ORIENTED_EDGE ( 'NONE', *, *, #46715, .F. ) ;
#46019 = CARTESIAN_POINT ( 'NONE',  ( 17.94287402913520069, 0.4902502636344967524, -13.88836422973777296 ) ) ;
#46020 = CARTESIAN_POINT ( 'NONE',  ( 8.876902336861418163, -3.730411824524082043, -6.500155937682547069 ) ) ;
#46021 = CARTESIAN_POINT ( 'NONE',  ( 3.799999782336999754, 2.725000000000000089, 0.000000000000000000 ) ) ;
#46022 = CARTESIAN_POINT ( 'NONE',  ( 11.49999672495000169, 3.632761979779000061, -11.06912554803999882 ) ) ;
#46023 = B_SPLINE_CURVE_WITH_KNOTS ( 'NONE', 3,
 ( #6768, #43146, #1885, #28107 ),
 .UNSPECIFIED., .F., .F.,
 ( 4, 4 ),
 ( 0.000000000000000000, 1.000000000000000000 ),
 .UNSPECIFIED. ) ;
#46024 = CARTESIAN_POINT ( 'NONE',  ( 12.60368798324988404, -0.5920240553917492932, -13.88302649426327307 ) ) ;
#46025 = CARTESIAN_POINT ( 'NONE',  ( 18.14681149257599913, -2.701359571199342113, 12.40239981104076072 ) ) ;
#46026 = ORIENTED_EDGE ( 'NONE', *, *, #45540, .T. ) ;
#46027 = SHAPE_REPRESENTATION ( 'Insulator', ( #9676 ), #21760 ) ;
#46028 = CARTESIAN_POINT ( 'NONE',  ( 10.73213259636989925, -4.907524392912299582, -7.994504989494399361 ) ) ;
#46029 = ORIENTED_EDGE ( 'NONE', *, *, #61787, .F. ) ;
#46030 = CARTESIAN_POINT ( 'NONE',  ( 11.07345995138000028, 3.998673170817999889, 8.920816085870999501 ) ) ;
#46031 = EDGE_CURVE ( 'NONE', #12604, #63987, #45612, .T. ) ;
#46032 = CARTESIAN_POINT ( 'NONE',  ( 10.89393020684959978, 2.750000000000000000, -7.500000000000000000 ) ) ;
#46033 = CARTESIAN_POINT ( 'NONE',  ( 10.12339528040999959, 3.988943694240999704, -8.966360307350999648 ) ) ;
#46034 = CONICAL_SURFACE ( 'NONE', #10342, 3.249989426617000188, 0.7853950157668545540 ) ;
#46035 = CARTESIAN_POINT ( 'NONE',  ( 3.438845187857999974, 1.765336245502999946, -3.260861573818000458 ) ) ;
#46036 = CARTESIAN_POINT ( 'NONE',  ( 11.19120431613999855, -3.005395205805000192, -6.023553580263000029 ) ) ;
#46037 = CARTESIAN_POINT ( 'NONE',  ( 17.55505043854143565, 1.875000000000000000, -25.00000000000000000 ) ) ;
#46038 = CYLINDRICAL_SURFACE ( 'NONE', #7116, 1.250000000000000222 ) ;
#46039 = ADVANCED_BREP_SHAPE_REPRESENTATION ( '', ( #30727, #9676 ), #38794 ) ;
#46040 = ORIENTED_EDGE ( 'NONE', *, *, #9291, .F. ) ;
#46041 = CARTESIAN_POINT ( 'NONE',  ( 10.87457053952200070, -4.448306506338299826, 8.548957288282998945 ) ) ;
#46042 = CARTESIAN_POINT ( 'NONE',  ( 9.758140238852000437, 2.901378080241999946, 6.555076849497999625 ) ) ;
#46043 = CARTESIAN_POINT ( 'NONE',  ( 15.76350100824699929, 9.023747925888001120, 8.341981946770999912 ) ) ;
#46044 = CARTESIAN_POINT ( 'NONE',  ( 8.271691940379001906, -5.629389383493999865, 8.631822608164000599 ) ) ;
#46046 = CARTESIAN_POINT ( 'NONE',  ( 12.75534451565254201, 1.787855198891418418, -13.88537265576022861 ) ) ;
#46045 = CARTESIAN_POINT ( 'NONE',  ( 9.104014120666999332, 5.045862207587999748, 8.527865280865999154 ) ) ;
#46047 = AXIS2_PLACEMENT_3D ( 'NONE', #65955, #54440, #22968 ) ;
#46048 = CARTESIAN_POINT ( 'NONE',  ( 11.60533460557258323, 4.184174550317700358, -8.625775273268001087 ) ) ;
#46049 = CARTESIAN_POINT ( 'NONE',  ( 20.75138802851920161, -5.760487483753345295, 0.05108123232907683942 ) ) ;
#46050 = EDGE_CURVE ( 'NONE', #32140, #48149, #38858, .T. ) ;
#46051 = VECTOR ( 'NONE', #25399, 1000.000000000000114 ) ;
#46052 = CARTESIAN_POINT ( 'NONE',  ( 10.16159632033899918, 3.070047649444500149, -7.120485934352199564 ) ) ;
#46053 = CARTESIAN_POINT ( 'NONE',  ( 17.81083341652436758, 0.6731412448965020667, 12.58200685883813108 ) ) ;
#46054 = CARTESIAN_POINT ( 'NONE',  ( 4.599999999999999645, -3.199698446519374073, -12.18695736643652694 ) ) ;
#46055 = CARTESIAN_POINT ( 'NONE',  ( 10.80502344389999791, 2.874741265256000489, 8.182900850620900002 ) ) ;
#46056 = EDGE_CURVE ( 'NONE', #67791, #44355, #31633, .T. ) ;
#46057 = DIRECTION ( 'NONE',  ( -1.000000000000000000, 0.000000000000000000, 0.000000000000000000 ) ) ;
#46058 = EDGE_LOOP ( 'NONE', ( #42412, #10736, #4574 ) ) ;
#46059 = CARTESIAN_POINT ( 'NONE',  ( 7.962144353208000069, -4.874569256861000177, 6.119503992241999590 ) ) ;
#46060 = CARTESIAN_POINT ( 'NONE',  ( 18.13115538416114703, 2.961380457613811412, 13.68321312766445175 ) ) ;
#46061 = CARTESIAN_POINT ( 'NONE',  ( 7.844724262280000637, -4.719412258162999585, 6.357657668295000342 ) ) ;
#46062 = CARTESIAN_POINT ( 'NONE',  ( 10.21924205624999971, 3.689072563647699976, 6.690659495528099576 ) ) ;
#46063 = ORIENTED_EDGE ( 'NONE', *, *, #1261, .F. ) ;
#46064 = CARTESIAN_POINT ( 'NONE',  ( 9.160308886257000793, 4.122021000979000149, 9.013569734175000292 ) ) ;
#46066 = CARTESIAN_POINT ( 'NONE',  ( 11.06456920625009843, 4.037149028919880145, 8.532838639935999225 ) ) ;
#46065 = CARTESIAN_POINT ( 'NONE',  ( 10.25944474310099785, -3.106516218291800246, -7.933599538786499039 ) ) ;
#46067 = CARTESIAN_POINT ( 'NONE',  ( 10.31966721959000033, 4.764593388688000530, -5.997651217580999727 ) ) ;
#46068 = ORIENTED_EDGE ( 'NONE', *, *, #3876, .T. ) ;
#46069 = CARTESIAN_POINT ( 'NONE',  ( 10.90000658885999840, -1.382741116750999977, 11.26545724788999969 ) ) ;
#46070 = DIRECTION ( 'NONE',  ( -1.000000000000000000, 0.000000000000000000, 0.000000000000000000 ) ) ;
#46071 = CARTESIAN_POINT ( 'NONE',  ( 11.48225819896749833, 2.879005208331999910, 7.288668995979000087 ) ) ;
#46072 = CARTESIAN_POINT ( 'NONE',  ( 7.945205862068529967, -5.100061878551159111, 6.648263158528791017 ) ) ;
#46073 = CARTESIAN_POINT ( 'NONE',  ( 11.09999999999999964, -5.299839462858000338, -5.135710755876000455 ) ) ;
#46074 = VERTEX_POINT ( 'NONE', #5050 ) ;
#46075 = CARTESIAN_POINT ( 'NONE',  ( 11.83936489023500194, -3.414328975993000004, 11.89720897182000137 ) ) ;
#46076 = CARTESIAN_POINT ( 'NONE',  ( 7.169089158768000125, 3.469376689055999829, -5.675721888027999817 ) ) ;
#46077 = CARTESIAN_POINT ( 'NONE',  ( 8.191826018243656193, -5.741591131932793246, 7.347086656645051228 ) ) ;
#46078 = CARTESIAN_POINT ( 'NONE',  ( 11.22056920625029974, -3.952687217764870198, -6.184582852561999466 ) ) ;
#46079 = CARTESIAN_POINT ( 'NONE',  ( 9.902671671056999969, -5.261543809652999393, 7.288123611975898974 ) ) ;
#46080 = ORIENTED_EDGE ( 'NONE', *, *, #53147, .F. ) ;
#46082 = CARTESIAN_POINT ( 'NONE',  ( 10.61565784046000083, -5.208090112546999606, -4.717379660883000092 ) ) ;
#46081 = AXIS2_PLACEMENT_3D ( 'NONE', #27147, #31703, #26455 ) ;
#46083 = CARTESIAN_POINT ( 'NONE',  ( 11.26426088462129904, -3.997280690308189666, 8.778009775371000245 ) ) ;
#46084 = ORIENTED_EDGE ( 'NONE', *, *, #17637, .T. ) ;
#46085 = CARTESIAN_POINT ( 'NONE',  ( 9.966846873515667227, -4.768183399968645375, 6.500416447002276499 ) ) ;
#46086 = VERTEX_POINT ( 'NONE', #63429 ) ;
#46087 = CARTESIAN_POINT ( 'NONE',  ( 9.663732219486000474, -2.297586052318000061, -7.360088033824999876 ) ) ;
#46088 = CARTESIAN_POINT ( 'NONE',  ( 10.33476917742999923, -3.241264537866999973, -4.626716660091000577 ) ) ;
#46089 = CARTESIAN_POINT ( 'NONE',  ( 8.216851002544000693, -2.832432432432000269, 6.822293592207000934 ) ) ;
#46090 = CARTESIAN_POINT ( 'NONE',  ( 11.51279632507520034, -3.375091146194399983, 6.341531314375999706 ) ) ;
#46091 = CARTESIAN_POINT ( 'NONE',  ( 12.35410221487141591, 2.932869452542227418, -12.34012701440640747 ) ) ;
#46092 = EDGE_CURVE ( 'NONE', #15201, #67663, #4721, .T. ) ;
#46093 = CARTESIAN_POINT ( 'NONE',  ( 11.24379975933729980, -2.921317947059999920, 7.871126858273000515 ) ) ;
#46094 = CARTESIAN_POINT ( 'NONE',  ( 7.475045280409000625, 3.276311362504999991, 5.841989464160999290 ) ) ;
#46095 = EDGE_CURVE ( 'NONE', #37303, #40878, #14525, .T. ) ;
#46096 = ORIENTED_EDGE ( 'NONE', *, *, #21601, .F. ) ;
#46097 = CARTESIAN_POINT ( 'NONE',  ( 25.44993910976900153, -11.77655473258999841, 4.190794510628000680 ) ) ;
#46098 = AXIS2_PLACEMENT_3D ( 'NONE', #41869, #3764, #20889 ) ;
#46099 = CARTESIAN_POINT ( 'NONE',  ( 7.609456853206999938, -3.276313010012999793, 5.841993238691999935 ) ) ;
#46100 = CARTESIAN_POINT ( 'NONE',  ( 9.989763540182750035, 4.327184855449099921, 6.282534154164604701 ) ) ;
#46101 = VERTEX_POINT ( 'NONE', #69026 ) ;
#46102 = CARTESIAN_POINT ( 'NONE',  ( 12.72061467711778171, -1.765703846569735669, -12.47566797393135474 ) ) ;
#46103 = CARTESIAN_POINT ( 'NONE',  ( 11.13349010443639919, 5.274453806861999716, 7.404690636538299842 ) ) ;
#46104 = CARTESIAN_POINT ( 'NONE',  ( 10.01676935320999995, -4.324998011277000565, -9.154075058362000306 ) ) ;
#46105 = DIRECTION ( 'NONE',  ( 0.000000000000000000, -0.9867381147929490393, -0.1623203401144079905 ) ) ;
#46106 = CARTESIAN_POINT ( 'NONE',  ( 18.44331666222400301, -2.998518551215999750, -12.10579027554000042 ) ) ;
#46107 = CARTESIAN_POINT ( 'NONE',  ( 24.44917776433500123, -8.894882193901999301, 9.199943407630001957 ) ) ;
#46108 = CARTESIAN_POINT ( 'NONE',  ( 12.32516769934784584, -3.065409648700736511, -13.66028300215598534 ) ) ;
#46109 = CARTESIAN_POINT ( 'NONE',  ( 11.41672066707849886, -3.258843737379200078, -7.051685395375099752 ) ) ;
#46110 = CARTESIAN_POINT ( 'NONE',  ( 11.01041369783139956, -4.064477673403060543, -8.776385133971000840 ) ) ;
#46111 = DIRECTION ( 'NONE',  ( 0.9999999999999473754, -3.241492823037153003E-07, -2.435227350522113568E-09 ) ) ;
#46112 = EDGE_LOOP ( 'NONE', ( #5725, #18009, #22986, #15484, #28108, #44455 ) ) ;
#46113 = ORIENTED_EDGE ( 'NONE', *, *, #65217, .F. ) ;
#46114 = CARTESIAN_POINT ( 'NONE',  ( 10.26651762500999965, -4.562321397865999550, 4.689499100602000148 ) ) ;
#46115 = EDGE_CURVE ( 'NONE', #61556, #60646, #3666, .T. ) ;
#46116 =( LENGTH_UNIT ( ) NAMED_UNIT ( * ) SI_UNIT ( .MILLI., .METRE. ) );
#46117 = CARTESIAN_POINT ( 'NONE',  ( 23.59999196693599899, 2.915561532799999966, -13.58550759281999909 ) ) ;
#46118 = CARTESIAN_POINT ( 'NONE',  ( 17.55505043854144276, -0.6250000000000001110, -13.88107975066922428 ) ) ;
#46119 = CARTESIAN_POINT ( 'NONE',  ( 10.57793656291999973, 4.393379542724999531, -6.024362243994999311 ) ) ;
#46120 = CARTESIAN_POINT ( 'NONE',  ( 10.60478570706233370, -2.868293641868291388, 6.886599490775120458 ) ) ;
#46121 = CARTESIAN_POINT ( 'NONE',  ( 17.81536569913635759, 3.068232145164245583, 12.30083422255798631 ) ) ;
#46122 = CARTESIAN_POINT ( 'NONE',  ( 25.50766902656323509, 2.874072089164859456, -11.25422662531584628 ) ) ;
#46123 = CARTESIAN_POINT ( 'NONE',  ( 10.37373942323999998, 2.215265813302000009, 7.703982730183001060 ) ) ;
#46124 = CARTESIAN_POINT ( 'NONE',  ( 8.064958992852089281, 5.350069970865218849, -7.500002487662858819 ) ) ;
#46125 = VERTEX_POINT ( 'NONE', #37216 ) ;
#46126 = CARTESIAN_POINT ( 'NONE',  ( 12.58267958641587114, -1.915804698272715934, 12.56868422206429869 ) ) ;
#46127 = CARTESIAN_POINT ( 'NONE',  ( 8.791809814040998816, -3.469640109842400122, -8.185876144228299012 ) ) ;
#46128 = CARTESIAN_POINT ( 'NONE',  ( 10.09181485429000169, 2.440912084162000006, 7.817367409531000177 ) ) ;
#46129 = CARTESIAN_POINT ( 'NONE',  ( 11.30502344389999969, -5.125258734743999511, 8.182900850620900002 ) ) ;
#46130 = CARTESIAN_POINT ( 'NONE',  ( 9.766460841231999979, 3.135494838036999798, -8.598037907310999373 ) ) ;
#46131 = CIRCLE ( 'NONE', #56160, 2.000000000000000888 ) ;
#46132 = B_SPLINE_CURVE_WITH_KNOTS ( 'NONE', 3,
 ( #55463, #17720, #29252, #34834 ),
 .UNSPECIFIED., .F., .F.,
 ( 4, 4 ),
 ( 0.000000000000000000, 1.000000000000000000 ),
 .UNSPECIFIED. ) ;
#46133 = PRODUCT ( 'Airflow Sleeve', 'Airflow Sleeve', '', ( #51238 ) ) ;
#46134 = CARTESIAN_POINT ( 'NONE',  ( 10.83810672858429847, 2.978701842912999886, -6.731711997412900494 ) ) ;
#46135 = CARTESIAN_POINT ( 'NONE',  ( 12.60420289721210985, 0.5919389804100245733, 12.68142457171642157 ) ) ;
#46136 = CARTESIAN_POINT ( 'NONE',  ( 8.417489158772999858, 2.029098103856999735, 7.726995416028000108 ) ) ;
#46137 = CARTESIAN_POINT ( 'NONE',  ( 10.84168637167000071, 2.681011538858999899, 6.554754637093000547 ) ) ;
#46138 = CARTESIAN_POINT ( 'NONE',  ( 5.699999999579000054, -0.3000000004212000082, -9.662944680462999258 ) ) ;
#46139 = ADVANCED_FACE ( 'NONE', ( #15551 ), #8928, .T. ) ;
#46140 = VERTEX_POINT ( 'NONE', #25006 ) ;
#46141 = CARTESIAN_POINT ( 'NONE',  ( 9.865910841232000905, 2.685250982074999904, -7.026194612421999608 ) ) ;
#46142 = CARTESIAN_POINT ( 'NONE',  ( 7.000000000000000000, 0.2708497377871000311, 3.000000000000000000 ) ) ;
#46143 = CARTESIAN_POINT ( 'NONE',  ( 10.82125723222524449, -4.080988682073267704, 9.237810993546167637 ) ) ;
#46145 = CARTESIAN_POINT ( 'NONE',  ( 3.354734521762166466, -0.9333907618945200824, -3.403975714020706977 ) ) ;
#46144 = CARTESIAN_POINT ( 'NONE',  ( 7.737831853206999178, -5.687202994508999687, 6.847270485579000088 ) ) ;
#46146 = CARTESIAN_POINT ( 'NONE',  ( 12.10000000000000142, -4.149724965537171073, 8.514310854298580367 ) ) ;
#46147 = CARTESIAN_POINT ( 'NONE',  ( 10.47718582084299932, -4.656536239972400182, -6.741111985563299491 ) ) ;
#46148 = ORIENTED_EDGE ( 'NONE', *, *, #19282, .T. ) ;
#46149 = AXIS2_PLACEMENT_3D ( 'NONE', #38791, #38088, #5927 ) ;
#46150 = CARTESIAN_POINT ( 'NONE',  ( 1.963474413114999928, 2.711246897165000114, -2.603366577799000048 ) ) ;
#46151 = DIRECTION ( 'NONE',  ( 1.000000000000000000, 0.000000000000000000, 0.000000000000000000 ) ) ;
#46152 = VECTOR ( 'NONE', #15068, 1000.000000000000114 ) ;
#46154 = CARTESIAN_POINT ( 'NONE',  ( 13.55563772304700088, -9.581334502426001265, -7.839063693813000278 ) ) ;
#46153 = CARTESIAN_POINT ( 'NONE',  ( 9.662145996929073277, 5.577690980164239143, 6.690401850488619573 ) ) ;
#46155 = CARTESIAN_POINT ( 'NONE',  ( 18.17508454104073934, -2.579277621784283436, 13.65633006993621557 ) ) ;
#46156 = CARTESIAN_POINT ( 'NONE',  ( 11.59999999999999964, 4.000000000000000000, -7.500000000000000000 ) ) ;
#46157 = CARTESIAN_POINT ( 'NONE',  ( 12.78089499409917451, -3.248109241121374335, 13.61799491149520946 ) ) ;
#46158 = CARTESIAN_POINT ( 'NONE',  ( 24.30000565784163058, -3.240508265789169506, -12.09374149026787570 ) ) ;
#46159 = CARTESIAN_POINT ( 'NONE',  ( 24.90043558836852000, -11.58828833617089948, 3.208336305466431781 ) ) ;
#46160 = CARTESIAN_POINT ( 'NONE',  ( 7.603418146792000343, -5.687202994508999687, 6.847270485579000088 ) ) ;
#46161 = ORIENTED_EDGE ( 'NONE', *, *, #46481, .F. ) ;
#46162 = CARTESIAN_POINT ( 'NONE',  ( 9.047982780412000992, 2.806082850903000026, 8.615880516515998622 ) ) ;
#46164 = CARTESIAN_POINT ( 'NONE',  ( 11.79999999471800010, 11.69117318561000118, 1.923227876431999883 ) ) ;
#46163 = CARTESIAN_POINT ( 'NONE',  ( 5.268135431812000391, 0.8487381973356000753, -1.373673328256999948 ) ) ;
#46165 = B_SPLINE_CURVE_WITH_KNOTS ( 'NONE', 3,
 ( #55880, #67720, #40150, #25085 ),
 .UNSPECIFIED., .F., .F.,
 ( 4, 4 ),
 ( 0.000000000000000000, 1.000000000000000000 ),
 .UNSPECIFIED. ) ;
#46166 = CARTESIAN_POINT ( 'NONE',  ( 7.627539246035633269, -5.077375723878345681, 6.132675721286665826 ) ) ;
#46167 = CARTESIAN_POINT ( 'NONE',  ( 8.725348536223823004, 2.649439212887079620, 7.500023728975156345 ) ) ;
#46168 = CARTESIAN_POINT ( 'NONE',  ( 1.743247751179000105, 3.109069236570999539, 1.438230559479999782 ) ) ;
#46169 = ORIENTED_EDGE ( 'NONE', *, *, #51828, .F. ) ;
#46170 = CARTESIAN_POINT ( 'NONE',  ( 1.763186445774021838, 3.257444789362515802, -0.5454670069368401375 ) ) ;
#46171 = CARTESIAN_POINT ( 'NONE',  ( 11.56795257254739973, -4.963546614172099858, 7.219770138693499817 ) ) ;
#46172 = CARTESIAN_POINT ( 'NONE',  ( 10.82447135085921097, -5.732128138688877605, -7.156556136856877970 ) ) ;
#46173 = CARTESIAN_POINT ( 'NONE',  ( 9.980433037259000884, 4.047223446241999589, 9.090360698422999874 ) ) ;
#46174 = CARTESIAN_POINT ( 'NONE',  ( 10.33364828895399867, 4.760196147278000112, 7.084788038520800413 ) ) ;
#46175 = B_SPLINE_CURVE_WITH_KNOTS ( 'NONE', 3,
 ( #19008, #22868, #34067, #2248, #40002, #44219 ),
 .UNSPECIFIED., .F., .F.,
 ( 4, 2, 4 ),
 ( 0.000000000000000000, 0.5000000000000000000, 1.000000000000000000 ),
 .UNSPECIFIED. ) ;
#46176 = CARTESIAN_POINT ( 'NONE',  ( 23.67741535593912161, -3.195755220888627957, 13.38330436814928248 ) ) ;
#46177 = PLANE ( 'NONE',  #20969 ) ;
#46178 = EDGE_CURVE ( 'NONE', #8371, #44325, #27730, .T. ) ;
#46179 = CARTESIAN_POINT ( 'NONE',  ( 12.17766954483535891, -3.284117569315500251, 8.604570063127999546 ) ) ;
#46180 = ADVANCED_FACE ( 'NONE', ( #62406 ), #57496, .T. ) ;
#46181 = CARTESIAN_POINT ( 'NONE',  ( 8.100081893396536614, 4.526455162270248245, 5.827331516791772970 ) ) ;
#46182 = ORIENTED_EDGE ( 'NONE', *, *, #27664, .T. ) ;
#46183 = CARTESIAN_POINT ( 'NONE',  ( 17.65776394871757660, -1.883156081309886432, 13.78509897404221718 ) ) ;
#46184 = CARTESIAN_POINT ( 'NONE',  ( 20.60000000000000142, 0.000000000000000000, 0.000000000000000000 ) ) ;
#46185 = ORIENTED_EDGE ( 'NONE', *, *, #65572, .F. ) ;
#46186 = EDGE_LOOP ( 'NONE', ( #24017, #25802, #23919, #18721 ) ) ;
#46187 = CARTESIAN_POINT ( 'NONE',  ( 25.29996559941400136, -2.596925179230000325, -11.35302181744000016 ) ) ;
#46188 = DIRECTION ( 'NONE',  ( 0.000000000000000000, -0.7626730937533933163, -0.6467841618844942797 ) ) ;
#46189 = CARTESIAN_POINT ( 'NONE',  ( 11.17056785386839834, 3.281375110759499947, 7.016391833292499491 ) ) ;
#46190 = CARTESIAN_POINT ( 'NONE',  ( 11.02786554143000153, 5.596226216413000110, 7.209502215883999199 ) ) ;
#46191 = PLANE ( 'NONE',  #2003 ) ;
#46192 = DIRECTION ( 'NONE',  ( -1.000000000000000000, 0.000000000000000000, 0.000000000000000000 ) ) ;
#46193 = CARTESIAN_POINT ( 'NONE',  ( 10.23808992278000041, -2.752437370156000540, 6.820045513931999537 ) ) ;
#46194 = CARTESIAN_POINT ( 'NONE',  ( 17.96742813929299132, 0.5917181940048636957, -12.58609996267493258 ) ) ;
#46195 = CARTESIAN_POINT ( 'NONE',  ( 10.75911128370000114, -4.477561100530000004, -5.708582007447000173 ) ) ;
#46196 = CARTESIAN_POINT ( 'NONE',  ( 10.77672335273219950, -3.698477709264200275, -8.312023951944400579 ) ) ;
#46197 = CARTESIAN_POINT ( 'NONE',  ( 7.983198341228001205, 5.321913229613000063, 8.118244847118999630 ) ) ;
#46198 = ORIENTED_EDGE ( 'NONE', *, *, #46715, .T. ) ;
#46199 = EDGE_CURVE ( 'NONE', #29598, #34355, #35513, .T. ) ;
#46200 = MECHANICAL_DESIGN_GEOMETRIC_PRESENTATION_REPRESENTATION (  '', ( #44002 ), #48435 ) ;
#46201 = CARTESIAN_POINT ( 'NONE',  ( 11.01665855156000084, -5.432782508532000065, -4.991872683331999738 ) ) ;
#46202 = FILL_AREA_STYLE ('',( #8795 ) ) ;
#46203 = DIRECTION ( 'NONE',  ( 1.000000000000000000, 0.000000000000000000, 0.000000000000000000 ) ) ;
#46204 = EDGE_CURVE ( 'NONE', #55375, #66241, #9257, .T. ) ;
#46205 = VECTOR ( 'NONE', #36927, 1000.000000000000114 ) ;
#46206 = CARTESIAN_POINT ( 'NONE',  ( 17.67442079356964868, 1.770331164897448684, 12.47501301698789433 ) ) ;
#46207 = CARTESIAN_POINT ( 'NONE',  ( 9.279101285863998072, 3.176316400316700150, -6.521261160937499746 ) ) ;
#46208 = CARTESIAN_POINT ( 'NONE',  ( 12.10694218860113125, 2.320713384140923097, 13.80631828123456906 ) ) ;
#46209 = CARTESIAN_POINT ( 'NONE',  ( 10.57893103570000015, -4.649956431060000561, 5.681096060554999383 ) ) ;
#46210 = ORIENTED_EDGE ( 'NONE', *, *, #55359, .T. ) ;
#46211 = CARTESIAN_POINT ( 'NONE',  ( 12.40964703161358607, 0.4840289223742854641, -12.68758247551030038 ) ) ;
#46212 = CARTESIAN_POINT ( 'NONE',  ( 12.50552075632584881, -0.6654101994098641226, 13.98418081573739435 ) ) ;
#46213 = ORIENTED_EDGE ( 'NONE', *, *, #5695, .T. ) ;
#46214 = PLANE ( 'NONE',  #36535 ) ;
#46215 = B_SPLINE_CURVE_WITH_KNOTS ( 'NONE', 3,
 ( #45671, #19087, #20119, #41448 ),
 .UNSPECIFIED., .F., .F.,
 ( 4, 4 ),
 ( 0.000000000000000000, 1.000000000000000000 ),
 .UNSPECIFIED. ) ;
#46216 = FACE_OUTER_BOUND ( 'NONE', #21603, .T. ) ;
#46217 = CARTESIAN_POINT ( 'NONE',  ( 13.99999999270239570, 8.951333082579457923, 8.002096037671929452 ) ) ;
#46218 = CARTESIAN_POINT ( 'NONE',  ( 11.00595525820100029, -4.081787880721680750, 8.362327856951900173 ) ) ;
#46219 = DIRECTION ( 'NONE',  ( -1.000000000000000000, 0.000000000000000000, 0.000000000000000000 ) ) ;
#46220 = CARTESIAN_POINT ( 'NONE',  ( 0.2605877078939999869, -3.617551005558000021, 0.7847820700415000239 ) ) ;
#46221 = CARTESIAN_POINT ( 'NONE',  ( 10.25000000000000000, 0.000000000000000000, 0.000000000000000000 ) ) ;
#46222 = CARTESIAN_POINT ( 'NONE',  ( 12.47126843887705938, 3.119056300612241373, 12.20784669583219895 ) ) ;
#46223 = CARTESIAN_POINT ( 'NONE',  ( 10.90000000000000036, -8.618205959414002137, -7.308661029293999967 ) ) ;
#46224 = CARTESIAN_POINT ( 'NONE',  ( 10.77256919669529900, 4.962345366016100101, -7.784327714719899483 ) ) ;
#46225 = DIRECTION ( 'NONE',  ( 1.000000000000000000, 0.000000000000000000, 0.000000000000000000 ) ) ;
#46226 = AXIS2_PLACEMENT_3D ( 'NONE', #57053, #46225, #45880 ) ;
#46227 = CARTESIAN_POINT ( 'NONE',  ( 10.53197665877000055, 2.323713329709999886, -8.279493667389999700 ) ) ;
#46228 = CARTESIAN_POINT ( 'NONE',  ( 9.379355082327998971, 3.488994418336600400, -6.478918346312998899 ) ) ;
#46230 = CARTESIAN_POINT ( 'NONE',  ( 12.19116924869954310, 2.617374924051761642, 12.42344294663814530 ) ) ;
#46229 = CARTESIAN_POINT ( 'NONE',  ( 15.83176382712000319, -8.647155996545000889, -8.162171193140999037 ) ) ;
#46231 = CARTESIAN_POINT ( 'NONE',  ( 23.57355549871708433, -13.35445022547162708, 4.160309226275855643 ) ) ;
#46232 = EDGE_LOOP ( 'NONE', ( #54420, #45079, #43430, #6994, #1479, #58408 ) ) ;
#46233 = AXIS2_PLACEMENT_3D ( 'NONE', #23149, #8457, #13020 ) ;
#46234 = FACE_OUTER_BOUND ( 'NONE', #27041, .T. ) ;
#46235 = CARTESIAN_POINT ( 'NONE',  ( 10.56492304196000021, -4.212244324161999565, 8.933470634735002136 ) ) ;
#46236 = EDGE_CURVE ( 'NONE', #62317, #44668, #34714, .T. ) ;
#46237 = EDGE_CURVE ( 'NONE', #42044, #50821, #67990, .T. ) ;
#46238 = CARTESIAN_POINT ( 'NONE',  ( 10.13626717315599990, 3.235527139800300045, 8.151477970733999712 ) ) ;
#46239 = FACE_OUTER_BOUND ( 'NONE', #51989, .T. ) ;
#46240 = CARTESIAN_POINT ( 'NONE',  ( 24.35365242081700288, 11.54878985755999388, -2.979915831581000152 ) ) ;
#46241 = CARTESIAN_POINT ( 'NONE',  ( 21.35000154058000277, 0.000000000000000000, 0.000000000000000000 ) ) ;
#46242 = CARTESIAN_POINT ( 'NONE',  ( 7.031302189457115048, -1.093890586381388585, -0.8417396958425467091 ) ) ;
#46243 = ORIENTED_EDGE ( 'NONE', *, *, #5537, .F. ) ;
#46244 = VECTOR ( 'NONE', #40816, 1000.000000000000114 ) ;
#46245 = CARTESIAN_POINT ( 'NONE',  ( 9.151392757686998891, -3.229293331742300044, -8.342464052342599246 ) ) ;
#46246 = CARTESIAN_POINT ( 'NONE',  ( 10.53293305405438218, -4.959011670376446190, -5.009116636279086876 ) ) ;
#46247 = CARTESIAN_POINT ( 'NONE',  ( 11.60612378248510090, -4.482960757953799558, 8.413720204863100349 ) ) ;
#46248 = CARTESIAN_POINT ( 'NONE',  ( 17.92144340210919395, 1.859318429515440796, -12.46206136722992319 ) ) ;
#46249 = CARTESIAN_POINT ( 'NONE',  ( 2.553056799209334038, 2.798833948393625537, 2.150913519912209360 ) ) ;
#46250 = AXIS2_PLACEMENT_3D ( 'NONE', #50140, #17279, #38604 ) ;
#46251 = CARTESIAN_POINT ( 'NONE',  ( 5.399999743830999677, 12.99045401563999924, 1.690592933733000125 ) ) ;
#46252 = CARTESIAN_POINT ( 'NONE',  ( 8.328793652375997780, 2.897388771918001371, 6.655272502545993341 ) ) ;
#46253 = CARTESIAN_POINT ( 'NONE',  ( 9.086718600414000591, -4.531444417037000072, -6.133284059228000018 ) ) ;
#46254 = CARTESIAN_POINT ( 'NONE',  ( 5.200000000000000178, 0.000000000000000000, 0.000000000000000000 ) ) ;
#46255 = CARTESIAN_POINT ( 'NONE',  ( 9.621289888149728853, -3.647081445668406197, 8.849739427182552021 ) ) ;
#46256 = CONICAL_SURFACE ( 'NONE', #68543, 12.71246950475999959, 0.8960553845711767273 ) ;
#46257 = CARTESIAN_POINT ( 'NONE',  ( 12.15449479986285830, 0.3231860383015842109, -13.99628497142876071 ) ) ;
#46258 = CARTESIAN_POINT ( 'NONE',  ( 23.56664318980499928, 10.37807351222000030, 9.381504534996999212 ) ) ;
#46259 = ADVANCED_FACE ( 'NONE', ( #57851 ), #65497, .T. ) ;
#46260 = CARTESIAN_POINT ( 'NONE',  ( -0.2999999999999999889, 0.000000000000000000, 0.000000000000000000 ) ) ;
#46261 = EDGE_CURVE ( 'NONE', #55299, #60029, #40517, .T. ) ;
#46262 = CARTESIAN_POINT ( 'NONE',  ( 2.381500749193374844, 0.2450796643850099432, -3.507702501826547081 ) ) ;
#46263 = CARTESIAN_POINT ( 'NONE',  ( 17.74639017890735104, -11.23193386242373748, 3.094113022437827265 ) ) ;
#46264 = FACE_OUTER_BOUND ( 'NONE', #29779, .T. ) ;
#46265 = VERTEX_POINT ( 'NONE', #64799 ) ;
#46266 = EDGE_CURVE ( 'NONE', #2928, #12641, #31359, .T. ) ;
#46267 = CARTESIAN_POINT ( 'NONE',  ( 4.000000000000000888, -2.094138670346414433, 0.5626148410812730205 ) ) ;
#46268 = CARTESIAN_POINT ( 'NONE',  ( 18.12530810765558087, 2.066994332627597686, -13.84657437950017922 ) ) ;
#46269 = VERTEX_POINT ( 'NONE', #43501 ) ;
#46270 = CARTESIAN_POINT ( 'NONE',  ( 10.26331740696899963, -3.838745722419000028, 6.648116790593900483 ) ) ;
#46271 = CARTESIAN_POINT ( 'NONE',  ( 25.21374952102824096, 2.724994458594768076, 11.40631079751203814 ) ) ;
#46272 = CARTESIAN_POINT ( 'NONE',  ( 18.41067102831330615, 3.015843532951033357, -11.25293825120812663 ) ) ;
#46273 = CARTESIAN_POINT ( 'NONE',  ( 9.803753476949818690, 2.991225470601273528, -8.479526507175020100 ) ) ;
#46274 = CARTESIAN_POINT ( 'NONE',  ( 10.64902344389989963, -4.883530143601199747, -6.963800219468099684 ) ) ;
#46275 = DIRECTION ( 'NONE',  ( 0.000000000000000000, 1.000000000000000000, 0.000000000000000000 ) ) ;
#46276 = CARTESIAN_POINT ( 'NONE',  ( 8.807788144226000426, -3.909067355573210278, -8.453461841935100196 ) ) ;
#46277 = ORIENTED_EDGE ( 'NONE', *, *, #51225, .T. ) ;
#46278 = CARTESIAN_POINT ( 'NONE',  ( 8.856463691917767278, 5.100000000000000533, 6.665341197415465935 ) ) ;
#46279 = CARTESIAN_POINT ( 'NONE',  ( 10.82309687351566474, -5.217465845835395299, 7.827184855449101697 ) ) ;
#46280 = CARTESIAN_POINT ( 'NONE',  ( 9.725595280412999699, 2.495531372253999791, -7.930944806125000746 ) ) ;
#46281 = EDGE_LOOP ( 'NONE', ( #21078, #61915, #67594, #22192 ) ) ;
#46282 = CARTESIAN_POINT ( 'NONE',  ( 10.39355883036999906, 4.089958667033000594, -9.188186800857998549 ) ) ;
#46283 = SURFACE_STYLE_FILL_AREA ( #35453 ) ;
#46284 = VERTEX_POINT ( 'NONE', #16575 ) ;
#46285 = CARTESIAN_POINT ( 'NONE',  ( 8.872772138681998655, 3.575113238066399912, 8.559813987224998755 ) ) ;
#46286 = CARTESIAN_POINT ( 'NONE',  ( 17.74796797082753130, -1.905496177146738690, -12.57037238745254548 ) ) ;
#46287 = EDGE_CURVE ( 'NONE', #21661, #26111, #50552, .T. ) ;
#46288 = CARTESIAN_POINT ( 'NONE',  ( 11.25913316395000052, -11.80170809442000035, -1.433206434934999995 ) ) ;
#46289 = PRODUCT_DEFINITION_SHAPE ( 'NONE', 'NONE',  #69208 ) ;
#46290 = CARTESIAN_POINT ( 'NONE',  ( 10.94591266939078267, -8.077553304357570241, -7.023431445364937353 ) ) ;
#46291 = DIRECTION ( 'NONE',  ( 0.6684585169941805738, 0.6684585169941805738, -0.3260773253629903334 ) ) ;
#46292 = ORIENTED_EDGE ( 'NONE', *, *, #56579, .F. ) ;
#46293 = CARTESIAN_POINT ( 'NONE',  ( 24.67921570607400383, -3.567514742249000115, 12.13750887372000165 ) ) ;
#46294 = CARTESIAN_POINT ( 'NONE',  ( 10.69016084123000176, 4.391264627567999845, -8.802335896973000118 ) ) ;
#46295 = B_SPLINE_CURVE_WITH_KNOTS ( 'NONE', 3,
 ( #43662, #47877, #64959, #21631 ),
 .UNSPECIFIED., .F., .F.,
 ( 4, 4 ),
 ( 0.000000000000000000, 1.000000000000000000 ),
 .UNSPECIFIED. ) ;
#46296 = CIRCLE ( 'NONE', #66342, 14.00000000000000000 ) ;
#46297 = CARTESIAN_POINT ( 'NONE',  ( 11.09999999999999964, -5.299524241844999928, -5.124965750789000296 ) ) ;
#46298 = CARTESIAN_POINT ( 'NONE',  ( 12.10810820711261471, 2.719264802799586267, -13.73338027651840321 ) ) ;
#46299 = CARTESIAN_POINT ( 'NONE',  ( 18.10028295948236732, 0.4818816852691620300, 13.99171642476389721 ) ) ;
#46300 = AXIS2_PLACEMENT_3D ( 'NONE', #14880, #46010, #36202 ) ;
#46301 = CARTESIAN_POINT ( 'NONE',  ( 17.79325612864500172, 3.315492466914999881, 11.22361417850999921 ) ) ;
#46302 = CARTESIAN_POINT ( 'NONE',  ( 10.21685100254000034, 2.832432432432000269, 6.822293592207000934 ) ) ;
#46303 = EDGE_LOOP ( 'NONE', ( #57510, #61595, #41096, #45031, #60634, #62765, #53615, #64521, #51591, #46947 ) ) ;
#46304 = EDGE_LOOP ( 'NONE', ( #27359, #22859, #31330, #12161, #8551, #11665, #11435, #23491 ) ) ;
#46305 = CARTESIAN_POINT ( 'NONE',  ( 9.924495280410999598, 4.946705552514000459, -6.253848946732999181 ) ) ;
#46306 = CARTESIAN_POINT ( 'NONE',  ( 5.000000000000000000, 0.8000000000000000444, 3.149999999999999911 ) ) ;
#46307 = CARTESIAN_POINT ( 'NONE',  ( 12.24279999538967623, -2.226287937550149199, 13.72772666894641880 ) ) ;
#46308 = CARTESIAN_POINT ( 'NONE',  ( 24.01983208508439560, 3.345235842750158728, 12.71056888070838475 ) ) ;
#46309 = CARTESIAN_POINT ( 'NONE',  ( 11.41486084871699802, -5.207010770456999893, -7.825000000000000178 ) ) ;
#46311 = AXIS2_PLACEMENT_3D ( 'NONE', #2757, #66727, #34240 ) ;
#46310 = CARTESIAN_POINT ( 'NONE',  ( 18.02410434383600091, -3.285250940561000199, -11.23276246309000115 ) ) ;
#46313 = DIRECTION ( 'NONE',  ( 0.000000000000000000, -1.000000000000000000, 0.000000000000000000 ) ) ;
#46312 = CARTESIAN_POINT ( 'NONE',  ( 9.701101285863998669, -4.735211557675400584, 8.373612278672599274 ) ) ;
#46314 = CARTESIAN_POINT ( 'NONE',  ( 8.887792786201996975, -4.894798647533995073, -6.157725077911004874 ) ) ;
#46315 = ORIENTED_EDGE ( 'NONE', *, *, #42192, .F. ) ;
#46316 = CARTESIAN_POINT ( 'NONE',  ( 10.02052890782000105, 2.899999999999999911, 6.152188490330000370 ) ) ;
#46317 = CARTESIAN_POINT ( 'NONE',  ( 10.48719816214000033, -2.975817524382000201, -4.781958908427999866 ) ) ;
#46318 = ADVANCED_FACE ( 'NONE', ( #65146 ), #47898, .F. ) ;
#46319 = EDGE_CURVE ( 'NONE', #4104, #16477, #23802, .T. ) ;
#46320 = CARTESIAN_POINT ( 'NONE',  ( 9.710316810687000810, -2.624921803719999946, -8.200122328058998988 ) ) ;
#46321 = CARTESIAN_POINT ( 'NONE',  ( 7.890669420221000152, 4.660296061153999858, 6.322498784873999078 ) ) ;
#46322 = FACE_OUTER_BOUND ( 'NONE', #39192, .T. ) ;
#46323 = LINE ( 'NONE', #35826, #16288 ) ;
#46324 = CARTESIAN_POINT ( 'NONE',  ( 8.994485841233000656, 3.854507394315999758, -9.394302886912999639 ) ) ;
#46325 = CARTESIAN_POINT ( 'NONE',  ( 11.59999999999999964, 4.000000000000000000, 7.500000000000000000 ) ) ;
#46326 = CARTESIAN_POINT ( 'NONE',  ( 7.100000000000000533, 5.326087788487999575, -7.247035225330000330 ) ) ;
#46327 = CARTESIAN_POINT ( 'NONE',  ( 10.88834686957516418, -2.694378745198784841, -7.104278543674422686 ) ) ;
#46328 = B_SPLINE_SURFACE_WITH_KNOTS ( 'NONE', 3, 3, ( 
 ( #50036, #11929, #54934, #17530, #39546, #28369, #49332, #54586, #17169, #11573, #60868, #39198, #59825, #6681, #1446, #60521, #28025, #6327, #12630, #49684, #27678, #38860, #12984, #60181, #22763, #1793, #2144, #44110, #34307, #33959, #48992, #55281, #23463, #44799, #55629 ),
 ( #66103, #7728, #29071, #50381, #12287, #2480, #23806, #45139, #16821, #1103, #22413, #43756, #65051, #35682, #25527, #30436, #8763, #62240, #57330, #4190, #46514, #56657, #8419, #18912, #24151, #2820, #41262, #51067, #45484, #29418, #66449, #24499, #56314, #24841, #56995 ),
 ( #66799, #40237, #8076, #45821, #30104, #50727, #29762, #40917, #67476, #61554, #67132, #36014, #51407, #13671, #34999, #3503, #3170, #9097, #51747, #39897, #3841, #19243, #19597, #55970, #46168, #67817, #14357, #40570, #18570, #61898, #13333, #14012, #35341, #25179, #19941 ),
 ( #62576, #14696, #9432, #34657, #30774, #61217, #52086, #68851, #63609, #5228, #42979, #64286, #53128, #11161, #26566, #68501, #53474, #32496, #37733, #42307, #16403, #16059, #52434, #15034, #68159, #47891, #15725, #20624, #5568, #37051, #31464, #58367, #26909, #42638, #67576 ) ),
 .UNSPECIFIED., .F., .F., .F.,
 ( 4, 4 ),
 ( 4, 1, 1, 1, 1, 1, 1, 1, 1, 1, 1, 1, 1, 1, 1, 1, 1, 1, 1, 1, 1, 1, 1, 1, 1, 1, 1, 1, 1, 1, 1, 1, 4 ),
 ( -0.1039370721279000015, 1.103937072127999963 ),
 ( -0.01999999999996000116, 0.01250000000003000100, 0.04500000000002999517, 0.07750000000003000322, 0.1100000000000000006, 0.1424999999999999878, 0.1749999999999999889, 0.2074999999999999900, 0.2399999999999999911, 0.2725000000000000200, 0.3049999999999999933, 0.3375000000000000222, 0.3699999999999999956, 0.4025000000000000244, 0.4349999999999999978, 0.4675000000000000266, 0.5000000000000000000, 0.5324999999999999734, 0.5649999999999999467, 0.5975000000000000311, 0.6300000000000000044, 0.6624999999999999778, 0.6949999999999999512, 0.7275000000000000355, 0.7600000000000000089, 0.7924999999999999822, 0.8249999999999999556, 0.8575000000000000400, 0.8900000000000000133, 0.9224999999999999867, 0.9549999999999999600, 0.9875000000000000444, 1.020000000000000018 ),
 .UNSPECIFIED. ) ;
#46329 = CARTESIAN_POINT ( 'NONE',  ( 0.2285438277137852858, 3.144824486749696835, 0.8442605543570111948 ) ) ;
#46330 = MECHANICAL_DESIGN_GEOMETRIC_PRESENTATION_REPRESENTATION (  '', ( #6139 ), #44097 ) ;
#46331 = CARTESIAN_POINT ( 'NONE',  ( 3.682430813395999980, 0.3301581287572999956, -3.242144429603999622 ) ) ;
#46332 = VERTEX_POINT ( 'NONE', #34053 ) ;
#46333 = CARTESIAN_POINT ( 'NONE',  ( 12.61399029061283450, -0.5951698179256268428, -12.68122092285041624 ) ) ;
#46334 = CARTESIAN_POINT ( 'NONE',  ( 12.18412391182395815, -2.571774448735478558, -12.43455553904774646 ) ) ;
#46335 = CARTESIAN_POINT ( 'NONE',  ( 6.965816936038000229, -1.147328252452000097, 0.8605332073374000190 ) ) ;
#46336 = CARTESIAN_POINT ( 'NONE',  ( 9.091114158770999154, 3.762712042852999872, 8.787816121229999666 ) ) ;
#46337 = CARTESIAN_POINT ( 'NONE',  ( 25.29987261392200182, 9.517611874540000017, -8.103398312166000039 ) ) ;
#46338 = ORIENTED_EDGE ( 'NONE', *, *, #68467, .T. ) ;
#46339 = DIRECTION ( 'NONE',  ( 0.000000000000000000, -1.000000000000000000, 0.000000000000000000 ) ) ;
#46340 = LINE ( 'NONE', #56832, #38487 ) ;
#46341 = CARTESIAN_POINT ( 'NONE',  ( 13.06873602477000063, -11.64657800763999873, -1.862567138450999860 ) ) ;
#46342 = LINE ( 'NONE', #34828, #12775 ) ;
#46343 = CARTESIAN_POINT ( 'NONE',  ( 10.44999293566599974, 4.720032669050099550, -8.383280442119700027 ) ) ;
#46344 = ORIENTED_EDGE ( 'NONE', *, *, #44289, .T. ) ;
#46345 = EDGE_CURVE ( 'NONE', #28156, #33506, #38951, .T. ) ;
#46346 = CARTESIAN_POINT ( 'NONE',  ( 10.87148543990999983, -5.567571293949000300, 7.772413914480000408 ) ) ;
#46347 = ORIENTED_EDGE ( 'NONE', *, *, #30419, .T. ) ;
#46348 = CARTESIAN_POINT ( 'NONE',  ( 7.632848000845192438, -2.819393604944880671, 8.180463276640507431 ) ) ;
#46349 = CARTESIAN_POINT ( 'NONE',  ( 7.598066940377999678, -3.554853390786000045, 8.889491623367000273 ) ) ;
#46350 = AXIS2_PLACEMENT_3D ( 'NONE', #55054, #8193, #29542 ) ;
#46351 = CARTESIAN_POINT ( 'NONE',  ( 18.23380192947725931, -0.2577288767859217122, -13.99764474128114777 ) ) ;
#46352 = EDGE_LOOP ( 'NONE', ( #4438, #42552, #14196, #28530, #67776 ) ) ;
#46353 = CARTESIAN_POINT ( 'NONE',  ( 23.59379317251364228, 10.17887641161417278, 9.580899070374313098 ) ) ;
#46354 = CYLINDRICAL_SURFACE ( 'NONE', #47248, 3.500000000000000000 ) ;
#46355 = CARTESIAN_POINT ( 'NONE',  ( 7.084404719589999289, 4.524560801752999240, -6.025559345696000157 ) ) ;
#46356 = CARTESIAN_POINT ( 'NONE',  ( 23.66004879239100234, 13.39256428908000096, 3.813547978107000080 ) ) ;
#46357 = CARTESIAN_POINT ( 'NONE',  ( 8.159240506820934158, -3.000393948763773633, 6.388924361663858242 ) ) ;
#46358 = ORIENTED_EDGE ( 'NONE', *, *, #58923, .F. ) ;
#46359 = CARTESIAN_POINT ( 'NONE',  ( 2.115556799206792071, 0.4581489286485002088, 3.500000000000001776 ) ) ;
#46360 = CARTESIAN_POINT ( 'NONE',  ( 12.19259091212767210, -2.624575865053327295, -13.64619539123898839 ) ) ;
#46361 = CARTESIAN_POINT ( 'NONE',  ( 12.09999922233642344, 11.66744139996707119, -3.971920075670921424 ) ) ;
#46362 = VERTEX_POINT ( 'NONE', #61639 ) ;
#46363 = CARTESIAN_POINT ( 'NONE',  ( 10.60519595724999853, -5.343977295764999802, -7.731524081231999190 ) ) ;
#46364 = CARTESIAN_POINT ( 'NONE',  ( 9.674960421382822418, -2.650268802167429438, 7.499999178247414910 ) ) ;
#46365 = VERTEX_POINT ( 'NONE', #33703 ) ;
#46366 = CARTESIAN_POINT ( 'NONE',  ( 24.13558027894506353, 12.48959359056989094, -3.366848964696536051 ) ) ;
#46367 = EDGE_CURVE ( 'NONE', #35521, #38774, #22185, .T. ) ;
#46368 = CARTESIAN_POINT ( 'NONE',  ( 17.60000000000000142, 52.95171880992000268, -18.02623547589999831 ) ) ;
#46369 = CARTESIAN_POINT ( 'NONE',  ( 15.39999999998900293, -9.471998555523999386, -8.194929586088999685 ) ) ;
#46370 = CARTESIAN_POINT ( 'NONE',  ( 10.92292960915206201, 5.090154163873960691, -5.014592317151394418 ) ) ;
#46371 = CARTESIAN_POINT ( 'NONE',  ( 12.23133660942382583, -0.2481576080865461609, -13.89702325994032961 ) ) ;
#46372 = AXIS2_PLACEMENT_3D ( 'NONE', #10681, #27120, #11709 ) ;
#46373 = CARTESIAN_POINT ( 'NONE',  ( 18.05401280175963663, -2.123066371663036023, 12.53147770072749623 ) ) ;
#46374 = VERTEX_POINT ( 'NONE', #44554 ) ;
#46375 = CARTESIAN_POINT ( 'NONE',  ( 8.251326917914997949, -4.957166827433998613, 6.172577619222003875 ) ) ;
#46376 = ORIENTED_EDGE ( 'NONE', *, *, #60926, .F. ) ;
#46377 = CARTESIAN_POINT ( 'NONE',  ( 9.959641781044998865, 5.406625910119999823, 7.700299649248999678 ) ) ;
#46378 = CARTESIAN_POINT ( 'NONE',  ( 11.14975833414749928, -4.796537143354000499, -7.825000000000000178 ) ) ;
#46379 = CARTESIAN_POINT ( 'NONE',  ( 8.979720280412999855, 5.524776413195999325, -7.147585171405999915 ) ) ;
#46380 = CARTESIAN_POINT ( 'NONE',  ( 2.719500174877999665, -3.192447183199000005, -1.538248846112000079 ) ) ;
#46381 = CARTESIAN_POINT ( 'NONE',  ( 17.80000000001300009, 3.351264566333000072, -11.15757590352999884 ) ) ;
#46382 = DIRECTION ( 'NONE',  ( -0.000000000000000000, -0.000000000000000000, 1.000000000000000000 ) ) ;
#46383 = VERTEX_POINT ( 'NONE', #45257 ) ;
#46384 = CARTESIAN_POINT ( 'NONE',  ( 7.100000000000000533, 5.221516520829000640, -8.074802043613001246 ) ) ;
#46385 = EDGE_LOOP ( 'NONE', ( #8222, #52801, #13135 ) ) ;
#46386 = CARTESIAN_POINT ( 'NONE',  ( 11.39149144726329865, -4.659577337894599935, 8.430724369296298093 ) ) ;
#46387 = CARTESIAN_POINT ( 'NONE',  ( 10.38355189346693663, 5.519214728663544456, -8.419505157002880935 ) ) ;
#46388 = CARTESIAN_POINT ( 'NONE',  ( 15.35870478550200069, 9.525289020731998235, 8.192348383776000276 ) ) ;
#46389 = CARTESIAN_POINT ( 'NONE',  ( 24.14474089025218717, 9.246824087223631139, 9.586721689821816383 ) ) ;
#46391 = CARTESIAN_POINT ( 'NONE',  ( 13.70003001321900271, 9.668726926528000476, 7.961868161445000425 ) ) ;
#46390 = CARTESIAN_POINT ( 'NONE',  ( 9.910790522921001156, 3.869345236050000025, 5.882548872612999524 ) ) ;
#46392 = CARTESIAN_POINT ( 'NONE',  ( 10.45257053952200010, 3.605640676136899980, -6.577269499510100204 ) ) ;
#46393 = CARTESIAN_POINT ( 'NONE',  ( 10.91620964606000044, 2.818413279081999789, -6.814156272943999504 ) ) ;
#46394 = AXIS2_PLACEMENT_3D ( 'NONE', #30158, #25234, #51461 ) ;
#46395 = CARTESIAN_POINT ( 'NONE',  ( 10.08560887879199797, 3.772542739612499751, -6.521682313853199631 ) ) ;
#46396 = EDGE_CURVE ( 'NONE', #7557, #5127, #66535, .T. ) ;
#46397 = EDGE_CURVE ( 'NONE', #7868, #44775, #39289, .T. ) ;
#46398 = CARTESIAN_POINT ( 'NONE',  ( 17.82189142195447573, 0.6689034848678535594, 12.58223305319197394 ) ) ;
#46399 = CARTESIAN_POINT ( 'NONE',  ( 24.43231275843400141, 3.176386277817000003, 12.00227839950999886 ) ) ;
#46400 = CARTESIAN_POINT ( 'NONE',  ( 10.52799293566599914, 4.806678152079100208, 6.510429574318199464 ) ) ;
#46401 = FACE_OUTER_BOUND ( 'NONE', #69055, .T. ) ;
#46402 = ORIENTED_EDGE ( 'NONE', *, *, #61237, .T. ) ;
#46403 = CARTESIAN_POINT ( 'NONE',  ( 7.935745559623000212, -5.430412429559000387, 7.210798766422999329 ) ) ;
#46404 = ADVANCED_FACE ( 'NONE', ( #28816, #39635 ), #60957, .T. ) ;
#46405 = EDGE_CURVE ( 'NONE', #56474, #27465, #38034, .T. ) ;
#46406 = DIRECTION ( 'NONE',  ( 0.7071067538246033068, -0.5063796871227020935, 0.4935378923296021569 ) ) ;
#46407 = CARTESIAN_POINT ( 'NONE',  ( 5.000030787343000327, -1.057581170753189248, -1.834918991542628275 ) ) ;
#46408 = CARTESIAN_POINT ( 'NONE',  ( 27.64127793187000037, -5.599999999999999645, 6.571291218949999902 ) ) ;
#46409 = EDGE_LOOP ( 'NONE', ( #51528, #42072, #12105, #62682, #37690, #7394, #40172, #30748 ) ) ;
#46410 = CARTESIAN_POINT ( 'NONE',  ( 17.98628609634500108, 3.388648274289000284, 11.90503202562999974 ) ) ;
#46411 = CARTESIAN_POINT ( 'NONE',  ( 10.51414141025500015, 4.615773412711500434, 6.403245959303999868 ) ) ;
#46412 = CARTESIAN_POINT ( 'NONE',  ( 10.05462971959000029, 3.531217403581000003, -9.119235467071000301 ) ) ;
#46413 = ORIENTED_EDGE ( 'NONE', *, *, #25309, .F. ) ;
#46414 = CARTESIAN_POINT ( 'NONE',  ( 1.530140132540667164, 3.408904368339106483, -0.9161175952574748260 ) ) ;
#46415 = CARTESIAN_POINT ( 'NONE',  ( 17.60408629075383047, -3.199716927301871738, 12.18695251432577464 ) ) ;
#46416 = CARTESIAN_POINT ( 'NONE',  ( 10.81349144726329925, 3.261052100888700345, 8.542723541016000510 ) ) ;
#46417 = CARTESIAN_POINT ( 'NONE',  ( 13.92020863217304338, -9.472241403191583586, -8.194648738509743069 ) ) ;
#46418 = CARTESIAN_POINT ( 'NONE',  ( 14.70000000000000107, 8.824259102667999954, 7.756628703356000187 ) ) ;
#46419 = EDGE_LOOP ( 'NONE', ( #36743, #47980, #9433, #43103 ) ) ;
#46420 = CARTESIAN_POINT ( 'NONE',  ( 5.000000000000000000, 0.000000000000000000, 0.000000000000000000 ) ) ;
#46421 = CARTESIAN_POINT ( 'NONE',  ( -1.222471984994595150E-05, -9.327013418423733093E-16, -2.899969545326207765 ) ) ;
#46422 = B_SPLINE_CURVE_WITH_KNOTS ( 'NONE', 3,
 ( #62847, #26151, #62169, #68433 ),
 .UNSPECIFIED., .F., .F.,
 ( 4, 4 ),
 ( 0.000000000000000000, 1.000000000000000000 ),
 .UNSPECIFIED. ) ;
#46423 = CARTESIAN_POINT ( 'NONE',  ( 8.199057584334923376, -5.747876374591468718, 7.505538406481026215 ) ) ;
#46424 = CONICAL_SURFACE ( 'NONE', #43071, 11.34994642770999818, 0.7853934433896081480 ) ;
#46425 = CARTESIAN_POINT ( 'NONE',  ( 10.35859632033900013, -5.184381781355999586, 7.983346856269500691 ) ) ;
#46426 = ORIENTED_EDGE ( 'NONE', *, *, #38350, .T. ) ;
#46427 = CARTESIAN_POINT ( 'NONE',  ( -0.2999999999999999889, 0.5773502691895999739, 1.000000000000000000 ) ) ;
#46428 = CARTESIAN_POINT ( 'NONE',  ( 11.14118447801630118, -2.722297859592000435, 7.528171279442569919 ) ) ;
#46429 = EDGE_LOOP ( 'NONE', ( #52328, #60539, #33799, #62894 ) ) ;
#46430 = CARTESIAN_POINT ( 'NONE',  ( 11.50029455687000102, -11.62161504227245779, -0.9384843035876943018 ) ) ;
#46431 = VECTOR ( 'NONE', #20686, 1000.000000000000000 ) ;
#46432 = EDGE_LOOP ( 'NONE', ( #54711, #1886, #45073, #2211 ) ) ;
#46433 = CARTESIAN_POINT ( 'NONE',  ( 9.756901401888999459, -3.283392111224999965, -8.676955243274001361 ) ) ;
#46434 = CARTESIAN_POINT ( 'NONE',  ( 2.342640132542833431, -3.058252359239902685, -1.762666431298148595 ) ) ;
#46435 = CARTESIAN_POINT ( 'NONE',  ( 10.93990547754509812, 5.032986398992000510, -7.532784233952049213 ) ) ;
#46436 = CARTESIAN_POINT ( 'NONE',  ( 12.05300581613033906, -2.892415530317000272, 6.788791567531699656 ) ) ;
#46437 = CARTESIAN_POINT ( 'NONE',  ( 12.24413029362356831, 2.775858423521469387, -12.38303112237259640 ) ) ;
#46438 = CARTESIAN_POINT ( 'NONE',  ( 10.77610941423800028, -3.155589807313900153, 8.266982106121901097 ) ) ;
#46439 = PLANE ( 'NONE',  #51039 ) ;
#46440 = ORIENTED_EDGE ( 'NONE', *, *, #54208, .F. ) ;
#46441 = CARTESIAN_POINT ( 'NONE',  ( 10.62947109217999930, -5.100000000000000533, 6.152188490330000370 ) ) ;
#46442 = B_SPLINE_CURVE_WITH_KNOTS ( 'NONE', 3,
 ( #5240, #25540, #63621, #68862 ),
 .UNSPECIFIED., .F., .F.,
 ( 4, 4 ),
 ( 0.000000000000000000, 1.000000000000000000 ),
 .UNSPECIFIED. ) ;
#46443 = CARTESIAN_POINT ( 'NONE',  ( 7.326308059621999824, -3.394845988290999816, 9.388942682504000103 ) ) ;
#46444 = DIRECTION ( 'NONE',  ( 1.000000000000000000, 0.000000000000000000, 0.000000000000000000 ) ) ;
#46445 = VERTEX_POINT ( 'NONE', #18655 ) ;
#46446 = CARTESIAN_POINT ( 'NONE',  ( 12.18120961385786849, -2.543048387066361382, -12.44145101111442919 ) ) ;
#46448 = CARTESIAN_POINT ( 'NONE',  ( 10.30072469555899950, 4.570852684939899824, 8.487632181750699445 ) ) ;
#46447 = CIRCLE ( 'NONE', #15191, 1.000000000000000000 ) ;
#46449 = EDGE_CURVE ( 'NONE', #38985, #12348, #8162, .T. ) ;
#46450 = CARTESIAN_POINT ( 'NONE',  ( 10.29666814679000097, -2.755511079787000384, -6.622434938646999392 ) ) ;
#46451 = CARTESIAN_POINT ( 'NONE',  ( 8.675198109782005673, 10.51530723774999032, -4.257112462104002404 ) ) ;
#46452 = CARTESIAN_POINT ( 'NONE',  ( 17.79403162610499933, -3.298115360370000193, -11.83441368098000090 ) ) ;
#46453 = CARTESIAN_POINT ( 'NONE',  ( 24.35146665670700017, -8.929414329885000612, 9.054894786836999998 ) ) ;
#46454 = CARTESIAN_POINT ( 'NONE',  ( 12.33271654538604523, -2.090191715682863993, -13.75184336857262402 ) ) ;
#46455 = EDGE_CURVE ( 'NONE', #64217, #52427, #45575, .T. ) ;
#46456 = CARTESIAN_POINT ( 'NONE',  ( 10.85056919669530018, -3.169300617545700138, -7.745432529082900253 ) ) ;
#46457 = CARTESIAN_POINT ( 'NONE',  ( 11.05964426047339799, -3.312306505177499805, -8.577215873335999774 ) ) ;
#46458 = DIRECTION ( 'NONE',  ( 0.000000000000000000, 0.000000000000000000, -1.000000000000000000 ) ) ;
#46459 = EDGE_LOOP ( 'NONE', ( #30311, #52407, #2240, #28740 ) ) ;
#46460 = VERTEX_POINT ( 'NONE', #35764 ) ;
#46461 = CARTESIAN_POINT ( 'NONE',  ( 12.15888864299428640, 0.3818843737314618902, -13.99543728850283131 ) ) ;
#46462 = CARTESIAN_POINT ( 'NONE',  ( 9.832537864288001472, 2.899999999999999911, 6.571291218949999902 ) ) ;
#46463 = CARTESIAN_POINT ( 'NONE',  ( 18.12469242171570372, 2.757364536613152062, 13.61544764691891629 ) ) ;
#46464 = CARTESIAN_POINT ( 'NONE',  ( 11.10062015617000064, 3.093053541899000169, -6.153678467293999255 ) ) ;
#46465 = CARTESIAN_POINT ( 'NONE',  ( 8.639949174999173920, 5.001557281985752113, 6.108253387157301262 ) ) ;
#46466 = CARTESIAN_POINT ( 'NONE',  ( 18.11139879660519014, 2.784965558754640913, 12.38059455073776505 ) ) ;
#46467 = CARTESIAN_POINT ( 'NONE',  ( 17.86534991953400109, 3.412585803847000054, -11.89775424487000066 ) ) ;
#46468 = CARTESIAN_POINT ( 'NONE',  ( 9.075483283097998566, 4.020836891789999257, 8.948690653012000951 ) ) ;
#46469 = CARTESIAN_POINT ( 'NONE',  ( 11.54292372906209074, -2.967457464456211280, -8.269164421058194492 ) ) ;
#46470 = VERTEX_POINT ( 'NONE', #26305 ) ;
#46471 = CARTESIAN_POINT ( 'NONE',  ( 10.15403136780999915, 5.267988602993999514, 5.992335067371000079 ) ) ;
#46472 = CARTESIAN_POINT ( 'NONE',  ( 9.045101285863999863, -4.558267473659599389, -6.836640842107200022 ) ) ;
#46473 = CARTESIAN_POINT ( 'NONE',  ( 10.53734212242000012, 2.992816679959000137, 8.731689474572998932 ) ) ;
#46474 = CARTESIAN_POINT ( 'NONE',  ( 11.97500581613029880, -3.011381429075500105, 6.865182626353099948 ) ) ;
#46475 = CARTESIAN_POINT ( 'NONE',  ( 11.66486084871730000, -2.792989229543000107, 7.825000000000000178 ) ) ;
#46476 = CARTESIAN_POINT ( 'NONE',  ( 9.049999337612000261, -3.819167204710999825E-14, 1.447065004412999939E-13 ) ) ;
#46477 = CARTESIAN_POINT ( 'NONE',  ( 24.98632682924400328, 8.514528481086999889, 8.479295295784998743 ) ) ;
#46478 = CARTESIAN_POINT ( 'NONE',  ( 12.42472005158248294, 0.4959841406075979342, 12.68696163625449103 ) ) ;
#46479 = AXIS2_PLACEMENT_3D ( 'NONE', #39406, #33131, #6891 ) ;
#46480 = CARTESIAN_POINT ( 'NONE',  ( 8.096551658772000337, 5.061727314042999915, 5.824077473724000420 ) ) ;
#46481 = EDGE_CURVE ( 'NONE', #36471, #65786, #6500, .T. ) ;
#46482 = CARTESIAN_POINT ( 'NONE',  ( 11.18051582549000145, 5.340073783367000892, 8.416152717850000187 ) ) ;
#46483 = DIRECTION ( 'NONE',  ( 1.000000000000000000, 0.000000000000000000, 0.000000000000000000 ) ) ;
#46484 = EDGE_LOOP ( 'NONE', ( #6511, #57928, #17100, #34429, #63522 ) ) ;
#46485 = CARTESIAN_POINT ( 'NONE',  ( 8.839404719593998649, 5.140767546012999567, -6.196177269779999719 ) ) ;
#46486 = CARTESIAN_POINT ( 'NONE',  ( 7.066756274120936432, 0.2616187012132839551, 3.032564036156813803 ) ) ;
#46487 = EDGE_CURVE ( 'NONE', #57987, #9965, #52523, .T. ) ;
#46488 = EDGE_CURVE ( 'NONE', #5900, #28902, #68861, .T. ) ;
#46489 = CARTESIAN_POINT ( 'NONE',  ( 17.92197813837931619, 1.993632751867237207, 13.76786175838295279 ) ) ;
#46490 = LINE ( 'NONE', #35991, #4994 ) ;
#46491 = CARTESIAN_POINT ( 'NONE',  ( 12.09999999999999609, -3.064876132552082577, 8.208828950335220753 ) ) ;
#46492 = CARTESIAN_POINT ( 'NONE',  ( 11.65871932425156920, -4.147141405561299621, -8.492622906483498824 ) ) ;
#46493 = ORIENTED_EDGE ( 'NONE', *, *, #38832, .T. ) ;
#46494 = CIRCLE ( 'NONE', #21922, 0.2999999999999993228 ) ;
#46495 = CARTESIAN_POINT ( 'NONE',  ( 2.158975548941000078, -3.419251011552999930, 1.101167613520000144 ) ) ;
#46496 = CARTESIAN_POINT ( 'NONE',  ( 10.32332547010959090, -4.027151052029898537, 9.388407014067791323 ) ) ;
#46499 = CARTESIAN_POINT ( 'NONE',  ( 4.550000802215999229, 1.829647544581999737E-13, 0.000000000000000000 ) ) ;
#46498 = CARTESIAN_POINT ( 'NONE',  ( 9.694764498856436319, 5.745394236816313338, 7.382991512957417513 ) ) ;
#46497 = UNCERTAINTY_MEASURE_WITH_UNIT (LENGTH_MEASURE( 1.000000000000000082E-05 ), #17480, 'distance_accuracy_value', 'NONE');
#46500 = DIRECTION ( 'NONE',  ( 0.000000000000000000, 0.1807154286440006141, -0.9835354258236025382 ) ) ;
#46501 = B_SPLINE_CURVE_WITH_KNOTS ( 'NONE', 3,
 ( #30559, #5010, #22121, #31253, #47674, #10258, #32291, #26346, #5696, #52563 ),
 .UNSPECIFIED., .F., .F.,
 ( 4, 2, 2, 2, 4 ),
 ( 0.000000000000000000, 0.1248149689023889258, 0.2496299378047778517, 0.3744449067071667914, 0.4992598756095557033 ),
 .UNSPECIFIED. ) ;
#46502 = CARTESIAN_POINT ( 'NONE',  ( 25.55273627768460543, -8.264546374049874800, 8.081436664941460180 ) ) ;
#46503 = CARTESIAN_POINT ( 'NONE',  ( 18.01397738364139300, -2.075598766708243836, -13.75431519107022815 ) ) ;
#46504 = CARTESIAN_POINT ( 'NONE',  ( 11.63825819896753977, 3.148796120250299868, 7.339530235223699073 ) ) ;
#46505 = CARTESIAN_POINT ( 'NONE',  ( 5.500000000000000000, -1.406666666667000021, -10.45580168561000001 ) ) ;
#46506 = CARTESIAN_POINT ( 'NONE',  ( 7.308879440377999970, -4.847802017252000439, 9.065364004483999594 ) ) ;
#46507 = VERTEX_POINT ( 'NONE', #57080 ) ;
#46508 = CARTESIAN_POINT ( 'NONE',  ( 9.202760841230999134, 2.542862824481000317, 7.419808961972999661 ) ) ;
#46509 = ADVANCED_FACE ( 'NONE', ( #9180 ), #42039, .F. ) ;
#46511 = CARTESIAN_POINT ( 'NONE',  ( 11.06205805961999999, -2.154403720901000518, -7.605897512385999981 ) ) ;
#46510 = CARTESIAN_POINT ( 'NONE',  ( 6.226007504534000425, 0.03883618666160999766, -1.614257485795999925 ) ) ;
#46512 = CARTESIAN_POINT ( 'NONE',  ( 7.468325272381751034, -2.307615737728840433, 7.097574564742653358 ) ) ;
#46513 = CARTESIAN_POINT ( 'NONE',  ( 17.98741890697079882, -0.4515201817464164491, 13.89013314510155261 ) ) ;
#46514 = CARTESIAN_POINT ( 'NONE',  ( 1.461929392595999966, -1.374622313384999961, -3.318774223758000019 ) ) ;
#46515 = ORIENTED_EDGE ( 'NONE', *, *, #64570, .F. ) ;
#46516 = DIRECTION ( 'NONE',  ( 0.000000000000000000, 0.9565994702956990281, 0.2914059941558995726 ) ) ;
#46517 = CARTESIAN_POINT ( 'NONE',  ( 12.08487348028855024, -4.882707455860599843, 7.022738645480499642 ) ) ;
#46518 = CARTESIAN_POINT ( 'NONE',  ( 10.70559276782025648, -5.069448745120865851, 5.072976836019464031 ) ) ;
#46519 = CARTESIAN_POINT ( 'NONE',  ( 9.813360311708999362, 5.349397258738000538, 6.657026394682000081 ) ) ;
#46520 = CARTESIAN_POINT ( 'NONE',  ( 11.60533460557258323, 4.184174550317700358, 6.374224726731999802 ) ) ;
#46521 = CARTESIAN_POINT ( 'NONE',  ( 23.65871200092008309, -3.166282759754092346, 13.42477648256529044 ) ) ;
#46522 = CARTESIAN_POINT ( 'NONE',  ( 9.525000000000000355, -4.417172942406000224, 8.783926296998000538 ) ) ;
#46523 = CARTESIAN_POINT ( 'NONE',  ( 10.98745755813032332, -5.203136861518676604, 6.684049838556305190 ) ) ;
#46524 = CARTESIAN_POINT ( 'NONE',  ( 24.48514017958100197, -3.324320173708000148, -12.08694633982000077 ) ) ;
#46525 = CIRCLE ( 'NONE', #57686, 11.84999999999999964 ) ;
#46526 = CARTESIAN_POINT ( 'NONE',  ( 18.06104743845540384, -3.040966990778160017, 13.66574534766771620 ) ) ;
#46527 = CARTESIAN_POINT ( 'NONE',  ( 17.75978284915347771, 3.091857219545061763, -13.52996931830681149 ) ) ;
#46529 = ORIENTED_EDGE ( 'NONE', *, *, #25332, .F. ) ;
#46528 = B_SPLINE_CURVE_WITH_KNOTS ( 'NONE', 3,
 ( #29307, #18811, #12524, #55520, #28259, #34555 ),
 .UNSPECIFIED., .F., .F.,
 ( 4, 2, 4 ),
 ( 0.000000000000000000, 0.5000000000000000000, 1.000000000000000000 ),
 .UNSPECIFIED. ) ;
#46530 = CARTESIAN_POINT ( 'NONE',  ( 5.002606837613999602, -0.4199405305951999789, 1.440017343911000003 ) ) ;
#46531 = CARTESIAN_POINT ( 'NONE',  ( 9.120327454391752298, -2.808826379911543825, -7.088789390544037339 ) ) ;
#46532 = ORIENTED_EDGE ( 'NONE', *, *, #60776, .T. ) ;
#46533 = FACE_OUTER_BOUND ( 'NONE', #44393, .T. ) ;
#46534 = CARTESIAN_POINT ( 'NONE',  ( 15.90018573812067260, 4.599694346030502423, 10.96245233228960814 ) ) ;
#46535 = AXIS2_PLACEMENT_3D ( 'NONE', #43528, #48420, #526 ) ;
#46536 = CARTESIAN_POINT ( 'NONE',  ( 9.848730799670999403, 2.769737997918999994, 6.441853401936000090 ) ) ;
#46537 = CARTESIAN_POINT ( 'NONE',  ( 10.98277660187000215, 2.518725482848000130, -8.314790074023999722 ) ) ;
#46538 = CARTESIAN_POINT ( 'NONE',  ( 10.08809113605762597, -4.810085401003767913, -7.169403702379763210 ) ) ;
#46539 = CARTESIAN_POINT ( 'NONE',  ( 10.37026726325999881, -5.571557883540000589, 7.748386351620999868 ) ) ;
#46540 = CARTESIAN_POINT ( 'NONE',  ( 18.17069881803083931, 0.3800566752825912387, -12.59427093624936767 ) ) ;
#46541 = EDGE_CURVE ( 'NONE', #23923, #16538, #9670, .T. ) ;
#46542 = CIRCLE ( 'NONE', #4093, 12.50000000000000178 ) ;
#46543 = CARTESIAN_POINT ( 'NONE',  ( 24.30000561204433396, -12.09374146552009499, -3.240508259158020987 ) ) ;
#46544 = CARTESIAN_POINT ( 'NONE',  ( 11.17056785386839834, -4.718624889240500053, -7.983608166707499620 ) ) ;
#46545 = CARTESIAN_POINT ( 'NONE',  ( 7.871384613761001070, -5.129340912189999990, 6.740051747100999968 ) ) ;
#46546 = VERTEX_POINT ( 'NONE', #36445 ) ;
#46547 = B_SPLINE_CURVE_WITH_KNOTS ( 'NONE', 3,
 ( #23346, #33845, #38387, #65984, #65296, #11464, #44344, #65641, #49220, #27215, #17768, #48540, #60410, #48886, #18110, #646, #39429 ),
 .UNSPECIFIED., .F., .F.,
 ( 4, 2, 2, 2, 1, 2, 2, 2, 4 ),
 ( 0.000000000000000000, 0.1250000000000000833, 0.2500000000000001665, 0.3750000000000000555, 0.5000000000000000000, 0.6250000000000000000, 0.7499999999999998890, 0.8750000000000000000, 1.000000000000000000 ),
 .UNSPECIFIED. ) ;
#46548 = CIRCLE ( 'NONE', #55478, 11.84999999999999964 ) ;
#46549 = CARTESIAN_POINT ( 'NONE',  ( 11.02039621389999979, -5.798238435757999909, -5.016446396665000584 ) ) ;
#46550 = SURFACE_SIDE_STYLE ('',( #57029 ) ) ;
#46551 = DIRECTION ( 'NONE',  ( 1.000000000000000000, 0.000000000000000000, 0.000000000000000000 ) ) ;
#46552 = CARTESIAN_POINT ( 'NONE',  ( 11.79999999550100220, -11.52577121388000059, -1.696750555870000010 ) ) ;
#46553 = DIRECTION ( 'NONE',  ( -1.000000000000000000, 0.000000000000000000, 0.000000000000000000 ) ) ;
#46554 = CARTESIAN_POINT ( 'NONE',  ( 12.22752497338536415, 2.076440593937394219, 13.84516123709150826 ) ) ;
#46555 = CARTESIAN_POINT ( 'NONE',  ( 10.35616740164000049, -2.777283710737999733, 8.995265811011998736 ) ) ;
#46556 = VERTEX_POINT ( 'NONE', #36797 ) ;
#46557 = CARTESIAN_POINT ( 'NONE',  ( 12.19608323748815160, 0.1421782556677775866, -12.69895087450945503 ) ) ;
#46558 = CARTESIAN_POINT ( 'NONE',  ( 12.78109998040213213, -0.7302151644511187811, 13.98094363559787467 ) ) ;
#46559 = VERTEX_POINT ( 'NONE', #56750 ) ;
#46560 = FACE_OUTER_BOUND ( 'NONE', #11407, .T. ) ;
#46561 = CARTESIAN_POINT ( 'NONE',  ( 24.44496483130000186, -3.224879855413000040, 12.03535978074999946 ) ) ;
#46562 = CARTESIAN_POINT ( 'NONE',  ( 10.69809687351600225, -3.672815144550895639, -6.282534154164608253 ) ) ;
#46563 = CARTESIAN_POINT ( 'NONE',  ( 12.08902763632552002, -4.786505910413500153, 7.862914650060299770 ) ) ;
#46564 = DIRECTION ( 'NONE',  ( -1.000000000000000000, 0.000000000000000000, 0.000000000000000000 ) ) ;
#46565 = LINE ( 'NONE', #61269, #804 ) ;
#46566 = CYLINDRICAL_SURFACE ( 'NONE', #52727, 0.4999999999999998335 ) ;
#46567 = CARTESIAN_POINT ( 'NONE',  ( 12.17424305300934151, 2.124765750614183712, 12.41957393385126451 ) ) ;
#46568 = CARTESIAN_POINT ( 'NONE',  ( 9.177304894000000601, -4.588307032459999490, -5.987050435448999508 ) ) ;
#46569 = CARTESIAN_POINT ( 'NONE',  ( 11.31410538575739899, 4.975963290822400076, -7.266662245194900116 ) ) ;
#46570 = CARTESIAN_POINT ( 'NONE',  ( 17.80000000005199823, 3.345268251980999974, 11.86064071431999878 ) ) ;
#46571 = EDGE_CURVE ( 'NONE', #32816, #2080, #16365, .T. ) ;
#46572 = EDGE_CURVE ( 'NONE', #2494, #18236, #32236, .T. ) ;
#46573 = CARTESIAN_POINT ( 'NONE',  ( 10.73724174883999893, 3.975468761016990094, -8.391788556008700439 ) ) ;
#46574 = CARTESIAN_POINT ( 'NONE',  ( 9.858596320338998353, 2.815618218644000414, -7.016653143730500197 ) ) ;
#46576 = CARTESIAN_POINT ( 'NONE',  ( 12.18869345029320606, 2.603827955627350477, 12.42676989083816252 ) ) ;
#46575 = CARTESIAN_POINT ( 'NONE',  ( 9.048601287889788125, -3.999999532294070459, -8.698595322193611423 ) ) ;
#46577 = CARTESIAN_POINT ( 'NONE',  ( 12.80505043854143388, 1.875000000000000000, -13.78631952119025073 ) ) ;
#46578 = ORIENTED_EDGE ( 'NONE', *, *, #28012, .F. ) ;
#46579 = CIRCLE ( 'NONE', #43220, 0.3000000000000007105 ) ;
#46580 = B_SPLINE_CURVE_WITH_KNOTS ( 'NONE', 3,
 ( #68961, #53575, #15142, #63711 ),
 .UNSPECIFIED., .F., .F.,
 ( 4, 4 ),
 ( 0.000000000000000000, 1.000000000000000000 ),
 .UNSPECIFIED. ) ;
#46581 = CARTESIAN_POINT ( 'NONE',  ( 11.11123293495519881, 3.108594079907299967, 7.535834283667469435 ) ) ;
#46582 = CARTESIAN_POINT ( 'NONE',  ( 10.00638553269999953, -5.119272496996000399, 8.420388242270998802 ) ) ;
#46583 = CARTESIAN_POINT ( 'NONE',  ( 10.13425461470299993, 3.159754091322399816, 7.286236678332599581 ) ) ;
#46584 = CARTESIAN_POINT ( 'NONE',  ( 23.51706668766000163, -2.929178272971999952, 13.82547084486999900 ) ) ;
#46585 = CARTESIAN_POINT ( 'NONE',  ( 10.81316193496000011, -3.756072284922999938, 6.071597915422999314 ) ) ;
#46587 = CARTESIAN_POINT ( 'NONE',  ( 25.44993529014200107, -2.258942858049999725, 12.29419282279000036 ) ) ;
#46586 = AXIS2_PLACEMENT_3D ( 'NONE', #34963, #12252, #2113 ) ;
#46588 = DIRECTION ( 'NONE',  ( 0.000000000000000000, 1.000000000000000000, 1.348567142399000110E-14 ) ) ;
#46589 = CARTESIAN_POINT ( 'NONE',  ( 23.55667344479600089, 3.263152516149000260, -13.70292389877999817 ) ) ;
#46590 = ORIENTED_EDGE ( 'NONE', *, *, #23357, .F. ) ;
#46591 = EDGE_CURVE ( 'NONE', #7896, #53136, #20026, .T. ) ;
#46592 = CARTESIAN_POINT ( 'NONE',  ( 4.558531403101000912, 1.112796118072999940, -0.2204328748767000190 ) ) ;
#46593 = CARTESIAN_POINT ( 'NONE',  ( 9.402671671056999969, -5.261543809652999393, -7.711876388024100137 ) ) ;
#46594 = CIRCLE ( 'NONE', #11944, 1.250000000000000000 ) ;
#46595 = CARTESIAN_POINT ( 'NONE',  ( 10.36409408021999923, -4.600000090830000943, -4.954046131267999087 ) ) ;
#46596 = CARTESIAN_POINT ( 'NONE',  ( 11.56456920625009843, -3.962850971080120299, 8.532838639935999225 ) ) ;
#46597 = EDGE_CURVE ( 'NONE', #5919, #23499, #29940, .T. ) ;
#46598 = CARTESIAN_POINT ( 'NONE',  ( 17.77951638133172452, 1.796077334879280896, -12.47133186514445313 ) ) ;
#46599 = CARTESIAN_POINT ( 'NONE',  ( 8.248383067018009385, -3.479335337562998731, -6.809779439446000282 ) ) ;
#46600 = CARTESIAN_POINT ( 'NONE',  ( 18.11819331236293706, 2.771443073929879208, 12.38417569151564734 ) ) ;
#46602 = CIRCLE ( 'NONE', #44364, 0.5000000000000001110 ) ;
#46601 = CARTESIAN_POINT ( 'NONE',  ( 12.22548351784790199, 2.734003476504523800, -13.62103941680929076 ) ) ;
#46603 = CARTESIAN_POINT ( 'NONE',  ( 9.311892889969000109, -5.494586520014999920, -6.370782351137999733 ) ) ;
#46604 = CARTESIAN_POINT ( 'NONE',  ( 10.15335805961999860, -3.144986649008000068, -5.860958514434000399 ) ) ;
#46605 = CARTESIAN_POINT ( 'NONE',  ( 23.66004879239100234, 3.393652551760000247, -13.50507492672999987 ) ) ;
#46606 = CARTESIAN_POINT ( 'NONE',  ( 12.53842061970401467, 0.6791475903684074389, -13.98351814429473094 ) ) ;
#46607 = CARTESIAN_POINT ( 'NONE',  ( 13.67059379716000045, -8.916337866955000635, -7.720150512555999711 ) ) ;
#46608 = CARTESIAN_POINT ( 'NONE',  ( 11.23052404082913291, -5.045680872279848295, -7.175009054135016662 ) ) ;
#46609 = CARTESIAN_POINT ( 'NONE',  ( 2.853056799211333594, -2.798833948393629534, -2.150913519912204031 ) ) ;
#46610 = CARTESIAN_POINT ( 'NONE',  ( 23.59999999999999787, -11.54195482626477798, -7.798368141167753897 ) ) ;
#46611 = CARTESIAN_POINT ( 'NONE',  ( 16.26901036074197648, 3.345264657739864145, 11.86070554647184316 ) ) ;
#46612 = ORIENTED_EDGE ( 'NONE', *, *, #9211, .F. ) ;
#46613 = CARTESIAN_POINT ( 'NONE',  ( 9.250458951833351762, -3.823380212705907777, -8.850046142581145858 ) ) ;
#46614 = CARTESIAN_POINT ( 'NONE',  ( 17.94045008455784185, 3.136494811772696067, -13.64413575143460911 ) ) ;
#46615 = ORIENTED_EDGE ( 'NONE', *, *, #13827, .T. ) ;
#46616 = CARTESIAN_POINT ( 'NONE',  ( 10.01002593514599859, -4.125890936441000356, 8.357822485499299958 ) ) ;
#46617 = CARTESIAN_POINT ( 'NONE',  ( 10.55569598648999907, 5.130952141044000214, 6.826612223887499553 ) ) ;
#46618 = CARTESIAN_POINT ( 'NONE',  ( 4.149992563291999836, -1.599290730647366932, -1.229060429538532562 ) ) ;
#46619 = CARTESIAN_POINT ( 'NONE',  ( 9.940137750233063230, 4.538038001511168318, -9.158081726654419441 ) ) ;
#46620 = CARTESIAN_POINT ( 'NONE',  ( 10.93990547754509812, -2.967013601007999934, -7.532784233952049213 ) ) ;
#46621 = CARTESIAN_POINT ( 'NONE',  ( 7.000000000000000000, 6.255435840762999966, 3.000000000000000000 ) ) ;
#46622 = CARTESIAN_POINT ( 'NONE',  ( 8.978248830702483474, -3.044910121894152333, -8.117373328463406423 ) ) ;
#46623 = VERTEX_POINT ( 'NONE', #30864 ) ;
#46624 = CARTESIAN_POINT ( 'NONE',  ( 10.08521345716899908, 4.924890298941200228, -8.340879262988799780 ) ) ;
#46625 = CARTESIAN_POINT ( 'NONE',  ( 9.485829719593997567, 4.953415418491999844, -8.946479654552000227 ) ) ;
#46626 = ORIENTED_EDGE ( 'NONE', *, *, #56853, .F. ) ;
#46627 = AXIS2_PLACEMENT_3D ( 'NONE', #37128, #63684, #31208 ) ;
#46628 = CARTESIAN_POINT ( 'NONE',  ( 10.36630583688000051, 5.852743870412999705, -7.568014644338999730 ) ) ;
#46629 = SURFACE_STYLE_USAGE ( .BOTH. , #25294 ) ;
#46630 = VERTEX_POINT ( 'NONE', #19685 ) ;
#46631 = CARTESIAN_POINT ( 'NONE',  ( 9.326684229509998758, 3.098260518542999886, 8.407331414124799451 ) ) ;
#46632 = CARTESIAN_POINT ( 'NONE',  ( 17.65155715295180627, -3.193702317672024282, -12.18853033496119842 ) ) ;
#46633 = PRODUCT_DEFINITION ( 'UNKNOWN', '', #3895, #31792 ) ;
#46634 = FACE_OUTER_BOUND ( 'NONE', #104, .T. ) ;
#46635 = B_SPLINE_CURVE_WITH_KNOTS ( 'NONE', 3,
 ( #38308, #22916, #17332, #53704, #33423, #54740 ),
 .UNSPECIFIED., .F., .F.,
 ( 4, 1, 1, 4 ),
 ( 0.0003621572724173774968, 0.3333333333333000081, 0.6666666666667000474, 1.000000000000000000 ),
 .UNSPECIFIED. ) ;
#46636 = AXIS2_PLACEMENT_3D ( 'NONE', #56889, #4075, #51297 ) ;
#46637 = CARTESIAN_POINT ( 'NONE',  ( 4.400023385887159577, -1.108947733447370521, -0.4820500775937197058 ) ) ;
#46638 = CARTESIAN_POINT ( 'NONE',  ( 11.07747771764000078, -8.037387346984001368, -6.930719685002999952 ) ) ;
#46639 = ORIENTED_EDGE ( 'NONE', *, *, #21218, .F. ) ;
#46640 = CARTESIAN_POINT ( 'NONE',  ( 8.020125753392001400, 4.498951069075999953, -6.245588651729999441 ) ) ;
#46641 = CARTESIAN_POINT ( 'NONE',  ( 7.249999999999997335, 4.000000000000000000, 9.109807621135335154 ) ) ;
#46642 = CARTESIAN_POINT ( 'NONE',  ( 11.79999999471800010, -3.216299622513999701, 11.40340969442000052 ) ) ;
#46643 = CYLINDRICAL_SURFACE ( 'NONE', #40555, 1.999999999999999556 ) ;
#46644 = CARTESIAN_POINT ( 'NONE',  ( 18.28003411566973213, 0.02431279293010887507, 13.99999914078079932 ) ) ;
#46645 = CARTESIAN_POINT ( 'NONE',  ( 18.18404792230800382, 3.205001206845999651, 11.25648540289999922 ) ) ;
#46646 = CARTESIAN_POINT ( 'NONE',  ( 10.13382174003999836, -5.176455793257000337, -8.189804425074999727 ) ) ;
#46647 = ORIENTED_EDGE ( 'NONE', *, *, #34974, .T. ) ;
#46648 = ORIENTED_EDGE ( 'NONE', *, *, #45404, .F. ) ;
#46649 = AXIS2_PLACEMENT_3D ( 'NONE', #28629, #44368, #34217 ) ;
#46650 = CARTESIAN_POINT ( 'NONE',  ( 9.318935841232999451, 2.644017913812000131, -7.838184857420000817 ) ) ;
#46651 = CYLINDRICAL_SURFACE ( 'NONE', #13308, 12.52500000000000036 ) ;
#46652 = CARTESIAN_POINT ( 'NONE',  ( 1.092640132541500053, 3.058252359239899132, 1.762666431298155034 ) ) ;
#46653 = CARTESIAN_POINT ( 'NONE',  ( 24.67326002361100024, 8.700705800976999527, -9.017089022949001276 ) ) ;
#46654 = EDGE_CURVE ( 'NONE', #9931, #47471, #9849, .T. ) ;
#46655 = ADVANCED_FACE ( 'NONE', ( #31551 ), #52871, .F. ) ;
#46656 = CARTESIAN_POINT ( 'NONE',  ( 24.32784158250700202, 9.023045772892999139, -9.340248004790000280 ) ) ;
#46657 = CARTESIAN_POINT ( 'NONE',  ( 18.38722619340700248, -3.117741388420999904, -11.18549237633000004 ) ) ;
#46659 = CARTESIAN_POINT ( 'NONE',  ( 1.284778341492999868E-07, -2.574999650349000024, 0.000000000000000000 ) ) ;
#46658 = CARTESIAN_POINT ( 'NONE',  ( 10.48429229006299934, -3.131390070940299974, 8.004340253666999416 ) ) ;
#46660 = CARTESIAN_POINT ( 'NONE',  ( 0.5181103717477000270, 3.205765437135000173, -1.404659375816999844 ) ) ;
#46661 = ORIENTED_EDGE ( 'NONE', *, *, #53745, .F. ) ;
#46662 = B_SPLINE_CURVE_WITH_KNOTS ( 'NONE', 3,
 ( #60168, #7715, #12970, #34984, #9082, #18207, #3824, #40902, #56300, #3152 ),
 .UNSPECIFIED., .F., .F.,
 ( 4, 2, 2, 2, 4 ),
 ( 0.000000000000000000, 0.1248149689018965974, 0.2496299378037931949, 0.3744449067056898062, 0.4992598756075863897 ),
 .UNSPECIFIED. ) ;
#46663 = CARTESIAN_POINT ( 'NONE',  ( 24.67921580316900076, -12.29514843751999997, 2.979196179828000002 ) ) ;
#46664 = CARTESIAN_POINT ( 'NONE',  ( 11.09999999999999964, -6.070676763699000666, 5.236526630994999820 ) ) ;
#46665 = CYLINDRICAL_SURFACE ( 'NONE', #60373, 5.000000000000000000 ) ;
#46666 = FACE_OUTER_BOUND ( 'NONE', #40354, .T. ) ;
#46667 = CYLINDRICAL_SURFACE ( 'NONE', #32117, 13.10000000000000142 ) ;
#46668 = CARTESIAN_POINT ( 'NONE',  ( 10.88033927340999973, -5.062718448322000242, 5.083949215177000269 ) ) ;
#46669 = CARTESIAN_POINT ( 'NONE',  ( 8.807788144226000426, 4.090932644426789722, 6.546538158064899804 ) ) ;
#46670 = CARTESIAN_POINT ( 'NONE',  ( 13.67488484168399943, 8.948943314763999624, 7.542122959438999352 ) ) ;
#46671 = DIRECTION ( 'NONE',  ( 0.000000000000000000, -1.000000000000000000, 0.000000000000000000 ) ) ;
#46672 = CARTESIAN_POINT ( 'NONE',  ( 5.908316242380999839, -0.7225053299333999979, -0.9279906512076999681 ) ) ;
#46673 = EDGE_CURVE ( 'NONE', #46748, #45774, #62185, .T. ) ;
#46674 = VECTOR ( 'NONE', #8067, 1000.000000000000000 ) ;
#46675 = CARTESIAN_POINT ( 'NONE',  ( 0.2483555794960837226, 2.598197151148166739, 1.995642445486431438 ) ) ;
#46676 = CARTESIAN_POINT ( 'NONE',  ( 3.396339116751999843, 1.123978401994000009, 3.059078227285999763 ) ) ;
#46677 = ORIENTED_EDGE ( 'NONE', *, *, #14470, .F. ) ;
#46678 = CARTESIAN_POINT ( 'NONE',  ( 12.33572460179970065, 0.5483668826291651088, -12.58806376549905082 ) ) ;
#46679 = CARTESIAN_POINT ( 'NONE',  ( 12.18009741656738854, -2.512104454550815991, -12.44873738066442925 ) ) ;
#46680 = DIRECTION ( 'NONE',  ( 0.000000000000000000, 1.000000000000000000, 0.000000000000000000 ) ) ;
#46682 = CARTESIAN_POINT ( 'NONE',  ( 3.499577856771284079, 0.2302043132029295003, -3.403026834754980356 ) ) ;
#46681 = VECTOR ( 'NONE', #65300, 1000.000000000000000 ) ;
#46683 = CARTESIAN_POINT ( 'NONE',  ( 1.634306799207666749, 1.762666431298139713, 3.058252359239908458 ) ) ;
#46684 = ORIENTED_EDGE ( 'NONE', *, *, #134, .F. ) ;
#46685 = CARTESIAN_POINT ( 'NONE',  ( 5.392306792578000163, -0.7698221690009998674, -0.8891327474049000035 ) ) ;
#46686 = APPLICATION_PROTOCOL_DEFINITION ( 'draft international standard', 'automotive_design', 1998, #25734 ) ;
#46687 = CARTESIAN_POINT ( 'NONE',  ( 0.7303395634860353480, -3.408546583648842887, 0.9194981686915635333 ) ) ;
#46688 = CARTESIAN_POINT ( 'NONE',  ( 10.91281046558188628, 5.099996679677031963, 5.078864286215828194 ) ) ;
#46689 = CARTESIAN_POINT ( 'NONE',  ( 10.05041772631199848, 4.549624259497900169, 6.368647051112000135 ) ) ;
#46690 = VECTOR ( 'NONE', #49944, 1000.000000000000114 ) ;
#46691 = CARTESIAN_POINT ( 'NONE',  ( 11.76588784977539781, 2.879134238109999799, -7.435950347916509884 ) ) ;
#46692 = VERTEX_POINT ( 'NONE', #38508 ) ;
#46693 = CARTESIAN_POINT ( 'NONE',  ( 10.76010362286999822, -4.535387425205000156, 6.001717576299999024 ) ) ;
#46694 = ORIENTED_EDGE ( 'NONE', *, *, #15247, .T. ) ;
#46695 = CARTESIAN_POINT ( 'NONE',  ( 21.60000000000000142, 0.000000000000000000, 0.000000000000000000 ) ) ;
#46696 = CARTESIAN_POINT ( 'NONE',  ( 8.814947692958833514, 2.650138447187985413, -7.499997389691697158 ) ) ;
#46697 = DIRECTION ( 'NONE',  ( 0.4384236320213994453, 0.6355252626312996034, -0.6355252626312994924 ) ) ;
#46698 = VERTEX_POINT ( 'NONE', #54236 ) ;
#46699 = CARTESIAN_POINT ( 'NONE',  ( 23.59644478421662583, 10.16908198660547846, 9.589309125383387311 ) ) ;
#46700 = CARTESIAN_POINT ( 'NONE',  ( 7.702599060372073758, 2.713167639879611848, 7.025738298870125575 ) ) ;
#46701 = CARTESIAN_POINT ( 'NONE',  ( 7.821420280405000369, 5.418947913204000599, -8.493927145653000110 ) ) ;
#46702 = DIRECTION ( 'NONE',  ( -1.000000000000000000, 0.000000000000000000, 0.000000000000000000 ) ) ;
#46703 = CARTESIAN_POINT ( 'NONE',  ( 10.21685100254000034, -2.832432432432000269, 6.822293592207000934 ) ) ;
#46704 = VERTEX_POINT ( 'NONE', #11580 ) ;
#46705 = CARTESIAN_POINT ( 'NONE',  ( 10.27814441345999974, -5.521593622715999850, 8.751220666652999469 ) ) ;
#46706 = CARTESIAN_POINT ( 'NONE',  ( 12.24260983038517914, -2.772891244653861609, -13.61173698548923028 ) ) ;
#46707 = FACE_OUTER_BOUND ( 'NONE', #1130, .T. ) ;
#46708 = VERTEX_POINT ( 'NONE', #16831 ) ;
#46709 = CARTESIAN_POINT ( 'NONE',  ( 9.976697000975999430, -4.172225768856000272, -6.147144998063999388 ) ) ;
#46710 = CARTESIAN_POINT ( 'NONE',  ( 9.332537864288001472, -2.899999999999999911, 6.571291218949999902 ) ) ;
#46711 = B_SPLINE_CURVE_WITH_KNOTS ( 'NONE', 3,
 ( #19275, #45853, #36388, #52116, #68532, #4221, #51777, #36041, #51099, #62272 ),
 .UNSPECIFIED., .F., .F.,
 ( 4, 2, 2, 2, 4 ),
 ( 0.000000000000000000, 0.2500000000000000000, 0.5000000000000000000, 0.7500000000000000000, 1.000000000000000000 ),
 .UNSPECIFIED. ) ;
#46712 = EDGE_LOOP ( 'NONE', ( #63974, #60589, #33036, #31481 ) ) ;
#46713 = CARTESIAN_POINT ( 'NONE',  ( 10.90184547699885087, 2.543465510515977357, 8.509880136748577684 ) ) ;
#46714 = CYLINDRICAL_SURFACE ( 'NONE', #12023, 0.6999999999999992895 ) ;
#46715 = EDGE_CURVE ( 'NONE', #59938, #18146, #8818, .T. ) ;
#46716 = CARTESIAN_POINT ( 'NONE',  ( 0.7000000000000000666, 0.000000000000000000, 0.5999999999999999778 ) ) ;
#46717 = CARTESIAN_POINT ( 'NONE',  ( 3.011390132543707576, 3.499999999999998224, 0.4581489286485194157 ) ) ;
#46718 = ADVANCED_FACE ( 'NONE', ( #59832 ), #923, .T. ) ;
#46719 = FACE_OUTER_BOUND ( 'NONE', #55408, .T. ) ;
#46720 = CARTESIAN_POINT ( 'NONE',  ( 18.13803896488302669, -2.274492816832912823, 12.50128160305151503 ) ) ;
#46721 = ORIENTED_EDGE ( 'NONE', *, *, #27930, .F. ) ;
#46722 = CARTESIAN_POINT ( 'NONE',  ( 7.634919074141999218, -4.860412626018001170, 6.427891721055999597 ) ) ;
#46723 = ORIENTED_EDGE ( 'NONE', *, *, #48260, .T. ) ;
#46724 = CARTESIAN_POINT ( 'NONE',  ( 10.73931450027999901, 2.763002390638999994, 6.801034082888999244 ) ) ;
#46725 = DIRECTION ( 'NONE',  ( 1.000000000000000000, 0.000000000000000000, 0.000000000000000000 ) ) ;
#46726 = CARTESIAN_POINT ( 'NONE',  ( 8.672510841228998402, 4.686731264770999772, -8.717075579553000608 ) ) ;
#46727 = CARTESIAN_POINT ( 'NONE',  ( 3.222503736606999958, -3.132127790629000152, -1.657619983915999740 ) ) ;
#46728 = CARTESIAN_POINT ( 'NONE',  ( 10.83767365324000131, -5.758089526411000136, -6.911472812823999945 ) ) ;
#46729 = CARTESIAN_POINT ( 'NONE',  ( 25.29987261392200182, 8.756202924575998026, -7.455126447192999883 ) ) ;
#46730 = CARTESIAN_POINT ( 'NONE',  ( 23.58312284468700071, 13.27301453609000070, 4.267237745444000474 ) ) ;
#46731 = VERTEX_POINT ( 'NONE', #64717 ) ;
#46732 = CARTESIAN_POINT ( 'NONE',  ( 11.31764560330029923, -3.650429500487800460, 8.585859374935999710 ) ) ;
#46733 = CARTESIAN_POINT ( 'NONE',  ( 9.383148997457999130, 5.167567567567999731, 6.822293592207000934 ) ) ;
#46734 = CYLINDRICAL_SURFACE ( 'NONE', #54986, 13.17499999999999893 ) ;
#46735 = ADVANCED_FACE ( 'NONE', ( #54594 ), #53558, .T. ) ;
#46736 = CARTESIAN_POINT ( 'NONE',  ( 5.000000001445999764, -1.799999998554000058, 4.283816198543999816E-09 ) ) ;
#46738 = CARTESIAN_POINT ( 'NONE',  ( 12.35713445931008359, 3.099811329670646209, -13.65268841750417650 ) ) ;
#46737 = CARTESIAN_POINT ( 'NONE',  ( 9.380783851237000093, 2.204242311415999911, 7.545378292079000460 ) ) ;
#46739 = CARTESIAN_POINT ( 'NONE',  ( 10.37872469555899890, 4.502158848185001006, -6.631215019384099740 ) ) ;
#46740 = EDGE_CURVE ( 'NONE', #27711, #12790, #20984, .T. ) ;
#46741 = CARTESIAN_POINT ( 'NONE',  ( 8.710288521113000115, -4.352953559891299840, -8.284550957747498501 ) ) ;
#46743 = AXIS2_PLACEMENT_3D ( 'NONE', #17830, #12579, #33909 ) ;
#46742 = CARTESIAN_POINT ( 'NONE',  ( 9.298392757686999133, 4.585219941293100732, -8.139707405630899117 ) ) ;
#46744 = CARTESIAN_POINT ( 'NONE',  ( 18.26841343935701190, -0.1288995356414823490, 12.59934597632939912 ) ) ;
#46745 = CARTESIAN_POINT ( 'NONE',  ( 6.902955114085999710, 1.212008421426999938, 0.9737989909727998716 ) ) ;
#46746 = CARTESIAN_POINT ( 'NONE',  ( 11.38678751119029897, 2.833702563575000166, 6.889827023674499173 ) ) ;
#46747 = CARTESIAN_POINT ( 'NONE',  ( 23.61702365891200373, 10.26369571899999933, 9.293522352232999495 ) ) ;
#46748 = VERTEX_POINT ( 'NONE', #6690 ) ;
#46749 = CARTESIAN_POINT ( 'NONE',  ( 8.283081853209001366, -2.376522687267000222, 7.686981355459999499 ) ) ;
#46750 = CARTESIAN_POINT ( 'NONE',  ( 3.999999999999999112, 1.082950885222931925, -1.878608423871279465 ) ) ;
#46751 = CARTESIAN_POINT ( 'NONE',  ( 7.761038909107502271, -3.347566356579097846, 6.284495591795857372 ) ) ;
#46752 = VERTEX_POINT ( 'NONE', #37819 ) ;
#46753 = CIRCLE ( 'NONE', #24449, 0.5000000000000002220 ) ;
#46754 = CARTESIAN_POINT ( 'NONE',  ( 0.6089841414396000019, -0.7435038563603999506, -3.122230671987999973 ) ) ;
#46755 = EDGE_CURVE ( 'NONE', #34355, #65484, #60063, .T. ) ;
#46756 = CARTESIAN_POINT ( 'NONE',  ( 11.35545123989519922, 4.475221369382300196, 6.582230774881299595 ) ) ;
#46757 = CARTESIAN_POINT ( 'NONE',  ( 10.90247028041000021, 4.554785930130000438, -6.081876607904999510 ) ) ;
#46758 = ORIENTED_EDGE ( 'NONE', *, *, #10957, .F. ) ;
#46759 = CARTESIAN_POINT ( 'NONE',  ( 11.79999999523987420, 3.306280043674564517, -11.23952258183352093 ) ) ;
#46760 = CARTESIAN_POINT ( 'NONE',  ( 24.30000000000000071, 3.224868684338999980, -12.03537377768999939 ) ) ;
#46761 = CARTESIAN_POINT ( 'NONE',  ( 10.91195257254739914, 2.772832764353999835, 7.143100915737699452 ) ) ;
#46762 = CARTESIAN_POINT ( 'NONE',  ( 7.955378155590884681, -4.974460548466400844, 6.453583785422088326 ) ) ;
#46763 = CARTESIAN_POINT ( 'NONE',  ( 7.565635841228000480, 3.206360348473000332, 5.681727837477000165 ) ) ;
#46764 = ORIENTED_EDGE ( 'NONE', *, *, #15312, .F. ) ;
#46765 = CARTESIAN_POINT ( 'NONE',  ( 7.834599687276918800, -4.856173268066945603, 6.415412167053935910 ) ) ;
#46766 = CARTESIAN_POINT ( 'NONE',  ( 7.318264158767999739, 5.899473592675000155, -7.539390303202999633 ) ) ;
#46767 = CARTESIAN_POINT ( 'NONE',  ( 8.251176002667504505, -5.392147303917279366, 8.543946155412404764 ) ) ;
#46768 = CARTESIAN_POINT ( 'NONE',  ( 10.25727973160899964, -3.885210315895800015, 8.774051692788999546 ) ) ;
#46769 = ORIENTED_EDGE ( 'NONE', *, *, #15011, .T. ) ;
#46770 = CARTESIAN_POINT ( 'NONE',  ( 2.761390132542709264, -3.499999999999999556, -0.4581489286485119772 ) ) ;
#46771 = CARTESIAN_POINT ( 'NONE',  ( 11.38733729122639993, -5.277570687708000641, 7.533608309972310124 ) ) ;
#46772 = ORIENTED_EDGE ( 'NONE', *, *, #65040, .F. ) ;
#46773 = LINE ( 'NONE', #57247, #66344 ) ;
#46774 = VERTEX_POINT ( 'NONE', #22075 ) ;
#46775 = LINE ( 'NONE', #20888, #8549 ) ;
#46776 = CARTESIAN_POINT ( 'NONE',  ( 10.76951263900000022, -2.736336172232000319, -4.838784512614000555 ) ) ;
#46777 = CIRCLE ( 'NONE', #6435, 1.550000000000000488 ) ;
#46778 = CARTESIAN_POINT ( 'NONE',  ( 10.52799293566599914, 4.806678152079100208, -8.489570425681801424 ) ) ;
#46779 = CARTESIAN_POINT ( 'NONE',  ( 11.67901463001530082, -3.302889347096799710, 8.616511311517999872 ) ) ;
#46780 = CARTESIAN_POINT ( 'NONE',  ( 12.49885887340285961, 1.955044097548213733, -12.56200003178136448 ) ) ;
#46781 = CARTESIAN_POINT ( 'NONE',  ( 11.19456919669529960, -2.906008650422999828, 7.176777099639999768 ) ) ;
#46782 = CARTESIAN_POINT ( 'NONE',  ( 7.795982780410000146, 3.164805384346000228, 9.104735843897000080 ) ) ;
#46783 = ORIENTED_EDGE ( 'NONE', *, *, #22917, .T. ) ;
#46784 = DIRECTION ( 'NONE',  ( 1.000000000000000000, 0.000000000000000000, 0.000000000000000000 ) ) ;
#46785 = CARTESIAN_POINT ( 'NONE',  ( 7.775620559622000272, -4.636725880537000855, 9.378965771357000492 ) ) ;
#46786 = CARTESIAN_POINT ( 'NONE',  ( 9.916846873516377059, 3.231816600031355069, 6.500416447002274722 ) ) ;
#46787 = ORIENTED_EDGE ( 'NONE', *, *, #11585, .F. ) ;
#46788 = CARTESIAN_POINT ( 'NONE',  ( 12.66194203315991906, -3.108482559131308332, -12.28874639354599374 ) ) ;
#46789 = CARTESIAN_POINT ( 'NONE',  ( 10.52226222744799955, 3.119510978356100139, 6.774721295617600170 ) ) ;
#46790 = CARTESIAN_POINT ( 'NONE',  ( 10.20608185320999972, -2.622355301673999772, -6.528538675937999969 ) ) ;
#46791 = CARTESIAN_POINT ( 'NONE',  ( 10.44065171787999802, 8.381973494822000603, -6.833921068867995885 ) ) ;
#46792 = CARTESIAN_POINT ( 'NONE',  ( 18.12310803393399894, -3.320912951897000198, -11.92519506916999994 ) ) ;
#46793 = EDGE_CURVE ( 'NONE', #49400, #4446, #52144, .T. ) ;
#46794 = LINE ( 'NONE', #31403, #40851 ) ;
#46795 = CARTESIAN_POINT ( 'NONE',  ( 12.38032181885351513, -3.110191202103278485, -13.65016103957348825 ) ) ;
#46796 = EDGE_CURVE ( 'NONE', #31999, #46284, #521, .T. ) ;
#46797 = CARTESIAN_POINT ( 'NONE',  ( 11.70794988689359961, -3.544213289744700290, -8.393984925606600811 ) ) ;
#46798 = CARTESIAN_POINT ( 'NONE',  ( 11.16486084871730000, 5.207010770456999893, 7.825000000000000178 ) ) ;
#46799 = EDGE_CURVE ( 'NONE', #36266, #28289, #36303, .T. ) ;
#46800 = CARTESIAN_POINT ( 'NONE',  ( 11.12299956498149811, -2.792989229543000107, -7.825000000000000178 ) ) ;
#46801 = ORIENTED_EDGE ( 'NONE', *, *, #39850, .F. ) ;
#46802 = ORIENTED_EDGE ( 'NONE', *, *, #64638, .T. ) ;
#46803 = CARTESIAN_POINT ( 'NONE',  ( 21.10000033274619824, 12.52499966719000035, 3.709620195857000057E-10 ) ) ;
#46804 = CARTESIAN_POINT ( 'NONE',  ( 19.94999927679900154, 1.497292381259999763E-13, 3.463895836829999943E-14 ) ) ;
#46805 = CARTESIAN_POINT ( 'NONE',  ( 18.10300909156940818, 2.800751615046049192, 13.60500513795867583 ) ) ;
#46806 = CARTESIAN_POINT ( 'NONE',  ( 10.53865537815000053, 3.647234352455999584, -6.014129666051999834 ) ) ;
#46807 = DIRECTION ( 'NONE',  ( -1.000000000000000000, 0.000000000000000000, 0.000000000000000000 ) ) ;
#46808 = CARTESIAN_POINT ( 'NONE',  ( 17.93780763597375483, 2.994506166037827377, 12.32249531978309243 ) ) ;
#46809 = CARTESIAN_POINT ( 'NONE',  ( 23.55340715333399970, -13.38991586735000183, 4.199558039904999873 ) ) ;
#46810 = CARTESIAN_POINT ( 'NONE',  ( 9.290193290418001126, 2.377818438998999806, 7.540992072119000689 ) ) ;
#46811 = ORIENTED_EDGE ( 'NONE', *, *, #29031, .T. ) ;
#46812 = CARTESIAN_POINT ( 'NONE',  ( 8.979535623375799247, 3.684598859393744430, -9.248984133260908180 ) ) ;
#46813 = EDGE_LOOP ( 'NONE', ( #68509, #21754, #32235, #15283 ) ) ;
#46814 = CARTESIAN_POINT ( 'NONE',  ( 12.78418516728952703, -3.124999463064650929, 12.28374650604039786 ) ) ;
#46815 = B_SPLINE_CURVE_WITH_KNOTS ( 'NONE', 3,
 ( #60330, #5796, #33073, #39011, #55083, #27836, #7189, #37962 ),
 .UNSPECIFIED., .F., .F.,
 ( 4, 2, 2, 4 ),
 ( 0.000000000000000000, 0.1251850562541942935, 0.2503701125083885870, 0.5007402250167770630 ),
 .UNSPECIFIED. ) ;
#46816 = CARTESIAN_POINT ( 'NONE',  ( 8.630000000000000782, 4.924138593003999809, -8.484107647018999998 ) ) ;
#46817 = CARTESIAN_POINT ( 'NONE',  ( 9.842764158772000727, 5.798263352390999437, -8.113145944980999502 ) ) ;
#46818 = CARTESIAN_POINT ( 'NONE',  ( 11.89189666366029918, -4.052152326617509459, 6.326270943800999191 ) ) ;
#46819 = CARTESIAN_POINT ( 'NONE',  ( 7.278633126552175980, -0.8622146015440113054, 0.7572888212223023441 ) ) ;
#46820 = FACE_OUTER_BOUND ( 'NONE', #15679, .T. ) ;
#46821 = B_SPLINE_CURVE_WITH_KNOTS ( 'NONE', 3,
 ( #16355, #59014, #11117, #64925 ),
 .UNSPECIFIED., .F., .F.,
 ( 4, 4 ),
 ( 0.8745530004746001618, 1.000000000000000000 ),
 .UNSPECIFIED. ) ;
#46822 = CARTESIAN_POINT ( 'NONE',  ( 10.05041772631199848, 4.549624259497900169, -8.631352948887998977 ) ) ;
#46823 = CARTESIAN_POINT ( 'NONE',  ( 12.78441639972302113, -0.6247443594537136491, 12.67930618256805886 ) ) ;
#46824 = B_SPLINE_CURVE_WITH_KNOTS ( 'NONE', 3,
 ( #3967, #47671, #68630, #20751 ),
 .UNSPECIFIED., .F., .F.,
 ( 4, 4 ),
 ( 0.000000000000000000, 1.000000000000000000 ),
 .UNSPECIFIED. ) ;
#46825 = CARTESIAN_POINT ( 'NONE',  ( 11.60000000000000142, 3.310169951859694315, -8.238968815098687060 ) ) ;
#46826 = CARTESIAN_POINT ( 'NONE',  ( 11.08992526467999973, 5.210543602612999869, 8.327598319864998544 ) ) ;
#46827 = CARTESIAN_POINT ( 'NONE',  ( 11.35562122949000141, -3.716778816705999855, 11.19591510979999960 ) ) ;
#46828 = ORIENTED_EDGE ( 'NONE', *, *, #47663, .T. ) ;
#46829 = CARTESIAN_POINT ( 'NONE',  ( 8.938854719593997800, 5.597201461420000967, -8.171008079894999554 ) ) ;
#46830 = CARTESIAN_POINT ( 'NONE',  ( 7.492862293499999993, -1.342370813310000077, 0.5333876762063000099 ) ) ;
#46831 = CARTESIAN_POINT ( 'NONE',  ( 17.57587252603347494, 1.875000554927097607, 13.78627161177572624 ) ) ;
#46832 = CARTESIAN_POINT ( 'NONE',  ( 25.30000327618300204, -10.83443035398000021, 3.855530949778000149 ) ) ;
#46833 = CARTESIAN_POINT ( 'NONE',  ( 24.66708179685990743, 8.738412505656103946, 9.169048259976223747 ) ) ;
#46834 = CARTESIAN_POINT ( 'NONE',  ( 10.28441772631199846, -3.627481539113199815, -8.266796319406900295 ) ) ;
#46835 = ORIENTED_EDGE ( 'NONE', *, *, #61960, .F. ) ;
#46836 = CARTESIAN_POINT ( 'NONE',  ( 2.392611958083999735, -0.3183524953527000489, -3.745328979271999703 ) ) ;
#46837 = CARTESIAN_POINT ( 'NONE',  ( 18.17180710801086008, -0.1030387082853383846, -12.69945707558994563 ) ) ;
#46838 = EDGE_CURVE ( 'NONE', #42806, #32174, #59708, .T. ) ;
#46840 = FACE_OUTER_BOUND ( 'NONE', #12196, .T. ) ;
#46839 = CARTESIAN_POINT ( 'NONE',  ( 9.760001502711011412, 5.278381895807264357, 8.694223062418139136 ) ) ;
#46841 = CARTESIAN_POINT ( 'NONE',  ( 1.593676744644999875E-07, -2.574999840614999425, -3.034235117293000092E-10 ) ) ;
#46842 = VERTEX_POINT ( 'NONE', #49341 ) ;
#46843 = FACE_OUTER_BOUND ( 'NONE', #31607, .T. ) ;
#46844 = EDGE_CURVE ( 'NONE', #15133, #18184, #14643, .T. ) ;
#46845 = CARTESIAN_POINT ( 'NONE',  ( 18.14812703077573275, -2.302545424703879462, -13.71331074879213219 ) ) ;
#46846 = CARTESIAN_POINT ( 'NONE',  ( 11.26902897915239876, 4.221721321201099997, 6.662660017635100296 ) ) ;
#46847 = DIRECTION ( 'NONE',  ( -1.000000000000000000, 0.000000000000000000, 0.000000000000000000 ) ) ;
#46848 = CARTESIAN_POINT ( 'NONE',  ( 7.346668146792000087, -2.374041291348000016, 8.293390875797999939 ) ) ;
#46849 = ORIENTED_EDGE ( 'NONE', *, *, #40724, .F. ) ;
#46850 = CARTESIAN_POINT ( 'NONE',  ( 9.694277465284496742, -4.746637270850415646, -8.655944162059842739 ) ) ;
#46852 = CARTESIAN_POINT ( 'NONE',  ( 10.39297979613035317, 2.713506317168391302, -7.026950959993602197 ) ) ;
#46851 = CARTESIAN_POINT ( 'NONE',  ( 13.70003001321900449, 11.73562684670656431, 4.491863874615371621 ) ) ;
#46853 = VECTOR ( 'NONE', #57493, 1000.000000000000114 ) ;
#46854 = CARTESIAN_POINT ( 'NONE',  ( 7.474209973045660149, -2.340228481589814002, 6.977344112086323769 ) ) ;
#46855 = CARTESIAN_POINT ( 'NONE',  ( 27.64127793187000037, -1.199999999999999956, 9.776630298829998011 ) ) ;
#46856 = CARTESIAN_POINT ( 'NONE',  ( 24.03127928945400171, 3.727176143476999659, 13.01575025216999926 ) ) ;
#46857 = ORIENTED_EDGE ( 'NONE', *, *, #50434, .T. ) ;
#46858 = CARTESIAN_POINT ( 'NONE',  ( 1.286366951365282674, 3.276871974290374467, 0.4130264870479211647 ) ) ;
#46859 = CARTESIAN_POINT ( 'NONE',  ( 11.74025954179439957, -3.228187097503200320, 6.858707791728399172 ) ) ;
#46860 = CARTESIAN_POINT ( 'NONE',  ( 9.471374412057000924, 2.030666183831999927, 7.549764512038000142 ) ) ;
#46861 = CARTESIAN_POINT ( 'NONE',  ( 10.85646369190733473, 5.100000000000000533, 6.665341197409740737 ) ) ;
#46862 = CARTESIAN_POINT ( 'NONE',  ( 10.71918447801630059, 5.140463864104999558, 7.525145395936648995 ) ) ;
#46863 = CARTESIAN_POINT ( 'NONE',  ( 9.765375278055641317, 5.100000000000000533, 6.445686799077642526 ) ) ;
#46864 = DIRECTION ( 'NONE',  ( 0.000000000000000000, 0.000000000000000000, 1.000000000000000000 ) ) ;
#46865 = CARTESIAN_POINT ( 'NONE',  ( 10.98478522172274907, -5.203339783596914181, 6.694122711083909216 ) ) ;
#46866 = CARTESIAN_POINT ( 'NONE',  ( 17.55505043854147118, -2.500000000000000000, -25.00000000000000000 ) ) ;
#46867 = CARTESIAN_POINT ( 'NONE',  ( 24.33654850364300160, -12.30574143627999995, -3.219652787269999816 ) ) ;
#46868 = CARTESIAN_POINT ( 'NONE',  ( 9.099999886593998610, 12.39999890530000037, 0.000000000000000000 ) ) ;
#46869 = ORIENTED_EDGE ( 'NONE', *, *, #48099, .T. ) ;
#46870 = CARTESIAN_POINT ( 'NONE',  ( 16.08259915475489166, -9.118254932978855365, -8.587227412616224242 ) ) ;
#46871 = CARTESIAN_POINT ( 'NONE',  ( 23.57776922997304681, 13.28350420490069617, 4.287209407939693406 ) ) ;
#46872 = ORIENTED_EDGE ( 'NONE', *, *, #29251, .T. ) ;
#46873 = CARTESIAN_POINT ( 'NONE',  ( 1.849999551004999798, 0.000000000000000000, 0.000000000000000000 ) ) ;
#46874 = CARTESIAN_POINT ( 'NONE',  ( 10.60441638348510018, 3.158410350011299883, 7.705001100909899314 ) ) ;
#46875 = CARTESIAN_POINT ( 'NONE',  ( 9.786671076420999427, 2.381202181614999525, 7.612749448318000489 ) ) ;
#46876 = CARTESIAN_POINT ( 'NONE',  ( 11.02205778663999958, 2.309481324353999554, -7.515673747780000191 ) ) ;
#46877 = CARTESIAN_POINT ( 'NONE',  ( 9.125583543129625497, -4.871885936991885657, -7.573124426811684629 ) ) ;
#46878 = CARTESIAN_POINT ( 'NONE',  ( 9.848253563160000112, -4.436921580929999998, 6.148020168057000134 ) ) ;
#46879 = EDGE_CURVE ( 'NONE', #13082, #48412, #7953, .T. ) ;
#46880 = CARTESIAN_POINT ( 'NONE',  ( 18.18297319953442681, 0.3597466176220722178, -12.59486741915706531 ) ) ;
#46881 = CARTESIAN_POINT ( 'NONE',  ( 12.64175205088856657, 3.104634757609924467, -12.28992885563447146 ) ) ;
#46882 = CARTESIAN_POINT ( 'NONE',  ( 11.70379573085659786, -2.893744357957000357, -7.691418046581699919 ) ) ;
#46883 = EDGE_CURVE ( 'NONE', #50331, #47262, #68983, .T. ) ;
#46884 = EDGE_CURVE ( 'NONE', #5820, #38087, #41388, .T. ) ;
#46885 = CARTESIAN_POINT ( 'NONE',  ( 10.90076029995999995, -5.100000000044000892, -5.152573207167999492 ) ) ;
#46886 = VERTEX_POINT ( 'NONE', #49694 ) ;
#46887 =( NAMED_UNIT ( * ) PLANE_ANGLE_UNIT ( ) SI_UNIT ( $, .RADIAN. ) );
#46888 = CARTESIAN_POINT ( 'NONE',  ( 7.000000000000000000, -9.370210309074998634, -5.370210309075000410 ) ) ;
#46889 = DIRECTION ( 'NONE',  ( 0.4384236320214023874, 0.000000000000000000, -0.8987684456439055669 ) ) ;
#46890 = CARTESIAN_POINT ( 'NONE',  ( 10.31059687351633158, -4.629523725463621453, -6.407767014557176566 ) ) ;
#46891 = CARTESIAN_POINT ( 'NONE',  ( 6.607274140103999827, 9.225079388580999407, 5.032532138881999018 ) ) ;
#46892 = CARTESIAN_POINT ( 'NONE',  ( 12.08550557360779365, 2.425787521189699980, 13.78826042901831528 ) ) ;
#46893 = CARTESIAN_POINT ( 'NONE',  ( 10.07771285905000092, -4.622037501707999319, 5.671359981946999973 ) ) ;
#46894 = CARTESIAN_POINT ( 'NONE',  ( 9.112942518363999156, -5.100000000000000533, 6.192000867487999827 ) ) ;
#46895 = B_SPLINE_CURVE_WITH_KNOTS ( 'NONE', 3,
 ( #59686, #43620, #18081, #17740 ),
 .UNSPECIFIED., .F., .F.,
 ( 4, 4 ),
 ( 0.000000000000000000, 1.000000000000000000 ),
 .UNSPECIFIED. ) ;
#46896 = CARTESIAN_POINT ( 'NONE',  ( 12.08032335320031159, 0.02332822437943948488, 13.99998565365491210 ) ) ;
#46897 = EDGE_LOOP ( 'NONE', ( #23157, #26283, #63868, #44915 ) ) ;
#46898 = CARTESIAN_POINT ( 'NONE',  ( 12.18347802452938211, -2.109676230065137936, 12.42212916133884981 ) ) ;
#46899 = LINE ( 'NONE', #9829, #19197 ) ;
#46900 = EDGE_CURVE ( 'NONE', #8563, #56058, #39907, .T. ) ;
#46901 = CIRCLE ( 'NONE', #59208, 1.299999999999999822 ) ;
#46902 = CARTESIAN_POINT ( 'NONE',  ( 10.53138988903999973, -5.607755226963999640, 7.280101849877000042 ) ) ;
#46903 = CARTESIAN_POINT ( 'NONE',  ( 10.76059687351620475, -4.629523725463621453, -6.407767014557177454 ) ) ;
#46904 = CARTESIAN_POINT ( 'NONE',  ( 11.27672335273219950, -3.698477709264200275, 6.687976048055599421 ) ) ;
#46905 = CARTESIAN_POINT ( 'NONE',  ( 10.07309687351575178, 5.217465845835396188, -7.827184855449103473 ) ) ;
#46906 = CARTESIAN_POINT ( 'NONE',  ( 5.000000000000000000, -10.75000000000000000, 0.000000000000000000 ) ) ;
#46907 = ADVANCED_BREP_SHAPE_REPRESENTATION ( '', ( #31875, #9676 ), #21760 ) ;
#46908 = CARTESIAN_POINT ( 'NONE',  ( 11.20158531382784162, 4.272452942476327564, 8.749999999999998224 ) ) ;
#46909 = CARTESIAN_POINT ( 'NONE',  ( 12.09756245983758127, 2.320968861236844649, 12.38441143973091485 ) ) ;
#46910 = CARTESIAN_POINT ( 'NONE',  ( 9.355894592352999695, -5.864995026133001055, -7.324074232821000230 ) ) ;
#46911 = CARTESIAN_POINT ( 'NONE',  ( 10.23103300763299828, 4.692441239783899931, -8.226274395107198600 ) ) ;
#46912 = DIRECTION ( 'NONE',  ( -1.000000000000000000, 0.000000000000000000, 0.000000000000000000 ) ) ;
#46913 = CARTESIAN_POINT ( 'NONE',  ( 10.28180471959000108, 3.991526675591000384, -5.814300410279999554 ) ) ;
#46914 = CARTESIAN_POINT ( 'NONE',  ( 9.782608878791998919, 3.710311786319799854, -6.254020414961999563 ) ) ;
#46916 = CARTESIAN_POINT ( 'NONE',  ( 12.23322259332536355, 2.246983130377972149, 12.50693187469323497 ) ) ;
#46915 = CARTESIAN_POINT ( 'NONE',  ( 15.39325612864500137, -8.820489328074000213, -7.691617095226000345 ) ) ;
#46917 = CARTESIAN_POINT ( 'NONE',  ( 8.002383708823000319, 5.117451078405999887, -6.702236199791999915 ) ) ;
#46918 = ORIENTED_EDGE ( 'NONE', *, *, #48078, .T. ) ;
#46919 = CARTESIAN_POINT ( 'NONE',  ( 12.33180295219017353, -0.4082649239379795847, 12.69116688080143618 ) ) ;
#46920 = PLANE ( 'NONE',  #3212 ) ;
#46921 = ADVANCED_FACE ( 'NONE', ( #61564 ), #45149, .T. ) ;
#46922 = CARTESIAN_POINT ( 'NONE',  ( 9.820206362952999868, -3.883324525498000224, 6.055606607331999847 ) ) ;
#46923 = CARTESIAN_POINT ( 'NONE',  ( 8.793822372493998785, 3.711294259598199918, 6.555546982591299532 ) ) ;
#46924 = CYLINDRICAL_SURFACE ( 'NONE', #68213, 1.350000000000000533 ) ;
#46925 = CARTESIAN_POINT ( 'NONE',  ( 23.66004879239100234, -3.393652723963000106, -13.50507488346000073 ) ) ;
#46926 = EDGE_CURVE ( 'NONE', #9447, #21198, #35576, .T. ) ;
#46927 = CARTESIAN_POINT ( 'NONE',  ( 12.70235978774141294, -3.116847232384803323, 13.52309701207074966 ) ) ;
#46928 = CARTESIAN_POINT ( 'NONE',  ( 23.56695615185851977, -3.042046339845886127, 13.65547877525810350 ) ) ;
#46929 = CARTESIAN_POINT ( 'NONE',  ( 23.73686952991999988, 3.437738207072000396, -13.35009212917000099 ) ) ;
#46930 = ORIENTED_EDGE ( 'NONE', *, *, #6212, .T. ) ;
#46931 = CARTESIAN_POINT ( 'NONE',  ( 4.876954876535999794, -1.207493506464999866, 0.4107732707878000156 ) ) ;
#46932 = B_SPLINE_CURVE_WITH_KNOTS ( 'NONE', 3,
 ( #51967, #36588, #25406, #46741 ),
 .UNSPECIFIED., .F., .F.,
 ( 4, 4 ),
 ( 0.1836163425310833319, 1.000000000000000000 ),
 .UNSPECIFIED. ) ;
#46933 = CARTESIAN_POINT ( 'NONE',  ( 9.579975701332999805, -3.061513547538400104, -8.369268408503399925 ) ) ;
#46934 = FACE_OUTER_BOUND ( 'NONE', #56749, .T. ) ;
#46935 = CARTESIAN_POINT ( 'NONE',  ( 11.40346005378009941, -3.213042707518099839, 7.920222357891399945 ) ) ;
#46936 = CARTESIAN_POINT ( 'NONE',  ( 17.74784205817676863, 3.094544633123687216, -12.29297002796977800 ) ) ;
#46937 = CARTESIAN_POINT ( 'NONE',  ( 8.908091524193990196, -3.442323470413000575, -6.178118798475003004 ) ) ;
#46938 = CARTESIAN_POINT ( 'NONE',  ( 18.14655301447361779, 2.701944876897162562, 12.40222020712343998 ) ) ;
#46939 = CARTESIAN_POINT ( 'NONE',  ( 12.18578014164085488, 2.585505937877283333, -13.65496065469440268 ) ) ;
#46940 = DIRECTION ( 'NONE',  ( 0.000000000000000000, -1.000000000000000000, 0.000000000000000000 ) ) ;
#46941 = CARTESIAN_POINT ( 'NONE',  ( 10.30480805961999913, -5.828319785709999756, -7.226592660401000678 ) ) ;
#46942 = CARTESIAN_POINT ( 'NONE',  ( 11.09999999999999964, -4.000000000000000000, 7.500000000000000000 ) ) ;
#46943 = DIRECTION ( 'NONE',  ( -1.000000000000000000, 0.000000000000000000, 0.000000000000000000 ) ) ;
#46944 = FACE_OUTER_BOUND ( 'NONE', #9464, .T. ) ;
#46945 = CARTESIAN_POINT ( 'NONE',  ( 11.59610237318921477, 3.189590050595149773, 7.825049231485562196 ) ) ;
#46946 = CARTESIAN_POINT ( 'NONE',  ( 18.17956732773302164, 2.474903466559772891, 12.45737214977695828 ) ) ;
#46947 = ORIENTED_EDGE ( 'NONE', *, *, #37551, .F. ) ;
#46948 = CARTESIAN_POINT ( 'NONE',  ( 9.740360841231000322, 4.047146749018000200, -5.600703114891000034 ) ) ;
#46949 = CARTESIAN_POINT ( 'NONE',  ( 11.49826088462129903, -3.998156935320088756, 8.366195817038299509 ) ) ;
#46950 = VERTEX_POINT ( 'NONE', #5495 ) ;
#46951 = B_SPLINE_CURVE_WITH_KNOTS ( 'NONE', 3,
 ( #1236, #55065, #1930, #45273 ),
 .UNSPECIFIED., .F., .F.,
 ( 4, 4 ),
 ( 0.000000000000000000, 1.000000000000000000 ),
 .UNSPECIFIED. ) ;
#46952 = CARTESIAN_POINT ( 'NONE',  ( 13.17784398560650061, 12.38705052588331590, 1.853828488290521159 ) ) ;
#46953 = CARTESIAN_POINT ( 'NONE',  ( 17.97013316094029989, 1.919230625394029888, -13.86782606946093743 ) ) ;
#46954 = ORIENTED_EDGE ( 'NONE', *, *, #5982, .T. ) ;
#46955 = CARTESIAN_POINT ( 'NONE',  ( 10.28864655415099882, -3.580250267348600079, 6.741370903243699253 ) ) ;
#46956 = CARTESIAN_POINT ( 'NONE',  ( 11.55811496860034815, 5.045590851977999947, 8.035816473382100256 ) ) ;
#46957 = CARTESIAN_POINT ( 'NONE',  ( 9.740360841231000322, 4.047146749018000200, -5.600703114891000034 ) ) ;
#46958 = B_SPLINE_CURVE_WITH_KNOTS ( 'NONE', 3,
 ( #36227, #41134, #37259, #68369, #9994 ),
 .UNSPECIFIED., .F., .F.,
 ( 4, 1, 4 ),
 ( 0.000000000000000000, 0.5000000000000000000, 1.000000000000000000 ),
 .UNSPECIFIED. ) ;
#46959 = DIRECTION ( 'NONE',  ( -0.000000000000000000, -0.000000000000000000, 1.000000000000000000 ) ) ;
#46960 = CARTESIAN_POINT ( 'NONE',  ( 10.82035090130999855, -3.241273085157000189, -7.969278253227299658 ) ) ;
#46961 = DIRECTION ( 'NONE',  ( 1.000000000000000000, 0.000000000000000000, 0.000000000000000000 ) ) ;
#46962 = CARTESIAN_POINT ( 'NONE',  ( 24.30000000000000071, -2.078227429405999693, -11.31065739696999906 ) ) ;
#46963 = VERTEX_POINT ( 'NONE', #36976 ) ;
#46964 = CARTESIAN_POINT ( 'NONE',  ( 8.045639775557999585, 4.604250840901999986, -6.230858151876000228 ) ) ;
#46965 = ADVANCED_FACE ( 'NONE', ( #61907 ), #3168, .T. ) ;
#46966 = CARTESIAN_POINT ( 'NONE',  ( 10.07367028041000090, 4.905765359186999852, -8.776126235875999271 ) ) ;
#46967 = VERTEX_POINT ( 'NONE', #58632 ) ;
#46968 = CARTESIAN_POINT ( 'NONE',  ( 10.07930935222999835, 2.718121894972999719, -6.397795030233000446 ) ) ;
#46969 = PRESENTATION_STYLE_ASSIGNMENT (( #9203 ) ) ;
#46970 = ORIENTED_EDGE ( 'NONE', *, *, #60528, .T. ) ;
#46971 = CARTESIAN_POINT ( 'NONE',  ( 9.909254614703000286, 2.760277452415999644, 7.184607557167700165 ) ) ;
#46972 = CARTESIAN_POINT ( 'NONE',  ( 17.55505043854147118, -1.875000000000000000, -12.57541666120756041 ) ) ;
#46973 = DIRECTION ( 'NONE',  ( 0.000000000000000000, 1.000000000000000000, 0.000000000000000000 ) ) ;
#46974 = B_SPLINE_CURVE_WITH_KNOTS ( 'NONE', 3,
 ( #21409, #27704, #10924, #5331, #22095, #4989, #53577, #36817, #31571, #5670, #27011, #64388, #54255, #49020, #43082, #16509, #26325, #53914, #37155 ),
 .UNSPECIFIED., .F., .F.,
 ( 4, 1, 1, 1, 1, 1, 1, 1, 1, 1, 1, 1, 1, 1, 1, 1, 4 ),
 ( 0.000000000000000000, 0.04500057695454640072, 0.1100005346419700436, 0.1750004923296970549, 0.2400004500171206978, 0.3050004077048477646, 0.3700003653922710467, 0.4350003230796946618, 0.5000002807674217564, 0.5650002384548453715, 0.6300001961425724106, 0.6950001538299960258, 0.7600001115177230648, 0.8250000692051463469, 0.8900000268925699620, 0.9549999845802970011, 1.000000000000000000 ),
 .UNSPECIFIED. ) ;
#46975 = DIRECTION ( 'NONE',  ( 1.000000000000000000, 0.000000000000000000, 0.000000000000000000 ) ) ;
#46976 = CARTESIAN_POINT ( 'NONE',  ( 11.72823073745748879, -4.169674042210387732, 6.639671036489041001 ) ) ;
#46977 = ORIENTED_EDGE ( 'NONE', *, *, #27623, .T. ) ;
#46978 = CARTESIAN_POINT ( 'NONE',  ( 11.93277786803400176, 12.01216300861999997, -3.678628708156000293 ) ) ;
#46979 = CARTESIAN_POINT ( 'NONE',  ( 10.87947334122999976, 2.817426144593000004, -6.828668581221999823 ) ) ;
#46980 = EDGE_CURVE ( 'NONE', #30974, #69017, #13042, .T. ) ;
#46981 = CARTESIAN_POINT ( 'NONE',  ( 9.975298369746534277, -5.350379160513648813, 7.499985214262776978 ) ) ;
#46982 = CARTESIAN_POINT ( 'NONE',  ( 8.962753061708918167, 2.887246877270963630, 7.646523492023315605 ) ) ;
#46983 = ADVANCED_FACE ( 'NONE', ( #31730 ), #58287, .T. ) ;
#46984 = AXIS2_PLACEMENT_3D ( 'NONE', #11123, #27905, #12162 ) ;
#46985 = CARTESIAN_POINT ( 'NONE',  ( 17.91761384724883399, 0.6327954766588940183, 13.98569611075749286 ) ) ;
#46986 = CARTESIAN_POINT ( 'NONE',  ( 18.23887202961200060, 3.252214874110999965, 11.14733497513999971 ) ) ;
#46987 = CARTESIAN_POINT ( 'NONE',  ( 10.38153277269999997, -2.772136814285999673, -8.408084799892998618 ) ) ;
#46988 = VERTEX_POINT ( 'NONE', #53396 ) ;
#46989 = ORIENTED_EDGE ( 'NONE', *, *, #34292, .T. ) ;
#46990 = AXIS2_PLACEMENT_3D ( 'NONE', #14162, #18716, #55777 ) ;
#46991 = CARTESIAN_POINT ( 'NONE',  ( 8.979720280412999855, 5.524776413195999325, -7.147585171405999915 ) ) ;
#46992 = CARTESIAN_POINT ( 'NONE',  ( 11.03521345716899837, -3.075109701058799772, 6.659120737011199331 ) ) ;
#46993 = CARTESIAN_POINT ( 'NONE',  ( 12.48673873075621188, -3.044366353203134423, 13.54286685750151165 ) ) ;
#46994 = CARTESIAN_POINT ( 'NONE',  ( 24.19015447988511269, 3.314354331839912682, 12.40233438014860035 ) ) ;
#46995 = DIRECTION ( 'NONE',  ( 0.000000000000000000, 0.8648648648648720183, -0.5020047465136825426 ) ) ;
#46996 = CARTESIAN_POINT ( 'NONE',  ( 9.408709346416998187, 4.783195203880800328, -7.128095150442700145 ) ) ;
#46998 = CARTESIAN_POINT ( 'NONE',  ( -0.2999999999999999889, 0.5773502691895999739, -1.000000000000000000 ) ) ;
#46997 = CARTESIAN_POINT ( 'NONE',  ( 10.30698825978599942, -4.131418345883800747, 6.504223158184999853 ) ) ;
#46999 = CARTESIAN_POINT ( 'NONE',  ( 7.666438387056996540, -3.213133027605000525, 6.349775630263004622 ) ) ;
#47000 = ORIENTED_EDGE ( 'NONE', *, *, #46449, .F. ) ;
#47001 = B_SPLINE_CURVE_WITH_KNOTS ( 'NONE', 3,
 ( #30276, #31303, #51581, #52613, #14870, #52272, #4367, #4707, #62751 ),
 .UNSPECIFIED., .F., .F.,
 ( 4, 1, 1, 1, 1, 1, 4 ),
 ( 0.000000000000000000, 0.1176715969261408201, 0.3173201826739890374, 0.5169687684225858781, 0.7166173541704341510, 0.9162659399182827569, 1.000000000000000000 ),
 .UNSPECIFIED. ) ;
#47002 = CARTESIAN_POINT ( 'NONE',  ( 25.37957500006017852, -11.36922400990947501, 3.069089490420214172 ) ) ;
#47003 = CARTESIAN_POINT ( 'NONE',  ( 10.33540755369000053, -3.434008644319000325, -4.713744271798000263 ) ) ;
#47004 = CARTESIAN_POINT ( 'NONE',  ( 9.962988259787000089, 3.832626376493700082, 6.231784538167999266 ) ) ;
#47005 = CARTESIAN_POINT ( 'NONE',  ( 7.944681758174191977, 4.857212911390003995, 6.360313247088151378 ) ) ;
#47006 = DIRECTION ( 'NONE',  ( 1.000000000000000000, -4.332706595949694629E-15, 1.401268137124204108E-14 ) ) ;
#47007 = ADVANCED_FACE ( 'NONE', ( #63529 ), #50085, .T. ) ;
#47008 = DIRECTION ( 'NONE',  ( -1.000000000000000000, 3.552713678678000297E-14, -1.776356839339000149E-14 ) ) ;
#47009 = CARTESIAN_POINT ( 'NONE',  ( 9.591185841232000797, 2.173570076733999823, -8.023168429484000441 ) ) ;
#47010 = CARTESIAN_POINT ( 'NONE',  ( 13.91144947526900033, 8.829982735797999638, 7.819410275689000045 ) ) ;
#47011 = CARTESIAN_POINT ( 'NONE',  ( 8.229954139086000708, -4.681838082657003852, 6.132216288069997745 ) ) ;
#47012 = CARTESIAN_POINT ( 'NONE',  ( 6.109973520848999584, 1.122942780917999928, 0.3495427174121999991 ) ) ;
#47013 = CARTESIAN_POINT ( 'NONE',  ( 25.37956046633510354, -3.026721893553028231, 11.38059512590412581 ) ) ;
#47014 = CARTESIAN_POINT ( 'NONE',  ( 25.60000000000000142, -10.55163788719000095, -3.754896668835000284 ) ) ;
#47015 = CARTESIAN_POINT ( 'NONE',  ( 3.714218779689999916, 1.510359751552999841, -2.741952990197999984 ) ) ;
#47016 = ORIENTED_EDGE ( 'NONE', *, *, #53784, .F. ) ;
#47017 = CARTESIAN_POINT ( 'NONE',  ( 12.49190496432325226, 0.5409888710114135746, -12.68448745112149645 ) ) ;
#47018 = CARTESIAN_POINT ( 'NONE',  ( 12.27188044046201654, -2.173264662115791168, -12.52171693736153557 ) ) ;
#47019 = CARTESIAN_POINT ( 'NONE',  ( 5.200000000000000178, 0.000000000000000000, -1.600000000000000089 ) ) ;
#47020 = CARTESIAN_POINT ( 'NONE',  ( 3.499698285111554785, -2.916600830549739065, -1.425132625272170550 ) ) ;
#47021 = CARTESIAN_POINT ( 'NONE',  ( 3.500000000000001332, -1.293366386299026782, 2.969361111422694766 ) ) ;
#47022 = ORIENTED_EDGE ( 'NONE', *, *, #48322, .F. ) ;
#47023 = CARTESIAN_POINT ( 'NONE',  ( 5.207454287316000574, -0.1144865814785000074, 1.118427654993999987 ) ) ;
#47024 = VECTOR ( 'NONE', #35490, 1000.000000000000000 ) ;
#47025 = APPLICATION_PROTOCOL_DEFINITION ( 'draft international standard', 'automotive_design', 1998, #50760 ) ;
#47026 = CARTESIAN_POINT ( 'NONE',  ( 10.95696410347983729, 8.982905668905601715, 6.421968592709950130 ) ) ;
#47027 = CARTESIAN_POINT ( 'NONE',  ( 11.08757144985999865, 2.712428550139000194, 6.571291218949999902 ) ) ;
#47028 = CARTESIAN_POINT ( 'NONE',  ( 7.759512367773170105, 2.953550066126335860, -8.377314763178624446 ) ) ;
#47029 = CARTESIAN_POINT ( 'NONE',  ( 11.10612378248509913, 3.517039242046199998, -6.586279795136899651 ) ) ;
#47030 = ORIENTED_EDGE ( 'NONE', *, *, #55190, .F. ) ;
#47031 = CARTESIAN_POINT ( 'NONE',  ( 9.442085454646999665, -4.742494605615999781, 8.809986937145000141 ) ) ;
#47032 = ORIENTED_EDGE ( 'NONE', *, *, #64153, .T. ) ;
#47033 = LINE ( 'NONE', #10309, #42902 ) ;
#47034 = CARTESIAN_POINT ( 'NONE',  ( 8.764831853209999579, -5.808258301303999893, 7.446016267012000256 ) ) ;
#47035 = CARTESIAN_POINT ( 'NONE',  ( 17.77667453761836214, -0.6953657024348838256, -13.98272072176121483 ) ) ;
#47036 = ORIENTED_EDGE ( 'NONE', *, *, #32524, .T. ) ;
#47037 = CARTESIAN_POINT ( 'NONE',  ( 23.58477818954033722, 10.21639588674304910, 9.547105905782643731 ) ) ;
#47038 = CARTESIAN_POINT ( 'NONE',  ( 7.954299074928001367, 3.414461172233999697, -6.283593702261001113 ) ) ;
#47039 = VECTOR ( 'NONE', #16096, 1000.000000000000000 ) ;
#47040 = CARTESIAN_POINT ( 'NONE',  ( 6.686604719590000023, 5.464161011425000325, -7.581039036848999935 ) ) ;
#47041 = CARTESIAN_POINT ( 'NONE',  ( 9.458513540183334456, -4.163624617374470205, -8.749999999999998224 ) ) ;
#47042 = CARTESIAN_POINT ( 'NONE',  ( 18.08168818188836724, -2.836704670462161904, 12.36674034547891488 ) ) ;
#47043 = VERTEX_POINT ( 'NONE', #30113 ) ;
#47044 = CARTESIAN_POINT ( 'NONE',  ( 9.566960887370999700, -5.215923019114000247, 6.177729435798999802 ) ) ;
#47045 = EDGE_CURVE ( 'NONE', #46559, #62089, #53882, .T. ) ;
#47046 = EDGE_CURVE ( 'NONE', #13775, #30230, #35473, .T. ) ;
#47047 = CARTESIAN_POINT ( 'NONE',  ( 12.25785601948557257, -2.186712656597046056, -13.73518136002139478 ) ) ;
#47048 = CARTESIAN_POINT ( 'NONE',  ( 5.459193173017250267, 0.3926218265389159190, 1.460959015002474715 ) ) ;
#47049 = ORIENTED_EDGE ( 'NONE', *, *, #9463, .T. ) ;
#47050 = CARTESIAN_POINT ( 'NONE',  ( 10.65650106607000147, -5.448187878199999723, -7.015213573792999036 ) ) ;
#47051 = CARTESIAN_POINT ( 'NONE',  ( 7.961495038489999843, 3.389986099490999827, -6.279439026173999849 ) ) ;
#47052 = EDGE_LOOP ( 'NONE', ( #114, #8452, #10909, #24997, #64391 ) ) ;
#47053 = CARTESIAN_POINT ( 'NONE',  ( 23.62975776114408077, -10.06704571337557574, 9.666453531962270418 ) ) ;
#47054 = CARTESIAN_POINT ( 'NONE',  ( 17.75510503584834865, 0.5924680672296399608, -13.88300198246877315 ) ) ;
#47055 = CARTESIAN_POINT ( 'NONE',  ( 5.240124045625999649, 0.9801419917718999786, -1.210444677476000264 ) ) ;
#47056 = CLOSED_SHELL ( 'NONE', ( #67794, #14447, #41600, #25420, #21, #22036, #2056, #31160, #10555, #65644, #54291, #37576, #41315, #29288, #23122, #18954, #475, #33881, #7085, #44419, #47625, #49562, #5345, #36706, #9918, #17542, #53184, #43800, #63389, #18478, #22808 ) ) ;
#47057 = CARTESIAN_POINT ( 'NONE',  ( 8.849999778957998942, -4.000000000000000000, -8.499999833805500060 ) ) ;
#47058 = DIRECTION ( 'NONE',  ( 0.7071067987106167685, 0.000000000000000000, 0.7071067636624778219 ) ) ;
#47059 = LINE ( 'NONE', #35875, #13177 ) ;
#47060 = CARTESIAN_POINT ( 'NONE',  ( 9.571013540182331525, -3.231816600031356845, -8.499583552997725278 ) ) ;
#47061 = FACE_OUTER_BOUND ( 'NONE', #39527, .T. ) ;
#47062 = ORIENTED_EDGE ( 'NONE', *, *, #39707, .F. ) ;
#47063 = CARTESIAN_POINT ( 'NONE',  ( 3.313591025678166435, -3.499999999999999112, -0.5549492644885768433 ) ) ;
#47064 = VERTEX_POINT ( 'NONE', #16324 ) ;
#47065 = CARTESIAN_POINT ( 'NONE',  ( 11.20563302462000088, 3.509134285281999777, 6.118194788334999856 ) ) ;
#47066 = ADVANCED_FACE ( 'NONE', ( #15981 ), #42314, .T. ) ;
#47067 = CARTESIAN_POINT ( 'NONE',  ( 27.64127793187000037, -11.00717859340000082, 1.432487142323000118 ) ) ;
#47068 = CARTESIAN_POINT ( 'NONE',  ( 12.22230712497529304, 2.273859679217653973, -13.71882920742291923 ) ) ;
#47069 = CARTESIAN_POINT ( 'NONE',  ( 2.929084992264999965, 3.537580394849999976, -0.2084549283189000013 ) ) ;
#47070 = ADVANCED_FACE ( 'NONE', ( #48065 ), #47729, .T. ) ;
#47071 = CARTESIAN_POINT ( 'NONE',  ( 25.37703081959900331, 2.612361302726000201, 11.31741887482999864 ) ) ;
#47072 = CARTESIAN_POINT ( 'NONE',  ( 9.769471092180999960, -5.100000000000000533, -6.152188490330000370 ) ) ;
#47073 = CARTESIAN_POINT ( 'NONE',  ( 18.03351232763409939, 0.4021407113610637185, 13.89217057782673592 ) ) ;
#47074 = VERTEX_POINT ( 'NONE', #52274 ) ;
#47075 = CARTESIAN_POINT ( 'NONE',  ( 12.60487368084097604, 0.5921679928993447417, 13.88301795523195459 ) ) ;
#47076 = CARTESIAN_POINT ( 'NONE',  ( 10.72687885159599830, -2.867290578374000365, 7.635128076451499268 ) ) ;
#47077 = CARTESIAN_POINT ( 'NONE',  ( 10.30208432104581640, 5.580039836084787375, -6.689420770392193738 ) ) ;
#47078 = CARTESIAN_POINT ( 'NONE',  ( 15.20000000000000107, 11.99088163391999906, -3.229229350024999778 ) ) ;
#47079 = CARTESIAN_POINT ( 'NONE',  ( 7.373066940378000034, -3.394845988290999816, 9.388942682504000103 ) ) ;
#47081 = CARTESIAN_POINT ( 'NONE',  ( 23.56666365135700403, -2.963314674624001999, -12.23574966054999358 ) ) ;
#47080 = CARTESIAN_POINT ( 'NONE',  ( 9.385781899350000401, 4.980865465981000106, 6.433345686594999613 ) ) ;
#47082 = CARTESIAN_POINT ( 'NONE',  ( 11.33041235500449950, 3.057642534728299832, -6.636704692336500067 ) ) ;
#47083 = B_SPLINE_CURVE_WITH_KNOTS ( 'NONE', 3,
 ( #11026, #53680, #27116, #48431, #64492, #37937, #59259, #32699, #27453, #48778, #886, #22200, #43537, #64837, #16949, #38280, #59607, #49812, #55058, #18007, #60991, #33743, #50162, #13111, #44587, #66227, #50847, #40353, #34778, #67253, #7159, #34440, #8196, #56087, #2942, #28499, #29546, #29190, #18349, #19026, #61337, #66572, #18691, #50501, #13455, #24622, #40025, #2600, #24275, #61675, #45609, #66915, #55407, #7856, #39672, #55754, #13790, #1923, #23244, #19368, #35122, #23583, #65880 ),
 .UNSPECIFIED., .F., .F.,
 ( 4, 2, 2, 2, 1, 1, 1, 2, 2, 2, 2, 2, 1, 1, 1, 1, 2, 2, 2, 2, 2, 1, 1, 1, 1, 2, 2, 2, 2, 2, 1, 1, 2, 2, 2, 2, 2, 4 ),
 ( 0.000000000000000000, 0.06250000000013906931, 0.09375000000020830559, 0.1093750000002429446, 0.1171875000002602502, 0.1210937500002680495, 0.1230468750002719491, 0.1240234375002725736, 0.1250000000002731981, 0.1875000000003121392, 0.2187500000003317346, 0.2343750000003415046, 0.2421875000003464173, 0.2460937500003494427, 0.2480468750003509415, 0.2490234375003515244, 0.2495117187503518019, 0.2500000000003520517, 0.3125000000003730904, 0.3437500000003835265, 0.3593750000003880229, 0.3671875000003914646, 0.3710937500003949618, 0.3730468750003929634, 0.3740234375003919642, 0.3745117187503915201, 0.3750000000003910205, 0.4375000000003100298, 0.4687500000002691181, 0.4843750000002488010, 0.4921875000002377543, 0.4960937500002333689, 0.4980468750002323697, 0.5000000000002312595, 0.6250000000001735279, 0.7500000000001156852, 0.8750000000000579536, 1.000000000000000000 ),
 .UNSPECIFIED. ) ;
#47084 = CARTESIAN_POINT ( 'NONE',  ( 24.87965828714900240, -11.54628276867000025, 3.248280990976000204 ) ) ;
#47085 = CARTESIAN_POINT ( 'NONE',  ( 10.13425461470299993, 3.159754091322399816, -7.713763321667399531 ) ) ;
#47086 = CARTESIAN_POINT ( 'NONE',  ( 18.28005836700933529, 0.01123479547583059769, 12.60000044989513412 ) ) ;
#47087 = CARTESIAN_POINT ( 'NONE',  ( 7.073405103028999719, 1.118341376545999966, -0.1779135255794999926 ) ) ;
#47088 = CIRCLE ( 'NONE', #16927, 0.5000000000000000000 ) ;
#47089 = CARTESIAN_POINT ( 'NONE',  ( 11.84388784977539899, 2.744254309011999737, 7.571757098260779806 ) ) ;
#47090 = CARTESIAN_POINT ( 'NONE',  ( 0.5000220334827000235, 3.499749845413000049, -0.04184518527856000147 ) ) ;
#47091 = ORIENTED_EDGE ( 'NONE', *, *, #50157, .T. ) ;
#47092 = CARTESIAN_POINT ( 'NONE',  ( 8.796581853210000190, -2.368260286481999710, 7.410200011629000549 ) ) ;
#47093 = CARTESIAN_POINT ( 'NONE',  ( 17.57920672810397278, 3.248146558128239381, 13.61798601073640924 ) ) ;
#47094 = CYLINDRICAL_SURFACE ( 'NONE', #15390, 14.00000000000000000 ) ;
#47095 = VERTEX_POINT ( 'NONE', #51925 ) ;
#47096 = DIRECTION ( 'NONE',  ( 0.000000000000000000, -0.4815106998112011483, -0.8764402124317022258 ) ) ;
#47097 = CARTESIAN_POINT ( 'NONE',  ( 10.60235971519489873, 4.605301262871499546, 8.506961598696999971 ) ) ;
#47098 = CARTESIAN_POINT ( 'NONE',  ( 11.24323278040999874, 2.479734175328000223, -7.587230544849999703 ) ) ;
#47099 = ADVANCED_FACE ( 'NONE', ( #9969 ), #64583, .T. ) ;
#47100 = ORIENTED_EDGE ( 'NONE', *, *, #9073, .T. ) ;
#47101 = EDGE_CURVE ( 'NONE', #31118, #36190, #22167, .T. ) ;
#47102 = B_SPLINE_CURVE_WITH_KNOTS ( 'NONE', 3,
 ( #16861, #27718, #17214, #54969, #792, #28405, #1831, #37505, #32278, #42754, #53925, #64057, #5684, #58828, #53589, #27365, #22108, #43452, #29415, #8759, #18217, #30101, #56653 ),
 .UNSPECIFIED., .F., .F.,
 ( 4, 2, 2, 1, 2, 2, 2, 2, 1, 1, 2, 2, 4 ),
 ( 0.000000000000000000, 0.2500000000000290323, 0.3750000000000388023, 0.4375000000000434652, 0.4687500000000431322, 0.5000000000000427436, 0.6250000000000321965, 0.6875000000000294209, 0.7187500000000291989, 0.7343750000000306422, 0.7421875000000303091, 0.7500000000000299760, 1.000000000000000000 ),
 .UNSPECIFIED. ) ;
#47103 = DIRECTION ( 'NONE',  ( 0.000000000000000000, 1.000000000000000000, 0.000000000000000000 ) ) ;
#47104 = CARTESIAN_POINT ( 'NONE',  ( 17.74741402337964047, -1.780171064341584453, 12.47366677607746333 ) ) ;
#47105 = CARTESIAN_POINT ( 'NONE',  ( 10.22687885159599830, 5.132709421626000079, 7.635128076451499268 ) ) ;
#47106 = CYLINDRICAL_SURFACE ( 'NONE', #56713, 1.350000000000000533 ) ;
#47107 = CARTESIAN_POINT ( 'NONE',  ( 13.99999997735699253, -8.821177874197182689, -7.709989353259452116 ) ) ;
#47108 = EDGE_LOOP ( 'NONE', ( #8181, #30886, #41968 ) ) ;
#47109 = CARTESIAN_POINT ( 'NONE',  ( 11.50001496185000249, 9.368387413230685468, -8.415797411492746960 ) ) ;
#47110 = CARTESIAN_POINT ( 'NONE',  ( 7.417714158767000576, 4.562063799276000253, -9.314837681783000534 ) ) ;
#47111 = CARTESIAN_POINT ( 'NONE',  ( 8.288382264724496906, -4.755866256346774179, 9.066382130443654930 ) ) ;
#47112 = CARTESIAN_POINT ( 'NONE',  ( 9.322113844317998499, -3.711648483798899889, 8.604802177355001191 ) ) ;
#47113 = ORIENTED_EDGE ( 'NONE', *, *, #49386, .F. ) ;
#47114 = CARTESIAN_POINT ( 'NONE',  ( 15.86395943152100330, -3.857419000648000029, -11.66670712924999975 ) ) ;
#47115 = DIRECTION ( 'NONE',  ( -1.000000000000000000, 0.000000000000000000, 0.000000000000000000 ) ) ;
#47116 = ORIENTED_EDGE ( 'NONE', *, *, #14370, .F. ) ;
#47117 = DIRECTION ( 'NONE',  ( 0.4682208595142289265, 0.4682208595142289265, 0.7493586947727458591 ) ) ;
#47118 = CARTESIAN_POINT ( 'NONE',  ( 10.90000053908999966, 9.856474340180000127, -5.627824942316999923 ) ) ;
#47119 = ORIENTED_EDGE ( 'NONE', *, *, #57395, .F. ) ;
#47120 = CARTESIAN_POINT ( 'NONE',  ( 17.71746485746498223, 0.6038715862870291939, -13.88233985103438251 ) ) ;
#47121 = CARTESIAN_POINT ( 'NONE',  ( 7.763685801543999787, -2.858332342511999968, 6.771142545925000533 ) ) ;
#47122 = CARTESIAN_POINT ( 'NONE',  ( 8.414360841228999632, 5.461114003844000031, -8.582501063019000398 ) ) ;
#47123 = CARTESIAN_POINT ( 'NONE',  ( 11.39700581613019992, 4.869652672166700391, -8.058426314824099990 ) ) ;
#47124 = CARTESIAN_POINT ( 'NONE',  ( 11.92834208742529967, -4.706521750018099581, 6.389420067180999752 ) ) ;
#47125 = CARTESIAN_POINT ( 'NONE',  ( 8.650129892594387471, -5.422427387162434442, 6.482324188058413483 ) ) ;
#47126 = CARTESIAN_POINT ( 'NONE',  ( 11.95348876160960039, -4.885820101980599794, 6.578783887955899523 ) ) ;
#47127 = CARTESIAN_POINT ( 'NONE',  ( 9.106135841230999617, 4.192919163547999872, 5.525472271700999194 ) ) ;
#47128 = EDGE_CURVE ( 'NONE', #39559, #7001, #4304, .T. ) ;
#47129 = ADVANCED_FACE ( 'NONE', ( #26402 ), #21152, .T. ) ;
#47130 = ORIENTED_EDGE ( 'NONE', *, *, #43411, .T. ) ;
#47131 = CARTESIAN_POINT ( 'NONE',  ( 10.81499708368641954, 2.650004840405624673, -7.499999822193707644 ) ) ;
#47132 = EDGE_CURVE ( 'NONE', #21322, #34155, #36894, .T. ) ;
#47133 = CARTESIAN_POINT ( 'NONE',  ( 7.518870559622000016, -3.206365290996999740, 5.681739161071000410 ) ) ;
#47134 = CARTESIAN_POINT ( 'NONE',  ( 25.59997324745700098, -8.218963665681000563, -8.043524865771999544 ) ) ;
#47135 = EDGE_LOOP ( 'NONE', ( #35944, #32971, #39929, #52858 ) ) ;
#47136 = CARTESIAN_POINT ( 'NONE',  ( 12.60240816447944034, -3.091259750208972701, -12.29394167103376923 ) ) ;
#47137 = CARTESIAN_POINT ( 'NONE',  ( 18.41451919223379718, 3.018310540774385764, 11.25254019301550379 ) ) ;
#47138 = CARTESIAN_POINT ( 'NONE',  ( 23.60205915885299888, -9.377218989194005871, 8.305825996818995804 ) ) ;
#47139 = CARTESIAN_POINT ( 'NONE',  ( 23.57777180426788277, -13.36543806030607939, -4.119497871640947828 ) ) ;
#47140 = CARTESIAN_POINT ( 'NONE',  ( 12.58303802678793559, -1.915668549203847437, -13.78011653961192629 ) ) ;
#47141 = CARTESIAN_POINT ( 'NONE',  ( 10.75210807141120029, -3.959980833595939664, -8.365272822098500427 ) ) ;
#47142 = CARTESIAN_POINT ( 'NONE',  ( 17.89019624313516843, 3.590943193543202572, 11.99920113072226080 ) ) ;
#47143 = CARTESIAN_POINT ( 'NONE',  ( 18.24341944916329794, -2.253723043306040008, 12.39680838072757574 ) ) ;
#47144 = ORIENTED_EDGE ( 'NONE', *, *, #27643, .F. ) ;
#47145 = ORIENTED_EDGE ( 'NONE', *, *, #19922, .T. ) ;
#47146 = CARTESIAN_POINT ( 'NONE',  ( 11.78627509987130040, -4.272452942476324900, 8.749999999999998224 ) ) ;
#47147 = FACE_OUTER_BOUND ( 'NONE', #19154, .T. ) ;
#47148 = CARTESIAN_POINT ( 'NONE',  ( 10.26368708477999903, 4.794139572939999816, -8.804452601708000259 ) ) ;
#47149 = ADVANCED_FACE ( 'NONE', ( #68000 ), #32847, .F. ) ;
#47150 = CARTESIAN_POINT ( 'NONE',  ( 18.40015514469800095, 2.597921877622999464E-14, -11.75015521449979516 ) ) ;
#47151 = CARTESIAN_POINT ( 'NONE',  ( 18.17176891181418341, 2.603394967838109864, 12.42689558795375682 ) ) ;
#47152 = AXIS2_PLACEMENT_3D ( 'NONE', #48881, #22299, #12165 ) ;
#47153 = CARTESIAN_POINT ( 'NONE',  ( 24.63805894150500109, -12.49525856262000012, 2.948554912134000006 ) ) ;
#47154 = CARTESIAN_POINT ( 'NONE',  ( 10.40726830891999910, 3.797905842462999892, 5.889914049998000500 ) ) ;
#47155 = ORIENTED_EDGE ( 'NONE', *, *, #16995, .F. ) ;
#47156 = CARTESIAN_POINT ( 'NONE',  ( 8.765417767663000959, 5.029951493281999753, -6.097931603992000404 ) ) ;
#47157 = VERTEX_POINT ( 'NONE', #28475 ) ;
#47158 = CARTESIAN_POINT ( 'NONE',  ( 9.305881816721999655, 4.945299866898000829, 9.077891794505999812 ) ) ;
#47159 = CARTESIAN_POINT ( 'NONE',  ( 8.867797255587998251, -3.133765047594600173, -7.463326341748410364 ) ) ;
#47160 = CARTESIAN_POINT ( 'NONE',  ( 10.11260611051000069, 3.359887741436999864, 5.859127722154000573 ) ) ;
#47161 = CARTESIAN_POINT ( 'NONE',  ( 11.80367835872029936, -5.113555564477999305, 8.201822467543799178 ) ) ;
#47162 = CARTESIAN_POINT ( 'NONE',  ( 11.79999999471800010, -11.69117318561000118, -1.923227876431999883 ) ) ;
#47163 = DIRECTION ( 'NONE',  ( 1.000000000000000000, 0.000000000000000000, 0.000000000000000000 ) ) ;
#47164 = CARTESIAN_POINT ( 'NONE',  ( 10.44426222744799837, 3.013556901740999994, -8.312555471636301263 ) ) ;
#47165 = CARTESIAN_POINT ( 'NONE',  ( 12.23548902587310216, -0.2575478136180257005, 12.69649014468029335 ) ) ;
#47166 = CARTESIAN_POINT ( 'NONE',  ( 11.60000000000000142, 4.325863785438847309, -8.622936771936917211 ) ) ;
#47167 = CARTESIAN_POINT ( 'NONE',  ( 10.13049857835000012, 3.092060693447000297, 8.629378633793999498 ) ) ;
#47168 = CARTESIAN_POINT ( 'NONE',  ( 9.115728395017272945, -3.733357885829600598, 8.827356134417316369 ) ) ;
#47169 = ORIENTED_EDGE ( 'NONE', *, *, #2599, .T. ) ;
#47170 = CARTESIAN_POINT ( 'NONE',  ( 10.12339528040999959, 3.988943694240999704, -8.966360307350999648 ) ) ;
#47171 = DIRECTION ( 'NONE',  ( 1.000000000000000000, 0.000000000000000000, 0.000000000000000000 ) ) ;
#47172 = CARTESIAN_POINT ( 'NONE',  ( 11.01356641589999974, -2.786433584103999994, 6.253463831328000211 ) ) ;
#47173 = CARTESIAN_POINT ( 'NONE',  ( 12.56893612375087876, -3.162115968203192740, -12.19677724224617599 ) ) ;
#47174 = APPLICATION_CONTEXT ( 'automotive_design' ) ;
#47175 = CARTESIAN_POINT ( 'NONE',  ( 12.10000000000000320, -3.304217902137880802, 8.404145852941008243 ) ) ;
#47176 = CARTESIAN_POINT ( 'NONE',  ( 10.71918447801630059, -2.859536135895000442, -7.474854604063350116 ) ) ;
#47177 = ORIENTED_EDGE ( 'NONE', *, *, #36607, .T. ) ;
#47178 = VECTOR ( 'NONE', #21075, 1000.000000000000114 ) ;
#47179 = CARTESIAN_POINT ( 'NONE',  ( 5.670648345173091798, -12.06568050912973611, 3.730933605404522790 ) ) ;
#47180 = CARTESIAN_POINT ( 'NONE',  ( 10.52052890781999928, -2.899999999999999911, 6.152188490330000370 ) ) ;
#47183 = CARTESIAN_POINT ( 'NONE',  ( 11.35194303199000032, 3.840151595817999919, -11.76830449990999838 ) ) ;
#47182 = CARTESIAN_POINT ( 'NONE',  ( 9.568039158772000619, 5.336630274082000192, -7.092011739486999922 ) ) ;
#47181 = UNCERTAINTY_MEASURE_WITH_UNIT (LENGTH_MEASURE( 1.000000000000000082E-05 ), #33994, 'distance_accuracy_value', 'NONE');
#47184 = CARTESIAN_POINT ( 'NONE',  ( 18.16657332793047175, -2.629115782240843302, 13.64522528451933425 ) ) ;
#47185 = ADVANCED_FACE ( 'NONE', ( #44218 ), #12210, .T. ) ;
#47186 = ORIENTED_EDGE ( 'NONE', *, *, #25918, .F. ) ;
#47187 = ADVANCED_FACE ( 'NONE', ( #31230 ), #37151, .F. ) ;
#47188 = CARTESIAN_POINT ( 'NONE',  ( 15.96663596566263976, 3.844870426479619852, 11.78010250471070997 ) ) ;
#47189 = CARTESIAN_POINT ( 'NONE',  ( 17.93716281226434717, -2.994693044426598671, -13.55594923565225329 ) ) ;
#47190 = CARTESIAN_POINT ( 'NONE',  ( 10.43210941423799909, 4.641185166475500168, 8.082391773166900606 ) ) ;
#47191 = CARTESIAN_POINT ( 'NONE',  ( 25.22257210903613611, -11.23352489450897451, 3.340298631152402997 ) ) ;
#47192 = CARTESIAN_POINT ( 'NONE',  ( 8.026331853209001110, -5.601799093797000140, 7.176147756900999930 ) ) ;
#47193 = ORIENTED_EDGE ( 'NONE', *, *, #8134, .F. ) ;
#47194 = CARTESIAN_POINT ( 'NONE',  ( 7.390489158771000433, 2.216873702600000051, 8.370081218683999680 ) ) ;
#47196 = CARTESIAN_POINT ( 'NONE',  ( 10.26694555961999988, -5.500014128486999887, -6.419508248405999318 ) ) ;
#47195 = CARTESIAN_POINT ( 'NONE',  ( 11.08126742035591228, 3.231380926423223166, -7.106626190113856545 ) ) ;
#47197 = CARTESIAN_POINT ( 'NONE',  ( 7.603848374511878561, -4.618107943694234940, 5.872280490120857621 ) ) ;
#47198 = VECTOR ( 'NONE', #66111, 1000.000000000000000 ) ;
#47199 = DIRECTION ( 'NONE',  ( -1.000000000000000000, 0.000000000000000000, 0.000000000000000000 ) ) ;
#47200 = CARTESIAN_POINT ( 'NONE',  ( 24.13681679563899962, 3.227440004341000090, 12.37874214852999977 ) ) ;
#47201 = ORIENTED_EDGE ( 'NONE', *, *, #51392, .T. ) ;
#47202 = CARTESIAN_POINT ( 'NONE',  ( 0.9049113558389121348, -0.1461257074673270873, 3.299567646954244093 ) ) ;
#47203 = CARTESIAN_POINT ( 'NONE',  ( 11.30133863405320049, -3.465595476214000215, 6.818303296693398963 ) ) ;
#47204 = CARTESIAN_POINT ( 'NONE',  ( 9.305881816721999655, 4.945299866898000829, 9.077891794505999812 ) ) ;
#47205 = CARTESIAN_POINT ( 'NONE',  ( 10.38314899745999931, 5.167567567567999731, 6.822293592207000934 ) ) ;
#47206 = CARTESIAN_POINT ( 'NONE',  ( 11.18687482311539938, 5.057677595549000316, 7.072673169413499217 ) ) ;
#47207 = ORIENTED_EDGE ( 'NONE', *, *, #61424, .T. ) ;
#47208 = CARTESIAN_POINT ( 'NONE',  ( 8.642077642326000841, 2.899999999999999911, 6.463854830420999953 ) ) ;
#47209 = CARTESIAN_POINT ( 'NONE',  ( 12.07980306947240301, 2.459616342362515695, -12.35762317364247487 ) ) ;
#47210 = CARTESIAN_POINT ( 'NONE',  ( 10.97843137008999825, -5.235400103863000254, 6.782920672145000829 ) ) ;
#47211 = CARTESIAN_POINT ( 'NONE',  ( 24.30000000000000071, -2.078227429405999693, 11.31065739696999906 ) ) ;
#47212 = CARTESIAN_POINT ( 'NONE',  ( 18.23515949175306261, -2.264077836046926251, 13.81573184862659431 ) ) ;
#47214 = ADVANCED_FACE ( 'NONE', ( #41020 ), #10574, .F. ) ;
#47213 = CARTESIAN_POINT ( 'NONE',  ( 25.44994113074799813, 11.77655473258999841, -4.190794510628000680 ) ) ;
#47215 = ORIENTED_EDGE ( 'NONE', *, *, #33625, .F. ) ;
#47216 = CARTESIAN_POINT ( 'NONE',  ( 9.096071945540000314, -5.102479135096000817, -6.621020973615999061 ) ) ;
#47217 = B_SPLINE_CURVE_WITH_KNOTS ( 'NONE', 3,
 ( #36288, #30705, #52015, #4116, #20554, #25453, #10061, #41533, #1646, #27183, #49191, #54087, #16339, #263, #12137, #1300 ),
 .UNSPECIFIED., .F., .F.,
 ( 4, 2, 2, 2, 2, 2, 2, 4 ),
 ( 0.000000000000000000, 0.06249999999999733546, 0.1249999999999946709, 0.2499999999999935607, 0.4999999999999946709, 0.7499999999999957812, 0.8749999999999978906, 1.000000000000000000 ),
 .UNSPECIFIED. ) ;
#47218 = CARTESIAN_POINT ( 'NONE',  ( 23.57777264369916992, 10.35461123704867781, -9.360203869705690849 ) ) ;
#47219 = ORIENTED_EDGE ( 'NONE', *, *, #40342, .T. ) ;
#47220 = CARTESIAN_POINT ( 'NONE',  ( 10.26195629121000152, -4.600000265269999389, 4.591198190832999515 ) ) ;
#47221 = CARTESIAN_POINT ( 'NONE',  ( 11.44133594839949986, 4.569506585117100173, 8.152656755002400502 ) ) ;
#47222 = CARTESIAN_POINT ( 'NONE',  ( 11.06923869026000062, 5.425682056982999768, 8.012911262916999178 ) ) ;
#47223 = CARTESIAN_POINT ( 'NONE',  ( 10.82565186280000091, 5.331165376905000031, -8.542144899688000947 ) ) ;
#47224 = CARTESIAN_POINT ( 'NONE',  ( 9.505520750864626223, -4.127043264527912925, -6.634325535862901191 ) ) ;
#47225 = CARTESIAN_POINT ( 'NONE',  ( 10.24478558459999888, -5.265199116477000452, 8.959495174640998982 ) ) ;
#47226 = CARTESIAN_POINT ( 'NONE',  ( 18.07652645701808325, -0.4998493492227053525, -12.59008424712975227 ) ) ;
#47227 = CARTESIAN_POINT ( 'NONE',  ( 12.42339251324506222, 2.995356603752234115, -12.32227076304033275 ) ) ;
#47228 = CARTESIAN_POINT ( 'NONE',  ( 11.09256785386839894, -4.832509746210599921, -8.060248494254899754 ) ) ;
#47229 = CARTESIAN_POINT ( 'NONE',  ( 8.099999999999999645, 0.000000000000000000, 0.000000000000000000 ) ) ;
#47230 = ORIENTED_EDGE ( 'NONE', *, *, #42579, .F. ) ;
#47231 = CIRCLE ( 'NONE', #40535, 1.000000000000000222 ) ;
#47232 = CARTESIAN_POINT ( 'NONE',  ( 10.89393020684959978, 2.750000000000000000, 7.500000000000000000 ) ) ;
#47233 = CARTESIAN_POINT ( 'NONE',  ( 9.433148997456999751, 5.167567567567999731, 6.822293592207000934 ) ) ;
#47234 = CARTESIAN_POINT ( 'NONE',  ( 25.29987654162099986, 8.533547811387000692, 7.925584028117998336 ) ) ;
#47235 = EDGE_CURVE ( 'NONE', #30098, #68740, #68021, .T. ) ;
#47236 = CARTESIAN_POINT ( 'NONE',  ( 6.207153620001000682, 9.294285739568001858, 4.825711238106001666 ) ) ;
#47237 = CARTESIAN_POINT ( 'NONE',  ( 12.50345261626379845, 3.182071724319534223, 13.63357796689959933 ) ) ;
#47238 = CARTESIAN_POINT ( 'NONE',  ( 10.69031285273999821, -5.903020122789000013, 7.830708506196000229 ) ) ;
#47239 = B_SPLINE_CURVE_WITH_KNOTS ( 'NONE', 3,
 ( #10235, #48675, #31570, #52889, #779, #26324, #15824, #68962, #16166, #37154, #10577, #50405, #7754, #11600, #49356, #44135, #39222, #38527 ),
 .UNSPECIFIED., .F., .F.,
 ( 4, 2, 2, 2, 2, 2, 2, 2, 4 ),
 ( 0.000000000000000000, 0.1250000000000000000, 0.2500000000000000000, 0.3750000000000000000, 0.5000000000000000000, 0.6250000000000000000, 0.7500000000000000000, 0.8750000000000000000, 1.000000000000000000 ),
 .UNSPECIFIED. ) ;
#47240 = DIRECTION ( 'NONE',  ( 1.000000000000000000, 0.000000000000000000, 0.000000000000000000 ) ) ;
#47241 = CARTESIAN_POINT ( 'NONE',  ( 12.58342633946452338, -0.6953657024348739446, 13.98272072176121661 ) ) ;
#47242 = ORIENTED_EDGE ( 'NONE', *, *, #52184, .F. ) ;
#47243 = CARTESIAN_POINT ( 'NONE',  ( 24.26682857475500299, 8.952388712744999921, 8.898287395196000205 ) ) ;
#47244 = CARTESIAN_POINT ( 'NONE',  ( 9.859659112603999631, -4.496147888241900148, -8.528383061402999843 ) ) ;
#47245 = CARTESIAN_POINT ( 'NONE',  ( 11.30000285318000230, 11.76356368987999979, 1.428410073821000159 ) ) ;
#47246 = CARTESIAN_POINT ( 'NONE',  ( 11.11845396862999991, -5.767021056207999763, 7.178419201465000121 ) ) ;
#47247 = CARTESIAN_POINT ( 'NONE',  ( 11.99056651104150006, -3.914543207408039738, 8.361971998931499783 ) ) ;
#47248 = AXIS2_PLACEMENT_3D ( 'NONE', #41107, #51928, #20460 ) ;
#47249 = CARTESIAN_POINT ( 'NONE',  ( 12.19582542658656976, 0.3901114995139722819, 12.59396323349878166 ) ) ;
#47250 = VECTOR ( 'NONE', #17483, 1000.000000000000000 ) ;
#47251 = CARTESIAN_POINT ( 'NONE',  ( 0.5651652630779999686, -0.7815069638253000495, -3.281818906455000295 ) ) ;
#47252 = CARTESIAN_POINT ( 'NONE',  ( 9.804402243952704765, 2.650150644870925110, -7.676800222058682621 ) ) ;
#47253 = CARTESIAN_POINT ( 'NONE',  ( 12.12451730110971582, 2.231694252990110261, 12.40079297172318107 ) ) ;
#47254 = CARTESIAN_POINT ( 'NONE',  ( 10.72180282791710049, -2.874603711572245146, 6.749639981085186591 ) ) ;
#47255 = CARTESIAN_POINT ( 'NONE',  ( 10.60026222744819790, 3.225465054973100099, -8.138001937130599828 ) ) ;
#47256 = CARTESIAN_POINT ( 'NONE',  ( 11.92270903091196921, 11.93179002798790123, -3.810633631264379595 ) ) ;
#47257 = CARTESIAN_POINT ( 'NONE',  ( 10.86460778041000097, 3.843601682313000367, -5.985271987931999327 ) ) ;
#47258 = CARTESIAN_POINT ( 'NONE',  ( 9.706621437244999484, 4.849675135054999586, -6.543738240676099771 ) ) ;
#47260 = CARTESIAN_POINT ( 'NONE',  ( 12.48631554272296640, 3.044136704961973638, 12.30804282041555275 ) ) ;
#47259 = DIRECTION ( 'NONE',  ( 0.000000000000000000, 0.000000000000000000, -1.000000000000000000 ) ) ;
#47261 = CARTESIAN_POINT ( 'NONE',  ( 8.789886373836322875, 4.000007821194420110, 6.560153657526067938 ) ) ;
#47262 = VERTEX_POINT ( 'NONE', #51847 ) ;
#47263 = CARTESIAN_POINT ( 'NONE',  ( 12.32623904992082942, -0.4017251368573808157, 12.69144801866960037 ) ) ;
#47264 = CARTESIAN_POINT ( 'NONE',  ( 7.726822586083000211, 2.853542176918999917, 6.781784851098000111 ) ) ;
#47265 = CARTESIAN_POINT ( 'NONE',  ( 10.13050497920000126, -3.092053006542000215, 8.629388195475000245 ) ) ;
#47266 = CARTESIAN_POINT ( 'NONE',  ( 9.300405316139999101, 3.786750623988900166, 6.518487389810699639 ) ) ;
#47267 = EDGE_CURVE ( 'NONE', #52043, #47074, #58863, .T. ) ;
#47268 = EDGE_CURVE ( 'NONE', #46445, #25251, #7105, .T. ) ;
#47269 = LINE ( 'NONE', #20695, #3112 ) ;
#47270 = CARTESIAN_POINT ( 'NONE',  ( 12.27207468729466022, -2.172927540677619618, 13.73742275803506452 ) ) ;
#47271 = LINE ( 'NONE', #10542, #31972 ) ;
#47272 = CYLINDRICAL_SURFACE ( 'NONE', #58945, 1.000000000000000444 ) ;
#47273 = EDGE_LOOP ( 'NONE', ( #4834, #48826, #63097, #63843 ) ) ;
#47274 = EDGE_CURVE ( 'NONE', #16661, #7255, #14668, .T. ) ;
#47275 = EDGE_CURVE ( 'NONE', #2379, #62671, #22782, .T. ) ;
#47276 = AXIS2_PLACEMENT_3D ( 'NONE', #47213, #53824, #32508 ) ;
#47277 = CARTESIAN_POINT ( 'NONE',  ( 4.500647932088999603, -0.4305483101668000079, -1.200584607419999950 ) ) ;
#47278 = CARTESIAN_POINT ( 'NONE',  ( 9.022734463322999332, -3.866750753272200303, -8.772253522581999974 ) ) ;
#47279 = CARTESIAN_POINT ( 'NONE',  ( 9.606596480940037708, -5.179845537100731256, -8.180011290786715961 ) ) ;
#47280 = CARTESIAN_POINT ( 'NONE',  ( 10.98280513895999988, -3.096689368913399854, 8.002155910165599906 ) ) ;
#47281 = CARTESIAN_POINT ( 'NONE',  ( 18.17157907633050939, 2.603049611614717485, -12.42699283961531265 ) ) ;
#47282 = CARTESIAN_POINT ( 'NONE',  ( 9.143927823787141307, -2.750011555256801188, -7.499999844943244121 ) ) ;
#47283 = CARTESIAN_POINT ( 'NONE',  ( 17.86986266960968450, 3.040316756266463027, 12.30911383021309824 ) ) ;
#47284 = CARTESIAN_POINT ( 'NONE',  ( 7.885003087483005046, 2.917683036408002195, 6.444041402419006914 ) ) ;
#47285 = CARTESIAN_POINT ( 'NONE',  ( 10.88932069782000056, -2.940686056611999888, -5.040625135843000315 ) ) ;
#47286 = CARTESIAN_POINT ( 'NONE',  ( 24.74075988380799984, 11.86917468414000076, 3.111330255459000327 ) ) ;
#47287 = DIRECTION ( 'NONE',  ( -1.000000000000000000, 0.000000000000000000, 0.000000000000000000 ) ) ;
#47288 = DIRECTION ( 'NONE',  ( -1.000000000000000000, 0.000000000000000000, 0.000000000000000000 ) ) ;
#47289 = CARTESIAN_POINT ( 'NONE',  ( 13.73937158902900180, -8.990218567665001714, -7.348698335466000486 ) ) ;
#47290 = DIRECTION ( 'NONE',  ( -0.4999999999999719669, 0.6407827956774649891, -0.5825782426110679424 ) ) ;
#47291 = CARTESIAN_POINT ( 'NONE',  ( 23.74082935151600182, 13.16168609087999819, -3.761290584336999920 ) ) ;
#47292 = EDGE_CURVE ( 'NONE', #55031, #67995, #55530, .T. ) ;
#47293 = ORIENTED_EDGE ( 'NONE', *, *, #31104, .F. ) ;
#47294 = CARTESIAN_POINT ( 'NONE',  ( 8.356920280409999791, 4.851303550474000303, -9.008742670124000540 ) ) ;
#47295 = CARTESIAN_POINT ( 'NONE',  ( 12.13410404293056999, -4.442327784369100030, 6.599279737936000423 ) ) ;
#47296 = EDGE_LOOP ( 'NONE', ( #51936, #8904, #3394, #13584 ) ) ;
#47297 = CARTESIAN_POINT ( 'NONE',  ( 7.912439085938001604, 3.534686866976279873, -6.215565689732485133 ) ) ;
#47298 = CARTESIAN_POINT ( 'NONE',  ( 11.35502763632549872, -5.160433036184000066, -6.964545474268299508 ) ) ;
#47299 = ORIENTED_EDGE ( 'NONE', *, *, #61873, .T. ) ;
#47300 = CARTESIAN_POINT ( 'NONE',  ( 11.17901463001529905, 4.697110652903200290, 8.616511311517999872 ) ) ;
#47302 = CARTESIAN_POINT ( 'NONE',  ( 9.640910841231999484, 2.212639797530000063, -6.855876382544999537 ) ) ;
#47301 = VECTOR ( 'NONE', #47925, 1000.000000000000000 ) ;
#47303 = DIRECTION ( 'NONE',  ( 1.000000000000000000, 0.000000000000000000, 0.000000000000000000 ) ) ;
#47304 = CARTESIAN_POINT ( 'NONE',  ( 11.23589666366019912, -4.039600775206940497, -8.391246537305399045 ) ) ;
#47305 = CARTESIAN_POINT ( 'NONE',  ( 12.31853810485765877, 0.3923498215458492977, -13.89254714539060132 ) ) ;
#47306 = CARTESIAN_POINT ( 'NONE',  ( 0.2500098862125000321, 0.000000000000000000, 0.000000000000000000 ) ) ;
#47307 = CARTESIAN_POINT ( 'NONE',  ( 11.09999999999999964, 5.759298710781000530, 5.143901506165000193 ) ) ;
#47308 = VERTEX_POINT ( 'NONE', #5327 ) ;
#47309 = DIRECTION ( 'NONE',  ( 1.000000000000000000, 0.000000000000000000, 0.000000000000000000 ) ) ;
#47310 = CARTESIAN_POINT ( 'NONE',  ( 8.640504719592000171, 2.305580295895999665, -7.860904109308999743 ) ) ;
#47311 = VERTEX_POINT ( 'NONE', #26669 ) ;
#47312 = CARTESIAN_POINT ( 'NONE',  ( 10.19715290653000217, 4.982626294267999967, -6.124313696433000054 ) ) ;
#47313 = SHAPE_REPRESENTATION_RELATIONSHIP ( 'NONE' , 'NONE' ,  #27655, #8521 ) ;
#47314 = EDGE_LOOP ( 'NONE', ( #8779, #17748, #15245, #14901 ) ) ;
#47315 = CARTESIAN_POINT ( 'NONE',  ( 9.757279731608999640, 4.114789684104199985, 8.774051692788999546 ) ) ;
#47316 = CARTESIAN_POINT ( 'NONE',  ( 18.17997390458975460, -2.522451123844925203, -12.44632513475228031 ) ) ;
#47317 = EDGE_CURVE ( 'NONE', #59008, #52535, #36329, .T. ) ;
#47318 = LINE ( 'NONE', #3620, #65297 ) ;
#47319 = B_SPLINE_SURFACE_WITH_KNOTS ( 'NONE', 3, 3, ( 
 ( #10961, #37185, #63045, #63744, #68644, #26010, #468, #42433, #58505, #58851, #26707, #16545, #48021, #9574, #31950, #21441, #21784, #124, #32301, #36496, #43119, #53267, #5369, #42776, #5020, #30916, #52229, #4329, #68297, #20416, #15172, #47685, #9926, #20762, #68996 ),
 ( #42092, #26359, #63400, #15521, #36848, #58168, #31602, #52924, #59542, #54292, #28432, #32978, #22477, #6393, #43475, #11993, #27743, #17940, #60240, #65116, #49056, #12343, #43819, #28786, #33329, #50097, #1162, #39261, #2206, #33676, #60584, #12689, #17239, #17593, #55339 ),
 ( #54647, #11296, #23519, #34026, #7435, #23173, #48714, #38561, #11637, #44859, #6049, #27388, #1506, #38213, #817, #7095, #22134, #64772, #66166, #44522, #59884, #16886, #49746, #18285, #59194, #6741, #28081, #54994, #49395, #32636, #22824, #44172, #53946, #65468, #1855 ),
 ( #38920, #65817, #40293, #2537, #45881, #55691, #29128, #45549, #56026, #57054, #14419, #35060, #67191, #61612, #23865, #35397, #24206, #9154, #24558, #18629, #51804, #60931, #46573, #35736, #8479, #19303, #66854, #3902, #13043, #39604, #30491, #18968, #2883, #7788, #3562 ) ),
 .UNSPECIFIED., .F., .F., .F.,
 ( 4, 4 ),
 ( 4, 1, 1, 1, 1, 1, 1, 1, 1, 1, 1, 1, 1, 1, 1, 1, 1, 1, 1, 1, 1, 1, 1, 1, 1, 1, 1, 1, 1, 1, 1, 1, 4 ),
 ( -0.02000000000000000042, 1.020000000000000018 ),
 ( 0.1633025096610999927, 0.1899619885200000136, 0.2166214673788000034, 0.2432809462376999965, 0.2699404250964999585, 0.2965999039553000038, 0.3232593828141999692, 0.3499188616730000145, 0.3765783405318000043, 0.4032378193906999697, 0.4298972982494999595, 0.4565567771083000048, 0.4832162559671999702, 0.5098757348260000155, 0.5365352136848999809, 0.5631946925437000262, 0.5898541714025000715, 0.6165136502614000369, 0.6431731291201999712, 0.6698326079790000165, 0.6964920868378999819, 0.7231515656967000272, 0.7498110445554999615, 0.7764705234143999268, 0.8031300022731999722, 0.8297894811320000175, 0.8564489599908999828, 0.8831084388497000282, 0.9097679177085999935, 0.9364273965674000388, 0.9630868754261999731, 0.9897463542851000495, 1.016405833144000015 ),
 .UNSPECIFIED. ) ;
#47320 = EDGE_CURVE ( 'NONE', #28416, #49162, #17193, .T. ) ;
#47321 = CARTESIAN_POINT ( 'NONE',  ( 4.049969279409727285, 2.099966510537780273, 9.844688305727672900E-09 ) ) ;
#47322 = CARTESIAN_POINT ( 'NONE',  ( 11.09999999999999964, 0.5000000000000000000, 5.124965750789000296 ) ) ;
#47323 = CIRCLE ( 'NONE', #22758, 5.000000000000000000 ) ;
#47324 = VERTEX_POINT ( 'NONE', #58813 ) ;
#47325 = CARTESIAN_POINT ( 'NONE',  ( 12.49732881085200020, 12.03818693049999844, -3.242368311117000079 ) ) ;
#47326 = CARTESIAN_POINT ( 'NONE',  ( 17.74071352830300086, 11.49974814740000006, -4.814170953196000191 ) ) ;
#47327 = CARTESIAN_POINT ( 'NONE',  ( 0.2000000000000000389, -1.649999999999999911, 0.000000000000000000 ) ) ;
#47328 = CARTESIAN_POINT ( 'NONE',  ( 9.843930206850000530, -5.250000000000000000, 7.500000000000000000 ) ) ;
#47329 = CARTESIAN_POINT ( 'NONE',  ( 9.196339158776000389, 4.112741311853999271, -5.603466076760000192 ) ) ;
#47330 = CARTESIAN_POINT ( 'NONE',  ( 18.35167777225700192, -2.962063834667000073, 12.02051524900000068 ) ) ;
#47331 = CARTESIAN_POINT ( 'NONE',  ( 9.898134631442999876, -2.965923230546999800, -6.610863544715000373 ) ) ;
#47332 = ORIENTED_EDGE ( 'NONE', *, *, #56063, .T. ) ;
#47333 = EDGE_LOOP ( 'NONE', ( #2318, #68683, #54062, #36468, #10749, #64560, #13838, #33335, #15957, #60564, #25782, #41472 ) ) ;
#47334 = CARTESIAN_POINT ( 'NONE',  ( 11.05213295625000036, 5.231718854540000407, -4.976717655758000625 ) ) ;
#47335 = CARTESIAN_POINT ( 'NONE',  ( 10.89393020684959978, 2.750000000000000000, 7.500000000000000000 ) ) ;
#47336 = CARTESIAN_POINT ( 'NONE',  ( 1.248890132540875220, -2.798833948393641080, 2.150913519912190708 ) ) ;
#47337 = CARTESIAN_POINT ( 'NONE',  ( 0.1499942179680000265, 0.7197945678028363492, -2.678379783547566895 ) ) ;
#47338 = B_SPLINE_CURVE_WITH_KNOTS ( 'NONE', 3,
 ( #21818, #58888, #54678, #44207, #39293, #50468, #60961, #55372, #55028, #17629, #28821, #33709, #2570, #1891 ),
 .UNSPECIFIED., .F., .F.,
 ( 4, 2, 2, 2, 2, 2, 4 ),
 ( 0.000000000000000000, 0.1250000000000011380, 0.2500000000000022760, 0.5000000000000034417, 0.6250000000000025535, 0.7500000000000016653, 1.000000000000000000 ),
 .UNSPECIFIED. ) ;
#47339 = PLANE ( 'NONE',  #67829 ) ;
#47340 = CARTESIAN_POINT ( 'NONE',  ( 8.826138961223998436, 4.718363881473300658, -7.985449642667900250 ) ) ;
#47342 = CARTESIAN_POINT ( 'NONE',  ( 8.349082721034115195, 4.945536839314570443, -6.215508931641162249 ) ) ;
#47341 = CARTESIAN_POINT ( 'NONE',  ( 10.00303849359899822, -3.273092657276900130, 8.193143574899998782 ) ) ;
#47343 = CARTESIAN_POINT ( 'NONE',  ( 8.149001627428001271, -3.121156835630000348, 6.130053226229998486 ) ) ;
#47344 = ORIENTED_EDGE ( 'NONE', *, *, #51321, .T. ) ;
#47345 = CARTESIAN_POINT ( 'NONE',  ( 12.79999999202000005, -11.41069016990000051, 4.623987642516999230 ) ) ;
#47346 = VECTOR ( 'NONE', #19428, 1000.000000000000000 ) ;
#47347 = DIRECTION ( 'NONE',  ( 6.273181768770000388E-11, -6.273307657911000434E-11, 1.000000000000000000 ) ) ;
#47348 = CARTESIAN_POINT ( 'NONE',  ( 10.57088779216199903, 5.183207142131999845, 7.073306690476799830 ) ) ;
#47349 = CARTESIAN_POINT ( 'NONE',  ( 10.49785673611999925, -3.776281940467000275, 5.717636230565000588 ) ) ;
#47350 = DIRECTION ( 'NONE',  ( 0.9999999999999967804, -7.921520927618944111E-08, 3.389354038770978966E-10 ) ) ;
#47351 = CARTESIAN_POINT ( 'NONE',  ( 16.13937158902900393, -3.642730659064999710, -11.02533040164999889 ) ) ;
#47352 = AXIS2_PLACEMENT_3D ( 'NONE', #42035, #21388, #51827 ) ;
#47353 = EDGE_CURVE ( 'NONE', #34779, #798, #53423, .T. ) ;
#47354 = ADVANCED_FACE ( 'NONE', ( #53909 ), #43455, .F. ) ;
#47355 = CARTESIAN_POINT ( 'NONE',  ( 13.67059379716000045, 8.916337866955000635, 7.720150512555999711 ) ) ;
#47356 = DIRECTION ( 'NONE',  ( 0.4384236320214023319, 0.000000000000000000, -0.8987684456439056779 ) ) ;
#47357 = CARTESIAN_POINT ( 'NONE',  ( 9.737988259786000356, -4.113440707072600233, -8.359557531806398600 ) ) ;
#47358 = FACE_OUTER_BOUND ( 'NONE', #6877, .T. ) ;
#47359 = CARTESIAN_POINT ( 'NONE',  ( 24.30000000000000071, -11.85420044612000012, -3.901016762742000488 ) ) ;
#47360 = CARTESIAN_POINT ( 'NONE',  ( 5.634820038283264054, 12.96111451950602245, -2.364727967815067888 ) ) ;
#47361 = CYLINDRICAL_SURFACE ( 'NONE', #5656, 2.750000000000000000 ) ;
#47362 = ORIENTED_EDGE ( 'NONE', *, *, #26487, .T. ) ;
#47363 = CARTESIAN_POINT ( 'NONE',  ( 12.34842979604855273, 0.4268810874232075170, -12.69034564040270396 ) ) ;
#47364 = CARTESIAN_POINT ( 'NONE',  ( 12.64124574432627313, -3.108970204240351975, -12.28865804429000264 ) ) ;
#47365 = DIRECTION ( 'NONE',  ( -1.000000000000000000, 0.000000000000000000, 0.000000000000000000 ) ) ;
#47366 = FACE_OUTER_BOUND ( 'NONE', #15563, .T. ) ;
#47367 = CARTESIAN_POINT ( 'NONE',  ( 10.16712151127302199, 5.079456268609247260, -8.329490867414714117 ) ) ;
#47368 = VERTEX_POINT ( 'NONE', #66125 ) ;
#47369 = CARTESIAN_POINT ( 'NONE',  ( 5.493135431812000036, 0.6181797131151999247, -1.000516987031000005 ) ) ;
#47370 = APPLICATION_PROTOCOL_DEFINITION ( 'draft international standard', 'automotive_design', 1998, #21734 ) ;
#47371 = CARTESIAN_POINT ( 'NONE',  ( 11.05946005378019947, -2.963614890480000152, -6.946587256304699309 ) ) ;
#47372 = CARTESIAN_POINT ( 'NONE',  ( 0.5000220334827000235, 3.499749845413000049, -0.04184518527856000147 ) ) ;
#47373 = EDGE_CURVE ( 'NONE', #64966, #1839, #6221, .T. ) ;
#47374 = CARTESIAN_POINT ( 'NONE',  ( 11.09999999999999964, -2.700000000000000178, -5.157071250680000496 ) ) ;
#47375 = DIRECTION ( 'NONE',  ( -0.7071067811865474617, -0.7071067811865474617, 1.247903205617082848E-09 ) ) ;
#47376 = CARTESIAN_POINT ( 'NONE',  ( 11.11123293495519881, 3.108594079907299967, -7.464165716332529676 ) ) ;
#47377 = ORIENTED_EDGE ( 'NONE', *, *, #30982, .F. ) ;
#47378 = CIRCLE ( 'NONE', #38435, 12.99999867215000116 ) ;
#47379 = CARTESIAN_POINT ( 'NONE',  ( 10.41185831014999863, -2.101597930377999912, 7.856264717901999539 ) ) ;
#47380 = VERTEX_POINT ( 'NONE', #55993 ) ;
#47381 = CARTESIAN_POINT ( 'NONE',  ( 7.570242946765014302, -3.646570892123639052, 8.816260394360254438 ) ) ;
#47382 = CARTESIAN_POINT ( 'NONE',  ( 7.454683059621999952, -2.138201851198999748, 6.814774777484000623 ) ) ;
#47383 = CARTESIAN_POINT ( 'NONE',  ( 17.82168025737886552, -0.6791475903684105475, -13.98351814429472917 ) ) ;
#47384 = VERTEX_POINT ( 'NONE', #28744 ) ;
#47385 = CARTESIAN_POINT ( 'NONE',  ( 8.289480787584649235, 3.351401960818187753, -6.090076450232053240 ) ) ;
#47386 = CARTESIAN_POINT ( 'NONE',  ( 8.268945280408999565, 5.730434958826999825, -7.416203477251000820 ) ) ;
#47387 = DIRECTION ( 'NONE',  ( 0.000000000000000000, 0.2461538461537955691, -0.9692307692307821076 ) ) ;
#47388 = CARTESIAN_POINT ( 'NONE',  ( 9.490614058485499882, 4.913414349029470607, 8.493955840285781989 ) ) ;
#47389 = ORIENTED_EDGE ( 'NONE', *, *, #10357, .F. ) ;
#47390 = CARTESIAN_POINT ( 'NONE',  ( 10.74609562913000005, -4.263104965433000437, 9.276976808608999647 ) ) ;
#47391 = DIRECTION ( 'NONE',  ( -1.000000000000000000, 0.000000000000000000, 0.000000000000000000 ) ) ;
#47392 = CARTESIAN_POINT ( 'NONE',  ( 9.343930206849998754, 2.750000000000000000, -7.500000000000000000 ) ) ;
#47393 = EDGE_LOOP ( 'NONE', ( #18924, #48892, #50513, #59859, #67494, #64233 ) ) ;
#47394 = CIRCLE ( 'NONE', #60761, 10.55000000000000249 ) ;
#47395 = CARTESIAN_POINT ( 'NONE',  ( 5.000000000000000000, 0.000000000000000000, 0.000000000000000000 ) ) ;
#47396 = VERTEX_POINT ( 'NONE', #39219 ) ;
#47397 = CARTESIAN_POINT ( 'NONE',  ( 23.60581810200095276, -10.13726319729669001, 9.615401152371266136 ) ) ;
#47398 = CARTESIAN_POINT ( 'NONE',  ( 17.77476912162670430, 0.5854932480697117025, -13.88340087527083000 ) ) ;
#47399 = CARTESIAN_POINT ( 'NONE',  ( 11.57299956498156845, 5.207010770456999893, -7.825000000000000178 ) ) ;
#47400 = AXIS2_PLACEMENT_3D ( 'NONE', #43784, #54258, #54960 ) ;
#47401 = DIRECTION ( 'NONE',  ( 1.000000000000000000, 0.000000000000000000, 0.000000000000000000 ) ) ;
#47402 = DIRECTION ( 'NONE',  ( 1.000000000000000000, 0.000000000000000000, 0.000000000000000000 ) ) ;
#47403 = DIRECTION ( 'NONE',  ( -1.000000000000000000, 0.000000000000000000, 0.000000000000000000 ) ) ;
#47404 = EDGE_CURVE ( 'NONE', #40252, #46507, #18019, .T. ) ;
#47405 = CARTESIAN_POINT ( 'NONE',  ( 12.24414859480283901, 2.775896286417996794, 13.61101139974200791 ) ) ;
#47406 = ORIENTED_EDGE ( 'NONE', *, *, #66914, .T. ) ;
#47407 = CARTESIAN_POINT ( 'NONE',  ( 10.77879632507499785, -3.576455950783300253, -8.285174533868300273 ) ) ;
#47408 = ORIENTED_EDGE ( 'NONE', *, *, #33310, .F. ) ;
#47409 = CARTESIAN_POINT ( 'NONE',  ( 9.500006116823001889, 2.279680316922000127, 7.877692351087999256 ) ) ;
#47410 = CARTESIAN_POINT ( 'NONE',  ( 10.53197665877000055, 2.323713329709999886, -8.279493667389999700 ) ) ;
#47411 = CARTESIAN_POINT ( 'NONE',  ( 8.200000998245998929, 0.000000000000000000, 0.000000000000000000 ) ) ;
#47412 = CARTESIAN_POINT ( 'NONE',  ( 12.52583694058614938, 1.940453150098576662, -13.77633667721135602 ) ) ;
#47413 = LINE ( 'NONE', #42172, #14764 ) ;
#47414 = CARTESIAN_POINT ( 'NONE',  ( 17.98272759268933285, -0.4562271229319647681, 13.88993195058941410 ) ) ;
#47415 = CARTESIAN_POINT ( 'NONE',  ( 18.11245875488958390, 0.2828881520042535458, 13.89612849061349387 ) ) ;
#47416 = ORIENTED_EDGE ( 'NONE', *, *, #56671, .T. ) ;
#47417 = CARTESIAN_POINT ( 'NONE',  ( 12.61467092241713850, 0.5953860544200658689, 13.88283270324807184 ) ) ;
#47418 = CARTESIAN_POINT ( 'NONE',  ( 10.62841772631199966, -3.509411006705700053, 6.490165927606000196 ) ) ;
#47419 = CARTESIAN_POINT ( 'NONE',  ( 21.72233714749290101, 0.000000000000000000, 0.000000000000000000 ) ) ;
#47420 = DIRECTION ( 'NONE',  ( 0.000000000000000000, 0.8660254037844288266, -0.5000000000000169864 ) ) ;
#47421 = CARTESIAN_POINT ( 'NONE',  ( 9.362879440377000151, -3.677416446733000388, 9.250734868033999803 ) ) ;
#47423 = CARTESIAN_POINT ( 'NONE',  ( 23.89320776801300283, -3.288740538451999651, -12.20874841473999872 ) ) ;
#47422 = CARTESIAN_POINT ( 'NONE',  ( 9.882259685352000389, 4.932708901218999742, 6.390989635557000170 ) ) ;
#47424 = VECTOR ( 'NONE', #67472, 1000.000000000000227 ) ;
#47425 = CARTESIAN_POINT ( 'NONE',  ( 10.81764560330029923, 4.349570499512200428, -6.414140625063999401 ) ) ;
#47426 = CYLINDRICAL_SURFACE ( 'NONE', #1227, 2.000000000000000444 ) ;
#47427 = CARTESIAN_POINT ( 'NONE',  ( 9.070430433046999141, 3.262177192690499883, -7.044669955395099770 ) ) ;
#47428 = CARTESIAN_POINT ( 'NONE',  ( 18.17115522622102830, 0.3798658283128530377, 12.59428767283704786 ) ) ;
#47429 = CARTESIAN_POINT ( 'NONE',  ( 6.936163246431000573, 0.7133195303071999671, 1.381457696855000084 ) ) ;
#47430 = CARTESIAN_POINT ( 'NONE',  ( 18.41194552103540261, -3.255591973356615210, 12.09481971601743844 ) ) ;
#47431 = ORIENTED_EDGE ( 'NONE', *, *, #47353, .T. ) ;
#47432 = CARTESIAN_POINT ( 'NONE',  ( 8.829019353210000531, -5.290204991635000020, 8.768102264518001121 ) ) ;
#47433 = CARTESIAN_POINT ( 'NONE',  ( 8.449245559625000013, -5.458705123429999695, 7.456451825584000659 ) ) ;
#47434 = ADVANCED_FACE ( 'NONE', ( #13006 ), #29990, .F. ) ;
#47435 = EDGE_CURVE ( 'NONE', #40911, #18837, #30516, .T. ) ;
#47436 = CARTESIAN_POINT ( 'NONE',  ( 3.999971066382000284, 2.149963194831999935, 0.000000000000000000 ) ) ;
#47437 = CARTESIAN_POINT ( 'NONE',  ( 23.60000000000000142, -11.77655473258999841, -4.190794510628000680 ) ) ;
#47438 = EDGE_LOOP ( 'NONE', ( #65881, #36139, #15731, #57859 ) ) ;
#47439 = B_SPLINE_CURVE_WITH_KNOTS ( 'NONE', 3,
 ( #16700, #6208, #48876, #26518, #37008, #58324, #984, #10425, #22295, #63208, #69157, #31767, #36664, #57986, #21265, #10083 ),
 .UNSPECIFIED., .F., .F.,
 ( 4, 2, 2, 2, 2, 2, 2, 4 ),
 ( 0.000000000000000000, 0.06249999999999894529, 0.1249999999999978906, 0.2500000000000000000, 0.5000000000000008882, 0.7500000000000017764, 0.8750000000000008882, 1.000000000000000000 ),
 .UNSPECIFIED. ) ;
#47440 = CARTESIAN_POINT ( 'NONE',  ( 0.2471211125914999640, 1.200150369511000070, -3.152926066752000267 ) ) ;
#47441 = VECTOR ( 'NONE', #17560, 1000.000000000000000 ) ;
#47442 = CARTESIAN_POINT ( 'NONE',  ( 10.93479632507519916, 4.557787252275099732, 6.465962698293999722 ) ) ;
#47443 = CARTESIAN_POINT ( 'NONE',  ( 10.69829221958999987, 2.534027248431999890, -6.667786804432999759 ) ) ;
#47444 = ORIENTED_EDGE ( 'NONE', *, *, #6916, .F. ) ;
#47445 = CARTESIAN_POINT ( 'NONE',  ( 23.60001133530950668, -1.983597864821140026E-14, -13.89477126879791058 ) ) ;
#47446 = CARTESIAN_POINT ( 'NONE',  ( 9.213943921932887804, -5.010983041355907552, -6.200064497110663986 ) ) ;
#47447 = CARTESIAN_POINT ( 'NONE',  ( 10.30072469555899950, 4.570852684939899824, 8.487632181750699445 ) ) ;
#47448 = CARTESIAN_POINT ( 'NONE',  ( 9.924988015501654104, -5.349815781278972615, 7.500001845592777272 ) ) ;
#47449 = CARTESIAN_POINT ( 'NONE',  ( 11.37299956498129916, 2.792989229543000107, 7.825000000000000178 ) ) ;
#47450 = EDGE_LOOP ( 'NONE', ( #17926, #5322, #24842, #4306 ) ) ;
#47451 = CARTESIAN_POINT ( 'NONE',  ( 1.750973465873000068, -3.500000000000000000, 0.000000000000000000 ) ) ;
#47452 = CARTESIAN_POINT ( 'NONE',  ( 8.412214158772000516, 4.642843096736999797, -9.160097874508000615 ) ) ;
#47453 = EDGE_CURVE ( 'NONE', #33299, #62147, #55679, .T. ) ;
#47454 = CARTESIAN_POINT ( 'NONE',  ( 8.265659026604867066, -5.174540709378380399, 8.786794945891818642 ) ) ;
#47455 = CARTESIAN_POINT ( 'NONE',  ( 10.96914282210478042, -3.732132604854249802, -6.667932297870764913 ) ) ;
#47456 = EDGE_LOOP ( 'NONE', ( #26951, #21370, #23572, #32933 ) ) ;
#47457 = FACE_OUTER_BOUND ( 'NONE', #57903, .T. ) ;
#47458 = CARTESIAN_POINT ( 'NONE',  ( 11.26375800691000073, 11.80847110903000186, 1.384521730739000089 ) ) ;
#47459 = VERTEX_POINT ( 'NONE', #7751 ) ;
#47460 = EDGE_CURVE ( 'NONE', #40087, #23714, #19939, .T. ) ;
#47461 = CARTESIAN_POINT ( 'NONE',  ( 11.50029455687000102, -11.56505190006999939, -1.404305717648999918 ) ) ;
#47462 = CARTESIAN_POINT ( 'NONE',  ( 18.50001572531400029, -2.908166856580999937, 12.18270046149000052 ) ) ;
#47463 = VERTEX_POINT ( 'NONE', #39567 ) ;
#47464 = CARTESIAN_POINT ( 'NONE',  ( 18.09667340657836476, 0.3125520594525350027, -13.89528657259774391 ) ) ;
#47465 = CARTESIAN_POINT ( 'NONE',  ( 10.31021345716899873, 4.636538040886300394, -8.078719053813800954 ) ) ;
#47466 = CARTESIAN_POINT ( 'NONE',  ( 8.845310841232000953, 5.851083642416999631, -7.072167224702999633 ) ) ;
#47467 = CARTESIAN_POINT ( 'NONE',  ( 11.56322412107030928, 4.054600656575539475, -6.467939235001000320 ) ) ;
#47468 = CARTESIAN_POINT ( 'NONE',  ( 11.31013259637009938, -5.031671030421000168, 6.937848198857199833 ) ) ;
#47469 = CARTESIAN_POINT ( 'NONE',  ( 12.54002611783803012, 3.066051210233499802, -12.30150130090889427 ) ) ;
#47470 = CARTESIAN_POINT ( 'NONE',  ( 11.90425819896749893, -5.255890247626999745, 7.263238376356399684 ) ) ;
#47471 = VERTEX_POINT ( 'NONE', #60891 ) ;
#47472 = CARTESIAN_POINT ( 'NONE',  ( 9.160308886257000793, 4.122021000979000149, 9.013569734175000292 ) ) ;
#47473 = ORIENTED_EDGE ( 'NONE', *, *, #2833, .F. ) ;
#47474 = CARTESIAN_POINT ( 'NONE',  ( 9.427263540183332680, 3.370476274536375438, -8.592232985442821658 ) ) ;
#47475 = CARTESIAN_POINT ( 'NONE',  ( 8.738433059624998833, -5.414909314743000301, 8.890670256079998168 ) ) ;
#47476 = CARTESIAN_POINT ( 'NONE',  ( 24.53429011008099891, 3.614318944477000084, -12.31267538233000103 ) ) ;
#47477 = VERTEX_POINT ( 'NONE', #39919 ) ;
#47478 = B_SPLINE_SURFACE_WITH_KNOTS ( 'NONE', 3, 3, ( 
 ( #49644, #1751, #44421, #60483, #12592, #33920, #34177, #45012, #29281, #29635, #28590, #45355, #2011, #18439, #17751, #39414, #28944, #50249, #6899, #61083, #2351, #66664, #18783, #7595, #34863, #12848, #33832, #7944, #23333, #23674, #13544, #1315, #39765, #28235, #38724 ),
 ( #13203, #43976, #60734, #22631, #50595, #17395, #60046, #44674, #65282, #65967, #34531, #12156, #18096, #22980, #33487, #24020, #55840, #2697, #66316, #65626, #40114, #56179, #61428, #54799, #8290, #39071, #49550, #1663, #44328, #60394, #12498, #55146, #7249, #49902, #55495 ),
 ( #63123, #51953, #68033, #4054, #35552, #51615, #19461, #9648, #14569, #25740, #46380, #36229, #25389, #4401, #57200, #47069, #35212, #57544, #29977, #19115, #45697, #35885, #46727, #30995, #9996, #8968, #68371, #3711, #20148, #67340, #19808, #9303, #30644, #56524, #41476 ),
 ( #62784, #30307, #25048, #40437, #14906, #52304, #20491, #41816, #67682, #15251, #36572, #57898, #50937, #40782, #3035, #24366, #67006, #41137, #61763, #13882, #8628, #51279, #62447, #3374, #24711, #46035, #62107, #14226, #56870, #59614, #54019, #16618, #64498, #32372, #26432 ) ),
 .UNSPECIFIED., .F., .F., .F.,
 ( 4, 4 ),
 ( 4, 1, 1, 1, 1, 1, 1, 1, 1, 1, 1, 1, 1, 1, 1, 1, 1, 1, 1, 1, 1, 1, 1, 1, 1, 1, 1, 1, 1, 1, 1, 1, 4 ),
 ( -0.1039370721279000015, 1.103937072127999963 ),
 ( -0.01758190005605000245, 0.01098868753504999955, 0.03955927512614999808, 0.06812986271724999487, 0.09670045030835000555, 0.1252710378995000040, 0.1538416254905999869, 0.1824122130816999976, 0.2109828006727999805, 0.2395533882639000189, 0.2681239758550000296, 0.2966945634461000125, 0.3252651510371999954, 0.3538357386283000339, 0.3824063262194000168, 0.4109769138104999997, 0.4395475014015999826, 0.4681180889926999655, 0.4966886765838000040, 0.5252592641748999869, 0.5538298517660000808, 0.5824004393571000637, 0.6109710269481999356, 0.6395416145393000296, 0.6681122021304000125, 0.6966827897214999954, 0.7252533773125999783, 0.7538239649036999612, 0.7823945524947999441, 0.8109651400858999271, 0.8395357276770000210, 0.8681063152681000039, 0.8966769028592000979 ),
 .UNSPECIFIED. ) ;
#47479 = CARTESIAN_POINT ( 'NONE',  ( 12.21010952511930903, -2.691762936255614580, -12.40482162467503890 ) ) ;
#47480 = CARTESIAN_POINT ( 'NONE',  ( 10.35410941423799791, 4.742797679580299963, 8.174686939644999484 ) ) ;
#47481 = CARTESIAN_POINT ( 'NONE',  ( 18.22968849645936729, 3.214251582955409692, 11.19784508593241235 ) ) ;
#47482 = CARTESIAN_POINT ( 'NONE',  ( 9.020964430773000586, 2.907392932634000005, 6.146188468825999784 ) ) ;
#47483 = CARTESIAN_POINT ( 'NONE',  ( 23.56664678325900297, -13.31363270032999857, -4.296980171176000063 ) ) ;
#47484 = CARTESIAN_POINT ( 'NONE',  ( 12.21441178144108619, -2.942030139115490606, -13.68739795509152479 ) ) ;
#47485 = CARTESIAN_POINT ( 'NONE',  ( 10.94903032197929882, -3.496160833528699996, -6.795411691360399686 ) ) ;
#47486 = CARTESIAN_POINT ( 'NONE',  ( 4.599999999999999645, -14.00000000000000000, 1.714505518806294638E-15 ) ) ;
#47487 = CARTESIAN_POINT ( 'NONE',  ( 17.85685707441191639, -3.134587784889875106, 12.20386770240991403 ) ) ;
#47488 = ORIENTED_EDGE ( 'NONE', *, *, #58104, .T. ) ;
#47489 = ORIENTED_EDGE ( 'NONE', *, *, #14872, .T. ) ;
#47490 = DIRECTION ( 'NONE',  ( 1.000000000000000000, 0.000000000000000000, 0.000000000000000000 ) ) ;
#47491 = CARTESIAN_POINT ( 'NONE',  ( 11.85565467195930367, -5.136173005413449566, 8.088082908809450799 ) ) ;
#47492 = CARTESIAN_POINT ( 'NONE',  ( 4.900006121741999010, 0.2617993877991516283, 1.999999999999999112 ) ) ;
#47493 = CARTESIAN_POINT ( 'NONE',  ( 11.06133897141000055, 2.503910831767000023, -6.712778933675999760 ) ) ;
#47494 = CARTESIAN_POINT ( 'NONE',  ( 11.04384236319999957, -1.500234901393999731, -5.035088906224999938 ) ) ;
#47495 = AXIS2_PLACEMENT_3D ( 'NONE', #32697, #43877, #884 ) ;
#47496 = CARTESIAN_POINT ( 'NONE',  ( 17.59673268120277356, 3.123957167259608259, 12.28404855389177719 ) ) ;
#47497 = PRODUCT_RELATED_PRODUCT_CATEGORY ( 'part', '', ( #3696 ) ) ;
#47498 = CARTESIAN_POINT ( 'NONE',  ( 23.55671020924400239, -13.49865072242999986, 4.025359669029000109 ) ) ;
#47499 = CARTESIAN_POINT ( 'NONE',  ( 10.56491664109999995, 4.212242527248999835, 8.933458498617000032 ) ) ;
#47500 = B_SPLINE_CURVE_WITH_KNOTS ( 'NONE', 3,
 ( #60578, #54642, #44854, #6735, #65463, #1850 ),
 .UNSPECIFIED., .F., .F.,
 ( 4, 2, 4 ),
 ( 0.000000000000000000, 0.5000000000000000000, 1.000000000000000000 ),
 .UNSPECIFIED. ) ;
#47501 = ORIENTED_EDGE ( 'NONE', *, *, #41706, .T. ) ;
#47502 = CARTESIAN_POINT ( 'NONE',  ( 8.616332388160998335, -5.167567399848000065, -6.822293593032000558 ) ) ;
#47503 = ORIENTED_EDGE ( 'NONE', *, *, #50328, .T. ) ;
#47504 = CARTESIAN_POINT ( 'NONE',  ( 12.26301939624444870, -2.811829068737872639, 12.37346575716766672 ) ) ;
#47505 = CARTESIAN_POINT ( 'NONE',  ( 23.66004879239100234, -9.998910854163000295, -9.691527647852998584 ) ) ;
#47506 = CARTESIAN_POINT ( 'NONE',  ( 9.520797373037000355, 3.270552986600999912, 5.711478154812000163 ) ) ;
#47507 = CARTESIAN_POINT ( 'NONE',  ( 11.73589666366019912, -4.039600775206940497, 6.608753462694600067 ) ) ;
#47508 = CARTESIAN_POINT ( 'NONE',  ( 7.100000000000000533, 5.221516520829000640, -8.074802043613001246 ) ) ;
#47509 = CARTESIAN_POINT ( 'NONE',  ( 11.56441235500451015, 3.361299021099800388, -6.914884925939399629 ) ) ;
#47510 = CARTESIAN_POINT ( 'NONE',  ( 10.93656785386839836, 2.939720539848000413, -8.213529149347399638 ) ) ;
#47511 = CARTESIAN_POINT ( 'NONE',  ( 12.33468944037056225, -0.4116921281473252536, 12.69102089861179294 ) ) ;
#47512 = CARTESIAN_POINT ( 'NONE',  ( 5.642739276337546350, -12.09235441392642052, -3.739144582074775958 ) ) ;
#47513 = LINE ( 'NONE', #68819, #59548 ) ;
#47514 = CARTESIAN_POINT ( 'NONE',  ( 21.49999863197000138, 0.000000000000000000, 0.000000000000000000 ) ) ;
#47515 = ORIENTED_EDGE ( 'NONE', *, *, #26522, .T. ) ;
#47516 = CARTESIAN_POINT ( 'NONE',  ( 9.825045280412000537, 3.116293075258000478, -6.208411413796000033 ) ) ;
#47517 = CARTESIAN_POINT ( 'NONE',  ( 10.07503300763299947, 4.881889043637199777, -8.424978748982498544 ) ) ;
#47518 = EDGE_CURVE ( 'NONE', #49517, #44553, #29093, .T. ) ;
#47519 = EDGE_CURVE ( 'NONE', #59694, #15201, #22071, .T. ) ;
#47520 = CARTESIAN_POINT ( 'NONE',  ( 24.30001694391200218, -12.21047201246000036, 3.271805662802000025 ) ) ;
#47521 = CARTESIAN_POINT ( 'NONE',  ( 18.29999999997147242, 11.00695868226823215, -3.817556993356255202 ) ) ;
#47522 = FACE_OUTER_BOUND ( 'NONE', #62535, .T. ) ;
#47523 = CARTESIAN_POINT ( 'NONE',  ( 11.38379707368349969, -4.566644629509899467, -6.509947486183500054 ) ) ;
#47524 = VERTEX_POINT ( 'NONE', #24171 ) ;
#47525 = CIRCLE ( 'NONE', #14045, 2.200000000000001954 ) ;
#47526 = B_SPLINE_CURVE_WITH_KNOTS ( 'NONE', 3,
 ( #68657, #63756, #31616, #32648 ),
 .UNSPECIFIED., .F., .F.,
 ( 4, 4 ),
 ( 0.000000000000000000, 1.000000000000000000 ),
 .UNSPECIFIED. ) ;
#47527 = B_SPLINE_CURVE_WITH_KNOTS ( 'NONE', 3,
 ( #10537, #47264, #36774, #9500, #43045 ),
 .UNSPECIFIED., .F., .F.,
 ( 4, 1, 4 ),
 ( 0.000000000000000000, 0.5000000000000000000, 1.000000000000000000 ),
 .UNSPECIFIED. ) ;
#47528 = CARTESIAN_POINT ( 'NONE',  ( 11.36486084871759950, 2.792989229543000107, -7.825000000000000178 ) ) ;
#47529 = CARTESIAN_POINT ( 'NONE',  ( 8.464260841230998977, 2.029098103856999735, 7.726995416028000108 ) ) ;
#47530 = VECTOR ( 'NONE', #4944, 1000.000000000000000 ) ;
#47532 = CARTESIAN_POINT ( 'NONE',  ( 11.59999999999999964, 3.182579051151299687, 7.825000000000000178 ) ) ;
#47531 = FACE_OUTER_BOUND ( 'NONE', #45313, .T. ) ;
#47533 = PLANE ( 'NONE',  #49189 ) ;
#47534 = ORIENTED_EDGE ( 'NONE', *, *, #20539, .F. ) ;
#47535 = CARTESIAN_POINT ( 'NONE',  ( 10.76010575649000067, 4.535386075958999896, 6.001721352166000223 ) ) ;
#47536 = CARTESIAN_POINT ( 'NONE',  ( 18.11732105061185649, -2.226901518982100203, -13.72755281718820797 ) ) ;
#47537 = CARTESIAN_POINT ( 'NONE',  ( 11.29364426047339975, 4.466097552695299733, 6.769896129503799820 ) ) ;
#47538 = CARTESIAN_POINT ( 'NONE',  ( 9.514108112060000622, -4.887639888682999256, 8.462756667353000140 ) ) ;
#47539 = CARTESIAN_POINT ( 'NONE',  ( 9.117519353207999444, -4.954907757874000396, 8.825780921426000347 ) ) ;
#47540 = ORIENTED_EDGE ( 'NONE', *, *, #66686, .F. ) ;
#47541 = CARTESIAN_POINT ( 'NONE',  ( 7.775614158771000817, 4.636729845879000500, 9.378977473003999421 ) ) ;
#47543 = CARTESIAN_POINT ( 'NONE',  ( 11.05675868674000029, 5.188533356467999624, 4.847347870993000463 ) ) ;
#47542 = CARTESIAN_POINT ( 'NONE',  ( 27.64127793187000037, 5.599999999999999645, -6.571291218949999902 ) ) ;
#47544 = B_SPLINE_CURVE_WITH_KNOTS ( 'NONE', 3,
 ( #16627, #37953, #59273, #22559, #38646, #59970, #12078, #33411, #51541, #67608, #40708, #50864, #3637, #40039, #3304, #24638 ),
 .UNSPECIFIED., .F., .F.,
 ( 4, 2, 2, 2, 1, 2, 1, 2, 4 ),
 ( 0.3333669949959171541, 0.4166961206214276348, 0.5000252462469381154, 0.5833543718724485405, 0.6666834974979589656, 0.7500126231234691687, 0.8333417487489794828, 0.9166708743744896859, 1.000000000000000000 ),
 .UNSPECIFIED. ) ;
#47545 = CARTESIAN_POINT ( 'NONE',  ( 7.575903374750492247, -4.040870700566189022, 5.761292496191131818 ) ) ;
#47546 = CARTESIAN_POINT ( 'NONE',  ( 18.12548987800779088, -0.2560590259945930147, 13.89684012171511540 ) ) ;
#47548 = CARTESIAN_POINT ( 'NONE',  ( 23.73547087796200117, 3.554272179136999998, 13.41695213092000039 ) ) ;
#47547 = CONICAL_SURFACE ( 'NONE', #18503, 1.600003888856000200, 0.7854004771980920285 ) ;
#47549 = EDGE_LOOP ( 'NONE', ( #30466, #62570, #64960, #49030 ) ) ;
#47550 = CARTESIAN_POINT ( 'NONE',  ( 5.782109839683332808, 0.9218200799623742503, -1.199500263597268912 ) ) ;
#47551 = CARTESIAN_POINT ( 'NONE',  ( 11.24795391537420031, -3.169881940022800215, 6.936213817702099327 ) ) ;
#47552 = EDGE_CURVE ( 'NONE', #17060, #7930, #65691, .T. ) ;
#47553 = CARTESIAN_POINT ( 'NONE',  ( 11.00366064676999933, 2.264078662261999941, 7.798351372501000078 ) ) ;
#47554 = AXIS2_PLACEMENT_3D ( 'NONE', #45318, #60351, #60695 ) ;
#47555 = CARTESIAN_POINT ( 'NONE',  ( 11.01456785386839954, 3.053605396817899997, 6.863111178199799767 ) ) ;
#47556 = ORIENTED_EDGE ( 'NONE', *, *, #42442, .T. ) ;
#47557 = CARTESIAN_POINT ( 'NONE',  ( 23.61437543478880485, -3.070577605751717787, 13.52804441183152484 ) ) ;
#47558 = CARTESIAN_POINT ( 'NONE',  ( 12.27226887596751759, 1.991660198615914590, -12.44160671058018863 ) ) ;
#47559 = CARTESIAN_POINT ( 'NONE',  ( 11.31013259637009938, -5.031671030421000168, 6.937848198857199833 ) ) ;
#47560 = B_SPLINE_CURVE_WITH_KNOTS ( 'NONE', 3,
 ( #28770, #54631, #55677, #64755, #7775, #38197, #39244, #44846, #28418 ),
 .UNSPECIFIED., .F., .F.,
 ( 4, 1, 1, 1, 1, 1, 4 ),
 ( 0.1253844953241992632, 0.1696563387730770645, 0.3365447927375280202, 0.5034332467025710578, 0.6703217006676136513, 0.8372101546320646070, 0.8746253901980668433 ),
 .UNSPECIFIED. ) ;
#47561 = CARTESIAN_POINT ( 'NONE',  ( 24.30000000000000071, -2.548720605937000006, 12.21654710926000220 ) ) ;
#47562 = CARTESIAN_POINT ( 'NONE',  ( 18.14661026973002933, -2.095745652224531685, 13.84225217829565580 ) ) ;
#47563 = CARTESIAN_POINT ( 'NONE',  ( 18.17918907329175227, 2.539311109804731181, -13.66506621000817212 ) ) ;
#47564 = ORIENTED_EDGE ( 'NONE', *, *, #32749, .F. ) ;
#47565 = CARTESIAN_POINT ( 'NONE',  ( 10.92028665956053324, 3.257584962274628460, 6.450604656432373574 ) ) ;
#47566 = DIRECTION ( 'NONE',  ( -1.000000000000000000, 0.000000000000000000, 0.000000000000000000 ) ) ;
#47567 = ORIENTED_EDGE ( 'NONE', *, *, #39227, .T. ) ;
#47568 = CARTESIAN_POINT ( 'NONE',  ( 8.435394291146250723, 3.652552720689497878, 6.005833249671993279 ) ) ;
#47569 = CARTESIAN_POINT ( 'NONE',  ( 11.12133729122639991, 3.134101783108900197, 7.522778681411049995 ) ) ;
#47570 = CARTESIAN_POINT ( 'NONE',  ( 6.633333333559363609, -12.50865242394284493, 2.924692581576780803 ) ) ;
#47571 = CARTESIAN_POINT ( 'NONE',  ( 10.42081182385000027, 2.488452444780999695, -7.717895019962999648 ) ) ;
#47572 = CARTESIAN_POINT ( 'NONE',  ( 8.354426260476000010, 5.125517035499999707, 6.367235573876004473 ) ) ;
#47573 = CARTESIAN_POINT ( 'NONE',  ( 9.409421956854998825, -2.113407700033000047, 7.914197133433000353 ) ) ;
#47574 = CARTESIAN_POINT ( 'NONE',  ( 18.05074276561662572, 0.3808128809978812979, -12.69231869260113754 ) ) ;
#47575 = CARTESIAN_POINT ( 'NONE',  ( 12.24260341322176870, 2.772876882482055994, -12.38382274644487602 ) ) ;
#47576 = CARTESIAN_POINT ( 'NONE',  ( 10.99410672858429905, -4.801902424331299990, -6.896755974168000236 ) ) ;
#47577 = CARTESIAN_POINT ( 'NONE',  ( 9.304732780410999382, 5.284130523641000110, 6.489275570566000795 ) ) ;
#47578 = VERTEX_POINT ( 'NONE', #66820 ) ;
#47579 = CARTESIAN_POINT ( 'NONE',  ( 11.09999999999999787, 2.311256224650723556, -7.128998340778534448 ) ) ;
#47580 = CARTESIAN_POINT ( 'NONE',  ( 11.09999999999999964, 4.000000000000000000, -7.500000000000000000 ) ) ;
#47581 = LINE ( 'NONE', #21341, #23581 ) ;
#47582 = AXIS2_PLACEMENT_3D ( 'NONE', #66170, #3235, #34719 ) ;
#47583 = LINE ( 'NONE', #68888, #45092 ) ;
#47584 = EDGE_CURVE ( 'NONE', #49775, #32306, #59011, .T. ) ;
#47585 = CARTESIAN_POINT ( 'NONE',  ( 17.80000000005199823, 3.345268251980999974, 11.86064071431999878 ) ) ;
#47586 = EDGE_CURVE ( 'NONE', #56864, #23992, #1814, .T. ) ;
#47587 = CARTESIAN_POINT ( 'NONE',  ( 11.01769844498000062, 7.854486692293001227, 6.517457990503000786 ) ) ;
#47588 = CARTESIAN_POINT ( 'NONE',  ( 12.40587394967876556, -0.4809228688773738991, -12.68774147671740415 ) ) ;
#47589 = DIRECTION ( 'NONE',  ( 1.000000000000000000, 0.000000000000000000, 0.000000000000000000 ) ) ;
#47590 = ORIENTED_EDGE ( 'NONE', *, *, #24535, .F. ) ;
#47591 = CARTESIAN_POINT ( 'NONE',  ( 24.51228084553499897, 8.787217699239999291, 8.912727655930000381 ) ) ;
#47592 = CARTESIAN_POINT ( 'NONE',  ( 10.44222949779799947, -3.366547096154099972, -8.449985803660998940 ) ) ;
#47593 = DIRECTION ( 'NONE',  ( 0.000000000000000000, 0.000000000000000000, -1.000000000000000000 ) ) ;
#47594 = CARTESIAN_POINT ( 'NONE',  ( 9.137549407199999862, -2.995696424181999884, 8.544763501938000161 ) ) ;
#47595 = CARTESIAN_POINT ( 'NONE',  ( 11.42441504065829960, -3.305585767322499979, 8.017771632862299214 ) ) ;
#47596 = CARTESIAN_POINT ( 'NONE',  ( 12.38296014331787553, 0.5849390254007664769, 12.58641711472857594 ) ) ;
#47597 = CARTESIAN_POINT ( 'NONE',  ( 0.6885616966234999747, 3.123219710863000209, -0.8105742342224000474 ) ) ;
#47598 = DIRECTION ( 'NONE',  ( 0.000000000000000000, 0.000000000000000000, -1.000000000000000000 ) ) ;
#47599 = CARTESIAN_POINT ( 'NONE',  ( 12.33234491188476767, 1.934664193338946792, 12.45058764867823164 ) ) ;
#47600 = CARTESIAN_POINT ( 'NONE',  ( 9.575903104272999400, -2.330665094450000030, -8.349943402163999551 ) ) ;
#47601 = CARTESIAN_POINT ( 'NONE',  ( 10.50180110216399854, 3.143606124884799957, -6.976989117212499814 ) ) ;
#47602 = CARTESIAN_POINT ( 'NONE',  ( 7.607791299150002295, 3.471796661068001999, -6.504286038290998384 ) ) ;
#47603 = ADVANCED_FACE ( 'NONE', ( #3193 ), #24520, .T. ) ;
#47604 = CARTESIAN_POINT ( 'NONE',  ( 10.15335165876999923, 3.144981324235999853, -5.860948306964999688 ) ) ;
#47605 = CARTESIAN_POINT ( 'NONE',  ( 9.934583761885999564, 2.921249888908000081, -8.187519150726398465 ) ) ;
#47607 = CARTESIAN_POINT ( 'NONE',  ( 12.80505043854143388, 3.124999999999999556, 12.28373071562070074 ) ) ;
#47606 = CARTESIAN_POINT ( 'NONE',  ( 9.065735834902588053, -3.588654020114534049, -8.662764376609992212 ) ) ;
#47608 = CARTESIAN_POINT ( 'NONE',  ( 8.795853127542962113, 4.029789221522053211, 6.554146822010631368 ) ) ;
#47609 = ORIENTED_EDGE ( 'NONE', *, *, #21909, .F. ) ;
#47610 = EDGE_CURVE ( 'NONE', #27264, #6697, #39683, .T. ) ;
#47611 = CARTESIAN_POINT ( 'NONE',  ( 23.60000000000000142, 9.517611874540000017, -8.103398312166000039 ) ) ;
#47612 = CARTESIAN_POINT ( 'NONE',  ( 9.136976429976831682, 5.100000000000000533, 6.167827406374086330 ) ) ;
#47613 = CARTESIAN_POINT ( 'NONE',  ( 9.432439766855527097, 4.712051993706990238, -9.127118574761283298 ) ) ;
#47614 = CARTESIAN_POINT ( 'NONE',  ( 8.819151519676999840, 4.021721698617580110, 6.495824366094999469 ) ) ;
#47615 = CARTESIAN_POINT ( 'NONE',  ( 7.000000000000000000, 1.250000000000000000, 0.000000000000000000 ) ) ;
#47616 = CARTESIAN_POINT ( 'NONE',  ( 12.31461592258506421, -2.887558836668430828, 13.58358613427759032 ) ) ;
#47617 = CARTESIAN_POINT ( 'NONE',  ( 12.19454236369542244, 2.633904202154401908, 13.64409272134985862 ) ) ;
#47618 = CARTESIAN_POINT ( 'NONE',  ( 8.157224700651678262, 3.176774960111513835, 6.225205742771084516 ) ) ;
#47619 = ORIENTED_EDGE ( 'NONE', *, *, #29634, .T. ) ;
#47620 = CARTESIAN_POINT ( 'NONE',  ( 4.774325709868000089, 0.05965109778420000369, 1.274055334230000058 ) ) ;
#47621 = CARTESIAN_POINT ( 'NONE',  ( 8.499265421555000088, -4.240073379563900069, -8.741861511046000288 ) ) ;
#47622 = VECTOR ( 'NONE', #37063, 1000.000000000000114 ) ;
#47623 = FACE_OUTER_BOUND ( 'NONE', #39783, .T. ) ;
#47624 = CARTESIAN_POINT ( 'NONE',  ( 25.59994555223599733, -2.024003533649000097, 11.01554633311000053 ) ) ;
#47625 = ADVANCED_FACE ( 'NONE', ( #3523 ), #16636, .F. ) ;
#47626 = CARTESIAN_POINT ( 'NONE',  ( 18.18008862603425158, 2.492635669256734854, -12.45330984115723361 ) ) ;
#47627 = CARTESIAN_POINT ( 'NONE',  ( 23.60000000000000142, -2.548720605937000006, 12.21654710926000220 ) ) ;
#47628 = CIRCLE ( 'NONE', #30858, 0.2999999999999993228 ) ;
#47629 = CARTESIAN_POINT ( 'NONE',  ( 17.93744643711270115, 2.994789699037250230, 12.32241545780499159 ) ) ;
#47630 = CARTESIAN_POINT ( 'NONE',  ( 17.60475804966352342, 1.787836225788080879, 13.88537509868915087 ) ) ;
#47631 = DIRECTION ( 'NONE',  ( 1.000000000000000000, 0.000000000000000000, 0.000000000000000000 ) ) ;
#47632 = CARTESIAN_POINT ( 'NONE',  ( 10.83488305961999920, -5.800181157098999840, -7.920538492179999501 ) ) ;
#47633 = CARTESIAN_POINT ( 'NONE',  ( 9.070134780760179538, -3.647129767632641517, 8.851447081754429291 ) ) ;
#47634 = CARTESIAN_POINT ( 'NONE',  ( 7.883148997456999929, -5.167567567567999731, 6.822293592207000934 ) ) ;
#47635 = CARTESIAN_POINT ( 'NONE',  ( 24.53002386606100060, 12.09082868768999930, 3.147845687315999896 ) ) ;
#47636 = CARTESIAN_POINT ( 'NONE',  ( 11.09999999999999964, 7.355239926129000239, 6.360395311517000216 ) ) ;
#47637 = CARTESIAN_POINT ( 'NONE',  ( -0.2999999999999999889, 0.000000000000000000, 0.000000000000000000 ) ) ;
#47638 = B_SPLINE_CURVE_WITH_KNOTS ( 'NONE', 3,
 ( #2487, #23117, #61905, #1801 ),
 .UNSPECIFIED., .F., .F.,
 ( 4, 4 ),
 ( 0.000000000000000000, 0.05661757269142905086 ),
 .UNSPECIFIED. ) ;
#47639 = ORIENTED_EDGE ( 'NONE', *, *, #68611, .T. ) ;
#47640 = CARTESIAN_POINT ( 'NONE',  ( 9.798945280410000791, 5.639765292528999829, -8.059103558718000215 ) ) ;
#47641 = CARTESIAN_POINT ( 'NONE',  ( 11.39979975933730039, -3.180925410802600162, 7.781807394638899922 ) ) ;
#47642 = VERTEX_POINT ( 'NONE', #39022 ) ;
#47643 = CARTESIAN_POINT ( 'NONE',  ( 13.69996357384220609, 12.28513767539633861, 2.441259368857655154 ) ) ;
#47644 = CARTESIAN_POINT ( 'NONE',  ( 10.57149279008999798, -4.296686446741600385, -8.601484120896000007 ) ) ;
#47645 = ORIENTED_EDGE ( 'NONE', *, *, #4519, .T. ) ;
#47646 = CARTESIAN_POINT ( 'NONE',  ( 10.63880513895979973, 5.150451045932999961, 8.139542779846600240 ) ) ;
#47647 = CARTESIAN_POINT ( 'NONE',  ( 18.36030550606429657, 3.088870463281629064, -11.23311224736100833 ) ) ;
#47648 = CARTESIAN_POINT ( 'NONE',  ( 9.996463691907599980, -5.100000000000000533, -6.665341197393335193 ) ) ;
#47649 = CARTESIAN_POINT ( 'NONE',  ( 17.55505043854144276, 0.000000000000000000, -25.00000000000000000 ) ) ;
#47650 = CARTESIAN_POINT ( 'NONE',  ( 12.29893553432339282, 0.3669576687960916517, -13.89348614081305655 ) ) ;
#47651 = CARTESIAN_POINT ( 'NONE',  ( 9.591433907306443629, -3.054280487670652189, 6.668243572402049679 ) ) ;
#47652 = CARTESIAN_POINT ( 'NONE',  ( 13.43176382712000105, 11.67665677335000041, 2.247227628037000269 ) ) ;
#47653 = VERTEX_POINT ( 'NONE', #18044 ) ;
#47654 = CARTESIAN_POINT ( 'NONE',  ( 8.548770280408998445, 5.203550244299999683, -8.391678825488000371 ) ) ;
#47655 = VERTEX_POINT ( 'NONE', #45646 ) ;
#47656 = LINE ( 'NONE', #32608, #51535 ) ;
#47657 = VERTEX_POINT ( 'NONE', #1959 ) ;
#47658 = CARTESIAN_POINT ( 'NONE',  ( 9.073392757686999488, 4.863450031739999346, 6.556157624301499176 ) ) ;
#47659 = CARTESIAN_POINT ( 'NONE',  ( 17.81536569913638601, -3.068232145164245583, -12.30083422255797565 ) ) ;
#47660 = B_SPLINE_CURVE_WITH_KNOTS ( 'NONE', 3,
 ( #387, #43038, #50614, #66682 ),
 .UNSPECIFIED., .F., .F.,
 ( 4, 4 ),
 ( 0.000000000000000000, 1.000000000000000000 ),
 .UNSPECIFIED. ) ;
#47661 = DIRECTION ( 'NONE',  ( 1.000000000000000000, 0.000000000000000000, 0.000000000000000000 ) ) ;
#47662 = ADVANCED_FACE ( 'NONE', ( #23282 ), #20914, .F. ) ;
#47663 = EDGE_CURVE ( 'NONE', #5496, #16917, #32127, .T. ) ;
#47664 = DIRECTION ( 'NONE',  ( 0.000000000000000000, 0.2461538461537955136, -0.9692307692307821076 ) ) ;
#47665 = ADVANCED_FACE ( 'NONE', ( #58182 ), #56777, .T. ) ;
#47666 = CARTESIAN_POINT ( 'NONE',  ( 9.009273505393998960, -8.692577137281000788, -6.276257937540999698 ) ) ;
#47667 = VERTEX_POINT ( 'NONE', #4683 ) ;
#47668 = CARTESIAN_POINT ( 'NONE',  ( 12.79272103475300071, 12.16747052068999935, -3.133256626080000107 ) ) ;
#47669 = CARTESIAN_POINT ( 'NONE',  ( 18.07302322422999907, 11.50538345640999971, -4.553133914476999777 ) ) ;
#47670 = B_SPLINE_CURVE_WITH_KNOTS ( 'NONE', 3,
 ( #68537, #67855, #58067, #53162 ),
 .UNSPECIFIED., .F., .F.,
 ( 4, 4 ),
 ( 0.8747102523717062983, 1.000000000000000000 ),
 .UNSPECIFIED. ) ;
#47671 = CARTESIAN_POINT ( 'NONE',  ( 8.428197172116432156, -5.125396288428772706, 6.749639981086941631 ) ) ;
#47672 = CARTESIAN_POINT ( 'NONE',  ( 18.29983863916000075, -2.861762957209999847, 11.98830831200999825 ) ) ;
#47673 = AXIS2_PLACEMENT_3D ( 'NONE', #66848, #3896, #62295 ) ;
#47674 = CARTESIAN_POINT ( 'NONE',  ( 12.37336427446135367, -11.82897199538900068, 3.432444870275719762 ) ) ;
#47675 = CONICAL_SURFACE ( 'NONE', #6332, 0.9346783463124002100, 0.7853981908209605178 ) ;
#47676 = CARTESIAN_POINT ( 'NONE',  ( 17.71545033449769235, 12.11985731843603098, -3.159854994125695704 ) ) ;
#47677 = CARTESIAN_POINT ( 'NONE',  ( 10.93146935944000120, -2.472881306517999978, -7.514158774805000718 ) ) ;
#47678 = ORIENTED_EDGE ( 'NONE', *, *, #68496, .F. ) ;
#47679 = ORIENTED_EDGE ( 'NONE', *, *, #43929, .T. ) ;
#47680 = FACE_OUTER_BOUND ( 'NONE', #26206, .T. ) ;
#47681 = CONICAL_SURFACE ( 'NONE', #51027, 13.94999927503000059, 0.7853981058017837080 ) ;
#47682 = LINE ( 'NONE', #57463, #51178 ) ;
#47683 = CARTESIAN_POINT ( 'NONE',  ( 1.186390132541125020, -0.4581489286485234680, 3.499999999999998668 ) ) ;
#47684 = CARTESIAN_POINT ( 'NONE',  ( 5.959193173016666734, 0.3926218265389159190, 1.460959015002474715 ) ) ;
#47685 = CARTESIAN_POINT ( 'NONE',  ( 10.59725056272499977, 5.316133253199000208, -7.519505747156228992 ) ) ;
#47686 = CARTESIAN_POINT ( 'NONE',  ( 8.800809814040999157, 4.530359890157599878, -8.185876144228299012 ) ) ;
#47688 = CARTESIAN_POINT ( 'NONE',  ( 10.27190963261000078, -3.431500491711999778, 4.846768348291999651 ) ) ;
#47687 = CARTESIAN_POINT ( 'NONE',  ( 10.63626717315599990, -4.764472860199700399, 8.151477970733999712 ) ) ;
#47689 = DIRECTION ( 'NONE',  ( 0.000000000000000000, -1.000000000000000000, 0.000000000000000000 ) ) ;
#47690 = ORIENTED_EDGE ( 'NONE', *, *, #45887, .T. ) ;
#47691 = CARTESIAN_POINT ( 'NONE',  ( 1.433329478674677748, 2.750000000000000000, 7.763105750930175534E-10 ) ) ;
#47692 = CARTESIAN_POINT ( 'NONE',  ( 8.268606633798000871, -2.876811830795998670, 6.331441650266997456 ) ) ;
#47693 = CARTESIAN_POINT ( 'NONE',  ( 9.557721904870000174, 5.115452802765999785, 6.873781641694999500 ) ) ;
#47694 = DIRECTION ( 'NONE',  ( 1.000000000000000000, 0.000000000000000000, 0.000000000000000000 ) ) ;
#47695 = VECTOR ( 'NONE', #36024, 1000.000000000000000 ) ;
#47696 = CARTESIAN_POINT ( 'NONE',  ( 10.52638330645999964, -2.451090818816000105, 6.282756943804999494 ) ) ;
#47697 = CARTESIAN_POINT ( 'NONE',  ( 17.55505043854143565, 3.125000000000000000, -12.28374638332999602 ) ) ;
#47698 = CARTESIAN_POINT ( 'NONE',  ( 15.90542051561399894, -3.482376784026000038, -11.36410125839000074 ) ) ;
#47699 = DIRECTION ( 'NONE',  ( -1.000000000000000000, 0.000000000000000000, 0.000000000000000000 ) ) ;
#47700 = CYLINDRICAL_SURFACE ( 'NONE', #8470, 1.350000000000000533 ) ;
#47701 = CARTESIAN_POINT ( 'NONE',  ( 9.813975701332999790, -3.363922674822000136, -8.089163458558500608 ) ) ;
#47702 = CARTESIAN_POINT ( 'NONE',  ( 6.607448840114000355, -0.9275392149503000061, 1.138410677097999812 ) ) ;
#47703 = ADVANCED_FACE ( 'NONE', ( #19405 ), #25334, .T. ) ;
#47704 = CARTESIAN_POINT ( 'NONE',  ( 6.999999999999998224, 8.700222682669624064, -4.587862420901095639 ) ) ;
#47705 = CARTESIAN_POINT ( 'NONE',  ( 10.27427156480999848, -3.399999787207999447, 4.944156960757000618 ) ) ;
#47706 = CARTESIAN_POINT ( 'NONE',  ( 18.36457177586861533, -3.090900475969966088, -11.23268385209002851 ) ) ;
#47707 = ORIENTED_EDGE ( 'NONE', *, *, #28495, .T. ) ;
#47708 = CARTESIAN_POINT ( 'NONE',  ( 12.19601995205470324, 0.1418569258565841595, -12.69895512164410079 ) ) ;
#47709 = CARTESIAN_POINT ( 'NONE',  ( 23.60000000000000497, 12.52449950949405277, 6.096395182155569081 ) ) ;
#47710 = EDGE_CURVE ( 'NONE', #21230, #50475, #40726, .T. ) ;
#47711 = CYLINDRICAL_SURFACE ( 'NONE', #7448, 11.50000000000000178 ) ;
#47712 = CARTESIAN_POINT ( 'NONE',  ( 8.599999952505998024, 4.000000000000000000, 7.500000000000000000 ) ) ;
#47713 = CARTESIAN_POINT ( 'NONE',  ( 1.717640132541333076, -1.762666431298159475, 3.058252359239895135 ) ) ;
#47714 = ORIENTED_EDGE ( 'NONE', *, *, #42633, .F. ) ;
#47715 = CARTESIAN_POINT ( 'NONE',  ( 9.523148997461001741, -5.167567567567999731, -6.822293592207000934 ) ) ;
#47716 = CARTESIAN_POINT ( 'NONE',  ( 10.73724174883999893, -4.024531238983009906, -8.391788556008700439 ) ) ;
#47717 = LINE ( 'NONE', #38244, #62728 ) ;
#47718 = DIRECTION ( 'NONE',  ( 0.7660444431195991832, 0.000000000000000000, 0.6427876096857990662 ) ) ;
#47719 = CARTESIAN_POINT ( 'NONE',  ( 27.64127793187000037, -3.399999999999999911, -4.505338571134999803 ) ) ;
#47720 = CARTESIAN_POINT ( 'NONE',  ( 12.99046541331000171, 12.43411100708999939, 1.799680151465999911 ) ) ;
#47721 = ORIENTED_EDGE ( 'NONE', *, *, #41871, .F. ) ;
#47722 = VECTOR ( 'NONE', #15115, 1000.000000000000227 ) ;
#47723 = CARTESIAN_POINT ( 'NONE',  ( 9.353731048338000065, -2.823575173856999410, 9.032043499493001448 ) ) ;
#47724 = CARTESIAN_POINT ( 'NONE',  ( 8.734997988989999129, -4.062652182992059657, -8.366433385397400002 ) ) ;
#47725 = ORIENTED_EDGE ( 'NONE', *, *, #44282, .T. ) ;
#47726 = CARTESIAN_POINT ( 'NONE',  ( 8.073148997456000231, 5.167567567567999731, -6.822293592207000934 ) ) ;
#47727 = CARTESIAN_POINT ( 'NONE',  ( 7.262120559621999760, -4.847802017252000439, 9.065364004483999594 ) ) ;
#47728 =( GEOMETRIC_REPRESENTATION_CONTEXT ( 3 ) GLOBAL_UNCERTAINTY_ASSIGNED_CONTEXT ( ( #17607 ) ) GLOBAL_UNIT_ASSIGNED_CONTEXT ( ( #17209, #11609, #54619 ) ) REPRESENTATION_CONTEXT ( 'NONE', 'WORKASPACE' ) );
#47729 = PLANE ( 'NONE',  #5405 ) ;
#47730 = ORIENTED_EDGE ( 'NONE', *, *, #29229, .F. ) ;
#47731 = LINE ( 'NONE', #51927, #66582 ) ;
#47732 = CARTESIAN_POINT ( 'NONE',  ( 6.976095280407999866, 2.557426065706999818, -8.459317650138999056 ) ) ;
#47733 = CIRCLE ( 'NONE', #53317, 12.39999890530000037 ) ;
#47734 = DIRECTION ( 'NONE',  ( -0.5298945030329009764, -0.5996714969964009878, -0.5996715028627009891 ) ) ;
#47735 = CARTESIAN_POINT ( 'NONE',  ( 7.925195780913999677, 5.124045530936999882, 6.724518838937999732 ) ) ;
#47736 = VERTEX_POINT ( 'NONE', #46326 ) ;
#47737 = CARTESIAN_POINT ( 'NONE',  ( 9.786673210037999837, -2.381198102024000285, 7.612749732462000374 ) ) ;
#47738 = CARTESIAN_POINT ( 'NONE',  ( 11.59999999999999964, 4.187315255316414131, 8.553266857751330221 ) ) ;
#47739 = LINE ( 'NONE', #36551, #4837 ) ;
#47740 = ORIENTED_EDGE ( 'NONE', *, *, #34508, .F. ) ;
#47741 = AXIS2_PLACEMENT_3D ( 'NONE', #9947, #15192, #8574 ) ;
#47742 = DIRECTION ( 'NONE',  ( 0.000000000000000000, -0.1218274111675001353, -0.9925512993736016476 ) ) ;
#47743 = VERTEX_POINT ( 'NONE', #20092 ) ;
#47744 = CARTESIAN_POINT ( 'NONE',  ( 9.828885904259971440, -2.649665795077092323, -7.263400371928318222 ) ) ;
#47745 = CARTESIAN_POINT ( 'NONE',  ( 18.15698508547102819, 0.1703860850723086517, -13.89862588397357790 ) ) ;
#47746 = CARTESIAN_POINT ( 'NONE',  ( 17.75635104740698722, -0.5917829749564899045, -12.68143435689272280 ) ) ;
#47747 = CARTESIAN_POINT ( 'NONE',  ( 8.112208753304994246, 4.887637668124002133, -6.169107735303001050 ) ) ;
#47748 = DIRECTION ( 'NONE',  ( 0.000000000000000000, 0.000000000000000000, 1.000000000000000000 ) ) ;
#47749 = CARTESIAN_POINT ( 'NONE',  ( 24.00938301694239740, 12.69723756695836236, 3.467595816675521636 ) ) ;
#47750 = EDGE_CURVE ( 'NONE', #57964, #38892, #44650, .T. ) ;
#47751 = CIRCLE ( 'NONE', #58922, 0.8000000000000000444 ) ;
#47752 = B_SPLINE_SURFACE_WITH_KNOTS ( 'NONE', 3, 3, ( 
 ( #40599, #4215, #39923, #36037, #8101, #24865, #25553, #46878, #8786, #51433, #51094, #57353, #3530, #30799, #46193, #61924, #18937, #35026, #9457, #62598, #14039, #67504, #35365, #3870, #14722, #56687, #35705, #19621, #40943, #62264, #56341, #8444, #41290, #45512, #67158 ),
 ( #40261, #14385, #3197, #61581, #67845, #52112, #24524, #57022, #13697, #29445, #18597, #51772, #19270, #9122, #30460, #66824, #61242, #25204, #46539, #19967, #13357, #34683, #45849, #55997, #50751, #2848, #24176, #47913, #350, #63969, #26932, #20650, #32519, #10496, #31158 ),
 ( #63281, #37414, #41976, #31488, #37756, #26592, #26245, #37078, #48246, #10, #4904, #15411, #21332, #52811, #59082, #20995, #42331, #32183, #36737, #58056, #10159, #42661, #5932, #10841, #16083, #64309, #16427, #5254, #41630, #62936, #58735, #11183, #53498, #5588, #21667 ),
 ( #31836, #63633, #36383, #43002, #47573, #53835, #27274, #68186, #68878, #20304, #15750, #58390, #15060, #53152, #57699, #9809, #52460, #4555, #25896, #47225, #68528, #38095, #11870, #60466, #49278, #59769, #17473, #48597, #11519, #54176, #33210, #23408, #22012, #28305, #12229 ) ),
 .UNSPECIFIED., .F., .F., .F.,
 ( 4, 4 ),
 ( 4, 1, 1, 1, 1, 1, 1, 1, 1, 1, 1, 1, 1, 1, 1, 1, 1, 1, 1, 1, 1, 1, 1, 1, 1, 1, 1, 1, 1, 1, 1, 1, 4 ),
 ( -0.1039086239011999951, 1.103908623900999864 ),
 ( -0.01735257130020999988, 0.01084535706264999969, 0.03904328542550000031, 0.06724121378835999641, 0.09543914215121999944, 0.1236370705141000004, 0.1518349988768999959, 0.1800329272397999947, 0.2082308556026999935, 0.2364287839655000167, 0.2646267123283999601, 0.2928246406912000110, 0.3210225690540999821, 0.3492204974169000331, 0.3774184257798000042, 0.4056163541427000307, 0.4338142825054999707, 0.4620122108683999973, 0.4902101392311999928, 0.5184080675940999638, 0.5466059959569999904, 0.5748039243197999859, 0.6030018526827000125, 0.6311997810455000080, 0.6593977094084000345, 0.6875956377712000300, 0.7157935661340999456, 0.7439914944969999722, 0.7721894228597999676, 0.8003873512226999942, 0.8285852795854999897, 0.8567832079484000163, 0.8849811363112999318 ),
 .UNSPECIFIED. ) ;
#47753 = EDGE_CURVE ( 'NONE', #23416, #37303, #41076, .T. ) ;
#47754 = EDGE_CURVE ( 'NONE', #47736, #25656, #20480, .T. ) ;
#47755 = ORIENTED_EDGE ( 'NONE', *, *, #14699, .T. ) ;
#47756 = CARTESIAN_POINT ( 'NONE',  ( 8.046447522772005811, -5.096470895078004659, 6.454903582004997808 ) ) ;
#47757 = ORIENTED_EDGE ( 'NONE', *, *, #5680, .T. ) ;
#47758 = CARTESIAN_POINT ( 'NONE',  ( 10.94796973825000030, 2.864322365205000054, 8.846249469408000721 ) ) ;
#47759 = CARTESIAN_POINT ( 'NONE',  ( 10.83487665876999984, 5.800192368099000184, -7.920541111170000370 ) ) ;
#47760 = CARTESIAN_POINT ( 'NONE',  ( 12.08810207955109917, -4.796537143354000499, 7.825000000000000178 ) ) ;
#47761 = CARTESIAN_POINT ( 'NONE',  ( 8.771960841230001193, 3.061731693614000438, -8.535706278603999664 ) ) ;
#47762 = CARTESIAN_POINT ( 'NONE',  ( 9.209204462306731287, 2.899999999999999911, 6.662590550601094286 ) ) ;
#47763 = CARTESIAN_POINT ( 'NONE',  ( 25.48370073006200087, 2.675502271624000006, 11.27075336431999908 ) ) ;
#47764 = CARTESIAN_POINT ( 'NONE',  ( 18.17607592425854079, -0.07112389991332161709, 13.89976024287835799 ) ) ;
#47765 = CARTESIAN_POINT ( 'NONE',  ( 18.06844887843520908, 0.3566139488609988417, 13.89384732035922632 ) ) ;
#47766 = ORIENTED_EDGE ( 'NONE', *, *, #48099, .F. ) ;
#47767 = CARTESIAN_POINT ( 'NONE',  ( 24.44496264144000364, 8.810483598181999554, -8.810508341310001157 ) ) ;
#47768 = B_SPLINE_CURVE_WITH_KNOTS ( 'NONE', 3,
 ( #22264, #65943, #21915, #12827 ),
 .UNSPECIFIED., .F., .F.,
 ( 4, 4 ),
 ( 0.000000000000000000, 1.000000000000000000 ),
 .UNSPECIFIED. ) ;
#47769 = AXIS2_PLACEMENT_3D ( 'NONE', #63108, #58226, #62092 ) ;
#47770 = CARTESIAN_POINT ( 'NONE',  ( 10.70226357027499908, -2.879914860223000250, 7.283900408233900059 ) ) ;
#47771 = DIRECTION ( 'NONE',  ( -1.000000000000000000, 0.000000000000000000, 0.000000000000000000 ) ) ;
#47772 = EDGE_CURVE ( 'NONE', #43157, #39090, #15870, .T. ) ;
#47773 = CARTESIAN_POINT ( 'NONE',  ( 8.528441940379998698, -2.472358291268000219, 6.234202627038999189 ) ) ;
#47776 = B_SPLINE_CURVE_WITH_KNOTS ( 'NONE', 3,
 ( #11578, #55977, #28728, #14021, #61562, #65763 ),
 .UNSPECIFIED., .F., .F.,
 ( 4, 2, 4 ),
 ( 0.000000000000000000, 0.5000000000000000000, 1.000000000000000000 ),
 .UNSPECIFIED. ) ;
#47775 = CARTESIAN_POINT ( 'NONE',  ( 13.50018479229300006, 11.60142623882999935, 2.415183939829000259 ) ) ;
#47774 = CARTESIAN_POINT ( 'NONE',  ( 13.99999999485600277, 9.471999751521998689, 8.194948195317001804 ) ) ;
#47777 = CARTESIAN_POINT ( 'NONE',  ( 11.55194988689359903, 4.580487242693600081, -8.638573882912000457 ) ) ;
#47778 = CIRCLE ( 'NONE', #17633, 12.52500000000000036 ) ;
#47779 = CARTESIAN_POINT ( 'NONE',  ( 10.70577346828306453, -5.100000000000000533, -6.304440314035878679 ) ) ;
#47780 = CARTESIAN_POINT ( 'NONE',  ( 10.08359632033899800, 3.197262364844699611, -7.172402329663099430 ) ) ;
#47781 = CARTESIAN_POINT ( 'NONE',  ( 17.84068610406497868, -0.5560043133243457447, 12.68361349193353860 ) ) ;
#47782 = CARTESIAN_POINT ( 'NONE',  ( 7.239445764754000479, -0.3967607077929999893, 1.060625802389000061 ) ) ;
#47783 = VECTOR ( 'NONE', #45215, 1000.000000000000000 ) ;
#47784 = CARTESIAN_POINT ( 'NONE',  ( 24.25969109951400071, 8.928491667350998640, 8.811171947794999681 ) ) ;
#47785 = ORIENTED_EDGE ( 'NONE', *, *, #25219, .F. ) ;
#47786 = CARTESIAN_POINT ( 'NONE',  ( 8.700644353210000403, -5.212258818969000451, 6.157189191035000064 ) ) ;
#47787 = CARTESIAN_POINT ( 'NONE',  ( 9.418864158773999407, 3.210851187372000037, -6.346613542714999667 ) ) ;
#47788 = CARTESIAN_POINT ( 'NONE',  ( 11.09393020684900044, -2.750000000000000000, 7.500000000000000000 ) ) ;
#47789 = FACE_OUTER_BOUND ( 'NONE', #53803, .T. ) ;
#47790 = VERTEX_POINT ( 'NONE', #16215 ) ;
#47791 = AXIS2_PLACEMENT_3D ( 'NONE', #21217, #68757, #51990 ) ;
#47792 = B_SPLINE_CURVE_WITH_KNOTS ( 'NONE', 3,
 ( #39426, #11809, #33150, #22991, #44340, #61093, #27908, #49217, #23343, #28602 ),
 .UNSPECIFIED., .F., .F.,
 ( 4, 2, 2, 2, 4 ),
 ( 0.000000000000000000, 0.2500000000000000000, 0.5000000000000000000, 0.7500000000000000000, 1.000000000000000000 ),
 .UNSPECIFIED. ) ;
#47793 = FACE_OUTER_BOUND ( 'NONE', #58740, .T. ) ;
#47794 = DIRECTION ( 'NONE',  ( 0.000000000000000000, 0.000000000000000000, -1.000000000000000000 ) ) ;
#47795 = CARTESIAN_POINT ( 'NONE',  ( 2.647747939885999990, 0.2284574491649999928, 3.751824152430999426 ) ) ;
#47796 = ORIENTED_EDGE ( 'NONE', *, *, #19656, .F. ) ;
#47797 = CARTESIAN_POINT ( 'NONE',  ( 12.68688152457048268, -0.7100593550700113887, -12.57997761080729582 ) ) ;
#47798 = CONICAL_SURFACE ( 'NONE', #22127, 1.150081764678999585, 0.7854598963975319981 ) ;
#47799 = CARTESIAN_POINT ( 'NONE',  ( 12.80505043854144276, 0.6249999999999994449, -25.00000000000000000 ) ) ;
#47800 = CARTESIAN_POINT ( 'NONE',  ( 10.13662282008599824, 4.594711216567399781, 6.540749699823199315 ) ) ;
#47801 = EDGE_CURVE ( 'NONE', #32730, #31652, #12940, .T. ) ;
#47802 = CARTESIAN_POINT ( 'NONE',  ( 5.592979883553708120, 12.14034187852289115, 3.752392258527085467 ) ) ;
#47803 = CARTESIAN_POINT ( 'NONE',  ( 7.410857780409000561, 2.302289264429000504, 6.875166305059000393 ) ) ;
#47804 = ORIENTED_EDGE ( 'NONE', *, *, #47584, .F. ) ;
#47805 = CARTESIAN_POINT ( 'NONE',  ( 11.26396921949000074, -3.857819209177999920, 11.66658462090000015 ) ) ;
#47806 = CARTESIAN_POINT ( 'NONE',  ( 7.018770280410000062, 5.447281585506000390, -7.886005609586001164 ) ) ;
#47807 = CARTESIAN_POINT ( 'NONE',  ( 8.535636967035518552, -3.193321067437692840, 5.957063580949454540 ) ) ;
#47808 = CARTESIAN_POINT ( 'NONE',  ( 9.117468108405999416, -2.769196120524999749, 7.151422676278199830 ) ) ;
#47809 = VERTEX_POINT ( 'NONE', #5720 ) ;
#47810 = DIRECTION ( 'NONE',  ( -1.000000000000000000, 0.000000000000000000, 0.000000000000000000 ) ) ;
#47811 = CARTESIAN_POINT ( 'NONE',  ( 6.250859839683334584, 0.3926218265389220807, -1.460959015002473382 ) ) ;
#47812 = EDGE_LOOP ( 'NONE', ( #2574, #32758 ) ) ;
#47813 = CARTESIAN_POINT ( 'NONE',  ( 12.80505043854143388, 1.760845406083386688, -12.47635457398814829 ) ) ;
#47814 = DIRECTION ( 'NONE',  ( 0.000000000000000000, 0.9519535082155350381, -0.3062425806385115079 ) ) ;
#47815 = CARTESIAN_POINT ( 'NONE',  ( 11.09378572506000005, -2.399999999999999911, 6.571291218949999902 ) ) ;
#47816 = ORIENTED_EDGE ( 'NONE', *, *, #18006, .T. ) ;
#47817 = DIRECTION ( 'NONE',  ( 1.000000000000000000, 1.063144863253999899E-13, 0.000000000000000000 ) ) ;
#47818 = CARTESIAN_POINT ( 'NONE',  ( 11.06456920625009843, 4.037149028919880145, -6.467161360063999886 ) ) ;
#47819 = CARTESIAN_POINT ( 'NONE',  ( 8.852395121421350765, -3.390746510554502713, 9.167721567650527703 ) ) ;
#47820 = CARTESIAN_POINT ( 'NONE',  ( 11.78118179236250107, -4.267047616085000605, 8.749800764654999341 ) ) ;
#47821 = ORIENTED_EDGE ( 'NONE', *, *, #20011, .F. ) ;
#47822 = CARTESIAN_POINT ( 'NONE',  ( 7.422239158771000156, 5.361039412362000434, 6.973453640356000349 ) ) ;
#47823 = ORIENTED_EDGE ( 'NONE', *, *, #894, .T. ) ;
#47824 = DIRECTION ( 'NONE',  ( 0.000000000000000000, -1.000000000000000000, 0.000000000000000000 ) ) ;
#47825 = CARTESIAN_POINT ( 'NONE',  ( 8.224933059623998233, -5.629389383493999865, 8.631822608164000599 ) ) ;
#47826 = CARTESIAN_POINT ( 'NONE',  ( 10.96855433372000022, 6.483894572015000080, -5.213062733535000604 ) ) ;
#47827 = ORIENTED_EDGE ( 'NONE', *, *, #45507, .F. ) ;
#47828 = CARTESIAN_POINT ( 'NONE',  ( 12.76340515712447221, -1.876302067334185475, -12.57520337466226223 ) ) ;
#47829 = CARTESIAN_POINT ( 'NONE',  ( 6.365984310645998789, 10.53289132855000076, -4.483227135235997807 ) ) ;
#47830 = LINE ( 'NONE', #11438, #18157 ) ;
#47831 = CARTESIAN_POINT ( 'NONE',  ( 10.20000030442999872, -12.49999969551000056, 3.568610900609000272E-10 ) ) ;
#47832 = CARTESIAN_POINT ( 'NONE',  ( 12.41959488098034292, -1.899094099299829530, -13.87060288894783433 ) ) ;
#47833 = AXIS2_PLACEMENT_3D ( 'NONE', #8647, #17771, #44348 ) ;
#47834 = CARTESIAN_POINT ( 'NONE',  ( 11.58487348028854846, -4.882707455860599843, -7.977261354519500358 ) ) ;
#47835 = CARTESIAN_POINT ( 'NONE',  ( 18.15060209887481690, 3.510419631054046530, 12.02305644365588400 ) ) ;
#47837 = EDGE_CURVE ( 'NONE', #54822, #62212, #21457, .T. ) ;
#47836 = CARTESIAN_POINT ( 'NONE',  ( 18.17388115328634868, -2.104502522679969179, 12.42302150255120807 ) ) ;
#47838 = VERTEX_POINT ( 'NONE', #44795 ) ;
#47839 = CARTESIAN_POINT ( 'NONE',  ( 9.541999884715579583, -4.156896875802718050, 6.308000049678228471 ) ) ;
#47840 = ORIENTED_EDGE ( 'NONE', *, *, #57765, .T. ) ;
#47841 = CARTESIAN_POINT ( 'NONE',  ( 0.000000000000000000, 0.000000000000000000, 0.000000000000000000 ) ) ;
#47842 = DIRECTION ( 'NONE',  ( -0.000000000000000000, -0.000000000000000000, 1.000000000000000000 ) ) ;
#47843 = CARTESIAN_POINT ( 'NONE',  ( 12.02285868696541549, -3.940189611494480992, 6.228129494253471066 ) ) ;
#47844 = CARTESIAN_POINT ( 'NONE',  ( 9.961465797930001642, 2.787126709928999801, -8.677707706574000923 ) ) ;
#47845 = CARTESIAN_POINT ( 'NONE',  ( 18.23777283046813125, 3.105167776281879899, -11.92942829619371103 ) ) ;
#47846 = CARTESIAN_POINT ( 'NONE',  ( 18.17229989573655047, 2.399660445438212442, -12.47442500975356872 ) ) ;
#47847 = CARTESIAN_POINT ( 'NONE',  ( 23.99071456098100086, -13.00908790436000118, 3.384982717025000198 ) ) ;
#47848 = CARTESIAN_POINT ( 'NONE',  ( 17.79999999998900151, 3.595165934733000057, 11.99793354950999991 ) ) ;
#47849 = VERTEX_POINT ( 'NONE', #18216 ) ;
#47850 = CARTESIAN_POINT ( 'NONE',  ( 9.160535748954998780, 2.900115872948000106, -6.152093930328999427 ) ) ;
#47851 = FACE_OUTER_BOUND ( 'NONE', #65549, .T. ) ;
#47852 = DIRECTION ( 'NONE',  ( -1.000000000000000000, 0.000000000000000000, 0.000000000000000000 ) ) ;
#47853 = CARTESIAN_POINT ( 'NONE',  ( 10.00122429346999908, 2.274087081648999753, 7.851326250696001097 ) ) ;
#47854 = EDGE_CURVE ( 'NONE', #48162, #46774, #38812, .T. ) ;
#47855 = CARTESIAN_POINT ( 'NONE',  ( 11.40346005378009941, -3.213042707518099839, 7.920222357891399945 ) ) ;
#47856 = CARTESIAN_POINT ( 'NONE',  ( 18.02410434383600091, 3.285250940561000199, -11.23276246309000115 ) ) ;
#47857 = CARTESIAN_POINT ( 'NONE',  ( 11.39210538575740017, 4.842454415653899780, -7.298582155985900322 ) ) ;
#47858 = EDGE_CURVE ( 'NONE', #64753, #53328, #412, .T. ) ;
#47859 = CARTESIAN_POINT ( 'NONE',  ( 12.22352039041727245, -0.2292434675627123553, 12.69722039463304952 ) ) ;
#47860 = CARTESIAN_POINT ( 'NONE',  ( 5.500000000000000000, -12.22296174243999900, -3.800101973039000214 ) ) ;
#47861 = CARTESIAN_POINT ( 'NONE',  ( 8.179999999999999716, 4.924138593003999809, -8.484107647018999998 ) ) ;
#47862 = CARTESIAN_POINT ( 'NONE',  ( 9.215338062334547331, -2.659994556414565725, 7.664869024387687801 ) ) ;
#47863 = ORIENTED_EDGE ( 'NONE', *, *, #37062, .T. ) ;
#47864 = CARTESIAN_POINT ( 'NONE',  ( 9.219485841232998524, 3.892978337449999771, -8.893414073324001023 ) ) ;
#47865 = CARTESIAN_POINT ( 'NONE',  ( 6.795873790635000411, -1.061937232448999957, 0.3932159216488000375 ) ) ;
#47866 = DIRECTION ( 'NONE',  ( 0.000000000000000000, -1.000000000000000000, 0.000000000000000000 ) ) ;
#47867 = CARTESIAN_POINT ( 'NONE',  ( 11.09999999999999964, -4.000000000000000000, -7.500000000000000000 ) ) ;
#47868 = CARTESIAN_POINT ( 'NONE',  ( 10.65729680893149656, 4.825159113303620906, 4.784047223868995502 ) ) ;
#47869 = CARTESIAN_POINT ( 'NONE',  ( 10.30072469555899950, -3.429147315060100176, -6.512367818249299667 ) ) ;
#47870 = ORIENTED_EDGE ( 'NONE', *, *, #30702, .F. ) ;
#47871 = CARTESIAN_POINT ( 'NONE',  ( 5.000000000000000000, 0.000000000000000000, 0.000000000000000000 ) ) ;
#47872 = CARTESIAN_POINT ( 'NONE',  ( 8.721010841230999233, 5.983047240001000411, 7.440798119034999658 ) ) ;
#47873 = CONICAL_SURFACE ( 'NONE', #43384, 0.9999998338055000602, 0.7853981908209605178 ) ;
#47876 = DIRECTION ( 'NONE',  ( 0.000000000000000000, 1.000000000000000000, 0.000000000000000000 ) ) ;
#47875 = CARTESIAN_POINT ( 'NONE',  ( 8.415504719592000527, 2.469361196073999842, -7.826019481986000059 ) ) ;
#47874 = PRODUCT_DEFINITION_CONTEXT ( 'detailed design', #25734, 'design' ) ;
#47877 = CARTESIAN_POINT ( 'NONE',  ( 24.96666885022127857, -10.83443035760302386, 3.855530939604538965 ) ) ;
#47878 = ORIENTED_EDGE ( 'NONE', *, *, #5437, .F. ) ;
#47879 = CARTESIAN_POINT ( 'NONE',  ( 11.24053267693000002, 2.774035422596999645, 6.782113650547000105 ) ) ;
#47881 = CARTESIAN_POINT ( 'NONE',  ( 17.88807090798128741, -1.970716457409874778, -13.77152834881607468 ) ) ;
#47880 = AXIS2_PLACEMENT_3D ( 'NONE', #14425, #18636, #56032 ) ;
#47882 = CARTESIAN_POINT ( 'NONE',  ( 10.97364560330029981, 4.265439025801100570, 8.324524538096799375 ) ) ;
#47883 = CARTESIAN_POINT ( 'NONE',  ( 10.48164908029000131, -4.022873587130999518, 9.090901241422999490 ) ) ;
#47884 = CARTESIAN_POINT ( 'NONE',  ( 7.293870559621999483, -3.416208448044999901, 6.162501393933999871 ) ) ;
#47885 = VERTEX_POINT ( 'NONE', #22757 ) ;
#47886 = CARTESIAN_POINT ( 'NONE',  ( 9.294718325437999695, 4.148133901461999784, 9.337478696773001019 ) ) ;
#47888 = CARTESIAN_POINT ( 'NONE',  ( 9.900941392955999731, -4.883847137081999357, -9.070879136699002032 ) ) ;
#47887 = CARTESIAN_POINT ( 'NONE',  ( 10.89529697814178100, 4.826567894363762434, -7.215614489968412926 ) ) ;
#47889 = CARTESIAN_POINT ( 'NONE',  ( 7.734707008367833758, -5.578007308158791311, 8.234535370972333013 ) ) ;
#47890 = CARTESIAN_POINT ( 'NONE',  ( 17.93438719500359824, -0.4968219660327466980, 13.88804946350949976 ) ) ;
#47891 = CARTESIAN_POINT ( 'NONE',  ( 1.881520261439000086, 1.670918626813999941, 2.798091744145999815 ) ) ;
#47892 = ORIENTED_EDGE ( 'NONE', *, *, #12273, .F. ) ;
#47893 = CARTESIAN_POINT ( 'NONE',  ( 5.750859839683333696, 0.3926218265389220807, -1.460959015002473382 ) ) ;
#47894 = CARTESIAN_POINT ( 'NONE',  ( 11.53918313518939875, -4.707599264529200411, 6.605241151424599444 ) ) ;
#47895 = CARTESIAN_POINT ( 'NONE',  ( 11.49977531252999974, 12.43119799159999950, 1.530013559959999991 ) ) ;
#47896 = CARTESIAN_POINT ( 'NONE',  ( 10.42795525820099911, 3.905250696375530239, 8.498986197235801399 ) ) ;
#47897 = ORIENTED_EDGE ( 'NONE', *, *, #29393, .T. ) ;
#47898 = B_SPLINE_SURFACE_WITH_KNOTS ( 'NONE', 3, 3, ( 
 ( #21471, #26735, #31984, #54673 ),
 ( #16228, #6770, #49421, #53296 ),
 ( #42807, #58882, #11666, #10988 ),
 ( #59222, #53639, #5734, #33007 ),
 ( #11323, #48392, #499, #32664 ),
 ( #53974, #6079, #50814, #7815 ),
 ( #18311, #13072, #60268, #3256 ),
 ( #18992, #2907, #28462, #7463 ) ),
 .UNSPECIFIED., .F., .F., .F.,
 ( 4, 1, 1, 1, 1, 4 ),
 ( 4, 4 ),
 ( 0.7453249619866000319, 0.7647058823529000460, 0.8235294117646999590, 0.8823529411764999830, 0.9411764705882000870, 0.9905820749711999884 ),
 ( -0.1830924788703000017, 1.182948957423999969 ),
 .UNSPECIFIED. ) ;
#47899 = CARTESIAN_POINT ( 'NONE',  ( 8.623264158775000965, 5.288433695693000480, -8.041290150997999930 ) ) ;
#47900 = CARTESIAN_POINT ( 'NONE',  ( 12.12887591290035338, 2.220077349933747168, -12.40287778440552557 ) ) ;
#47901 = CARTESIAN_POINT ( 'NONE',  ( 11.63746005378019888, -2.838900981960999825, 8.120007936598501175 ) ) ;
#47903 = CARTESIAN_POINT ( 'NONE',  ( 25.52344528808500002, -2.888780152759999886, -11.27718479156999898 ) ) ;
#47902 = B_SPLINE_CURVE_WITH_KNOTS ( 'NONE', 3,
 ( #63243, #42966, #16045, #37376, #48903, #32145 ),
 .UNSPECIFIED., .F., .F.,
 ( 4, 2, 4 ),
 ( 0.000000000000000000, 0.5000000000000000000, 1.000000000000000000 ),
 .UNSPECIFIED. ) ;
#47904 = CARTESIAN_POINT ( 'NONE',  ( 25.46373029971899982, -8.354610197568000274, -8.148451206582999262 ) ) ;
#47905 = ORIENTED_EDGE ( 'NONE', *, *, #26760, .T. ) ;
#47906 = CARTESIAN_POINT ( 'NONE',  ( 11.09999999999999964, 4.000000000000000000, -7.500000000000000000 ) ) ;
#47907 = CARTESIAN_POINT ( 'NONE',  ( 5.700000000000000178, -1.300000000000000044, 9.662944685757000940 ) ) ;
#47908 = EDGE_LOOP ( 'NONE', ( #55105, #40430, #25323, #32776, #54515 ) ) ;
#47909 = CARTESIAN_POINT ( 'NONE',  ( 11.46179707368349909, 3.501542828836900156, 8.370914060838998694 ) ) ;
#47910 = CARTESIAN_POINT ( 'NONE',  ( 10.90000000296000060, -5.100000000009000445, 5.160242730682999657 ) ) ;
#47911 = CARTESIAN_POINT ( 'NONE',  ( 10.62924593896999959, 3.609487840896999700, -5.855139066690000504 ) ) ;
#47912 = DIRECTION ( 'NONE',  ( 0.000000000000000000, 0.000000000000000000, -1.000000000000000000 ) ) ;
#47913 = CARTESIAN_POINT ( 'NONE',  ( 10.87148543990999983, -5.567571293949000300, 7.772413914480000408 ) ) ;
#47914 = CARTESIAN_POINT ( 'NONE',  ( 17.59617179617751859, 0.6239794389693675836, -12.67935706666153450 ) ) ;
#47915 = CARTESIAN_POINT ( 'NONE',  ( 12.30936054499994725, 2.880824963415391959, -12.35466577907433638 ) ) ;
#47916 = CARTESIAN_POINT ( 'NONE',  ( 11.31410538575739899, -3.024036709177600368, -7.266662245194900116 ) ) ;
#47917 = EDGE_CURVE ( 'NONE', #8013, #1268, #53782, .T. ) ;
#47919 = EDGE_CURVE ( 'NONE', #17344, #18643, #12626, .T. ) ;
#47918 = CARTESIAN_POINT ( 'NONE',  ( 7.374100552923999352, 4.389299166881000858, 9.135259451319999613 ) ) ;
#47920 = ORIENTED_EDGE ( 'NONE', *, *, #46591, .T. ) ;
#47921 = CARTESIAN_POINT ( 'NONE',  ( 11.08482133862618113, 4.942979055179590908, 6.626386139742055370 ) ) ;
#47922 = CARTESIAN_POINT ( 'NONE',  ( 13.50003721581400029, 9.159934378815998812, 7.517910889891000537 ) ) ;
#47923 = CARTESIAN_POINT ( 'NONE',  ( 11.79999998400527161, -11.58088844914904314, -1.772255231651884477 ) ) ;
#47924 = CARTESIAN_POINT ( 'NONE',  ( 18.25660817874744168, 2.298073654326294957, 12.38866391276716961 ) ) ;
#47925 = DIRECTION ( 'NONE',  ( -1.000000000000000000, -0.000000000000000000, -0.000000000000000000 ) ) ;
#47926 = CARTESIAN_POINT ( 'NONE',  ( 11.07072893487999998, 7.292360037005000351, 6.230956250625999893 ) ) ;
#47927 = CARTESIAN_POINT ( 'NONE',  ( 9.237253426484580032, -2.665099273114828193, 7.298819532238196572 ) ) ;
#47928 = CARTESIAN_POINT ( 'NONE',  ( 10.07309687351575178, -2.782534154164605589, -7.827184855449103473 ) ) ;
#47929 = ORIENTED_EDGE ( 'NONE', *, *, #27223, .F. ) ;
#47930 = CARTESIAN_POINT ( 'NONE',  ( 24.46580263708699832, 8.828315330680998940, 8.953816637776000675 ) ) ;
#47931 = CARTESIAN_POINT ( 'NONE',  ( 10.11295058442699890, -3.546800160410199965, -6.451980747609000311 ) ) ;
#47932 = DIRECTION ( 'NONE',  ( 0.000000000000000000, -0.9565994702956989171, -0.2914059941558995170 ) ) ;
#47933 = CARTESIAN_POINT ( 'NONE',  ( 9.944325809452999820, -5.443013936195000291, 7.367349259341000156 ) ) ;
#47934 = CARTESIAN_POINT ( 'NONE',  ( 12.18333460557258974, -3.837988184179999873, 6.509695444280099608 ) ) ;
#47935 = ADVANCED_FACE ( 'NONE', ( #26374 ), #47700, .F. ) ;
#47936 = CARTESIAN_POINT ( 'NONE',  ( 10.67410807141119911, 4.046361247106100123, -8.502397868920999358 ) ) ;
#47937 = CARTESIAN_POINT ( 'NONE',  ( 12.30932062623505807, 0.5250004125410563383, 12.58906021966015842 ) ) ;
#47938 = CARTESIAN_POINT ( 'NONE',  ( 0.4500951013211000329, -1.019984463426999888, 3.043156295769000153 ) ) ;
#47939 = CARTESIAN_POINT ( 'NONE',  ( 9.648120195397835275, 4.680076409640555823, -8.679834369160927210 ) ) ;
#47940 = CARTESIAN_POINT ( 'NONE',  ( 12.10312773382966434, 2.298350437047141259, 12.38862788998081754 ) ) ;
#47942 = CARTESIAN_POINT ( 'NONE',  ( 9.087338750556188671, 5.286506002567208817, -7.027083108977566717 ) ) ;
#47941 = CARTESIAN_POINT ( 'NONE',  ( 9.150442991499998513, 3.928121959910110483, -6.360452723514999462 ) ) ;
#47943 = CARTESIAN_POINT ( 'NONE',  ( 11.35918179236250047, 3.761636028845500412, -6.384440618559000136 ) ) ;
#47944 = CARTESIAN_POINT ( 'NONE',  ( 8.200215151753006637, 2.889589711576002085, -6.692116421364998402 ) ) ;
#47945 = CARTESIAN_POINT ( 'NONE',  ( 10.30480165877000154, 5.828331171948000211, -7.226590957700000928 ) ) ;
#47946 = CARTESIAN_POINT ( 'NONE',  ( 8.594151519676998419, 4.024693162376980382, -8.641543873690000765 ) ) ;
#47948 = CARTESIAN_POINT ( 'NONE',  ( 12.24831336537904036, 2.784226791580946436, 12.38079107516542798 ) ) ;
#47947 = CARTESIAN_POINT ( 'NONE',  ( 18.28136615179828794, -11.72522190381090823, 3.796555440338472032 ) ) ;
#47949 = CIRCLE ( 'NONE', #2191, 10.55000000000000426 ) ;
#47950 = CARTESIAN_POINT ( 'NONE',  ( 11.25361999289386716, -4.544092497359195626, -6.342116603374311268 ) ) ;
#47951 = ORIENTED_EDGE ( 'NONE', *, *, #59616, .F. ) ;
#47952 = CARTESIAN_POINT ( 'NONE',  ( 1.024155438487000191, -3.140063525497999830, -0.8725182546194000244 ) ) ;
#47953 = FACE_OUTER_BOUND ( 'NONE', #42758, .T. ) ;
#47954 = CARTESIAN_POINT ( 'NONE',  ( 3.483675495044915138, 1.122406039528702104, -3.256770312453929783 ) ) ;
#47956 = B_SPLINE_CURVE_WITH_KNOTS ( 'NONE', 3,
 ( #23652, #44991, #2673, #66294 ),
 .UNSPECIFIED., .F., .F.,
 ( 4, 4 ),
 ( 0.000000000000000000, 1.000000000000000000 ),
 .UNSPECIFIED. ) ;
#47955 = CARTESIAN_POINT ( 'NONE',  ( 9.906292290062998163, 4.749786674456300872, 7.935348007132199122 ) ) ;
#47957 = CARTESIAN_POINT ( 'NONE',  ( 12.18088137079345579, -2.461818645006702777, 13.68150212747531214 ) ) ;
#47958 = CARTESIAN_POINT ( 'NONE',  ( 12.22895947712403952, 2.742405092596572391, 13.61899867097569050 ) ) ;
#47959 = CARTESIAN_POINT ( 'NONE',  ( 8.180538548868272031, 3.349946943197689819, 6.152974595870256636 ) ) ;
#47960 = ORIENTED_EDGE ( 'NONE', *, *, #62176, .F. ) ;
#47961 = CARTESIAN_POINT ( 'NONE',  ( 4.603277098756000107, 1.034008087237999973, -0.7467278779783999010 ) ) ;
#47962 = CARTESIAN_POINT ( 'NONE',  ( 8.718784697134999817, -3.305825103746500293, -6.425520776924999566 ) ) ;
#47963 = LINE ( 'NONE', #31542, #26509 ) ;
#47964 = CARTESIAN_POINT ( 'NONE',  ( 10.94635971519499940, -3.540377183549800133, 8.264615166761799969 ) ) ;
#47965 = CARTESIAN_POINT ( 'NONE',  ( 17.83364017334648111, 3.059569048391924451, -12.30342972110860167 ) ) ;
#47966 = CARTESIAN_POINT ( 'NONE',  ( 8.521585069485796637, 5.099999999999998757, 6.419216326168621478 ) ) ;
#47967 = CARTESIAN_POINT ( 'NONE',  ( 18.14478511896022184, 2.707036753601618440, 12.40091620380301407 ) ) ;
#47968 = EDGE_CURVE ( 'NONE', #51168, #19886, #29667, .T. ) ;
#47969 = ADVANCED_FACE ( 'NONE', ( #28874 ), #37279, .F. ) ;
#47970 = DIRECTION ( 'NONE',  ( 1.000000000000000000, 0.000000000000000000, 0.000000000000000000 ) ) ;
#47971 = CARTESIAN_POINT ( 'NONE',  ( 10.03977055961999909, -2.255583827894000137, -8.111980070942999888 ) ) ;
#47972 = CARTESIAN_POINT ( 'NONE',  ( 4.813359839683166719, 1.310679582531387943, -0.7554284705563468760 ) ) ;
#47973 = LINE ( 'NONE', #71, #63224 ) ;
#47974 = CARTESIAN_POINT ( 'NONE',  ( 24.08742282057739104, 9.230907236166416396, -9.184803071643798944 ) ) ;
#47975 = LINE ( 'NONE', #74, #43201 ) ;
#47976 = CARTESIAN_POINT ( 'NONE',  ( 23.95226698060700343, 12.88010722568999888, -3.487952265340000135 ) ) ;
#47977 = EDGE_LOOP ( 'NONE', ( #30991, #3599, #48530, #47556 ) ) ;
#47978 = CARTESIAN_POINT ( 'NONE',  ( 8.316054719590999511, 3.826300099041999747, -9.055335252254000267 ) ) ;
#47979 = CARTESIAN_POINT ( 'NONE',  ( 11.91256651104150066, -3.901000349726440053, 8.498573944230598087 ) ) ;
#47980 = ORIENTED_EDGE ( 'NONE', *, *, #63735, .F. ) ;
#47981 = CARTESIAN_POINT ( 'NONE',  ( 13.42725895570834460, 12.36922847561466732, 1.970373770725430518 ) ) ;
#47982 = CARTESIAN_POINT ( 'NONE',  ( 11.23610538575739959, -2.890527834009000152, -7.234742334405199315 ) ) ;
#47983 = ORIENTED_EDGE ( 'NONE', *, *, #162, .F. ) ;
#47984 = CARTESIAN_POINT ( 'NONE',  ( 11.59456039236534330, 5.314711678001000195, 7.436015812896529020 ) ) ;
#47985 = CARTESIAN_POINT ( 'NONE',  ( 24.30001694968100168, 3.271769180623000040, -12.21048179117000032 ) ) ;
#47986 = CARTESIAN_POINT ( 'NONE',  ( 17.86871151025999893, -3.252328409732000214, 11.33729656921000029 ) ) ;
#47987 = CARTESIAN_POINT ( 'NONE',  ( 10.61257802013489737, -4.891884252872400474, -7.479237407015119743 ) ) ;
#47988 = CARTESIAN_POINT ( 'NONE',  ( 12.64261640806205200, 0.6049408601271634156, -13.88227884472453155 ) ) ;
#47989 = CARTESIAN_POINT ( 'NONE',  ( 11.59999999999999964, -3.983295036746754558, -6.452290402036156891 ) ) ;
#47990 = DIRECTION ( 'NONE',  ( 0.000000000000000000, 1.000000000000000000, 0.000000000000000000 ) ) ;
#47991 = VERTEX_POINT ( 'NONE', #45204 ) ;
#47992 = EDGE_CURVE ( 'NONE', #67648, #31059, #67193, .T. ) ;
#47994 = EDGE_CURVE ( 'NONE', #60155, #24623, #7437, .T. ) ;
#47993 = FACE_OUTER_BOUND ( 'NONE', #55264, .T. ) ;
#47995 = ORIENTED_EDGE ( 'NONE', *, *, #53264, .F. ) ;
#47996 = VECTOR ( 'NONE', #57416, 1000.000000000000000 ) ;
#47997 = CARTESIAN_POINT ( 'NONE',  ( 0.1103081484368000076, -1.521127753326000143, -2.712944034833999929 ) ) ;
#47998 = EDGE_CURVE ( 'NONE', #31887, #65107, #29825, .T. ) ;
#47999 = ORIENTED_EDGE ( 'NONE', *, *, #50235, .F. ) ;
#48000 = CARTESIAN_POINT ( 'NONE',  ( 8.820101285864000218, 3.176316400316700150, 8.478738839062499366 ) ) ;
#48001 = CARTESIAN_POINT ( 'NONE',  ( 18.08671436482210026, -2.829189290800525391, -12.36876367364216911 ) ) ;
#48002 = CARTESIAN_POINT ( 'NONE',  ( 13.49980696792482959, 11.86896009962647724, 3.468589882356392540 ) ) ;
#48003 = CARTESIAN_POINT ( 'NONE',  ( 3.999971066382000284, 2.149963194831999935, 0.000000000000000000 ) ) ;
#48004 = CARTESIAN_POINT ( 'NONE',  ( 12.49177480397739615, 0.5412024733746015892, 13.88582008197803219 ) ) ;
#48005 = ORIENTED_EDGE ( 'NONE', *, *, #10269, .F. ) ;
#48006 = CARTESIAN_POINT ( 'NONE',  ( 21.59999953993000332, -12.84999890301999947, 0.000000000000000000 ) ) ;
#48007 = CARTESIAN_POINT ( 'NONE',  ( 18.26357047620399854, 11.66478987891999886, -3.865847705614000152 ) ) ;
#48008 = CARTESIAN_POINT ( 'NONE',  ( 9.910787105781626138, 4.756649759826824919, 7.939332914627393656 ) ) ;
#48009 = CARTESIAN_POINT ( 'NONE',  ( 8.396419424012274035, -5.286796060078613912, 7.027454876807410322 ) ) ;
#48010 = ADVANCED_FACE ( 'NONE', ( #55693 ), #6200, .T. ) ;
#48011 = CARTESIAN_POINT ( 'NONE',  ( 10.01622971959000097, 4.325866256860000369, -9.125812605905000652 ) ) ;
#48012 = CARTESIAN_POINT ( 'NONE',  ( 18.38480835425833249, 11.99871668716868989, -3.594320732042694644 ) ) ;
#48013 = CARTESIAN_POINT ( 'NONE',  ( 10.34225158793000077, -3.348983461003999906, -8.881464249475000017 ) ) ;
#48014 = ORIENTED_EDGE ( 'NONE', *, *, #54920, .T. ) ;
#48015 = VERTEX_POINT ( 'NONE', #19305 ) ;
#48016 = CARTESIAN_POINT ( 'NONE',  ( 11.05669206990999953, 5.189224932640000176, -4.849214782927999678 ) ) ;
#48017 = FACE_OUTER_BOUND ( 'NONE', #13236, .T. ) ;
#48018 = CARTESIAN_POINT ( 'NONE',  ( 10.90000000000000036, -1.300000000000000044, -10.66294468575417120 ) ) ;
#48019 = CARTESIAN_POINT ( 'NONE',  ( 12.26369778072670691, -2.812515541958659604, 13.60219590381264254 ) ) ;
#48020 = CARTESIAN_POINT ( 'NONE',  ( 5.699999999579000054, -0.3000000004212000082, -9.662944680462999258 ) ) ;
#48021 = CARTESIAN_POINT ( 'NONE',  ( 11.38678751119029897, 2.833702563575000166, -8.110172976325500827 ) ) ;
#48022 = CARTESIAN_POINT ( 'NONE',  ( 9.104759580228998672, 3.156743194445300382, -7.298441312785299395 ) ) ;
#48024 = CARTESIAN_POINT ( 'NONE',  ( 4.399638951366856787, 1.439362632458823121, 0.1347012276008314191 ) ) ;
#48023 = CARTESIAN_POINT ( 'NONE',  ( 10.71225461470299933, -4.973404788313100511, 7.252360304610999897 ) ) ;
#48025 = CARTESIAN_POINT ( 'NONE',  ( 4.690443173016667799, 0.1963495408493637351, -1.499999999999999778 ) ) ;
#48026 = ORIENTED_EDGE ( 'NONE', *, *, #50851, .F. ) ;
#48027 = CARTESIAN_POINT ( 'NONE',  ( 10.55518582084299872, -4.566724035220099509, -6.844925608615599621 ) ) ;
#48028 = CARTESIAN_POINT ( 'NONE',  ( 8.166819129144998968, -2.890362633264002667, 6.359808956951005676 ) ) ;
#48029 = CARTESIAN_POINT ( 'NONE',  ( 10.34292546752099895, 2.723846966067000164, 7.588418444866789514 ) ) ;
#48030 = CARTESIAN_POINT ( 'NONE',  ( 8.849999778957998942, 4.000000000000000000, -8.499999833805500060 ) ) ;
#48031 = CARTESIAN_POINT ( 'NONE',  ( 11.02286109245999945, -2.398753588646000079, 6.352476128646999065 ) ) ;
#48032 = CARTESIAN_POINT ( 'NONE',  ( 9.878359312497996925, -5.126777126181800703, 6.752018918865849706 ) ) ;
#48033 = CARTESIAN_POINT ( 'NONE',  ( 16.22809631267600139, -3.350750460640000039, -11.21314580301999797 ) ) ;
#48034 = FACE_OUTER_BOUND ( 'NONE', #55517, .T. ) ;
#48035 = VECTOR ( 'NONE', #27784, 1000.000000000000114 ) ;
#48036 = DIRECTION ( 'NONE',  ( -0.5000000000000150990, -0.08222066253632250021, 0.8621135439442261239 ) ) ;
#48037 = CARTESIAN_POINT ( 'NONE',  ( 8.876797255587998592, -3.133765047594600173, -7.463326341748410364 ) ) ;
#48038 = CARTESIAN_POINT ( 'NONE',  ( 5.555416005062999929, 1.090514925437999993, -0.4404064970261999945 ) ) ;
#48039 = B_SPLINE_SURFACE_WITH_KNOTS ( 'NONE', 3, 3, ( 
 ( #68404, #31373, #20874, #41509, #58968, #46763, #37297, #58275, #25776, #5483, #5819, #68755, #21553, #15289, #42211, #20527, #53036, #20182, #63513, #15630, #52685, #41853, #26470, #36612, #62821, #32066, #57581, #9686, #57938, #52343, #4437, #53382, #26818, #31035, #16311 ),
 ( #10034, #36961, #10378, #64196, #47803, #63854, #48134, #15967, #238, #42889, #37635, #11072, #1970, #22589, #16997, #38679, #39032, #48825, #11751, #1274, #21895, #39370, #27158, #17709, #60000, #6158, #55104, #55452, #54410, #23292, #43582, #60347, #64537, #43931, #64883 ),
 ( #65584, #12455, #65236, #28191, #6510, #17351, #38324, #48479, #37980, #60689, #1619, #33093, #33788, #22934, #7210, #586, #59654, #6854, #43233, #28547, #12806, #27855, #59304, #34135, #12111, #49506, #18053, #16654, #11406, #32745, #49161, #934, #54061, #49857, #44633 ),
 ( #27499, #22244, #65925, #33439, #54755, #44286, #30262, #40071, #29238, #19067, #51568, #18395, #24664, #61038, #35505, #66961, #19414, #45654, #50548, #23977, #39720, #55798, #13159, #3663, #40738, #35839, #62063, #40394, #3331, #67638, #14522, #56825, #61717, #34487, #46336 ) ),
 .UNSPECIFIED., .F., .F., .F.,
 ( 4, 4 ),
 ( 4, 1, 1, 1, 1, 1, 1, 1, 1, 1, 1, 1, 1, 1, 1, 1, 1, 1, 1, 1, 1, 1, 1, 1, 1, 1, 1, 1, 1, 1, 1, 1, 4 ),
 ( -0.1039370721279000015, 1.103937072127999963 ),
 ( -0.02000000000000000042, 0.01250000000000000069, 0.04499999999999999833, 0.07749999999999999944, 0.1100000000000000006, 0.1424999999999999878, 0.1749999999999999889, 0.2074999999999999900, 0.2399999999999999911, 0.2725000000000000200, 0.3049999999999999933, 0.3375000000000000222, 0.3699999999999999956, 0.4025000000000000244, 0.4349999999999999978, 0.4675000000000000266, 0.5000000000000000000, 0.5324999999999999734, 0.5649999999999999467, 0.5975000000000000311, 0.6300000000000000044, 0.6624999999999999778, 0.6949999999999999512, 0.7275000000000000355, 0.7600000000000000089, 0.7924999999999999822, 0.8249999999999999556, 0.8575000000000000400, 0.8900000000000000133, 0.9224999999999999867, 0.9549999999999999600, 0.9875000000000000444, 1.020000000000000018 ),
 .UNSPECIFIED. ) ;
#48040 = CARTESIAN_POINT ( 'NONE',  ( 10.81021345716900051, -3.363461959113699606, 6.921280946186199934 ) ) ;
#48041 = CARTESIAN_POINT ( 'NONE',  ( 8.810863317747999801, 4.960863370448500120, -7.500000000073117512 ) ) ;
#48042 = VERTEX_POINT ( 'NONE', #23521 ) ;
#48043 = ADVANCED_FACE ( 'NONE', ( #24208 ), #48459, .F. ) ;
#48044 = EDGE_CURVE ( 'NONE', #40500, #22839, #1777, .T. ) ;
#48045 = CARTESIAN_POINT ( 'NONE',  ( 12.21006921427117398, -0.1916424759571759007, -12.69805926625132919 ) ) ;
#48046 = CARTESIAN_POINT ( 'NONE',  ( 10.94903032197929882, 4.503839166471300004, -6.795411691360399686 ) ) ;
#48047 = CARTESIAN_POINT ( 'NONE',  ( 21.60000000000000142, 0.000000000000000000, 0.000000000000000000 ) ) ;
#48048 = DIRECTION ( 'NONE',  ( 0.000000000000000000, -0.9630775332544029288, 0.2692241908533009043 ) ) ;
#48049 = CARTESIAN_POINT ( 'NONE',  ( 8.728568342702292426, -2.857753672535667366, -6.775205634707461400 ) ) ;
#48050 = ORIENTED_EDGE ( 'NONE', *, *, #46572, .F. ) ;
#48051 = CARTESIAN_POINT ( 'NONE',  ( 11.29996927726999978, -12.23272628844000032, -1.505586261403999870 ) ) ;
#48052 = EDGE_CURVE ( 'NONE', #67920, #54071, #51312, .T. ) ;
#48053 = ITEM_DEFINED_TRANSFORMATION ( 'NONE', 'NONE', #20675,  #9676 ) ;
#48054 = CARTESIAN_POINT ( 'NONE',  ( 10.44125056272499918, -2.966599088466999934, -7.515315513715298934 ) ) ;
#48055 = CARTESIAN_POINT ( 'NONE',  ( 18.07980528506707074, 0.3396180385544777525, 12.69389128024067936 ) ) ;
#48056 = CARTESIAN_POINT ( 'NONE',  ( 10.81905590578999998, -2.899999999999999911, -6.571291218949999902 ) ) ;
#48057 = CARTESIAN_POINT ( 'NONE',  ( 11.12299956498149811, 5.207010770456999893, -7.825000000000000178 ) ) ;
#48058 = CARTESIAN_POINT ( 'NONE',  ( 11.06967835872019812, 3.245266201729799960, -7.024326263066900111 ) ) ;
#48059 = ORIENTED_EDGE ( 'NONE', *, *, #9794, .F. ) ;
#48060 = CARTESIAN_POINT ( 'NONE',  ( 10.07771285905000092, -4.622037501707999319, 5.671359981946999973 ) ) ;
#48061 = DIRECTION ( 'NONE',  ( 0.000000000000000000, 1.000000000000000000, 0.000000000000000000 ) ) ;
#48062 = ORIENTED_EDGE ( 'NONE', *, *, #48377, .T. ) ;
#48063 = CARTESIAN_POINT ( 'NONE',  ( 13.18179592083890483, 11.52326738618035940, 1.714065324702974458 ) ) ;
#48064 = CARTESIAN_POINT ( 'NONE',  ( 8.315519353208999931, -5.485781663882000281, 8.532068390166999805 ) ) ;
#48065 = FACE_OUTER_BOUND ( 'NONE', #4118, .T. ) ;
#48066 = ORIENTED_EDGE ( 'NONE', *, *, #65815, .T. ) ;
#48067 = CARTESIAN_POINT ( 'NONE',  ( 17.55505043854147118, -1.875000000000000000, -13.78627172894481667 ) ) ;
#48068 = CARTESIAN_POINT ( 'NONE',  ( 7.224720280406000228, 5.425783499582999880, -6.515903575897000088 ) ) ;
#48069 = CARTESIAN_POINT ( 'NONE',  ( 9.448096873516666605, -4.327184855449103473, -8.717465845835395299 ) ) ;
#48070 = CARTESIAN_POINT ( 'NONE',  ( 7.229686263356974507, 4.176830497180914037, -8.849626747523609893 ) ) ;
#48071 = ORIENTED_EDGE ( 'NONE', *, *, #24503, .T. ) ;
#48072 = CARTESIAN_POINT ( 'NONE',  ( 10.00137895011999944, -3.855365288061999962, 5.709482985498999241 ) ) ;
#48073 = CARTESIAN_POINT ( 'NONE',  ( 24.46225035397799985, 11.93532144209000023, -3.254112264712999636 ) ) ;
#48074 = CARTESIAN_POINT ( 'NONE',  ( 11.30565467195989093, 2.863826994586553099, -6.911917091190549201 ) ) ;
#48075 = ORIENTED_EDGE ( 'NONE', *, *, #24617, .T. ) ;
#48076 = LINE ( 'NONE', #59245, #9118 ) ;
#48077 = CARTESIAN_POINT ( 'NONE',  ( 10.91732944037999964, -3.256268970540999952, -6.361552695759000287 ) ) ;
#48078 = EDGE_CURVE ( 'NONE', #68596, #61815, #68913, .T. ) ;
#48079 = ORIENTED_EDGE ( 'NONE', *, *, #43882, .T. ) ;
#48080 = CARTESIAN_POINT ( 'NONE',  ( 7.674792391072008613, -2.650477653308784376, 7.499986425013215552 ) ) ;
#48081 = CARTESIAN_POINT ( 'NONE',  ( 17.96719322760356974, 0.4698824118409584694, -13.88931020048284815 ) ) ;
#48082 = CARTESIAN_POINT ( 'NONE',  ( 4.726978212288999615, 0.7677468988916000825, -1.355145506237000141 ) ) ;
#48083 = AXIS2_PLACEMENT_3D ( 'NONE', #41644, #58406, #5602 ) ;
#48084 = CARTESIAN_POINT ( 'NONE',  ( 11.59999999999999964, 4.804380105966678194, -6.677026092743739483 ) ) ;
#48085 = FACE_OUTER_BOUND ( 'NONE', #28192, .T. ) ;
#48086 = CARTESIAN_POINT ( 'NONE',  ( 7.315000000000000391, 2.649999999999999911, -7.500000000000000000 ) ) ;
#48087 = CARTESIAN_POINT ( 'NONE',  ( 43.76123417800000226, -13.94845324556000143, 4.312847325879000770 ) ) ;
#48088 = ORIENTED_EDGE ( 'NONE', *, *, #53701, .T. ) ;
#48089 = CARTESIAN_POINT ( 'NONE',  ( 13.60806600681794087, -12.33328427344383016, -2.183404734278298509 ) ) ;
#48090 = VERTEX_POINT ( 'NONE', #31523 ) ;
#48091 = CARTESIAN_POINT ( 'NONE',  ( 9.778460659405999067, 5.743717947473999885, 7.748300625457000379 ) ) ;
#48092 =( REPRESENTATION_RELATIONSHIP ('NONE','NONE', #10823, #24587 ) REPRESENTATION_RELATIONSHIP_WITH_TRANSFORMATION ( #21815 )SHAPE_REPRESENTATION_RELATIONSHIP( ) );
#48093 = CARTESIAN_POINT ( 'NONE',  ( 10.11548915876999999, 2.489190114737999782, -6.434635778494999236 ) ) ;
#48094 = AXIS2_PLACEMENT_3D ( 'NONE', #34211, #50282, #2046 ) ;
#48095 = CARTESIAN_POINT ( 'NONE',  ( 11.09999999999999964, -5.350000000000000533, 7.500000000000000000 ) ) ;
#48096 = CARTESIAN_POINT ( 'NONE',  ( 12.66121447289696000, 1.891428313113427073, -13.78385349382385527 ) ) ;
#48097 = DIRECTION ( 'NONE',  ( 0.000000000000000000, 1.000000000000000000, 0.000000000000000000 ) ) ;
#48098 =( NAMED_UNIT ( * ) SI_UNIT ( $, .STERADIAN. ) SOLID_ANGLE_UNIT ( ) );
#48099 = EDGE_CURVE ( 'NONE', #14453, #13264, #36198, .T. ) ;
#48100 = FACE_OUTER_BOUND ( 'NONE', #48353, .T. ) ;
#48101 = CARTESIAN_POINT ( 'NONE',  ( 17.96218347287557648, 0.4743995194917912661, 13.88910611340307533 ) ) ;
#48102 = B_SPLINE_CURVE_WITH_KNOTS ( 'NONE', 3,
 ( #27833, #49139, #42863, #16286, #11049, #16631, #37959, #11381, #27475, #50523 ),
 .UNSPECIFIED., .F., .F.,
 ( 4, 2, 2, 2, 4 ),
 ( 0.4999999998130718604, 0.6249999998598039230, 0.7499999999065358747, 0.8749999999532679373, 1.000000000000000000 ),
 .UNSPECIFIED. ) ;
#48103 = B_SPLINE_CURVE_WITH_KNOTS ( 'NONE', 1,
 ( #66749, #46118 ),
 .UNSPECIFIED., .F., .F.,
 ( 2, 2 ),
 ( 0.000000000000000000, 1.000000000000000000 ),
 .UNSPECIFIED. ) ;
#48104 = ORIENTED_EDGE ( 'NONE', *, *, #25669, .F. ) ;
#48105 = CARTESIAN_POINT ( 'NONE',  ( 12.65912070212100105, -11.49976653515000002, 4.814127980893999847 ) ) ;
#48106 = CARTESIAN_POINT ( 'NONE',  ( 11.87964291764649971, -5.268358781405000357, 7.656787697937099679 ) ) ;
#48107 = CARTESIAN_POINT ( 'NONE',  ( 1.750973465873000068, -3.500000000000000000, 0.000000000000000000 ) ) ;
#48108 = CARTESIAN_POINT ( 'NONE',  ( 7.191894353207000101, -3.501517589953999643, 9.055975309745999624 ) ) ;
#48110 = DIRECTION ( 'NONE',  ( -1.000000000000000000, 0.000000000000000000, 0.000000000000000000 ) ) ;
#48109 = CARTESIAN_POINT ( 'NONE',  ( 10.71756692516999898, 3.040224182812999665, 8.808452309630000698 ) ) ;
#48111 = CARTESIAN_POINT ( 'NONE',  ( 10.57149279008999798, 3.703313553258400059, -8.601484120896000007 ) ) ;
#48112 = CARTESIAN_POINT ( 'NONE',  ( 25.40548364110799895, -11.40418634689999955, 3.013945778314000012 ) ) ;
#48113 = CARTESIAN_POINT ( 'NONE',  ( 9.602342523874998648, 3.142972170141900001, -7.368808371628100318 ) ) ;
#48114 = CARTESIAN_POINT ( 'NONE',  ( 17.96724410757352786, -0.4699213205053990872, 12.68829855189361844 ) ) ;
#48115 = CARTESIAN_POINT ( 'NONE',  ( 6.716245473203000138, -1.254186399022999998, -0.6529324254944000039 ) ) ;
#48116 = CARTESIAN_POINT ( 'NONE',  ( 18.46577960219898173, -3.126461091541029358, 12.12859619074140838 ) ) ;
#48117 = ORIENTED_EDGE ( 'NONE', *, *, #62115, .T. ) ;
#48118 = CARTESIAN_POINT ( 'NONE',  ( 7.609456853206999938, -3.276313010012999793, 5.841993238691999935 ) ) ;
#48119 = CARTESIAN_POINT ( 'NONE',  ( 8.577620559625000141, -3.981661727120999750, 8.959239802162999311 ) ) ;
#48120 = CARTESIAN_POINT ( 'NONE',  ( 8.849999778957998942, 4.000000000000000000, 7.500000000000000000 ) ) ;
#48121 = LINE ( 'NONE', #226, #61298 ) ;
#48122 = ORIENTED_EDGE ( 'NONE', *, *, #55681, .T. ) ;
#48123 = CARTESIAN_POINT ( 'NONE',  ( 0.9630201129275000049, 2.655425791298000160, -2.578923811134000044 ) ) ;
#48124 = AXIS2_PLACEMENT_3D ( 'NONE', #56859, #14556, #10329 ) ;
#48125 = CARTESIAN_POINT ( 'NONE',  ( 10.82035090130999855, 4.758726914843000699, 7.030721746772699454 ) ) ;
#48126 = CARTESIAN_POINT ( 'NONE',  ( 2.743111838768000244, -3.411508600277999737, 1.577969057705999933 ) ) ;
#48127 = VERTEX_POINT ( 'NONE', #21030 ) ;
#48128 = EDGE_CURVE ( 'NONE', #5569, #33837, #42364, .T. ) ;
#48129 = EDGE_CURVE ( 'NONE', #52415, #30037, #64006, .T. ) ;
#48130 = CARTESIAN_POINT ( 'NONE',  ( 5.252943173016666023, 1.199500263597271577, -0.9218200799623702535 ) ) ;
#48131 = DIRECTION ( 'NONE',  ( -1.000000000000000000, 0.000000000000000000, 0.000000000000000000 ) ) ;
#48132 = CARTESIAN_POINT ( 'NONE',  ( 10.22272469555899832, 4.639546521693399761, 8.606479382885998675 ) ) ;
#48133 = CARTESIAN_POINT ( 'NONE',  ( 7.955340622697639752, -4.963707560450432155, 6.442270077056470257 ) ) ;
#48134 = CARTESIAN_POINT ( 'NONE',  ( 7.539232780409000689, 4.696238830159999544, 5.830273622963999536 ) ) ;
#48135 = ORIENTED_EDGE ( 'NONE', *, *, #5842, .F. ) ;
#48136 = CARTESIAN_POINT ( 'NONE',  ( 6.945013804402999646, -1.256780975885000151, 0.6254553495446000255 ) ) ;
#48137 = EDGE_CURVE ( 'NONE', #14332, #34343, #57056, .T. ) ;
#48138 = ADVANCED_FACE ( 'NONE', ( #30493 ), #47547, .F. ) ;
#48139 = CARTESIAN_POINT ( 'NONE',  ( 7.160229719588000030, 2.268824274702999855, -7.434159913875999948 ) ) ;
#48140 = CARTESIAN_POINT ( 'NONE',  ( 8.416338094939373349, -2.406415503492966845, 8.196916887838668231 ) ) ;
#48141 = CARTESIAN_POINT ( 'NONE',  ( 11.53154461883053017, -12.41096831814673251, -1.687237690270050994 ) ) ;
#48142 = ORIENTED_EDGE ( 'NONE', *, *, #11730, .F. ) ;
#48143 = CARTESIAN_POINT ( 'NONE',  ( 15.95279538704000366, -3.847565940079000324, -11.76597731123000123 ) ) ;
#48144 = CARTESIAN_POINT ( 'NONE',  ( 11.75761329816000078, 11.49411629629000053, 1.653020190619000074 ) ) ;
#48145 = ORIENTED_EDGE ( 'NONE', *, *, #45924, .T. ) ;
#48146 = CARTESIAN_POINT ( 'NONE',  ( 25.29989948031900227, 2.596966625103000137, -11.35305524894999962 ) ) ;
#48147 = CARTESIAN_POINT ( 'NONE',  ( 7.000000000000000000, 0.000000000000000000, 0.000000000000000000 ) ) ;
#48148 = CARTESIAN_POINT ( 'NONE',  ( 17.59627693841142104, 0.6239806250735592252, -13.88114166035887997 ) ) ;
#48149 = VERTEX_POINT ( 'NONE', #20336 ) ;
#48150 = DIRECTION ( 'NONE',  ( 1.000000000000000000, 0.000000000000000000, 0.000000000000000000 ) ) ;
#48151 = CARTESIAN_POINT ( 'NONE',  ( 9.049999337612000261, 3.268496584495999908E-13, 3.612668863294000056E-14 ) ) ;
#48152 = CARTESIAN_POINT ( 'NONE',  ( 11.52677869730533011, 3.596497913043499750, -6.704332466833498927 ) ) ;
#48153 = CYLINDRICAL_SURFACE ( 'NONE', #11879, 1.449999999999999734 ) ;
#48154 = CARTESIAN_POINT ( 'NONE',  ( 10.87041638348499895, -5.241705141469999774, 7.802464414828100381 ) ) ;
#48155 = ORIENTED_EDGE ( 'NONE', *, *, #60926, .T. ) ;
#48156 = CARTESIAN_POINT ( 'NONE',  ( 7.358051658771000092, 4.561643343497000735, 6.153061759127000485 ) ) ;
#48157 = EDGE_CURVE ( 'NONE', #38001, #51068, #63674, .T. ) ;
#48158 = VERTEX_POINT ( 'NONE', #31191 ) ;
#48159 = CARTESIAN_POINT ( 'NONE',  ( 11.39975833414730033, 4.796537143354000499, 7.825000000000000178 ) ) ;
#48160 = CYLINDRICAL_SURFACE ( 'NONE', #54889, 0.5000000000000004441 ) ;
#48161 = CARTESIAN_POINT ( 'NONE',  ( 11.12439302932000018, 5.546250282613000238, -5.163688852187999778 ) ) ;
#48162 = VERTEX_POINT ( 'NONE', #36075 ) ;
#48163 = CARTESIAN_POINT ( 'NONE',  ( 12.24247500090515928, -2.227530134987962818, -12.51087939115179104 ) ) ;
#48164 = DIRECTION ( 'NONE',  ( 0.000000000000000000, 0.7614089499631907509, 0.6482718649732928107 ) ) ;
#48165 = CARTESIAN_POINT ( 'NONE',  ( 23.89320776801300283, -8.283889223723997830, 7.778387373039001851 ) ) ;
#48166 = DIRECTION ( 'NONE',  ( 0.000000000000000000, 0.6195591179857981023, -0.7849499979748136846 ) ) ;
#48167 = CARTESIAN_POINT ( 'NONE',  ( 12.08002314427570312, -2.496413253464126569, -13.77564875264238253 ) ) ;
#48168 = CARTESIAN_POINT ( 'NONE',  ( 11.62994988689359843, -3.481863023525599843, -8.516279404258998653 ) ) ;
#48169 = CARTESIAN_POINT ( 'NONE',  ( 18.30000000000000071, 7.694584455362999620, -1.879999999999999893 ) ) ;
#48170 = CARTESIAN_POINT ( 'NONE',  ( 18.23375231277521635, -2.733957939387008818, 12.29982111303847603 ) ) ;
#48171 = ORIENTED_EDGE ( 'NONE', *, *, #62265, .F. ) ;
#48172 = CARTESIAN_POINT ( 'NONE',  ( 7.642284736835422088, -9.077862420372133201, 5.774202551531083749 ) ) ;
#48173 = ORIENTED_EDGE ( 'NONE', *, *, #10045, .T. ) ;
#48174 = PLANE ( 'NONE',  #31146 ) ;
#48175 = CARTESIAN_POINT ( 'NONE',  ( 10.31498017945866685, 2.650031506806222570, -7.499998780888569527 ) ) ;
#48176 = B_SPLINE_CURVE_WITH_KNOTS ( 'NONE', 3,
 ( #27692, #23126, #65064, #38872, #55295 ),
 .UNSPECIFIED., .F., .F.,
 ( 4, 1, 4 ),
 ( 0.000000000000000000, 0.5000000000000000000, 1.000000000000000000 ),
 .UNSPECIFIED. ) ;
#48177 = CARTESIAN_POINT ( 'NONE',  ( 9.947306532704999427, 4.892812229297999416, -9.067756197920999739 ) ) ;
#48178 = CARTESIAN_POINT ( 'NONE',  ( 17.92628954468417390, 3.345291551440209954, -11.86067033211894106 ) ) ;
#48179 = EDGE_CURVE ( 'NONE', #63173, #47736, #53127, .T. ) ;
#48180 = CARTESIAN_POINT ( 'NONE',  ( 11.82299956498189886, -5.207010770456999893, 7.825000000000000178 ) ) ;
#48181 = CARTESIAN_POINT ( 'NONE',  ( 23.81910887196500326, -12.91783950482999899, 3.708435756594000043 ) ) ;
#48182 = CARTESIAN_POINT ( 'NONE',  ( 8.727215710425999973, 3.626036035117899736, -8.308760775591800041 ) ) ;
#48183 = AXIS2_PLACEMENT_3D ( 'NONE', #19979, #9819, #41985 ) ;
#48184 = EDGE_LOOP ( 'NONE', ( #54681, #5079, #34688, #43161, #60001, #38994, #63150, #53662, #5420, #42572, #65454, #45760, #2746, #57106, #46578, #20990, #63624, #8420, #1915, #60522, #38452, #8161, #39216, #55580, #2137, #39770, #64106 ) ) ;
#48185 = ADVANCED_FACE ( 'NONE', ( #57734 ), #8869, .F. ) ;
#48186 = CARTESIAN_POINT ( 'NONE',  ( 1.831685767832333722, -3.258006849854496956, -1.322661048612402857 ) ) ;
#48187 = CARTESIAN_POINT ( 'NONE',  ( 11.15982925107999968, 5.578232410510000072, 8.067793621926998782 ) ) ;
#48188 = FACE_BOUND ( 'NONE', #28481, .T. ) ;
#48189 = CARTESIAN_POINT ( 'NONE',  ( 11.23213259636990102, -4.907524392912299582, 7.005495010505599751 ) ) ;
#48190 = CARTESIAN_POINT ( 'NONE',  ( 11.09999999999999964, -2.700158290619000034, -5.135706284511000419 ) ) ;
#48191 = CARTESIAN_POINT ( 'NONE',  ( 11.17056785386839834, 3.281375110759499947, -7.983608166707499620 ) ) ;
#48192 = CARTESIAN_POINT ( 'NONE',  ( 12.57501510860068272, -0.5812174491462195336, 12.68209204657793165 ) ) ;
#48193 = AXIS2_PLACEMENT_3D ( 'NONE', #7499, #3288, #45942 ) ;
#48194 = CARTESIAN_POINT ( 'NONE',  ( 9.123551658772999673, 5.558938731259999599, 6.272977177425000050 ) ) ;
#48195 = DIRECTION ( 'NONE',  ( 0.000000000000000000, 0.000000000000000000, -1.000000000000000000 ) ) ;
#48196 = SURFACE_STYLE_USAGE ( .BOTH. , #22649 ) ;
#48197 = ORIENTED_EDGE ( 'NONE', *, *, #30925, .T. ) ;
#48198 = DIRECTION ( 'NONE',  ( 1.000000000000000000, 0.000000000000000000, 0.000000000000000000 ) ) ;
#48199 = CARTESIAN_POINT ( 'NONE',  ( 6.961787026899999731, -0.7800294017036001337, -0.9775269195634000985 ) ) ;
#48200 = CARTESIAN_POINT ( 'NONE',  ( 17.71791196170127591, 3.103760126671077035, 13.52664063941735151 ) ) ;
#48201 = CARTESIAN_POINT ( 'NONE',  ( 24.43231275843400141, 8.806084858360998524, -8.751970408576999816 ) ) ;
#48202 = CARTESIAN_POINT ( 'NONE',  ( 11.28533594839949750, -3.249987070165300196, -6.640482273977399430 ) ) ;
#48203 = ORIENTED_EDGE ( 'NONE', *, *, #60777, .T. ) ;
#48204 = CARTESIAN_POINT ( 'NONE',  ( 5.563312991718063927, -12.16892724396389447, 3.760371626689057223 ) ) ;
#48205 = CARTESIAN_POINT ( 'NONE',  ( 7.988545280410000338, 3.566637212418000136, 5.743604853744000316 ) ) ;
#48207 = CARTESIAN_POINT ( 'NONE',  ( 17.60000001287599858, 11.53033693765999779, -4.891431908114999949 ) ) ;
#48206 = CARTESIAN_POINT ( 'NONE',  ( 9.301695280414000067, 5.619431609641999614, -8.115423117607999615 ) ) ;
#48208 = CARTESIAN_POINT ( 'NONE',  ( 25.59997295081500113, -11.07537799752999952, 3.096069084855000320 ) ) ;
#48209 = VERTEX_POINT ( 'NONE', #32222 ) ;
#48210 = CARTESIAN_POINT ( 'NONE',  ( 10.81579666500999970, 5.374569445151000657, 6.698728322222000209 ) ) ;
#48211 = CARTESIAN_POINT ( 'NONE',  ( 17.81482613222766531, -3.068547461637705975, -13.53623828841521259 ) ) ;
#48212 = CARTESIAN_POINT ( 'NONE',  ( 10.57564694612699974, 3.068007311611700150, 7.128058497017000228 ) ) ;
#48213 = CARTESIAN_POINT ( 'NONE',  ( 9.701976361057999654, -3.399137684422000039, 6.026753338319999820 ) ) ;
#48214 = CARTESIAN_POINT ( 'NONE',  ( 8.732394353210001015, -2.806079842068999852, 8.615883328687999665 ) ) ;
#48215 = ORIENTED_EDGE ( 'NONE', *, *, #6126, .F. ) ;
#48216 = CARTESIAN_POINT ( 'NONE',  ( 7.583051658771000625, 4.763536573491999881, 5.668879554882000349 ) ) ;
#48217 = EDGE_CURVE ( 'NONE', #56420, #36190, #64694, .T. ) ;
#48218 = ADVANCED_FACE ( 'NONE', ( #11555 ), #1083, .T. ) ;
#48220 = CARTESIAN_POINT ( 'NONE',  ( 10.44811814679000150, -5.235603901491000300, -6.609968500665999613 ) ) ;
#48219 = CARTESIAN_POINT ( 'NONE',  ( 10.79683585285767577, 4.539293524411616154, -8.187933206668011721 ) ) ;
#48221 = CARTESIAN_POINT ( 'NONE',  ( 7.855373981381045034, -3.323613655148000667, 9.112573541682413847 ) ) ;
#48222 = CARTESIAN_POINT ( 'NONE',  ( 10.15402496696000156, -5.267980706381999667, 5.992344456606999437 ) ) ;
#48223 = CARTESIAN_POINT ( 'NONE',  ( 24.02092352968800171, 3.259160059610999749, 12.61376570420999954 ) ) ;
#48224 = ORIENTED_EDGE ( 'NONE', *, *, #68111, .T. ) ;
#48226 = CARTESIAN_POINT ( 'NONE',  ( 5.100000001045000175, 0.000000000000000000, 0.000000000000000000 ) ) ;
#48225 = CIRCLE ( 'NONE', #24771, 2.000000000000001776 ) ;
#48227 = CARTESIAN_POINT ( 'NONE',  ( 12.17918044953561996, -2.988516238873000219, 6.972563939641199582 ) ) ;
#48228 = CARTESIAN_POINT ( 'NONE',  ( 11.30579707368350029, 3.365167912142600137, 8.609190966793999422 ) ) ;
#48229 = ORIENTED_EDGE ( 'NONE', *, *, #27728, .F. ) ;
#48230 = CARTESIAN_POINT ( 'NONE',  ( 8.275189158773001097, 3.061731693614000438, -8.535706278603999664 ) ) ;
#48231 = CARTESIAN_POINT ( 'NONE',  ( 12.48133867187396007, 1.836397482308027129, -12.46545911376217042 ) ) ;
#48232 = CARTESIAN_POINT ( 'NONE',  ( 11.92834208742529967, -4.706521750018099581, 6.389420067180999752 ) ) ;
#48233 = EDGE_CURVE ( 'NONE', #68795, #7995, #49312, .T. ) ;
#48234 = CARTESIAN_POINT ( 'NONE',  ( 9.168971206446350664, 4.353237884208152053, -8.814534730582089139 ) ) ;
#48235 = CARTESIAN_POINT ( 'NONE',  ( 7.100000000000000533, 12.03770622561999915, -3.722046322334000124 ) ) ;
#48236 = ORIENTED_EDGE ( 'NONE', *, *, #19334, .F. ) ;
#48237 = CARTESIAN_POINT ( 'NONE',  ( 7.555275273711000494, -4.314043295739000250, 8.819145559946001356 ) ) ;
#48238 = CARTESIAN_POINT ( 'NONE',  ( 9.293111399473126255, -5.011294126480321687, -6.748153640515438312 ) ) ;
#48239 = ORIENTED_EDGE ( 'NONE', *, *, #26439, .T. ) ;
#48240 = CARTESIAN_POINT ( 'NONE',  ( 10.11344336607715988, -2.323991353769818247, -6.990216894119677171 ) ) ;
#48241 = CARTESIAN_POINT ( 'NONE',  ( 11.78179573085659904, 4.973133828855400118, 7.331616337578100051 ) ) ;
#48242 = CIRCLE ( 'NONE', #8083, 1.800000000000000044 ) ;
#48243 = CARTESIAN_POINT ( 'NONE',  ( 9.261662452849000360, 2.944259351255000379, 6.507396354981000108 ) ) ;
#48244 = CARTESIAN_POINT ( 'NONE',  ( 10.36630583688000051, 5.852743870412999705, -7.568014644338999730 ) ) ;
#48245 = CARTESIAN_POINT ( 'NONE',  ( 8.076862807906000086, 5.120521186033995420, 6.727223554611003742 ) ) ;
#48246 = CARTESIAN_POINT ( 'NONE',  ( 9.722771884505998941, -5.493781611190000191, 6.566828939965000167 ) ) ;
#48247 = CARTESIAN_POINT ( 'NONE',  ( 17.63863136176617985, -0.7145943380091489550, -12.57972004139934974 ) ) ;
#48248 = CARTESIAN_POINT ( 'NONE',  ( 12.72076653474564978, 3.120601141701319747, -12.28508997180393436 ) ) ;
#48249 = CARTESIAN_POINT ( 'NONE',  ( 10.92026088462129962, -3.997864853650589634, -6.496532863517000322 ) ) ;
#48250 = CARTESIAN_POINT ( 'NONE',  ( 9.433107780409999421, 4.954905351382000944, 8.825777580285999235 ) ) ;
#48251 = EDGE_LOOP ( 'NONE', ( #17306, #46758, #20791, #19792 ) ) ;
#48252 = CARTESIAN_POINT ( 'NONE',  ( 24.87149173865001472, -3.035096352711473600, 11.66330508788991516 ) ) ;
#48253 = CARTESIAN_POINT ( 'NONE',  ( 4.599999999999999645, -1.760910691117812954, -12.47634535983622861 ) ) ;
#48254 = CARTESIAN_POINT ( 'NONE',  ( 11.64585080655600002, 12.33238363550000116, 1.848877788567000024 ) ) ;
#48255 = B_SPLINE_CURVE_WITH_KNOTS ( 'NONE', 3,
 ( #24917, #40649, #45569, #35081, #46249, #52173, #41346, #9175, #14093, #51153, #30513, #67212, #4274, #35419, #3250, #67904, #50808, #8841 ),
 .UNSPECIFIED., .F., .F.,
 ( 4, 2, 2, 2, 2, 2, 2, 2, 4 ),
 ( 0.000000000000000000, 0.1250000000000000000, 0.2500000000000000000, 0.3750000000000000000, 0.5000000000000000000, 0.6250000000000000000, 0.7500000000000000000, 0.8750000000000000000, 1.000000000000000000 ),
 .UNSPECIFIED. ) ;
#48256 = B_SPLINE_CURVE_WITH_KNOTS ( 'NONE', 3,
 ( #2616, #51540, #23948, #3636 ),
 .UNSPECIFIED., .F., .F.,
 ( 4, 4 ),
 ( 0.000000000000000000, 1.000000000000000000 ),
 .UNSPECIFIED. ) ;
#48257 = CARTESIAN_POINT ( 'NONE',  ( 18.14725124545925539, 2.065010783240463166, 12.42963489304855962 ) ) ;
#48258 = LINE ( 'NONE', #26947, #47301 ) ;
#48259 = CARTESIAN_POINT ( 'NONE',  ( 11.00881343608999963, 8.459666197630999918, 6.608740754140999485 ) ) ;
#48260 = EDGE_CURVE ( 'NONE', #60537, #29347, #11184, .T. ) ;
#48261 = CARTESIAN_POINT ( 'NONE',  ( 12.39297475254648262, -0.4699412923507725881, -12.68829632720558465 ) ) ;
#48262 = CARTESIAN_POINT ( 'NONE',  ( 9.231616107288068918, -3.999997736744774546, 6.618420992905502231 ) ) ;
#48263 = ORIENTED_EDGE ( 'NONE', *, *, #63645, .F. ) ;
#48264 = CARTESIAN_POINT ( 'NONE',  ( 12.17440657078186028, -2.124933824806643390, 12.41953149444585769 ) ) ;
#48265 = CARTESIAN_POINT ( 'NONE',  ( 10.11093802597399893, -4.522194782554399772, -6.642005297568199573 ) ) ;
#48266 = DIRECTION ( 'NONE',  ( 1.000000000000000000, 0.000000000000000000, 0.000000000000000000 ) ) ;
#48267 = B_SPLINE_CURVE_WITH_KNOTS ( 'NONE', 3,
 ( #63907, #16019, #37348, #32118, #53433, #5530, #41223, #19897, #14655, #35971 ),
 .UNSPECIFIED., .F., .F.,
 ( 4, 2, 2, 2, 4 ),
 ( 0.000000000000000000, 0.2500000000000006661, 0.5000000000000013323, 0.7500000000000006661, 1.000000000000000000 ),
 .UNSPECIFIED. ) ;
#48268 = CARTESIAN_POINT ( 'NONE',  ( 10.75110221171000013, -2.822135527917999820, 6.655890318096999714 ) ) ;
#48269 = CARTESIAN_POINT ( 'NONE',  ( 11.22333863405319931, -3.380905141010200232, 6.710270673950399889 ) ) ;
#48270 = AXIS2_PLACEMENT_3D ( 'NONE', #434, #32600, #59503 ) ;
#48271 = CARTESIAN_POINT ( 'NONE',  ( 11.26072066707849828, 4.976067344118500380, -6.909591111168198907 ) ) ;
#48272 = CARTESIAN_POINT ( 'NONE',  ( 12.11487221662462055, 0.2205548374446844873, 12.59807454672507632 ) ) ;
#48273 = CARTESIAN_POINT ( 'NONE',  ( 0.6968879684122999407, 0.8965373106021000682, -3.081807587122999958 ) ) ;
#48274 = CARTESIAN_POINT ( 'NONE',  ( 8.793505787816332742, 5.100000000000000533, 6.515557531858333640 ) ) ;
#48275 = CARTESIAN_POINT ( 'NONE',  ( 12.24387941792141099, 2.775899267521869884, 12.38300827451278607 ) ) ;
#48277 = CARTESIAN_POINT ( 'NONE',  ( 8.560885841230001958, 4.228291488957999888, 8.941375734143997889 ) ) ;
#48276 = CARTESIAN_POINT ( 'NONE',  ( 10.48444474310099928, 5.015709705366000470, -7.992914665944799602 ) ) ;
#48278 = CARTESIAN_POINT ( 'NONE',  ( 10.96533729122639933, 2.859653469230999612, -7.470001566214039990 ) ) ;
#48279 = CARTESIAN_POINT ( 'NONE',  ( 7.928980562030001344, 3.137685067990001020, -6.261915436850998162 ) ) ;
#48280 = B_SPLINE_CURVE_WITH_KNOTS ( 'NONE', 3,
 ( #5168, #37329, #31065, #42922, #20906, #41542, #42243, #52718, #10754, #15662, #62854, #63549, #20560, #52373, #68099, #26158, #58306, #58653 ),
 .UNSPECIFIED., .F., .F.,
 ( 4, 2, 2, 2, 2, 2, 2, 2, 4 ),
 ( 0.000000000000000000, 0.1250000000000000000, 0.2500000000000000000, 0.3750000000000000000, 0.5000000000000000000, 0.6250000000000000000, 0.7500000000000000000, 0.8750000000000000000, 1.000000000000000000 ),
 .UNSPECIFIED. ) ;
#48281 = CARTESIAN_POINT ( 'NONE',  ( 10.00190165877000048, 2.729646201450000031, -8.843033333815998986 ) ) ;
#48282 = CARTESIAN_POINT ( 'NONE',  ( 12.80000000000000071, -43.96540072520999587, 14.96704326274999985 ) ) ;
#48284 = CARTESIAN_POINT ( 'NONE',  ( 18.18005043855005809, -0.04052604701685407623, 12.70000016496815221 ) ) ;
#48283 = CARTESIAN_POINT ( 'NONE',  ( 7.935109315130008056, 5.090269470254001227, 6.488511505667004187 ) ) ;
#48285 = LINE ( 'NONE', #7016, #44193 ) ;
#48286 = ORIENTED_EDGE ( 'NONE', *, *, #32793, .F. ) ;
#48287 = VECTOR ( 'NONE', #63075, 1000.000000000000000 ) ;
#48288 = CARTESIAN_POINT ( 'NONE',  ( 9.520528907821001141, 2.899999999999999911, 6.152188490330000370 ) ) ;
#48289 = DIRECTION ( 'NONE',  ( 1.000000000000000000, 0.000000000000000000, 0.000000000000000000 ) ) ;
#48290 = DIRECTION ( 'NONE',  ( -1.000000000000000000, 1.065814103617000051E-13, -1.598721155425999962E-13 ) ) ;
#48291 = CARTESIAN_POINT ( 'NONE',  ( 9.247734463322998977, 4.090312251411040378, 6.637705594503099604 ) ) ;
#48292 = CARTESIAN_POINT ( 'NONE',  ( 12.21197387330461481, -2.302545343651723808, 13.71336076199744625 ) ) ;
#48293 = CARTESIAN_POINT ( 'NONE',  ( 11.09999999999999964, 4.000000000000000000, -7.500000000000000000 ) ) ;
#48294 = CARTESIAN_POINT ( 'NONE',  ( 9.035395982797805203, -4.311073552809154386, -8.654212551762981320 ) ) ;
#48295 = ORIENTED_EDGE ( 'NONE', *, *, #4410, .T. ) ;
#48296 = EDGE_CURVE ( 'NONE', #47380, #64893, #38674, .T. ) ;
#48297 = EDGE_CURVE ( 'NONE', #26090, #48851, #48977, .T. ) ;
#48298 = CARTESIAN_POINT ( 'NONE',  ( 7.000000000000000000, 0.000000000000000000, 0.000000000000000000 ) ) ;
#48299 = CARTESIAN_POINT ( 'NONE',  ( 11.33830977893730108, -4.976598135215292373, -6.673569913327194847 ) ) ;
#48300 = CARTESIAN_POINT ( 'NONE',  ( 25.46371819568200223, 2.879482785682999868, 11.30954024936000124 ) ) ;
#48301 = CARTESIAN_POINT ( 'NONE',  ( 18.02331223754164924, -3.318306765102383871, 11.16743751352547420 ) ) ;
#48302 = CARTESIAN_POINT ( 'NONE',  ( 17.71812653075899391, 3.103437839927554176, -12.29028812931823644 ) ) ;
#48303 = CARTESIAN_POINT ( 'NONE',  ( 8.554392358909119309, 5.071045932662843647, 6.303914025558337464 ) ) ;
#48304 = CARTESIAN_POINT ( 'NONE',  ( 11.39210538575740017, 4.842454415653899780, 7.701417844014099678 ) ) ;
#48305 = B_SPLINE_CURVE_WITH_KNOTS ( 'NONE', 3,
 ( #65919, #59993, #2303, #34128, #61376 ),
 .UNSPECIFIED., .F., .F.,
 ( 4, 1, 4 ),
 ( 0.000000000000000000, 0.5000000000000000000, 1.000000000000000000 ),
 .UNSPECIFIED. ) ;
#48306 = CARTESIAN_POINT ( 'NONE',  ( 11.03521345716899837, -3.075109701058799772, 6.659120737011199331 ) ) ;
#48307 = CARTESIAN_POINT ( 'NONE',  ( 10.63743064679000128, -3.721475434679999861, -8.997096235511000017 ) ) ;
#48308 = CARTESIAN_POINT ( 'NONE',  ( 4.688359839682667562, -0.7554284705563480973, -1.310679582531387277 ) ) ;
#48309 = B_SPLINE_SURFACE_WITH_KNOTS ( 'NONE', 3, 3, ( 
 ( #61389, #39377, #18404, #18748, #23637, #39729, #60007, #33099, #38685, #12118, #6516, #44639, #55458, #33796, #28553, #27861, #1281, #33446, #28198, #61046, #44294, #65591, #17715, #39038, #55111, #49863, #65931, #18059, #60697, #2315, #28910, #40746, #14532, #8934, #62070 ),
 ( #46691, #50900, #25012, #61724, #34829, #35514, #68332, #56141, #30952, #2996, #19769, #20451, #41777, #3671, #24330, #67994, #14185, #45662, #51577, #62746, #41095, #66968, #29941, #52267, #57501, #30270, #62411, #56836, #19074, #9262, #14866, #40402, #29597, #46343, #35848 ),
 ( #67645, #57164, #13510, #4363, #30603, #35173, #51918, #24673, #56486, #36189, #25697, #67306, #4014, #13844, #8590, #47029, #20110, #25351, #41439, #9610, #8249, #51244, #3339, #45993, #19422, #26742, #58201, #63779, #504, #52960, #4702, #64119, #15890, #68680, #58890 ),
 ( #58538, #15558, #21820, #5057, #26048, #16234, #37221, #20798, #10994, #43153, #36885, #27422, #5406, #47376, #48058, #10645, #64458, #160, #42129, #21477, #32334, #31990, #9962, #21145, #42812, #16582, #53644, #48747, #5740, #851, #37558, #27082, #32670, #48398, #37906 ) ),
 .UNSPECIFIED., .F., .F., .F.,
 ( 4, 4 ),
 ( 4, 1, 1, 1, 1, 1, 1, 1, 1, 1, 1, 1, 1, 1, 1, 1, 1, 1, 1, 1, 1, 1, 1, 1, 1, 1, 1, 1, 1, 1, 1, 1, 4 ),
 ( -0.02000000000000000042, 1.020000000000000018 ),
 ( 0.1633025096610999927, 0.1899619885200000136, 0.2166214673788000034, 0.2432809462376999965, 0.2699404250964999585, 0.2965999039553000038, 0.3232593828141999692, 0.3499188616730000145, 0.3765783405318000043, 0.4032378193906999697, 0.4298972982494999595, 0.4565567771083000048, 0.4832162559671999702, 0.5098757348260000155, 0.5365352136848999809, 0.5631946925437000262, 0.5898541714025000715, 0.6165136502614000369, 0.6431731291201999712, 0.6698326079790000165, 0.6964920868378999819, 0.7231515656967000272, 0.7498110445554999615, 0.7764705234143999268, 0.8031300022731999722, 0.8297894811320000175, 0.8564489599908999828, 0.8831084388497000282, 0.9097679177085999935, 0.9364273965674000388, 0.9630868754261999731, 0.9897463542851000495, 1.016405833144000015 ),
 .UNSPECIFIED. ) ;
#48310 = DIRECTION ( 'NONE',  ( 0.000000000000000000, 0.000000000000000000, -1.000000000000000000 ) ) ;
#48311 = CARTESIAN_POINT ( 'NONE',  ( 23.59999441188499958, 10.30760541648000128, -9.317696302454001156 ) ) ;
#48312 = DIRECTION ( 'NONE',  ( 0.000000000000000000, 0.2588190451024934835, 0.9659258262890757507 ) ) ;
#48313 = EDGE_CURVE ( 'NONE', #15051, #56866, #29543, .T. ) ;
#48314 = ORIENTED_EDGE ( 'NONE', *, *, #39934, .T. ) ;
#48315 = CARTESIAN_POINT ( 'NONE',  ( 9.749220280410998640, 5.656948148960999845, -6.994239053114000626 ) ) ;
#48316 = CARTESIAN_POINT ( 'NONE',  ( 11.17826222744820086, -4.668580868411999596, 6.949274830123499669 ) ) ;
#48317 = ORIENTED_EDGE ( 'NONE', *, *, #13448, .F. ) ;
#48318 = CIRCLE ( 'NONE', #19320, 1.999999999999999778 ) ;
#48319 = CARTESIAN_POINT ( 'NONE',  ( 17.55505043854147118, -3.125000000000000000, 13.52084414783465860 ) ) ;
#48320 = CARTESIAN_POINT ( 'NONE',  ( 10.52226222744799955, -4.880489021643899861, -8.225278704382400718 ) ) ;
#48321 = ORIENTED_EDGE ( 'NONE', *, *, #17136, .F. ) ;
#48322 = EDGE_CURVE ( 'NONE', #8116, #36015, #33741, .T. ) ;
#48323 = CARTESIAN_POINT ( 'NONE',  ( 10.81013259637009938, 2.968328969579000276, 6.937848198857199833 ) ) ;
#48324 = CARTESIAN_POINT ( 'NONE',  ( 6.310040576531521062, -1.097834706587868192, 0.2821293189078559194 ) ) ;
#48325 = CARTESIAN_POINT ( 'NONE',  ( 8.712501735000000025, -4.358851904410700584, -8.276078370613198842 ) ) ;
#48326 = CARTESIAN_POINT ( 'NONE',  ( 18.44503807197100187, -2.664600154114999953, 11.39639460691000039 ) ) ;
#48327 = CARTESIAN_POINT ( 'NONE',  ( 10.90346005378009941, -3.213042707518099839, -7.079777642108599167 ) ) ;
#48328 = CARTESIAN_POINT ( 'NONE',  ( 12.44245189064305457, 0.5091685953835116685, -13.88744776337133402 ) ) ;
#48329 = CARTESIAN_POINT ( 'NONE',  ( 15.90018573812399971, 8.493548356068000516, 8.263529029821000904 ) ) ;
#48330 = CARTESIAN_POINT ( 'NONE',  ( 13.09162860438300058, 11.49399796109000071, 1.653788228654999859 ) ) ;
#48331 = VERTEX_POINT ( 'NONE', #18200 ) ;
#48332 = CARTESIAN_POINT ( 'NONE',  ( 8.722235841230000730, 3.844886277615000125, -8.888911790991000927 ) ) ;
#48333 = VERTEX_POINT ( 'NONE', #29048 ) ;
#48334 = AXIS2_PLACEMENT_3D ( 'NONE', #35021, #50401, #61918 ) ;
#48335 = CARTESIAN_POINT ( 'NONE',  ( 0.4680276591073351256, -2.422374426748084009, 2.170046970593778823 ) ) ;
#48336 = ORIENTED_EDGE ( 'NONE', *, *, #22188, .T. ) ;
#48337 = CARTESIAN_POINT ( 'NONE',  ( 4.555026506349999948, -1.500000000000000000, 0.000000000000000000 ) ) ;
#48338 = CARTESIAN_POINT ( 'NONE',  ( 17.92152980461526468, -3.006687145500352543, -12.31895938800957957 ) ) ;
#48339 = CARTESIAN_POINT ( 'NONE',  ( 10.69837472757367713, 3.526507217177279330, 6.765225077371590956 ) ) ;
#48340 = PLANE ( 'NONE',  #10599 ) ;
#48341 = CARTESIAN_POINT ( 'NONE',  ( 17.65865034516105325, -1.883559157718814880, 12.57405095325165334 ) ) ;
#48342 = FACE_OUTER_BOUND ( 'NONE', #40093, .T. ) ;
#48343 = CARTESIAN_POINT ( 'NONE',  ( 12.19008165514798669, -0.1119984579798063151, 13.89939774083726576 ) ) ;
#48344 = ORIENTED_EDGE ( 'NONE', *, *, #43902, .T. ) ;
#48345 = CARTESIAN_POINT ( 'NONE',  ( 12.68129448069100107, 12.04903608036000051, -3.200077553391999619 ) ) ;
#48346 = CARTESIAN_POINT ( 'NONE',  ( 18.28867698203100289, 11.62873132690000055, -4.501748577889000735 ) ) ;
#48347 = CARTESIAN_POINT ( 'NONE',  ( 9.708153928322625248, 3.619812067603167538, 6.711971190259613529 ) ) ;
#48348 = CARTESIAN_POINT ( 'NONE',  ( 4.500442376531999855, 0.9099999783214999249, 1.169932331390999947 ) ) ;
#48349 = CARTESIAN_POINT ( 'NONE',  ( 9.246064158776000852, 5.200883864107000321, -6.027780766890000308 ) ) ;
#48350 = CARTESIAN_POINT ( 'NONE',  ( 18.53493609108600282, -3.035043098171999798, 12.19104765307000093 ) ) ;
#48351 = CARTESIAN_POINT ( 'NONE',  ( 10.40558062080000035, -5.599331384652000310, -8.437753779290000367 ) ) ;
#48352 = ADVANCED_FACE ( 'NONE', ( #55948 ), #33422, .T. ) ;
#48353 = EDGE_LOOP ( 'NONE', ( #41014, #26768, #32527, #19182, #42262 ) ) ;
#48354 = ORIENTED_EDGE ( 'NONE', *, *, #36470, .T. ) ;
#48355 = CARTESIAN_POINT ( 'NONE',  ( 8.672510841228998402, 4.686731264770999772, -8.717075579553000608 ) ) ;
#48356 = CARTESIAN_POINT ( 'NONE',  ( 10.08061813254432693, 5.349721876211404492, -7.768808602171199951 ) ) ;
#48357 = CARTESIAN_POINT ( 'NONE',  ( 8.637503779817164329, -3.056533381831490814, -6.534278797312786047 ) ) ;
#48358 = CARTESIAN_POINT ( 'NONE',  ( 4.000000000000000000, 0.000000000000000000, 0.000000000000000000 ) ) ;
#48359 = CARTESIAN_POINT ( 'NONE',  ( 12.75651925148578414, 0.7192569394297179119, 12.57945425907934300 ) ) ;
#48360 = TOROIDAL_SURFACE ( 'NONE', #58443, 12.35000000006999876, 0.5000000000000000000 ) ;
#48361 = CARTESIAN_POINT ( 'NONE',  ( 5.500000000000000000, 1.449999999999999956, 0.000000000000000000 ) ) ;
#48362 = CARTESIAN_POINT ( 'NONE',  ( 9.737988259786000356, 3.886559292927400211, -8.359557531806398600 ) ) ;
#48364 = CARTESIAN_POINT ( 'NONE',  ( 2.029064736457000251, 3.399126080497508973, -0.9633645835951684111 ) ) ;
#48363 = CARTESIAN_POINT ( 'NONE',  ( 10.22898825978600001, -4.113440707072600233, 6.640442468193600511 ) ) ;
#48365 = CARTESIAN_POINT ( 'NONE',  ( 7.905017292225999803, -2.916160783733999562, 6.437838678341997856 ) ) ;
#48366 = VERTEX_POINT ( 'NONE', #33773 ) ;
#48367 = AXIS2_PLACEMENT_3D ( 'NONE', #46054, #40131, #19481 ) ;
#48368 = PRODUCT_DEFINITION_SHAPE ( 'NONE', 'NONE',  #69199 ) ;
#48369 = CARTESIAN_POINT ( 'NONE',  ( 7.100000000000000533, -4.000000000000000000, -7.500000000000000000 ) ) ;
#48370 = CARTESIAN_POINT ( 'NONE',  ( 9.533427734455999669, -2.564762519363000148, 6.150594768287000136 ) ) ;
#48371 = CARTESIAN_POINT ( 'NONE',  ( 10.03696314287999947, 5.117257953482000410, 7.735518817439499983 ) ) ;
#48372 = CARTESIAN_POINT ( 'NONE',  ( 11.29998578400000042, -3.824193979571000046, 11.71675423233000046 ) ) ;
#48373 = CARTESIAN_POINT ( 'NONE',  ( 10.96080136920999948, -2.054580854576999904, 7.810082699133999995 ) ) ;
#48374 = CARTESIAN_POINT ( 'NONE',  ( 18.15015087275886074, 2.691082634156150899, -12.40501869842431937 ) ) ;
#48375 = CARTESIAN_POINT ( 'NONE',  ( 10.14393020684899938, 5.250000000000000000, 7.500000000000000000 ) ) ;
#48376 = ADVANCED_FACE ( 'NONE', ( #919 ), #16980, .T. ) ;
#48377 = EDGE_CURVE ( 'NONE', #29064, #65266, #1954, .T. ) ;
#48378 = AXIS2_PLACEMENT_3D ( 'NONE', #29268, #2339, #44316 ) ;
#48379 = CARTESIAN_POINT ( 'NONE',  ( 9.735975701333000387, -3.263119632394099856, -8.182531775206799196 ) ) ;
#48380 = ADVANCED_FACE ( 'NONE', ( #64867 ), #12967, .T. ) ;
#48381 = CARTESIAN_POINT ( 'NONE',  ( 5.526874906801999998, 1.281289678559000000, 0.3267609307802000207 ) ) ;
#48382 = CARTESIAN_POINT ( 'NONE',  ( 11.02606775832648189, -4.343526402396090447, 8.303790528164435969 ) ) ;
#48383 = VECTOR ( 'NONE', #5356, 1000.000000000000000 ) ;
#48384 = CARTESIAN_POINT ( 'NONE',  ( 0.1499942179679999987, -2.750000000000000000, 0.000000000000000000 ) ) ;
#48385 = VERTEX_POINT ( 'NONE', #55088 ) ;
#48386 = CARTESIAN_POINT ( 'NONE',  ( 12.24208977126479070, 0.2715269968477689311, -12.69609476950841831 ) ) ;
#48387 = CARTESIAN_POINT ( 'NONE',  ( 11.73671932425159881, 3.872987101045399783, -8.356835045446798560 ) ) ;
#48388 = CARTESIAN_POINT ( 'NONE',  ( 10.99999970531878013, -5.098631745860898512, -7.597293174631950308 ) ) ;
#48389 = CARTESIAN_POINT ( 'NONE',  ( 8.392328736400999745, 5.100230418103000041, 6.589669365926999589 ) ) ;
#48390 = CARTESIAN_POINT ( 'NONE',  ( 5.660639688932317171, 12.98305835826268151, 2.241106542164481130 ) ) ;
#48391 = ORIENTED_EDGE ( 'NONE', *, *, #25587, .F. ) ;
#48392 = CARTESIAN_POINT ( 'NONE',  ( 24.98214874725099932, -11.60529347923999843, -3.133086993850000113 ) ) ;
#48393 = APPLICATION_PROTOCOL_DEFINITION ( 'draft international standard', 'automotive_design', 1998, #24408 ) ;
#48394 = CARTESIAN_POINT ( 'NONE',  ( 10.89835090130999973, -3.121033016283800254, -8.043647632228999811 ) ) ;
#48395 = CARTESIAN_POINT ( 'NONE',  ( 12.09999999999999964, -2.792989229543000107, 7.174999999999999822 ) ) ;
#48396 = CARTESIAN_POINT ( 'NONE',  ( 25.44993821361100217, -11.77655473258999841, -4.190794510628000680 ) ) ;
#48397 = DIRECTION ( 'NONE',  ( 1.000000000000000000, 0.000000000000000000, 0.000000000000000000 ) ) ;
#48398 = CARTESIAN_POINT ( 'NONE',  ( 10.29399293566599916, 4.546741702992100009, -8.170700474995699736 ) ) ;
#48399 = ORIENTED_EDGE ( 'NONE', *, *, #44196, .T. ) ;
#48400 = CARTESIAN_POINT ( 'NONE',  ( 9.834153701540001791, -5.173926576843999925, 8.813045240277000758 ) ) ;
#48401 = CARTESIAN_POINT ( 'NONE',  ( 17.63808658539555907, 3.119809217581025251, -13.52227901589168546 ) ) ;
#48402 = ORIENTED_EDGE ( 'NONE', *, *, #61726, .T. ) ;
#48403 = EDGE_CURVE ( 'NONE', #7217, #46086, #16991, .T. ) ;
#48404 = CARTESIAN_POINT ( 'NONE',  ( 11.01356641589999974, 2.786433584103999994, 6.253463831328000211 ) ) ;
#48405 = CARTESIAN_POINT ( 'NONE',  ( 9.497293146791999874, -3.734278838175999482, 8.942129638874000364 ) ) ;
#48406 = CARTESIAN_POINT ( 'NONE',  ( 15.39518154839200115, 8.837017240434999366, 7.949877004991000362 ) ) ;
#48407 = EDGE_LOOP ( 'NONE', ( #30383, #39440, #67146, #59676, #38816, #5549 ) ) ;
#48408 = CARTESIAN_POINT ( 'NONE',  ( 6.388158200622003235, 1.399447465758937303, 0.6237406411839149234 ) ) ;
#48409 = CARTESIAN_POINT ( 'NONE',  ( 7.116410841227000184, 2.101490574575000103, -7.427795877530000368 ) ) ;
#48410 = CARTESIAN_POINT ( 'NONE',  ( 10.27101354018233437, -4.768183399968641822, -6.500416447002272058 ) ) ;
#48411 = CARTESIAN_POINT ( 'NONE',  ( 9.498145159330512399, 4.816870420262897134, 8.576492378600933719 ) ) ;
#48412 = VERTEX_POINT ( 'NONE', #39356 ) ;
#48413 = CARTESIAN_POINT ( 'NONE',  ( 11.15982711745999900, -5.578228817597000955, 8.067792329320999656 ) ) ;
#48414 = B_SPLINE_CURVE_WITH_KNOTS ( 'NONE', 3,
 ( #61651, #67228, #35098, #20034, #14110, #45239, #23903, #8513, #30194, #34751, #24596, #24246, #66889, #29861, #24933, #41015, #51169, #46267, #3264, #61997 ),
 .UNSPECIFIED., .F., .F.,
 ( 4, 2, 2, 2, 2, 2, 2, 2, 2, 4 ),
 ( 0.000000000000000000, 0.06250000000000000000, 0.1250000000000000000, 0.2500000000000000555, 0.3750000000000001110, 0.5000000000000001110, 0.6250000000000001110, 0.7500000000000001110, 0.8750000000000001110, 1.000000000000000000 ),
 .UNSPECIFIED. ) ;
#48415 = B_SPLINE_CURVE_WITH_KNOTS ( 'NONE', 3,
 ( #61020, #34115, #34801, #67619 ),
 .UNSPECIFIED., .F., .F.,
 ( 4, 4 ),
 ( 0.000000000000000000, 1.000000000000000000 ),
 .UNSPECIFIED. ) ;
#48416 = LINE ( 'NONE', #63452, #20586 ) ;
#48417 = ORIENTED_EDGE ( 'NONE', *, *, #64332, .T. ) ;
#48418 = CIRCLE ( 'NONE', #49566, 12.99999854704999969 ) ;
#48419 = CARTESIAN_POINT ( 'NONE',  ( 11.29998636608000062, -3.695122995756999984, 11.25914041192000070 ) ) ;
#48420 = DIRECTION ( 'NONE',  ( -1.000000000000000000, 0.000000000000000000, 0.000000000000000000 ) ) ;
#48421 = ORIENTED_EDGE ( 'NONE', *, *, #49081, .T. ) ;
#48422 = CARTESIAN_POINT ( 'NONE',  ( 24.30000000000000071, 3.224868684338999980, 12.03537377768999939 ) ) ;
#48423 = DIRECTION ( 'NONE',  ( 0.000000000000000000, 0.2461538461537955691, -0.9692307692307821076 ) ) ;
#48424 = CARTESIAN_POINT ( 'NONE',  ( 4.442764461075999982, -1.247736568755000164, 0.6705067152884000015 ) ) ;
#48425 = CARTESIAN_POINT ( 'NONE',  ( 8.389220148804989563, 5.100598871404000256, -6.637806542482997507 ) ) ;
#48426 = B_SPLINE_CURVE_WITH_KNOTS ( 'NONE', 3,
 ( #27593, #5911, #10134, #48919, #10470, #47550, #68853, #47893, #42309, #1027, #5570, #64288, #48574, #42641, #32842, #41951, #4879, #63950 ),
 .UNSPECIFIED., .F., .F.,
 ( 4, 2, 2, 2, 2, 2, 2, 2, 4 ),
 ( 0.000000000000000000, 0.1250000000000000000, 0.2500000000000000000, 0.3750000000000000000, 0.5000000000000000000, 0.6250000000000000000, 0.7500000000000000000, 0.8750000000000000000, 1.000000000000000000 ),
 .UNSPECIFIED. ) ;
#48427 = CARTESIAN_POINT ( 'NONE',  ( 16.27269624719400198, 3.670072847095000146, 12.01573327568000060 ) ) ;
#48428 = CARTESIAN_POINT ( 'NONE',  ( 10.60454270958608625, 3.072761288248648359, 8.633924816819705583 ) ) ;
#48429 = DIRECTION ( 'NONE',  ( 0.000000000000000000, -0.9421243786071877846, -0.3352635608502959608 ) ) ;
#48430 = ORIENTED_EDGE ( 'NONE', *, *, #14747, .F. ) ;
#48431 = CARTESIAN_POINT ( 'NONE',  ( 9.321533510307233428, -4.073328655874168369, 9.239113755467350586 ) ) ;
#48432 = ORIENTED_EDGE ( 'NONE', *, *, #53352, .F. ) ;
#48433 = CARTESIAN_POINT ( 'NONE',  ( 10.83658792121999959, 5.133186143592999962, 8.848368005200001107 ) ) ;
#48434 = CARTESIAN_POINT ( 'NONE',  ( 10.07762665876999897, 2.169012810937000157, -7.244984731085000185 ) ) ;
#48435 =( GEOMETRIC_REPRESENTATION_CONTEXT ( 3 ) GLOBAL_UNCERTAINTY_ASSIGNED_CONTEXT ( ( #55353 ) ) GLOBAL_UNIT_ASSIGNED_CONTEXT ( ( #65933, #38335, #7558 ) ) REPRESENTATION_CONTEXT ( 'NONE', 'WORKASPACE' ) );
#48436 = CARTESIAN_POINT ( 'NONE',  ( 17.82402932260216133, -11.54140372737312425, 4.865356140869725898 ) ) ;
#48437 = CARTESIAN_POINT ( 'NONE',  ( 12.57359775157566695, 3.080655040460396066, -13.53300991339124870 ) ) ;
#48438 = CARTESIAN_POINT ( 'NONE',  ( 21.60000000000000142, 0.000000000000000000, 0.000000000000000000 ) ) ;
#48439 = B_SPLINE_CURVE_WITH_KNOTS ( 'NONE', 3,
 ( #13699, #67848, #66475, #18599 ),
 .UNSPECIFIED., .F., .F.,
 ( 4, 4 ),
 ( 0.000000000000000000, 1.000000000000000000 ),
 .UNSPECIFIED. ) ;
#48440 = DIRECTION ( 'NONE',  ( 1.000000000000000000, 0.000000000000000000, 0.000000000000000000 ) ) ;
#48441 = CARTESIAN_POINT ( 'NONE',  ( 18.11587426570509862, 0.2766185922798710117, 13.89631150889696798 ) ) ;
#48442 = AXIS2_PLACEMENT_3D ( 'NONE', #23486, #6355, #27703 ) ;
#48443 = CARTESIAN_POINT ( 'NONE',  ( 9.266298948830003823, -5.052976874734789625, -6.103419532891559030 ) ) ;
#48444 = EDGE_CURVE ( 'NONE', #19018, #46752, #6979, .T. ) ;
#48446 = EDGE_CURVE ( 'NONE', #58012, #39722, #2893, .T. ) ;
#48445 = B_SPLINE_CURVE_WITH_KNOTS ( 'NONE', 3,
 ( #22397, #38481, #7011, #43736, #53534, #5626, #32897, #65032, #59804, #28345 ),
 .UNSPECIFIED., .F., .F.,
 ( 4, 2, 2, 2, 4 ),
 ( 0.000000000000000000, 0.2500000000000000000, 0.5000000000000000000, 0.7500000000000000000, 1.000000000000000000 ),
 .UNSPECIFIED. ) ;
#48447 = EDGE_LOOP ( 'NONE', ( #66010, #56360, #27343, #68722 ) ) ;
#48448 = CARTESIAN_POINT ( 'NONE',  ( 12.31443335393315586, 0.3873583149501338418, 13.89273910398916279 ) ) ;
#48449 = CARTESIAN_POINT ( 'NONE',  ( 10.77610941423800028, -3.155589807313900153, 8.266982106121901097 ) ) ;
#48450 = FACE_BOUND ( 'NONE', #17989, .T. ) ;
#48451 = CARTESIAN_POINT ( 'NONE',  ( 6.899999691988000450, -12.99045401563999924, -1.690592933733000125 ) ) ;
#48452 = CARTESIAN_POINT ( 'NONE',  ( 8.849379440379999906, -3.975070057433999438, 9.483761758588999058 ) ) ;
#48454 = CARTESIAN_POINT ( 'NONE',  ( 7.866263695695000280, -4.690788429020999573, 6.339954069160000039 ) ) ;
#48453 = CARTESIAN_POINT ( 'NONE',  ( 10.53138775541999905, 5.607751175212000838, 7.280102404048999887 ) ) ;
#48455 = CARTESIAN_POINT ( 'NONE',  ( 11.61759063708296047, 5.217265640542000149, -7.842242470354300110 ) ) ;
#48456 = CARTESIAN_POINT ( 'NONE',  ( 24.51228084553499897, -8.787217699239999291, -8.912727655930000381 ) ) ;
#48457 = CARTESIAN_POINT ( 'NONE',  ( 7.000000000000000000, 0.8000000000000000444, -3.149999999999999911 ) ) ;
#48458 = CARTESIAN_POINT ( 'NONE',  ( 17.95947714806421658, -0.4766234715920697473, 12.68796191786312910 ) ) ;
#48459 = B_SPLINE_SURFACE_WITH_KNOTS ( 'NONE', 3, 3, ( 
 ( #35062, #8137, #39960, #51130 ),
 ( #24899, #40295, #61277, #67536 ),
 ( #62303, #3564, #45551, #61614 ),
 ( #19660, #28788, #55341, #46229 ),
 ( #13395, #44862, #40629, #66856 ),
 ( #34717, #56028, #3233, #45883 ),
 ( #61963, #35399, #40980, #14421 ),
 ( #50099, #2208, #4593, #58091 ),
 ( #25929, #46915, #5287, #26629 ),
 ( #63665, #57389, #47, #53189 ) ),
 .UNSPECIFIED., .F., .F., .F.,
 ( 4, 1, 1, 1, 1, 1, 1, 4 ),
 ( 4, 4 ),
 ( 0.04183311431308000400, 0.1428571428570999946, 0.2857142857143000203, 0.4285714285713999594, 0.5714285714286000406, 0.7142857142856999797, 0.8571428571429000609, 0.9292981235707000742 ),
 ( -0.1917799910644999994, 1.191756862851000021 ),
 .UNSPECIFIED. ) ;
#48460 = AXIS2_PLACEMENT_3D ( 'NONE', #36835, #15510, #25304 ) ;
#48461 = CARTESIAN_POINT ( 'NONE',  ( 11.09999999999999964, -5.520231155209834206, 6.955941087530958633 ) ) ;
#48462 = CARTESIAN_POINT ( 'NONE',  ( 18.36021383541356400, -3.331512994333476030, 12.07398673550533630 ) ) ;
#48463 = ORIENTED_EDGE ( 'NONE', *, *, #59342, .F. ) ;
#48464 = CARTESIAN_POINT ( 'NONE',  ( 7.930394353207000258, -3.164807285701999984, 9.104732190648000767 ) ) ;
#48465 = CARTESIAN_POINT ( 'NONE',  ( 8.921614158776000281, 3.251172436837000301, -6.320036569851000152 ) ) ;
#48466 = EDGE_CURVE ( 'NONE', #58398, #23213, #4484, .T. ) ;
#48467 = CARTESIAN_POINT ( 'NONE',  ( 10.98768553379999879, -5.299329486732999861, 4.945210549701000602 ) ) ;
#48468 = DIRECTION ( 'NONE',  ( 0.000000000000000000, 1.000000000000000000, 0.000000000000000000 ) ) ;
#48469 = AXIS2_PLACEMENT_3D ( 'NONE', #51131, #35739, #36076 ) ;
#48470 = EDGE_CURVE ( 'NONE', #23714, #62083, #52014, .T. ) ;
#48471 = CARTESIAN_POINT ( 'NONE',  ( 13.49980696792482959, -11.86896009962648613, -3.468589882356420073 ) ) ;
#48472 = CARTESIAN_POINT ( 'NONE',  ( 10.73724174883999893, 3.975468761016990094, 6.608211443991299561 ) ) ;
#48473 = CARTESIAN_POINT ( 'NONE',  ( 10.72802334123000101, 3.751278653658999929, -8.836901076820000256 ) ) ;
#48474 = ORIENTED_EDGE ( 'NONE', *, *, #66377, .T. ) ;
#48475 = CARTESIAN_POINT ( 'NONE',  ( 9.341834235717472623, 3.000408294236256435, -6.731799792051354814 ) ) ;
#48476 = DIRECTION ( 'NONE',  ( 1.000000000000000000, 0.000000000000000000, 0.000000000000000000 ) ) ;
#48477 = CARTESIAN_POINT ( 'NONE',  ( 17.60324894539389717, 3.198552395131802228, -12.18725844837785210 ) ) ;
#48478 = CARTESIAN_POINT ( 'NONE',  ( 5.584969860380273765, 12.14796130796948859, 3.754865623502155358 ) ) ;
#48479 = CARTESIAN_POINT ( 'NONE',  ( 7.512829719590000010, 5.524123123935000379, 6.910361319981999095 ) ) ;
#48480 = ORIENTED_EDGE ( 'NONE', *, *, #19012, .F. ) ;
#48481 = CARTESIAN_POINT ( 'NONE',  ( 5.903117865652999896, -0.8041423837011999476, 1.228772791746999937 ) ) ;
#48482 = CARTESIAN_POINT ( 'NONE',  ( 8.254179719588000452, 3.402419637676000086, -5.873899751133000002 ) ) ;
#48483 = CARTESIAN_POINT ( 'NONE',  ( 8.449875654718679741, -2.260415483100814082, 7.498025105998177509 ) ) ;
#48484 = PRESENTATION_LAYER_ASSIGNMENT (  '', '', ( #472 ) ) ;
#48485 = CARTESIAN_POINT ( 'NONE',  ( 9.320101285864000218, -4.823683599683300294, 8.478738839062499366 ) ) ;
#48486 = EDGE_LOOP ( 'NONE', ( #30873, #20052, #12930, #26910, #59841 ) ) ;
#48487 = CARTESIAN_POINT ( 'NONE',  ( 16.07476513888299863, -3.720976809451999934, -11.90233817890000090 ) ) ;
#48488 = CARTESIAN_POINT ( 'NONE',  ( 11.84802180303800156, 11.72322844712000034, 1.964617572541000001 ) ) ;
#48489 = VERTEX_POINT ( 'NONE', #45297 ) ;
#48490 = EDGE_CURVE ( 'NONE', #4028, #42555, #55403, .T. ) ;
#48491 = CARTESIAN_POINT ( 'NONE',  ( 0.2153359931920000025, 3.215315751876999695, 1.126573897625000029E-09 ) ) ;
#48492 = CARTESIAN_POINT ( 'NONE',  ( 7.717918984469999799, -2.852331559125000027, 6.784354950350999225 ) ) ;
#48493 = VECTOR ( 'NONE', #53394, 1000.000000000000000 ) ;
#48494 = CARTESIAN_POINT ( 'NONE',  ( 18.17602483311041439, -0.07155107330948752564, -13.89975717292030311 ) ) ;
#48495 = ORIENTED_EDGE ( 'NONE', *, *, #50970, .F. ) ;
#48496 = CARTESIAN_POINT ( 'NONE',  ( 15.96457203294418470, -8.635839794705725936, -7.819790491317134773 ) ) ;
#48497 = CARTESIAN_POINT ( 'NONE',  ( 8.893204545404998385, -3.399999999998999822, -6.188268997420999007 ) ) ;
#48498 = DIRECTION ( 'NONE',  ( 1.000000000000000000, 0.000000000000000000, 0.000000000000000000 ) ) ;
#48499 = CARTESIAN_POINT ( 'NONE',  ( 11.53935385204242436, 3.267863779230346211, -11.38835623221634741 ) ) ;
#48500 = CARTESIAN_POINT ( 'NONE',  ( 11.75656651104150008, -3.873914634362100262, 8.771777834828998976 ) ) ;
#48501 = ORIENTED_EDGE ( 'NONE', *, *, #37497, .T. ) ;
#48502 = CARTESIAN_POINT ( 'NONE',  ( 8.566232780412001091, 5.212261578733999201, 6.157186134061999994 ) ) ;
#48503 = ORIENTED_EDGE ( 'NONE', *, *, #64818, .F. ) ;
#48504 = CARTESIAN_POINT ( 'NONE',  ( 11.16486084871730000, 5.207010770456999893, 7.825000000000000178 ) ) ;
#48505 = FACE_OUTER_BOUND ( 'NONE', #59729, .T. ) ;
#48506 = CARTESIAN_POINT ( 'NONE',  ( 9.009297488802992859, -5.100000000000000533, 6.455145051482742424 ) ) ;
#48507 = ORIENTED_EDGE ( 'NONE', *, *, #11583, .T. ) ;
#48508 = CARTESIAN_POINT ( 'NONE',  ( 12.29407742813166493, -2.139519579705956076, -12.52828553530646793 ) ) ;
#48509 = CARTESIAN_POINT ( 'NONE',  ( 16.10004050617000004, -3.886235259787000018, -11.90683839252000098 ) ) ;
#48510 = CARTESIAN_POINT ( 'NONE',  ( 9.099999931440999390, 5.246365646610000155, -7.404749409716440134 ) ) ;
#48511 = CARTESIAN_POINT ( 'NONE',  ( 9.112942518363999156, 5.100000000000000533, 6.192000867487999827 ) ) ;
#48512 = CARTESIAN_POINT ( 'NONE',  ( 12.09886375431306682, -2.684759089869698467, -13.74018286504950659 ) ) ;
#48513 = CARTESIAN_POINT ( 'NONE',  ( 11.70379573085659786, -2.893744357957000357, -7.691418046581699919 ) ) ;
#48514 = CARTESIAN_POINT ( 'NONE',  ( 12.75601781081296693, -1.760880198315417200, 12.47634966360013919 ) ) ;
#48515 = CARTESIAN_POINT ( 'NONE',  ( 17.99878237954355598, -3.049368882785702173, 12.22543920180491384 ) ) ;
#48516 = EDGE_LOOP ( 'NONE', ( #40118, #15313, #46977, #11502, #55324 ) ) ;
#48517 = CARTESIAN_POINT ( 'NONE',  ( 11.47500581613029880, -3.011381429075500105, -8.134817373646898275 ) ) ;
#48518 = ORIENTED_EDGE ( 'NONE', *, *, #4916, .F. ) ;
#48519 = VECTOR ( 'NONE', #2476, 1000.000000000000000 ) ;
#48520 = CARTESIAN_POINT ( 'NONE',  ( 5.700000000000000178, 0.000000000000000000, 0.000000000000000000 ) ) ;
#48521 = CARTESIAN_POINT ( 'NONE',  ( 11.99200216175158396, -4.419830582853482071, 6.297929225185963986 ) ) ;
#48522 = CARTESIAN_POINT ( 'NONE',  ( 5.152393060466970987, -0.3471830745757842340, 1.190476739849418042 ) ) ;
#48523 = B_SPLINE_CURVE_WITH_KNOTS ( 'NONE', 3,
 ( #20086, #35825, #67283, #8569 ),
 .UNSPECIFIED., .F., .F.,
 ( 4, 4 ),
 ( 0.000000000000000000, 1.000000000000000000 ),
 .UNSPECIFIED. ) ;
#48524 = CARTESIAN_POINT ( 'NONE',  ( 10.29094647910999782, -2.903513699412000104, -8.310923036409999298 ) ) ;
#48525 = CARTESIAN_POINT ( 'NONE',  ( 24.30000000000000071, 12.03537377768999939, -3.224868684338999980 ) ) ;
#48526 = CARTESIAN_POINT ( 'NONE',  ( 8.045433776029998540, 2.903894639863001892, -6.425841880607995549 ) ) ;
#48527 = EDGE_CURVE ( 'NONE', #59889, #49507, #676, .T. ) ;
#48529 = EDGE_CURVE ( 'NONE', #19729, #10762, #14167, .T. ) ;
#48528 = LINE ( 'NONE', #43284, #6540 ) ;
#48530 = ORIENTED_EDGE ( 'NONE', *, *, #66687, .T. ) ;
#48531 = CARTESIAN_POINT ( 'NONE',  ( 18.26001156276199922, 2.811979134698999960, 11.55266638147999991 ) ) ;
#48532 = EDGE_CURVE ( 'NONE', #8437, #26260, #46323, .T. ) ;
#48533 = EDGE_CURVE ( 'NONE', #4646, #49898, #27913, .T. ) ;
#48534 = CARTESIAN_POINT ( 'NONE',  ( 9.352253013669001191, 2.817757427878999632, 6.388459691516000127 ) ) ;
#48535 = CARTESIAN_POINT ( 'NONE',  ( 10.47094409420000005, 5.100000000000000533, 6.571291218949999902 ) ) ;
#48536 = CARTESIAN_POINT ( 'NONE',  ( 11.36190547754509872, -3.108323067758099967, 7.471700551735359852 ) ) ;
#48537 = CARTESIAN_POINT ( 'NONE',  ( 9.222206734151470187, 2.649920175418960078, 7.547759605734272625 ) ) ;
#48538 = VECTOR ( 'NONE', #49732, 1000.000000000000000 ) ;
#48539 = CARTESIAN_POINT ( 'NONE',  ( 11.37299956498129916, 2.792989229543000107, 7.825000000000000178 ) ) ;
#48540 = CARTESIAN_POINT ( 'NONE',  ( 7.100000000000436629, 3.640294921184452637, -6.161369192892991897 ) ) ;
#48541 = AXIS2_PLACEMENT_3D ( 'NONE', #57873, #25366, #67318 ) ;
#48542 = CARTESIAN_POINT ( 'NONE',  ( 23.61700687049500047, -10.26325659442000138, -9.294095019069999353 ) ) ;
#48543 = CARTESIAN_POINT ( 'NONE',  ( 24.21981597650900042, -9.186995683914000566, 9.646844606695998081 ) ) ;
#48544 = CARTESIAN_POINT ( 'NONE',  ( 23.59999999999999787, -12.52456686791425966, 6.096434097048058831 ) ) ;
#48545 = ORIENTED_EDGE ( 'NONE', *, *, #7883, .T. ) ;
#48546 = FACE_OUTER_BOUND ( 'NONE', #7662, .T. ) ;
#48547 = CARTESIAN_POINT ( 'NONE',  ( 7.028330717051000320, 0.9502619346694000102, -0.6159082020391000167 ) ) ;
#48548 = CARTESIAN_POINT ( 'NONE',  ( 18.15864108120890208, 2.662504769557530793, 13.63760133890561654 ) ) ;
#48549 = CARTESIAN_POINT ( 'NONE',  ( 10.87208388804061698, 5.035013780143576589, 4.888821408800270163 ) ) ;
#48550 = AXIS2_PLACEMENT_3D ( 'NONE', #6425, #49781, #38246 ) ;
#48551 = CARTESIAN_POINT ( 'NONE',  ( 10.91610672858429965, -4.911600290708499905, -6.814233985789400094 ) ) ;
#48552 = VERTEX_POINT ( 'NONE', #3317 ) ;
#48553 = B_SPLINE_CURVE_WITH_KNOTS ( 'NONE', 3,
 ( #29652, #64691, #11905, #45372 ),
 .UNSPECIFIED., .F., .F.,
 ( 4, 4 ),
 ( 0.000000000000000000, 1.000000000000000000 ),
 .UNSPECIFIED. ) ;
#48554 = CARTESIAN_POINT ( 'NONE',  ( 6.987460761722542379, -1.412538709148827731, 0.3006784195689278238 ) ) ;
#48555 = CARTESIAN_POINT ( 'NONE',  ( 8.026329719592000700, 5.601795057054999916, 7.176148573050999957 ) ) ;
#48557 = DIRECTION ( 'NONE',  ( -0.000000000000000000, -0.000000000000000000, 1.000000000000000000 ) ) ;
#48556 = CARTESIAN_POINT ( 'NONE',  ( 9.500595280412998278, 2.334550724494000029, -7.977056617806000283 ) ) ;
#48559 = B_SPLINE_CURVE_WITH_KNOTS ( 'NONE', 3,
 ( #60044, #59012, #11115, #12154 ),
 .UNSPECIFIED., .F., .F.,
 ( 4, 4 ),
 ( 0.5000000000000044409, 1.000000000000000000 ),
 .UNSPECIFIED. ) ;
#48558 = CARTESIAN_POINT ( 'NONE',  ( 2.771536717063348476, 3.252280351444815309, -0.1916433810219522749 ) ) ;
#48560 = ORIENTED_EDGE ( 'NONE', *, *, #14607, .T. ) ;
#48561 = CARTESIAN_POINT ( 'NONE',  ( 10.48165121391000021, 4.022873529486999722, 9.090897232145000117 ) ) ;
#48562 = CARTESIAN_POINT ( 'NONE',  ( 18.27459401263896055, -2.425695574333701199, -13.78827716170582107 ) ) ;
#48563 = CARTESIAN_POINT ( 'NONE',  ( 11.77359063708300013, 4.955772084214699724, 7.231278212164300001 ) ) ;
#48564 = CARTESIAN_POINT ( 'NONE',  ( 10.57223537388000167, -4.020426196685999543, 8.920680607665000039 ) ) ;
#48565 = CARTESIAN_POINT ( 'NONE',  ( 9.079730646793999327, -5.421531391267000011, 6.381128921159999301 ) ) ;
#48566 = ORIENTED_EDGE ( 'NONE', *, *, #37701, .F. ) ;
#48567 = CARTESIAN_POINT ( 'NONE',  ( 24.46225079000999969, 12.39903786276999931, -3.098987673317000091 ) ) ;
#48569 = CARTESIAN_POINT ( 'NONE',  ( 10.33453064679000200, -3.295701412239999684, -6.149875347297999895 ) ) ;
#48568 = CARTESIAN_POINT ( 'NONE',  ( 12.18555568849200021, -11.56145208044000050, 4.416819796118000241 ) ) ;
#48570 = CARTESIAN_POINT ( 'NONE',  ( 7.898140067141143028, -2.604783987062581296, 8.538297895486305578 ) ) ;
#48571 = CARTESIAN_POINT ( 'NONE',  ( 10.34020413671000149, -4.202027362542999356, 9.459588031742001135 ) ) ;
#48572 = CARTESIAN_POINT ( 'NONE',  ( 10.04762827527057212, -4.043475410182937324, 8.964136762659371982 ) ) ;
#48573 = ORIENTED_EDGE ( 'NONE', *, *, #24217, .F. ) ;
#48574 = CARTESIAN_POINT ( 'NONE',  ( 5.677943173016667622, -0.9218200799623716968, -1.199500263597270910 ) ) ;
#48575 = CARTESIAN_POINT ( 'NONE',  ( 11.42026088462129962, -3.997864853650589634, 8.503467136482999678 ) ) ;
#48576 = ADVANCED_FACE ( 'NONE', ( #56467 ), #27424, .F. ) ;
#48577 = CARTESIAN_POINT ( 'NONE',  ( 11.03502897915239878, 4.327133900127000388, 6.264564938179000286 ) ) ;
#48578 = MECHANICAL_DESIGN_GEOMETRIC_PRESENTATION_REPRESENTATION (  '', ( #45245 ), #25117 ) ;
#48579 = ORIENTED_EDGE ( 'NONE', *, *, #46541, .F. ) ;
#48580 = CARTESIAN_POINT ( 'NONE',  ( 9.459729719592999686, 2.527713920559999661, -6.969421869128999525 ) ) ;
#48581 = ADVANCED_FACE ( 'NONE', ( #61706 ), #41071, .T. ) ;
#48582 = CARTESIAN_POINT ( 'NONE',  ( 12.58121427537365022, 1.795950320080887730, -12.47134981075813087 ) ) ;
#48583 = CARTESIAN_POINT ( 'NONE',  ( 12.22433327354039889, -4.983220429128399687, 8.143111181492699302 ) ) ;
#48584 = VERTEX_POINT ( 'NONE', #50879 ) ;
#48585 = CARTESIAN_POINT ( 'NONE',  ( 9.314928906318884927, 2.650140463285438397, -7.499996151983930659 ) ) ;
#48586 = DIRECTION ( 'NONE',  ( -0.9999999999999978906, 6.450930526679976792E-08, 1.612071427334991320E-09 ) ) ;
#48587 = VERTEX_POINT ( 'NONE', #67974 ) ;
#48588 = CARTESIAN_POINT ( 'NONE',  ( 8.753441940380000119, -2.876278577719999952, 6.568889245344999850 ) ) ;
#48589 = CARTESIAN_POINT ( 'NONE',  ( 23.61437340957948194, 10.18034756477473124, 9.423219428857132485 ) ) ;
#48590 = ORIENTED_EDGE ( 'NONE', *, *, #31575, .F. ) ;
#48591 = CARTESIAN_POINT ( 'NONE',  ( 12.56425374667833950, -3.158898859712414797, -12.19759658245784628 ) ) ;
#48593 = CARTESIAN_POINT ( 'NONE',  ( 11.60948876160955479, 3.304472173606900043, 6.776679950459500112 ) ) ;
#48592 = AXIS2_PLACEMENT_3D ( 'NONE', #26287, #20693, #62977 ) ;
#48594 = CARTESIAN_POINT ( 'NONE',  ( 10.99933470386000067, 5.081013421858999735, 8.239043921879998678 ) ) ;
#48595 = CARTESIAN_POINT ( 'NONE',  ( 9.947306532704999427, 4.892812229297999416, -9.067756197920999739 ) ) ;
#48596 = CARTESIAN_POINT ( 'NONE',  ( 9.216851002545999094, 2.832432432432000269, 6.822293592207000934 ) ) ;
#48597 = CARTESIAN_POINT ( 'NONE',  ( 10.69031285273999821, -5.903020122789000013, 7.830708506196000229 ) ) ;
#48598 = CARTESIAN_POINT ( 'NONE',  ( 13.73732479921000049, 9.700721122729000001, 7.982825098500999417 ) ) ;
#48599 = CARTESIAN_POINT ( 'NONE',  ( 17.98240372392063335, 0.4561785182478261813, -12.68897339690747295 ) ) ;
#48600 = CARTESIAN_POINT ( 'NONE',  ( 12.19483627237708134, 2.635236894562234866, -12.41905446250361678 ) ) ;
#48601 = CARTESIAN_POINT ( 'NONE',  ( 10.69456919669529960, -2.906008650422999828, -7.823222900359999343 ) ) ;
#48602 = CARTESIAN_POINT ( 'NONE',  ( 8.560885841230001958, 4.228291488957999888, 8.941375734143997889 ) ) ;
#48603 = ORIENTED_EDGE ( 'NONE', *, *, #32196, .F. ) ;
#48604 =( LENGTH_UNIT ( ) NAMED_UNIT ( * ) SI_UNIT ( .MILLI., .METRE. ) );
#48605 = CARTESIAN_POINT ( 'NONE',  ( 10.35685100253999913, 2.832432432432000269, -6.822293592207000934 ) ) ;
#48606 = FACE_OUTER_BOUND ( 'NONE', #57449, .T. ) ;
#48607 = CARTESIAN_POINT ( 'NONE',  ( 11.80877518040099972, 12.11591042788000117, 2.033719807695000270 ) ) ;
#48608 = CARTESIAN_POINT ( 'NONE',  ( 18.15405049586274444, 2.074720874654909064, 12.42801810613654823 ) ) ;
#48609 = CARTESIAN_POINT ( 'NONE',  ( 11.12484646121000154, 6.576544621967000737, 5.637917610392999990 ) ) ;
#48611 = ADVANCED_FACE ( 'NONE', ( #29577 ), #30825, .T. ) ;
#48610 = CARTESIAN_POINT ( 'NONE',  ( 11.01659397126999984, 7.354769923016999833, 6.171139243954000264 ) ) ;
#48612 = CARTESIAN_POINT ( 'NONE',  ( 10.23348307550462621, -4.114479073428862321, 6.632574608010647133 ) ) ;
#48613 = EDGE_CURVE ( 'NONE', #66385, #55988, #19401, .T. ) ;
#48614 = CARTESIAN_POINT ( 'NONE',  ( 9.927263540182998725, -4.629523725463626782, -8.592232985442821658 ) ) ;
#48615 = AXIS2_PLACEMENT_3D ( 'NONE', #12907, #55206, #23390 ) ;
#48616 = EDGE_CURVE ( 'NONE', #57662, #54751, #66604, .T. ) ;
#48617 = ORIENTED_EDGE ( 'NONE', *, *, #34586, .T. ) ;
#48618 = CARTESIAN_POINT ( 'NONE',  ( 12.61495819220213832, -3.174994159617159806, 12.19341885412869964 ) ) ;
#48619 = CARTESIAN_POINT ( 'NONE',  ( 8.947809814040999399, -3.301541394817099739, -8.403266072559899769 ) ) ;
#48620 = CARTESIAN_POINT ( 'NONE',  ( 9.532678149083000818, 4.663044775770000427, 8.669813205957000335 ) ) ;
#48621 = CARTESIAN_POINT ( 'NONE',  ( 8.267367474942998840, 3.071849710027000135, -6.244583336620999958 ) ) ;
#48622 = CARTESIAN_POINT ( 'NONE',  ( 11.21149010443640037, 5.137564434800999891, -7.585072163144589652 ) ) ;
#48623 = CARTESIAN_POINT ( 'NONE',  ( 12.23004733766517838, 0.4382646521645816584, 12.59237917444261434 ) ) ;
#48624 = CARTESIAN_POINT ( 'NONE',  ( 8.432510841230001830, 5.430400319332999715, 7.210801214872999410 ) ) ;
#48625 = CYLINDRICAL_SURFACE ( 'NONE', #359, 2.000000000000000444 ) ;
#48626 = CARTESIAN_POINT ( 'NONE',  ( 12.21010952511927350, 2.691762936255612360, 12.40482162467503535 ) ) ;
#48627 = CARTESIAN_POINT ( 'NONE',  ( 17.84552287012977700, -3.595130221969362605, -11.99794414424696676 ) ) ;
#48628 = CARTESIAN_POINT ( 'NONE',  ( 10.20226357027499908, 5.120085139777000194, -7.716099591766099053 ) ) ;
#48629 = CARTESIAN_POINT ( 'NONE',  ( 7.798085185677998687, 3.459333709783000366, -6.382131374430003667 ) ) ;
#48630 = CARTESIAN_POINT ( 'NONE',  ( 10.59957028040999916, 4.438147096284001059, -8.958385582135001357 ) ) ;
#48631 = ADVANCED_FACE ( 'NONE', ( #8570 ), #7191, .F. ) ;
#48632 = CARTESIAN_POINT ( 'NONE',  ( 17.55505043854143565, 1.787816316115923954, -13.88537766212463254 ) ) ;
#48634 = CARTESIAN_POINT ( 'NONE',  ( 12.32868821305151563, 2.904730879156684153, 12.34800599561342516 ) ) ;
#48633 = CARTESIAN_POINT ( 'NONE',  ( 8.060004013849999538, 5.097451875645002239, 6.450907456765003545 ) ) ;
#48635 = B_SPLINE_CURVE_WITH_KNOTS ( 'NONE', 3,
 ( #57191, #9638, #29623, #66993, #14896 ),
 .UNSPECIFIED., .F., .F.,
 ( 4, 1, 4 ),
 ( 0.000000000000000000, 0.5000000000000000000, 1.000000000000000000 ),
 .UNSPECIFIED. ) ;
#48636 = CARTESIAN_POINT ( 'NONE',  ( 8.959699012653233652, 5.323639004032087563, 7.230967499102583851 ) ) ;
#48637 = ORIENTED_EDGE ( 'NONE', *, *, #32219, .T. ) ;
#48638 = VECTOR ( 'NONE', #63058, 1000.000000000000000 ) ;
#48639 = CARTESIAN_POINT ( 'NONE',  ( 12.52212199951356020, 0.5573870966591139009, 12.68353347973583389 ) ) ;
#48640 = LINE ( 'NONE', #6669, #57904 ) ;
#48641 = AXIS2_PLACEMENT_3D ( 'NONE', #1503, #17590, #5366 ) ;
#48642 = CARTESIAN_POINT ( 'NONE',  ( 12.21312755196904298, -11.61418968116107386, 4.689146002353852261 ) ) ;
#48643 = CARTESIAN_POINT ( 'NONE',  ( 9.273063610504998167, 4.355629271815800507, 6.709281487801199262 ) ) ;
#48644 = CARTESIAN_POINT ( 'NONE',  ( 12.08553199184723681, -2.425689856710292247, 13.78827816593212141 ) ) ;
#48645 = CARTESIAN_POINT ( 'NONE',  ( 8.200000304434999165, 12.49999969551000056, -3.568532357647000425E-10 ) ) ;
#48646 = CARTESIAN_POINT ( 'NONE',  ( 24.38581055541800069, 3.342338751372999628, -12.19042545898000185 ) ) ;
#48647 = EDGE_LOOP ( 'NONE', ( #63236, #4782, #39384, #1752, #3973, #64824, #29335 ) ) ;
#48648 = CARTESIAN_POINT ( 'NONE',  ( 4.216434180875999971, -0.2452535255997999875, 1.107593380736000110 ) ) ;
#48649 = CARTESIAN_POINT ( 'NONE',  ( 11.54684497800060150, -4.976842342332563618, -7.824998645711865208 ) ) ;
#48650 = CARTESIAN_POINT ( 'NONE',  ( 17.80000000009400196, -3.216307036143000175, 11.40341376487999980 ) ) ;
#48651 = CARTESIAN_POINT ( 'NONE',  ( 11.32035090130999855, -3.241273085157000189, 7.030721746772699454 ) ) ;
#48652 = CARTESIAN_POINT ( 'NONE',  ( 18.06602350563007775, 2.139519659637397986, -12.52832261142687642 ) ) ;
#48653 = LINE ( 'NONE', #53554, #65590 ) ;
#48654 = CARTESIAN_POINT ( 'NONE',  ( 10.62903166480609940, 3.135947233695900227, 7.439078678739090122 ) ) ;
#48655 = DIRECTION ( 'NONE',  ( -0.9999999999997783995, 6.656251822948856315E-07, -7.419225572296834004E-10 ) ) ;
#48656 = CARTESIAN_POINT ( 'NONE',  ( 10.24394435321000074, -3.220344030624999743, -6.005416930865999703 ) ) ;
#48657 = EDGE_CURVE ( 'NONE', #47657, #65244, #24569, .T. ) ;
#48658 = CARTESIAN_POINT ( 'NONE',  ( 12.80505043854143210, 3.248147246781388553, 13.61798588129781251 ) ) ;
#48659 = LINE ( 'NONE', #22078, #65431 ) ;
#48660 = CARTESIAN_POINT ( 'NONE',  ( 11.43937577273821482, -4.461177266722074819, 6.300114087089554893 ) ) ;
#48661 = CARTESIAN_POINT ( 'NONE',  ( 8.748821772879614045, -3.697635112905263366, -8.374063393888503626 ) ) ;
#48662 = ORIENTED_EDGE ( 'NONE', *, *, #33730, .F. ) ;
#48663 = CARTESIAN_POINT ( 'NONE',  ( 8.895035841232999729, 5.751585344281000545, -8.235867044345999588 ) ) ;
#48664 = CARTESIAN_POINT ( 'NONE',  ( 12.05610404293055993, -4.502836909561000134, 6.476063885290000322 ) ) ;
#48665 = ORIENTED_EDGE ( 'NONE', *, *, #38201, .F. ) ;
#48666 = CARTESIAN_POINT ( 'NONE',  ( 17.92121436125180978, -3.006915247989151219, 13.55278817016120385 ) ) ;
#48667 = CARTESIAN_POINT ( 'NONE',  ( 11.62579573085663043, -2.760622544769000264, -7.714452430741599365 ) ) ;
#48668 = ORIENTED_EDGE ( 'NONE', *, *, #45454, .F. ) ;
#48669 = CARTESIAN_POINT ( 'NONE',  ( 11.02301463001509774, 4.547357026650399980, 8.376661845795100092 ) ) ;
#48670 = CARTESIAN_POINT ( 'NONE',  ( 6.568578067412807364, 1.121778872040013253, -0.1568744671984653172 ) ) ;
#48671 = CARTESIAN_POINT ( 'NONE',  ( 23.97710144266886090, 3.345395384879282119, -12.79000143593332695 ) ) ;
#48672 = AXIS2_PLACEMENT_3D ( 'NONE', #48719, #50102, #2210 ) ;
#48673 = CARTESIAN_POINT ( 'NONE',  ( 18.26087544840899923, -2.716371057353000218, 11.57326339378999869 ) ) ;
#48674 = CARTESIAN_POINT ( 'NONE',  ( 12.08061556837366091, -2.709898641945338138, -13.73658242091784309 ) ) ;
#48675 = CARTESIAN_POINT ( 'NONE',  ( 9.883513540182333301, -5.249999999999998224, -7.336375382625530683 ) ) ;
#48676 = LINE ( 'NONE', #10236, #47178 ) ;
#48677 = CARTESIAN_POINT ( 'NONE',  ( 10.14584566409999944, -5.370505908760000224, -6.826219946961000318 ) ) ;
#48678 = CARTESIAN_POINT ( 'NONE',  ( 13.38404792230800133, 11.55332361678999931, 1.871151989399000071 ) ) ;
#48679 = ORIENTED_EDGE ( 'NONE', *, *, #10336, .F. ) ;
#48680 = CARTESIAN_POINT ( 'NONE',  ( 8.579854990165880935, 4.352864158102216940, 8.850923404438425734 ) ) ;
#48681 = ORIENTED_EDGE ( 'NONE', *, *, #3274, .F. ) ;
#48682 = VECTOR ( 'NONE', #24504, 1000.000000000000000 ) ;
#48683 = CARTESIAN_POINT ( 'NONE',  ( 10.13061872827999998, 2.189311095934999951, -7.101639631284999865 ) ) ;
#48684 = ORIENTED_EDGE ( 'NONE', *, *, #66350, .F. ) ;
#48685 = CARTESIAN_POINT ( 'NONE',  ( 18.27929200419409028, -2.710634889731355912, -13.73643850021282020 ) ) ;
#48686 = B_SPLINE_CURVE_WITH_KNOTS ( 'NONE', 3,
 ( #45363, #39425, #60404, #12509 ),
 .UNSPECIFIED., .F., .F.,
 ( 4, 4 ),
 ( 0.000000000000000000, 1.000000000000000000 ),
 .UNSPECIFIED. ) ;
#48687 = CARTESIAN_POINT ( 'NONE',  ( 17.59673268120281264, -3.123957167259608259, -12.28404855389177541 ) ) ;
#48688 = VECTOR ( 'NONE', #51942, 1000.000000000000000 ) ;
#48689 = CARTESIAN_POINT ( 'NONE',  ( 10.59991360228957191, 3.150711065775904984, 7.706876553803710728 ) ) ;
#48690 = CARTESIAN_POINT ( 'NONE',  ( 21.00000012402669824, -12.42499880353999941, 0.000000000000000000 ) ) ;
#48691 = B_SPLINE_CURVE_WITH_KNOTS ( 'NONE', 3,
 ( #58400, #63639, #47921, #5596, #20310, #25902, #53160, #52467, #26940, #47232 ),
 .UNSPECIFIED., .F., .F.,
 ( 4, 2, 2, 2, 4 ),
 ( 0.000000000000000000, 0.2500000000000001665, 0.5000000000000003331, 0.7500000000000001110, 1.000000000000000000 ),
 .UNSPECIFIED. ) ;
#48692 = CARTESIAN_POINT ( 'NONE',  ( 9.508513540182335078, -4.163624617374471093, -8.749999999999998224 ) ) ;
#48693 = CARTESIAN_POINT ( 'NONE',  ( 11.29621718459000057, -3.561654022787999807, 6.266039799355000106 ) ) ;
#48694 = CARTESIAN_POINT ( 'NONE',  ( 10.33253786428999987, 2.899999999999999911, 6.571291218949999902 ) ) ;
#48695 = EDGE_CURVE ( 'NONE', #21003, #61003, #69008, .T. ) ;
#48696 = CARTESIAN_POINT ( 'NONE',  ( 12.29698918160474364, -0.3645810575750318971, 13.89357890581305099 ) ) ;
#48697 = EDGE_CURVE ( 'NONE', #28877, #8998, #4342, .T. ) ;
#48698 = ORIENTED_EDGE ( 'NONE', *, *, #38391, .F. ) ;
#48699 = CARTESIAN_POINT ( 'NONE',  ( 7.015090560819000842, 4.719833207100999850, -8.789699670502999496 ) ) ;
#48700 = CARTESIAN_POINT ( 'NONE',  ( 18.53712219996399924, 11.93788271774999998, -3.912105503483000124 ) ) ;
#48701 = CARTESIAN_POINT ( 'NONE',  ( 10.28877584378239796, 4.466001735846802490, 6.763172759027206382 ) ) ;
#48702 = CARTESIAN_POINT ( 'NONE',  ( 4.471808905520999744, 1.206178254336000233, -0.5711989167972000292 ) ) ;
#48703 = CARTESIAN_POINT ( 'NONE',  ( 8.649364158774000444, 3.038023536984999939, -5.861661709981000001 ) ) ;
#48704 = CARTESIAN_POINT ( 'NONE',  ( 18.30830001818700126, -3.300182612895000478, 12.02694835946000040 ) ) ;
#48705 = CARTESIAN_POINT ( 'NONE',  ( 10.62924380535000068, -3.609488729914999805, -5.855142811286000004 ) ) ;
#48706 = B_SPLINE_CURVE_WITH_KNOTS ( 'NONE', 3,
 ( #7305, #35265, #56239, #40167 ),
 .UNSPECIFIED., .F., .F.,
 ( 4, 4 ),
 ( 0.000000000000000000, 1.000000000000000000 ),
 .UNSPECIFIED. ) ;
#48707 = EDGE_LOOP ( 'NONE', ( #40810, #12325, #35930, #60148 ) ) ;
#48708 = CARTESIAN_POINT ( 'NONE',  ( 3.259306799210500927, -3.058252359239909346, 1.762666431298136605 ) ) ;
#48709 = CARTESIAN_POINT ( 'NONE',  ( 8.871410841230998656, 2.721111233225000259, -6.936528696292000085 ) ) ;
#48710 = DIRECTION ( 'NONE',  ( 0.000000000000000000, 1.000000000000000000, 0.000000000000000000 ) ) ;
#48711 = LINE ( 'NONE', #59538, #18510 ) ;
#48712 = CARTESIAN_POINT ( 'NONE',  ( 5.200000000000000178, -1.199999999999999956, -11.22663029882996710 ) ) ;
#48713 = CARTESIAN_POINT ( 'NONE',  ( 24.59180579038299896, 8.769928687672001288, -9.082967714861000630 ) ) ;
#48714 = CARTESIAN_POINT ( 'NONE',  ( 11.48011496860029901, 4.919769165942200040, -7.028661263734299780 ) ) ;
#48715 = EDGE_CURVE ( 'NONE', #49491, #27465, #21210, .T. ) ;
#48716 = CARTESIAN_POINT ( 'NONE',  ( 9.102747021775998704, 3.245052836381700168, -8.162493079567200382 ) ) ;
#48718 = CARTESIAN_POINT ( 'NONE',  ( 4.399695933186626995, 0.9886387176649684694, -0.8895061925674412340 ) ) ;
#48717 = CARTESIAN_POINT ( 'NONE',  ( 9.646417874593998576, -4.797903641662700558, 7.160798403412399260 ) ) ;
#48719 = CARTESIAN_POINT ( 'NONE',  ( 23.56665676678700194, 0.000000000000000000, -3.819167204710999951E-13 ) ) ;
#48720 = VERTEX_POINT ( 'NONE', #20428 ) ;
#48721 = EDGE_CURVE ( 'NONE', #59889, #36471, #41757, .T. ) ;
#48722 = CARTESIAN_POINT ( 'NONE',  ( 11.43856039236529831, 5.032284719763000069, 7.449760924956519759 ) ) ;
#48723 = AXIS2_PLACEMENT_3D ( 'NONE', #59929, #10655, #26752 ) ;
#48724 = CARTESIAN_POINT ( 'NONE',  ( 10.71256247620999957, -5.951803124515000043, 7.233045248871000865 ) ) ;
#48725 = CARTESIAN_POINT ( 'NONE',  ( 10.34091290906799898, 3.277531639390499851, 6.615820196229499572 ) ) ;
#48726 = DIRECTION ( 'NONE',  ( -1.000000000000000000, 0.000000000000000000, 0.000000000000000000 ) ) ;
#48727 = CARTESIAN_POINT ( 'NONE',  ( 11.25041341105000114, -5.730771985297000271, 8.122672103119001008 ) ) ;
#48728 = CARTESIAN_POINT ( 'NONE',  ( 10.90378878155999942, -2.900209876291999667, -5.134763467624999578 ) ) ;
#48729 = CARTESIAN_POINT ( 'NONE',  ( 16.42348875342600323, -3.378076265369000186, -11.11016813414000204 ) ) ;
#48730 = CARTESIAN_POINT ( 'NONE',  ( 9.406696787962999906, -3.827518619249500098, -6.510508982544899403 ) ) ;
#48731 = AXIS2_PLACEMENT_3D ( 'NONE', #39888, #40908, #13325 ) ;
#48732 = B_SPLINE_CURVE_WITH_KNOTS ( 'NONE', 3,
 ( #58192, #53635, #5046, #5730 ),
 .UNSPECIFIED., .F., .F.,
 ( 4, 4 ),
 ( 0.000000000000000000, 0.1254132184345819190 ),
 .UNSPECIFIED. ) ;
#48733 = CARTESIAN_POINT ( 'NONE',  ( 5.353758726594999295, -1.146783406111000048, -0.2608682635935000160 ) ) ;
#48734 = DIRECTION ( 'NONE',  ( 0.000000000000000000, -0.1807154286439995039, 0.9835354258236027603 ) ) ;
#48735 = CARTESIAN_POINT ( 'NONE',  ( 5.500000000000000000, -7.849276784099999367E-14, -1.865174681369999824E-14 ) ) ;
#48736 = CARTESIAN_POINT ( 'NONE',  ( 11.52287616594230002, -4.261927842557799551, 8.325646653015098764 ) ) ;
#48737 = CARTESIAN_POINT ( 'NONE',  ( 10.70287750876920008, 3.530799696887600092, -8.228113772635300194 ) ) ;
#48738 = CARTESIAN_POINT ( 'NONE',  ( 6.877770285292999830, -9.263688577134999491, -5.299267108162999840 ) ) ;
#48739 = CARTESIAN_POINT ( 'NONE',  ( 1.985247277619000217, 2.372532593102000043, -2.573147701680999599 ) ) ;
#48740 = DIRECTION ( 'NONE',  ( -1.000000000000000000, 0.000000000000000000, 0.000000000000000000 ) ) ;
#48741 = ORIENTED_EDGE ( 'NONE', *, *, #9483, .F. ) ;
#48742 = CARTESIAN_POINT ( 'NONE',  ( 5.000000000000000000, 0.000000000000000000, 0.000000000000000000 ) ) ;
#48743 = CARTESIAN_POINT ( 'NONE',  ( 10.37199293566600034, -3.366612813978900220, -8.276990458557699881 ) ) ;
#48744 = CARTESIAN_POINT ( 'NONE',  ( 25.44994642811700203, 2.930988785009999904E-14, 1.731947918414999972E-14 ) ) ;
#48745 = DIRECTION ( 'NONE',  ( 0.000000000000000000, 0.9659258262890757507, -0.2588190451024927063 ) ) ;
#48746 = CARTESIAN_POINT ( 'NONE',  ( 7.000000000000000000, 10.29799223392326546, 4.279123368246552594 ) ) ;
#48747 = CARTESIAN_POINT ( 'NONE',  ( 10.52946886766499901, 3.569835351907400423, -6.718432993015899690 ) ) ;
#48748 = ORIENTED_EDGE ( 'NONE', *, *, #41103, .F. ) ;
#48749 = CARTESIAN_POINT ( 'NONE',  ( 8.762289945692000259, -4.238022715896200054, -8.411288920148800585 ) ) ;
#48750 = ORIENTED_EDGE ( 'NONE', *, *, #32023, .T. ) ;
#48751 = DIRECTION ( 'NONE',  ( 0.000000000000000000, 0.7506664619968553831, -0.6606813625592322659 ) ) ;
#48752 = CARTESIAN_POINT ( 'NONE',  ( 18.29999744860993616, 2.794302574217389701, 11.51706234583376087 ) ) ;
#48753 = CARTESIAN_POINT ( 'NONE',  ( 9.658629719592001450, 5.496789211521000418, -7.043125396300999874 ) ) ;
#48754 = ORIENTED_EDGE ( 'NONE', *, *, #23916, .T. ) ;
#48755 = CARTESIAN_POINT ( 'NONE',  ( 12.07299956498157023, -2.792989229543000107, 7.174999999999999822 ) ) ;
#48756 = CARTESIAN_POINT ( 'NONE',  ( 11.00000000000000000, 4.991767524623399233, -7.174999999999999822 ) ) ;
#48757 = CARTESIAN_POINT ( 'NONE',  ( 6.876645280409000804, 4.455038580940000159, -9.171635993214000138 ) ) ;
#48758 = CARTESIAN_POINT ( 'NONE',  ( 10.29184687351566829, -4.999583552997724389, -6.731816600031356401 ) ) ;
#48759 = CARTESIAN_POINT ( 'NONE',  ( 9.493540423042883702, 4.876969314220700014, 8.526773713797128451 ) ) ;
#48760 = ORIENTED_EDGE ( 'NONE', *, *, #48529, .F. ) ;
#48761 = CARTESIAN_POINT ( 'NONE',  ( 10.62698276521000196, -3.142914536759000121, 8.668455626664998803 ) ) ;
#48762 = CARTESIAN_POINT ( 'NONE',  ( 25.31135467044800080, 11.20186433212000132, -3.316420822239999566 ) ) ;
#48763 = CARTESIAN_POINT ( 'NONE',  ( 11.36486084871759950, 2.792989229543000107, 7.174999999999999822 ) ) ;
#48764 = VERTEX_POINT ( 'NONE', #42446 ) ;
#48765 = B_SPLINE_CURVE_WITH_KNOTS ( 'NONE', 3,
 ( #68317, #62732, #66955, #19062, #67633 ),
 .UNSPECIFIED., .F., .F.,
 ( 4, 1, 4 ),
 ( 0.7874025540483345909, 0.8749496349986518595, 1.000000000000000000 ),
 .UNSPECIFIED. ) ;
#48766 = AXIS2_PLACEMENT_3D ( 'NONE', #9973, #14879, #4714 ) ;
#48767 = CARTESIAN_POINT ( 'NONE',  ( 9.099999931440999390, 5.246365646610000155, -7.404749409716440134 ) ) ;
#48768 = DIRECTION ( 'NONE',  ( 0.9999999999999762412, -2.179566601840950490E-07, 9.624126031003771506E-10 ) ) ;
#48769 = VERTEX_POINT ( 'NONE', #38574 ) ;
#48770 = CARTESIAN_POINT ( 'NONE',  ( 10.18144474310099845, 5.015709705366000470, 7.007085334055199510 ) ) ;
#48771 = CARTESIAN_POINT ( 'NONE',  ( 18.11727536442213093, 0.2737665426068931485, -13.89638618295544248 ) ) ;
#48772 = CARTESIAN_POINT ( 'NONE',  ( 4.374345016631999705, -0.3062339383746999766, 1.382988000970999831 ) ) ;
#48773 = FACE_OUTER_BOUND ( 'NONE', #62928, .T. ) ;
#48774 = DIRECTION ( 'NONE',  ( 0.000000000000000000, -1.000000000000000000, 0.000000000000000000 ) ) ;
#48775 = B_SPLINE_CURVE_WITH_KNOTS ( 'NONE', 3,
 ( #31900, #53213, #5995, #5315 ),
 .UNSPECIFIED., .F., .F.,
 ( 4, 4 ),
 ( 0.000000000000000000, 1.000000000000000000 ),
 .UNSPECIFIED. ) ;
#48776 = AXIS2_PLACEMENT_3D ( 'NONE', #44632, #1968, #28546 ) ;
#48777 = EDGE_CURVE ( 'NONE', #61687, #27541, #17887, .T. ) ;
#48778 = CARTESIAN_POINT ( 'NONE',  ( 9.327269112000164952, -3.948692165092429374, 9.238904779716392568 ) ) ;
#48779 = EDGE_CURVE ( 'NONE', #67055, #28653, #45371, .T. ) ;
#48780 = VERTEX_POINT ( 'NONE', #49406 ) ;
#48781 = CARTESIAN_POINT ( 'NONE',  ( 11.09999999999999964, 4.000000000000000000, 7.500000000000000000 ) ) ;
#48782 = CARTESIAN_POINT ( 'NONE',  ( 10.41838915877000105, 4.531912033713999755, -9.270484952459998595 ) ) ;
#48783 = CARTESIAN_POINT ( 'NONE',  ( 1.250973465874999802, -3.500000000000000000, 0.000000000000000000 ) ) ;
#48784 = AXIS2_PLACEMENT_3D ( 'NONE', #24055, #29316, #7631 ) ;
#48785 = CARTESIAN_POINT ( 'NONE',  ( 12.18523880347860811, 2.582858790010647887, -13.65555696386475582 ) ) ;
#48786 = CARTESIAN_POINT ( 'NONE',  ( 24.30000000000000071, 2.258942858049999725, -12.29419282279000036 ) ) ;
#48787 = CARTESIAN_POINT ( 'NONE',  ( 10.96080136920999948, -2.054580854576999904, 7.810082699133999995 ) ) ;
#48788 = CARTESIAN_POINT ( 'NONE',  ( 8.599999952505998024, -3.250000006358199744, -7.500000000000000000 ) ) ;
#48789 = CARTESIAN_POINT ( 'NONE',  ( 25.08549383408500333, -2.791071255704999921, 11.47627186989000059 ) ) ;
#48790 = ORIENTED_EDGE ( 'NONE', *, *, #23518, .F. ) ;
#48791 = ORIENTED_EDGE ( 'NONE', *, *, #53763, .F. ) ;
#48792 = AXIS2_PLACEMENT_3D ( 'NONE', #16495, #28035, #58457 ) ;
#48793 = CARTESIAN_POINT ( 'NONE',  ( 12.24748039825137624, 0.2825697096154566323, 13.89613713856509136 ) ) ;
#48794 = CARTESIAN_POINT ( 'NONE',  ( 12.35321263090787269, -0.4320316581265434275, -13.89096707190848790 ) ) ;
#48795 = CARTESIAN_POINT ( 'NONE',  ( 9.385788300200999856, -4.980873770300999759, 6.433336655958999728 ) ) ;
#48796 = CARTESIAN_POINT ( 'NONE',  ( 18.01482774842505918, -0.4234772792228427285, -13.89131919812468929 ) ) ;
#48797 = CARTESIAN_POINT ( 'NONE',  ( 7.897956853208000005, -3.608524635952000459, 5.913372239166000632 ) ) ;
#48798 = DIRECTION ( 'NONE',  ( 1.000000000000000000, 0.000000000000000000, 0.000000000000000000 ) ) ;
#48800 = CARTESIAN_POINT ( 'NONE',  ( 9.843930206850000530, 2.750000000000000000, 7.500000000000000000 ) ) ;
#48799 = CARTESIAN_POINT ( 'NONE',  ( 10.31101337669300122, -5.140392946802999852, 8.079558723821699928 ) ) ;
#48801 = CARTESIAN_POINT ( 'NONE',  ( 10.91195257254739914, 2.772832764353999835, -7.856899084262298771 ) ) ;
#48802 = EDGE_CURVE ( 'NONE', #41119, #67742, #17955, .T. ) ;
#48803 = CARTESIAN_POINT ( 'NONE',  ( 24.46225079000999969, -8.883320982495000351, -9.188387934989000527 ) ) ;
#48804 = CARTESIAN_POINT ( 'NONE',  ( 8.521235029058406241, 5.099999848902339039, -6.534141629449454314 ) ) ;
#48805 = CARTESIAN_POINT ( 'NONE',  ( 18.14682445378390341, -0.2013262877421428398, 12.69785743964334834 ) ) ;
#48806 = CARTESIAN_POINT ( 'NONE',  ( 20.60000000000000142, 12.34999999999999964, 4.046978687741000012E-05 ) ) ;
#48807 = CARTESIAN_POINT ( 'NONE',  ( 18.14797787939609464, -3.506662021210539049, 12.02412632936538905 ) ) ;
#48808 = ORIENTED_EDGE ( 'NONE', *, *, #40106, .T. ) ;
#48809 = CARTESIAN_POINT ( 'NONE',  ( 11.75361999289386894, -4.544092497359195626, 8.657883396625688732 ) ) ;
#48810 = FACE_OUTER_BOUND ( 'NONE', #21379, .T. ) ;
#48811 = B_SPLINE_CURVE_WITH_KNOTS ( 'NONE', 3,
 ( #38343, #11769, #54426, #6528 ),
 .UNSPECIFIED., .F., .F.,
 ( 4, 4 ),
 ( 0.000000000000000000, 1.000000000000000000 ),
 .UNSPECIFIED. ) ;
#48812 = DIRECTION ( 'NONE',  ( -2.017751170287999915E-09, -7.180968446191999491E-11, 1.000000000000000000 ) ) ;
#48813 = DIRECTION ( 'NONE',  ( 0.7071067388045961799, 0.7071068235684964121, -1.176037761303994353E-10 ) ) ;
#48814 = AXIS2_PLACEMENT_3D ( 'NONE', #810, #1500, #28074 ) ;
#48815 = CARTESIAN_POINT ( 'NONE',  ( 13.49994651945300284, -12.07042783918999795, -2.492331243371999960 ) ) ;
#48816 = COLOUR_RGB ( '', 0.66274510, 0.83137255, 0.94901961) ;
#48817 = CARTESIAN_POINT ( 'NONE',  ( 10.57102344389999971, 3.237334151971200225, 7.962849245488699879 ) ) ;
#48818 = CARTESIAN_POINT ( 'NONE',  ( 10.46298584122999920, 3.993164721578000176, -6.140176455708999725 ) ) ;
#48819 = ORIENTED_EDGE ( 'NONE', *, *, #3525, .F. ) ;
#48820 = CARTESIAN_POINT ( 'NONE',  ( 12.08123681970976193, -0.04734719685817544849, -12.59993264914401401 ) ) ;
#48821 = CARTESIAN_POINT ( 'NONE',  ( 10.97755399909358154, -3.866653594937912608, -8.778526265510096849 ) ) ;
#48822 = CARTESIAN_POINT ( 'NONE',  ( 17.96998260175200102, 3.070456082915652640, -12.22016143605431004 ) ) ;
#48823 = CARTESIAN_POINT ( 'NONE',  ( 5.536227981746089988, 12.19240621326732388, 3.776122996995809888 ) ) ;
#48825 = CARTESIAN_POINT ( 'NONE',  ( 8.245295280410999794, 4.283000592898000392, 9.286795422009001655 ) ) ;
#48824 = AXIS2_PLACEMENT_3D ( 'NONE', #30652, #19470, #29987 ) ;
#48826 = ORIENTED_EDGE ( 'NONE', *, *, #2048, .T. ) ;
#48827 = CARTESIAN_POINT ( 'NONE',  ( 6.205603783354000313, 1.388436026523999889, -0.4783021510498000062 ) ) ;
#48828 = CARTESIAN_POINT ( 'NONE',  ( 8.055279719587000287, 3.504660014889999786, -9.160103207264000957 ) ) ;
#48829 = CARTESIAN_POINT ( 'NONE',  ( 8.442993682891730245, -2.265460329437196219, 7.647905870472889944 ) ) ;
#48830 = AXIS2_PLACEMENT_3D ( 'NONE', #59727, #53459, #47876 ) ;
#48831 = CARTESIAN_POINT ( 'NONE',  ( 11.08126742035591228, -4.768619073576778611, -7.106626190113856545 ) ) ;
#48832 = ORIENTED_EDGE ( 'NONE', *, *, #3527, .F. ) ;
#48833 = DIRECTION ( 'NONE',  ( 0.000000000000000000, -0.8765967884314782577, -0.4812255921203881792 ) ) ;
#48834 = CARTESIAN_POINT ( 'NONE',  ( 6.146693173016666734, -1.310679582531386611, -0.7554284705563495406 ) ) ;
#48835 = ORIENTED_EDGE ( 'NONE', *, *, #2319, .F. ) ;
#48836 = CARTESIAN_POINT ( 'NONE',  ( 24.63611025208533789, 3.161149086942907527, -11.86231087104421356 ) ) ;
#48837 = CARTESIAN_POINT ( 'NONE',  ( 25.22251911269240665, -8.509543809242357426, -8.058442543228641952 ) ) ;
#48838 = CARTESIAN_POINT ( 'NONE',  ( 17.60287317832943543, 0.7290248443971264480, -13.98100598729141097 ) ) ;
#48839 = ADVANCED_FACE ( 'NONE', ( #22147, #55351 ), #49758, .T. ) ;
#48840 = EDGE_CURVE ( 'NONE', #27697, #10337, #2871, .T. ) ;
#48841 = ORIENTED_EDGE ( 'NONE', *, *, #33481, .T. ) ;
#48842 = CARTESIAN_POINT ( 'NONE',  ( 10.83253786428999987, -2.899999999999999911, 6.571291218949999902 ) ) ;
#48843 = B_SPLINE_CURVE_WITH_KNOTS ( 'NONE', 3,
 ( #26969, #10195, #20685, #21031 ),
 .UNSPECIFIED., .F., .F.,
 ( 4, 4 ),
 ( 0.000000000000000000, 1.000000000000000000 ),
 .UNSPECIFIED. ) ;
#48844 = AXIS2_PLACEMENT_3D ( 'NONE', #59422, #32864, #47309 ) ;
#48845 = CARTESIAN_POINT ( 'NONE',  ( 11.40211496860029783, 4.793947479907100018, -7.093139000852099585 ) ) ;
#48846 = CARTESIAN_POINT ( 'NONE',  ( 8.919816864363674824, -2.358207424585543777, 8.150886335909103053 ) ) ;
#48847 = CARTESIAN_POINT ( 'NONE',  ( 10.82118582084300051, -4.836160649475099937, 8.466515260542900378 ) ) ;
#48848 = ORIENTED_EDGE ( 'NONE', *, *, #52310, .T. ) ;
#48849 = CARTESIAN_POINT ( 'NONE',  ( 9.250899447075999760, 4.135077451221000011, 9.175524215473998879 ) ) ;
#48850 = CARTESIAN_POINT ( 'NONE',  ( 18.13255570286232654, -2.076448383791634544, 13.84516006853288950 ) ) ;
#48851 = VERTEX_POINT ( 'NONE', #39273 ) ;
#48852 = CARTESIAN_POINT ( 'NONE',  ( 9.864763540183334456, -5.217465845835395299, 7.172815144550902744 ) ) ;
#48853 = CYLINDRICAL_SURFACE ( 'NONE', #63805, 1.250000000000000222 ) ;
#48854 = CARTESIAN_POINT ( 'NONE',  ( 10.08351354018237345, 5.250000000000000888, 7.336375382625531572 ) ) ;
#48855 = ORIENTED_EDGE ( 'NONE', *, *, #43001, .F. ) ;
#48856 = CARTESIAN_POINT ( 'NONE',  ( 12.18001225342677607, -2.492635468222105910, -12.45327835951381346 ) ) ;
#48857 = CARTESIAN_POINT ( 'NONE',  ( -0.2999999999999999889, 1.649999999999999911, 0.000000000000000000 ) ) ;
#48858 = CARTESIAN_POINT ( 'NONE',  ( 7.888897165042807913, 5.521107890873540036, -8.565486907688864449 ) ) ;
#48859 = CYLINDRICAL_SURFACE ( 'NONE', #5111, 0.6250000000000005551 ) ;
#48860 = CARTESIAN_POINT ( 'NONE',  ( 12.27297424062793141, -2.021448577728832685, -13.85330429709570765 ) ) ;
#48861 = CARTESIAN_POINT ( 'NONE',  ( 10.99410672858429905, -4.801902424331299990, -6.896755974168000236 ) ) ;
#48862 = CARTESIAN_POINT ( 'NONE',  ( 10.42363156114900136, 3.315688435009791935, 6.424401362931539516 ) ) ;
#48863 = CARTESIAN_POINT ( 'NONE',  ( 17.69815883927268985, -3.108482560213371215, 12.28876257455221221 ) ) ;
#48864 = ORIENTED_EDGE ( 'NONE', *, *, #42524, .F. ) ;
#48865 = FACE_OUTER_BOUND ( 'NONE', #54851, .T. ) ;
#48866 = EDGE_CURVE ( 'NONE', #1541, #46332, #2031, .T. ) ;
#48867 = ORIENTED_EDGE ( 'NONE', *, *, #15179, .T. ) ;
#48868 = CARTESIAN_POINT ( 'NONE',  ( 11.71271957899600125, -12.11624328427999941, -2.031646723569000113 ) ) ;
#48869 = CARTESIAN_POINT ( 'NONE',  ( 8.450464158772000189, 3.789127741898000057, -9.388182174781999123 ) ) ;
#48870 = EDGE_CURVE ( 'NONE', #36697, #7217, #33343, .T. ) ;
#48871 = CARTESIAN_POINT ( 'NONE',  ( 11.11264834745999863, 2.146077493652999824, -7.517188756437000130 ) ) ;
#48872 = CARTESIAN_POINT ( 'NONE',  ( 10.70780617489000086, -5.157482071823000780, -6.267811103859000532 ) ) ;
#48873 = STYLED_ITEM ( 'NONE', ( #41298 ), #18558 ) ;
#48874 = DIRECTION ( 'NONE',  ( 0.000000000000000000, -0.2588190451024934835, -0.9659258262890757507 ) ) ;
#48875 = CARTESIAN_POINT ( 'NONE',  ( 24.02034026765100094, 12.55451516185999949, 3.484863126418999979 ) ) ;
#48876 = CARTESIAN_POINT ( 'NONE',  ( 17.65093666541812212, -1.765655615497803588, -12.47567830514637066 ) ) ;
#48877 = ORIENTED_EDGE ( 'NONE', *, *, #32625, .T. ) ;
#48878 = CIRCLE ( 'NONE', #18739, 13.17499999999999893 ) ;
#48879 = CARTESIAN_POINT ( 'NONE',  ( 1.816329616853666673, -3.450786940248409707, -0.6753594422426503208 ) ) ;
#48880 = CARTESIAN_POINT ( 'NONE',  ( 10.87021720923999979, 2.226038107033000202, 7.782753921296999167 ) ) ;
#48881 = CARTESIAN_POINT ( 'NONE',  ( 5.500000000000000000, -6.661338147750999827E-14, -1.931788062847999572E-14 ) ) ;
#48882 = CARTESIAN_POINT ( 'NONE',  ( 11.27368717260499942, -4.539928529895099985, 6.618743573831199711 ) ) ;
#48883 = CARTESIAN_POINT ( 'NONE',  ( 11.09999999999999964, -2.700000001949000250, -5.146415525425999782 ) ) ;
#48884 = CARTESIAN_POINT ( 'NONE',  ( 10.95616034570999986, 9.845173301957000689, -5.754287415814000717 ) ) ;
#48885 = EDGE_CURVE ( 'NONE', #65585, #23416, #64784, .T. ) ;
#48886 = CARTESIAN_POINT ( 'NONE',  ( 7.100000000000589395, 4.595628095797888335, -6.248885204747992361 ) ) ;
#48887 = CARTESIAN_POINT ( 'NONE',  ( 24.08772785482500112, -9.257913837711999605, -9.301533136437999616 ) ) ;
#48888 = CARTESIAN_POINT ( 'NONE',  ( 11.40221299665285670, -3.091095606691090847, -7.824988380119695996 ) ) ;
#48889 = AXIS2_PLACEMENT_3D ( 'NONE', #66365, #18486, #38775 ) ;
#48890 = CARTESIAN_POINT ( 'NONE',  ( 5.700000000378000031, -0.2999999996220999443, 3.150000004979999879 ) ) ;
#48891 = B_SPLINE_SURFACE_WITH_KNOTS ( 'NONE', 3, 3, ( 
 ( #60135, #12244, #12588, #61171 ),
 ( #54890, #6990, #28321, #45098 ),
 ( #2104, #55585, #55236, #34617 ),
 ( #2436, #7688, #7333, #23763 ),
 ( #39502, #60825, #66407, #39851 ),
 ( #4141, #24108, #62868, #56953 ),
 ( #67091, #25135, #57630, #62532 ),
 ( #19203, #30062, #46467, #45441 ),
 ( #30392, #20233, #3798, #14651 ),
 ( #9733, #14986, #50685, #35968 ) ),
 .UNSPECIFIED., .F., .F., .F.,
 ( 4, 1, 1, 1, 1, 1, 1, 4 ),
 ( 4, 4 ),
 ( 0.04111222701784000150, 0.1428571428570999946, 0.2857142857143000203, 0.4285714285713999594, 0.5714285714286000406, 0.7142857142856999797, 0.8571428571429000609, 0.9278613184711000939 ),
 ( -0.1900620218102000158, 1.190128522698000069 ),
 .UNSPECIFIED. ) ;
#48892 = ORIENTED_EDGE ( 'NONE', *, *, #67402, .F. ) ;
#48893 = CARTESIAN_POINT ( 'NONE',  ( 9.667010841233000917, 4.769103072373000352, -8.666849124598000387 ) ) ;
#48894 = CARTESIAN_POINT ( 'NONE',  ( 6.961659601440000067, -1.366112286775999829, -0.08575370944440000032 ) ) ;
#48895 = CARTESIAN_POINT ( 'NONE',  ( 18.16587897468625812, 2.632730956727242333, 13.64436436691515908 ) ) ;
#48896 = CARTESIAN_POINT ( 'NONE',  ( 4.400000000000000355, 0.000000000000000000, 0.000000000000000000 ) ) ;
#48897 = CARTESIAN_POINT ( 'NONE',  ( 11.37964291764649971, -5.268358781405000357, -7.343212302062899433 ) ) ;
#48898 = ORIENTED_EDGE ( 'NONE', *, *, #49045, .T. ) ;
#48899 = CARTESIAN_POINT ( 'NONE',  ( 25.19214439740800060, 2.891371816527999794, -11.44528675289000041 ) ) ;
#48900 = CARTESIAN_POINT ( 'NONE',  ( 7.475045280409000625, 3.276311362504999991, 5.841989464160999290 ) ) ;
#48902 = CARTESIAN_POINT ( 'NONE',  ( 10.91301932002725650, -5.250000000000000888, -7.799851088612626882 ) ) ;
#48901 = CARTESIAN_POINT ( 'NONE',  ( 9.061929719594999710, 4.092867382745001059, -5.937785237406000505 ) ) ;
#48903 = CARTESIAN_POINT ( 'NONE',  ( 25.37957165016208450, 11.36922881883540803, -3.069087598897670244 ) ) ;
#48904 = ORIENTED_EDGE ( 'NONE', *, *, #7422, .T. ) ;
#48905 = CARTESIAN_POINT ( 'NONE',  ( 9.980433037259000884, 4.047223446241999589, 9.090360698422999874 ) ) ;
#48907 = CARTESIAN_POINT ( 'NONE',  ( 18.27051424461486562, -2.638143613628455064, -13.74920933505747733 ) ) ;
#48906 = B_SPLINE_CURVE_WITH_KNOTS ( 'NONE', 3,
 ( #65716, #6641, #18180, #38810 ),
 .UNSPECIFIED., .F., .F.,
 ( 4, 4 ),
 ( 0.000000000000000000, 1.000000000000000000 ),
 .UNSPECIFIED. ) ;
#48908 = CARTESIAN_POINT ( 'NONE',  ( 10.82179975933729921, 4.948878321068100661, 7.826467126457498757 ) ) ;
#48909 = CARTESIAN_POINT ( 'NONE',  ( 9.903944471677000649, -5.205019707614999547, 6.747219600580999455 ) ) ;
#48910 = CARTESIAN_POINT ( 'NONE',  ( 8.320870559624999885, -3.894643656844000379, 6.044452984962999764 ) ) ;
#48911 = VERTEX_POINT ( 'NONE', #1175 ) ;
#48912 = CARTESIAN_POINT ( 'NONE',  ( 24.40628504395400000, 12.24027098590999962, -3.187905388597000123 ) ) ;
#48914 = CARTESIAN_POINT ( 'NONE',  ( 11.17788601987000163, -2.412142864687000010, -7.075602314719000141 ) ) ;
#48913 = CARTESIAN_POINT ( 'NONE',  ( 11.91753023736700179, -11.77475711121000224, 4.379243463657999769 ) ) ;
#48915 = CARTESIAN_POINT ( 'NONE',  ( 7.645471844114070770, -5.358564433078305100, 6.414118424940338237 ) ) ;
#48916 = CARTESIAN_POINT ( 'NONE',  ( 11.09999999999999964, 2.700000000000000178, -6.461133846875999787 ) ) ;
#48917 = CARTESIAN_POINT ( 'NONE',  ( 23.62017948775300269, 2.980885128520999849, 13.51681883505999870 ) ) ;
#48918 = ORIENTED_EDGE ( 'NONE', *, *, #51913, .F. ) ;
#48919 = CARTESIAN_POINT ( 'NONE',  ( 5.813359839683332808, 1.310679582531387943, -0.7554284705563468760 ) ) ;
#48920 = CARTESIAN_POINT ( 'NONE',  ( 11.73610538575739959, -2.890527834009000152, 7.765257665594799796 ) ) ;
#48921 = CARTESIAN_POINT ( 'NONE',  ( 18.28072526159958144, 2.330763871450813429, 13.80597059069190458 ) ) ;
#48922 = CARTESIAN_POINT ( 'NONE',  ( 11.23195122972050086, 4.507250159094099651, 8.673036084990000560 ) ) ;
#48923 = VERTEX_POINT ( 'NONE', #11654 ) ;
#48924 = EDGE_CURVE ( 'NONE', #20236, #65247, #64531, .T. ) ;
#48925 = EDGE_CURVE ( 'NONE', #4028, #16280, #12702, .T. ) ;
#48926 = CARTESIAN_POINT ( 'NONE',  ( 9.468589158772999781, 4.034680274230000308, -6.102912434217000026 ) ) ;
#48927 = CIRCLE ( 'NONE', #16526, 5.760713961201000544 ) ;
#48928 = EDGE_CURVE ( 'NONE', #63789, #16959, #61223, .T. ) ;
#48929 = CARTESIAN_POINT ( 'NONE',  ( 12.78084111884633600, 3.199751093817826408, -12.18694350317453079 ) ) ;
#48930 = CARTESIAN_POINT ( 'NONE',  ( 11.51279632507520034, -3.375091146194399983, 6.341531314375999706 ) ) ;
#48931 = ORIENTED_EDGE ( 'NONE', *, *, #49385, .F. ) ;
#48932 = DIRECTION ( 'NONE',  ( 0.000000000000000000, 0.000000000000000000, -1.000000000000000000 ) ) ;
#48933 = CARTESIAN_POINT ( 'NONE',  ( 24.63002439619599926, 0.000000000000000000, 0.000000000000000000 ) ) ;
#48934 = ORIENTED_EDGE ( 'NONE', *, *, #10025, .T. ) ;
#48935 = CARTESIAN_POINT ( 'NONE',  ( 9.331129440379999807, -4.141908960411000429, 6.047561724438000219 ) ) ;
#48936 = CARTESIAN_POINT ( 'NONE',  ( 17.80000000005199823, 3.345268251980999974, 11.86064071431999878 ) ) ;
#48937 = ORIENTED_EDGE ( 'NONE', *, *, #29934, .F. ) ;
#48938 = CARTESIAN_POINT ( 'NONE',  ( 10.12284001496798780, -2.396628744330400629, -6.794529262851803253 ) ) ;
#48939 = CARTESIAN_POINT ( 'NONE',  ( 11.41256651104150066, 4.098999650273559503, 8.498573944230598087 ) ) ;
#48940 = CARTESIAN_POINT ( 'NONE',  ( 10.68903608760000168, 2.568976842941999905, 7.728092503410000091 ) ) ;
#48941 = CARTESIAN_POINT ( 'NONE',  ( 10.83768005408999890, 5.758100475276000552, -6.911469147650000977 ) ) ;
#48942 = CARTESIAN_POINT ( 'NONE',  ( 27.25811388278000180, 0.000000000000000000, 0.000000000000000000 ) ) ;
#48943 = CARTESIAN_POINT ( 'NONE',  ( 9.150818738817875442, 4.951062758656399332, -6.673278530809400699 ) ) ;
#48944 = CARTESIAN_POINT ( 'NONE',  ( 13.64506009312500190, 9.630614656729999723, 7.923290881757000470 ) ) ;
#48945 = CARTESIAN_POINT ( 'NONE',  ( 18.09667132770093545, -0.3125562302819428484, -12.69484091569604089 ) ) ;
#48946 = CIRCLE ( 'NONE', #66806, 1.000000000000000444 ) ;
#48947 = DIRECTION ( 'NONE',  ( -0.000000000000000000, 1.000000000000000000, 0.000000000000000000 ) ) ;
#48948 = CARTESIAN_POINT ( 'NONE',  ( 10.49764694612699856, -5.059486515935999407, -7.922821994243300914 ) ) ;
#48949 = CARTESIAN_POINT ( 'NONE',  ( 8.406107780410998487, 5.342170561818999630, 8.432311822615000452 ) ) ;
#48950 = ORIENTED_EDGE ( 'NONE', *, *, #46980, .F. ) ;
#48951 = CARTESIAN_POINT ( 'NONE',  ( 0.2066231058121046349, -2.618168328974044765E-06, -3.206444164765644977 ) ) ;
#48952 = CARTESIAN_POINT ( 'NONE',  ( 11.09999999999999964, 4.000000000000000000, -7.500000000000000000 ) ) ;
#48953 = CARTESIAN_POINT ( 'NONE',  ( 11.72764643456600098, 12.22218869479000070, 1.954421350659000023 ) ) ;
#48954 = CARTESIAN_POINT ( 'NONE',  ( 18.06277981064209115, 1.966570380498756654, 12.44558849270348944 ) ) ;
#48955 = CARTESIAN_POINT ( 'NONE',  ( 10.96237843380999877, 6.768007902811000065, 5.462774374486000895 ) ) ;
#48956 = CARTESIAN_POINT ( 'NONE',  ( 10.94962848994000026, 8.455114238872999621, 6.519461126146000929 ) ) ;
#48957 = CARTESIAN_POINT ( 'NONE',  ( 10.63874943042162613, -4.847937002157847175, 7.284280020558234980 ) ) ;
#48958 = CARTESIAN_POINT ( 'NONE',  ( 10.02101354018262569, -3.231816600031356845, -8.499583552997725278 ) ) ;
#48959 = EDGE_LOOP ( 'NONE', ( #15210, #16206, #30244, #46764 ) ) ;
#48960 = CARTESIAN_POINT ( 'NONE',  ( 12.22799143493891627, -2.916631933635871476, 12.25779765684317191 ) ) ;
#48961 = CARTESIAN_POINT ( 'NONE',  ( 9.530380199233999150, -2.867101906753999785, -7.357604921762999517 ) ) ;
#48962 = CARTESIAN_POINT ( 'NONE',  ( 10.01533268956000100, 4.946987614118000032, 8.559212393557999121 ) ) ;
#48963 = CARTESIAN_POINT ( 'NONE',  ( 30.60000000000000142, 0.000000000000000000, 0.000000000000000000 ) ) ;
#48964 = CARTESIAN_POINT ( 'NONE',  ( 10.37872469555899890, 4.502158848185001006, -6.631215019384099740 ) ) ;
#48965 = ADVANCED_FACE ( 'NONE', ( #39972 ), #14085, .F. ) ;
#48966 = CARTESIAN_POINT ( 'NONE',  ( 12.08004251007355023, -0.01123479547583346692, 12.60000044989513412 ) ) ;
#48967 = CARTESIAN_POINT ( 'NONE',  ( 9.240545280410998430, 4.158911560497999815, 5.873540104660999184 ) ) ;
#48968 = CARTESIAN_POINT ( 'NONE',  ( 9.877261637240000169, 2.207988120125000009, 7.624813826992999921 ) ) ;
#48969 = ADVANCED_FACE ( 'NONE', ( #57067 ), #34386, .F. ) ;
#48970 = AXIS2_PLACEMENT_3D ( 'NONE', #3731, #476, #25759 ) ;
#48971 = CARTESIAN_POINT ( 'NONE',  ( 12.61719528873169338, 3.096122730228594300, 12.29247817764211348 ) ) ;
#48972 = ORIENTED_EDGE ( 'NONE', *, *, #1177, .T. ) ;
#48973 = CARTESIAN_POINT ( 'NONE',  ( 7.854823341228001077, 4.561643343497000735, 6.153061759127000485 ) ) ;
#48974 = CARTESIAN_POINT ( 'NONE',  ( 11.26072066707849828, 4.976067344118500380, -6.909591111168198907 ) ) ;
#48975 = DIRECTION ( 'NONE',  ( 1.000000000000000000, 0.000000000000000000, 0.000000000000000000 ) ) ;
#48976 = DIRECTION ( 'NONE',  ( 1.000000000000000000, 0.000000000000000000, 0.000000000000000000 ) ) ;
#48978 = FACE_OUTER_BOUND ( 'NONE', #16317, .T. ) ;
#48977 = LINE ( 'NONE', #16461, #14063 ) ;
#48979 = CARTESIAN_POINT ( 'NONE',  ( 11.53926573058028282, 12.16827677310549660, 1.947218181066149745 ) ) ;
#48980 = ORIENTED_EDGE ( 'NONE', *, *, #16186, .F. ) ;
#48981 = CARTESIAN_POINT ( 'NONE',  ( 12.31853785129944434, 0.3923495136273177364, 12.69184251826150955 ) ) ;
#48982 = CARTESIAN_POINT ( 'NONE',  ( 18.29983863916000075, -2.861762957209999847, 11.98830831200999825 ) ) ;
#48983 = LINE ( 'NONE', #54574, #37409 ) ;
#48984 = CARTESIAN_POINT ( 'NONE',  ( 17.65093748396062523, 3.195004315067500045, -12.18819265947668207 ) ) ;
#48985 = CARTESIAN_POINT ( 'NONE',  ( 12.20814394425996419, -2.932476687367341128, 13.68943695263251570 ) ) ;
#48986 = CARTESIAN_POINT ( 'NONE',  ( 11.30000285318000230, 11.76356368987999979, 1.428410073821000159 ) ) ;
#48987 = CARTESIAN_POINT ( 'NONE',  ( 8.688612068284298218, -2.650857310365693831, 7.263856826349748275 ) ) ;
#48988 = ORIENTED_EDGE ( 'NONE', *, *, #67649, .T. ) ;
#48989 = CARTESIAN_POINT ( 'NONE',  ( 12.80000000000000071, 11.23412379136000006, -3.084957477885999833 ) ) ;
#48990 = CARTESIAN_POINT ( 'NONE',  ( 7.000000000000000000, 0.000000000000000000, 0.000000000000000000 ) ) ;
#48991 = CARTESIAN_POINT ( 'NONE',  ( 9.679055905794999859, 2.899999999999999911, 6.571291218949999902 ) ) ;
#48992 = CARTESIAN_POINT ( 'NONE',  ( 1.848158326185999956, -2.375092696518000146, -2.913277015014000160 ) ) ;
#48993 = CARTESIAN_POINT ( 'NONE',  ( 18.41067102831979341, -3.015843532943014438, 11.25293825121027780 ) ) ;
#48994 = CARTESIAN_POINT ( 'NONE',  ( 17.56547987801834410, 1.875000035136120458, -12.57545641098305289 ) ) ;
#48995 = CARTESIAN_POINT ( 'NONE',  ( 9.779336721442295044, -4.163631234563185401, 8.749993199158904389 ) ) ;
#48996 = CARTESIAN_POINT ( 'NONE',  ( 11.61364291764652812, 3.140345330584100036, 7.606265891492399511 ) ) ;
#48997 = ADVANCED_FACE ( 'NONE', ( #3575 ), #19646, .T. ) ;
#48998 = CARTESIAN_POINT ( 'NONE',  ( 15.89994436294300151, 8.847904542234999781, 8.580301953175000662 ) ) ;
#48999 = CARTESIAN_POINT ( 'NONE',  ( 11.26847231345999845, -2.565616654150999931, -7.116622328138999976 ) ) ;
#49000 = CARTESIAN_POINT ( 'NONE',  ( 11.32240614981507854, 4.732436490098000270, -7.982093918858203629 ) ) ;
#49001 = ADVANCED_FACE ( 'NONE', ( #35411 ), #50935, .F. ) ;
#49002 = CARTESIAN_POINT ( 'NONE',  ( 9.881157842586999251, -5.290169207169999943, -8.858081286661999343 ) ) ;
#49003 = ADVANCED_FACE ( 'NONE', ( #24908 ), #61018, .F. ) ;
#49004 = CARTESIAN_POINT ( 'NONE',  ( 11.00000000000000000, -5.058572498595999889, -7.825000000000000178 ) ) ;
#49005 = CARTESIAN_POINT ( 'NONE',  ( 11.07907162307749793, -4.814611760850799449, -7.174999999999999822 ) ) ;
#49006 = B_SPLINE_CURVE_WITH_KNOTS ( 'NONE', 3,
 ( #19649, #36064, #24199, #14065 ),
 .UNSPECIFIED., .F., .F.,
 ( 4, 4 ),
 ( 0.000000000000000000, 1.000000000000000000 ),
 .UNSPECIFIED. ) ;
#49007 = ORIENTED_EDGE ( 'NONE', *, *, #43758, .T. ) ;
#49008 = CARTESIAN_POINT ( 'NONE',  ( 7.343717773735517262, 3.601282447181377577, 9.195592440584203331 ) ) ;
#49009 = CARTESIAN_POINT ( 'NONE',  ( 12.15456516821461008, -3.197083038490000195, 6.689681884064299311 ) ) ;
#49010 = ORIENTED_EDGE ( 'NONE', *, *, #44922, .F. ) ;
#49011 = CARTESIAN_POINT ( 'NONE',  ( 17.88731995174124734, -3.029458325253037820, 13.54679862780130151 ) ) ;
#49012 = CARTESIAN_POINT ( 'NONE',  ( 10.54272335273199879, -3.555125495332600138, -8.698083075453000745 ) ) ;
#49013 = ORIENTED_EDGE ( 'NONE', *, *, #30867, .T. ) ;
#49014 = CARTESIAN_POINT ( 'NONE',  ( 10.68546886766499959, 3.433493735705800187, 8.529286361367999447 ) ) ;
#49015 = CARTESIAN_POINT ( 'NONE',  ( 5.550586697066033359, 1.058569194974100736, -0.4045265221279905066 ) ) ;
#49016 = CARTESIAN_POINT ( 'NONE',  ( 24.09353084724989813, 3.337595895983183958, -12.57553257596956975 ) ) ;
#49017 = CARTESIAN_POINT ( 'NONE',  ( 18.31386961183700279, -3.086648833569000328, 11.29009770192999973 ) ) ;
#49018 = DIRECTION ( 'NONE',  ( 0.000000000000000000, 1.000000000000000000, 0.000000000000000000 ) ) ;
#49019 = DIRECTION ( 'NONE',  ( 1.000000000000000000, 0.000000000000000000, 0.000000000000000000 ) ) ;
#49020 = CARTESIAN_POINT ( 'NONE',  ( 6.901403243225498585, -0.7129370139181090416, -0.8934472489575943088 ) ) ;
#49021 = AXIS2_PLACEMENT_3D ( 'NONE', #41498, #62811, #14929 ) ;
#49022 = CARTESIAN_POINT ( 'NONE',  ( 9.766127544684000128, -4.735430008785999512, -8.791396910319001279 ) ) ;
#49023 = LINE ( 'NONE', #49360, #17300 ) ;
#49024 = VERTEX_POINT ( 'NONE', #19315 ) ;
#49025 = CARTESIAN_POINT ( 'NONE',  ( 10.06481084123000080, 5.336630274082000192, -7.092011739486999922 ) ) ;
#49026 = VERTEX_POINT ( 'NONE', #29837 ) ;
#49027 = EDGE_CURVE ( 'NONE', #10085, #798, #61626, .T. ) ;
#49028 = DIRECTION ( 'NONE',  ( 1.000000000000000000, 0.000000000000000000, 0.000000000000000000 ) ) ;
#49029 = SHAPE_REPRESENTATION_RELATIONSHIP ( 'NONE' , 'NONE' ,  #24587, #46039 ) ;
#49030 = ORIENTED_EDGE ( 'NONE', *, *, #67100, .F. ) ;
#49031 = DIRECTION ( 'NONE',  ( 1.000000000000000000, 0.000000000000000000, 0.000000000000000000 ) ) ;
#49032 = CARTESIAN_POINT ( 'NONE',  ( 10.37837607040047594, 4.867967756586605965, 7.603545367532808186 ) ) ;
#49033 = CARTESIAN_POINT ( 'NONE',  ( 10.36825461470400001, 2.760277452415999644, -7.815392442832299835 ) ) ;
#49034 = CARTESIAN_POINT ( 'NONE',  ( 9.393930206848999376, -5.250000000000000000, -7.500000000000000000 ) ) ;
#49035 = B_SPLINE_SURFACE_WITH_KNOTS ( 'NONE', 3, 3, ( 
 ( #39274, #65483, #65131, #38575 ),
 ( #49760, #59899, #44535, #33344 ),
 ( #49407, #54306, #60596, #17608 ),
 ( #22489, #55352, #7450, #49068 ),
 ( #28802, #50112, #44185, #3154 ),
 ( #45809, #67120, #6409, #27757 ),
 ( #1176, #14682, #25512, #20262 ),
 ( #20955, #42291, #47183, #10118 ),
 ( #15709, #67458, #52070, #36344 ) ),
 .UNSPECIFIED., .F., .F., .F.,
 ( 4, 1, 1, 1, 1, 1, 4 ),
 ( 4, 4 ),
 ( 0.05182816266979999725, 0.1666666666667000196, 0.3333333333333000081, 0.5000000000000000000, 0.6666666666667000474, 0.8333333333333000637, 0.9772240888782000034 ),
 ( -0.1900389547208000129, 1.190219847277000031 ),
 .UNSPECIFIED. ) ;
#49036 = CARTESIAN_POINT ( 'NONE',  ( 4.399997082757114875, 2.000000000000000000, 4.865849894060234886E-09 ) ) ;
#49037 = DIRECTION ( 'NONE',  ( 0.000000000000000000, 1.000000000000000000, -1.290201028711000169E-14 ) ) ;
#49038 = CARTESIAN_POINT ( 'NONE',  ( 12.19601928331639051, 0.1418539764880151210, 13.89904537328360767 ) ) ;
#49039 = ORIENTED_EDGE ( 'NONE', *, *, #13240, .T. ) ;
#49040 = CARTESIAN_POINT ( 'NONE',  ( 7.062228317541999978, 5.346164515353000191, -7.398308812559000636 ) ) ;
#49041 = LINE ( 'NONE', #44158, #21719 ) ;
#49042 = DIRECTION ( 'NONE',  ( 0.000000000000000000, 1.000000000000000000, 0.000000000000000000 ) ) ;
#49043 = CARTESIAN_POINT ( 'NONE',  ( 4.851842514214999902, 1.628762548987999992, 0.05628454206072999733 ) ) ;
#49044 = CARTESIAN_POINT ( 'NONE',  ( 8.681370280410998674, 2.949305648881000330, -8.659807625323999503 ) ) ;
#49045 = EDGE_CURVE ( 'NONE', #53731, #54722, #54262, .T. ) ;
#49046 = CARTESIAN_POINT ( 'NONE',  ( 9.885596873516499627, 2.907767014557175678, -8.129523725463620565 ) ) ;
#49047 = CARTESIAN_POINT ( 'NONE',  ( 10.01276877312999858, -3.440626575163999945, -9.267592337498999910 ) ) ;
#49048 = ORIENTED_EDGE ( 'NONE', *, *, #56063, .F. ) ;
#49049 = CARTESIAN_POINT ( 'NONE',  ( 6.953052440528999512, -9.233022020364000326, -5.200634764108000851 ) ) ;
#49050 = CARTESIAN_POINT ( 'NONE',  ( 10.90000000000000036, -5.100000000000000533, -6.436740704805999691 ) ) ;
#49051 = ADVANCED_FACE ( 'NONE', ( #24571 ), #2550, .F. ) ;
#49052 = DIRECTION ( 'NONE',  ( 0.000000000000000000, -0.2588190451024934280, -0.9659258262890756397 ) ) ;
#49053 = DIRECTION ( 'NONE',  ( 1.000000000000000000, 0.000000000000000000, 4.770489558936215471E-13 ) ) ;
#49054 = CARTESIAN_POINT ( 'NONE',  ( 11.76133460557259980, 4.139849081322200419, -8.354833838171700222 ) ) ;
#49055 = CARTESIAN_POINT ( 'NONE',  ( 1.021806799209249883, 3.408904368339103375, 0.9161175952574877046 ) ) ;
#49056 = CARTESIAN_POINT ( 'NONE',  ( 10.97635090131019986, 4.999207052587699707, -8.118017011233499503 ) ) ;
#49057 = CARTESIAN_POINT ( 'NONE',  ( 9.710646554150999421, 4.486270025758400060, -8.378853663802400931 ) ) ;
#49059 = CARTESIAN_POINT ( 'NONE',  ( 11.50000000000000000, -5.058572498595999889, 7.174999999999999822 ) ) ;
#49058 = CARTESIAN_POINT ( 'NONE',  ( 9.572442991499999110, -4.063228561016970275, 8.502419298200999620 ) ) ;
#49060 = CYLINDRICAL_SURFACE ( 'NONE', #68767, 13.10000000000000142 ) ;
#49061 = ORIENTED_EDGE ( 'NONE', *, *, #59962, .T. ) ;
#49062 = CARTESIAN_POINT ( 'NONE',  ( 10.89835090130999973, 4.878966983716200190, 6.956352367771000189 ) ) ;
#49063 = CARTESIAN_POINT ( 'NONE',  ( 10.40226385995999969, -2.765692573780999641, 9.035345396600000356 ) ) ;
#49064 = CARTESIAN_POINT ( 'NONE',  ( 10.08762143724499794, 4.758411336345700349, 8.353549467159899322 ) ) ;
#49065 = CARTESIAN_POINT ( 'NONE',  ( 5.684131420607005936, -13.00367204148822253, 2.123909540366339499 ) ) ;
#49066 = CARTESIAN_POINT ( 'NONE',  ( 9.724613486786999772, -2.928302463146000179, 8.718481221599999387 ) ) ;
#49067 = CARTESIAN_POINT ( 'NONE',  ( 9.718562776053557783, -5.699238565681682189, 7.915948022123772354 ) ) ;
#49068 = CARTESIAN_POINT ( 'NONE',  ( 11.56571517796000137, 3.339665324758999798, -11.82228365027999928 ) ) ;
#49069 = CARTESIAN_POINT ( 'NONE',  ( 9.001430433046998303, -4.854750075120300323, -6.972511033848699746 ) ) ;
#49070 = CARTESIAN_POINT ( 'NONE',  ( 11.43344776364301474, -11.63114020343308752, -1.412330517650108197 ) ) ;
#49071 = CARTESIAN_POINT ( 'NONE',  ( 6.232675381438999906, -1.260983081135999884, 0.3979920142897999669 ) ) ;
#49072 = CARTESIAN_POINT ( 'NONE',  ( 11.59999999999999964, 4.000000000000000000, 7.500000000000000000 ) ) ;
#49073 = CARTESIAN_POINT ( 'NONE',  ( 8.599999952505998024, 4.000000000000000000, -7.500000000000000000 ) ) ;
#49074 = CARTESIAN_POINT ( 'NONE',  ( 12.69240093715870188, 0.6148490057825425348, -12.67995724530760526 ) ) ;
#49075 = CARTESIAN_POINT ( 'NONE',  ( 11.17056785386839834, 3.281375110759499947, -7.983608166707499620 ) ) ;
#49076 = CARTESIAN_POINT ( 'NONE',  ( 5.500000000000000000, 12.43893545635000031, -2.828937028792000152 ) ) ;
#49077 = CARTESIAN_POINT ( 'NONE',  ( 25.52344582623700120, -8.321938514753998817, 8.140348312953999965 ) ) ;
#49078 = CARTESIAN_POINT ( 'NONE',  ( 12.70917152006029660, 3.194951439744890820, 12.18820651941773470 ) ) ;
#49079 = VERTEX_POINT ( 'NONE', #45894 ) ;
#49080 = CARTESIAN_POINT ( 'NONE',  ( 7.683561622480320707, -2.820687929279365846, 8.178835501142698305 ) ) ;
#49081 = EDGE_CURVE ( 'NONE', #17996, #40048, #66544, .T. ) ;
#49082 = ITEM_DEFINED_TRANSFORMATION ( 'NONE', 'NONE', #65285,  #9676 ) ;
#49083 = EDGE_CURVE ( 'NONE', #15974, #18846, #33602, .T. ) ;
#49084 = CARTESIAN_POINT ( 'NONE',  ( 11.02301463001509774, -3.452642973349600464, -6.623338154204899908 ) ) ;
#49085 = FACE_OUTER_BOUND ( 'NONE', #47450, .T. ) ;
#49086 = CARTESIAN_POINT ( 'NONE',  ( 7.933148997457998952, -5.167567567567999731, 6.822293592207000934 ) ) ;
#49087 = CARTESIAN_POINT ( 'NONE',  ( 7.000000000000000888, 9.534618748583843839, 4.680683473982556464 ) ) ;
#49088 = CARTESIAN_POINT ( 'NONE',  ( 13.55500032369700136, 12.12437004458000089, 2.498522620030000141 ) ) ;
#49089 = ORIENTED_EDGE ( 'NONE', *, *, #55802, .T. ) ;
#49090 = CARTESIAN_POINT ( 'NONE',  ( 23.60205915885299888, 9.230633470673003771, 8.204162215335996322 ) ) ;
#49091 = CARTESIAN_POINT ( 'NONE',  ( 18.12879638218879208, 2.748081584522202192, -13.61770999214558486 ) ) ;
#49092 = EDGE_LOOP ( 'NONE', ( #45729, #13141, #36890, #43676, #4018 ) ) ;
#49093 = LINE ( 'NONE', #12384, #59668 ) ;
#49094 = CARTESIAN_POINT ( 'NONE',  ( 2.800973465877999669, -3.500000000000000000, 0.000000000000000000 ) ) ;
#49095 = CARTESIAN_POINT ( 'NONE',  ( 9.369139158774000720, 2.685250982074999904, -7.026194612421999608 ) ) ;
#49096 = FACE_OUTER_BOUND ( 'NONE', #36125, .T. ) ;
#49097 = FACE_OUTER_BOUND ( 'NONE', #22666, .T. ) ;
#49098 = CARTESIAN_POINT ( 'NONE',  ( 7.622520280405000292, 3.458959908335999867, -5.854223596299999777 ) ) ;
#49099 = CARTESIAN_POINT ( 'NONE',  ( 10.23976354018233259, -4.327184855449098144, -6.282534154164605589 ) ) ;
#49100 = CARTESIAN_POINT ( 'NONE',  ( 10.99166666666866909, -4.098468854244173620, 8.958105619229149497 ) ) ;
#49101 = ORIENTED_EDGE ( 'NONE', *, *, #54172, .T. ) ;
#49102 = DIRECTION ( 'NONE',  ( 1.000000000000000000, 0.000000000000000000, 0.000000000000000000 ) ) ;
#49103 = CARTESIAN_POINT ( 'NONE',  ( 17.75984001016927394, -3.091833346833228191, -13.52991597408320068 ) ) ;
#49104 = ORIENTED_EDGE ( 'NONE', *, *, #61642, .F. ) ;
#49105 = EDGE_CURVE ( 'NONE', #26424, #873, #47271, .T. ) ;
#49106 = CARTESIAN_POINT ( 'NONE',  ( 8.807788144226000426, 4.090932644426789722, -8.453461841935100196 ) ) ;
#49107 = DIRECTION ( 'NONE',  ( -0.8660254038714592095, 4.159366548383805334E-14, 0.4999999998492760667 ) ) ;
#49108 = VERTEX_POINT ( 'NONE', #58101 ) ;
#49109 = CARTESIAN_POINT ( 'NONE',  ( 9.936596320338999533, 2.942832934044000037, 7.931430460958599049 ) ) ;
#49110 = CARTESIAN_POINT ( 'NONE',  ( 18.04064113784076184, 0.3934955818404124450, -13.89250369607471036 ) ) ;
#49111 = CARTESIAN_POINT ( 'NONE',  ( 5.058539461080999722, -0.8103260286165000492, -1.161807459232000017 ) ) ;
#49112 = CARTESIAN_POINT ( 'NONE',  ( 8.474485200571999499, -5.100000000000000533, 6.560614371780999043 ) ) ;
#49113 = CARTESIAN_POINT ( 'NONE',  ( 15.95563772304700301, 3.878390400849000219, 11.75631652949000205 ) ) ;
#49114 = CARTESIAN_POINT ( 'NONE',  ( 10.42499241036494162, 5.349775919985349404, 7.500001834605750872 ) ) ;
#49115 = CARTESIAN_POINT ( 'NONE',  ( 9.737988259786000356, 3.886559292927400211, 6.640442468193600511 ) ) ;
#49116 = CARTESIAN_POINT ( 'NONE',  ( 13.09019624054849551, -12.38961571551778640, -1.836606440307318788 ) ) ;
#49117 = ORIENTED_EDGE ( 'NONE', *, *, #30747, .F. ) ;
#49118 = CARTESIAN_POINT ( 'NONE',  ( 9.470944094206000585, 5.100000000000000533, 6.571291218949999902 ) ) ;
#49119 = CARTESIAN_POINT ( 'NONE',  ( 10.86460778041000097, 3.843601682313000367, -5.985271987931999327 ) ) ;
#49120 = CARTESIAN_POINT ( 'NONE',  ( 18.49944584006882309, -11.81600967868165775, 4.156020558874723214 ) ) ;
#49121 = CARTESIAN_POINT ( 'NONE',  ( 12.48119050255584739, 1.864280969780519825, -13.87532308892432553 ) ) ;
#49122 = CARTESIAN_POINT ( 'NONE',  ( 11.22934687351609817, -4.163624617374463099, 8.750000000000000000 ) ) ;
#49123 = B_SPLINE_CURVE_WITH_KNOTS ( 'NONE', 3,
 ( #50710, #35664, #18899, #56979 ),
 .UNSPECIFIED., .F., .F.,
 ( 4, 4 ),
 ( 0.000000000000000000, 1.000000000000000000 ),
 .UNSPECIFIED. ) ;
#49124 = CARTESIAN_POINT ( 'NONE',  ( 10.40226385995999969, -2.765692573780999641, 9.035345396600000356 ) ) ;
#49125 = CARTESIAN_POINT ( 'NONE',  ( 18.22962728801296350, -0.2678304234474040424, 13.99744223245316199 ) ) ;
#49126 = CARTESIAN_POINT ( 'NONE',  ( 24.37898897380600260, -3.167411416339000141, 12.03697664498000108 ) ) ;
#49127 = ORIENTED_EDGE ( 'NONE', *, *, #49921, .T. ) ;
#49128 = VERTEX_POINT ( 'NONE', #36779 ) ;
#49129 = CARTESIAN_POINT ( 'NONE',  ( 11.09999999999999964, -1.406666666667000021, -10.45580168561000001 ) ) ;
#49130 = EDGE_CURVE ( 'NONE', #58398, #40087, #52793, .T. ) ;
#49131 = CARTESIAN_POINT ( 'NONE',  ( 12.72381130736580346, -0.6210784669183123663, 13.88131957737377675 ) ) ;
#49132 = CARTESIAN_POINT ( 'NONE',  ( 12.47605349752420523, -0.5315089155663856868, -13.88632137824048485 ) ) ;
#49133 = CARTESIAN_POINT ( 'NONE',  ( 7.100000000000000533, 0.000000000000000000, 0.000000000000000000 ) ) ;
#49134 = CARTESIAN_POINT ( 'NONE',  ( 17.77470470791479684, -0.5852235853112173203, -13.88341353704719161 ) ) ;
#49135 = CARTESIAN_POINT ( 'NONE',  ( 7.000000000000000000, -0.2897247358851999799, 3.000000000000000000 ) ) ;
#49137 = VECTOR ( 'NONE', #63881, 1000.000000000000000 ) ;
#49136 = CARTESIAN_POINT ( 'NONE',  ( 8.724024145839393896, 3.782477278638352036, -8.345440805164775711 ) ) ;
#49139 = CARTESIAN_POINT ( 'NONE',  ( 18.30000000002853255, 11.04996330603946930, -3.691231741019871837 ) ) ;
#49138 = CARTESIAN_POINT ( 'NONE',  ( 8.766851002546001581, 2.832432432432000269, 6.822293592207000934 ) ) ;
#49140 = FACE_OUTER_BOUND ( 'NONE', #65168, .T. ) ;
#49141 = CARTESIAN_POINT ( 'NONE',  ( 12.09999999999999964, -4.883784007588900522, 7.174999999999999822 ) ) ;
#49142 = CARTESIAN_POINT ( 'NONE',  ( 8.943784697134999462, 4.470490447737899942, -6.771750947090999340 ) ) ;
#49143 = CARTESIAN_POINT ( 'NONE',  ( 17.98979505986429572, -0.4491390935506889281, 12.68931154995401123 ) ) ;
#49144 = CARTESIAN_POINT ( 'NONE',  ( 6.703706320014999775, -0.3939706863108000112, -1.504006644519000124 ) ) ;
#49145 = CARTESIAN_POINT ( 'NONE',  ( 18.12474152633276958, -2.757110843054713989, -12.38793583424880040 ) ) ;
#49146 = EDGE_LOOP ( 'NONE', ( #4485, #50759, #37149, #357 ) ) ;
#49148 = CARTESIAN_POINT ( 'NONE',  ( 17.60000000000000142, 10.78295181803999903, -4.410266442048000002 ) ) ;
#49147 = CARTESIAN_POINT ( 'NONE',  ( 23.85395670473670648, -3.593170000430095712, 13.20269580752050054 ) ) ;
#49149 = CARTESIAN_POINT ( 'NONE',  ( 9.202245280414000916, 5.095038542659000136, -6.157541456184000062 ) ) ;
#49150 = B_SPLINE_CURVE_WITH_KNOTS ( 'NONE', 3,
 ( #44108, #44460, #16141, #37463, #17878, #50724, #66796, #24838, #55279, #29069, #8417, #66447, #7726, #34655, #65755, #28716, #2142, #50379 ),
 .UNSPECIFIED., .F., .F.,
 ( 4, 2, 2, 2, 2, 2, 2, 2, 4 ),
 ( 0.5009155270902381218, 0.5633010862039566913, 0.5944938657608158650, 0.6256866453176750387, 0.6568794248745342124, 0.6880722044313933861, 0.7504577635451146200, 0.8752288817725573100, 1.000000000000000000 ),
 .UNSPECIFIED. ) ;
#49151 = DIRECTION ( 'NONE',  ( 1.000000000000000000, 0.000000000000000000, 0.000000000000000000 ) ) ;
#49152 = CARTESIAN_POINT ( 'NONE',  ( 23.89320776801300283, 8.928716006355012169, -8.952507060126997374 ) ) ;
#49153 = CARTESIAN_POINT ( 'NONE',  ( 0.8807558238970999431, -0.8575131787502999758, -3.600995375387999964 ) ) ;
#49154 = CARTESIAN_POINT ( 'NONE',  ( 10.69568717260499824, 3.533932086969799879, 6.739296831621899742 ) ) ;
#49155 = CARTESIAN_POINT ( 'NONE',  ( 1.948412681420000014, 1.958206349467000118, -3.033258895291999657 ) ) ;
#49156 = ORIENTED_EDGE ( 'NONE', *, *, #1092, .F. ) ;
#49157 = CARTESIAN_POINT ( 'NONE',  ( 12.32690578124262615, -0.5408165383911121005, -12.58839068838662456 ) ) ;
#49158 = CARTESIAN_POINT ( 'NONE',  ( 9.970944094204998720, 5.100000000000000533, 6.571291218949999902 ) ) ;
#49159 = CARTESIAN_POINT ( 'NONE',  ( 18.27387565520746193, 2.575953525795611210, -12.33388021351436770 ) ) ;
#49160 = CARTESIAN_POINT ( 'NONE',  ( 7.142264750549939478, -3.320997592312212365, 8.680193631428091194 ) ) ;
#49161 = CARTESIAN_POINT ( 'NONE',  ( 8.989142219592000771, 5.284130523641000110, 6.489275570566000795 ) ) ;
#49162 = VERTEX_POINT ( 'NONE', #68574 ) ;
#49163 = CARTESIAN_POINT ( 'NONE',  ( 6.133316242380999483, -0.9919734638370999447, -1.274097314648999779 ) ) ;
#49164 = EDGE_CURVE ( 'NONE', #21413, #1641, #42026, .T. ) ;
#49165 = ADVANCED_FACE ( 'NONE', ( #6674 ), #21715, .F. ) ;
#49166 = CARTESIAN_POINT ( 'NONE',  ( 7.300545280410000615, 2.766448485756999975, -6.536937350656000234 ) ) ;
#49168 = CARTESIAN_POINT ( 'NONE',  ( 10.89227882974000039, 3.998355201738000630, 9.261308739708001170 ) ) ;
#49167 = CARTESIAN_POINT ( 'NONE',  ( 8.520843751322205506, -2.921428602731328539, 6.124930925903640855 ) ) ;
#49169 = CARTESIAN_POINT ( 'NONE',  ( 10.31021345716899873, -3.363461959113699606, -8.078719053813800954 ) ) ;
#49170 = ORIENTED_EDGE ( 'NONE', *, *, #41654, .T. ) ;
#49171 = DIRECTION ( 'NONE',  ( 0.5298945044129826920, -2.133608886496929164E-08, -0.8480635673066725388 ) ) ;
#49172 = B_SPLINE_CURVE_WITH_KNOTS ( 'NONE', 3,
 ( #45336, #66646, #8610, #34847, #8266, #51261, #36206, #57523, #25370, #41114, #47048, #19787, #5075, #52626, #56852, #26412, #57183, #25030 ),
 .UNSPECIFIED., .F., .F.,
 ( 4, 2, 2, 2, 2, 2, 2, 2, 4 ),
 ( 0.000000000000000000, 0.1250000000000000833, 0.2500000000000001665, 0.3750000000000001665, 0.5000000000000002220, 0.6250000000000002220, 0.7500000000000001110, 0.8750000000000001110, 1.000000000000000000 ),
 .UNSPECIFIED. ) ;
#49173 = CARTESIAN_POINT ( 'NONE',  ( 10.07101719722999889, -4.042170815906999337, 8.920201479886998186 ) ) ;
#49174 = ORIENTED_EDGE ( 'NONE', *, *, #49735, .T. ) ;
#49175 = CARTESIAN_POINT ( 'NONE',  ( 10.88314899746000108, 5.167567567567999731, 6.822293592207000934 ) ) ;
#49177 = CARTESIAN_POINT ( 'NONE',  ( 16.39947726215000046, 3.188035298175999621, 11.45126509954999960 ) ) ;
#49176 = CIRCLE ( 'NONE', #6747, 0.5500000000000001554 ) ;
#49178 = CARTESIAN_POINT ( 'NONE',  ( 18.17882709566423216, 0.04040202251154540597, -13.89992604541789589 ) ) ;
#49179 = EDGE_LOOP ( 'NONE', ( #9275, #43932, #5410 ) ) ;
#49180 = CARTESIAN_POINT ( 'NONE',  ( 16.09997386696500143, -8.350085070477001992, -8.123950967096998710 ) ) ;
#49181 = LINE ( 'NONE', #60018, #18205 ) ;
#49182 = CARTESIAN_POINT ( 'NONE',  ( 10.60746886766490071, 3.501664543805500074, -6.594573315824700188 ) ) ;
#49183 = CARTESIAN_POINT ( 'NONE',  ( 9.020964430773000586, -2.907392932634000005, 6.146188468825999784 ) ) ;
#49184 = CARTESIAN_POINT ( 'NONE',  ( 11.83041235500449950, -4.942357465271699724, 8.363295307663500822 ) ) ;
#49185 = VERTEX_POINT ( 'NONE', #28016 ) ;
#49186 = CARTESIAN_POINT ( 'NONE',  ( 8.449239158774000558, 5.458692773671000253, 7.456452194274000078 ) ) ;
#49187 = CARTESIAN_POINT ( 'NONE',  ( 18.03598133453871810, -1.971494603937298029, 13.86049335245054337 ) ) ;
#49188 = EDGE_CURVE ( 'NONE', #53432, #38357, #10746, .T. ) ;
#49189 = AXIS2_PLACEMENT_3D ( 'NONE', #41249, #31117, #52420 ) ;
#49190 = DIRECTION ( 'NONE',  ( 0.000000000000000000, 0.7614089499631908620, -0.6482718649732928107 ) ) ;
#49191 = CARTESIAN_POINT ( 'NONE',  ( 18.20247741952565690, 0.3746922850090889101, 12.59513687151705241 ) ) ;
#49192 = EDGE_LOOP ( 'NONE', ( #59119, #21065, #8069, #36374, #26938 ) ) ;
#49193 = B_SPLINE_SURFACE_WITH_KNOTS ( 'NONE', 1, 3, ( 
 ( #35228, #40130, #24382, #45713, #18802, #50953, #28961, #22396, #38480, #3051, #17148, #56198, #61443, #2369, #59803, #3390, #40454, #23693, #24726, #67022, #61781, #55858, #66679, #45027, #39779, #32895, #24037, #50611, #8644, #13900, #66332, #29994, #51294, #11552, #54206, #33243, #13562, #34882, #6307, #7963, #27654, #1081, #43733, #54564, #18456, #7613, #61100, #29300, #2713, #46744, #67699, #5113, #68737, #31352, #10014, #47086, #41157, #26102, #57917, #20163, #35900, #15612, #67357, #62123, #3729, #63491, #41833, #36942, #9318, #68387, #19480, #57216, #68049, #30323, #51969, #36591, #47428, #20507, #53017, #40800, #41490, #14242, #52665, #51633, #30660, #63142, #14921, #4072, #4761, #25064, #31014, #31694, #62802, #20854, #52324, #15267, #58256, #46398, #46053, #42190, #25409, #10360, #62463, #35570, #56885, #36244, #4419, #25757, #19826, #8983, #14583, #57563 ),
 ( #9664, #11387, #65214, #27837, #5797, #59979, #6490, #59635, #26449, #42869, #6140, #43563, #69089, #64517, #47781, #33074, #42526, #63835, #27140, #21195, #568, #64863, #15949, #48458, #48114, #54739, #49143, #11732, #54388, #27481, #21535, #1254, #38307, #21878, #16292, #17331, #37278, #58599, #53361, #43912, #22226, #38660, #58947, #48805, #10700, #37615, #43212, #32045, #32389, #16976, #22569, #914, #33421, #5463, #16635, #26800, #12090, #217, #11054, #64178, #37963, #53703, #59283, #32727, #54040, #61704, #23610, #13483, #13138, #23959, #19053, #7190, #13821, #40052, #44268, #35150, #44613, #12437, #33769, #49488, #40380, #28527, #6838, #29218, #34804, #7526, #66942, #29573, #7884, #2972, #60331, #55434, #34467, #49839, #1598, #61021, #45639, #28171, #22915, #65565, #50530, #17687, #39012, #2632, #56114, #8226, #45293, #18718, #39352, #55084, #1950, #50875 ) ),
 .UNSPECIFIED., .F., .F., .F.,
 ( 2, 2 ),
 ( 4, 2, 2, 2, 2, 2, 2, 2, 2, 2, 2, 2, 2, 2, 2, 2, 2, 2, 2, 2, 2, 2, 2, 2, 2, 2, 2, 2, 2, 2, 2, 2, 2, 2, 2, 2, 2, 2, 2, 2, 2, 2, 2, 2, 2, 2, 2, 2, 2, 2, 2, 2, 2, 2, 2, 4 ),
 ( 0.000000000000000000, 1.000000000000000000 ),
 ( 0.000000000000000000, 7.083325941644265020E-05, 0.0001416665188328853004, 0.0002124997782493279370, 0.0002479164079575492960, 0.0002833330376657706008, 0.0003187496673739919056, 0.0003541662970822132646, 0.0004249995564986558741, 0.0004604161862068772331, 0.0004781245010609879126, 0.0004958328159150985921, 0.0005312494456233198426, 0.0005666660753315412016, 0.0006374993347479838111, 0.0006729159644562051701, 0.0007083325941644265291, 0.0007437492238726477797, 0.0007791658535808691386, 0.0008145824832890904976, 0.0008499991129973117482, 0.0008854157427055331072, 0.0009208323724137544661, 0.0009562490021219758251, 0.0009916656318301971841, 0.001027082261538418435, 0.001062498891246639685, 0.001133332150663082403, 0.001168748780371303871, 0.001204165410079525121, 0.001239582039787746372, 0.001274998669495967622, 0.001345831928912410340, 0.001381248558620631808, 0.001416665188328853058, 0.001452081818037074309, 0.001469790132891184934, 0.001487498447745295559, 0.001558331707161738277, 0.001629164966578180995, 0.001664581596286402246, 0.001699998225994623496, 0.001735414855702844747, 0.001770831485411066214, 0.001841664744827508932, 0.001877081374535730183, 0.001912498004243951650, 0.001947914633952173118, 0.001983331263660394368, 0.002018747893368615619, 0.002054164523076836869, 0.002124997782493279370, 0.002160414412201500621, 0.002195831041909721872, 0.002231247671617943122, 0.002266664301326164806 ),
 .UNSPECIFIED. ) ;
#49194 = CARTESIAN_POINT ( 'NONE',  ( 12.60184172746871845, -1.908867898185656165, -12.56980895172865687 ) ) ;
#49195 = ADVANCED_FACE ( 'NONE', ( #11230 ), #64703, .T. ) ;
#49196 = CARTESIAN_POINT ( 'NONE',  ( 4.600001223043999943, 0.000000000000000000, 0.000000000000000000 ) ) ;
#49197 = FACE_OUTER_BOUND ( 'NONE', #45773, .T. ) ;
#49198 = CARTESIAN_POINT ( 'NONE',  ( 5.000030787342999439, 0.2748844998327762412, 2.099962892531004766 ) ) ;
#49199 = CARTESIAN_POINT ( 'NONE',  ( 7.100000000000000533, -2.649999999999999911, -7.500000000000000000 ) ) ;
#49200 = CARTESIAN_POINT ( 'NONE',  ( 11.28533594839949750, -3.249987070165300196, -6.640482273977399430 ) ) ;
#49201 = CARTESIAN_POINT ( 'NONE',  ( 12.35703415365825997, -3.053811614365077531, 12.22452321716729529 ) ) ;
#49202 = CARTESIAN_POINT ( 'NONE',  ( 17.85753477061702199, -1.826313832178724228, 12.46694048874451077 ) ) ;
#49203 = VERTEX_POINT ( 'NONE', #7369 ) ;
#49204 = CARTESIAN_POINT ( 'NONE',  ( 11.72433327354039889, -4.983220429128399687, -6.856888818507299810 ) ) ;
#49205 = ORIENTED_EDGE ( 'NONE', *, *, #23357, .T. ) ;
#49206 = CARTESIAN_POINT ( 'NONE',  ( 11.84785375340600133, -12.11644693747000012, -2.030267990277999868 ) ) ;
#49207 = CARTESIAN_POINT ( 'NONE',  ( 9.444964158775000840, 3.920043641733999884, -9.398198753036000497 ) ) ;
#49208 = CARTESIAN_POINT ( 'NONE',  ( 10.07930935222999835, 2.718121894972999719, -6.397795030233000446 ) ) ;
#49209 = CARTESIAN_POINT ( 'NONE',  ( 10.57793869653000129, -4.393380534095000733, -6.024358525186999991 ) ) ;
#49210 = DIRECTION ( 'NONE',  ( 0.000000000000000000, 0.7071067811865475727, -0.7071067811865475727 ) ) ;
#49211 = CARTESIAN_POINT ( 'NONE',  ( 7.928980562030001344, 3.137685067990001020, -6.261915436850998162 ) ) ;
#49212 = CARTESIAN_POINT ( 'NONE',  ( 12.09999999999999964, -4.000000000000000000, 7.500000000000000000 ) ) ;
#49213 = VERTEX_POINT ( 'NONE', #16814 ) ;
#49214 = CARTESIAN_POINT ( 'NONE',  ( 13.00000000001300116, -11.52577654661000039, -1.696746661728000038 ) ) ;
#49215 = CARTESIAN_POINT ( 'NONE',  ( 9.215291255903000689, 4.861981595026999337, 8.938817176893000038 ) ) ;
#49216 = CARTESIAN_POINT ( 'NONE',  ( 10.43314899746000002, 5.167567567567999731, 6.822293592207000934 ) ) ;
#49217 = CARTESIAN_POINT ( 'NONE',  ( 10.50333291544900050, 4.531093146757585899, -8.658936933361777832 ) ) ;
#49218 = FACE_OUTER_BOUND ( 'NONE', #35683, .T. ) ;
#49219 = CARTESIAN_POINT ( 'NONE',  ( 11.60948876160955479, 3.304472173606900043, -8.223320049540498999 ) ) ;
#49220 = CARTESIAN_POINT ( 'NONE',  ( 7.100000000000255440, 2.544001923346042027, -7.316064667941583721 ) ) ;
#49221 = EDGE_CURVE ( 'NONE', #58532, #52202, #68624, .T. ) ;
#49222 = CARTESIAN_POINT ( 'NONE',  ( 24.02105235195200095, -9.294045785069000587, -9.129243723463000393 ) ) ;
#49223 = CARTESIAN_POINT ( 'NONE',  ( 23.64693289005300159, -10.02912268983000033, 9.634668899592000457 ) ) ;
#49224 = AXIS2_PLACEMENT_3D ( 'NONE', #7265, #28605, #17412 ) ;
#49225 = CARTESIAN_POINT ( 'NONE',  ( 11.64596081258699911, -3.342173145742999729, 11.21570452027999920 ) ) ;
#49226 = ORIENTED_EDGE ( 'NONE', *, *, #43260, .F. ) ;
#49227 = CARTESIAN_POINT ( 'NONE',  ( 8.656816940379998826, -5.329429281359999493, 6.027400270608000099 ) ) ;
#49228 = CARTESIAN_POINT ( 'NONE',  ( 7.160908395509999025, 1.148632353890999935, -0.7444811394398999083 ) ) ;
#49229 = CARTESIAN_POINT ( 'NONE',  ( 18.04548494004247772, 2.887558854919742402, 13.58353091070611107 ) ) ;
#49230 = CARTESIAN_POINT ( 'NONE',  ( 15.90003771078200145, -3.695138809391000034, -11.25918926437999978 ) ) ;
#49231 = CARTESIAN_POINT ( 'NONE',  ( 11.55194988689359903, -3.419512757306400363, -8.638573882912000457 ) ) ;
#49232 = ORIENTED_EDGE ( 'NONE', *, *, #21455, .T. ) ;
#49233 = CARTESIAN_POINT ( 'NONE',  ( 24.59232953626900198, 3.480949472584999871, -12.13588208332000029 ) ) ;
#49234 = CARTESIAN_POINT ( 'NONE',  ( 9.143920280410000601, 5.791553967443999973, 7.752111263209999770 ) ) ;
#49236 = CARTESIAN_POINT ( 'NONE',  ( 9.241072744221000335, -4.062652182992059657, 6.633566614602499634 ) ) ;
#49235 = CARTESIAN_POINT ( 'NONE',  ( 9.012204719595001023, 3.161445734422999809, -6.178649910536000434 ) ) ;
#49237 = AXIS2_PLACEMENT_3D ( 'NONE', #66466, #62257, #14032 ) ;
#49238 = CARTESIAN_POINT ( 'NONE',  ( 2.813453680541110113, 2.907771984247602859, 1.469325272863359899 ) ) ;
#49239 = EDGE_LOOP ( 'NONE', ( #38621, #13364, #38680, #21173 ) ) ;
#49240 = CARTESIAN_POINT ( 'NONE',  ( 10.57892463485000079, 4.649960478797999563, 5.681084732956000138 ) ) ;
#49241 = CARTESIAN_POINT ( 'NONE',  ( 17.55505043854147118, -3.125000000000000000, -13.52078605991414761 ) ) ;
#49242 = CARTESIAN_POINT ( 'NONE',  ( 11.09256785386839894, 3.167490253789400523, 6.939751505745099358 ) ) ;
#49243 = CARTESIAN_POINT ( 'NONE',  ( 10.12670810574000058, -3.117521507207000386, 8.613544937223998943 ) ) ;
#49244 = CARTESIAN_POINT ( 'NONE',  ( 8.040182825300005831, 3.147885656133000420, 6.175979896252004053 ) ) ;
#49245 = ORIENTED_EDGE ( 'NONE', *, *, #41572, .F. ) ;
#49246 = DIRECTION ( 'NONE',  ( 1.000000000000000000, 5.940303217303999818E-14, -2.897679909401000343E-10 ) ) ;
#49247 = ADVANCED_FACE ( 'NONE', ( #59467 ), #22802, .F. ) ;
#49248 = EDGE_CURVE ( 'NONE', #13653, #36985, #27319, .T. ) ;
#49250 = CARTESIAN_POINT ( 'NONE',  ( 11.20536814679000059, -2.688541832249000230, -8.273932507170000505 ) ) ;
#49249 = CARTESIAN_POINT ( 'NONE',  ( 11.95406170795600076, -11.84685177148000079, 3.896686237526999719 ) ) ;
#49251 = CARTESIAN_POINT ( 'NONE',  ( 7.762804160121919317, -5.211073624054318287, 8.750271362508501127 ) ) ;
#49252 = CARTESIAN_POINT ( 'NONE',  ( 9.215289122285998502, -4.861979632688999686, 8.938813901364000003 ) ) ;
#49253 = CARTESIAN_POINT ( 'NONE',  ( 11.59456039236534330, -2.685288321999000249, -7.563984187103470092 ) ) ;
#49254 = ORIENTED_EDGE ( 'NONE', *, *, #37583, .F. ) ;
#49255 = DIRECTION ( 'NONE',  ( -1.000000000000000000, 0.000000000000000000, 0.000000000000000000 ) ) ;
#49256 = EDGE_CURVE ( 'NONE', #7350, #45182, #5236, .T. ) ;
#49257 = CARTESIAN_POINT ( 'NONE',  ( 11.80579707368350029, -4.634832087857400751, 8.609190966793999422 ) ) ;
#49258 = CARTESIAN_POINT ( 'NONE',  ( 17.74540238977778728, 1.811773551572771757, 13.88227535917423339 ) ) ;
#49259 = CARTESIAN_POINT ( 'NONE',  ( 10.12841772631199966, 4.490588993294299947, 6.490165927606000196 ) ) ;
#49260 = VERTEX_POINT ( 'NONE', #27671 ) ;
#49261 = CARTESIAN_POINT ( 'NONE',  ( 9.559179719593000613, 4.038835765825999680, -5.935509327774999733 ) ) ;
#49262 = CARTESIAN_POINT ( 'NONE',  ( 23.66588327052700080, 13.24635834669000012, -3.906781946131000716 ) ) ;
#49263 = CARTESIAN_POINT ( 'NONE',  ( 12.31158149911128596, 3.007516552431691359, -12.23580242208396562 ) ) ;
#49264 = CARTESIAN_POINT ( 'NONE',  ( 11.77234208742519961, -4.554746427620499638, 6.627995351445298944 ) ) ;
#49265 = ORIENTED_EDGE ( 'NONE', *, *, #31405, .F. ) ;
#49266 = CARTESIAN_POINT ( 'NONE',  ( 7.975798314879130935, 5.079350072276184846, -6.595737603274040239 ) ) ;
#49267 = CARTESIAN_POINT ( 'NONE',  ( 27.64127793187000037, -4.599999999999999645, 8.890528821780000257 ) ) ;
#49268 = ORIENTED_EDGE ( 'NONE', *, *, #29423, .F. ) ;
#49269 = CARTESIAN_POINT ( 'NONE',  ( 24.35365242081700288, 11.54878985765998500, 2.979915831562000239 ) ) ;
#49270 = CARTESIAN_POINT ( 'NONE',  ( 9.343930206849998754, -5.250000000000000000, -7.500000000000000000 ) ) ;
#49271 = VERTEX_POINT ( 'NONE', #65045 ) ;
#49272 = CARTESIAN_POINT ( 'NONE',  ( 9.953700334934390881, -4.258430994261761526, -9.268957274791640444 ) ) ;
#49273 = EDGE_CURVE ( 'NONE', #13267, #46704, #11918, .T. ) ;
#49274 = CARTESIAN_POINT ( 'NONE',  ( 11.16641369783139837, 3.949373449607799902, 6.497808498716000081 ) ) ;
#49275 = CARTESIAN_POINT ( 'NONE',  ( 10.11549555961999936, -2.489199523559999960, -6.434642413229999747 ) ) ;
#49276 = CARTESIAN_POINT ( 'NONE',  ( 11.07336716268999943, 2.375546981533999791, -8.393546861057000541 ) ) ;
#49277 = CARTESIAN_POINT ( 'NONE',  ( 8.523148997455999520, 5.167567567567999731, -6.822293592207000934 ) ) ;
#49278 = CARTESIAN_POINT ( 'NONE',  ( 10.52324012719000024, -3.325647021086999722, 5.689999163383999026 ) ) ;
#49279 = CARTESIAN_POINT ( 'NONE',  ( 13.64647714749800045, 9.589793698018000967, 7.972185502806999224 ) ) ;
#49280 = CARTESIAN_POINT ( 'NONE',  ( 18.17477462772146524, 0.08167875237853183812, -12.69965198491187230 ) ) ;
#49281 = AXIS2_PLACEMENT_3D ( 'NONE', #48781, #38282, #11707 ) ;
#49282 = CARTESIAN_POINT ( 'NONE',  ( 12.17997668546742318, 2.480562828885295446, -12.45612489592983074 ) ) ;
#49283 = CARTESIAN_POINT ( 'NONE',  ( 10.66995391537419913, -3.056324258617099776, -8.140910455049299443 ) ) ;
#49284 = CARTESIAN_POINT ( 'NONE',  ( 9.123551658772999673, 5.558938731259999599, 6.272977177425000050 ) ) ;
#49285 = VERTEX_POINT ( 'NONE', #17160 ) ;
#49286 = CARTESIAN_POINT ( 'NONE',  ( 10.34286678428570383, 2.713835889960351633, -7.027064066396564890 ) ) ;
#49287 = CARTESIAN_POINT ( 'NONE',  ( 7.256896516720705570, 2.725911303287724685, 6.976330978549669659 ) ) ;
#49288 = CARTESIAN_POINT ( 'NONE',  ( 11.26490954471000094, 12.17992731521000138, 1.606774076355000025 ) ) ;
#49289 = CARTESIAN_POINT ( 'NONE',  ( 18.06139486453144372, 2.995281757671052425, 12.23880324656448693 ) ) ;
#49290 = CLOSED_SHELL ( 'NONE', ( #2301, #23208, #37669, #24746, #38196, #9393 ) ) ;
#49291 = DIRECTION ( 'NONE',  ( -1.000000000000000000, -0.000000000000000000, -0.000000000000000000 ) ) ;
#49292 = CARTESIAN_POINT ( 'NONE',  ( 10.89874804681000064, 2.834828962328999502, 9.088465460431999432 ) ) ;
#49293 = CARTESIAN_POINT ( 'NONE',  ( 10.78877584378239973, -3.533998264153197955, 6.763172759027205494 ) ) ;
#49294 = CARTESIAN_POINT ( 'NONE',  ( 12.35923484894303748, 0.5750310236204370096, -12.58704914195723568 ) ) ;
#49295 = ORIENTED_EDGE ( 'NONE', *, *, #49256, .T. ) ;
#49296 = CARTESIAN_POINT ( 'NONE',  ( 12.21409778435358184, -2.897922531322536077, 12.26223633105722222 ) ) ;
#49297 = CARTESIAN_POINT ( 'NONE',  ( 9.733013376692998264, -5.017903082085999777, -6.982691809975100306 ) ) ;
#49298 = CARTESIAN_POINT ( 'NONE',  ( 24.31006797060300073, -3.215953369236999926, -12.14991815011999954 ) ) ;
#49299 = LINE ( 'NONE', #22728, #54409 ) ;
#49300 = B_SPLINE_CURVE_WITH_KNOTS ( 'NONE', 3,
 ( #43348, #64649, #15402, #58046 ),
 .UNSPECIFIED., .F., .F.,
 ( 4, 4 ),
 ( 0.000000000000000000, 0.1254120260046326096 ),
 .UNSPECIFIED. ) ;
#49301 = CARTESIAN_POINT ( 'NONE',  ( 10.47718582084299932, 3.343463760027599818, -6.741111985563299491 ) ) ;
#49302 = CARTESIAN_POINT ( 'NONE',  ( 12.14435919815819176, -0.2964030593063875507, 12.59651778044212378 ) ) ;
#49303 = EDGE_CURVE ( 'NONE', #29214, #57373, #34990, .T. ) ;
#49304 = EDGE_CURVE ( 'NONE', #13153, #62671, #30095, .T. ) ;
#49305 = CARTESIAN_POINT ( 'NONE',  ( 7.571670280409000142, 2.531201476950000195, 8.216704145297999418 ) ) ;
#49306 = CARTESIAN_POINT ( 'NONE',  ( 10.46432998405999903, 2.042755206296999582, 7.723699495214000343 ) ) ;
#49307 = CARTESIAN_POINT ( 'NONE',  ( 12.60240816447940837, 3.091259750208972701, 12.29394167103376390 ) ) ;
#49308 = ORIENTED_EDGE ( 'NONE', *, *, #1590, .T. ) ;
#49309 = CARTESIAN_POINT ( 'NONE',  ( 18.40806533024301572, -3.252985697207277038, -12.09525697359445218 ) ) ;
#49310 = CARTESIAN_POINT ( 'NONE',  ( 10.47303166480599934, 2.862083839376000416, -7.580230465881790280 ) ) ;
#49311 = CARTESIAN_POINT ( 'NONE',  ( 9.549696181504543802, 3.998651493754435737, 8.867000060670969575 ) ) ;
#49313 = CARTESIAN_POINT ( 'NONE',  ( 24.81043930399565056, 11.68078854696337920, 3.195146919645313943 ) ) ;
#49312 = LINE ( 'NONE', #65033, #24083 ) ;
#49314 = CARTESIAN_POINT ( 'NONE',  ( 11.83518044953559922, -3.231951024059400268, -7.900497508315099893 ) ) ;
#49315 = FACE_OUTER_BOUND ( 'NONE', #21295, .T. ) ;
#49316 = ORIENTED_EDGE ( 'NONE', *, *, #24784, .F. ) ;
#49317 = CARTESIAN_POINT ( 'NONE',  ( 0.8874568971869000178, 2.877489654231000227, -1.904074875451999826 ) ) ;
#49318 = CARTESIAN_POINT ( 'NONE',  ( 24.07541249139060824, -9.249162196257124435, -9.196989795079192120 ) ) ;
#49319 = CARTESIAN_POINT ( 'NONE',  ( 17.92027680870444328, -0.6284010951786941357, -12.58437167746846264 ) ) ;
#49320 = CARTESIAN_POINT ( 'NONE',  ( 18.00351343197331389, 3.053300080854057796, -12.22464702761365807 ) ) ;
#49321 = CARTESIAN_POINT ( 'NONE',  ( 24.54687940532700097, -12.52318695592999909, 3.000795290450999797 ) ) ;
#49322 = CARTESIAN_POINT ( 'NONE',  ( 12.15287239299860289, -2.198919866763854092, 13.82623858331039912 ) ) ;
#49323 = CARTESIAN_POINT ( 'NONE',  ( 3.500000000000000000, 0.000000000000000000, 0.000000000000000000 ) ) ;
#49324 = CARTESIAN_POINT ( 'NONE',  ( 24.51193165880900082, 3.518222998965000237, -12.24296030234999932 ) ) ;
#49325 = CARTESIAN_POINT ( 'NONE',  ( 7.933148997457998952, 5.167567567567999731, 6.822293592207000934 ) ) ;
#49326 = ORIENTED_EDGE ( 'NONE', *, *, #61644, .T. ) ;
#49327 = CARTESIAN_POINT ( 'NONE',  ( 6.649999999999999467, 5.221516520829000640, -8.074802043613001246 ) ) ;
#49328 = CYLINDRICAL_SURFACE ( 'NONE', #24823, 0.6250000000000005551 ) ;
#49329 = FACE_OUTER_BOUND ( 'NONE', #16064, .T. ) ;
#49330 = CIRCLE ( 'NONE', #67197, 10.55000000000000426 ) ;
#49331 = CARTESIAN_POINT ( 'NONE',  ( 10.49646369190720030, 5.100000000000000533, -6.665341197380429961 ) ) ;
#49332 = CARTESIAN_POINT ( 'NONE',  ( 0.7037915396055000050, -2.255103325128000158, 3.007138987545999953 ) ) ;
#49333 = PLANE ( 'NONE',  #26594 ) ;
#49334 = EDGE_CURVE ( 'NONE', #68619, #93, #24142, .T. ) ;
#49335 = CARTESIAN_POINT ( 'NONE',  ( 17.60000001072100062, -11.41073498373000028, 4.623967591968000335 ) ) ;
#49336 = FACE_OUTER_BOUND ( 'NONE', #42980, .T. ) ;
#49337 = CARTESIAN_POINT ( 'NONE',  ( 11.41672066707849886, 4.741156262620799922, 7.948314604624900248 ) ) ;
#49338 = VECTOR ( 'NONE', #1995, 1000.000000000000114 ) ;
#49339 = DIRECTION ( 'NONE',  ( -1.000000000000000000, 0.000000000000000000, 0.000000000000000000 ) ) ;
#49340 = CARTESIAN_POINT ( 'NONE',  ( 9.991527686541001430, -4.805948463426999773, -8.932428271061001013 ) ) ;
#49341 = CARTESIAN_POINT ( 'NONE',  ( 8.893204545428000429, -4.599999999999999645, -6.188268997401999982 ) ) ;
#49342 = CARTESIAN_POINT ( 'NONE',  ( 4.599999999999999645, -3.199751711897561801, 12.18694338143115452 ) ) ;
#49343 = DIRECTION ( 'NONE',  ( 0.000000000000000000, -1.000000000000000000, 0.000000000000000000 ) ) ;
#49344 = ORIENTED_EDGE ( 'NONE', *, *, #979, .F. ) ;
#49345 = CARTESIAN_POINT ( 'NONE',  ( 8.646410841231000788, 2.261390688294000029, -6.733978371730000134 ) ) ;
#49346 = EDGE_LOOP ( 'NONE', ( #10572, #56821, #41329, #54320 ) ) ;
#49347 = CARTESIAN_POINT ( 'NONE',  ( 18.08663229464172773, -2.829323725363763753, 13.59808899811969773 ) ) ;
#49348 = CARTESIAN_POINT ( 'NONE',  ( 10.76426088462129904, -3.997280690308189666, -6.221990224628999755 ) ) ;
#49349 = ORIENTED_EDGE ( 'NONE', *, *, #59134, .F. ) ;
#49350 = CARTESIAN_POINT ( 'NONE',  ( 10.76857802013509868, 2.825431102905000103, 7.527343341769989316 ) ) ;
#49351 = CARTESIAN_POINT ( 'NONE',  ( 6.617053846953221630, 1.009847974094061351, 0.5132427797214026421 ) ) ;
#49352 = EDGE_CURVE ( 'NONE', #2919, #11428, #44791, .T. ) ;
#49353 = CARTESIAN_POINT ( 'NONE',  ( 10.31905590579000176, -2.899999999999999911, -6.571291218949999902 ) ) ;
#49354 = CARTESIAN_POINT ( 'NONE',  ( 9.409314688805999083, 2.634692233435000031, 8.920311306029999443 ) ) ;
#49355 = CARTESIAN_POINT ( 'NONE',  ( 24.44496412535000118, -8.810486166165000910, -8.810507954003998776 ) ) ;
#49356 = CARTESIAN_POINT ( 'NONE',  ( 9.685596873515667227, -2.907767014557174790, -6.870476274536379435 ) ) ;
#49357 = CARTESIAN_POINT ( 'NONE',  ( 17.88638781139529144, 0.6398865404514834099, -12.58374251866278648 ) ) ;
#49358 = CARTESIAN_POINT ( 'NONE',  ( 10.86493091395000121, -4.678465004315999209, -9.048463592221999363 ) ) ;
#49359 = B_SPLINE_CURVE_WITH_KNOTS ( 'NONE', 3,
 ( #63771, #64111, #26038, #41429, #21137, #68672, #47713, #10637, #4356, #16226, #15882, #46683, #37214, #68323, #52951, #62738, #58194, #53294 ),
 .UNSPECIFIED., .F., .F.,
 ( 4, 2, 2, 2, 2, 2, 2, 2, 4 ),
 ( 0.000000000000000000, 0.1250000000000000278, 0.2500000000000000000, 0.3749999999999999445, 0.4999999999999999445, 0.6249999999999998890, 0.7499999999999998890, 0.8750000000000000000, 1.000000000000000000 ),
 .UNSPECIFIED. ) ;
#49360 = CARTESIAN_POINT ( 'NONE',  ( 11.10000000044000146, -0.5000000004447999746, 9.662944680343001025 ) ) ;
#49361 = ORIENTED_EDGE ( 'NONE', *, *, #49797, .F. ) ;
#49362 = FACE_OUTER_BOUND ( 'NONE', #41549, .T. ) ;
#49363 = VERTEX_POINT ( 'NONE', #51058 ) ;
#49364 = B_SPLINE_CURVE_WITH_KNOTS ( 'NONE', 3,
 ( #30681, #29319, #24404, #24058 ),
 .UNSPECIFIED., .F., .F.,
 ( 4, 4 ),
 ( 0.000000000000000000, 0.8163836489557121379 ),
 .UNSPECIFIED. ) ;
#49365 = CARTESIAN_POINT ( 'NONE',  ( 8.916525748329496182, 3.463676007238745136, -6.567753456898077324 ) ) ;
#49366 = CIRCLE ( 'NONE', #2464, 12.50000000000000000 ) ;
#49367 = ORIENTED_EDGE ( 'NONE', *, *, #23853, .T. ) ;
#49368 = CARTESIAN_POINT ( 'NONE',  ( 24.53428985367600390, -3.614319203926000146, 12.31267510079000083 ) ) ;
#49369 = CARTESIAN_POINT ( 'NONE',  ( 10.52606775832647656, 3.656473597603909553, 8.303790528164435969 ) ) ;
#49370 = DIRECTION ( 'NONE',  ( 0.000000000000000000, 1.000000000000000000, 0.000000000000000000 ) ) ;
#49371 = CARTESIAN_POINT ( 'NONE',  ( 12.28917444793833269, 2.147008681356603610, 13.74197010666757635 ) ) ;
#49372 = CARTESIAN_POINT ( 'NONE',  ( 17.66882634972352761, -1.885356762137523345, 12.57375482825836421 ) ) ;
#49373 = CARTESIAN_POINT ( 'NONE',  ( 13.99999999485600277, -9.471999751521998689, -8.194948195317001804 ) ) ;
#49374 = CARTESIAN_POINT ( 'NONE',  ( 12.18407604397246580, -0.07155107330948952404, 13.89975717292031376 ) ) ;
#49375 = ORIENTED_EDGE ( 'NONE', *, *, #10664, .T. ) ;
#49376 = CARTESIAN_POINT ( 'NONE',  ( 7.488771682458000178, 4.037115771921000018, -6.023232697733999608 ) ) ;
#49377 = DIRECTION ( 'NONE',  ( 0.000000000000000000, -0.9553735099700839672, -0.2954005017724949389 ) ) ;
#49378 = CARTESIAN_POINT ( 'NONE',  ( 9.657495633957626779, 3.225830943932614048, 7.092330352431370777 ) ) ;
#49379 = CARTESIAN_POINT ( 'NONE',  ( 4.712147656733999490, -0.01772054397006999835, 1.186896354132999987 ) ) ;
#49380 = CIRCLE ( 'NONE', #32624, 1.700000201121000032 ) ;
#49381 = CARTESIAN_POINT ( 'NONE',  ( 9.336654719594999818, 5.095038542659000136, -6.157541456184000062 ) ) ;
#49382 = CARTESIAN_POINT ( 'NONE',  ( 11.09999999999999964, -4.000000000000000000, 7.500000000000000000 ) ) ;
#49383 = TOROIDAL_SURFACE ( 'NONE', #21429, 12.35000000006999876, 0.5000000000000000000 ) ;
#49384 = CARTESIAN_POINT ( 'NONE',  ( 10.47211906628000122, -2.640759929160000130, -8.505246563374999624 ) ) ;
#49385 = EDGE_CURVE ( 'NONE', #40403, #29347, #29754, .T. ) ;
#49386 = EDGE_CURVE ( 'NONE', #21433, #37252, #51399, .T. ) ;
#49387 = CARTESIAN_POINT ( 'NONE',  ( 7.883148997456999929, -5.167567567567999731, 6.822293592207000934 ) ) ;
#49388 = CARTESIAN_POINT ( 'NONE',  ( 8.296466976089000411, -2.897909218876999926, 6.617342437405000055 ) ) ;
#49389 = CARTESIAN_POINT ( 'NONE',  ( 5.000000000000000000, -1.352284263959000032, 11.01731942304999912 ) ) ;
#49390 = LINE ( 'NONE', #22821, #5064 ) ;
#49391 = EDGE_CURVE ( 'NONE', #49620, #50564, #62801, .T. ) ;
#49392 = EDGE_CURVE ( 'NONE', #56588, #25932, #49439, .T. ) ;
#49393 = CARTESIAN_POINT ( 'NONE',  ( 11.79999999550100220, 11.52577121388000059, 1.696750555870000010 ) ) ;
#49394 = CARTESIAN_POINT ( 'NONE',  ( 12.07990771228651461, -0.1878083608152754658, 12.60000737103648660 ) ) ;
#49395 = CARTESIAN_POINT ( 'NONE',  ( 10.56591429142999949, 4.019686495353769651, -6.466681092390999197 ) ) ;
#49396 = CARTESIAN_POINT ( 'NONE',  ( 9.128076168957999670, 3.490299597736799875, -8.365475476407400635 ) ) ;
#49398 = CARTESIAN_POINT ( 'NONE',  ( 10.90000000000000036, -8.263403946409999534, -6.953859016290999229 ) ) ;
#49397 = CARTESIAN_POINT ( 'NONE',  ( 10.00102593514599825, -4.125890936441000356, 8.357822485499299958 ) ) ;
#49399 = CARTESIAN_POINT ( 'NONE',  ( 7.744301850232000461, 3.130385018321999890, 6.467396599055999395 ) ) ;
#49400 = VERTEX_POINT ( 'NONE', #8411 ) ;
#49401 = CARTESIAN_POINT ( 'NONE',  ( 11.18412378248529926, 3.450971646934100079, 8.538714411016998795 ) ) ;
#49402 = CARTESIAN_POINT ( 'NONE',  ( 9.629020610622001541, -5.794331084664000819, 7.414872097535999629 ) ) ;
#49403 = CARTESIAN_POINT ( 'NONE',  ( 9.960975701332998256, 4.837683410033799980, 6.724099908144899551 ) ) ;
#49404 = CARTESIAN_POINT ( 'NONE',  ( 9.556179045228626379, 3.383234358265068575, -6.879409626165266189 ) ) ;
#49405 = CARTESIAN_POINT ( 'NONE',  ( 10.25462442569999943, -2.860634389522000109, 6.604605425112000994 ) ) ;
#49406 = CARTESIAN_POINT ( 'NONE',  ( 10.81499708368641954, 2.650004840405624673, -7.499999822193707644 ) ) ;
#49407 = CARTESIAN_POINT ( 'NONE',  ( 11.75744248190100016, 3.642994321184000128, -12.02392698342999999 ) ) ;
#49408 = ORIENTED_EDGE ( 'NONE', *, *, #4656, .F. ) ;
#49409 = APPLICATION_CONTEXT ( 'automotive_design' ) ;
#49410 = CARTESIAN_POINT ( 'NONE',  ( 9.508013376692998619, -4.895413217368500547, -7.044942343771899651 ) ) ;
#49411 = AXIS2_PLACEMENT_3D ( 'NONE', #1944, #44607, #65900 ) ;
#49412 = CARTESIAN_POINT ( 'NONE',  ( 10.98768472639999949, 2.860900986606000007, -4.945212061661000469 ) ) ;
#49413 = CARTESIAN_POINT ( 'NONE',  ( 5.923521586833000896, 0.9584732047324999726, 1.299486219972000089 ) ) ;
#49414 = CARTESIAN_POINT ( 'NONE',  ( 9.573148997458000409, -5.167567567567999731, -6.822293592207000934 ) ) ;
#49415 = DIRECTION ( 'NONE',  ( -1.000000000000000000, 0.000000000000000000, 0.000000000000000000 ) ) ;
#49416 = CARTESIAN_POINT ( 'NONE',  ( 11.96595122972050085, -3.656201404350900130, 8.295047870239098842 ) ) ;
#49417 = CARTESIAN_POINT ( 'NONE',  ( 10.38287885159599888, 4.860099138268600072, -7.397393329751199786 ) ) ;
#49418 = CARTESIAN_POINT ( 'NONE',  ( 12.20071655345841677, 2.340273578635414076, -13.70604138522239523 ) ) ;
#49419 = CARTESIAN_POINT ( 'NONE',  ( 25.25777540049900338, -8.562684835218000501, 7.910837537672998465 ) ) ;
#49420 = ORIENTED_EDGE ( 'NONE', *, *, #68552, .F. ) ;
#49421 = CARTESIAN_POINT ( 'NONE',  ( 25.47112424053799984, -11.11940461786000078, -3.299559200952000282 ) ) ;
#49422 = CARTESIAN_POINT ( 'NONE',  ( 12.68599131528412371, -0.7206971133477613201, -13.98143832535762776 ) ) ;
#49423 = CARTESIAN_POINT ( 'NONE',  ( 13.94806348789000161, -8.812672976752997656, -7.562028778248000016 ) ) ;
#49424 = CARTESIAN_POINT ( 'NONE',  ( 2.304719994299625707, -2.744941749261882169, -2.197574953528184771 ) ) ;
#49425 = DIRECTION ( 'NONE',  ( 0.000000000000000000, 0.000000000000000000, -1.000000000000000000 ) ) ;
#49426 = DIRECTION ( 'NONE',  ( 1.000000000000000000, 0.000000000000000000, 0.000000000000000000 ) ) ;
#49428 = AXIS2_PLACEMENT_3D ( 'NONE', #62583, #15041, #36721 ) ;
#49427 = DIRECTION ( 'NONE',  ( -1.000000000000000000, 0.000000000000000000, 1.665334536957000056E-14 ) ) ;
#49429 = VERTEX_POINT ( 'NONE', #66790 ) ;
#49430 = CARTESIAN_POINT ( 'NONE',  ( 10.84999882987999875, 0.000000000000000000, 0.000000000000000000 ) ) ;
#49431 = CARTESIAN_POINT ( 'NONE',  ( 17.63746348810182951, 1.880115813469444230, -13.78555441649718460 ) ) ;
#49432 = ORIENTED_EDGE ( 'NONE', *, *, #66052, .T. ) ;
#49433 = CARTESIAN_POINT ( 'NONE',  ( 10.47094409420000005, -5.100000000000000533, 6.571291218949999902 ) ) ;
#49434 = CARTESIAN_POINT ( 'NONE',  ( 2.790556799211291406, -3.500000000000002220, 0.4581489286484968781 ) ) ;
#49435 = EDGE_CURVE ( 'NONE', #10933, #8116, #35322, .T. ) ;
#49436 = CARTESIAN_POINT ( 'NONE',  ( 15.36427412810700055, 8.819457004710999470, 7.692809699200999773 ) ) ;
#49437 = CARTESIAN_POINT ( 'NONE',  ( 11.09999999999999964, -2.274006712557999688, -7.281956340829000673 ) ) ;
#49438 = CARTESIAN_POINT ( 'NONE',  ( 10.59725056272499977, -2.683866746800999792, -7.519505747156228992 ) ) ;
#49439 = B_SPLINE_CURVE_WITH_KNOTS ( 'NONE', 3,
 ( #66094, #61888, #18904, #50027 ),
 .UNSPECIFIED., .F., .F.,
 ( 4, 4 ),
 ( 0.000000000000000000, 1.000000000000000000 ),
 .UNSPECIFIED. ) ;
#49440 = CARTESIAN_POINT ( 'NONE',  ( 9.323795176894432046, -5.066048497541554063, -6.242748793373607441 ) ) ;
#49441 = EDGE_CURVE ( 'NONE', #24902, #49079, #17445, .T. ) ;
#49442 = CARTESIAN_POINT ( 'NONE',  ( 18.30003129334700063, 2.732683817159999862, -11.53064095410000078 ) ) ;
#49443 = PLANE ( 'NONE',  #56336 ) ;
#49444 = ORIENTED_EDGE ( 'NONE', *, *, #38934, .T. ) ;
#49445 = CARTESIAN_POINT ( 'NONE',  ( 8.861802827888666911, 2.874603711572078613, -6.749639981085472584 ) ) ;
#49446 = CARTESIAN_POINT ( 'NONE',  ( 18.11601457983865515, -2.775767521436611318, -13.61104273374189511 ) ) ;
#49447 = CARTESIAN_POINT ( 'NONE',  ( 9.942214158770999788, 3.986577607995999806, -9.280166295424001177 ) ) ;
#49448 = ORIENTED_EDGE ( 'NONE', *, *, #11731, .T. ) ;
#49449 = CARTESIAN_POINT ( 'NONE',  ( 10.42081182385000027, 2.488452444780999695, -7.717895019962999648 ) ) ;
#49450 = FACE_OUTER_BOUND ( 'NONE', #8711, .T. ) ;
#49451 = ORIENTED_EDGE ( 'NONE', *, *, #353, .F. ) ;
#49452 = CARTESIAN_POINT ( 'NONE',  ( 9.837292290062999101, 4.868609929059700470, 8.004340253666999416 ) ) ;
#49453 = CARTESIAN_POINT ( 'NONE',  ( 18.07822721942930855, -2.978550302103504688, -12.24288824562991174 ) ) ;
#49454 = CARTESIAN_POINT ( 'NONE',  ( 9.539763540182331525, 4.327184855449099921, 6.282534154164603812 ) ) ;
#49455 = CARTESIAN_POINT ( 'NONE',  ( 8.433536308088498856, 2.899999999999999911, -6.665341197412902652 ) ) ;
#49456 = CARTESIAN_POINT ( 'NONE',  ( 11.80432898647400108, -11.49396319796999855, -1.654000935039000142 ) ) ;
#49457 = CARTESIAN_POINT ( 'NONE',  ( 8.902126402770997871, 4.811247217215600003, 7.805918119494599239 ) ) ;
#49458 = CARTESIAN_POINT ( 'NONE',  ( 7.600000000000000533, 0.000000000000000000, 0.000000000000000000 ) ) ;
#49459 = ORIENTED_EDGE ( 'NONE', *, *, #20825, .F. ) ;
#49460 = CARTESIAN_POINT ( 'NONE',  ( 10.96876099447000108, 2.333339469804000199, 6.524055942683999021 ) ) ;
#49461 = CARTESIAN_POINT ( 'NONE',  ( 10.05462971959000029, 3.531217403581000003, -9.119235467071000301 ) ) ;
#49462 = CARTESIAN_POINT ( 'NONE',  ( 13.49994651945300284, 12.07042783918999795, 2.492331243371999960 ) ) ;
#49463 = CARTESIAN_POINT ( 'NONE',  ( 12.34743845434965159, 2.926178772989069365, -13.57378949252271028 ) ) ;
#49464 = AXIS2_PLACEMENT_3D ( 'NONE', #48282, #39175, #17507 ) ;
#49465 = B_SPLINE_CURVE_WITH_KNOTS ( 'NONE', 3,
 ( #40751, #62415, #62074, #14190 ),
 .UNSPECIFIED., .F., .F.,
 ( 4, 4 ),
 ( 0.000000000000000000, 1.000000000000000000 ),
 .UNSPECIFIED. ) ;
#49466 = FACE_OUTER_BOUND ( 'NONE', #61004, .T. ) ;
#49467 = CARTESIAN_POINT ( 'NONE',  ( 24.63407876950900288, 3.094019437545999729, 11.81700057174999863 ) ) ;
#49468 = CARTESIAN_POINT ( 'NONE',  ( 18.02507847443574818, 0.4124479947379854905, 13.89177559470776302 ) ) ;
#49469 = CARTESIAN_POINT ( 'NONE',  ( 24.85113725905400273, -3.384275653315000021, 11.84838802887999876 ) ) ;
#49470 = ORIENTED_EDGE ( 'NONE', *, *, #39979, .F. ) ;
#49471 = EDGE_LOOP ( 'NONE', ( #4945, #56728, #67634, #20033 ) ) ;
#49472 = CARTESIAN_POINT ( 'NONE',  ( 9.336654719594999818, 5.095038542659000136, -6.157541456184000062 ) ) ;
#49473 = CARTESIAN_POINT ( 'NONE',  ( 12.31508838531384420, -0.3880332713699820024, 13.89271023030023500 ) ) ;
#49474 = ADVANCED_FACE ( 'NONE', ( #61545, #2134, #56305, #23454 ), #24831, .F. ) ;
#49475 = CARTESIAN_POINT ( 'NONE',  ( 12.49453886781196310, -0.5425156946746918507, -13.88574935928999921 ) ) ;
#49476 = EDGE_CURVE ( 'NONE', #3659, #64075, #36065, .T. ) ;
#49477 = CARTESIAN_POINT ( 'NONE',  ( 10.62698276521000196, -3.142914536759000121, 8.668455626664998803 ) ) ;
#49478 = CARTESIAN_POINT ( 'NONE',  ( 9.228231092913778966, -5.653336912713888829, 8.124910183455536838 ) ) ;
#49479 = CARTESIAN_POINT ( 'NONE',  ( 8.898558059623999483, -5.146736128384000075, 6.597417125647000447 ) ) ;
#49480 = DIRECTION ( 'NONE',  ( 0.000000000000000000, 0.8350135785638144181, -0.5502293372895092904 ) ) ;
#49482 = DIRECTION ( 'NONE',  ( -1.000000000000000000, 0.000000000000000000, 3.552713678810000077E-14 ) ) ;
#49481 = CARTESIAN_POINT ( 'NONE',  ( 10.20969678796400082, -3.780328739572700325, 8.760209873321999297 ) ) ;
#49483 = CIRCLE ( 'NONE', #40552, 2.200000000000001954 ) ;
#49484 = CARTESIAN_POINT ( 'NONE',  ( 8.974845122786007323, -5.117933181718998803, -6.719699903140006647 ) ) ;
#49485 = CARTESIAN_POINT ( 'NONE',  ( 12.09999999999999964, -3.674136214561153135, 6.377063228063083677 ) ) ;
#49486 = AXIS2_PLACEMENT_3D ( 'NONE', #31252, #52561, #4658 ) ;
#49487 = CARTESIAN_POINT ( 'NONE',  ( 8.867797255587998251, 4.866234952405400271, -7.463326341748410364 ) ) ;
#49488 = CARTESIAN_POINT ( 'NONE',  ( 18.03207563512528111, 0.4039503557775008247, 12.69135589213615667 ) ) ;
#49489 = CARTESIAN_POINT ( 'NONE',  ( 8.379867906070000316, -2.923743482135000349, 6.439439799216000182 ) ) ;
#49490 = CARTESIAN_POINT ( 'NONE',  ( 18.14478511901992874, -2.707036753431580678, -12.40091620384611026 ) ) ;
#49491 = VERTEX_POINT ( 'NONE', #29061 ) ;
#49493 = CARTESIAN_POINT ( 'NONE',  ( 11.04298866606778162, 3.494581883632823516, 8.213191510014491215 ) ) ;
#49492 = CARTESIAN_POINT ( 'NONE',  ( 9.187745559622999991, -5.964711531933999389, 7.776478361891000723 ) ) ;
#49494 = CARTESIAN_POINT ( 'NONE',  ( 9.102795280413999990, 3.071719032003000116, -6.037263251225000182 ) ) ;
#49495 =( BOUNDED_SURFACE ( )  B_SPLINE_SURFACE ( 3, 3, ( 
 ( #51127, #3230, #40626, #61958, #47944, #59111, #10528, #385, #58767 ),
 ( #21364, #37790, #68560, #21701, #63313, #52492, #9842, #44, #10874 ),
 ( #43391, #42361, #11217, #31520, #48279, #4589, #31868, #42694, #64002 ),
 ( #5624, #16120, #32553, #53866, #37446, #48629, #26625, #47602, #43037 ) ),
 .UNSPECIFIED., .F., .F., .F. ) 
 B_SPLINE_SURFACE_WITH_KNOTS ( ( 4, 4 ),
 ( 4, 1, 1, 1, 1, 1, 4 ),
 ( 0.000000000000000000, 1.000000000000000000 ),
 ( -0.004646279661397999423, 0.000000000000000000, 0.03269534097185999855, 0.06255479614191999937, 0.08986301827557000022, 0.1148786485006999952, 0.1376622693536999897 ),
 .UNSPECIFIED. ) 
 GEOMETRIC_REPRESENTATION_ITEM ( )  RATIONAL_B_SPLINE_SURFACE ( (
 ( 1.187699524740999824, 1.187699524740999824, 1.187699524740999824, 1.187699524740999824, 1.187699524740999824, 1.187699524740999824, 1.187699524740999824, 1.187699524740999824, 1.187699524740999824),
 ( 0.9374334917530999789, 0.9374334917530999789, 0.9374334917530999789, 0.9374334917530999789, 0.9374334917530999789, 0.9374334917530999789, 0.9374334917530999789, 0.9374334917530999789, 0.9374334917530999789),
 ( 0.9374334917530999789, 0.9374334917530999789, 0.9374334917530999789, 0.9374334917530999789, 0.9374334917530999789, 0.9374334917530999789, 0.9374334917530999789, 0.9374334917530999789, 0.9374334917530999789),
 ( 1.187699524740999824, 1.187699524740999824, 1.187699524740999824, 1.187699524740999824, 1.187699524740999824, 1.187699524740999824, 1.187699524740999824, 1.187699524740999824, 1.187699524740999824) ) ) 
 REPRESENTATION_ITEM ( '' )  SURFACE ( )  );
#49496 = CARTESIAN_POINT ( 'NONE',  ( 12.80505043854146940, -1.875000000000000000, 13.78631952119025605 ) ) ;
#49497 = EDGE_CURVE ( 'NONE', #13866, #95, #2471, .T. ) ;
#49498 = DIRECTION ( 'NONE',  ( 0.000000000000000000, 0.9516614099929482373, -0.3071490855109836327 ) ) ;
#49499 = CARTESIAN_POINT ( 'NONE',  ( 0.8724295521082999771, 2.537743131474000435, -2.464631551651000230 ) ) ;
#49500 = FACE_OUTER_BOUND ( 'NONE', #7246, .T. ) ;
#49501 = CARTESIAN_POINT ( 'NONE',  ( 2.352109567116000388, -0.7825563863409999987, 3.335029682752000291 ) ) ;
#49502 = ORIENTED_EDGE ( 'NONE', *, *, #60714, .T. ) ;
#49503 = CARTESIAN_POINT ( 'NONE',  ( 12.16275096843966885, 0.3336735144251337659, -12.59558214381612551 ) ) ;
#49504 = CARTESIAN_POINT ( 'NONE',  ( 6.983066481085000277, 12.13287628867999857, -3.076835277494999854 ) ) ;
#49505 = CARTESIAN_POINT ( 'NONE',  ( 24.15442778489675035, -12.45811728158824749, -3.353956205876204688 ) ) ;
#49506 = CARTESIAN_POINT ( 'NONE',  ( 8.668204719592999652, 3.979464555644999901, 9.134076336209998814 ) ) ;
#49507 = VERTEX_POINT ( 'NONE', #66440 ) ;
#49508 = CARTESIAN_POINT ( 'NONE',  ( 6.334973520849000117, 1.541759477651000187, 0.4799094010597000359 ) ) ;
#49509 = CARTESIAN_POINT ( 'NONE',  ( 8.137010841226000935, 5.144639763962000067, -8.301783154141999077 ) ) ;
#49511 = FACE_OUTER_BOUND ( 'NONE', #17704, .T. ) ;
#49510 = DIRECTION ( 'NONE',  ( 0.000000000000000000, 1.000000000000000000, 0.000000000000000000 ) ) ;
#49512 = CARTESIAN_POINT ( 'NONE',  ( 10.69837472757367713, -4.473492782822720670, -8.234774922628410820 ) ) ;
#49513 = ORIENTED_EDGE ( 'NONE', *, *, #54861, .F. ) ;
#49515 = FACE_OUTER_BOUND ( 'NONE', #34557, .T. ) ;
#49514 = CIRCLE ( 'NONE', #23819, 0.5000000000000014433 ) ;
#49516 = CARTESIAN_POINT ( 'NONE',  ( 9.681180837610000367, -2.612237299844000216, 7.804680206899999639 ) ) ;
#49517 = VERTEX_POINT ( 'NONE', #18561 ) ;
#49518 = CARTESIAN_POINT ( 'NONE',  ( 23.60000000000000142, -9.305479840184000651, -8.315530346521999405 ) ) ;
#49519 = CARTESIAN_POINT ( 'NONE',  ( 16.04649313145500145, 3.595593625533999749, 11.13765277391999931 ) ) ;
#49520 = CARTESIAN_POINT ( 'NONE',  ( 18.09636517151066215, -0.3125842563278192210, -13.89527356689842996 ) ) ;
#49521 = ORIENTED_EDGE ( 'NONE', *, *, #25790, .F. ) ;
#49522 = FACE_OUTER_BOUND ( 'NONE', #64493, .T. ) ;
#49523 = LINE ( 'NONE', #7567, #5907 ) ;
#49524 = CARTESIAN_POINT ( 'NONE',  ( 10.86190547754509872, 4.891676932241900033, -7.528299448264639260 ) ) ;
#49525 = ADVANCED_FACE ( 'NONE', ( #34649 ), #55959, .F. ) ;
#49526 = CARTESIAN_POINT ( 'NONE',  ( 8.158337970077000990E-06, 0.000000000000000000, 0.000000000000000000 ) ) ;
#49527 = CARTESIAN_POINT ( 'NONE',  ( 11.50000000000000000, -2.920245322398999921, 7.174999999999999822 ) ) ;
#49528 = ORIENTED_EDGE ( 'NONE', *, *, #58253, .F. ) ;
#49529 = CARTESIAN_POINT ( 'NONE',  ( 10.09999999999999964, 0.000000000000000000, 0.000000000000000000 ) ) ;
#49530 = CARTESIAN_POINT ( 'NONE',  ( 23.85292906093700083, -13.16237798046000051, -3.534274979399000038 ) ) ;
#49531 = CARTESIAN_POINT ( 'NONE',  ( 11.09999999999999964, 2.649999999999999911, 7.500000000000000000 ) ) ;
#49532 = COLOUR_RGB ( '', 0.66274510, 0.83137255, 0.94901961) ;
#49533 = CARTESIAN_POINT ( 'NONE',  ( 15.95309301929700219, -8.865091978629999758, -8.639514276306002216 ) ) ;
#49534 = ORIENTED_EDGE ( 'NONE', *, *, #59257, .F. ) ;
#49535 = CARTESIAN_POINT ( 'NONE',  ( 8.849999778957998942, 4.000000000000000000, -7.500000000000000000 ) ) ;
#49536 = AXIS2_PLACEMENT_3D ( 'NONE', #28747, #65779, #33986 ) ;
#49537 = CARTESIAN_POINT ( 'NONE',  ( 0.3738300074506999970, -3.373808768376999723, -1.182108054635000026E-09 ) ) ;
#49538 = DIRECTION ( 'NONE',  ( -1.000000000000000000, 0.000000000000000000, 0.000000000000000000 ) ) ;
#49539 = CARTESIAN_POINT ( 'NONE',  ( 5.000030787343000327, 2.045306479342562600, 0.5496608443529819032 ) ) ;
#49540 = DIRECTION ( 'NONE',  ( 0.000000000000000000, 1.000000000000000000, 0.000000000000000000 ) ) ;
#49541 = CARTESIAN_POINT ( 'NONE',  ( 10.21462282008599942, -3.476853648246800432, -8.343818446627699004 ) ) ;
#49542 = CARTESIAN_POINT ( 'NONE',  ( 7.150172442432219277, 1.249827089371011279, -0.1627375339325294601 ) ) ;
#49543 = CARTESIAN_POINT ( 'NONE',  ( 18.10394395700119929, -2.009981277211916328, 12.43865165640890069 ) ) ;
#49544 = ORIENTED_EDGE ( 'NONE', *, *, #28498, .F. ) ;
#49545 = CARTESIAN_POINT ( 'NONE',  ( 11.38678751119029897, -5.166297436425000278, -8.110172976325500827 ) ) ;
#49546 = B_SPLINE_CURVE_WITH_KNOTS ( 'NONE', 1,
 ( #9020, #16671 ),
 .UNSPECIFIED., .F., .F.,
 ( 2, 2 ),
 ( 0.000000000000000000, 1.000000000000000000 ),
 .UNSPECIFIED. ) ;
#49547 = EDGE_LOOP ( 'NONE', ( #60357, #58658, #60113, #58160 ) ) ;
#49548 = CARTESIAN_POINT ( 'NONE',  ( 11.25951067610000145, -12.19482939020999979, -1.501993453007000046 ) ) ;
#49549 = CARTESIAN_POINT ( 'NONE',  ( 9.494689158774999527, 2.824732249080000202, -8.992748220058999209 ) ) ;
#49550 = CARTESIAN_POINT ( 'NONE',  ( 3.299581029697000290, 2.884784742943000246, -1.760185852660000050 ) ) ;
#49551 = B_SPLINE_CURVE_WITH_KNOTS ( 'NONE', 3,
 ( #19718, #25646, #41040, #51865 ),
 .UNSPECIFIED., .F., .F.,
 ( 4, 4 ),
 ( 0.000000000000000000, 1.000000000000000000 ),
 .UNSPECIFIED. ) ;
#49552 = CARTESIAN_POINT ( 'NONE',  ( 10.42081395746000005, -2.488448635474999726, -7.717895569088000229 ) ) ;
#49553 = CARTESIAN_POINT ( 'NONE',  ( 6.666460567079824706, -1.086035832535817702, -1.060422689362632731 ) ) ;
#49554 = CARTESIAN_POINT ( 'NONE',  ( 23.83530392115299890, 13.04092488338999978, 3.622230473245000137 ) ) ;
#49555 = B_SPLINE_CURVE_WITH_KNOTS ( 'NONE', 3,
 ( #1998, #24009, #3023, #65954 ),
 .UNSPECIFIED., .F., .F.,
 ( 4, 4 ),
 ( 0.000000000000000000, 1.000000000000000000 ),
 .UNSPECIFIED. ) ;
#49556 = CARTESIAN_POINT ( 'NONE',  ( 11.37077408945317103, 2.816736291912564027, 7.086869749530762874 ) ) ;
#49557 = ORIENTED_EDGE ( 'NONE', *, *, #59360, .F. ) ;
#49558 = CARTESIAN_POINT ( 'NONE',  ( 1.923822673704333575, -0.09607108383954165998, -3.514941141763996413 ) ) ;
#49559 = EDGE_CURVE ( 'NONE', #50475, #1441, #67754, .T. ) ;
#49560 = CARTESIAN_POINT ( 'NONE',  ( 11.05103166480599874, -5.000984463463999496, 7.429424106427209296 ) ) ;
#49561 = CARTESIAN_POINT ( 'NONE',  ( 10.58844943056000076, 3.754657019866000311, 5.545350295858999523 ) ) ;
#49562 = ADVANCED_FACE ( 'NONE', ( #19234 ), #1599, .F. ) ;
#49563 = DIRECTION ( 'NONE',  ( 1.000000000000000000, 0.000000000000000000, 0.000000000000000000 ) ) ;
#49564 = CARTESIAN_POINT ( 'NONE',  ( 5.500000000000000000, -1.300000000000000044, -9.662944685757000940 ) ) ;
#49565 = CARTESIAN_POINT ( 'NONE',  ( 9.218906920141307637, 2.654016165387476089, 7.603667288042461614 ) ) ;
#49566 = AXIS2_PLACEMENT_3D ( 'NONE', #43292, #59362, #990 ) ;
#49567 = CARTESIAN_POINT ( 'NONE',  ( 11.31410538575739899, 4.975963290822400076, -7.266662245194900116 ) ) ;
#49568 = DIRECTION ( 'NONE',  ( 0.000000000000000000, -0.7418296051989918816, -0.6705884258248929752 ) ) ;
#49569 = CARTESIAN_POINT ( 'NONE',  ( 9.378405316141000370, 3.757578743663700038, -8.615780615741000403 ) ) ;
#49570 = CARTESIAN_POINT ( 'NONE',  ( 24.25970375769299991, -8.928473527296000967, -8.811154394041999183 ) ) ;
#49571 = B_SPLINE_CURVE_WITH_KNOTS ( 'NONE', 3,
 ( #56406, #45579, #51496, #14105, #3935, #66885, #52183, #9184, #25272, #4284, #25619, #35430, #57768, #46609, #40661, #3591, #40324, #31221 ),
 .UNSPECIFIED., .F., .F.,
 ( 4, 2, 2, 2, 2, 2, 2, 2, 4 ),
 ( 0.000000000000000000, 0.1250000000000000000, 0.2500000000000000000, 0.3750000000000000000, 0.5000000000000000000, 0.6250000000000000000, 0.7500000000000000000, 0.8750000000000000000, 1.000000000000000000 ),
 .UNSPECIFIED. ) ;
#49572 = CARTESIAN_POINT ( 'NONE',  ( 24.23190313298700360, -9.065335089760999665, 9.162789734983000756 ) ) ;
#49573 = VERTEX_POINT ( 'NONE', #27853 ) ;
#49574 = CARTESIAN_POINT ( 'NONE',  ( 8.822980646795000936, -2.678334737187000325, 8.735278777293000729 ) ) ;
#49575 = CARTESIAN_POINT ( 'NONE',  ( 9.529144223516999190, -2.330665094450000030, -8.349943402163999551 ) ) ;
#49576 = CARTESIAN_POINT ( 'NONE',  ( 17.91230600709723220, 3.012931617833825904, 13.55113455194568495 ) ) ;
#49577 = ADVANCED_FACE ( 'NONE', ( #22242 ), #55203, .T. ) ;
#49578 = CARTESIAN_POINT ( 'NONE',  ( 11.09999999999999964, -2.685305999535000154, 6.664030027596000494 ) ) ;
#49579 = CARTESIAN_POINT ( 'NONE',  ( 10.13662282008599824, -3.405288783432600219, -8.459250300176799797 ) ) ;
#49580 = VERTEX_POINT ( 'NONE', #66107 ) ;
#49581 = CARTESIAN_POINT ( 'NONE',  ( 25.25798305592800119, 2.569270360355000005, -11.37081726145000005 ) ) ;
#49582 = EDGE_CURVE ( 'NONE', #65344, #57358, #30874, .T. ) ;
#49583 = CARTESIAN_POINT ( 'NONE',  ( 8.849385841230999361, 3.975069902178000270, 9.483774112875002160 ) ) ;
#49584 = CIRCLE ( 'NONE', #16097, 1.999999999999999778 ) ;
#49586 = CARTESIAN_POINT ( 'NONE',  ( 0.5647703222817161972, 3.481129241836969701, 0.6274791494510446599 ) ) ;
#49585 = CARTESIAN_POINT ( 'NONE',  ( 8.994485841233000656, 3.854507394315999758, -9.394302886912999639 ) ) ;
#49587 = DIRECTION ( 'NONE',  ( 0.000000000000000000, -1.000000000000000000, 0.000000000000000000 ) ) ;
#49588 = ORIENTED_EDGE ( 'NONE', *, *, #4079, .T. ) ;
#49589 = DIRECTION ( 'NONE',  ( 0.000000000000000000, -1.000000000000000000, -0.000000000000000000 ) ) ;
#49590 = CARTESIAN_POINT ( 'NONE',  ( 18.27399547846089689, -2.614774648920896727, -13.75367307402544270 ) ) ;
#49591 = CARTESIAN_POINT ( 'NONE',  ( 11.56025819896753859, 3.013900664291200293, 7.314099615601099558 ) ) ;
#49592 = CARTESIAN_POINT ( 'NONE',  ( 10.44675369521999997, -2.885048926231000177, 8.863479194807000638 ) ) ;
#49593 = CARTESIAN_POINT ( 'NONE',  ( 7.778861800931997195, 3.520498707107000858, 6.411393241748998051 ) ) ;
#49595 = VERTEX_POINT ( 'NONE', #23466 ) ;
#49594 = CIRCLE ( 'NONE', #11603, 0.7499999936418002555 ) ;
#49596 = CARTESIAN_POINT ( 'NONE',  ( 8.330224159023998709, 2.898680183691999979, -6.607597200868999820 ) ) ;
#49598 = CARTESIAN_POINT ( 'NONE',  ( 10.28180685320999999, -3.991526694881000203, -5.814304247846999729 ) ) ;
#49597 = CARTESIAN_POINT ( 'NONE',  ( 11.95023821374600104, -11.77429045505000005, 4.110796463462000006 ) ) ;
#49599 = CARTESIAN_POINT ( 'NONE',  ( 8.091091889490169109, -4.367519155558725608, 5.800091099343307022 ) ) ;
#49600 = CARTESIAN_POINT ( 'NONE',  ( 11.20904026220999938, -5.937811873294999820, 7.147336919140999001 ) ) ;
#49601 = CARTESIAN_POINT ( 'NONE',  ( 11.03644315172999946, 5.222804237133000349, 5.023246923241000417 ) ) ;
#49602 = CARTESIAN_POINT ( 'NONE',  ( 9.374784697135000400, -3.454948069423500190, 8.343659109631099469 ) ) ;
#49603 = EDGE_LOOP ( 'NONE', ( #7416, #50894, #8662, #571, #6582, #5424, #8624, #19108, #44070, #66122 ) ) ;
#49604 = CARTESIAN_POINT ( 'NONE',  ( 23.79457325321444827, -9.731831237395766721, 9.426946816267429696 ) ) ;
#49605 = CARTESIAN_POINT ( 'NONE',  ( 11.26841504065830080, -3.085489673376300424, 8.181880472491098288 ) ) ;
#49606 = ORIENTED_EDGE ( 'NONE', *, *, #59616, .T. ) ;
#49607 = CARTESIAN_POINT ( 'NONE',  ( 7.453125355210004521, 3.231590054310000237, 6.459270056246999125 ) ) ;
#49608 = ORIENTED_EDGE ( 'NONE', *, *, #38593, .T. ) ;
#49609 = B_SPLINE_SURFACE_WITH_KNOTS ( 'NONE', 1, 3, ( 
 ( #49496, #55786, #3914, #25248, #1606, #22924, #44275, #65573, #17696, #39020, #12444, #7198, #60680, #12795, #7534, #28889, #50198, #23618, #44959, #18384, #25600, #41674, #36778, #4606, #32232, #47270, #42025, #16135, #31201, #68573, #15791, #68927, #397, #48292, #52855, #5298, #26978, #10541, #26640, #47957, #58438, #21714, #53545, #31536, #36429, #20696, #31884, #58100, #57746, #9856, #52506, #4954, #25940, #42373, #63326, #15456, #10203, #62646, #21041, #26290, #47616, #15107, #63676, #55, #62980, #37458, #37122, #53197, #21376, #42709, #10888, #64014, #58780, #5635, #14769, #36086, #57401, #9506, #30848, #52160, #4263, #46927, #68230, #20350, #1784, #64702 ),
 ( #60511, #44101, #12620, #59466, #65400, #33260, #59125, #28015, #43050, #12278, #23100, #17871, #16813, #17519, #6319, #33949, #65044, #11564, #7024, #11229, #38492, #64352, #37804, #17159, #59815, #1437, #39188, #55272, #49322, #16474, #32566, #22752, #7368, #38849, #28359, #33604, #50026, #54923, #48644, #53878, #5978, #27318, #60172, #745, #44451, #28709, #2133, #49675, #22058, #65747, #43406, #38140, #11919, #54221, #32907, #27670, #22406, #48985, #1095, #43749, #54578, #6673, #30426, #9087, #13660, #35332, #56984, #40560, #56646, #29753, #39536, #12975, #29409, #39887, #40907, #67461, #18903, #62229, #61887, #45812, #14346, #61207, #2811, #51736, #46157, #24489 ) ),
 .UNSPECIFIED., .F., .F., .F.,
 ( 2, 2 ),
 ( 4, 2, 2, 2, 2, 2, 2, 2, 2, 2, 2, 2, 2, 2, 2, 2, 2, 2, 2, 2, 2, 2, 2, 2, 2, 2, 2, 2, 2, 2, 2, 2, 2, 2, 2, 2, 2, 2, 2, 2, 2, 2, 4 ),
 ( 0.000000000000000000, 1.000000000000000000 ),
 ( 0.000000000000000000, 7.142430198406411052E-05, 0.0001428486039681282210, 0.0002142729059521923315, 0.0002856972079362564421, 0.0003571215099203205526, 0.0004285458119043846631, 0.0004999701138884487736, 0.0005356822648804808289, 0.0005713944158725128841, 0.0006071065668645449394, 0.0006428187178565769946, 0.0007142430198406411052, 0.0007856673218247052157, 0.0008213794728167372709, 0.0008570916238087693262, 0.0008928037748008013814, 0.0009285159257928334367, 0.0009999402277768975472, 0.001071364529760961658, 0.001142788831745025768, 0.001214213133729089879, 0.001285637435713153989, 0.001321349586705186045, 0.001357061737697218100, 0.001428486039681282210, 0.001499910341665346321, 0.001535622492657378376, 0.001571334643649410431, 0.001607046794641442487, 0.001642758945633474542, 0.001714183247617538652, 0.001785607549601602763, 0.001821319700593634818, 0.001857031851585666873, 0.001928456153569730984, 0.001964168304561763039, 0.001999880455553795094, 0.002035592606545827150, 0.002071304757537859205, 0.002142729059521923315, 0.002214153361505987426, 0.002285577663490051536 ),
 .UNSPECIFIED. ) ;
#49610 = CARTESIAN_POINT ( 'NONE',  ( 9.202245280414000916, 5.095038542659000136, -6.157541456184000062 ) ) ;
#49611 = CARTESIAN_POINT ( 'NONE',  ( 24.03158892672100322, 13.13525790609000055, -3.279774679148000249 ) ) ;
#49612 = CARTESIAN_POINT ( 'NONE',  ( 12.43939714311201428, 3.101706251878831644, -12.21226669259267794 ) ) ;
#49613 = CARTESIAN_POINT ( 'NONE',  ( 11.52301463001509951, -3.452642973349600464, 8.376661845795100092 ) ) ;
#49614 = ORIENTED_EDGE ( 'NONE', *, *, #29564, .F. ) ;
#49615 = CARTESIAN_POINT ( 'NONE',  ( 8.832537864289999874, -2.899999999999999911, 6.571291218949999902 ) ) ;
#49616 = CIRCLE ( 'NONE', #62973, 0.2000000000000004274 ) ;
#49617 = ORIENTED_EDGE ( 'NONE', *, *, #56184, .F. ) ;
#49618 = CARTESIAN_POINT ( 'NONE',  ( 23.89320776801300283, 10.87822567738999346, 3.284864823361000941 ) ) ;
#49619 = CARTESIAN_POINT ( 'NONE',  ( 5.805026506351000037, 1.500000000000000000, 0.000000000000000000 ) ) ;
#49620 = VERTEX_POINT ( 'NONE', #17532 ) ;
#49621 = B_SPLINE_SURFACE_WITH_KNOTS ( 'NONE', 3, 3, ( 
 ( #25230, #51458, #9486, #18962, #56019, #8127, #13386, #3224, #14066, #34708, #40288, #46220, #3556, #45541, #8473, #36066, #35391, #29473, #50782 ),
 ( #61604, #40971, #19650, #23859, #35729, #13722, #67528, #39950, #56715, #50427, #9147, #24552, #2531, #35051, #66501, #56369, #45875, #45195, #18622 ),
 ( #21358, #42687, #63308, #25920, #37784, #53526, #21021, #32211, #53178, #63996, #68905, #31862, #10185, #4932, #47251, #52138, #41656, #10521, #47597 ),
 ( #26618, #58082, #5277, #15773, #26959, #21695, #30828, #43031, #4240, #47938, #10867, #64334, #58417, #25580, #42356, #48273, #31514, #57726, #5616 ) ),
 .UNSPECIFIED., .F., .F., .F.,
 ( 4, 4 ),
 ( 4, 1, 1, 1, 1, 1, 1, 1, 1, 1, 1, 1, 1, 1, 1, 1, 4 ),
 ( -0.1039370721279000015, 1.103937072127999963 ),
 ( 0.5600558712726999566, 0.5880915265348000132, 0.6161271817967999276, 0.6441628370587999530, 0.6721984923209000096, 0.7002341475828999240, 0.7282698028449000605, 0.7563054581070000060, 0.7843411133690000314, 0.8123767686310000569, 0.8404124238931000024, 0.8684480791551000278, 0.8964837344171000533, 0.9245193896790999677, 0.9525550449412000242, 0.9805907002032000497, 1.008626355465000124 ),
 .UNSPECIFIED. ) ;
#49622 = CARTESIAN_POINT ( 'NONE',  ( 12.60431942020951546, -3.171686099353038024, -12.19427817519220625 ) ) ;
#49623 = CARTESIAN_POINT ( 'NONE',  ( 10.74379975933729980, 5.078682052940000524, 7.871126858273000515 ) ) ;
#49624 = PRODUCT_DEFINITION ( 'UNKNOWN', '', #28476, #9415 ) ;
#49625 = CARTESIAN_POINT ( 'NONE',  ( 23.89320776801300283, 2.594336453560998734, -11.06325219636999435 ) ) ;
#49626 = CARTESIAN_POINT ( 'NONE',  ( 10.87376707263999975, 2.935913933350999816, -5.106852029161000672 ) ) ;
#49627 = CARTESIAN_POINT ( 'NONE',  ( 18.29840632282400037, -11.61484981121999915, 4.280299090734999368 ) ) ;
#49628 = LINE ( 'NONE', #66044, #36366 ) ;
#49629 = CYLINDRICAL_SURFACE ( 'NONE', #67847, 1.600000000000000089 ) ;
#49630 = CARTESIAN_POINT ( 'NONE',  ( 18.17882706751078814, -0.04040257046694439164, -12.69991905489011685 ) ) ;
#49631 = CARTESIAN_POINT ( 'NONE',  ( 12.19537138483636873, 2.360847786583726737, -12.48294616049518524 ) ) ;
#49632 = CARTESIAN_POINT ( 'NONE',  ( 11.23610538575739959, -2.890527834009000152, -7.234742334405199315 ) ) ;
#49633 = CARTESIAN_POINT ( 'NONE',  ( 8.032364158772001161, 3.524748802314000340, 5.573833469815000718 ) ) ;
#49634 = EDGE_LOOP ( 'NONE', ( #52929, #53239, #3516, #39828 ) ) ;
#49635 = AXIS2_PLACEMENT_3D ( 'NONE', #18663, #39995, #13430 ) ;
#49636 = CARTESIAN_POINT ( 'NONE',  ( 11.60000000000000320, -4.689830048140306573, -8.238968815098687060 ) ) ;
#49637 = CARTESIAN_POINT ( 'NONE',  ( 7.209999981161347549, 2.651351331278276380, 7.772802126760149477 ) ) ;
#49638 = CARTESIAN_POINT ( 'NONE',  ( 7.933148997457998952, -5.167567567567999731, 6.822293592207000934 ) ) ;
#49639 = CARTESIAN_POINT ( 'NONE',  ( 23.62003957313999791, -2.980470172838999954, 13.51719708605000037 ) ) ;
#49640 = CARTESIAN_POINT ( 'NONE',  ( 17.84060712062126086, 3.141591522576398177, 12.20206574396288524 ) ) ;
#49641 = CARTESIAN_POINT ( 'NONE',  ( 10.96237823296000080, 5.422576852879000597, 4.905482803814000370 ) ) ;
#49642 = FACE_OUTER_BOUND ( 'NONE', #10048, .T. ) ;
#49643 = CARTESIAN_POINT ( 'NONE',  ( 9.904204162135625822, -3.209635909649031671, 7.875309037467246753 ) ) ;
#49644 = CARTESIAN_POINT ( 'NONE',  ( 2.161066381942999826, 1.253716066476000091, -2.802099984798000154 ) ) ;
#49645 = EDGE_CURVE ( 'NONE', #29376, #67920, #32002, .T. ) ;
#49646 = ORIENTED_EDGE ( 'NONE', *, *, #15919, .F. ) ;
#49647 = CARTESIAN_POINT ( 'NONE',  ( 12.09778329087094839, -2.320992115139767886, 12.38439064982923021 ) ) ;
#49648 = EDGE_CURVE ( 'NONE', #9344, #24123, #59856, .T. ) ;
#49649 = CARTESIAN_POINT ( 'NONE',  ( 9.378405316141000370, -4.242421256336299962, -8.615780615741000403 ) ) ;
#49650 = CARTESIAN_POINT ( 'NONE',  ( 24.36958145701300182, -3.196690648311999894, -12.07804156775000060 ) ) ;
#49651 = AXIS2_PLACEMENT_3D ( 'NONE', #61148, #26149, #31056 ) ;
#49652 = CARTESIAN_POINT ( 'NONE',  ( 9.211801307670125283, 4.111875952999886508, 8.755178286007271993 ) ) ;
#49653 = CARTESIAN_POINT ( 'NONE',  ( 11.18272066707849888, 5.093522884867000222, -6.838543969064300398 ) ) ;
#49654 = ORIENTED_EDGE ( 'NONE', *, *, #43586, .F. ) ;
#49655 = CARTESIAN_POINT ( 'NONE',  ( 12.27537049189643525, -0.4912829912815118716, 12.59042165808839897 ) ) ;
#49656 = CARTESIAN_POINT ( 'NONE',  ( 9.074385841230999006, 3.981661882377999895, 8.959227447876999761 ) ) ;
#49657 = CARTESIAN_POINT ( 'NONE',  ( 10.77462860031000069, 5.575476001419000127, 8.682676628339999425 ) ) ;
#49658 = CARTESIAN_POINT ( 'NONE',  ( 12.67197039647509982, 3.110753821461598623, 12.28805851341191158 ) ) ;
#49659 = ORIENTED_EDGE ( 'NONE', *, *, #1367, .T. ) ;
#49660 = CARTESIAN_POINT ( 'NONE',  ( 9.693589158772999426, 4.047146749018000200, -5.600703114891000034 ) ) ;
#49661 = CARTESIAN_POINT ( 'NONE',  ( 11.35502763632549872, 2.839566963815999934, -6.964545474268299508 ) ) ;
#49662 = DIRECTION ( 'NONE',  ( 1.000000000000000000, 0.000000000000000000, 0.000000000000000000 ) ) ;
#49664 = CARTESIAN_POINT ( 'NONE',  ( 17.85612272112348364, -0.5477996803818093730, 12.68409554377261905 ) ) ;
#49663 = CARTESIAN_POINT ( 'NONE',  ( 8.229964631809997044, 4.681828315382999151, 6.132208354562998842 ) ) ;
#49665 = CARTESIAN_POINT ( 'NONE',  ( 9.756734463322999318, -3.909687748588949852, 6.637705594503099604 ) ) ;
#49666 = CARTESIAN_POINT ( 'NONE',  ( 11.66287348028854964, -4.761955701524100526, -7.911973420841600380 ) ) ;
#49667 = EDGE_LOOP ( 'NONE', ( #51876, #61574, #27822, #9901 ) ) ;
#49668 = VECTOR ( 'NONE', #28887, 999.9999999999998863 ) ;
#49669 = CARTESIAN_POINT ( 'NONE',  ( 1.357929084572999878, 0.7969358895047999880, 3.160091737778000009 ) ) ;
#49670 = ADVANCED_FACE ( 'NONE', ( #65760 ), #64712, .T. ) ;
#49671 = CARTESIAN_POINT ( 'NONE',  ( 24.17202345320177059, -9.108252266928689167, -9.092754609100827778 ) ) ;
#49672 = CARTESIAN_POINT ( 'NONE',  ( 11.16486084871730000, 5.207010770456999893, 7.825000000000000178 ) ) ;
#49673 = CARTESIAN_POINT ( 'NONE',  ( 18.00435067848273718, 1.907656978610660081, -12.45493970930200511 ) ) ;
#49674 = CARTESIAN_POINT ( 'NONE',  ( 24.26682857568000173, -12.18233728966999863, 3.303852351893000083 ) ) ;
#49675 = CARTESIAN_POINT ( 'NONE',  ( 12.10494519979310368, -2.707806787687958572, 13.73564420130113994 ) ) ;
#49676 = CARTESIAN_POINT ( 'NONE',  ( 10.91165259814999899, 2.977149300665999476, 4.913708281391000021 ) ) ;
#49677 = DIRECTION ( 'NONE',  ( 1.000000000000000000, 0.000000000000000000, -1.147230458784000007E-14 ) ) ;
#49678 = CARTESIAN_POINT ( 'NONE',  ( 13.55500032369700136, -12.12437004458000089, -2.498522620030000141 ) ) ;
#49679 = ORIENTED_EDGE ( 'NONE', *, *, #51605, .T. ) ;
#49680 = CARTESIAN_POINT ( 'NONE',  ( 6.758001042874380637, 3.668692617901999853, -8.939602259005999585 ) ) ;
#49681 = CARTESIAN_POINT ( 'NONE',  ( 17.60000000000000142, 10.78295181803999903, -4.410266442048000002 ) ) ;
#49682 = LINE ( 'NONE', #6679, #60917 ) ;
#49683 = CARTESIAN_POINT ( 'NONE',  ( 17.89269116643194479, -3.351202196788405807, -11.15759579123230338 ) ) ;
#49684 = CARTESIAN_POINT ( 'NONE',  ( 1.323656882336000207, -3.146289470026999879, -2.056511572473000093 ) ) ;
#49685 = VERTEX_POINT ( 'NONE', #65411 ) ;
#49686 = CARTESIAN_POINT ( 'NONE',  ( 10.63590686542921304, 5.314851119340273655, -7.853271763851206622 ) ) ;
#49687 = B_SPLINE_CURVE_WITH_KNOTS ( 'NONE', 3,
 ( #4034, #25374, #1217, #32012 ),
 .UNSPECIFIED., .F., .F.,
 ( 4, 4 ),
 ( 0.000000000000000000, 1.000000000000000000 ),
 .UNSPECIFIED. ) ;
#49688 = CARTESIAN_POINT ( 'NONE',  ( 17.57589479786107844, 1.875260891896569415, -12.57541370809468440 ) ) ;
#49689 = CARTESIAN_POINT ( 'NONE',  ( 0.000000000000000000, 2.899999999999999911, 7.500000000000000000 ) ) ;
#49690 = AXIS2_PLACEMENT_3D ( 'NONE', #26686, #31931, #36829 ) ;
#49691 = CARTESIAN_POINT ( 'NONE',  ( 11.85979573085659844, 4.840012015667699785, 7.354650721737899133 ) ) ;
#49692 = CARTESIAN_POINT ( 'NONE',  ( 11.07907162307749793, 3.185388239149200107, -7.174999999999999822 ) ) ;
#49693 = CARTESIAN_POINT ( 'NONE',  ( 10.62256935321000029, -2.471463903746000224, -8.210787855397999380 ) ) ;
#49694 = CARTESIAN_POINT ( 'NONE',  ( 5.105026506350000659, -1.500000000000000000, 0.000000000000000000 ) ) ;
#49695 = DIRECTION ( 'NONE',  ( -1.000000000000000000, 0.000000000000000000, 0.000000000000000000 ) ) ;
#49696 = CARTESIAN_POINT ( 'NONE',  ( 12.60033281152288964, -3.091857377022406705, 12.29379371307645208 ) ) ;
#49697 = ORIENTED_EDGE ( 'NONE', *, *, #21997, .F. ) ;
#49698 = CARTESIAN_POINT ( 'NONE',  ( 8.447510841229000533, 4.933589693325000525, -9.154576215408999573 ) ) ;
#49699 = ORIENTED_EDGE ( 'NONE', *, *, #47267, .F. ) ;
#49700 = CARTESIAN_POINT ( 'NONE',  ( 17.99129208686614945, -2.947687251868547520, 13.56825406139790680 ) ) ;
#49701 = CARTESIAN_POINT ( 'NONE',  ( 7.749582268678000929, 3.139123315411999737, 6.460037574229000157 ) ) ;
#49702 = ORIENTED_EDGE ( 'NONE', *, *, #10087, .T. ) ;
#49703 = CARTESIAN_POINT ( 'NONE',  ( 10.81524174883999834, 3.971581146373189597, 6.466884287543999577 ) ) ;
#49704 = FACE_OUTER_BOUND ( 'NONE', #30691, .T. ) ;
#49705 = DIRECTION ( 'NONE',  ( 0.000000000000000000, 1.000000000000000000, 0.000000000000000000 ) ) ;
#49706 = EDGE_CURVE ( 'NONE', #3171, #43113, #28373, .T. ) ;
#49707 = CARTESIAN_POINT ( 'NONE',  ( 18.50003594170800270, 2.686563649653999963, -11.33603604535000109 ) ) ;
#49708 = EDGE_CURVE ( 'NONE', #33837, #63101, #56661, .T. ) ;
#49709 = CARTESIAN_POINT ( 'NONE',  ( 24.44496488041000148, -12.03536727282999941, 3.224852091355999928 ) ) ;
#49710 = CARTESIAN_POINT ( 'NONE',  ( 10.84184687351645593, -4.999583552997724389, 8.268183399968647151 ) ) ;
#49711 = B_SPLINE_CURVE_WITH_KNOTS ( 'NONE', 3,
 ( #61602, #51456, #56710, #23161, #67180, #66154, #18272, #19294, #29118, #39592, #66496, #40619 ),
 .UNSPECIFIED., .F., .F.,
 ( 4, 2, 2, 2, 2, 4 ),
 ( 0.000000000000000000, 0.2500000000000009992, 0.3750000000000003331, 0.4375000000000012768, 0.5000000000000022204, 1.000000000000000000 ),
 .UNSPECIFIED. ) ;
#49712 = CARTESIAN_POINT ( 'NONE',  ( 11.55275411606000269, 3.402594452619000176, -11.19752650018000040 ) ) ;
#49713 = CARTESIAN_POINT ( 'NONE',  ( 10.15786958814999963, -4.213496663054999480, -5.822956951053000374 ) ) ;
#49714 = CARTESIAN_POINT ( 'NONE',  ( 11.01333310117409248, 5.463772421452093297, -7.751599404485491007 ) ) ;
#49715 = VECTOR ( 'NONE', #16616, 1000.000000000000000 ) ;
#49716 = ORIENTED_EDGE ( 'NONE', *, *, #50188, .F. ) ;
#49717 = CARTESIAN_POINT ( 'NONE',  ( 10.08521345716899908, 4.924890298941200228, 6.659120737011199331 ) ) ;
#49718 = EDGE_LOOP ( 'NONE', ( #45402, #38071, #9979, #43172, #54411, #31670, #59286, #44784, #61570, #63374, #69146, #15726, #4076, #43594, #52566, #1204, #28199, #33029, #31328, #8584, #25152 ) ) ;
#49719 = CARTESIAN_POINT ( 'NONE',  ( 10.73994861561131486, 3.062995749313938365, -4.824365178346956107 ) ) ;
#49720 = CARTESIAN_POINT ( 'NONE',  ( 11.00127285756000006, -5.155741062898000493, 5.106993030795000443 ) ) ;
#49721 = CARTESIAN_POINT ( 'NONE',  ( 10.66951519566999806, 4.592673277375999952, 5.841403042559999648 ) ) ;
#49722 = CARTESIAN_POINT ( 'NONE',  ( 17.80000000009400196, 3.216307036143000175, 11.40341376487999980 ) ) ;
#49723 = CARTESIAN_POINT ( 'NONE',  ( 10.54555864497999984, 5.007105485494000696, -8.288745882156399958 ) ) ;
#49724 = CARTESIAN_POINT ( 'NONE',  ( 12.31340688242389625, 2.113974262928780767, 13.74774419251637880 ) ) ;
#49725 = CARTESIAN_POINT ( 'NONE',  ( 10.16829915263999951, -4.567213659083999566, 5.832528837986999726 ) ) ;
#49726 = ORIENTED_EDGE ( 'NONE', *, *, #54379, .T. ) ;
#49727 = CARTESIAN_POINT ( 'NONE',  ( 7.849248001123737772, 3.014156315379637352, -6.506962576755648264 ) ) ;
#49728 = CARTESIAN_POINT ( 'NONE',  ( 12.40062321164033499, -0.4766231184928889086, 13.88900205690512735 ) ) ;
#49729 = ORIENTED_EDGE ( 'NONE', *, *, #54528, .F. ) ;
#49730 = FACE_OUTER_BOUND ( 'NONE', #27293, .T. ) ;
#49731 = EDGE_CURVE ( 'NONE', #42529, #60343, #53657, .T. ) ;
#49732 = DIRECTION ( 'NONE',  ( -0.7071067811864980568, 0.7071067811865969777, 6.440255933040979921E-09 ) ) ;
#49733 = CARTESIAN_POINT ( 'NONE',  ( 23.66461408848299897, -3.237974624424999615, -13.42763586457999914 ) ) ;
#49734 = CARTESIAN_POINT ( 'NONE',  ( 4.873530990069000701, -1.057166785643999907, -0.5398479887613999439 ) ) ;
#49735 = EDGE_CURVE ( 'NONE', #2498, #51230, #55270, .T. ) ;
#49736 = CARTESIAN_POINT ( 'NONE',  ( 9.427245280414000561, 4.989193221215000307, -6.287302145481000082 ) ) ;
#49737 = CIRCLE ( 'NONE', #66498, 0.2999999999999999889 ) ;
#49738 = LINE ( 'NONE', #59875, #17948 ) ;
#49739 = CARTESIAN_POINT ( 'NONE',  ( 10.52342417510000061, -3.209670667763000029, -9.177087527572998837 ) ) ;
#49740 = CARTESIAN_POINT ( 'NONE',  ( 9.550978115722108086, -5.350351920099831737, -7.263395478037801389 ) ) ;
#49741 = CARTESIAN_POINT ( 'NONE',  ( 8.256788585354000176, -2.896778558933000181, 6.628796229400999884 ) ) ;
#49742 = CARTESIAN_POINT ( 'NONE',  ( 4.490432128704166637, -1.044347811062755982, 1.103919035642354940 ) ) ;
#49743 = DIRECTION ( 'NONE',  ( 1.000000000000000000, 0.000000000000000000, 0.000000000000000000 ) ) ;
#49744 = DIRECTION ( 'NONE',  ( 1.000000000000000000, 0.000000000000000000, 0.000000000000000000 ) ) ;
#49745 = CARTESIAN_POINT ( 'NONE',  ( 1.084306799208999861, 1.762666431298138825, 3.058252359239908014 ) ) ;
#49746 = CARTESIAN_POINT ( 'NONE',  ( 10.81524174883999834, 3.971581146373189597, -8.533115712456000423 ) ) ;
#49747 = CARTESIAN_POINT ( 'NONE',  ( 9.204063610504999104, 4.411988005505000032, -8.416028484082099581 ) ) ;
#49749 = DIRECTION ( 'NONE',  ( 1.000000000000000000, 0.000000000000000000, 0.000000000000000000 ) ) ;
#49748 = CARTESIAN_POINT ( 'NONE',  ( 10.68491290906799840, -4.548591194283900130, 6.828616613600999585 ) ) ;
#49750 = CARTESIAN_POINT ( 'NONE',  ( 6.966665954281333839, 12.09896498756869576, -3.276379939815991627 ) ) ;
#49751 = EDGE_LOOP ( 'NONE', ( #57274, #11413, #55046, #52740 ) ) ;
#49752 = EDGE_CURVE ( 'NONE', #39042, #51109, #13016, .T. ) ;
#49753 = CARTESIAN_POINT ( 'NONE',  ( 11.48011496860029901, 4.919769165942200040, 7.971338736265699332 ) ) ;
#49754 = FACE_OUTER_BOUND ( 'NONE', #13059, .T. ) ;
#49755 = CARTESIAN_POINT ( 'NONE',  ( 10.29025461470400060, 2.893436332050999926, 7.218483930889299849 ) ) ;
#49756 = CARTESIAN_POINT ( 'NONE',  ( 10.82101354018296391, -4.768183399968640934, -6.500416447002272946 ) ) ;
#49757 = CARTESIAN_POINT ( 'NONE',  ( 9.385788300200999856, -4.980873770300999759, 6.433336655958999728 ) ) ;
#49758 = PLANE ( 'NONE',  #33014 ) ;
#49760 = CARTESIAN_POINT ( 'NONE',  ( 11.80415302574500203, 3.641975138519000232, -12.02422332381999937 ) ) ;
#49759 = UNCERTAINTY_MEASURE_WITH_UNIT (LENGTH_MEASURE( 1.000000000000000082E-05 ), #64260, 'distance_accuracy_value', 'NONE');
#49761 = ORIENTED_EDGE ( 'NONE', *, *, #58869, .T. ) ;
#49762 = VECTOR ( 'NONE', #63102, 1000.000000000000114 ) ;
#49763 = CARTESIAN_POINT ( 'NONE',  ( 9.761304848515999666, -3.086535948898899928, -7.917643062525700159 ) ) ;
#49764 = PLANE ( 'NONE',  #36587 ) ;
#49765 = CARTESIAN_POINT ( 'NONE',  ( 5.570621349514000009, -1.512468930016000135, 0.5654847974100999375 ) ) ;
#49766 = B_SPLINE_SURFACE_WITH_KNOTS ( 'NONE', 3, 3, ( 
 ( #10789, #5544, #51218, #23002, #9238, #56811, #60074, #30579, #60417, #28255, #49575, #14164, #8907, #33508, #62387, #45971, #30248, #24300, #14504 ),
 ( #54824, #45638, #24649, #57140, #33853, #51892, #6923, #8567, #35823, #22652, #43997, #67280, #12178, #29913, #24986, #65304, #17419, #51551, #19398 ),
 ( #28612, #2037, #38745, #3649, #44351, #35489, #40719, #55167, #17774, #1685, #46320, #13820, #67620, #62047, #19745, #61703, #41068, #66941, #19052 ),
 ( #65650, #39092, #12522, #7272, #49926, #40379, #35149, #56464, #3314, #20425, #52933, #3990, #58514, #37532, #9934, #14842, #10969, #42102, #5028 ) ),
 .UNSPECIFIED., .F., .F., .F.,
 ( 4, 4 ),
 ( 4, 1, 1, 1, 1, 1, 1, 1, 1, 1, 1, 1, 1, 1, 1, 1, 4 ),
 ( -0.1039086239011999951, 1.103908623900999864 ),
 ( -0.008849010032007000384, 0.01991027257200999809, 0.04866955517603999831, 0.07742883778006000306, 0.1061881203840999988, 0.1349474029881000126, 0.1637066855920999986, 0.1924659681960999846, 0.2212252508002000018, 0.2499845334042000156, 0.2787438160081999738, 0.3075030986121999876, 0.3362623812162000014, 0.3650216638202999908, 0.3937809464243000046, 0.4225402290282999629, 0.4512995116322999767 ),
 .UNSPECIFIED. ) ;
#49767 = CARTESIAN_POINT ( 'NONE',  ( 10.45769129028899869, -4.889436474118637577, 6.586710612921466534 ) ) ;
#49768 = AXIS2_PLACEMENT_3D ( 'NONE', #65390, #43396, #59459 ) ;
#49769 = CARTESIAN_POINT ( 'NONE',  ( 0.000000000000000000, -5.100000000000000533, 7.500000000000000000 ) ) ;
#49770 = CARTESIAN_POINT ( 'NONE',  ( 11.59672200990539892, -4.817867935977999672, 7.785290430335599865 ) ) ;
#49771 = CARTESIAN_POINT ( 'NONE',  ( 11.26487482311540056, 4.930401445321599851, -7.875904247640098887 ) ) ;
#49772 = CARTESIAN_POINT ( 'NONE',  ( 9.332537864288001472, 2.899999999999999911, 6.571291218949999902 ) ) ;
#49773 = CARTESIAN_POINT ( 'NONE',  ( 25.20343629728800394, -8.548126091438000174, 7.997439774512999477 ) ) ;
#49774 = CARTESIAN_POINT ( 'NONE',  ( 12.43753697073189279, 3.107573092027756001, 12.21083123505777479 ) ) ;
#49775 = VERTEX_POINT ( 'NONE', #24154 ) ;
#49776 = CARTESIAN_POINT ( 'NONE',  ( -0.000000000000000000, -0.7586348975815445650, -2.824745580908569309 ) ) ;
#49777 = CARTESIAN_POINT ( 'NONE',  ( 12.08233492791619490, -0.05915529127692992217, -13.99988012777929036 ) ) ;
#49778 = CARTESIAN_POINT ( 'NONE',  ( 13.89314246895800231, -8.838637615320999785, -7.948101024408999571 ) ) ;
#49779 = CARTESIAN_POINT ( 'NONE',  ( 24.63772188294200305, -8.684914509799000371, -8.585234952018000243 ) ) ;
#49780 = CARTESIAN_POINT ( 'NONE',  ( 10.50851354018319128, -4.163624617374471093, -8.749999999999998224 ) ) ;
#49781 = DIRECTION ( 'NONE',  ( -1.000000000000000000, 0.000000000000000000, 0.000000000000000000 ) ) ;
#49782 = CARTESIAN_POINT ( 'NONE',  ( 5.536712913981922668, 12.19258561489269255, -3.773936784932935051 ) ) ;
#49783 = ORIENTED_EDGE ( 'NONE', *, *, #7426, .T. ) ;
#49784 = B_SPLINE_CURVE_WITH_KNOTS ( 'NONE', 3,
 ( #45903, #68585, #57757, #58451, #9516, #15466, #16146, #47283, #37132, #36792, #47629, #42721, #30859, #37468, #63689, #67905, #58795, #68240, #36098, #57414, #3924, #25262, #20022, #21051, #15120, #14779, #46600, #25610, #15804, #4275, #68938, #52174, #47967, #46938, #58113, #10554, #63338, #5309, #25950, #10213, #20707, #30514, #41347, #4968, #31896, #53208, #52866, #42383, #62992, #20362, #41686, #26651, #36439 ),
 .UNSPECIFIED., .F., .F.,
 ( 4, 2, 2, 2, 2, 2, 2, 2, 2, 2, 2, 2, 2, 1, 2, 2, 2, 2, 2, 2, 2, 2, 2, 2, 1, 1, 2, 4 ),
 ( 0.000000000000000000, 0.06264497286344758442, 0.1252899457268951688, 0.1566124321586186696, 0.1879349185903421704, 0.2192574050220656989, 0.2349186482379256591, 0.2505798914537856192, 0.2819023778855022089, 0.2975636211013604759, 0.3132248643172187430, 0.3288861075330770101, 0.3445473507489353326, 0.3602085939647935997, 0.3680392155727237880, 0.3758698371806540317, 0.3915310803965136865, 0.3993617020044440968, 0.4071923236123745071, 0.4228535668282352722, 0.4306841884361666262, 0.4385148100440979246, 0.4541760532599614653, 0.4698372964758249504, 0.4854985396916884910, 0.4933291612996200115, 0.4972444721035861326, 0.5011597829075521426 ),
 .UNSPECIFIED. ) ;
#49785 = DIRECTION ( 'NONE',  ( -1.000000000000000000, 0.000000000000000000, 0.000000000000000000 ) ) ;
#49786 = CARTESIAN_POINT ( 'NONE',  ( 17.74479774746056293, 3.223061189501813750, -13.62394687717147335 ) ) ;
#49787 = ORIENTED_EDGE ( 'NONE', *, *, #60247, .T. ) ;
#49788 = CARTESIAN_POINT ( 'NONE',  ( 8.424688440789140031, 5.350083765069828523, 7.500019236172019710 ) ) ;
#49789 = CARTESIAN_POINT ( 'NONE',  ( 8.995183059623999000, -2.707994276285999646, 5.994456121676999594 ) ) ;
#49790 = AXIS2_PLACEMENT_3D ( 'NONE', #32781, #23323, #1305 ) ;
#49791 = CARTESIAN_POINT ( 'NONE',  ( 8.822164158776001130, 2.644017913812000131, -7.838184857420000817 ) ) ;
#49792 = ADVANCED_FACE ( 'NONE', ( #25183 ), #35686, .F. ) ;
#49793 = CARTESIAN_POINT ( 'NONE',  ( 24.22569895090174086, -12.33866087468328132, 3.306132354845392030 ) ) ;
#49794 = ADVANCED_FACE ( 'NONE', ( #61220 ), #5161, .T. ) ;
#49795 = CARTESIAN_POINT ( 'NONE',  ( 17.81256277267584309, 1.835326726223542426, -13.87917840078988263 ) ) ;
#49796 = CARTESIAN_POINT ( 'NONE',  ( 17.97807132158231980, 0.4608801934710635706, -12.68876176375646736 ) ) ;
#49797 = EDGE_CURVE ( 'NONE', #56062, #50502, #46494, .T. ) ;
#49798 = CARTESIAN_POINT ( 'NONE',  ( 10.90000000000000036, -5.283926297003000094, 7.082827057608000132 ) ) ;
#49799 = ORIENTED_EDGE ( 'NONE', *, *, #66872, .T. ) ;
#49800 = CARTESIAN_POINT ( 'NONE',  ( 9.385788300200999856, -4.980873770300999759, 6.433336655958999728 ) ) ;
#49801 = DIRECTION ( 'NONE',  ( 1.000000000000000000, 0.000000000000000000, 0.000000000000000000 ) ) ;
#49802 = CARTESIAN_POINT ( 'NONE',  ( 18.18005043857346692, -2.459498578984929296, 13.68200151021939348 ) ) ;
#49803 = ORIENTED_EDGE ( 'NONE', *, *, #16306, .F. ) ;
#49804 = CARTESIAN_POINT ( 'NONE',  ( 9.898128230592000421, 2.965931985296999862, -6.610871072364999712 ) ) ;
#49805 = EDGE_LOOP ( 'NONE', ( #14031, #39242, #48980, #36682, #13949 ) ) ;
#49806 = CARTESIAN_POINT ( 'NONE',  ( 9.128076168957999670, 3.490299597736799875, 6.634524523592600254 ) ) ;
#49807 = CARTESIAN_POINT ( 'NONE',  ( 18.17187109576076764, -2.859211385468993782, -12.27132042014886970 ) ) ;
#49808 = CARTESIAN_POINT ( 'NONE',  ( 9.633513540182331525, 5.250000000000001776, 7.336375382625529795 ) ) ;
#49809 = DIRECTION ( 'NONE',  ( -1.000000000000000000, 0.000000000000000000, 0.000000000000000000 ) ) ;
#49810 = CARTESIAN_POINT ( 'NONE',  ( 11.80890711774500090, -11.72268911462999874, -1.968096114907999628 ) ) ;
#49811 = CARTESIAN_POINT ( 'NONE',  ( 9.560684229509998744, 3.388828644390000200, 8.114961396014498618 ) ) ;
#49812 = CARTESIAN_POINT ( 'NONE',  ( 9.348645089171384370, -3.479920518481517178, 9.160150987731649153 ) ) ;
#49813 = ORIENTED_EDGE ( 'NONE', *, *, #57512, .T. ) ;
#49814 = CARTESIAN_POINT ( 'NONE',  ( 9.099999931440999390, 4.000000000000000000, -7.500000000000000000 ) ) ;
#49815 = CARTESIAN_POINT ( 'NONE',  ( 10.59957028040999916, 4.438147096284001059, -8.958385582135001357 ) ) ;
#49816 = CARTESIAN_POINT ( 'NONE',  ( 11.13359725006000112, -5.335216433401000380, -5.114389220295000982 ) ) ;
#49817 = CARTESIAN_POINT ( 'NONE',  ( 12.72264977853953027, 3.119885623323980006, -13.52225790872756228 ) ) ;
#49818 = CARTESIAN_POINT ( 'NONE',  ( 10.44424205625099944, -4.458751122174599679, -8.694123841252999085 ) ) ;
#49819 = CARTESIAN_POINT ( 'NONE',  ( 10.52638330645999964, -2.451090818816000105, 6.282756943804999494 ) ) ;
#49820 = CARTESIAN_POINT ( 'NONE',  ( 18.01141113125041571, 0.4275223103465155550, 13.89116040406442032 ) ) ;
#49821 = CIRCLE ( 'NONE', #25261, 1.350000000000000089 ) ;
#49822 = CARTESIAN_POINT ( 'NONE',  ( 25.29883272499000313, -2.991636379912000265, 11.41426982500999898 ) ) ;
#49823 = EDGE_LOOP ( 'NONE', ( #58103, #64480, #38281, #33646, #15515, #45854, #63104, #25289, #30878, #19276, #22509, #1924, #16816, #53645, #55548, #49853, #25482, #48014, #45564, #9981, #45228, #21920, #40678, #18144, #43074, #37866, #7206, #52212, #3236, #30604, #47823, #59020, #43845, #2310 ) ) ;
#49824 = ORIENTED_EDGE ( 'NONE', *, *, #63215, .F. ) ;
#49825 = CARTESIAN_POINT ( 'NONE',  ( 8.798539158775000146, 5.851083642416999631, -7.072167224702999633 ) ) ;
#49826 = DIRECTION ( 'NONE',  ( 0.7071065367651552247, -0.7071070256078553218, 1.045642193243934103E-09 ) ) ;
#49827 = CARTESIAN_POINT ( 'NONE',  ( 10.69810941423799910, -3.053977294209000437, 8.359277272599898723 ) ) ;
#49828 = CARTESIAN_POINT ( 'NONE',  ( 10.93728138146000006, -5.425439422033999648, 7.240583766112999697 ) ) ;
#49829 = DIRECTION ( 'NONE',  ( 0.000000000000000000, -1.000000000000000000, 0.000000000000000000 ) ) ;
#49830 = CARTESIAN_POINT ( 'NONE',  ( 9.160311019873999427, -4.122021308488999836, 9.013573548576999883 ) ) ;
#49831 = FACE_OUTER_BOUND ( 'NONE', #53516, .T. ) ;
#49833 = CARTESIAN_POINT ( 'NONE',  ( 10.96256888877000080, -5.431976784349000553, 4.905455483671000039 ) ) ;
#49832 = CARTESIAN_POINT ( 'NONE',  ( 10.58963399569799968, -2.728594541839999721, 7.358888170452400068 ) ) ;
#49834 = CARTESIAN_POINT ( 'NONE',  ( 10.96118313518939935, 3.207251432249800249, -8.502430091786999711 ) ) ;
#49835 = VECTOR ( 'NONE', #1796, 1000.000000000000000 ) ;
#49836 = CARTESIAN_POINT ( 'NONE',  ( 7.460824085303098485, 4.353476288197968280, -6.184976426942008665 ) ) ;
#49837 = EDGE_CURVE ( 'NONE', #31652, #25814, #61902, .T. ) ;
#49838 = CARTESIAN_POINT ( 'NONE',  ( 10.26947109217999810, 5.100000000000000533, -6.152188490330000370 ) ) ;
#49839 = CARTESIAN_POINT ( 'NONE',  ( 17.84124069827834091, 0.5557204214162413392, 12.68363025601216520 ) ) ;
#49840 = CARTESIAN_POINT ( 'NONE',  ( 11.09999999999999964, -5.435899401150079413, 6.701932011082668339 ) ) ;
#49841 = ADVANCED_FACE ( 'NONE', ( #34310 ), #3175, .F. ) ;
#49842 = CARTESIAN_POINT ( 'NONE',  ( 4.149992563291998948, -0.2617923565148011500, 1.999946284944287722 ) ) ;
#49843 = VERTEX_POINT ( 'NONE', #19602 ) ;
#49845 = CARTESIAN_POINT ( 'NONE',  ( 10.79683585285767577, 4.539293524411616154, 6.812066793331982950 ) ) ;
#49844 = CARTESIAN_POINT ( 'NONE',  ( 8.995183059623999000, -2.707994276285999646, 5.994456121676999594 ) ) ;
#49846 = CARTESIAN_POINT ( 'NONE',  ( 8.266329719591000824, 4.769017407621999993, -8.862909124839001507 ) ) ;
#49847 = CARTESIAN_POINT ( 'NONE',  ( 7.550000000000000711, -4.000000000000000000, 8.849999999999999645 ) ) ;
#49848 = CARTESIAN_POINT ( 'NONE',  ( 7.051113898392529222, -0.6785257367072009549, -1.178968686944157129 ) ) ;
#49849 = CARTESIAN_POINT ( 'NONE',  ( 10.09964828895399869, 5.121614868497999851, 6.887384543790600056 ) ) ;
#49850 = CARTESIAN_POINT ( 'NONE',  ( 11.09999999999999964, 0.5000000000000000000, -5.124965750789000296 ) ) ;
#49851 = CARTESIAN_POINT ( 'NONE',  ( 18.29998537156714633, -2.924732060074958007, -11.97422863287303407 ) ) ;
#49852 = CARTESIAN_POINT ( 'NONE',  ( 2.356882905178000254, -3.556067323659000134, 0.5081678699474000416 ) ) ;
#49853 = ORIENTED_EDGE ( 'NONE', *, *, #4347, .F. ) ;
#49854 = CARTESIAN_POINT ( 'NONE',  ( 12.30932062623504741, -0.5250004125410564493, -12.58906021966015842 ) ) ;
#49855 = CARTESIAN_POINT ( 'NONE',  ( 11.89975833414730033, -3.203462856645999945, 7.825000000000000178 ) ) ;
#49856 = FACE_OUTER_BOUND ( 'NONE', #66269, .T. ) ;
#49857 = CARTESIAN_POINT ( 'NONE',  ( 9.160308886257000793, 4.122021000979000149, 9.013569734175000292 ) ) ;
#49858 = ORIENTED_EDGE ( 'NONE', *, *, #63158, .T. ) ;
#49859 = CARTESIAN_POINT ( 'NONE',  ( 5.896449988747999527, -0.7225053299333999979, -0.9279906512076999681 ) ) ;
#49860 = CARTESIAN_POINT ( 'NONE',  ( 10.91988774271260709, 9.626587645410168648, 5.949865614865760932 ) ) ;
#49862 = CARTESIAN_POINT ( 'NONE',  ( 0.5181103717477000270, 3.205765437135000173, -1.404659375816999844 ) ) ;
#49861 = CARTESIAN_POINT ( 'NONE',  ( 8.572516478978494447, -3.946509990130368184, 5.760726263960903815 ) ) ;
#49863 = CARTESIAN_POINT ( 'NONE',  ( 10.84657802013509986, 2.684088780794000151, -7.469366283838649423 ) ) ;
#49864 = ORIENTED_EDGE ( 'NONE', *, *, #10357, .T. ) ;
#49865 = VECTOR ( 'NONE', #42660, 1000.000000000000000 ) ;
#49866 = B_SPLINE_CURVE_WITH_KNOTS ( 'NONE', 3,
 ( #62892, #52760, #35992, #68138, #46491, #41242, #19223, #31442, #20601, #47175, #31108, #56637, #35660, #19577, #41926, #13994, #35319, #9410, #46146, #8740, #15012, #30085, #68477, #51387, #4853, #9758, #3484, #67452, #62553, #30754 ),
 .UNSPECIFIED., .F., .F.,
 ( 4, 2, 1, 1, 2, 2, 2, 2, 2, 2, 2, 2, 2, 2, 2, 4 ),
 ( 0.000000000000000000, 0.1250000000000048017, 0.1875000000000072164, 0.2187500000000076883, 0.2343750000000070777, 0.2500000000000064948, 0.3750000000000048850, 0.4375000000000044409, 0.5000000000000038858, 0.5625000000000034417, 0.6250000000000028866, 0.6875000000000024425, 0.7500000000000018874, 0.8125000000000014433, 0.8750000000000009992, 1.000000000000000000 ),
 .UNSPECIFIED. ) ;
#49867 = ORIENTED_EDGE ( 'NONE', *, *, #16333, .T. ) ;
#49868 = CARTESIAN_POINT ( 'NONE',  ( 9.489405368643582861, -4.927979915958162316, 8.480323300091150429 ) ) ;
#49869 = CARTESIAN_POINT ( 'NONE',  ( 11.32299956498189886, 2.792989229543000107, 7.825000000000000178 ) ) ;
#49870 = PRESENTATION_LAYER_ASSIGNMENT (  '', '', ( #10781 ) ) ;
#49871 = CARTESIAN_POINT ( 'NONE',  ( 18.15028930682391106, 0.1908382484571590487, -13.89824168789394854 ) ) ;
#49872 = ORIENTED_EDGE ( 'NONE', *, *, #61002, .F. ) ;
#49873 = CARTESIAN_POINT ( 'NONE',  ( 10.98768472638000127, 7.408460564924999936, -6.159405844198999169 ) ) ;
#49874 = EDGE_CURVE ( 'NONE', #1219, #6746, #57004, .T. ) ;
#49875 = CARTESIAN_POINT ( 'NONE',  ( 8.383148997457999130, 5.167567567567999731, 6.822293592207000934 ) ) ;
#49876 = FACE_OUTER_BOUND ( 'NONE', #221, .T. ) ;
#49877 = VECTOR ( 'NONE', #66531, 1000.000000000000227 ) ;
#49878 = CARTESIAN_POINT ( 'NONE',  ( 9.599999931441001166, -2.935682118448999844, 6.844464000216799349 ) ) ;
#49879 = ADVANCED_FACE ( 'NONE', ( #57677 ), #4881, .F. ) ;
#49880 = CARTESIAN_POINT ( 'NONE',  ( 18.16572637375661969, -2.633126308906749369, 12.41957822429843539 ) ) ;
#49881 = ORIENTED_EDGE ( 'NONE', *, *, #48157, .T. ) ;
#49882 = CARTESIAN_POINT ( 'NONE',  ( 7.100000000000000533, -4.000000000000000000, 7.500000000000000000 ) ) ;
#49883 = ADVANCED_FACE ( 'NONE', ( #10136 ), #23387, .F. ) ;
#49884 = CARTESIAN_POINT ( 'NONE',  ( 12.49122810692607288, -3.040889930152274268, -13.54369178477776714 ) ) ;
#49885 = CARTESIAN_POINT ( 'NONE',  ( 9.654346873515669003, 5.250000000000002665, 7.663624617374463988 ) ) ;
#49886 = VECTOR ( 'NONE', #68752, 1000.000000000000000 ) ;
#49887 = CARTESIAN_POINT ( 'NONE',  ( 12.09999999999999964, -4.000000000000000000, 7.500000000000000000 ) ) ;
#49888 = ORIENTED_EDGE ( 'NONE', *, *, #28497, .F. ) ;
#49889 = CARTESIAN_POINT ( 'NONE',  ( 25.34046074233263823, 11.16058629745575814, 3.348985358652643463 ) ) ;
#49890 = CARTESIAN_POINT ( 'NONE',  ( 10.96685777392725036, -2.822345360332068509, -6.668352631380622064 ) ) ;
#49891 = CARTESIAN_POINT ( 'NONE',  ( 7.341922165042849890, 5.856757650166058760, -7.538504482028591802 ) ) ;
#49892 = CARTESIAN_POINT ( 'NONE',  ( 5.500000000000000000, 6.217248937900999058E-14, 3.708144902247999495E-14 ) ) ;
#49893 = CARTESIAN_POINT ( 'NONE',  ( 6.877497653516999598, -9.263786119211999903, 5.299649687518000363 ) ) ;
#49894 = CARTESIAN_POINT ( 'NONE',  ( 10.51927318630899855, 4.756452637475340417, 6.473854711408037588 ) ) ;
#49895 = CARTESIAN_POINT ( 'NONE',  ( 17.89568490471444662, -3.024116370425395939, 12.31388631808445133 ) ) ;
#49896 = ORIENTED_EDGE ( 'NONE', *, *, #53598, .F. ) ;
#49897 = CARTESIAN_POINT ( 'NONE',  ( 11.60988784977536348, -4.851105903694400645, -7.451365240271489832 ) ) ;
#49898 = VERTEX_POINT ( 'NONE', #9659 ) ;
#49899 = EDGE_CURVE ( 'NONE', #34575, #34779, #18552, .T. ) ;
#49900 = CARTESIAN_POINT ( 'NONE',  ( 18.15909587493458233, 2.338249772848897123, 13.70640098171117671 ) ) ;
#49901 = CARTESIAN_POINT ( 'NONE',  ( 9.784179719593000257, 4.042991257420999851, -5.768106221333000327 ) ) ;
#49902 = CARTESIAN_POINT ( 'NONE',  ( 3.579027452879000037, -3.225412259932999959, 0.5737794949255000665 ) ) ;
#49903 = CARTESIAN_POINT ( 'NONE',  ( 10.18512684885999953, -5.526147823900999789, -7.556025229989000280 ) ) ;
#49904 = CARTESIAN_POINT ( 'NONE',  ( 6.777068426484442298, 0.8477796283345830908, -1.258946551967616179 ) ) ;
#49905 = CARTESIAN_POINT ( 'NONE',  ( 8.061825939490002924, 3.419144686567003877, -6.221559872366999144 ) ) ;
#49906 = DIRECTION ( 'NONE',  ( 1.000000000000000000, 0.000000000000000000, 0.000000000000000000 ) ) ;
#49907 = ORIENTED_EDGE ( 'NONE', *, *, #53316, .F. ) ;
#49908 = CARTESIAN_POINT ( 'NONE',  ( 11.09999999999999964, -2.700469802787999640, -5.124965750789000296 ) ) ;
#49909 = CARTESIAN_POINT ( 'NONE',  ( 12.23256516821459883, -3.293702443348299980, 6.787191910456499500 ) ) ;
#49910 = CARTESIAN_POINT ( 'NONE',  ( 10.65550720192000078, 4.237674045823999869, 9.105219676299999065 ) ) ;
#49911 = CARTESIAN_POINT ( 'NONE',  ( 11.00000000066999917, -1.300000000000000044, 9.662944685757000940 ) ) ;
#49912 = DIRECTION ( 'NONE',  ( 0.7071058810608746859, 0.7071076813110745984, -3.975036265697858125E-09 ) ) ;
#49913 = CARTESIAN_POINT ( 'NONE',  ( 9.220176284132802991, 2.652345181577336231, 7.581873060868147718 ) ) ;
#49914 = CARTESIAN_POINT ( 'NONE',  ( 10.28441772631199846, 4.372518460886800185, -8.266796319406900295 ) ) ;
#49915 = AXIS2_PLACEMENT_3D ( 'NONE', #15232, #11018, #37245 ) ;
#49916 = CARTESIAN_POINT ( 'NONE',  ( 10.51293291887318659, 2.761699336110873926, 6.264570408027259063 ) ) ;
#49917 =( GEOMETRIC_REPRESENTATION_CONTEXT ( 3 ) GLOBAL_UNCERTAINTY_ASSIGNED_CONTEXT ( ( #47181 ) ) GLOBAL_UNIT_ASSIGNED_CONTEXT ( ( #33994, #50762, #29105 ) ) REPRESENTATION_CONTEXT ( 'NONE', 'WORKASPACE' ) );
#49918 = CARTESIAN_POINT ( 'NONE',  ( 9.733013376692998264, 2.982096917914000223, -6.982691809975100306 ) ) ;
#49919 = CARTESIAN_POINT ( 'NONE',  ( 23.73668232013400115, -9.842998214831000681, 9.652221460371999129 ) ) ;
#49920 = CARTESIAN_POINT ( 'NONE',  ( 8.129977276175630152, 4.943140683036665983, -6.335257674860757859 ) ) ;
#49921 = EDGE_CURVE ( 'NONE', #4160, #45907, #41156, .T. ) ;
#49922 = AXIS2_PLACEMENT_3D ( 'NONE', #7343, #55247, #13302 ) ;
#49923 = CARTESIAN_POINT ( 'NONE',  ( 10.19794834123000093, 4.262170647947000290, -8.834315641189999013 ) ) ;
#49924 = ORIENTED_EDGE ( 'NONE', *, *, #16412, .T. ) ;
#49925 = CARTESIAN_POINT ( 'NONE',  ( 7.218293146793000048, -4.773080213113000347, 8.927399220053999329 ) ) ;
#49926 = CARTESIAN_POINT ( 'NONE',  ( 10.06491331857999860, -5.318469253323000245, -7.099528416287999910 ) ) ;
#49927 = CARTESIAN_POINT ( 'NONE',  ( 18.27459401263892502, 2.425695574333697646, 13.78827716170582285 ) ) ;
#49928 = DIRECTION ( 'NONE',  ( 0.000000000000000000, 1.000000000000000000, 0.000000000000000000 ) ) ;
#49929 = CARTESIAN_POINT ( 'NONE',  ( 10.56733863405299800, -3.211524470605299886, -8.505794571537999005 ) ) ;
#49930 = VERTEX_POINT ( 'NONE', #26444 ) ;
#49931 = DIRECTION ( 'NONE',  ( 0.000000000000000000, 0.000000000000000000, -1.000000000000000000 ) ) ;
#49932 = CARTESIAN_POINT ( 'NONE',  ( 7.358051658771000092, 4.561643343497000735, 6.153061759127000485 ) ) ;
#49934 = CARTESIAN_POINT ( 'NONE',  ( 11.80233327354039830, 2.898463260143000042, 8.220500279733599314 ) ) ;
#49933 = DIRECTION ( 'NONE',  ( 0.000000000000000000, -0.9999830366945593463, -0.005824630728861762523 ) ) ;
#49935 = CARTESIAN_POINT ( 'NONE',  ( 16.39999999379500295, 3.351248059343999941, 11.15756683833000018 ) ) ;
#49936 = ORIENTED_EDGE ( 'NONE', *, *, #6736, .F. ) ;
#49937 = CARTESIAN_POINT ( 'NONE',  ( 9.242342830452999536, 5.206708472530999998, 8.808826521083998884 ) ) ;
#49938 = VECTOR ( 'NONE', #6165, 1000.000000000000000 ) ;
#49939 = CARTESIAN_POINT ( 'NONE',  ( 17.87779404330691690, -3.171907921506158967, -13.63594617280361199 ) ) ;
#49940 = CARTESIAN_POINT ( 'NONE',  ( 10.28026357027499849, 4.985299147223100746, 7.309904858193100097 ) ) ;
#49941 = CARTESIAN_POINT ( 'NONE',  ( 9.778462793022999477, -5.743713977826000239, 7.748300060190000060 ) ) ;
#49942 = CARTESIAN_POINT ( 'NONE',  ( 7.540307192462002206, 2.929979193199001575, 6.558004150875995641 ) ) ;
#49943 = ORIENTED_EDGE ( 'NONE', *, *, #44678, .F. ) ;
#49944 = DIRECTION ( 'NONE',  ( -0.9999999999999992228, 2.758142135616997833E-08, 2.614631440159998134E-08 ) ) ;
#49945 = CARTESIAN_POINT ( 'NONE',  ( 1.292640132541499565, -3.058252359239901796, -1.762666431298149039 ) ) ;
#49946 = CARTESIAN_POINT ( 'NONE',  ( 7.934858580180682353, -2.291129595918548922, 7.825900736742252839 ) ) ;
#49947 = CARTESIAN_POINT ( 'NONE',  ( 10.22109127278999807, -2.983266195621000261, 8.764707262515999631 ) ) ;
#49948 = CARTESIAN_POINT ( 'NONE',  ( 10.16967105008495587, -2.650360704944366042, 7.590422644555561149 ) ) ;
#49949 = CARTESIAN_POINT ( 'NONE',  ( 9.904684229509999938, -4.804883439508000897, 8.309874741421300115 ) ) ;
#49950 = ORIENTED_EDGE ( 'NONE', *, *, #6797, .F. ) ;
#49951 = CARTESIAN_POINT ( 'NONE',  ( 23.60000648730661155, -10.25354231743684075, 9.380090008360967957 ) ) ;
#49952 = CARTESIAN_POINT ( 'NONE',  ( 11.12072335273220069, -3.602909566644000083, 6.430603299050000388 ) ) ;
#49953 = ORIENTED_EDGE ( 'NONE', *, *, #4719, .T. ) ;
#49954 = CARTESIAN_POINT ( 'NONE',  ( 10.59393020684899867, -2.750000000000000000, 7.500000000000000000 ) ) ;
#49955 = ORIENTED_EDGE ( 'NONE', *, *, #23599, .T. ) ;
#49956 = CARTESIAN_POINT ( 'NONE',  ( 9.003345280414000840, 2.319062457810000311, -7.919229449146000022 ) ) ;
#49957 = FACE_OUTER_BOUND ( 'NONE', #28438, .T. ) ;
#49958 = CARTESIAN_POINT ( 'NONE',  ( 24.63332959156766577, 8.756202931479766249, 7.455126439085037582 ) ) ;
#49959 = CARTESIAN_POINT ( 'NONE',  ( 12.33364759508187802, 3.027124203391257762, -12.23096800428945663 ) ) ;
#49960 = ADVANCED_FACE ( 'NONE', ( #53355 ), #63760, .F. ) ;
#49961 = CARTESIAN_POINT ( 'NONE',  ( 11.68923293495519999, -5.032672437899000428, 7.541513160549049744 ) ) ;
#49962 = EDGE_CURVE ( 'NONE', #62127, #2041, #34223, .T. ) ;
#49963 = CARTESIAN_POINT ( 'NONE',  ( 9.823096873516664829, 2.782534154164606921, 7.827184855449101697 ) ) ;
#49964 = CIRCLE ( 'NONE', #23162, 0.5999999999999999778 ) ;
#49965 = ORIENTED_EDGE ( 'NONE', *, *, #18673, .T. ) ;
#49966 = CARTESIAN_POINT ( 'NONE',  ( 7.545269353206999874, -2.302293129340000188, 6.875167727519000849 ) ) ;
#49967 = CARTESIAN_POINT ( 'NONE',  ( 9.099999886593998610, 3.268496584495999908E-13, -12.39999890529996485 ) ) ;
#49968 = ORIENTED_EDGE ( 'NONE', *, *, #65652, .F. ) ;
#49969 = CARTESIAN_POINT ( 'NONE',  ( 12.47010838183371462, -1.842148406394420013, -12.46461078478868423 ) ) ;
#49970 = CARTESIAN_POINT ( 'NONE',  ( 11.58071932425156980, 3.832730087831799803, 6.371589232479998977 ) ) ;
#49971 =( GEOMETRIC_REPRESENTATION_CONTEXT ( 3 ) GLOBAL_UNCERTAINTY_ASSIGNED_CONTEXT ( ( #25510 ) ) GLOBAL_UNIT_ASSIGNED_CONTEXT ( ( #33563, #7328, #8027 ) ) REPRESENTATION_CONTEXT ( 'NONE', 'WORKASPACE' ) );
#49972 = CARTESIAN_POINT ( 'NONE',  ( 10.21160513988086294, 3.634030556546760327, -8.817876221680393201 ) ) ;
#49973 = CARTESIAN_POINT ( 'NONE',  ( 6.649999999999999467, 5.221516520829000640, -8.074802043613001246 ) ) ;
#49974 = CARTESIAN_POINT ( 'NONE',  ( 18.26719328781100060, -11.65592881096000077, 3.892957952850000236 ) ) ;
#49975 = CARTESIAN_POINT ( 'NONE',  ( 9.120327454391752298, 5.191173620088457064, -7.088789390544037339 ) ) ;
#49976 = CARTESIAN_POINT ( 'NONE',  ( 12.36880880067038291, -2.947687262017098409, -13.56819815501604154 ) ) ;
#49977 = CARTESIAN_POINT ( 'NONE',  ( 18.03207563512528111, -0.4039503557775012688, -12.69135589213616377 ) ) ;
#49978 = B_SPLINE_CURVE_WITH_KNOTS ( 'NONE', 3,
 ( #47528, #68832, #42620, #5209 ),
 .UNSPECIFIED., .F., .F.,
 ( 4, 4 ),
 ( 0.000000000000000000, 1.000000000000000000 ),
 .UNSPECIFIED. ) ;
#49979 = AXIS2_PLACEMENT_3D ( 'NONE', #10955, #21105, #58847 ) ;
#49980 = CARTESIAN_POINT ( 'NONE',  ( 12.21062133718143627, 2.693099985209356451, -12.40450382421715680 ) ) ;
#49981 = B_SPLINE_CURVE_WITH_KNOTS ( 'NONE', 3,
 ( #38772, #49948, #54501, #12546, #48572, #64972, #28281, #39116, #66015 ),
 .UNSPECIFIED., .F., .F.,
 ( 4, 1, 1, 1, 1, 1, 4 ),
 ( 0.1253905405517105054, 0.1733119344633363701, 0.3402003772241184443, 0.5070888199843091027, 0.6739772627450910658, 0.8408657055052815021, 0.8746295857519847949 ),
 .UNSPECIFIED. ) ;
#49982 = CARTESIAN_POINT ( 'NONE',  ( 10.42380110216399913, -4.973546009874400653, -6.905442784147899360 ) ) ;
#49983 = CARTESIAN_POINT ( 'NONE',  ( 8.481676658773000810, 2.472348777564000066, 6.234194744024999402 ) ) ;
#49984 = ORIENTED_EDGE ( 'NONE', *, *, #64540, .T. ) ;
#49985 = ADVANCED_FACE ( 'NONE', ( #19201, #67426, #68113, #41219 ), #20231, .F. ) ;
#49986 = AXIS2_PLACEMENT_3D ( 'NONE', #54204, #17146, #10871 ) ;
#49987 = SURFACE_STYLE_FILL_AREA ( #22714 ) ;
#49988 = CARTESIAN_POINT ( 'NONE',  ( 11.59999999999999787, -4.874497702741446226, -7.869208573981368637 ) ) ;
#49989 = DIRECTION ( 'NONE',  ( 0.000000000000000000, 1.000000000000000000, 0.000000000000000000 ) ) ;
#49990 = CARTESIAN_POINT ( 'NONE',  ( 10.60518955639999916, 5.343965917319999370, -7.731522121091999544 ) ) ;
#49991 = EDGE_CURVE ( 'NONE', #35342, #32947, #9439, .T. ) ;
#49992 = CARTESIAN_POINT ( 'NONE',  ( 17.86252378965066612, 3.131846597291652046, 12.20457061699601731 ) ) ;
#49993 = CARTESIAN_POINT ( 'NONE',  ( 17.55505043854144276, 0.6250000000000001110, -13.88107975066922428 ) ) ;
#49994 = CARTESIAN_POINT ( 'NONE',  ( 10.34021053755999908, 4.202028620710000162, 9.459600235481000041 ) ) ;
#49995 = VECTOR ( 'NONE', #8957, 1000.000000000000000 ) ;
#49996 = CARTESIAN_POINT ( 'NONE',  ( 17.80000000001300009, 3.351264566333000072, 11.15757590352999884 ) ) ;
#49997 = CARTESIAN_POINT ( 'NONE',  ( 12.15762345757241825, 0.3746922850242029313, -12.59513687151644845 ) ) ;
#49998 = EDGE_LOOP ( 'NONE', ( #50633, #47785, #38392 ) ) ;
#49999 = CARTESIAN_POINT ( 'NONE',  ( 12.20120475779648572, -2.662482513922677985, 12.41227208748765598 ) ) ;
#50000 = CARTESIAN_POINT ( 'NONE',  ( 9.629684229509999582, -4.708027397558999461, -6.787581931282099745 ) ) ;
#50001 = CARTESIAN_POINT ( 'NONE',  ( 24.46275371508600216, -3.515554276222999874, -12.28676815851000015 ) ) ;
#50002 = DIRECTION ( 'NONE',  ( 1.000000000000000000, 0.000000000000000000, 0.000000000000000000 ) ) ;
#50003 = CARTESIAN_POINT ( 'NONE',  ( 10.37457053952199892, 3.551693493661699730, -6.451042711717000167 ) ) ;
#50004 = CARTESIAN_POINT ( 'NONE',  ( 12.68606859785047725, -0.7096370184368634426, 12.58000072970462924 ) ) ;
#50005 = CARTESIAN_POINT ( 'NONE',  ( 8.020982780409999791, 3.245534453799999941, 8.949623695221001540 ) ) ;
#50006 = CARTESIAN_POINT ( 'NONE',  ( 11.08492721656000057, 3.668390701878999849, 5.558148445539999649 ) ) ;
#50007 = CARTESIAN_POINT ( 'NONE',  ( 12.80505043854143388, 1.875000000000000000, -13.78631952119025428 ) ) ;
#50008 = EDGE_CURVE ( 'NONE', #48587, #26079, #37803, .T. ) ;
#50009 = ORIENTED_EDGE ( 'NONE', *, *, #62888, .T. ) ;
#50010 = CARTESIAN_POINT ( 'NONE',  ( 9.196339158776000389, 4.112741311853999271, -5.603466076760000192 ) ) ;
#50011 = CARTESIAN_POINT ( 'NONE',  ( 10.66579975933730040, 5.208485784810999775, -7.084213409908699965 ) ) ;
#50012 = AXIS2_PLACEMENT_3D ( 'NONE', #22093, #37835, #65778 ) ;
#50013 = CARTESIAN_POINT ( 'NONE',  ( 13.49994651945300284, 12.07042783918999795, 2.492331243371999960 ) ) ;
#50015 = CARTESIAN_POINT ( 'NONE',  ( 17.72542258371771950, -0.6019459913954784414, 12.68079480700004957 ) ) ;
#50014 = CARTESIAN_POINT ( 'NONE',  ( 11.49999672495000169, -3.632761979779000061, 11.06912554803999882 ) ) ;
#50016 = CARTESIAN_POINT ( 'NONE',  ( 10.61591290906799934, -4.635529777446699917, 6.722218404915299317 ) ) ;
#50017 = B_SPLINE_CURVE_WITH_KNOTS ( 'NONE', 3,
 ( #7335, #33572, #59097, #38464, #65011 ),
 .UNSPECIFIED., .F., .F.,
 ( 4, 1, 4 ),
 ( 0.000000000000000000, 0.4040625160519999981, 1.000000000000000000 ),
 .UNSPECIFIED. ) ;
#50018 = CARTESIAN_POINT ( 'NONE',  ( 11.51518179236248862, -4.180996681294200101, -6.652923384986699773 ) ) ;
#50019 = EDGE_LOOP ( 'NONE', ( #49013, #43409, #15827, #60198 ) ) ;
#50020 = CARTESIAN_POINT ( 'NONE',  ( 1.977794427304000013, -3.102129433205000009, 0.9990388109167002151 ) ) ;
#50021 = CARTESIAN_POINT ( 'NONE',  ( 24.22565958376758388, -9.032573813968939547, -9.032576340893927025 ) ) ;
#50022 = CIRCLE ( 'NONE', #35497, 1.250000000000000888 ) ;
#50023 = CARTESIAN_POINT ( 'NONE',  ( 25.37956961487633833, 11.36923106309306775, 3.069084611032080190 ) ) ;
#50024 = CARTESIAN_POINT ( 'NONE',  ( 18.09696660045537442, -2.811537062166766354, 13.60243477577289717 ) ) ;
#50025 = DIRECTION ( 'NONE',  ( 1.000000000000000000, 0.000000000000000000, 0.000000000000000000 ) ) ;
#50026 = CARTESIAN_POINT ( 'NONE',  ( 12.09788000779848183, -2.355563551342477968, 13.80043034480240394 ) ) ;
#50027 = CARTESIAN_POINT ( 'NONE',  ( 8.472537864290000442, 2.899999999999999911, -6.571291218949999902 ) ) ;
#50028 = CARTESIAN_POINT ( 'NONE',  ( 9.422954534637428381, -5.349869571284899372, 7.471026763531456893 ) ) ;
#50029 = CARTESIAN_POINT ( 'NONE',  ( 13.46005557146100173, -12.04952288628000012, -2.412084176363999966 ) ) ;
#50030 = EDGE_LOOP ( 'NONE', ( #23035, #29351, #9735, #57392, #8294 ) ) ;
#50031 = CARTESIAN_POINT ( 'NONE',  ( 7.594166666663750398, 5.314863113502227066, -7.146640356114973613 ) ) ;
#50032 = B_SPLINE_CURVE_WITH_KNOTS ( 'NONE', 3,
 ( #1389, #18167, #6977, #65354 ),
 .UNSPECIFIED., .F., .F.,
 ( 4, 4 ),
 ( 0.000000000000000000, 0.1836163425310829433 ),
 .UNSPECIFIED. ) ;
#50033 = CARTESIAN_POINT ( 'NONE',  ( 10.86068541168999957, 5.063199384101999989, 5.173500105045000019 ) ) ;
#50034 = CARTESIAN_POINT ( 'NONE',  ( 7.448092524957871774, -2.260623559829979090, 7.520946136199704313 ) ) ;
#50035 = DIRECTION ( 'NONE',  ( 0.9999999999938153916, 3.516990153967782703E-06, 1.152484550329262306E-11 ) ) ;
#50036 = CARTESIAN_POINT ( 'NONE',  ( 0.4653817924015999918, 2.512752844666000129, -2.494243791339000094 ) ) ;
#50037 = ORIENTED_EDGE ( 'NONE', *, *, #13363, .T. ) ;
#50038 = CARTESIAN_POINT ( 'NONE',  ( 10.86501009699162701, 2.649983380500041008, -7.500000587580665901 ) ) ;
#50039 = CARTESIAN_POINT ( 'NONE',  ( 17.83452421831947987, 1.940868773865736197, -12.56443418441918425 ) ) ;
#50040 = CARTESIAN_POINT ( 'NONE',  ( 9.873082992855456652, -5.217431357650285761, 7.827172124334913939 ) ) ;
#50041 = CARTESIAN_POINT ( 'NONE',  ( 10.84641504065830020, 4.804462279649600376, 8.099826052678000821 ) ) ;
#50042 = CARTESIAN_POINT ( 'NONE',  ( 9.525000000000000355, -4.417172942406000224, 8.783926296998000538 ) ) ;
#50043 = DIRECTION ( 'NONE',  ( 1.000000000000000000, 0.000000000000000000, 0.000000000000000000 ) ) ;
#50044 = CARTESIAN_POINT ( 'NONE',  ( 10.99245660749487463, -6.449695542863823405, 5.237054987098043846 ) ) ;
#50045 = CARTESIAN_POINT ( 'NONE',  ( 24.56046482271400322, 12.50678080147000060, 2.996392338889999785 ) ) ;
#50046 = ADVANCED_FACE ( 'NONE', ( #14984, #9050 ), #8717, .T. ) ;
#50047 = CARTESIAN_POINT ( 'NONE',  ( 12.52707377837015024, -3.060156797972230169, 12.30326077405791274 ) ) ;
#50048 = EDGE_CURVE ( 'NONE', #45049, #23998, #61952, .T. ) ;
#50049 = ORIENTED_EDGE ( 'NONE', *, *, #4679, .F. ) ;
#50050 = CARTESIAN_POINT ( 'NONE',  ( 7.337806197067810565, 3.730756353036506656, 9.220484948575563777 ) ) ;
#50051 = VERTEX_POINT ( 'NONE', #61513 ) ;
#50052 = EDGE_CURVE ( 'NONE', #38357, #43600, #44265, .T. ) ;
#50053 = B_SPLINE_CURVE_WITH_KNOTS ( 'NONE', 3,
 ( #8950, #40764, #15227, #30291 ),
 .UNSPECIFIED., .F., .F.,
 ( 4, 4 ),
 ( 0.000000000000000000, 1.000000000000000000 ),
 .UNSPECIFIED. ) ;
#50054 = CARTESIAN_POINT ( 'NONE',  ( 18.08228063350341230, -2.164202898012135279, 13.73897034938254613 ) ) ;
#50055 = CARTESIAN_POINT ( 'NONE',  ( 10.81349144726329925, -4.738947899111299655, -6.457276458983999490 ) ) ;
#50056 = ORIENTED_EDGE ( 'NONE', *, *, #16520, .F. ) ;
#50057 = ORIENTED_EDGE ( 'NONE', *, *, #698, .F. ) ;
#50058 = CARTESIAN_POINT ( 'NONE',  ( 11.02812378248509795, 3.583106837161099900, 8.288725998710999576 ) ) ;
#50059 = FACE_OUTER_BOUND ( 'NONE', #35960, .T. ) ;
#50060 = DIRECTION ( 'NONE',  ( 1.000000000000000000, 0.000000000000000000, 0.000000000000000000 ) ) ;
#50061 = CARTESIAN_POINT ( 'NONE',  ( 10.36409408021999923, -3.399999909169000301, -4.954046131279000065 ) ) ;
#50062 = CARTESIAN_POINT ( 'NONE',  ( 11.09999999999999964, 4.000000000000000000, 7.500000000000000000 ) ) ;
#50063 = CARTESIAN_POINT ( 'NONE',  ( 21.10000109091659937, 0.000000000000000000, 0.000000000000000000 ) ) ;
#50064 = CARTESIAN_POINT ( 'NONE',  ( 11.48831242699000121, 3.364143239851999923, -11.30418287150000012 ) ) ;
#50065 = CARTESIAN_POINT ( 'NONE',  ( 11.17811058788999823, -2.762459764047000110, -6.187206491620000470 ) ) ;
#50066 = CARTESIAN_POINT ( 'NONE',  ( 4.000000000000000888, -0.5626148410807586542, -2.094138670346520126 ) ) ;
#50067 = CARTESIAN_POINT ( 'NONE',  ( 23.57776920565314427, -10.35458434377875747, 9.360247510821011474 ) ) ;
#50068 = ORIENTED_EDGE ( 'NONE', *, *, #53664, .T. ) ;
#50069 = ADVANCED_FACE ( 'NONE', ( #66751 ), #3457, .T. ) ;
#50070 = CARTESIAN_POINT ( 'NONE',  ( 11.09999999999999964, 4.000000000000000000, -7.500000000000000000 ) ) ;
#50071 = CARTESIAN_POINT ( 'NONE',  ( 5.700000000000000178, 11.06886219213000011, -1.536526853569999851 ) ) ;
#50072 = CARTESIAN_POINT ( 'NONE',  ( 10.95931585633000083, -5.066484979568000035, 5.182226135408999568 ) ) ;
#50073 = EDGE_CURVE ( 'NONE', #44936, #58927, #4144, .T. ) ;
#50074 = CARTESIAN_POINT ( 'NONE',  ( 10.39393020684899938, -5.250000000000000000, 7.500000000000000000 ) ) ;
#50075 = CARTESIAN_POINT ( 'NONE',  ( 9.393930206848999376, 2.750000000000000000, 7.500000000000000000 ) ) ;
#50076 = CARTESIAN_POINT ( 'NONE',  ( 12.30715842069478505, 2.122066859011512818, 13.74633992746440114 ) ) ;
#50077 = CARTESIAN_POINT ( 'NONE',  ( 10.03612181215999932, -3.011786236723999810, 8.746965724352000038 ) ) ;
#50078 = VERTEX_POINT ( 'NONE', #35965 ) ;
#50079 = CARTESIAN_POINT ( 'NONE',  ( 10.98768472638000127, 7.408460511344000743, 6.159405790617999976 ) ) ;
#50080 = CARTESIAN_POINT ( 'NONE',  ( 12.70954970454857502, 0.7242550212505937113, 13.98125389334239799 ) ) ;
#50081 = EDGE_LOOP ( 'NONE', ( #66975, #4924, #55545 ) ) ;
#50082 = CARTESIAN_POINT ( 'NONE',  ( 7.067909439180999343, 3.037137096735000430, -6.379793420563999895 ) ) ;
#50083 = CARTESIAN_POINT ( 'NONE',  ( 8.879093088636166087, 2.650571520623451249, -7.263234620901792837 ) ) ;
#50084 = CARTESIAN_POINT ( 'NONE',  ( 23.83526264196600053, -3.383500917634999716, -13.10496161808000082 ) ) ;
#50085 = CONICAL_SURFACE ( 'NONE', #54517, 0.3062142749367001149, 0.7853981633972997312 ) ;
#50086 = CARTESIAN_POINT ( 'NONE',  ( 5.000000000000000000, 0.000000000000000000, -1.799999999999970512 ) ) ;
#50087 = CARTESIAN_POINT ( 'NONE',  ( 8.880270280412998929, 4.146787477634999775, -5.941926545671999627 ) ) ;
#50088 = CARTESIAN_POINT ( 'NONE',  ( 17.76396973669300294, -3.526704268670000086, 11.96114524401999901 ) ) ;
#50089 = CARTESIAN_POINT ( 'NONE',  ( 11.01430358291000111, 8.153755387268001087, -6.595354411296000308 ) ) ;
#50090 = STYLED_ITEM ( 'NONE', ( #27100 ), #7958 ) ;
#50091 = CARTESIAN_POINT ( 'NONE',  ( 8.148264992380649829, 4.679617213703884282, -8.679508107075978529 ) ) ;
#50092 = DIRECTION ( 'NONE',  ( 1.000000000000000000, 0.000000000000000000, 0.000000000000000000 ) ) ;
#50093 = CARTESIAN_POINT ( 'NONE',  ( 13.00000000001300116, 11.52577654661000039, 1.696746661728000038 ) ) ;
#50094 = CARTESIAN_POINT ( 'NONE',  ( 9.790745838555999114, -4.301175052434000001, -8.935144319903001175 ) ) ;
#50095 = CARTESIAN_POINT ( 'NONE',  ( 10.43210941423799909, 4.641185166475500168, -6.917608226833099394 ) ) ;
#50096 = CARTESIAN_POINT ( 'NONE',  ( 1.000973465875999890, 3.500000000000000000, 0.000000000000000000 ) ) ;
#50097 = CARTESIAN_POINT ( 'NONE',  ( 10.76857802013509868, 2.825431102905000103, -7.472656658230009796 ) ) ;
#50098 = CARTESIAN_POINT ( 'NONE',  ( 9.278038493598998571, 4.826346105011899645, -6.712036445818600150 ) ) ;
#50100 = CARTESIAN_POINT ( 'NONE',  ( 10.53455565919999870, -3.019620544914000337, 5.071252824073000376 ) ) ;
#50099 = CARTESIAN_POINT ( 'NONE',  ( 15.49162860438300271, -8.811474098792000831, -7.563394002770000846 ) ) ;
#50101 = VECTOR ( 'NONE', #37339, 1000.000000000000000 ) ;
#50102 = DIRECTION ( 'NONE',  ( -1.000000000000000000, 0.000000000000000000, 0.000000000000000000 ) ) ;
#50103 = EDGE_LOOP ( 'NONE', ( #19069, #22616, #62761, #18196, #25383 ) ) ;
#50104 = CARTESIAN_POINT ( 'NONE',  ( 11.23078751119019891, 3.084247107206000038, 7.020904658857499925 ) ) ;
#50105 = CARTESIAN_POINT ( 'NONE',  ( 11.05639424537999993, -5.030223832177999732, 6.028291574375000295 ) ) ;
#50106 = EDGE_CURVE ( 'NONE', #16959, #65259, #58598, .T. ) ;
#50107 = EDGE_CURVE ( 'NONE', #44936, #14966, #29720, .T. ) ;
#50108 = CARTESIAN_POINT ( 'NONE',  ( 9.099784697134998268, 4.619613413415000203, 8.459069166353199165 ) ) ;
#50109 = CARTESIAN_POINT ( 'NONE',  ( 10.24006601915162484, 3.957587222814286321, -8.373918476712228554 ) ) ;
#50110 = CARTESIAN_POINT ( 'NONE',  ( 10.53138988903999973, -5.607755226963999640, 7.280101849877000042 ) ) ;
#50111 = CARTESIAN_POINT ( 'NONE',  ( 9.637090959179923644, -5.238013552912343940, 6.265105236445105419 ) ) ;
#50112 = CARTESIAN_POINT ( 'NONE',  ( 11.55259020248000112, 3.617313325735000085, -11.93403632987999963 ) ) ;
#50113 = ORIENTED_EDGE ( 'NONE', *, *, #7764, .T. ) ;
#50114 = B_SPLINE_CURVE_WITH_KNOTS ( 'NONE', 3,
 ( #11418, #18062, #33107, #49869 ),
 .UNSPECIFIED., .F., .F.,
 ( 4, 4 ),
 ( 0.000000000000000000, 1.000000000000000000 ),
 .UNSPECIFIED. ) ;
#50115 = CARTESIAN_POINT ( 'NONE',  ( 8.999417874593998334, -5.050800927762999493, -7.946712276748498560 ) ) ;
#50116 = CARTESIAN_POINT ( 'NONE',  ( 9.843930206850000530, -5.250000000000000000, -7.500000000000000000 ) ) ;
#50117 = CARTESIAN_POINT ( 'NONE',  ( 5.498333808541000955, 0.9320062393831999303, 1.134853260389000029 ) ) ;
#50118 = FACE_OUTER_BOUND ( 'NONE', #37928, .T. ) ;
#50119 = FACE_OUTER_BOUND ( 'NONE', #61719, .T. ) ;
#50120 = CARTESIAN_POINT ( 'NONE',  ( 10.67826222744820086, 3.331419131587999960, -8.050725169876500331 ) ) ;
#50121 = CARTESIAN_POINT ( 'NONE',  ( 7.773264358664000007, -2.859518314699000197, 6.768377407145999669 ) ) ;
#50123 = CARTESIAN_POINT ( 'NONE',  ( 9.174722005181999762, -5.536248950452999473, -7.355084988757000453 ) ) ;
#50122 = VECTOR ( 'NONE', #54572, 1000.000000000000000 ) ;
#50124 = CARTESIAN_POINT ( 'NONE',  ( 25.18907900072800032, 11.36138750656000163, 3.216791237253000091 ) ) ;
#50125 = ORIENTED_EDGE ( 'NONE', *, *, #75, .T. ) ;
#50126 = CARTESIAN_POINT ( 'NONE',  ( 17.65075606732844449, 1.792616958745788525, -13.88476197432903092 ) ) ;
#50127 = CARTESIAN_POINT ( 'NONE',  ( 12.64343601369307279, 0.6040897852209334840, -13.88232707694115398 ) ) ;
#50128 = FACE_OUTER_BOUND ( 'NONE', #52579, .T. ) ;
#50129 = EDGE_CURVE ( 'NONE', #31174, #34088, #53080, .T. ) ;
#50130 = ADVANCED_FACE ( 'NONE', ( #21596 ), #21261, .T. ) ;
#50131 = CARTESIAN_POINT ( 'NONE',  ( 25.40545359959300242, -8.312255038417999842, -8.369389122269998538 ) ) ;
#50132 = CARTESIAN_POINT ( 'NONE',  ( 3.500000000000000000, -2.850358864693896432, 1.327510396322337138 ) ) ;
#50133 = FACE_OUTER_BOUND ( 'NONE', #48251, .T. ) ;
#50134 = CARTESIAN_POINT ( 'NONE',  ( 5.666085114159494118, 12.07002994274871099, -3.732314430517552850 ) ) ;
#50135 = ORIENTED_EDGE ( 'NONE', *, *, #30867, .F. ) ;
#50136 = EDGE_CURVE ( 'NONE', #34308, #12604, #15675, .T. ) ;
#50137 = CARTESIAN_POINT ( 'NONE',  ( 18.17999014114397482, 2.522019970189117277, -13.66878426939142877 ) ) ;
#50139 = VERTEX_POINT ( 'NONE', #43280 ) ;
#50138 = B_SPLINE_CURVE_WITH_KNOTS ( 'NONE', 3,
 ( #37454, #41670, #52851, #57740, #30842, #52153, #36425, #31197, #5294, #9851, #68569, #31877, #20691, #26973, #15450, #64011, #37118, #42021 ),
 .UNSPECIFIED., .F., .F.,
 ( 4, 2, 2, 2, 2, 2, 2, 2, 4 ),
 ( 0.000000000000000000, 0.1250000000000000000, 0.2500000000000000000, 0.3750000000000000000, 0.5000000000000000000, 0.6250000000000000000, 0.7500000000000000000, 0.8750000000000000000, 1.000000000000000000 ),
 .UNSPECIFIED. ) ;
#50140 = CARTESIAN_POINT ( 'NONE',  ( 11.09999999999999964, -4.000000000000000000, -7.500000000000000000 ) ) ;
#50141 = CARTESIAN_POINT ( 'NONE',  ( 9.893930206848997599, -5.250000000000000000, -7.500000000000000000 ) ) ;
#50142 = CARTESIAN_POINT ( 'NONE',  ( 9.500595280412998278, 2.334550724494000029, -7.977056617806000283 ) ) ;
#50143 = CARTESIAN_POINT ( 'NONE',  ( 23.99449523565688125, -12.72126087833753338, 3.481288081613541419 ) ) ;
#50144 = CARTESIAN_POINT ( 'NONE',  ( 11.42834208742529967, -4.706521750018099581, -8.610579932818998472 ) ) ;
#50145 = CARTESIAN_POINT ( 'NONE',  ( 17.93439305972981401, 0.4967428619047934979, -12.68692192486979486 ) ) ;
#50146 = CARTESIAN_POINT ( 'NONE',  ( 21.54999911806000057, -1.749711486808999826E-13, -3.819167204710999825E-14 ) ) ;
#50147 = ORIENTED_EDGE ( 'NONE', *, *, #44372, .F. ) ;
#50148 = CARTESIAN_POINT ( 'NONE',  ( 5.399998535875000449, -12.99045401563999924, -1.690592933733000125 ) ) ;
#50149 = CYLINDRICAL_SURFACE ( 'NONE', #36209, 1.500000000000000000 ) ;
#50150 = CARTESIAN_POINT ( 'NONE',  ( 17.94172469444382401, -2.002341272864497146, 13.76666224253383142 ) ) ;
#50151 = EDGE_LOOP ( 'NONE', ( #24152, #20565, #4058, #649, #3216, #18896 ) ) ;
#50152 = CARTESIAN_POINT ( 'NONE',  ( 10.90634530628000043, 3.089682683751000081, -6.534327427410000055 ) ) ;
#50153 = CYLINDRICAL_SURFACE ( 'NONE', #45439, 13.10000000000000142 ) ;
#50154 = VERTEX_POINT ( 'NONE', #26170 ) ;
#50155 = CARTESIAN_POINT ( 'NONE',  ( 10.13922949779699856, 4.633452903845899584, 6.550014196338999284 ) ) ;
#50156 = CARTESIAN_POINT ( 'NONE',  ( 18.23533704695771362, -2.231030541001939760, -12.40091240268597694 ) ) ;
#50157 = EDGE_CURVE ( 'NONE', #15157, #14563, #47733, .T. ) ;
#50158 = CARTESIAN_POINT ( 'NONE',  ( 9.393930206848999376, 2.750000000000000000, 7.500000000000000000 ) ) ;
#50159 = CARTESIAN_POINT ( 'NONE',  ( 23.50387503050299998, 0.000000000000000000, 0.000000000000000000 ) ) ;
#50160 = CARTESIAN_POINT ( 'NONE',  ( 23.56666365135700403, 2.920993777382001166, 11.72568747150000412 ) ) ;
#50161 = CARTESIAN_POINT ( 'NONE',  ( 9.003442991499998271, 3.945420918055940085, 8.365291319916600798 ) ) ;
#50162 = CARTESIAN_POINT ( 'NONE',  ( 9.354106685273835708, -3.367328683712668802, 9.120272287704549896 ) ) ;
#50163 = B_SPLINE_CURVE_WITH_KNOTS ( 'NONE', 3,
 ( #23229, #44575, #33380, #40009, #65519, #60632, #22877, #44227, #38971, #54697, #7486, #55044, #60980, #33031, #18335, #29178, #28131, #13092, #44909, #12396, #60289, #49446, #1555, #33727, #28839, #66213, #28483, #38616, #65867, #2254, #34427, #12047, #6446, #6794, #39311, #55739, #50485, #45252, #54343, #66558, #27796, #49103, #1215, #22527, #13778, #19357 ),
 .UNSPECIFIED., .F., .F.,
 ( 4, 2, 2, 2, 2, 1, 2, 2, 2, 1, 2, 2, 2, 2, 2, 2, 1, 2, 2, 1, 2, 2, 2, 2, 4 ),
 ( 0.4988098180369952006, 0.5301342044096829520, 0.5457963975960268277, 0.5614585907823708144, 0.5653741390789567278, 0.5692896873755427523, 0.5771207839687148011, 0.5927829771550601201, 0.6006140737482328351, 0.6084451703414054391, 0.6241073635277518683, 0.6397695567140984085, 0.6554317499004448377, 0.6710939430867912669, 0.6867561362731376962, 0.7024183294594841254, 0.7180805226458306656, 0.7494049090185193052, 0.7650671022048636249, 0.7807292953912079447, 0.8120536817638925875, 0.8433780681365772303, 0.8747024545092618730, 0.9373512272546309365, 1.000000000000000000 ),
 .UNSPECIFIED. ) ;
#50164 = ORIENTED_EDGE ( 'NONE', *, *, #48466, .F. ) ;
#50165 = CARTESIAN_POINT ( 'NONE',  ( 10.91307008594999850, 2.096286256021000050, 7.827189715349000210 ) ) ;
#50166 = CARTESIAN_POINT ( 'NONE',  ( 10.58470471959000037, 2.966809777448999874, -8.831980808885999679 ) ) ;
#50167 = CARTESIAN_POINT ( 'NONE',  ( 10.95345670791000003, -5.155055429684999524, -5.171522713314000264 ) ) ;
#50168 = CARTESIAN_POINT ( 'NONE',  ( 12.08613047971136467, 2.614761652440394268, -13.75367554324229680 ) ) ;
#50169 = CARTESIAN_POINT ( 'NONE',  ( 10.26693802597399952, -4.665064168510499876, -6.407263051216999017 ) ) ;
#50170 = CARTESIAN_POINT ( 'NONE',  ( 10.09196524370999981, -3.841385669346000231, 5.536421174581999338 ) ) ;
#50171 = CARTESIAN_POINT ( 'NONE',  ( 18.09636517151065860, 0.3125842563278199426, 13.89527356689843884 ) ) ;
#50172 = CARTESIAN_POINT ( 'NONE',  ( 17.72543224092255798, 0.6019432101436682503, 13.88245510389148230 ) ) ;
#50173 = B_SPLINE_CURVE_WITH_KNOTS ( 'NONE', 3,
 ( #14061, #51335, #13260, #24076, #7653, #12557, #44387, #60794, #45069, #18151, #3429, #67061 ),
 .UNSPECIFIED., .F., .F.,
 ( 4, 2, 2, 2, 2, 4 ),
 ( 0.000000000000000000, 0.2500000000000015543, 0.3750000000000009992, 0.5000000000000004441, 0.7500000000000002220, 1.000000000000000000 ),
 .UNSPECIFIED. ) ;
#50174 = ORIENTED_EDGE ( 'NONE', *, *, #22958, .T. ) ;
#50175 = ORIENTED_EDGE ( 'NONE', *, *, #29202, .T. ) ;
#50176 = CARTESIAN_POINT ( 'NONE',  ( 9.734454719592999794, 3.021734963141999852, -6.070209284876999511 ) ) ;
#50177 = CARTESIAN_POINT ( 'NONE',  ( 12.23478023522865321, -0.2564316839802910364, 13.89683092737489822 ) ) ;
#50178 = CARTESIAN_POINT ( 'NONE',  ( 12.22445506978716168, -2.731418685756656473, 13.62164890397837347 ) ) ;
#50179 = CARTESIAN_POINT ( 'NONE',  ( 9.393930206848999376, 2.750000000000000000, 7.500000000000000000 ) ) ;
#50180 = CARTESIAN_POINT ( 'NONE',  ( 7.293870559621999483, -3.416208448044999901, 6.162501393933999871 ) ) ;
#50181 = LINE ( 'NONE', #65557, #22614 ) ;
#50183 = DIRECTION ( 'NONE',  ( 1.000000000000000000, 0.000000000000000000, 0.000000000000000000 ) ) ;
#50182 = CARTESIAN_POINT ( 'NONE',  ( 10.71627973161000114, -3.885210315895700095, 8.774051692788999546 ) ) ;
#50184 = DIRECTION ( 'NONE',  ( 0.8480635683784220058, 0.000000000000000000, -0.5298945026977139872 ) ) ;
#50185 = VERTEX_POINT ( 'NONE', #11453 ) ;
#50186 = DIRECTION ( 'NONE',  ( 0.7070598748788616827, 0.000000000000000000, -0.7071536843828846175 ) ) ;
#50187 = CARTESIAN_POINT ( 'NONE',  ( 23.56666365135700403, -12.07812737769999245, -3.551569042642998664 ) ) ;
#50188 = EDGE_CURVE ( 'NONE', #29053, #37826, #51135, .T. ) ;
#50189 = EDGE_CURVE ( 'NONE', #59809, #18846, #283, .T. ) ;
#50190 = CARTESIAN_POINT ( 'NONE',  ( 11.09999999999999787, 5.584137149005704792, 7.273593798865315208 ) ) ;
#50191 = B_SPLINE_SURFACE_WITH_KNOTS ( 'NONE', 3, 3, ( 
 ( #47538, #63939, #43321, #58703, #64625, #59734, #27583, #65318, #48909, #17434, #16733, #22325, #49243, #1017, #64964, #37381, #16050, #42971, #6241, #38763, #48564, #11487, #59051, #53801, #21980, #5898, #11835, #38062, #42629, #59387, #43667, #10806, #32827, #32150, #54143 ),
 ( #26901, #17078, #64278, #1353, #32488, #22670, #48213, #33175, #44014, #26556, #38410, #53466, #5559, #54492, #6593, #27934, #10460, #53118, #5220, #31802, #47883, #69187, #21299, #320, #21636, #16395, #37722, #11153, #27240, #668, #55879, #1700, #18823, #23019, #40149 ),
 ( #39453, #29671, #34216, #29318, #56218, #2052, #66008, #61124, #60431, #49941, #33522, #34902, #28272, #13582, #13241, #28980, #55536, #60772, #18131, #45390, #7633, #49592, #23371, #50287, #44711, #2732, #12887, #2388, #23712, #24057, #7985, #45733, #50974, #45047, #33868 ),
 ( #39800, #7288, #28628, #8328, #17789, #66355, #39107, #12539, #54841, #60088, #3070, #18474, #34566, #44367, #66701, #50631, #12194, #61463, #24403, #67042, #6937, #65666, #19152, #55183, #68403, #20526, #51652, #4780, #68065, #20181, #57937, #8668, #68754, #14263, #19502 ) ),
 .UNSPECIFIED., .F., .F., .F.,
 ( 4, 4 ),
 ( 4, 1, 1, 1, 1, 1, 1, 1, 1, 1, 1, 1, 1, 1, 1, 1, 1, 1, 1, 1, 1, 1, 1, 1, 1, 1, 1, 1, 1, 1, 1, 1, 4 ),
 ( -0.1039086239011999951, 1.103908623900999864 ),
 ( -0.01735257130020999988, 0.01084535706264999969, 0.03904328542550000031, 0.06724121378835999641, 0.09543914215121999944, 0.1236370705141000004, 0.1518349988768999959, 0.1800329272397999947, 0.2082308556026999935, 0.2364287839655000167, 0.2646267123283999601, 0.2928246406912000110, 0.3210225690540999821, 0.3492204974169000331, 0.3774184257798000042, 0.4056163541427000307, 0.4338142825054999707, 0.4620122108683999973, 0.4902101392311999928, 0.5184080675940999638, 0.5466059959569999904, 0.5748039243197999859, 0.6030018526827000125, 0.6311997810455000080, 0.6593977094084000345, 0.6875956377712000300, 0.7157935661340999456, 0.7439914944969999722, 0.7721894228597999676, 0.8003873512226999942, 0.8285852795854999897, 0.8567832079484000163, 0.8849811363112999318 ),
 .UNSPECIFIED. ) ;
#50192 = CARTESIAN_POINT ( 'NONE',  ( 12.21931228141710690, -0.2190605493744586796, 12.69747807323868116 ) ) ;
#50193 = CARTESIAN_POINT ( 'NONE',  ( 18.15011306042656969, -2.691200174357349706, -12.40496142758472509 ) ) ;
#50194 = ORIENTED_EDGE ( 'NONE', *, *, #24702, .F. ) ;
#50196 = CARTESIAN_POINT ( 'NONE',  ( 12.61270316628418975, -1.780234759020672852, -12.47365767676673798 ) ) ;
#50195 = CARTESIAN_POINT ( 'NONE',  ( 11.09999999999999964, 5.350000000000000533, 7.500000000000000000 ) ) ;
#50197 = CARTESIAN_POINT ( 'NONE',  ( 9.500595280412998278, 2.334550724494000029, -7.977056617806000283 ) ) ;
#50198 = CARTESIAN_POINT ( 'NONE',  ( 12.39034978066174197, -2.032288297489023066, 13.76160266677045740 ) ) ;
#50199 = CIRCLE ( 'NONE', #26739, 0.7499999936418002555 ) ;
#50200 = CARTESIAN_POINT ( 'NONE',  ( 10.69041504065829962, 5.024558373595999328, 8.263934892306599167 ) ) ;
#50201 = B_SPLINE_SURFACE_WITH_KNOTS ( 'NONE', 3, 3, ( 
 ( #17362, #1284, #6519, #60356, #49516, #44977, #12464, #50559, #23302, #23987, #27864, #49173, #33798, #22598, #43942, #55114, #35175, #56488, #25699, #35850, #25354, #8593, #14188, #20112, #24332, #35516, #45664, #19772, #19077, #30273, #41097, #36191, #29943, #62413, #8936 ),
 ( #51246, #47031, #34832, #3341, #13847, #57167, #24676, #9264, #56143, #61391, #45996, #67308, #18750, #41441, #51579, #62749, #14534, #30606, #56838, #51920, #19426, #62072, #40748, #3673, #4017, #46693, #25015, #46346, #14868, #67647, #67996, #40082, #57503, #9612, #30956 ),
 ( #52269, #4365, #13512, #8252, #29599, #50902, #2999, #66970, #40404, #61727, #48400, #68682, #10647, #163, #16584, #15562, #21479, #58541, #15209, #53305, #68334, #37560, #27086, #43155, #42133, #41780, #5742, #37224, #31993, #36887, #32337, #36536, #63781, #20453, #63085 ),
 ( #10996, #5408, #42814, #47723, #42474, #5059, #58203, #64122, #16236, #26396, #10306, #21822, #69035, #53646, #57861, #31640, #48060, #26744, #507, #58893, #21147, #9964, #47379, #15893, #27425, #59229, #31301, #11331, #52611, #64461, #37908, #32673, #53986, #20800, #4705 ) ),
 .UNSPECIFIED., .F., .F., .F.,
 ( 4, 4 ),
 ( 4, 1, 1, 1, 1, 1, 1, 1, 1, 1, 1, 1, 1, 1, 1, 1, 1, 1, 1, 1, 1, 1, 1, 1, 1, 1, 1, 1, 1, 1, 1, 1, 4 ),
 ( -0.1039086239011999951, 1.103908623900999864 ),
 ( -0.01735257130020999988, 0.01084535706264999969, 0.03904328542550000031, 0.06724121378835999641, 0.09543914215121999944, 0.1236370705141000004, 0.1518349988768999959, 0.1800329272397999947, 0.2082308556026999935, 0.2364287839655000167, 0.2646267123283999601, 0.2928246406912000110, 0.3210225690540999821, 0.3492204974169000331, 0.3774184257798000042, 0.4056163541427000307, 0.4338142825054999707, 0.4620122108683999973, 0.4902101392311999928, 0.5184080675940999638, 0.5466059959569999904, 0.5748039243197999859, 0.6030018526827000125, 0.6311997810455000080, 0.6593977094084000345, 0.6875956377712000300, 0.7157935661340999456, 0.7439914944969999722, 0.7721894228597999676, 0.8003873512226999942, 0.8285852795854999897, 0.8567832079484000163, 0.8849811363112999318 ),
 .UNSPECIFIED. ) ;
#50202 = CARTESIAN_POINT ( 'NONE',  ( 5.500000000000000000, -0.2500000000000000000, -3.149999999999999911 ) ) ;
#50203 = CARTESIAN_POINT ( 'NONE',  ( 2.642974601824000125, 3.419206998487000160, 1.101304841644999977 ) ) ;
#50204 = ORIENTED_EDGE ( 'NONE', *, *, #68078, .T. ) ;
#50205 = CARTESIAN_POINT ( 'NONE',  ( 12.08032332909579765, 0.02297882141077639551, -12.59998453421652442 ) ) ;
#50206 = DIRECTION ( 'NONE',  ( 1.000000000000000000, 0.000000000000000000, 0.000000000000000000 ) ) ;
#50207 = CYLINDRICAL_SURFACE ( 'NONE', #28678, 1.050000000000000044 ) ;
#50208 = CARTESIAN_POINT ( 'NONE',  ( 11.59999999999999964, -4.000000000000000000, -7.500000000000000000 ) ) ;
#50209 = ORIENTED_EDGE ( 'NONE', *, *, #67775, .T. ) ;
#50210 = CARTESIAN_POINT ( 'NONE',  ( 6.299764545682999817, -1.121550593885000113, 0.3539842735925000095 ) ) ;
#50211 = CARTESIAN_POINT ( 'NONE',  ( 10.92974439901735906, 9.483709363500846479, 6.097296706918701403 ) ) ;
#50213 = CARTESIAN_POINT ( 'NONE',  ( 7.890669420221000152, 4.660296061153999858, 6.322498784873999078 ) ) ;
#50212 = DIRECTION ( 'NONE',  ( 0.000000000000000000, -0.9421243786071880066, -0.3352635608502960718 ) ) ;
#50214 = CARTESIAN_POINT ( 'NONE',  ( 12.80505043854143388, 1.798940460745208636, 12.50936912696000469 ) ) ;
#50215 = ORIENTED_EDGE ( 'NONE', *, *, #1738, .F. ) ;
#50216 = EDGE_CURVE ( 'NONE', #56969, #64650, #37004, .T. ) ;
#50217 = DIRECTION ( 'NONE',  ( 1.000000000000000000, 0.000000000000000000, 0.000000000000000000 ) ) ;
#50218 = VERTEX_POINT ( 'NONE', #59015 ) ;
#50219 = CARTESIAN_POINT ( 'NONE',  ( 9.458880069675531743, -5.224811350022368295, 8.067608271712991552 ) ) ;
#50220 = CARTESIAN_POINT ( 'NONE',  ( 16.18329442974999921, 3.298233714334000144, 11.32377282473999891 ) ) ;
#50221 = CARTESIAN_POINT ( 'NONE',  ( 18.26375728754769767, -0.1544074001204070734, -13.99915345895492003 ) ) ;
#50222 = ORIENTED_EDGE ( 'NONE', *, *, #12185, .F. ) ;
#50223 = CARTESIAN_POINT ( 'NONE',  ( 10.98803924503897989, 7.901889936912171564, -6.474652332642743424 ) ) ;
#50224 = CARTESIAN_POINT ( 'NONE',  ( 10.85685100254000091, 2.832432432432000269, -6.822293592207000934 ) ) ;
#50225 = CARTESIAN_POINT ( 'NONE',  ( 11.09999999999999964, -2.649999999999999911, -7.500000000000000000 ) ) ;
#50226 = CARTESIAN_POINT ( 'NONE',  ( 9.051550650638001017, -2.899999999999999911, 6.227445478845999638 ) ) ;
#50227 = CARTESIAN_POINT ( 'NONE',  ( 18.14658900058367408, -2.701839613306171728, 12.40227423849764321 ) ) ;
#50228 = ORIENTED_EDGE ( 'NONE', *, *, #48157, .F. ) ;
#50229 = CARTESIAN_POINT ( 'NONE',  ( 8.999999695565000124, -12.49999969551000056, 3.568600202703999990E-10 ) ) ;
#50230 = CARTESIAN_POINT ( 'NONE',  ( 24.08756612923799878, -12.68456084474000001, -3.366943214815000029 ) ) ;
#50231 = CARTESIAN_POINT ( 'NONE',  ( 10.97763601423218027, 5.200850044898188251, 6.714742154986239164 ) ) ;
#50232 = FACE_OUTER_BOUND ( 'NONE', #19362, .T. ) ;
#50233 = ORIENTED_EDGE ( 'NONE', *, *, #39725, .F. ) ;
#50234 = CARTESIAN_POINT ( 'NONE',  ( 10.43353630809276922, -2.899999999999999911, -6.665341197409489382 ) ) ;
#50235 = EDGE_CURVE ( 'NONE', #68269, #16464, #59412, .T. ) ;
#50236 = CARTESIAN_POINT ( 'NONE',  ( 8.962753061708914615, -5.112753122729035482, -7.353476507976679954 ) ) ;
#50237 = FACE_OUTER_BOUND ( 'NONE', #43741, .T. ) ;
#50238 = CARTESIAN_POINT ( 'NONE',  ( 10.17905590578999941, -2.899999999999999911, 6.571291218949999902 ) ) ;
#50239 = CARTESIAN_POINT ( 'NONE',  ( 6.928038431245999718, -9.243192864701999412, 5.233546977967000302 ) ) ;
#50240 = CARTESIAN_POINT ( 'NONE',  ( 12.34820889858482396, -0.4270206790917092654, -13.89118144889037509 ) ) ;
#50241 = CARTESIAN_POINT ( 'NONE',  ( 17.68813047654961323, -3.110753822336481011, 12.28807462416255092 ) ) ;
#50242 = ORIENTED_EDGE ( 'NONE', *, *, #25983, .T. ) ;
#50243 = CARTESIAN_POINT ( 'NONE',  ( 11.02812378248509795, -4.416893162838900544, -6.711274001288999536 ) ) ;
#50244 = ORIENTED_EDGE ( 'NONE', *, *, #48695, .F. ) ;
#50245 = CONICAL_SURFACE ( 'NONE', #31278, 12.37499919541000004, 0.7853980884875938484 ) ;
#50246 = B_SPLINE_CURVE_WITH_KNOTS ( 'NONE', 3,
 ( #51075, #23469, #8427, #13340 ),
 .UNSPECIFIED., .F., .F.,
 ( 4, 4 ),
 ( 0.8746253901980668433, 1.000000000000000000 ),
 .UNSPECIFIED. ) ;
#50247 = CARTESIAN_POINT ( 'NONE',  ( 0.1499942179679999987, -1.689975037551099124, 2.199046806507070517 ) ) ;
#50248 = CARTESIAN_POINT ( 'NONE',  ( 9.345514158774999913, 5.775964236216999836, -8.174909295649001706 ) ) ;
#50249 = CARTESIAN_POINT ( 'NONE',  ( 2.831737797580999860, 1.751601373051000055, 2.696006073548000259 ) ) ;
#50250 = CARTESIAN_POINT ( 'NONE',  ( 9.792315001194999979, -4.284154785471999460, -9.000488933596999530 ) ) ;
#50251 = CARTESIAN_POINT ( 'NONE',  ( 6.740199140016398971, 0.1957492585445249622, -1.505191492485322913 ) ) ;
#50252 = CARTESIAN_POINT ( 'NONE',  ( 8.227131012390005438, 3.380163391545999207, -6.126525137394006393 ) ) ;
#50253 = DIRECTION ( 'NONE',  ( -1.000000000000000000, 0.000000000000000000, 0.000000000000000000 ) ) ;
#50254 = ORIENTED_EDGE ( 'NONE', *, *, #47518, .F. ) ;
#50255 = CARTESIAN_POINT ( 'NONE',  ( 18.05609597790000009, 3.343430715100999873, 11.12052764821000039 ) ) ;
#50256 = CARTESIAN_POINT ( 'NONE',  ( 11.24795391537420031, -3.169881940022800215, 6.936213817702099327 ) ) ;
#50257 = CARTESIAN_POINT ( 'NONE',  ( 10.75109581085999899, 2.822145500011000063, 6.655897464539000552 ) ) ;
#50258 = CARTESIAN_POINT ( 'NONE',  ( 10.69839231854608563, -4.679932939043313311, -8.679767489841967887 ) ) ;
#50259 = CARTESIAN_POINT ( 'NONE',  ( 24.44496350777200178, -12.03536639536000052, -3.224849854974999985 ) ) ;
#50260 = CYLINDRICAL_SURFACE ( 'NONE', #3839, 1.350000000000000089 ) ;
#50261 = CARTESIAN_POINT ( 'NONE',  ( 11.58487348028854846, 3.117292544139400157, -7.977261354519500358 ) ) ;
#50262 = CARTESIAN_POINT ( 'NONE',  ( 24.67559771067699970, -12.15673408770999941, 3.025797809546999950 ) ) ;
#50263 = CARTESIAN_POINT ( 'NONE',  ( 9.226430433046999724, 3.028322657068899915, -6.900352112302299723 ) ) ;
#50264 = EDGE_CURVE ( 'NONE', #46125, #38406, #18689, .T. ) ;
#50265 = EDGE_CURVE ( 'NONE', #66927, #35108, #29407, .T. ) ;
#50266 = CARTESIAN_POINT ( 'NONE',  ( 11.40000482165000228, 7.371880883511000048E-13, 4.000966224993000022E-14 ) ) ;
#50267 = CARTESIAN_POINT ( 'NONE',  ( 24.56046482271400322, 3.658438515550000325, 12.32938606307999940 ) ) ;
#50268 = CARTESIAN_POINT ( 'NONE',  ( 8.128093775834376089, 4.971510557325522939, -6.368084714047306250 ) ) ;
#50269 = CARTESIAN_POINT ( 'NONE',  ( 11.14451084122999980, 5.035416949823999566, -8.381520599479999944 ) ) ;
#50270 = ORIENTED_EDGE ( 'NONE', *, *, #31881, .T. ) ;
#50271 = CARTESIAN_POINT ( 'NONE',  ( 9.106129440379998385, -4.192917962110999319, 5.525484568403999930 ) ) ;
#50272 = ADVANCED_FACE ( 'NONE', ( #59351 ), #4885, .F. ) ;
#50273 = EDGE_CURVE ( 'NONE', #30098, #13517, #14570, .T. ) ;
#50274 = CARTESIAN_POINT ( 'NONE',  ( 18.23381869303822356, 2.775531333002567713, 13.72213247881303033 ) ) ;
#50275 = CARTESIAN_POINT ( 'NONE',  ( 23.59425252148539087, 3.210776961502446181, 13.60476513765082451 ) ) ;
#50276 = CARTESIAN_POINT ( 'NONE',  ( 11.15810538575740019, -2.757018958839999812, -7.202822423614300362 ) ) ;
#50277 = EDGE_LOOP ( 'NONE', ( #61359, #64054, #38440, #68494 ) ) ;
#50278 = CARTESIAN_POINT ( 'NONE',  ( 8.411454719592999396, 3.882020551409000042, 5.870058896428999695 ) ) ;
#50279 = CIRCLE ( 'NONE', #55869, 12.99999867215000116 ) ;
#50281 = CARTESIAN_POINT ( 'NONE',  ( 9.198396402459000143, -4.369105567410300317, 6.701746336527099501 ) ) ;
#50280 = CARTESIAN_POINT ( 'NONE',  ( 8.944760841233000193, 4.990139824845000405, -9.121472988377998803 ) ) ;
#50282 = DIRECTION ( 'NONE',  ( -1.000000000000000000, 0.000000000000000000, 0.000000000000000000 ) ) ;
#50283 = EDGE_LOOP ( 'NONE', ( #37215, #51305, #42240, #32738 ) ) ;
#50284 = CARTESIAN_POINT ( 'NONE',  ( 10.78089701270000056, 5.735299658853000082, 7.801561896854000366 ) ) ;
#50285 = CARTESIAN_POINT ( 'NONE',  ( 17.99827832423969909, -3.095912246742690499, -13.65340184222058184 ) ) ;
#50286 = CARTESIAN_POINT ( 'NONE',  ( 11.69559063708295987, 5.086518862378000883, 7.194517870904999945 ) ) ;
#50287 = CARTESIAN_POINT ( 'NONE',  ( 10.55813551225999980, -2.466564559586000183, 6.633531786299999844 ) ) ;
#50288 = DIRECTION ( 'NONE',  ( 1.000000000000000000, 0.000000000000000000, 0.000000000000000000 ) ) ;
#50289 = ORIENTED_EDGE ( 'NONE', *, *, #33056, .F. ) ;
#50290 = DIRECTION ( 'NONE',  ( 0.000000000000000000, 0.000000000000000000, -1.000000000000000000 ) ) ;
#50291 = B_SPLINE_CURVE_WITH_KNOTS ( 'NONE', 3,
 ( #18999, #62335, #66887, #56408, #46611, #18661 ),
 .UNSPECIFIED., .F., .F.,
 ( 4, 2, 4 ),
 ( 0.000000000000000000, 0.5000000000000000000, 1.000000000000000000 ),
 .UNSPECIFIED. ) ;
#50292 = EDGE_CURVE ( 'NONE', #46963, #57158, #66106, .T. ) ;
#50293 = CARTESIAN_POINT ( 'NONE',  ( 1.334306799207999994, -1.762666431298145708, -3.058252359239904461 ) ) ;
#50294 = AXIS2_PLACEMENT_3D ( 'NONE', #29751, #19231, #39885 ) ;
#50295 = CARTESIAN_POINT ( 'NONE',  ( 8.056002428396427106, -3.587487886595424058, 5.808910377708588868 ) ) ;
#50296 = CARTESIAN_POINT ( 'NONE',  ( 10.80815535238000002, -2.937528991339000140, 8.948455587554001056 ) ) ;
#50297 = CARTESIAN_POINT ( 'NONE',  ( 11.17901463001529905, -3.302889347096799710, -6.383488688482000128 ) ) ;
#50298 = CARTESIAN_POINT ( 'NONE',  ( 9.349455549952999434, -3.218304396998100003, 8.130709350565298976 ) ) ;
#50299 = EDGE_LOOP ( 'NONE', ( #68252, #33537, #17120, #11965 ) ) ;
#50300 = CARTESIAN_POINT ( 'NONE',  ( 24.72250368810516363, -11.76899691939735781, -3.190821781878062424 ) ) ;
#50301 = B_SPLINE_CURVE_WITH_KNOTS ( 'NONE', 3,
 ( #46816, #68121, #58328, #20240, #36319, #57636 ),
 .UNSPECIFIED., .F., .F.,
 ( 4, 2, 4 ),
 ( 0.000000000000000000, 0.3041826760188173218, 0.6083653520376346435 ),
 .UNSPECIFIED. ) ;
#50302 = CARTESIAN_POINT ( 'NONE',  ( 11.16995391537419913, -3.056324258617099776, 6.859089544950699668 ) ) ;
#50303 = ORIENTED_EDGE ( 'NONE', *, *, #34943, .T. ) ;
#50304 = CARTESIAN_POINT ( 'NONE',  ( 12.80505043854144276, -0.6250000000000001110, -13.88107975066922428 ) ) ;
#50305 = ORIENTED_EDGE ( 'NONE', *, *, #55322, .F. ) ;
#50306 = CARTESIAN_POINT ( 'NONE',  ( 9.971744136172999262, -5.176458967229000230, -8.738385553646999426 ) ) ;
#50307 = CARTESIAN_POINT ( 'NONE',  ( 9.143660841233000269, 2.235961884443999459, -6.794506518623999902 ) ) ;
#50308 = CARTESIAN_POINT ( 'NONE',  ( -0.2999999999999999889, 0.000000000000000000, 0.000000000000000000 ) ) ;
#50309 = CARTESIAN_POINT ( 'NONE',  ( 11.00000000058999916, -1.300000000000000044, -9.662944685757000940 ) ) ;
#50310 = CARTESIAN_POINT ( 'NONE',  ( 12.15423239032306668, 2.797846099084077665, -12.28544569950199516 ) ) ;
#50311 = CARTESIAN_POINT ( 'NONE',  ( 11.86333594839950045, -3.340240242524600056, 8.256087240512899328 ) ) ;
#50312 = CARTESIAN_POINT ( 'NONE',  ( 11.86056039236529891, -3.108928759355700233, 7.456633480985620288 ) ) ;
#50313 = ORIENTED_EDGE ( 'NONE', *, *, #69128, .T. ) ;
#50314 = CARTESIAN_POINT ( 'NONE',  ( 9.739763540183334456, 3.672815144550903632, 8.717465845835395299 ) ) ;
#50315 = ORIENTED_EDGE ( 'NONE', *, *, #20598, .T. ) ;
#50316 = CARTESIAN_POINT ( 'NONE',  ( 7.828418146791999099, -5.524126964933000927, 6.910359834012999691 ) ) ;
#50317 = CARTESIAN_POINT ( 'NONE',  ( 25.60000000000000142, -8.527654132749999505, 7.260537518967999482 ) ) ;
#50318 = ORIENTED_EDGE ( 'NONE', *, *, #48527, .F. ) ;
#50319 = CARTESIAN_POINT ( 'NONE',  ( 12.21223476585298862, -2.065380716993684196, -12.42958554107382163 ) ) ;
#50320 = CARTESIAN_POINT ( 'NONE',  ( 10.35410941423799791, 4.742797679580299963, 8.174686939644999484 ) ) ;
#50321 = EDGE_CURVE ( 'NONE', #61617, #10663, #19352, .T. ) ;
#50322 = CARTESIAN_POINT ( 'NONE',  ( 10.30480805961999913, -5.828319785709999756, -7.226592660401000678 ) ) ;
#50323 = CARTESIAN_POINT ( 'NONE',  ( 6.482109839683335650, -0.9218200799623778030, 1.199500263597266914 ) ) ;
#50324 = CARTESIAN_POINT ( 'NONE',  ( 18.07669116111300056, -11.89294021643999955, 3.415331764990000352 ) ) ;
#50325 = CARTESIAN_POINT ( 'NONE',  ( 12.80505043854146940, -1.875000000000000444, -25.00000000000000000 ) ) ;
#50326 = CARTESIAN_POINT ( 'NONE',  ( 12.26307976823776968, -2.811936524129938331, -13.60229516772050040 ) ) ;
#50327 = CARTESIAN_POINT ( 'NONE',  ( 18.11574795581002562, -0.2761699508452428176, -12.69595998167825357 ) ) ;
#50328 = EDGE_CURVE ( 'NONE', #44831, #18982, #1105, .T. ) ;
#50329 = CARTESIAN_POINT ( 'NONE',  ( 10.83810672858429847, -5.021298157087000114, -6.731711997412900494 ) ) ;
#50330 = CARTESIAN_POINT ( 'NONE',  ( 9.214142219592000416, 5.421534627450999899, 6.381126373995999579 ) ) ;
#50331 = VERTEX_POINT ( 'NONE', #43197 ) ;
#50332 =( NAMED_UNIT ( * ) SI_UNIT ( $, .STERADIAN. ) SOLID_ANGLE_UNIT ( ) );
#50333 = CARTESIAN_POINT ( 'NONE',  ( 8.445434020356069382, -4.175608670059299143, 6.000036809310114627 ) ) ;
#50334 = CARTESIAN_POINT ( 'NONE',  ( 10.57314899745999881, -5.167567567567999731, -6.822293592207000934 ) ) ;
#50335 = CARTESIAN_POINT ( 'NONE',  ( 23.55360225935400109, -3.060278671086000379, 13.69502875873999947 ) ) ;
#50336 = AXIS2_PLACEMENT_3D ( 'NONE', #68198, #37771, #54190 ) ;
#50337 = CARTESIAN_POINT ( 'NONE',  ( 18.14814637199130232, 2.302603452852429733, 12.49536313902244622 ) ) ;
#50338 = CARTESIAN_POINT ( 'NONE',  ( 11.12484647810999938, 5.434130742615000287, 5.164716346185000972 ) ) ;
#50339 = CARTESIAN_POINT ( 'NONE',  ( 11.14698693981000055, 5.129806801114000336, 5.886034047559999927 ) ) ;
#50340 = AXIS2_PLACEMENT_3D ( 'NONE', #49382, #12335, #59532 ) ;
#50341 = CARTESIAN_POINT ( 'NONE',  ( 27.64127793187000037, 2.399999999999999911, 6.571291218949999902 ) ) ;
#50342 = CARTESIAN_POINT ( 'NONE',  ( 12.44006281454390717, -0.6285461057554440067, -12.58436427553342618 ) ) ;
#50343 = ORIENTED_EDGE ( 'NONE', *, *, #61893, .F. ) ;
#50344 = CARTESIAN_POINT ( 'NONE',  ( 12.31295406811165449, -2.114551508724276108, 12.53308940647968939 ) ) ;
#50345 = CARTESIAN_POINT ( 'NONE',  ( 10.00760887879199856, -4.196341783741199372, -6.655513263298900029 ) ) ;
#50346 = CARTESIAN_POINT ( 'NONE',  ( 10.25888757983999966, 4.512388525173999909, 5.993701490107000929 ) ) ;
#50347 = VECTOR ( 'NONE', #65408, 1000.000000000000000 ) ;
#50348 = CARTESIAN_POINT ( 'NONE',  ( 9.333766445374624965, 2.750000000000000444, 7.659651991919251834 ) ) ;
#50349 = CARTESIAN_POINT ( 'NONE',  ( 10.84226088462129844, 4.002427228022017225, -6.359261544073000039 ) ) ;
#50350 = CARTESIAN_POINT ( 'NONE',  ( 12.57519818727761596, 0.5812897767837151841, 12.68208758371477352 ) ) ;
#50351 = CARTESIAN_POINT ( 'NONE',  ( 9.385308886257000438, 4.135077451221000011, 9.175524215473998879 ) ) ;
#50352 = CARTESIAN_POINT ( 'NONE',  ( 10.76685100253999927, 2.832432432432000269, 6.822293592207000934 ) ) ;
#50353 = CARTESIAN_POINT ( 'NONE',  ( 8.832537864289999874, -2.899999999999999911, 6.571291218949999902 ) ) ;
#50354 = ORIENTED_EDGE ( 'NONE', *, *, #67687, .T. ) ;
#50355 = CARTESIAN_POINT ( 'NONE',  ( 8.649364158774000444, 3.038023536984999939, -5.861661709981000001 ) ) ;
#50356 = CARTESIAN_POINT ( 'NONE',  ( 11.01041369783139956, 3.935522326596939902, -8.776385133971000840 ) ) ;
#50357 = EDGE_CURVE ( 'NONE', #61329, #64377, #1032, .T. ) ;
#50358 = EDGE_CURVE ( 'NONE', #64677, #21396, #16276, .T. ) ;
#50359 = CARTESIAN_POINT ( 'NONE',  ( 23.66004879239100234, 0.000000000000000000, 0.000000000000000000 ) ) ;
#50361 = CARTESIAN_POINT ( 'NONE',  ( 24.98034512773276816, 11.50384160472775896, 3.228646524593837608 ) ) ;
#50360 = CARTESIAN_POINT ( 'NONE',  ( 25.30000327618300204, 10.36736154742121130, 5.168041346173475326 ) ) ;
#50362 = CARTESIAN_POINT ( 'NONE',  ( 10.46393802597400047, -4.522194782554399772, 8.357994702431799539 ) ) ;
#50363 = CARTESIAN_POINT ( 'NONE',  ( 10.80133863405319872, -3.465595476214000215, -8.181696703306599261 ) ) ;
#50364 = ORIENTED_EDGE ( 'NONE', *, *, #27928, .F. ) ;
#50365 = CARTESIAN_POINT ( 'NONE',  ( 2.073158326185999822, -2.059315964850999769, -2.525946829712999886 ) ) ;
#50366 = CARTESIAN_POINT ( 'NONE',  ( 17.97862686927833309, -0.4596875344175958000, -12.68880368817494642 ) ) ;
#50367 = CARTESIAN_POINT ( 'NONE',  ( 0.7431103717477000048, 2.848815883361000001, -1.248255999701999963 ) ) ;
#50368 = DIRECTION ( 'NONE',  ( 1.000000000000000000, 0.000000000000000000, 0.000000000000000000 ) ) ;
#50369 = CARTESIAN_POINT ( 'NONE',  ( 24.43232361760200178, -11.98245802077999933, 3.250304477315000273 ) ) ;
#50370 = CARTESIAN_POINT ( 'NONE',  ( 17.57587252603351402, -1.875000554927097607, -13.78627161177572269 ) ) ;
#50371 = CARTESIAN_POINT ( 'NONE',  ( 4.599999999999999645, -0.7192913403693006469, 12.57945229203838444 ) ) ;
#50372 = FACE_OUTER_BOUND ( 'NONE', #34869, .T. ) ;
#50373 = CARTESIAN_POINT ( 'NONE',  ( 7.930984150159567037, 5.149131057101222986, 6.790530764775851935 ) ) ;
#50374 = ORIENTED_EDGE ( 'NONE', *, *, #31061, .T. ) ;
#50375 = VECTOR ( 'NONE', #136, 1000.000000000000227 ) ;
#50376 = CARTESIAN_POINT ( 'NONE',  ( 7.416892219589999335, 3.448180532882000104, 9.222462917385000125 ) ) ;
#50377 = ADVANCED_FACE ( 'NONE', ( #26433 ), #4402, .F. ) ;
#50378 = CARTESIAN_POINT ( 'NONE',  ( 11.13224000276999881, 5.320481470723000150, 4.955559672663000015 ) ) ;
#50379 = CARTESIAN_POINT ( 'NONE',  ( 17.55505043854143565, 1.875000000000000000, -13.78631952119025073 ) ) ;
#50380 = CARTESIAN_POINT ( 'NONE',  ( 6.899999691988000450, -12.20988339176000004, 3.111064831549000154 ) ) ;
#50381 = CARTESIAN_POINT ( 'NONE',  ( 0.6513362521023000618, 3.284885639805000146, 1.453889781857000019 ) ) ;
#50382 = ORIENTED_EDGE ( 'NONE', *, *, #66834, .F. ) ;
#50383 = CARTESIAN_POINT ( 'NONE',  ( 1.959306799206333105, 3.058252359239905793, -1.762666431298143488 ) ) ;
#50384 = CARTESIAN_POINT ( 'NONE',  ( 10.90437023801000116, -5.099522774867000230, 5.132565236215000049 ) ) ;
#50385 = CARTESIAN_POINT ( 'NONE',  ( 10.01533268956000100, 4.946987614118000032, 8.559212393557999121 ) ) ;
#50386 = CARTESIAN_POINT ( 'NONE',  ( 10.62487750876920067, 3.456442671114800191, 6.656497609330299881 ) ) ;
#50388 = CARTESIAN_POINT ( 'NONE',  ( 11.00000000000000000, -5.058572498595999889, -7.825000000000000178 ) ) ;
#50387 = VECTOR ( 'NONE', #34442, 1000.000000000000114 ) ;
#50389 = CARTESIAN_POINT ( 'NONE',  ( 10.23580444037999904, -3.621838308198000345, -8.806219190581000333 ) ) ;
#50390 = CARTESIAN_POINT ( 'NONE',  ( 17.55505043854143921, 0.7302158263239199032, -13.98094363220830871 ) ) ;
#50391 = CARTESIAN_POINT ( 'NONE',  ( 24.44917776433500123, 12.41482580133999924, 3.103222239774000357 ) ) ;
#50392 = CARTESIAN_POINT ( 'NONE',  ( 12.18033843151457063, -2.521515055314785592, 12.44655896212852930 ) ) ;
#50393 = CARTESIAN_POINT ( 'NONE',  ( 7.787671094692007578, 4.786296140223255335, 9.071322605277833517 ) ) ;
#50394 = EDGE_LOOP ( 'NONE', ( #60503, #47905, #56575, #28560 ) ) ;
#50395 = CARTESIAN_POINT ( 'NONE',  ( 18.14566850323243230, -2.942004589604671150, 13.68740344564952416 ) ) ;
#50396 = CARTESIAN_POINT ( 'NONE',  ( 10.73964560330029983, -3.608363763633400279, -6.283473206644000442 ) ) ;
#50397 = ORIENTED_EDGE ( 'NONE', *, *, #8467, .T. ) ;
#50398 = MANIFOLD_SOLID_BREP ( 'Stock-MAS-678-1', #29199 ) ;
#50399 = CARTESIAN_POINT ( 'NONE',  ( 8.975133088423635996, -5.349981448246158955, 7.499992563499107590 ) ) ;
#50400 = CARTESIAN_POINT ( 'NONE',  ( 10.90000000000000036, -8.618205959414002137, 7.308661029293999967 ) ) ;
#50401 = DIRECTION ( 'NONE',  ( -1.000000000000000000, 0.000000000000000000, 0.000000000000000000 ) ) ;
#50402 = CARTESIAN_POINT ( 'NONE',  ( 10.61094409420999973, 5.100000000000000533, -6.571291218949999902 ) ) ;
#50403 = CARTESIAN_POINT ( 'NONE',  ( 11.02286749330999882, 2.398743616553999924, 6.352468982205000891 ) ) ;
#50404 = CARTESIAN_POINT ( 'NONE',  ( 10.80159548023000049, 2.805082485475999476, -8.157276499959001725 ) ) ;
#50405 = CARTESIAN_POINT ( 'NONE',  ( 9.727263540182331525, -3.370476274536371442, -6.407767014557179230 ) ) ;
#50406 = CARTESIAN_POINT ( 'NONE',  ( 11.35180279716000129, 3.678144743825999985, -11.20807767738999949 ) ) ;
#50407 = EDGE_CURVE ( 'NONE', #48584, #523, #41888, .T. ) ;
#50408 = CARTESIAN_POINT ( 'NONE',  ( 10.32701825126999928, -5.663784181836000187, -6.682035927671000408 ) ) ;
#50409 = CARTESIAN_POINT ( 'NONE',  ( 11.76133460557259980, -3.860150918677800025, -8.354833838171700222 ) ) ;
#50410 = VERTEX_POINT ( 'NONE', #26784 ) ;
#50411 = CARTESIAN_POINT ( 'NONE',  ( 11.03765229723000019, -2.753052473772000130, -5.025182086257999892 ) ) ;
#50412 = DIRECTION ( 'NONE',  ( 3.942933415072992810E-06, -0.7070925352470988079, 0.7071210268279988220 ) ) ;
#50413 = CARTESIAN_POINT ( 'NONE',  ( 5.000030787343001215, 1.057581170753189248, -1.834918991542628275 ) ) ;
#50414 = CARTESIAN_POINT ( 'NONE',  ( 23.56665676678199972, 13.31363904818000066, -4.296982115204999175 ) ) ;
#50415 = CARTESIAN_POINT ( 'NONE',  ( 12.68504826104523175, 3.238474326485677679, 13.62029029943391834 ) ) ;
#50416 = CARTESIAN_POINT ( 'NONE',  ( 9.869049086607999399, -5.575175898444999945, 7.724300702620999104 ) ) ;
#50417 = VERTEX_POINT ( 'NONE', #63472 ) ;
#50418 = CARTESIAN_POINT ( 'NONE',  ( 12.21236377913539961, 0.1994069032837916255, -12.69791261745714905 ) ) ;
#50419 = CARTESIAN_POINT ( 'NONE',  ( 12.66324396017929388, -0.6090406077983148148, 13.88203505342131550 ) ) ;
#50420 = ORIENTED_EDGE ( 'NONE', *, *, #45065, .F. ) ;
#50421 = CARTESIAN_POINT ( 'NONE',  ( 24.53428985175800037, 12.47024902693999948, -3.026245299674999778 ) ) ;
#50422 = CARTESIAN_POINT ( 'NONE',  ( 10.63445696062572310, 4.782035257973576314, -4.772905834451544926 ) ) ;
#50423 = CARTESIAN_POINT ( 'NONE',  ( 23.62001255296500446, -2.979299042067999892, -13.51746985525000078 ) ) ;
#50424 = LINE ( 'NONE', #45189, #45110 ) ;
#50425 = DIRECTION ( 'NONE',  ( 0.000000000000000000, 0.000000000000000000, 1.000000000000000000 ) ) ;
#50426 = CARTESIAN_POINT ( 'NONE',  ( 25.60000000000000142, 10.55164198324999880, 3.754898126455999741 ) ) ;
#50427 = CARTESIAN_POINT ( 'NONE',  ( 0.2689139796826999773, -1.124254478562000115, 3.354249223527999924 ) ) ;
#50428 = VECTOR ( 'NONE', #44503, 1000.000000000000114 ) ;
#50429 = CARTESIAN_POINT ( 'NONE',  ( 10.43314899746000002, 5.167567567567999731, 6.822293592207000934 ) ) ;
#50430 = CARTESIAN_POINT ( 'NONE',  ( 12.45041481799818506, 3.107897655637143153, 12.21069225363714494 ) ) ;
#50431 = DIRECTION ( 'NONE',  ( 0.000000000000000000, -0.9466492601157001641, 0.3222656952305000266 ) ) ;
#50432 = CARTESIAN_POINT ( 'NONE',  ( 11.07210672858429845, 3.307795442047700263, -6.979277962544199632 ) ) ;
#50433 = PLANE ( 'NONE',  #56166 ) ;
#50434 = EDGE_CURVE ( 'NONE', #51958, #46074, #11986, .T. ) ;
#50435 = ADVANCED_FACE ( 'NONE', ( #15595 ), #44614, .F. ) ;
#50436 = FACE_OUTER_BOUND ( 'NONE', #51310, .T. ) ;
#50437 = CARTESIAN_POINT ( 'NONE',  ( 8.822113844317998499, 4.288351516201100111, -6.395197822644999697 ) ) ;
#50439 = CARTESIAN_POINT ( 'NONE',  ( 11.50000000000000000, -4.968589424331200100, 7.825000000000000178 ) ) ;
#50438 = CARTESIAN_POINT ( 'NONE',  ( 9.418455549952998496, -3.325238030324599858, 8.044430187461498960 ) ) ;
#50440 = CARTESIAN_POINT ( 'NONE',  ( 23.60347242227338427, -13.39430291987660482, 3.981273882526325192 ) ) ;
#50441 = ORIENTED_EDGE ( 'NONE', *, *, #8303, .T. ) ;
#50442 = DIRECTION ( 'NONE',  ( -0.8660254037930258386, -1.085712934586031895E-07, 0.4999999999851149068 ) ) ;
#50443 = CIRCLE ( 'NONE', #10260, 12.35000000006999876 ) ;
#50444 = CARTESIAN_POINT ( 'NONE',  ( 10.28315099603999982, -2.387772357283999725, 7.684266429524000408 ) ) ;
#50445 = CARTESIAN_POINT ( 'NONE',  ( 8.922480666858998433, 4.380700808321400075, 6.423523106103999680 ) ) ;
#50446 = CARTESIAN_POINT ( 'NONE',  ( 9.860128811416625894, 4.869607263996035940, -7.596516710088708990 ) ) ;
#50447 = CARTESIAN_POINT ( 'NONE',  ( 9.786673210037999837, -2.381198102024000285, 7.612749732462000374 ) ) ;
#50448 = CARTESIAN_POINT ( 'NONE',  ( 12.31588542590557722, 2.889160216979992590, 13.58313038422180696 ) ) ;
#50449 = UNCERTAINTY_MEASURE_WITH_UNIT (LENGTH_MEASURE( 1.000000000000000082E-05 ), #63078, 'distance_accuracy_value', 'NONE');
#50450 = EDGE_LOOP ( 'NONE', ( #7980, #59593, #25468, #37653, #41928 ) ) ;
#50451 = ADVANCED_FACE ( 'NONE', ( #59266 ), #31695, .T. ) ;
#50452 = CARTESIAN_POINT ( 'NONE',  ( 8.568822372493999140, -4.328199826929600036, -8.573651380901999630 ) ) ;
#50453 = CARTESIAN_POINT ( 'NONE',  ( 23.60000000000000142, -11.77655473258999841, 4.190794510628000680 ) ) ;
#50454 = CARTESIAN_POINT ( 'NONE',  ( 5.318549751428999883, 1.497237214918999859, -0.6046620561147000306 ) ) ;
#50455 = EDGE_CURVE ( 'NONE', #48923, #38467, #52159, .T. ) ;
#50456 = CARTESIAN_POINT ( 'NONE',  ( 18.24702988622816591, 2.264821834935298206, -12.39478563874201633 ) ) ;
#50457 = DIRECTION ( 'NONE',  ( 0.000000000000000000, -0.7614089499631907509, 0.6482718649732929217 ) ) ;
#50458 = CARTESIAN_POINT ( 'NONE',  ( 8.849999778957998942, 4.000000000000000000, 6.500000166194499940 ) ) ;
#50459 = CARTESIAN_POINT ( 'NONE',  ( 10.43210941423799909, 4.641185166475500168, -6.917608226833099394 ) ) ;
#50460 = DIRECTION ( 'NONE',  ( -1.000000000000000000, 1.446714696031000002E-14, -6.365544662537999944E-14 ) ) ;
#50461 = CARTESIAN_POINT ( 'NONE',  ( 9.221306596384000187, -5.362859773739999447, -6.470306978669999154 ) ) ;
#50462 = CARTESIAN_POINT ( 'NONE',  ( 25.36444586457099959, 11.12587325612000022, 3.379815864972000039 ) ) ;
#50463 = EDGE_LOOP ( 'NONE', ( #31239, #44280, #9222, #35074, #40338 ) ) ;
#50464 = CARTESIAN_POINT ( 'NONE',  ( -1.222471984994595150E-05, -9.327013418423733093E-16, -2.899969545326207765 ) ) ;
#50465 = CARTESIAN_POINT ( 'NONE',  ( 12.44955560269365158, 0.5141525164327367392, -13.88720023103245360 ) ) ;
#50466 = CARTESIAN_POINT ( 'NONE',  ( 10.58521345716900086, -3.075109701058799772, 6.659120737011199331 ) ) ;
#50467 = CARTESIAN_POINT ( 'NONE',  ( 25.09300670485700024, -8.442812854790998855, -8.583344465159997938 ) ) ;
#50468 = CARTESIAN_POINT ( 'NONE',  ( 13.61451884198179663, -11.47057857663875424, -2.038550092594244134 ) ) ;
#50469 = CARTESIAN_POINT ( 'NONE',  ( 9.070789158774999805, 5.349936549139000519, -7.138437102151999447 ) ) ;
#50470 = CARTESIAN_POINT ( 'NONE',  ( 8.241912900173000267, -4.599999999999999645, 6.117539782833000928 ) ) ;
#50471 = VERTEX_POINT ( 'NONE', #27297 ) ;
#50472 = CONICAL_SURFACE ( 'NONE', #22566, 13.94232983116000035, 1.233427434088588903 ) ;
#50473 = CARTESIAN_POINT ( 'NONE',  ( 9.187962132612033983, -4.829473580601618465, -8.579511985892374071 ) ) ;
#50474 = CARTESIAN_POINT ( 'NONE',  ( 18.04669395734977044, 2.113974215446797089, -13.74779306078356456 ) ) ;
#50475 = VERTEX_POINT ( 'NONE', #5274 ) ;
#50476 = CARTESIAN_POINT ( 'NONE',  ( 11.58810207955109917, -4.796537143354000499, -7.174999999999999822 ) ) ;
#50477 = CARTESIAN_POINT ( 'NONE',  ( 24.79995638510570544, 3.079655890133128349, 11.72210376764452278 ) ) ;
#50478 = CARTESIAN_POINT ( 'NONE',  ( 9.450870280412999591, 2.928319778732999978, -8.861178115809998701 ) ) ;
#50479 = CARTESIAN_POINT ( 'NONE',  ( 11.10000000000000142, -2.546822617228925001, -8.294562688910756876 ) ) ;
#50480 = CARTESIAN_POINT ( 'NONE',  ( 10.76857802013509868, -5.174568897094999897, -7.472656658230009796 ) ) ;
#50481 = CARTESIAN_POINT ( 'NONE',  ( 9.368002778646790318, -5.097707675583217579, -6.362033401427927615 ) ) ;
#50482 = CARTESIAN_POINT ( 'NONE',  ( 10.15434687351566723, -2.749999999999998668, 7.663624617374463988 ) ) ;
#50483 = ORIENTED_EDGE ( 'NONE', *, *, #31744, .T. ) ;
#50484 = CARTESIAN_POINT ( 'NONE',  ( 10.11501430098003773, -5.350017391163235381, -7.499999134156934311 ) ) ;
#50485 = CARTESIAN_POINT ( 'NONE',  ( 17.92070696550175768, -3.007249353073734088, -13.55264287718867244 ) ) ;
#50486 = CARTESIAN_POINT ( 'NONE',  ( 9.842764158772000727, 5.798263352390999437, -8.113145944980999502 ) ) ;
#50487 = ORIENTED_EDGE ( 'NONE', *, *, #68166, .F. ) ;
#50488 = AXIS2_PLACEMENT_3D ( 'NONE', #58077, #52481, #47932 ) ;
#50489 = CARTESIAN_POINT ( 'NONE',  ( 10.81362367151999848, 3.876947539724999725, -9.022206283674000460 ) ) ;
#50490 = DIRECTION ( 'NONE',  ( 1.000000000000000000, 0.000000000000000000, 0.000000000000000000 ) ) ;
#50491 = ORIENTED_EDGE ( 'NONE', *, *, #46396, .F. ) ;
#50492 = CARTESIAN_POINT ( 'NONE',  ( 9.885938025973999288, 3.406370524467499994, 8.475365825607600101 ) ) ;
#50493 = CARTESIAN_POINT ( 'NONE',  ( 18.27918563591884293, -2.436421501371052400, -12.36221688302662791 ) ) ;
#50494 = VECTOR ( 'NONE', #28600, 1000.000000000000000 ) ;
#50495 = CARTESIAN_POINT ( 'NONE',  ( 9.414763540182331525, 2.782534154164605589, 7.172815144550902744 ) ) ;
#50496 = PRODUCT_DEFINITION ( 'UNKNOWN', '', #53015, #52068 ) ;
#50497 = CARTESIAN_POINT ( 'NONE',  ( 10.37835931247723309, -5.126777126138700957, 6.752018918791596214 ) ) ;
#50498 = CARTESIAN_POINT ( 'NONE',  ( 11.42387073792000152, -11.74429294849999827, -1.827310270344000065 ) ) ;
#50499 = EDGE_CURVE ( 'NONE', #12624, #58906, #41098, .T. ) ;
#50500 = CARTESIAN_POINT ( 'NONE',  ( 9.130088727410999638, 3.136022381937999981, 7.427538838030949719 ) ) ;
#50501 = CARTESIAN_POINT ( 'NONE',  ( 9.395841836927720792, -2.641307054571064850, 8.590477017151444628 ) ) ;
#50502 = VERTEX_POINT ( 'NONE', #22034 ) ;
#50503 = CYLINDRICAL_SURFACE ( 'NONE', #54878, 2.000000000000000444 ) ;
#50504 = CARTESIAN_POINT ( 'NONE',  ( 10.97819528041000048, 5.476824759564999923, -7.128718425160999850 ) ) ;
#50505 = B_SPLINE_CURVE_WITH_KNOTS ( 'NONE', 3,
 ( #14379, #14713, #25546, #15050 ),
 .UNSPECIFIED., .F., .F.,
 ( 4, 4 ),
 ( 0.000000000000000000, 1.000000000000000000 ),
 .UNSPECIFIED. ) ;
#50506 = CARTESIAN_POINT ( 'NONE',  ( 11.04878770808000077, -5.241617395113999933, -5.060603459065999843 ) ) ;
#50507 = CARTESIAN_POINT ( 'NONE',  ( 12.08107629042315700, 2.473358331846538860, -13.77980712931822183 ) ) ;
#50508 = CARTESIAN_POINT ( 'NONE',  ( 9.210288521113000115, -4.352953559891299840, 6.715449042252499723 ) ) ;
#50509 = CARTESIAN_POINT ( 'NONE',  ( 10.31167756636999933, -2.874479384703000129, 8.900026329558999194 ) ) ;
#50510 = CARTESIAN_POINT ( 'NONE',  ( 17.65055117253430339, -0.7242550212505970419, 13.98125389334239799 ) ) ;
#50511 = CARTESIAN_POINT ( 'NONE',  ( 18.17229989573039717, -2.399660445407139076, 12.47442500975930635 ) ) ;
#50512 = EDGE_LOOP ( 'NONE', ( #42625, #47609, #9631, #54328 ) ) ;
#50513 = ORIENTED_EDGE ( 'NONE', *, *, #62055, .F. ) ;
#50514 = CARTESIAN_POINT ( 'NONE',  ( 9.544414158773999901, 2.173570076733999823, -8.023168429484000441 ) ) ;
#50515 = CARTESIAN_POINT ( 'NONE',  ( 9.186946766250802199, 5.739007437171039783, 7.194229541610464018 ) ) ;
#50516 = CARTESIAN_POINT ( 'NONE',  ( 12.20341915911530961, -2.330389505191049704, 13.70797212925131348 ) ) ;
#50517 = PLANE ( 'NONE',  #50676 ) ;
#50518 = EDGE_CURVE ( 'NONE', #37829, #20140, #21354, .T. ) ;
#50519 = ADVANCED_FACE ( 'NONE', ( #38118 ), #32543, .T. ) ;
#50520 = CARTESIAN_POINT ( 'NONE',  ( 23.99165867875700187, 9.434723935140999274, -9.573197871853999175 ) ) ;
#50521 = CARTESIAN_POINT ( 'NONE',  ( 18.44504292973000048, -2.664685748803000021, -11.39637496735000077 ) ) ;
#50523 = CARTESIAN_POINT ( 'NONE',  ( 17.60000000000000142, 11.23412379136000006, -3.084957477885999833 ) ) ;
#50522 = CARTESIAN_POINT ( 'NONE',  ( 9.878405316141000370, -4.242421256336299962, 6.384219384258999597 ) ) ;
#50524 = CARTESIAN_POINT ( 'NONE',  ( 9.057169810767971896, 4.203513387681364399, -8.707169876682314680 ) ) ;
#50525 = ORIENTED_EDGE ( 'NONE', *, *, #39142, .T. ) ;
#50526 = AXIS2_PLACEMENT_3D ( 'NONE', #64857, #38299, #16968 ) ;
#50527 = ADVANCED_FACE ( 'NONE', ( #43724 ), #36545, .T. ) ;
#50528 = CARTESIAN_POINT ( 'NONE',  ( 12.80505043854144098, 0.7302158263239095781, 13.98094363220830871 ) ) ;
#50529 = CARTESIAN_POINT ( 'NONE',  ( 8.174990947233153449, 2.650692654198087972, 7.500004443805798005 ) ) ;
#50530 = CARTESIAN_POINT ( 'NONE',  ( 17.74668184667432769, 0.5949840079737193088, 12.68123264482375490 ) ) ;
#50531 = CARTESIAN_POINT ( 'NONE',  ( 12.35320888692065999, -0.4320279633463514068, 12.69011309769952867 ) ) ;
#50532 = CARTESIAN_POINT ( 'NONE',  ( 4.149992563291999836, 1.999946284944287722, 0.2617923565147994291 ) ) ;
#50533 = ORIENTED_EDGE ( 'NONE', *, *, #46178, .F. ) ;
#50535 = CARTESIAN_POINT ( 'NONE',  ( 12.15446082642243830, -2.110350925006974077, -12.42276656537216084 ) ) ;
#50534 = CARTESIAN_POINT ( 'NONE',  ( 10.87173209806000074, -5.066009632528999163, 5.128393832781000583 ) ) ;
#50536 = CARTESIAN_POINT ( 'NONE',  ( 8.713854719593998155, 5.442817578555000146, -8.106149115450000053 ) ) ;
#50537 = CARTESIAN_POINT ( 'NONE',  ( 9.293536308085233344, 2.899999999999999911, 6.665341197415443730 ) ) ;
#50538 = CARTESIAN_POINT ( 'NONE',  ( 7.613711861438999584, -4.858906194260998568, 6.437673909214002954 ) ) ;
#50539 = AXIS2_PLACEMENT_3D ( 'NONE', #39752, #28932, #27885 ) ;
#50540 = FILL_AREA_STYLE ('',( #45647 ) ) ;
#50541 = ADVANCED_FACE ( 'NONE', ( #5610 ), #16429, .F. ) ;
#50542 = CARTESIAN_POINT ( 'NONE',  ( 17.92628981779797570, -3.345291551605441782, -11.86067033226837530 ) ) ;
#50543 = CARTESIAN_POINT ( 'NONE',  ( 2.976748247909999812, -0.7364029526790000224, -3.515900957781999736 ) ) ;
#50544 = ORIENTED_EDGE ( 'NONE', *, *, #36134, .T. ) ;
#50545 = CARTESIAN_POINT ( 'NONE',  ( 12.29717897459458875, -0.3644117276601275823, -12.69296657371244841 ) ) ;
#50546 = CARTESIAN_POINT ( 'NONE',  ( 7.808687732304345985, -3.149842433176995193, 6.423753202348916780 ) ) ;
#50547 = DIRECTION ( 'NONE',  ( 0.000000000000000000, -1.000000000000000000, 0.000000000000000000 ) ) ;
#50548 = CARTESIAN_POINT ( 'NONE',  ( 8.128301658772999261, 3.117378429069999957, 8.662179062556001341 ) ) ;
#50549 = SURFACE_STYLE_FILL_AREA ( #40739 ) ;
#50550 = ORIENTED_EDGE ( 'NONE', *, *, #50216, .F. ) ;
#50551 = CARTESIAN_POINT ( 'NONE',  ( 5.420847890839000094, -1.289352866216999960, -0.2932997125499000046 ) ) ;
#50552 = B_SPLINE_CURVE_WITH_KNOTS ( 'NONE', 3,
 ( #6421, #43148, #28109, #38240, #37550, #1534, #10639, #17624, #33359, #844, #59569, #37900, #58533, #21814, #49080, #59914, #64113, #17267 ),
 .UNSPECIFIED., .F., .F.,
 ( 4, 2, 2, 2, 2, 2, 2, 2, 4 ),
 ( 0.000000000000000000, 0.1070823790245061802, 0.2141647580490123604, 0.3212471370735185405, 0.4283295160980247207, 0.5354118951225302903, 0.6424942741470358598, 0.7495766531715415404, 0.8566590321960471099 ),
 .UNSPECIFIED. ) ;
#50553 = CARTESIAN_POINT ( 'NONE',  ( 7.192235841229000393, 4.367071440064000498, -8.848478693904000991 ) ) ;
#50555 = FACE_OUTER_BOUND ( 'NONE', #23275, .T. ) ;
#50554 = CARTESIAN_POINT ( 'NONE',  ( 8.601293559883481876, -4.584462925737535777, 5.854726763232750208 ) ) ;
#50556 = CARTESIAN_POINT ( 'NONE',  ( 10.78887616594230003, 3.613544262574699850, 8.718182393403999697 ) ) ;
#50557 = CARTESIAN_POINT ( 'NONE',  ( 8.267367474942998840, 3.071849710027000135, -6.244583336620999958 ) ) ;
#50558 = ORIENTED_EDGE ( 'NONE', *, *, #68167, .F. ) ;
#50559 = CARTESIAN_POINT ( 'NONE',  ( 9.848253563160000112, -4.436921580929999998, 6.148020168057000134 ) ) ;
#50560 = ORIENTED_EDGE ( 'NONE', *, *, #48533, .T. ) ;
#50561 = DIRECTION ( 'NONE',  ( 0.000000000000000000, 0.000000000000000000, 1.000000000000000000 ) ) ;
#50562 = CARTESIAN_POINT ( 'NONE',  ( 9.587879440377001572, -3.762710033898000184, 8.787827024292999667 ) ) ;
#50563 = CARTESIAN_POINT ( 'NONE',  ( 18.05077945915501303, -0.5329747956505088702, -13.98985355243729423 ) ) ;
#50564 = VERTEX_POINT ( 'NONE', #60146 ) ;
#50565 = CARTESIAN_POINT ( 'NONE',  ( 10.92306252329737504, 9.582901050001986221, -5.997835859251378743 ) ) ;
#50566 = CARTESIAN_POINT ( 'NONE',  ( 0.7431103717477000048, 2.848815883361000001, -1.248255999701999963 ) ) ;
#50567 = CARTESIAN_POINT ( 'NONE',  ( 4.599999999999999645, 1.875000000000000000, 13.78627172894481667 ) ) ;
#50568 = CARTESIAN_POINT ( 'NONE',  ( 9.343930206849998754, -5.250000000000000000, -7.500000000000000000 ) ) ;
#50569 = CARTESIAN_POINT ( 'NONE',  ( 24.53428991195500330, 3.614319144953999530, 12.31267516478999902 ) ) ;
#50570 = ORIENTED_EDGE ( 'NONE', *, *, #27386, .T. ) ;
#50571 = CARTESIAN_POINT ( 'NONE',  ( 24.37808886034967770, 8.911082506783134960, 9.054599869853928951 ) ) ;
#50572 = CARTESIAN_POINT ( 'NONE',  ( 23.74058054779100146, -13.16199033518000050, -3.761701342105999935 ) ) ;
#50573 = FACE_OUTER_BOUND ( 'NONE', #50621, .T. ) ;
#50574 = CARTESIAN_POINT ( 'NONE',  ( 6.899999691988000450, -12.99045401563999924, 1.690592933733000125 ) ) ;
#50575 = AXIS2_PLACEMENT_3D ( 'NONE', #15009, #9075, #20599 ) ;
#50576 = CARTESIAN_POINT ( 'NONE',  ( 9.765375278055641317, -5.100000000000000533, 6.445686799077642526 ) ) ;
#50577 = ORIENTED_EDGE ( 'NONE', *, *, #46884, .F. ) ;
#50578 = PRODUCT ( 'Terminal Screw 2', 'Terminal Screw 2', '', ( #53975 ) ) ;
#50579 = CARTESIAN_POINT ( 'NONE',  ( 5.200000000000000178, 0.000000000000000000, 0.000000000000000000 ) ) ;
#50580 = CYLINDRICAL_SURFACE ( 'NONE', #38830, 1.350000000000000533 ) ;
#50581 = CARTESIAN_POINT ( 'NONE',  ( 3.500000000000000000, 2.135761500787233036, 2.632305434550216816 ) ) ;
#50582 = EDGE_CURVE ( 'NONE', #10441, #19590, #63626, .T. ) ;
#50583 = CARTESIAN_POINT ( 'NONE',  ( 23.84134220052430209, -3.319692114198800503, -13.04897312825259093 ) ) ;
#50584 = DIRECTION ( 'NONE',  ( 0.000000000000000000, 1.000000000000000000, 0.000000000000000000 ) ) ;
#50585 = EDGE_CURVE ( 'NONE', #13082, #1379, #49299, .T. ) ;
#50586 = B_SPLINE_CURVE_WITH_KNOTS ( 'NONE', 3,
 ( #21097, #36481, #48009, #109 ),
 .UNSPECIFIED., .F., .F.,
 ( 4, 4 ),
 ( 0.8744711628437967788, 1.000000000000000000 ),
 .UNSPECIFIED. ) ;
#50587 = CARTESIAN_POINT ( 'NONE',  ( 12.18004362304668575, -0.009762789003247420577, -13.90000041479088289 ) ) ;
#50588 = CARTESIAN_POINT ( 'NONE',  ( 18.03475265876380007, -2.099231872491031936, 12.53598779768162785 ) ) ;
#50589 = ORIENTED_EDGE ( 'NONE', *, *, #56712, .T. ) ;
#50590 = CARTESIAN_POINT ( 'NONE',  ( 11.06456920625009843, -3.962850971080120299, -6.467161360063999886 ) ) ;
#50591 = VERTEX_POINT ( 'NONE', #44077 ) ;
#50592 = AXIS2_PLACEMENT_3D ( 'NONE', #67655, #53570, #15218 ) ;
#50593 = CARTESIAN_POINT ( 'NONE',  ( 18.18005044575082252, 2.500000006795693785, 13.67340643792831045 ) ) ;
#50594 = CARTESIAN_POINT ( 'NONE',  ( 8.581920280410001212, 4.769017407621999993, -8.862909124839001507 ) ) ;
#50595 = CARTESIAN_POINT ( 'NONE',  ( 2.377407833194000286, 3.071536117060000404, 1.409200688889000075 ) ) ;
#50596 = CARTESIAN_POINT ( 'NONE',  ( 10.09133114265999964, -2.216726401468000152, -8.007130485478999304 ) ) ;
#50597 = CARTESIAN_POINT ( 'NONE',  ( 11.50000000000000000, -2.920245322398999921, 7.174999999999999822 ) ) ;
#50598 = CARTESIAN_POINT ( 'NONE',  ( 9.051836062923225512, -4.773613032258291256, 8.611988568103887687 ) ) ;
#50599 = ORIENTED_EDGE ( 'NONE', *, *, #66861, .F. ) ;
#50600 = CARTESIAN_POINT ( 'NONE',  ( 12.19559063708295987, -2.913481137622000006, 7.194517870904999945 ) ) ;
#50601 = CARTESIAN_POINT ( 'NONE',  ( 9.724611353170001138, 2.928305163963000446, 8.718478150869000132 ) ) ;
#50602 = DIRECTION ( 'NONE',  ( -1.000000000000000000, 0.000000000000000000, 0.000000000000000000 ) ) ;
#50603 = EDGE_CURVE ( 'NONE', #19919, #55891, #35295, .T. ) ;
#50604 = FACE_OUTER_BOUND ( 'NONE', #15883, .T. ) ;
#50606 = CARTESIAN_POINT ( 'NONE',  ( 10.93333333333430524, 5.319670837135273445, 7.972931767323618857 ) ) ;
#50605 = CARTESIAN_POINT ( 'NONE',  ( 10.43579914648999996, 2.587602126999999808, 6.390037244031000263 ) ) ;
#50607 = CARTESIAN_POINT ( 'NONE',  ( 10.55518582084299872, 3.433275964779900047, -6.844925608615599621 ) ) ;
#50608 = ADVANCED_FACE ( 'NONE', ( #65375 ), #56280, .T. ) ;
#50609 = CARTESIAN_POINT ( 'NONE',  ( 5.700000001242999659, 1.249999998757000075, -1.883720587326999896E-09 ) ) ;
#50610 = CARTESIAN_POINT ( 'NONE',  ( 9.224417874593999755, 3.075647715286899953, -7.892956936667999912 ) ) ;
#50611 = CARTESIAN_POINT ( 'NONE',  ( 18.08442823429787794, -0.4920215530101185175, 12.59040071882420797 ) ) ;
#50612 = CARTESIAN_POINT ( 'NONE',  ( 25.44994642811700203, 0.000000000000000000, -2.282618538628999739E-13 ) ) ;
#50613 = DIRECTION ( 'NONE',  ( -0.7071067811864980568, 0.7071067811865969777, -1.029442514143995792E-08 ) ) ;
#50614 = CARTESIAN_POINT ( 'NONE',  ( 17.60000000044533408, 11.94788429102075789, -3.252375031275762218 ) ) ;
#50615 = ORIENTED_EDGE ( 'NONE', *, *, #44458, .F. ) ;
#50616 = CARTESIAN_POINT ( 'NONE',  ( 7.694004440376999376, -5.850279024084999335, 6.784181137144999596 ) ) ;
#50617 = AXIS2_PLACEMENT_3D ( 'NONE', #49267, #1040, #13862 ) ;
#50618 = CARTESIAN_POINT ( 'NONE',  ( 18.03607885879097594, 1.971554139641144454, 13.86048489721954624 ) ) ;
#50619 = DIRECTION ( 'NONE',  ( 0.000000000000000000, 1.000000000000000000, 0.000000000000000000 ) ) ;
#50620 = CARTESIAN_POINT ( 'NONE',  ( 9.965950584426998660, 4.344127791340399725, 8.295791434820300125 ) ) ;
#50621 = EDGE_LOOP ( 'NONE', ( #68290, #33753, #58481, #23735, #23893, #37222, #64568 ) ) ;
#50622 = CARTESIAN_POINT ( 'NONE',  ( 7.229676658770999964, 2.630487280353000390, 6.995957894972000268 ) ) ;
#50623 = EDGE_CURVE ( 'NONE', #8532, #27164, #16074, .T. ) ;
#50625 = CARTESIAN_POINT ( 'NONE',  ( 0.6001188040607291496, 2.874384006252894252, 2.063114442910663815 ) ) ;
#50624 = CARTESIAN_POINT ( 'NONE',  ( 9.889535841229999846, 5.798263352390999437, -8.113145944980999502 ) ) ;
#50626 = CARTESIAN_POINT ( 'NONE',  ( 10.53197665877000055, 2.323713329709999886, -8.279493667389999700 ) ) ;
#50627 = EDGE_LOOP ( 'NONE', ( #62983, #58459, #27736, #62843 ) ) ;
#50628 = CARTESIAN_POINT ( 'NONE',  ( 10.85737917744000036, 2.754548910086000113, 8.976376585747001258 ) ) ;
#50629 = CARTESIAN_POINT ( 'NONE',  ( 13.70003001321900271, -9.668726926528000476, -7.961868161445000425 ) ) ;
#50630 = CARTESIAN_POINT ( 'NONE',  ( 10.76841504065829902, 4.914510326623699576, 8.181880472491098288 ) ) ;
#50631 = CARTESIAN_POINT ( 'NONE',  ( 10.02202195053999922, -3.298019507654999849, 5.700533868754000366 ) ) ;
#50632 = CARTESIAN_POINT ( 'NONE',  ( 11.59999999999999964, 4.000000000000000000, -7.500000000000000000 ) ) ;
#50633 = ORIENTED_EDGE ( 'NONE', *, *, #55741, .T. ) ;
#50634 = CARTESIAN_POINT ( 'NONE',  ( -14.79345512259999929, -10.48174933044999868, 5.405686454350000503 ) ) ;
#50635 = CARTESIAN_POINT ( 'NONE',  ( 1.365556799207875205, -0.4581489286485082579, -3.500000000000000888 ) ) ;
#50636 = CARTESIAN_POINT ( 'NONE',  ( 7.965749382700749059, -2.298601573531716458, 7.139296998118509485 ) ) ;
#50637 = VECTOR ( 'NONE', #4550, 1000.000000000000000 ) ;
#50638 = CARTESIAN_POINT ( 'NONE',  ( 9.476374593785998002, -5.098398394707999159, 6.305533045879999854 ) ) ;
#50639 = CARTESIAN_POINT ( 'NONE',  ( 10.76857802013509868, -5.174568897094999897, -7.472656658230009796 ) ) ;
#50640 = CARTESIAN_POINT ( 'NONE',  ( 9.678734463322999915, -3.895375416816699854, 6.501052555474699624 ) ) ;
#50641 = ORIENTED_EDGE ( 'NONE', *, *, #59175, .T. ) ;
#50642 = CARTESIAN_POINT ( 'NONE',  ( 24.66906539831122558, -11.82198933512809802, -3.190506366364596058 ) ) ;
#50643 = CARTESIAN_POINT ( 'NONE',  ( 10.65303300763299887, -3.212834858289399964, 6.674373427955200277 ) ) ;
#50644 = ORIENTED_EDGE ( 'NONE', *, *, #21304, .F. ) ;
#50645 = CARTESIAN_POINT ( 'NONE',  ( 9.136057238048000073, -5.084840204920000772, -6.477689566282000655 ) ) ;
#50646 = AXIS2_PLACEMENT_3D ( 'NONE', #20919, #32449, #37002 ) ;
#50647 = ORIENTED_EDGE ( 'NONE', *, *, #40876, .T. ) ;
#50648 = CARTESIAN_POINT ( 'NONE',  ( 9.443723707566000769, -5.531435376468999188, -8.256621485025000595 ) ) ;
#50649 = CARTESIAN_POINT ( 'NONE',  ( 9.243110841233001196, 4.112741311853999271, -5.603466076760000192 ) ) ;
#50650 = B_SPLINE_CURVE_WITH_KNOTS ( 'NONE', 3,
 ( #37345, #41900, #15336, #21264, #58669, #53429 ),
 .UNSPECIFIED., .F., .F.,
 ( 4, 2, 4 ),
 ( 0.000000000000000000, 0.5000000000000000000, 1.000000000000000000 ),
 .UNSPECIFIED. ) ;
#50651 = CARTESIAN_POINT ( 'NONE',  ( 21.47500033997000202, 7.283063041541000399E-14, -6.705747068735999778E-14 ) ) ;
#50652 = PLANE ( 'NONE',  #3126 ) ;
#50653 = CARTESIAN_POINT ( 'NONE',  ( 12.34586232581678900, 2.075512354070471410, -12.54043254740683899 ) ) ;
#50654 = CARTESIAN_POINT ( 'NONE',  ( 11.76487482311540056, -3.069598554678400149, 7.124095752359899336 ) ) ;
#50655 = CARTESIAN_POINT ( 'NONE',  ( 11.15413259636999932, -4.783377755405500587, 7.073141822156699732 ) ) ;
#50656 = EDGE_LOOP ( 'NONE', ( #14656, #37180, #3333, #27782, #612 ) ) ;
#50657 = CARTESIAN_POINT ( 'NONE',  ( 9.760596873516666605, 3.370476274536378547, 8.592232985442823434 ) ) ;
#50658 = B_SPLINE_CURVE_WITH_KNOTS ( 'NONE', 3,
 ( #9948, #52944, #31285, #26030, #47360, #15542, #36871, #10289, #33696 ),
 .UNSPECIFIED., .F., .F.,
 ( 4, 1, 2, 2, 4 ),
 ( 0.000000000000000000, 0.2499999999999983902, 0.3749999999999983347, 0.4999999999999983347, 1.000000000000000000 ),
 .UNSPECIFIED. ) ;
#50659 = ORIENTED_EDGE ( 'NONE', *, *, #48444, .F. ) ;
#50660 = CARTESIAN_POINT ( 'NONE',  ( 7.930394353207000258, -3.164807285701999984, 9.104732190648000767 ) ) ;
#50661 = LINE ( 'NONE', #2761, #23445 ) ;
#50662 = EDGE_LOOP ( 'NONE', ( #5216, #62941 ) ) ;
#50663 = CARTESIAN_POINT ( 'NONE',  ( 12.22616922475387291, -2.046442494456577332, -12.43271557125384419 ) ) ;
#50664 = CARTESIAN_POINT ( 'NONE',  ( 10.96533729122639933, 2.859653469230999612, 7.529998433785960010 ) ) ;
#50665 = CARTESIAN_POINT ( 'NONE',  ( 11.03905685320999908, -3.855072944465999907, -9.179476187420998912 ) ) ;
#50666 = DIRECTION ( 'NONE',  ( 0.000000000000000000, -0.8615889394142682844, 0.5076066385292812289 ) ) ;
#50667 = CARTESIAN_POINT ( 'NONE',  ( 17.56496177128000369, -11.49815673738000044, 4.817809077628999681 ) ) ;
#50668 = EDGE_CURVE ( 'NONE', #33164, #21338, #61103, .T. ) ;
#50669 = CARTESIAN_POINT ( 'NONE',  ( 24.41555929959800153, -8.820896577839000940, 8.766783479516000455 ) ) ;
#50670 = DIRECTION ( 'NONE',  ( 1.000000000000000000, 0.000000000000000000, 0.000000000000000000 ) ) ;
#50671 = EDGE_CURVE ( 'NONE', #41535, #57987, #10843, .T. ) ;
#50672 = CARTESIAN_POINT ( 'NONE',  ( 5.137494878958000832, -0.8910062039905000120, -1.277482911150999989 ) ) ;
#50673 = CARTESIAN_POINT ( 'NONE',  ( 11.04749144726329924, -4.500836215462999945, -6.793273974143599681 ) ) ;
#50674 = CARTESIAN_POINT ( 'NONE',  ( 11.25656651104150008, -3.873914634362100262, -6.228222165170999247 ) ) ;
#50675 = ADVANCED_FACE ( 'NONE', ( #33578 ), #44769, .T. ) ;
#50676 = AXIS2_PLACEMENT_3D ( 'NONE', #44605, #34793, #66589 ) ;
#50677 = CARTESIAN_POINT ( 'NONE',  ( 8.570147025264834184, -5.044616720184398773, 6.241050644686979787 ) ) ;
#50678 = ORIENTED_EDGE ( 'NONE', *, *, #49645, .T. ) ;
#50679 = AXIS2_PLACEMENT_3D ( 'NONE', #27229, #10796, #43310 ) ;
#50680 =( NAMED_UNIT ( * ) SI_UNIT ( $, .STERADIAN. ) SOLID_ANGLE_UNIT ( ) );
#50681 = CARTESIAN_POINT ( 'NONE',  ( 12.73341324600965585, -11.23412379136210681, 3.084957477879898935 ) ) ;
#50682 = CARTESIAN_POINT ( 'NONE',  ( 17.83309906212661744, 3.060119824089694962, 13.53852211359576785 ) ) ;
#50683 = CARTESIAN_POINT ( 'NONE',  ( 24.08773761151700299, -3.426406091450999725, 12.66833900763000109 ) ) ;
#50684 = CARTESIAN_POINT ( 'NONE',  ( 17.76275439675989887, 1.910499210220269362, 12.56953514877129940 ) ) ;
#50685 = CARTESIAN_POINT ( 'NONE',  ( 17.76910169249500271, 3.411882384414000047, -11.89794055422999897 ) ) ;
#50686 = CARTESIAN_POINT ( 'NONE',  ( 11.02286749330999882, 2.398743616553999924, 6.352468982205000891 ) ) ;
#50687 = DIRECTION ( 'NONE',  ( 0.000000000000000000, 1.000000000000000000, 0.000000000000000000 ) ) ;
#50688 = ORIENTED_EDGE ( 'NONE', *, *, #2544, .F. ) ;
#50689 = CARTESIAN_POINT ( 'NONE',  ( 12.19329499274041773, -2.371606608387609505, 12.48058234101797126 ) ) ;
#50690 = CARTESIAN_POINT ( 'NONE',  ( 9.325734463322998380, -3.895375416816699854, -8.498947444525299488 ) ) ;
#50691 = B_SPLINE_CURVE_WITH_KNOTS ( 'NONE', 3,
 ( #671, #5901, #11156, #23022, #1356 ),
 .UNSPECIFIED., .F., .F.,
 ( 4, 1, 4 ),
 ( 0.000000000000000000, 0.5000000000000000000, 1.000000000000000000 ),
 .UNSPECIFIED. ) ;
#50692 = CARTESIAN_POINT ( 'NONE',  ( 10.42596030538999941, 5.042177533603999784, 8.702224267793999601 ) ) ;
#50693 = DIRECTION ( 'NONE',  ( -4.468466013035191386E-09, -0.2714605545367115846, 0.9624495661231402543 ) ) ;
#50694 = AXIS2_PLACEMENT_3D ( 'NONE', #29752, #51735, #24829 ) ;
#50695 = CARTESIAN_POINT ( 'NONE',  ( 10.25149413291699929, 5.037815157227999663, -7.026470926762800495 ) ) ;
#50696 = CARTESIAN_POINT ( 'NONE',  ( 12.21327642329898389, 0.2013262877421457264, 12.69785743964334834 ) ) ;
#50697 = CARTESIAN_POINT ( 'NONE',  ( 8.508079719592000600, 2.202812441249000219, 7.706988150133999405 ) ) ;
#50698 = CARTESIAN_POINT ( 'NONE',  ( 9.137543006348998631, 2.995704926864999784, 8.544754656710999541 ) ) ;
#50699 = CARTESIAN_POINT ( 'NONE',  ( 12.47171258541602512, 1.971212359000195313, 12.55915788719762993 ) ) ;
#50700 = ORIENTED_EDGE ( 'NONE', *, *, #54779, .F. ) ;
#50701 = CARTESIAN_POINT ( 'NONE',  ( 25.57799081801000085, 8.344607266676000279, 8.013922886049000383 ) ) ;
#50702 = CARTESIAN_POINT ( 'NONE',  ( 10.88733729122639993, 2.722429312291999803, -7.466391690027689876 ) ) ;
#50703 = CARTESIAN_POINT ( 'NONE',  ( 10.81962466143134804, -4.116062333401275808, 9.235854717643961820 ) ) ;
#50705 = CARTESIAN_POINT ( 'NONE',  ( 11.39975833414730033, 4.796537143354000499, -7.174999999999999822 ) ) ;
#50704 = CARTESIAN_POINT ( 'NONE',  ( 8.213543146793000460, -3.608524635952000459, 5.913372239166000632 ) ) ;
#50706 = CARTESIAN_POINT ( 'NONE',  ( 9.427455549952998837, -3.325238030324599858, 8.044430187461498960 ) ) ;
#50707 = CARTESIAN_POINT ( 'NONE',  ( 11.63410404293056999, -4.442327784369100030, -8.400720262063998689 ) ) ;
#50708 = VERTEX_POINT ( 'NONE', #39510 ) ;
#50709 = CARTESIAN_POINT ( 'NONE',  ( 1.539110206209999943, 0.8784043042010000191, 3.483138632238000021 ) ) ;
#50710 = CARTESIAN_POINT ( 'NONE',  ( 11.37299956498129916, 2.792989229543000107, 7.825000000000000178 ) ) ;
#50711 = EDGE_CURVE ( 'NONE', #48720, #64156, #28686, .T. ) ;
#50712 = CARTESIAN_POINT ( 'NONE',  ( 0.9681103717476999826, 3.205765437135000173, -1.404659375816999844 ) ) ;
#50713 = CARTESIAN_POINT ( 'NONE',  ( 18.08654171825435597, -2.829006819437166254, 13.59815647009357953 ) ) ;
#50714 = B_SPLINE_CURVE_WITH_KNOTS ( 'NONE', 3,
 ( #53428, #43282, #58668, #59700 ),
 .UNSPECIFIED., .F., .F.,
 ( 4, 4 ),
 ( 0.000000000000000000, 1.000000000000000000 ),
 .UNSPECIFIED. ) ;
#50715 = CARTESIAN_POINT ( 'NONE',  ( 24.51228084510600169, -12.11225741719000126, 3.153589928299999734 ) ) ;
#50716 = ADVANCED_FACE ( 'NONE', ( #45106 ), #16065, .F. ) ;
#50717 = CARTESIAN_POINT ( 'NONE',  ( 4.900006121742000786, -0.5234957687185600728, -1.947945353336631991 ) ) ;
#50718 = CARTESIAN_POINT ( 'NONE',  ( 11.77769289846838241, -5.045673698156681652, 7.175017342370984430 ) ) ;
#50719 = CARTESIAN_POINT ( 'NONE',  ( 4.805026506350000837, 1.500000000000000000, 0.000000000000000000 ) ) ;
#50720 = CARTESIAN_POINT ( 'NONE',  ( 7.437254440376999121, -2.216884807317999861, 8.370075800106999253 ) ) ;
#50721 = VERTEX_POINT ( 'NONE', #1325 ) ;
#50722 = CARTESIAN_POINT ( 'NONE',  ( 8.689260841231000398, 2.550241116032999855, 7.666973618349000041 ) ) ;
#50723 = CARTESIAN_POINT ( 'NONE',  ( 23.58885776300258641, -2.922211427196971911, 13.61646868590587545 ) ) ;
#50724 = CARTESIAN_POINT ( 'NONE',  ( 18.14740543753152124, 2.299612738907994114, -13.71393688410719491 ) ) ;
#50725 = VECTOR ( 'NONE', #39694, 1000.000000000000114 ) ;
#50726 = CARTESIAN_POINT ( 'NONE',  ( 17.81163220004817660, -0.5699871458820113812, 13.88426688812672971 ) ) ;
#50727 = CARTESIAN_POINT ( 'NONE',  ( 0.8372907118031999163, -0.1515593316830000370, 3.422260710200999867 ) ) ;
#50728 = ORIENTED_EDGE ( 'NONE', *, *, #3932, .T. ) ;
#50729 = CARTESIAN_POINT ( 'NONE',  ( 13.99999999270239570, -8.951333082579457923, -8.002096037671929452 ) ) ;
#50730 = CARTESIAN_POINT ( 'NONE',  ( 10.66405417102151887, -5.056489201926463117, 5.060659056817709889 ) ) ;
#50731 = CARTESIAN_POINT ( 'NONE',  ( 10.00122429346999908, 2.274087081648999753, 7.851326250696001097 ) ) ;
#50732 = CARTESIAN_POINT ( 'NONE',  ( 10.50180110216399854, 3.143606124884799957, 8.023010882787499298 ) ) ;
#50733 = FACE_OUTER_BOUND ( 'NONE', #11683, .T. ) ;
#50734 = CARTESIAN_POINT ( 'NONE',  ( 10.34939194037999854, -2.653148377029999949, -7.312413909354000374 ) ) ;
#50735 = CARTESIAN_POINT ( 'NONE',  ( 15.89979320885400327, -3.824231472901999496, -11.71686814605000038 ) ) ;
#50736 = CARTESIAN_POINT ( 'NONE',  ( 11.43328525708585630, 3.653536053513361637, -11.13242455109464046 ) ) ;
#50737 = CARTESIAN_POINT ( 'NONE',  ( 12.39978108236764598, -2.975905172436775992, 12.32787332407853143 ) ) ;
#50738 = CARTESIAN_POINT ( 'NONE',  ( 8.591260603588073863, 4.340498360229820385, 5.786730013295068531 ) ) ;
#50739 = AXIS2_PLACEMENT_3D ( 'NONE', #23568, #49801, #12744 ) ;
#50740 = ORIENTED_EDGE ( 'NONE', *, *, #41270, .T. ) ;
#50741 = CARTESIAN_POINT ( 'NONE',  ( 17.72176632460248769, -3.228945123492078739, 13.62255252064306354 ) ) ;
#50742 = CARTESIAN_POINT ( 'NONE',  ( 10.35685100253999913, -2.832432432432000269, -6.822293592207000934 ) ) ;
#50743 = ORIENTED_EDGE ( 'NONE', *, *, #55406, .F. ) ;
#50744 = CARTESIAN_POINT ( 'NONE',  ( 10.90000000000000036, -1.376649746192999846, -11.21582968292000082 ) ) ;
#50745 = CARTESIAN_POINT ( 'NONE',  ( 11.15278751119019773, 3.209519379020799867, 7.086443476450299706 ) ) ;
#50746 = CARTESIAN_POINT ( 'NONE',  ( 4.149992563291998948, 1.229060429538529009, -1.599290730647369152 ) ) ;
#50747 = CARTESIAN_POINT ( 'NONE',  ( 8.741252916288999586, -3.907441415015589836, -8.374574604871998673 ) ) ;
#50748 = CARTESIAN_POINT ( 'NONE',  ( 9.843732751558000871, 4.115124343450999866, 9.466620196856998959 ) ) ;
#50749 = CARTESIAN_POINT ( 'NONE',  ( 9.858847045824999711, 2.668090821818000169, -7.206973500459000093 ) ) ;
#50750 = CARTESIAN_POINT ( 'NONE',  ( 10.17726354018233081, -3.370476274536371442, -6.407767014557179230 ) ) ;
#50751 = CARTESIAN_POINT ( 'NONE',  ( 10.70441271436000008, -3.444516450945999786, 6.009051312948000323 ) ) ;
#50752 = EDGE_CURVE ( 'NONE', #36042, #68830, #55852, .T. ) ;
#50753 = CARTESIAN_POINT ( 'NONE',  ( 11.53713315544000118, 3.620704573398000115, -11.03277391605000091 ) ) ;
#50754 = CARTESIAN_POINT ( 'NONE',  ( 10.71983009893999927, -3.571743996388999864, -5.696159701115999674 ) ) ;
#50755 = CARTESIAN_POINT ( 'NONE',  ( 11.51102763632551884, -4.911148285670300595, -7.079572058049399708 ) ) ;
#50756 = ADVANCED_FACE ( 'NONE', ( #50604 ), #51077, .T. ) ;
#50757 = EDGE_CURVE ( 'NONE', #56244, #7917, #20926, .T. ) ;
#50758 = CARTESIAN_POINT ( 'NONE',  ( 10.69180966889106088, -2.945054940980131875, -5.060957807827213273 ) ) ;
#50759 = ORIENTED_EDGE ( 'NONE', *, *, #24784, .T. ) ;
#50760 = APPLICATION_CONTEXT ( 'automotive_design' ) ;
#50761 = CARTESIAN_POINT ( 'NONE',  ( 10.06927318630900103, 4.756452637475338641, 6.473854711408034923 ) ) ;
#50762 =( NAMED_UNIT ( * ) PLANE_ANGLE_UNIT ( ) SI_UNIT ( $, .RADIAN. ) );
#50763 = CARTESIAN_POINT ( 'NONE',  ( 24.68355587878626523, 8.667372866500036466, 8.629868536354566189 ) ) ;
#50764 = CARTESIAN_POINT ( 'NONE',  ( 12.79999999975700042, 11.86189249994999884, -3.298671769835999967 ) ) ;
#50765 = CARTESIAN_POINT ( 'NONE',  ( 9.329759580229000093, 2.755835090116000696, -7.202614619576299226 ) ) ;
#50766 = CARTESIAN_POINT ( 'NONE',  ( 12.18011073905423736, 2.522020058064990522, 13.66873259811636032 ) ) ;
#50767 = CARTESIAN_POINT ( 'NONE',  ( 9.646285452541999206, -2.591464128784999765, 6.760053199270999791 ) ) ;
#50768 = ORIENTED_EDGE ( 'NONE', *, *, #25754, .F. ) ;
#50769 = CARTESIAN_POINT ( 'NONE',  ( 12.24304070169736747, 0.2736148576388583442, -12.69603606445786959 ) ) ;
#50770 = CARTESIAN_POINT ( 'NONE',  ( 12.63955452181609651, 0.7113363331415045732, 13.98191770012929958 ) ) ;
#50771 = B_SPLINE_CURVE_WITH_KNOTS ( 'NONE', 3,
 ( #61159, #34940, #66737, #13277, #61499, #34603, #51009, #24441, #55916, #18856 ),
 .UNSPECIFIED., .F., .F.,
 ( 4, 2, 2, 2, 4 ),
 ( 0.000000000000000000, 0.2499999999999996669, 0.4999999999999993339, 0.7499999999999996669, 1.000000000000000000 ),
 .UNSPECIFIED. ) ;
#50772 = ORIENTED_EDGE ( 'NONE', *, *, #35203, .F. ) ;
#50773 = DIRECTION ( 'NONE',  ( 0.000000000000000000, -1.000000000000000000, 0.000000000000000000 ) ) ;
#50774 = FACE_OUTER_BOUND ( 'NONE', #23178, .T. ) ;
#50775 = EDGE_CURVE ( 'NONE', #42540, #19870, #34434, .T. ) ;
#50776 = CARTESIAN_POINT ( 'NONE',  ( 24.51038697288600332, -3.518813880144999739, -12.24495765776000056 ) ) ;
#50777 = DIRECTION ( 'NONE',  ( 0.7071062208423759543, 0.7071073415302749909, -1.056390868722963888E-09 ) ) ;
#50778 = VECTOR ( 'NONE', #59984, 1000.000000000000227 ) ;
#50779 = B_SPLINE_SURFACE_WITH_KNOTS ( 'NONE', 3, 3, ( 
 ( #5225, #56992, #46511, #68156, #10465, #37048, #9778, #20621, #15031, #67813, #58028, #58363, #41602, #4527, #30433, #4874, #31807, #41258, #3837, #62910, #36355, #25863, #20967, #47196, #14353, #68498, #42304, #53124, #41945, #19937, #25176, #62573, #63254, #47888, #21306 ),
 ( #37730, #48914, #60093, #38416, #59741, #11842, #6246, #28277, #17442, #5905, #16738, #38067, #32155, #33180, #59392, #54498, #1359, #64283, #6945, #58709, #43327, #27588, #10813, #64632, #6598, #49598, #53806, #16400, #22676, #32493, #1705, #53471, #27246, #59056, #27939 ),
 ( #11492, #32837, #11158, #49250, #5564, #54149, #42635, #37386, #1022, #22332, #43672, #38769, #12199, #64969, #17083, #26906, #44021, #42976, #65324, #33527, #54846, #63944, #16056, #48220, #326, #21641, #48569, #673, #21985, #2058, #40480, #61807, #18827, #39112, #34907 ),
 ( #13924, #51320, #13245, #67046, #35251, #28633, #60436, #44374, #3076, #24061, #34570, #23376, #56565, #8672, #40153, #12543, #56222, #55189, #44715, #66359, #55885, #45396, #8332, #28986, #29675, #61128, #65672, #33874, #45737, #60778, #7990, #7293, #50978, #30019, #61467 ) ),
 .UNSPECIFIED., .F., .F., .F.,
 ( 4, 4 ),
 ( 4, 1, 1, 1, 1, 1, 1, 1, 1, 1, 1, 1, 1, 1, 1, 1, 1, 1, 1, 1, 1, 1, 1, 1, 1, 1, 1, 1, 1, 1, 1, 1, 4 ),
 ( -0.1039086239011999951, 1.103908623900999864 ),
 ( 0.2233333333344000027, 0.2480800653604999795, 0.2728267973865999840, 0.2975735294126999886, 0.3223202614387999931, 0.3470669934649999733, 0.3718137254910999778, 0.3965604575171999824, 0.4213071895433000424, 0.4460539215694000470, 0.4708006535954999960, 0.4955473856216000006, 0.5202941176476999496, 0.5450408496738000652, 0.5697875816999000698, 0.5945343137260000743, 0.6192810457521999989, 0.6440277777783000035, 0.6687745098044000081, 0.6935212418305000126, 0.7182679738566000172, 0.7430147058827000217, 0.7677614379088000263, 0.7925081699349000308, 0.8172549019609999243, 0.8420016339870999289, 0.8667483660132000445, 0.8914950980394000801, 0.9162418300655000847, 0.9409885620915999782, 0.9657352941176999828, 0.9904820261437999873, 1.015228758169999912 ),
 .UNSPECIFIED. ) ;
#50780 = CARTESIAN_POINT ( 'NONE',  ( 8.854734522757450321, 2.650072343410613485, -7.676796296823138022 ) ) ;
#50781 = CARTESIAN_POINT ( 'NONE',  ( 10.57435795695566583, 5.250000000000000000, 7.192559817601734906 ) ) ;
#50782 = CARTESIAN_POINT ( 'NONE',  ( 0.5073805749851999503, 3.426971461775999650, -0.8894074146212000986 ) ) ;
#50783 = FACE_OUTER_BOUND ( 'NONE', #57604, .T. ) ;
#50784 = CARTESIAN_POINT ( 'NONE',  ( 12.78084604758900333, 3.199697762315041771, 12.18695750762853081 ) ) ;
#50785 = CARTESIAN_POINT ( 'NONE',  ( 9.685492310842999331, -4.505165106450999879, -8.732017808253001334 ) ) ;
#50786 = CARTESIAN_POINT ( 'NONE',  ( 10.35826357027499789, 4.850513154668600002, -7.664090691848299386 ) ) ;
#50787 = CARTESIAN_POINT ( 'NONE',  ( 18.29998537156716054, 2.924732060074958895, 11.97422863287303052 ) ) ;
#50788 = CARTESIAN_POINT ( 'NONE',  ( 10.83487665876999984, 5.800192368099000184, -7.920541111170000370 ) ) ;
#50789 = CARTESIAN_POINT ( 'NONE',  ( 9.531329965421999617, 3.206942993865000258, -8.321459087847200564 ) ) ;
#50791 = CARTESIAN_POINT ( 'NONE',  ( 12.18494477640587270, 2.419331844832663503, 12.47000601351364324 ) ) ;
#50790 = CARTESIAN_POINT ( 'NONE',  ( 9.519772138681998896, -4.322628849750500102, 8.304747519296199698 ) ) ;
#50792 = DIRECTION ( 'NONE',  ( 0.000000000000000000, 0.5000000000000169864, -0.8660254037844288266 ) ) ;
#50793 = ORIENTED_EDGE ( 'NONE', *, *, #29393, .F. ) ;
#50794 = B_SPLINE_CURVE_WITH_KNOTS ( 'NONE', 3,
 ( #56253, #12921, #67073, #8360 ),
 .UNSPECIFIED., .F., .F.,
 ( 4, 4 ),
 ( 0.000000000000000000, 1.000000000000000000 ),
 .UNSPECIFIED. ) ;
#50795 = CARTESIAN_POINT ( 'NONE',  ( 9.934999999999998721, -4.640430492595999823, -9.117542781427999898 ) ) ;
#50796 = CIRCLE ( 'NONE', #48541, 1.350000000000000533 ) ;
#50797 = CARTESIAN_POINT ( 'NONE',  ( 9.352255147285999826, -2.817754448466000206, 6.388456890282999900 ) ) ;
#50798 = B_SPLINE_CURVE_WITH_KNOTS ( 'NONE', 3,
 ( #12447, #50542, #60341, #18732, #2642, #55098, #49851, #1961 ),
 .UNSPECIFIED., .F., .F.,
 ( 4, 2, 2, 4 ),
 ( 0.000000000000000000, 0.5000000000000000000, 0.7500000000000000000, 1.000000000000000000 ),
 .UNSPECIFIED. ) ;
#50799 = CARTESIAN_POINT ( 'NONE',  ( 9.781659112603998452, 3.563556310301200014, 6.595367916746299741 ) ) ;
#50800 = CARTESIAN_POINT ( 'NONE',  ( 10.01210369451062654, 3.801861024511436593, -6.647783351891156656 ) ) ;
#50801 = LINE ( 'NONE', #41335, #1969 ) ;
#50802 = ADVANCED_FACE ( 'NONE', ( #17764 ), #39082, .T. ) ;
#50803 = CARTESIAN_POINT ( 'NONE',  ( 12.72092075291582880, 3.120619064207561077, 13.52200130461806005 ) ) ;
#50804 = ORIENTED_EDGE ( 'NONE', *, *, #23853, .F. ) ;
#50805 = CARTESIAN_POINT ( 'NONE',  ( 9.733963142879998642, -2.882742046518000034, -7.264481182560499128 ) ) ;
#50806 = DIRECTION ( 'NONE',  ( 1.000000000000000000, 0.000000000000000000, 0.000000000000000000 ) ) ;
#50807 = CARTESIAN_POINT ( 'NONE',  ( 18.13398081625433633, 2.046400819240500546, -12.43272243325428406 ) ) ;
#50808 = CARTESIAN_POINT ( 'NONE',  ( 2.740556799209334038, -3.500000000000003109, 0.4581489286484972667 ) ) ;
#50809 = FACE_OUTER_BOUND ( 'NONE', #30969, .T. ) ;
#50810 = CARTESIAN_POINT ( 'NONE',  ( 12.26369778066962901, 2.812515541859847534, -13.60219590383643684 ) ) ;
#50811 = CARTESIAN_POINT ( 'NONE',  ( 9.084135711596999840, -5.371875912611999482, -7.370590366721999409 ) ) ;
#50812 = CARTESIAN_POINT ( 'NONE',  ( 9.064883232718324635, 5.349954811645839747, -7.500006748065883855 ) ) ;
#50813 = VERTEX_POINT ( 'NONE', #59709 ) ;
#50814 = CARTESIAN_POINT ( 'NONE',  ( 24.84741819964900245, -11.95754057833999973, -2.993661166240999982 ) ) ;
#50815 = CARTESIAN_POINT ( 'NONE',  ( 12.75722769875344476, -0.7290248443971383274, -13.98100598729141097 ) ) ;
#50816 = CARTESIAN_POINT ( 'NONE',  ( 13.99974593105000231, -8.811008772734998828, -7.563940656188999689 ) ) ;
#50817 = LINE ( 'NONE', #8507, #49938 ) ;
#50818 = CARTESIAN_POINT ( 'NONE',  ( 25.47131263472500251, -8.417328722977000410, -7.979452786042999790 ) ) ;
#50819 = CARTESIAN_POINT ( 'NONE',  ( 8.573539158775000502, 5.361622798585000460, -7.185294144754000634 ) ) ;
#50820 = CARTESIAN_POINT ( 'NONE',  ( 12.28594988689359901, -3.606563555963900214, 6.728309553046099012 ) ) ;
#50821 = VERTEX_POINT ( 'NONE', #39774 ) ;
#50822 = CARTESIAN_POINT ( 'NONE',  ( 11.00000000000000000, -4.000000000000000000, -7.500000000000000000 ) ) ;
#50823 = CARTESIAN_POINT ( 'NONE',  ( 17.88735652878715499, 1.970265470216408410, -13.77164815731349634 ) ) ;
#50824 = ORIENTED_EDGE ( 'NONE', *, *, #7740, .F. ) ;
#50825 = CARTESIAN_POINT ( 'NONE',  ( 8.539089945104599622, 4.176610156107851246, 8.851086029037343650 ) ) ;
#50826 = CARTESIAN_POINT ( 'NONE',  ( 24.44496351116800170, 3.224881296174999967, 12.03535797436000010 ) ) ;
#50827 = CARTESIAN_POINT ( 'NONE',  ( 9.251970280414001380, 5.673443217382001080, -7.051790060464000476 ) ) ;
#50828 = CARTESIAN_POINT ( 'NONE',  ( 18.30003129332100187, 2.732683818840999646, 11.53064095373000164 ) ) ;
#50829 = CARTESIAN_POINT ( 'NONE',  ( 11.01790547754519878, -2.825704134258000266, -7.537269019642879542 ) ) ;
#50830 = CYLINDRICAL_SURFACE ( 'NONE', #64974, 0.5000000000000002220 ) ;
#50831 = CARTESIAN_POINT ( 'NONE',  ( 9.051300837857860770, -2.809882456706737308, -7.723566111296684689 ) ) ;
#50832 = ORIENTED_EDGE ( 'NONE', *, *, #57561, .T. ) ;
#50833 = CARTESIAN_POINT ( 'NONE',  ( 7.785267505008289568, 3.263780494496031359, -8.649333714453984356 ) ) ;
#50834 = EDGE_CURVE ( 'NONE', #60944, #32326, #47792, .T. ) ;
#50835 = CARTESIAN_POINT ( 'NONE',  ( 10.66684687351566652, -3.231816600031351516, 8.499583552997723501 ) ) ;
#50836 = CARTESIAN_POINT ( 'NONE',  ( 8.699089158774000907, 4.178200486578000472, -5.608493638783999202 ) ) ;
#50837 = ORIENTED_EDGE ( 'NONE', *, *, #64332, .F. ) ;
#50838 = CARTESIAN_POINT ( 'NONE',  ( 10.85290485628999946, 3.170386876061999537, -8.782184998573001167 ) ) ;
#50839 = ORIENTED_EDGE ( 'NONE', *, *, #44982, .F. ) ;
#50840 = CARTESIAN_POINT ( 'NONE',  ( 9.303367640780999537, 4.538247246588100303, 8.506987760366000018 ) ) ;
#50841 = CARTESIAN_POINT ( 'NONE',  ( 18.05422494319417481, -1.958382419481337955, -12.44687927882536194 ) ) ;
#50842 = AXIS2_PLACEMENT_3D ( 'NONE', #20397, #3286, #57796 ) ;
#50843 = DIRECTION ( 'NONE',  ( 0.000000000000000000, -0.2588190451024932059, 0.9659258262890756397 ) ) ;
#50844 = CARTESIAN_POINT ( 'NONE',  ( 25.29987261392200182, 8.756202924575998026, -7.455126447192999883 ) ) ;
#50845 = B_SPLINE_CURVE_WITH_KNOTS ( 'NONE', 3,
 ( #40972, #62961, #67874, #14749 ),
 .UNSPECIFIED., .F., .F.,
 ( 4, 4 ),
 ( 0.000000000000000000, 1.000000000000000000 ),
 .UNSPECIFIED. ) ;
#50846 = CARTESIAN_POINT ( 'NONE',  ( 24.25375554908000097, -12.19812635653999955, -3.308082274583000526 ) ) ;
#50847 = CARTESIAN_POINT ( 'NONE',  ( 9.354587383407045209, -3.357689054377400062, 9.116474598616981950 ) ) ;
#50848 = VERTEX_POINT ( 'NONE', #60744 ) ;
#50849 = LINE ( 'NONE', #3625, #18051 ) ;
#50850 = CARTESIAN_POINT ( 'NONE',  ( 11.10664834123000055, 5.324188120986000250, -7.809342242343999985 ) ) ;
#50851 = EDGE_CURVE ( 'NONE', #12119, #5014, #55506, .T. ) ;
#50852 = CARTESIAN_POINT ( 'NONE',  ( 8.710288521113000115, 3.647046440108700160, 6.715449042252499723 ) ) ;
#50853 = CARTESIAN_POINT ( 'NONE',  ( 12.38095956647852880, 3.110256499846526079, -13.65014134263124390 ) ) ;
#50854 = CARTESIAN_POINT ( 'NONE',  ( 9.051138961223999857, -2.940105638081000006, -8.216246114996598848 ) ) ;
#50855 = EDGE_CURVE ( 'NONE', #42399, #20484, #38733, .T. ) ;
#50856 = CARTESIAN_POINT ( 'NONE',  ( 10.80815535238000002, -2.937528991339000140, 8.948455587554001056 ) ) ;
#50857 = CARTESIAN_POINT ( 'NONE',  ( 18.26112155826667305, 0.1662062226620437122, 13.99901824074930978 ) ) ;
#50858 = FACE_OUTER_BOUND ( 'NONE', #26493, .T. ) ;
#50859 = VERTEX_POINT ( 'NONE', #12859 ) ;
#50860 = ORIENTED_EDGE ( 'NONE', *, *, #1062, .F. ) ;
#50861 = CARTESIAN_POINT ( 'NONE',  ( 8.839404719593998649, 5.140767546012999567, -6.196177269779999719 ) ) ;
#50862 = CARTESIAN_POINT ( 'NONE',  ( 7.000000000000000000, -0.2897247358851999799, 3.000000000000000000 ) ) ;
#50863 = CIRCLE ( 'NONE', #27401, 1.300177795737000874 ) ;
#50864 = CARTESIAN_POINT ( 'NONE',  ( 7.413221459149189840, -4.978041439725138240, 6.521863944591406614 ) ) ;
#50865 = CARTESIAN_POINT ( 'NONE',  ( 3.999985533191000364, -6.914809019160056625E-16, -2.149963194831858715 ) ) ;
#50866 = CARTESIAN_POINT ( 'NONE',  ( 4.900006121741999010, -2.000000000000000000, 0.000000000000000000 ) ) ;
#50867 = CARTESIAN_POINT ( 'NONE',  ( 18.44382898362900036, -2.795331802377000407, -11.36579223931000016 ) ) ;
#50869 = CARTESIAN_POINT ( 'NONE',  ( 11.07071167063000061, -5.425576677726000163, 5.078384236784999395 ) ) ;
#50868 = CARTESIAN_POINT ( 'NONE',  ( 10.96755864497999866, -3.101067942814400347, 6.795973491698399371 ) ) ;
#50871 = AXIS2_PLACEMENT_3D ( 'NONE', #30051, #40513, #62180 ) ;
#50870 = CARTESIAN_POINT ( 'NONE',  ( 0.7431103717477000048, 2.848815883361000001, -1.248255999701999963 ) ) ;
#50872 = ORIENTED_EDGE ( 'NONE', *, *, #46487, .F. ) ;
#50873 = CARTESIAN_POINT ( 'NONE',  ( 12.07990818254330989, 0.1906559481176479942, 14.00000681886699816 ) ) ;
#50874 = CARTESIAN_POINT ( 'NONE',  ( 10.71991265383000069, -2.957947977237000092, -5.111881366068000254 ) ) ;
#50875 = CARTESIAN_POINT ( 'NONE',  ( 17.55505043854144631, 0.6250000000000001110, 12.67928921589117586 ) ) ;
#50876 = CARTESIAN_POINT ( 'NONE',  ( 12.60485626885975030, -0.5921620644301640590, 12.68141136812944758 ) ) ;
#50877 = CARTESIAN_POINT ( 'NONE',  ( 9.865041550948088656, -2.650034642413194419, -7.500002425457253707 ) ) ;
#50878 = VERTEX_POINT ( 'NONE', #50259 ) ;
#50880 = CARTESIAN_POINT ( 'NONE',  ( 9.911030043039486870, 5.348901746907112731, 7.263562664566891591 ) ) ;
#50879 = CARTESIAN_POINT ( 'NONE',  ( 8.316694475082000437, 2.898380349184999982, 6.611503672649000407 ) ) ;
#50881 = DIRECTION ( 'NONE',  ( 0.000000000000000000, -0.1807154286440006141, 0.9835354258236025382 ) ) ;
#50882 = CARTESIAN_POINT ( 'NONE',  ( 10.37041638348499895, 2.758294858530000226, 7.802464414828100381 ) ) ;
#50883 = VECTOR ( 'NONE', #17251, 1000.000000000000000 ) ;
#50884 = CYLINDRICAL_SURFACE ( 'NONE', #36699, 11.35000000000000142 ) ;
#50885 = VECTOR ( 'NONE', #23461, 1000.000000000000114 ) ;
#50886 = DIRECTION ( 'NONE',  ( 0.000000000000000000, -1.000000000000000000, 0.000000000000000000 ) ) ;
#50887 = CARTESIAN_POINT ( 'NONE',  ( 3.405885792876999663, -3.196388832542000014, -1.639155108791999993 ) ) ;
#50888 = ORIENTED_EDGE ( 'NONE', *, *, #47268, .F. ) ;
#50889 = CARTESIAN_POINT ( 'NONE',  ( 12.51625386035102139, 0.6598665579121970604, -12.58271022457859978 ) ) ;
#50890 = CARTESIAN_POINT ( 'NONE',  ( 11.97822875044625057, -3.830319670899316353, 8.360317195474184615 ) ) ;
#50891 = DIRECTION ( 'NONE',  ( 1.000000000000000000, 0.000000000000000000, 0.000000000000000000 ) ) ;
#50892 = DIRECTION ( 'NONE',  ( -5.700570686033077343E-06, 0.7070792536779096915, 0.7071343076006096906 ) ) ;
#50893 = CARTESIAN_POINT ( 'NONE',  ( 5.500000000000000000, -1.199999999999999956, 9.776630298829998011 ) ) ;
#50894 = ORIENTED_EDGE ( 'NONE', *, *, #21851, .F. ) ;
#50895 = CARTESIAN_POINT ( 'NONE',  ( 6.328305643943999748, -0.7806768893493000183, 1.067248597240000096 ) ) ;
#50896 = B_SPLINE_CURVE_WITH_KNOTS ( 'NONE', 3,
 ( #30102, #51405, #67130, #18568, #24497, #39196, #39894, #51065, #45819, #61214, #19240, #44797, #13331, #39544, #60518, #12628, #66100, #60866, #34997, #12982, #23804, #45136, #34304, #33956, #8073, #29416, #40568, #13668, #3501, #3167, #50034, #2818, #61895, #35339, #14010, #45481, #8760, #55627, #35680, #3838, #19595, #42305, #63607, #46512, #56993, #37049, #10130, #46854, #25864, #68157, #25177, #15723, #41946, #63255, #15381, #9779, #68499, #4188, #36710, #20622, #9095, #58030, #4875, #41603, #47545, #51745, #62911, #67814, #40915, #62237, #19938, #41260, #31462, #62574, #9429, #58364, #4528, #25525, #15032, #26217, #47197, #52780, #31808, #68849, #53125, #52432, #20968, #10466, #5226, #36356, #57328, #46166, #30434, #14694, #14354, #57671, #67473, #20277, #31129, #36012, #30772, #52084, #48915, #59742, #64970, #33528, #60094, #26563, #11843, #12200, #47889, #33181, #59057, #69194, #37387, #6599, #42636, #54847, #21307, #27941, #54499, #22677, #37731, #32494, #27589, #26907, #16401, #63945, #1360, #16057, #49251, #1023, #64633, #674, #17443, #58710, #10814, #11493, #22334, #32156, #53472, #42977, #44022, #65325, #21986, #59394, #43329, #38770, #5566, #16740, #43673, #38068, #32838, #6247, #64284, #11159, #48221, #327, #5906, #21642, #53807, #54150, #27247, #48570, #17084, #38417, #60779, #34571, #39806, #23717, #61470, #50979, #2393, #24062, #45052, #66360, #55887, #23377, #44716, #29676, #33875, #45738, #7991, #28634, #13246, #18136, #49946, #56223, #67048, #12893, #29324, #7294, #65673, #19157, #40154, #7639, #50636, #28987, #55192, #3077, #2737, #45397, #61129, #66707, #34221, #18828, #13589, #17795, #34909, #50295, #12544, #8333, #24410, #2059, #40481, #18481, #39114, #61808, #13926, #35252, #6946, #39458, #28278, #49599, #55541, #1706, #23025, #44375, #60437, #66013, #9692, #19850, #26127, #9341, #30686, #20532, #3753, #30350, #25093, #31039, #63520, #30020, #25434, #57585, #35928, #51994, #8673, #20878, #10038, #36618, #41858, #46077, #46423, #9009, #68070, #4098, #24752, #52347, #51658, #42215, #31377, #67385, #57942, #3417, #15634, #51322, #52689, #63164, #19507, #20187, #35596, #40824, #46767, #56568, #62150, #4785, #14268, #62826, #56910, #67725, #41515, #47454, #41179, #62486, #14944, #4441, #14610, #57240, #36270, #68410, #25780, #47111, #68759, #15293, #37642, #16659, #58974, #63858, #33097, #32752, #54065, #1279, #22593, #38330, #11076, #64887, #10382, #32411, #27503, #17001, #53726, #59660, #42550, #5825, #58623, #31720, #53042, #37301, #32071, #6162, #10724, #21899, #48140, #53386, #5137, #27162, #590, #11756, #48829, #43936, #938, #65240, #43237, #22250, #6514, #43588, #48483, #243, #27859, #26474, #15972, #64543, #54414, #49167, #37984, #47807, #69113, #59310, #36965, #11411, #58279, #21221, #5487, #26822, #21557, #42893, #64200, #16315, #39726, #33794, #38683, #28551, #28907, #44637, #49861, #2653, #23296, #44973, #29244, #55109, #7214, #7553, #44292, #12460, #60004, #50554, #33444, #55805 ),
 .UNSPECIFIED., .F., .F.,
 ( 4, 2, 2, 2, 2, 2, 1, 1, 1, 2, 2, 2, 2, 2, 2, 1, 2, 2, 2, 2, 1, 2, 2, 2, 2, 1, 1, 2, 2, 1, 2, 2, 2, 2, 2, 2, 2, 2, 2, 2, 2, 2, 2, 2, 2, 2, 2, 2, 1, 2, 2, 2, 2, 1, 1, 1, 2, 2, 2, 2, 2, 2, 2, 2, 1, 2, 2, 2, 2, 2, 2, 1, 2, 1, 2, 2, 1, 2, 2, 2, 2, 2, 1, 1, 2, 2, 2, 2, 2, 2, 2, 2, 1, 2, 2, 2, 2, 2, 2, 2, 2, 2, 2, 1, 2, 2, 2, 2, 1, 1, 1, 2, 2, 2, 2, 2, 2, 2, 2, 1, 1, 2, 2, 2, 2, 2, 2, 2, 1, 1, 2, 2, 2, 2, 1, 1, 1, 2, 2, 2, 2, 2, 2, 2, 2, 2, 2, 2, 2, 2, 1, 2, 2, 2, 2, 1, 2, 2, 2, 2, 1, 1, 1, 2, 2, 2, 2, 2, 2, 2, 2, 1, 2, 2, 2, 2, 2, 2, 2, 1, 1, 2, 2, 2, 2, 1, 1, 1, 2, 2, 2, 2, 2, 2, 2, 2, 1, 2, 2, 2, 2, 2, 1, 2, 2, 2, 2, 1, 2, 2, 4 ),
 ( 0.000000000000000000, 0.01562500000001094264, 0.03125000000002188527, 0.06250000000004377054, 0.07031250000004928002, 0.07421875000005202783, 0.07617187500005341561, 0.07714843750005409562, 0.07763671875005451195, 0.07788085937505478951, 0.07812500000005508094, 0.08203125000006007694, 0.08398437500006267209, 0.08447265625006321332, 0.08496093750006374068, 0.08593750000006465661, 0.09375000000007154000, 0.09765625000007492618, 0.09814453125007535639, 0.09863281250007577272, 0.09960937500007630008, 0.1015625000000773409, 0.1093750000000812406, 0.1113281250000822259, 0.1118164062500824757, 0.1123046875000827116, 0.1132812500000833084, 0.1171875000000856676, 0.1210937500000880268, 0.1230468750000891509, 0.1240234375000897199, 0.1250000000000902611, 0.1562500000001111611, 0.1718750000001215972, 0.1875000000001320333, 0.1953125000001372236, 0.1962890625001378897, 0.1972656250001385281, 0.1992187500001398603, 0.2031250000001424694, 0.2070312500001451061, 0.2089843750001464384, 0.2099609375001471323, 0.2109375000001477984, 0.2187500000001537104, 0.2226562500001565970, 0.2231445312501569300, 0.2236328125001572908, 0.2246093750001579570, 0.2265625000001592892, 0.2343750000001645628, 0.2421875000001698364, 0.2460937500001725009, 0.2480468750001738609, 0.2490234375001745271, 0.2495117187501748601, 0.2497558593751748324, 0.2500000000001748046, 0.2656250000001770806, 0.2812500000001793565, 0.3125000000001840195, 0.3203125000001850742, 0.3242187500001856293, 0.3261718750001860179, 0.3271484375001862399, 0.3276367187501863509, 0.3281250000001865175, 0.3320312500001871281, 0.3339843750001875167, 0.3344726562501874056, 0.3349609375001872946, 0.3359375000001870726, 0.3437500000001854628, 0.3476562500001845746, 0.3481445312501844636, 0.3486328125001843525, 0.3496093750001842415, 0.3515625000001838529, 0.3593750000001824096, 0.3671875000001809108, 0.3710937500001801892, 0.3730468750001795231, 0.3740234375001792455, 0.3745117187501793010, 0.3747558593751790235, 0.3750000000001787459, 0.4062500000001486589, 0.4218750000001336153, 0.4375000000001185718, 0.4453125000001111333, 0.4462890625001101896, 0.4467773437501098011, 0.4472656250001093570, 0.4492187500001074696, 0.4531250000001035283, 0.4570312500000995315, 0.4589843750000976441, 0.4599609375000966449, 0.4609375000000956457, 0.4687500000000878742, 0.4726562500000838773, 0.4731445312500832112, 0.4736328125000825451, 0.4746093750000812128, 0.4765625000000783817, 0.4843750000000671130, 0.4921875000000557887, 0.4960937500000501821, 0.4980468750000473510, 0.4990234375000460743, 0.4995117187500454081, 0.4997558593750451861, 0.5000000000000449640, 0.5156250000000307532, 0.5312500000000164313, 0.5624999999999878986, 0.5703124999999807931, 0.5712890624999799050, 0.5715332031249795719, 0.5717773437499793499, 0.5722656249999789058, 0.5742187499999770184, 0.5781249999999733546, 0.5859374999999660272, 0.5937499999999586997, 0.5976562499999550360, 0.5981445312499544809, 0.5983886718749541478, 0.5986328124999537037, 0.5996093749999521494, 0.6015624999999492628, 0.6093749999999371614, 0.6171874999999250599, 0.6210937499999190647, 0.6230468749999160671, 0.6240234374999148459, 0.6245117187499145128, 0.6247558593749144018, 0.6249999999999141798, 0.6562499999998935296, 0.6718749999998830935, 0.6874999999998727684, 0.6953124999998676614, 0.6962890624998668843, 0.6972656249998661071, 0.6992187499998651079, 0.7031249999998631095, 0.7070312499998612221, 0.7089843749998602229, 0.7099609374998596678, 0.7109374999998592237, 0.7187499999998558931, 0.7226562499998542277, 0.7231445312498538946, 0.7236328124998535616, 0.7246093749998531175, 0.7265624999998522293, 0.7343749999998488986, 0.7421874999998456790, 0.7460937499998440137, 0.7480468749998432365, 0.7490234374998427924, 0.7495117187498425704, 0.7497558593748424594, 0.7499999999998424594, 0.7656249999998324673, 0.7812499999998223643, 0.8124999999998024913, 0.8203124999997976063, 0.8212890624997970512, 0.8217773437497968292, 0.8222656249997966071, 0.8242187499997956079, 0.8281249999997936095, 0.8359374999997895017, 0.8437499999997853939, 0.8476562499997833955, 0.8481445312497839506, 0.8483886718747842837, 0.8486328124997845057, 0.8496093749997857270, 0.8515624999997882805, 0.8593749999997979394, 0.8671874999998075983, 0.8710937499998125944, 0.8730468749998150368, 0.8740234374998161471, 0.8745117187498168132, 0.8747558593748171463, 0.8749999999998173683, 0.9062499999998596678, 0.9218749999998806510, 0.9374999999999017453, 0.9453124999999122924, 0.9462890624999136246, 0.9467773437499142908, 0.9472656249999149569, 0.9492187499999179545, 0.9531249999999238387, 0.9570312499999298339, 0.9589843749999327205, 0.9599609374999341638, 0.9609374999999357181, 0.9687499999999472644, 0.9726562499999531486, 0.9731445312499539257, 0.9736328124999547029, 0.9746093749999563682, 0.9765624999999596989, 0.9843749999999731326, 1.000000000000000000 ),
 .UNSPECIFIED. ) ;
#50897 = CARTESIAN_POINT ( 'NONE',  ( 8.286185841226000548, 2.892522941075999832, -8.352379580902999479 ) ) ;
#50898 = CARTESIAN_POINT ( 'NONE',  ( 7.400000000000000355, 0.000000000000000000, -0.5999999999999999778 ) ) ;
#50899 = CARTESIAN_POINT ( 'NONE',  ( 7.805634476667997035, 3.004029196385564759, 6.538900385249459823 ) ) ;
#50900 = CARTESIAN_POINT ( 'NONE',  ( 11.75203632436369894, 2.890282938442000127, -7.240848640331599917 ) ) ;
#50901 = ORIENTED_EDGE ( 'NONE', *, *, #20787, .F. ) ;
#50902 = CARTESIAN_POINT ( 'NONE',  ( 9.555699158955999195, -2.440755924888999839, 6.680881588809999272 ) ) ;
#50903 = VERTEX_POINT ( 'NONE', #28956 ) ;
#50904 = CARTESIAN_POINT ( 'NONE',  ( 25.60000000000000142, 0.000000000000000000, 0.000000000000000000 ) ) ;
#50905 = CARTESIAN_POINT ( 'NONE',  ( 8.496691940379001551, -5.198566224659999513, 8.332559954171999905 ) ) ;
#50906 = CARTESIAN_POINT ( 'NONE',  ( 18.16428164030675418, -0.3960277493246738278, -13.99440111282555499 ) ) ;
#50907 = ORIENTED_EDGE ( 'NONE', *, *, #22102, .F. ) ;
#50908 = CARTESIAN_POINT ( 'NONE',  ( 10.92189663471096672, 9.599264226479007789, -5.980252649074441429 ) ) ;
#50909 = CARTESIAN_POINT ( 'NONE',  ( 9.099999952505998024, -4.000000000000000000, 6.750000006358199300 ) ) ;
#50910 = CYLINDRICAL_SURFACE ( 'NONE', #45977, 2.149999999999999911 ) ;
#50911 = CARTESIAN_POINT ( 'NONE',  ( 4.500000125099000492, -12.99999867215000116, 0.000000000000000000 ) ) ;
#50912 = CARTESIAN_POINT ( 'NONE',  ( 24.62769666370868293, 3.584151135403405242, 12.19978398757196203 ) ) ;
#50913 = EDGE_LOOP ( 'NONE', ( #17772, #47431, #38486, #6588, #57246, #24542, #11109, #27694, #9753 ) ) ;
#50914 = CARTESIAN_POINT ( 'NONE',  ( 10.71256247620999957, -5.951803124515000043, 7.233045248871000865 ) ) ;
#50915 = EDGE_CURVE ( 'NONE', #11428, #25814, #38542, .T. ) ;
#50916 = EDGE_CURVE ( 'NONE', #2080, #65525, #13549, .T. ) ;
#50917 = CARTESIAN_POINT ( 'NONE',  ( 12.18032316970823992, -2.521073842608297255, -13.66891947082361369 ) ) ;
#50918 = CARTESIAN_POINT ( 'NONE',  ( 10.63351354018304740, 5.250000000000001776, -7.663624617374467540 ) ) ;
#50919 = CARTESIAN_POINT ( 'NONE',  ( 11.00152743473872796, 5.208048404074126836, 6.643475722637898429 ) ) ;
#50920 = DIRECTION ( 'NONE',  ( -1.000000000000000000, 0.000000000000000000, 0.000000000000000000 ) ) ;
#50921 = ORIENTED_EDGE ( 'NONE', *, *, #5813, .F. ) ;
#50922 = CARTESIAN_POINT ( 'NONE',  ( 23.59999462723899910, 13.22316330987000121, -4.267799687262000319 ) ) ;
#50923 = CARTESIAN_POINT ( 'NONE',  ( 10.93769855012999948, 2.936883479403999964, 4.920828759365000415 ) ) ;
#50924 = CARTESIAN_POINT ( 'NONE',  ( 3.500000000000000444, 1.881896910667459455, 2.804129112111227062 ) ) ;
#50925 = CARTESIAN_POINT ( 'NONE',  ( 24.63328775060330855, 2.078227413906825305, 11.31065739981925766 ) ) ;
#50926 = CARTESIAN_POINT ( 'NONE',  ( 12.80505043854144276, 0.6249999999999994449, 12.67928921589117586 ) ) ;
#50927 = B_SPLINE_CURVE_WITH_KNOTS ( 'NONE', 3,
 ( #41850, #35589, #42208, #68401 ),
 .UNSPECIFIED., .F., .F.,
 ( 4, 4 ),
 ( 0.000000000000000000, 1.000000000000000000 ),
 .UNSPECIFIED. ) ;
#50928 = CARTESIAN_POINT ( 'NONE',  ( 12.39257741226468745, -0.4700078255514623660, -13.88931146942755390 ) ) ;
#50929 = CARTESIAN_POINT ( 'NONE',  ( 18.08682736286122150, -2.829024318083993794, 12.36883279713290484 ) ) ;
#50930 = EDGE_LOOP ( 'NONE', ( #25100, #11831, #22005, #41380, #34609 ) ) ;
#50931 = CARTESIAN_POINT ( 'NONE',  ( 11.52166954483529793, -3.437903757373499847, -6.632714178206799538 ) ) ;
#50932 = ORIENTED_EDGE ( 'NONE', *, *, #51607, .F. ) ;
#50933 = CARTESIAN_POINT ( 'NONE',  ( 10.09181485429000169, 2.440912084162000006, 7.817367409531000177 ) ) ;
#50934 = DIRECTION ( 'NONE',  ( -1.000000000000000000, 0.000000000000000000, 0.000000000000000000 ) ) ;
#50935 = CONICAL_SURFACE ( 'NONE', #38654, 2.049993715513000136, 0.7853981633972997312 ) ;
#50936 = CARTESIAN_POINT ( 'NONE',  ( 9.924495280410999598, 4.946705552514000459, -6.253848946732999181 ) ) ;
#50937 = CARTESIAN_POINT ( 'NONE',  ( 2.893924662652000102, -0.2530398175331999844, -3.699405519438999868 ) ) ;
#50938 = EDGE_CURVE ( 'NONE', #14252, #63419, #28245, .T. ) ;
#50939 = CARTESIAN_POINT ( 'NONE',  ( 10.05204995789999955, -2.669899884077999719, -8.791535702747999892 ) ) ;
#50940 = CIRCLE ( 'NONE', #55381, 12.99999854704999969 ) ;
#50941 = CARTESIAN_POINT ( 'NONE',  ( 24.96666885022796478, -8.756202917673951092, -7.455126455300256083 ) ) ;
#50942 = CARTESIAN_POINT ( 'NONE',  ( 9.016026733244713043, -5.181567068652970676, 8.154973437734131636 ) ) ;
#50943 = ORIENTED_EDGE ( 'NONE', *, *, #45395, .F. ) ;
#50944 = CARTESIAN_POINT ( 'NONE',  ( 11.19456919669529960, -2.906008650422999828, 7.176777099639999768 ) ) ;
#50945 = CARTESIAN_POINT ( 'NONE',  ( 10.44079719460000000, 5.435719122931000236, 7.303631812894000319 ) ) ;
#50946 = CARTESIAN_POINT ( 'NONE',  ( 13.00000000009400303, -11.69118001589999878, -1.923222888683999932 ) ) ;
#50947 = FACE_OUTER_BOUND ( 'NONE', #63772, .T. ) ;
#50949 = DIRECTION ( 'NONE',  ( 1.000000000000000000, 0.000000000000000000, 0.000000000000000000 ) ) ;
#50948 = CARTESIAN_POINT ( 'NONE',  ( 9.600491906670001185, 5.206545077004999911, 8.585111878242999595 ) ) ;
#50950 = CARTESIAN_POINT ( 'NONE',  ( 10.74795391537419853, 4.830118059977199785, -8.063786182297898009 ) ) ;
#50951 = FACE_OUTER_BOUND ( 'NONE', #58910, .T. ) ;
#50952 = CARTESIAN_POINT ( 'NONE',  ( 9.958963142879998287, 4.982812171771600518, -7.292822454528599785 ) ) ;
#50953 = CARTESIAN_POINT ( 'NONE',  ( 17.71955056974169906, -0.7009231686363515124, 12.58048995873113896 ) ) ;
#50954 = DIRECTION ( 'NONE',  ( -1.000000000000000000, 0.000000000000000000, 0.000000000000000000 ) ) ;
#50955 = CARTESIAN_POINT ( 'NONE',  ( 4.400000000000000355, 1.000000000000000000, 0.000000000000000000 ) ) ;
#50956 = CARTESIAN_POINT ( 'NONE',  ( 23.58665614796800014, 10.27456427064999822, 9.417482135191999504 ) ) ;
#50957 = ORIENTED_EDGE ( 'NONE', *, *, #6656, .T. ) ;
#50958 = CARTESIAN_POINT ( 'NONE',  ( 7.384456853207000293, -3.346260729029000291, 6.002247316312999459 ) ) ;
#50959 = CARTESIAN_POINT ( 'NONE',  ( 18.23099845246958850, 2.253777188809247711, 13.81740256423587709 ) ) ;
#50960 = LINE ( 'NONE', #25764, #25568 ) ;
#50961 = CARTESIAN_POINT ( 'NONE',  ( 10.06726717315599906, 3.340104753140699767, 8.062357722167599050 ) ) ;
#50962 = ORIENTED_EDGE ( 'NONE', *, *, #52334, .F. ) ;
#50963 = CARTESIAN_POINT ( 'NONE',  ( 7.486426658771000220, 5.321913229613000063, 8.118244847118999630 ) ) ;
#50964 = VECTOR ( 'NONE', #47817, 1000.000000000000000 ) ;
#50966 = CARTESIAN_POINT ( 'NONE',  ( 0.6119016313204127533, 2.532497055143216880, 2.470245038604635734 ) ) ;
#50965 = CARTESIAN_POINT ( 'NONE',  ( 9.591185841232000797, 2.173570076733999823, -8.023168429484000441 ) ) ;
#50967 = CARTESIAN_POINT ( 'NONE',  ( 9.964039158770999549, 3.485905350467000119, -9.275749134703000109 ) ) ;
#50968 = EDGE_CURVE ( 'NONE', #14810, #33733, #18448, .T. ) ;
#50969 = ORIENTED_EDGE ( 'NONE', *, *, #29634, .F. ) ;
#50970 = EDGE_CURVE ( 'NONE', #39042, #59819, #39906, .T. ) ;
#50971 = CARTESIAN_POINT ( 'NONE',  ( 5.200859839683333874, 0.3926218265389221362, -1.460959015002473160 ) ) ;
#50972 = CARTESIAN_POINT ( 'NONE',  ( 17.91962727382265541, -3.149549635603927200, -13.64113161598087665 ) ) ;
#50973 = CARTESIAN_POINT ( 'NONE',  ( 10.44841638348500013, 2.891666689023999925, 7.769976643522699788 ) ) ;
#50974 = CARTESIAN_POINT ( 'NONE',  ( 11.05935368890999904, -2.480241580537000168, 6.610077204591000566 ) ) ;
#50975 = DIRECTION ( 'NONE',  ( 0.000000000000000000, 1.000000000000000000, 0.000000000000000000 ) ) ;
#50976 = ORIENTED_EDGE ( 'NONE', *, *, #10420, .T. ) ;
#50977 = CARTESIAN_POINT ( 'NONE',  ( 11.56571517796000137, -3.339665324758999798, 11.82228365027999928 ) ) ;
#50978 = CARTESIAN_POINT ( 'NONE',  ( 10.19794194037999979, -4.262172867567000090, -8.834326937932999613 ) ) ;
#50979 = CARTESIAN_POINT ( 'NONE',  ( 7.908383208917886265, -2.485710556326794496, 8.356913658884913332 ) ) ;
#50980 = CARTESIAN_POINT ( 'NONE',  ( 10.40727044253999978, -3.797905333157999941, 5.889909992361999969 ) ) ;
#50982 = CARTESIAN_POINT ( 'NONE',  ( 11.39700581613019992, -3.130347327833300053, -8.058426314824099990 ) ) ;
#50981 = AXIS2_PLACEMENT_3D ( 'NONE', #5479, #22241, #37294 ) ;
#50983 = CARTESIAN_POINT ( 'NONE',  ( 10.63922949779700033, -3.366547096154099972, 6.550014196338999284 ) ) ;
#50984 = ORIENTED_EDGE ( 'NONE', *, *, #3173, .F. ) ;
#50985 = CARTESIAN_POINT ( 'NONE',  ( 10.31663362093999936, -4.574952992312999456, -4.565089889767000031 ) ) ;
#50986 = CARTESIAN_POINT ( 'NONE',  ( 11.01810807141099957, -3.940954591493389891, 6.223352037434000117 ) ) ;
#50987 = EDGE_LOOP ( 'NONE', ( #54004, #55603, #5843, #7134 ) ) ;
#50988 = CARTESIAN_POINT ( 'NONE',  ( 17.60000000798000386, 11.41069016990000051, -4.623987642516999230 ) ) ;
#50989 = EDGE_LOOP ( 'NONE', ( #37159, #7803, #38251 ) ) ;
#50990 = CARTESIAN_POINT ( 'NONE',  ( 11.09461754388165389, 3.670987266763324985, -9.018203014673396467 ) ) ;
#50991 = CARTESIAN_POINT ( 'NONE',  ( 8.854170280414001226, 4.902869380824999901, -8.978557145469999057 ) ) ;
#50992 = CARTESIAN_POINT ( 'NONE',  ( 21.05000000000000426, 0.000000000000000000, 0.000000000000000000 ) ) ;
#50993 = CYLINDRICAL_SURFACE ( 'NONE', #17659, 1.250000000000000222 ) ;
#50994 = CARTESIAN_POINT ( 'NONE',  ( 12.26301939624441317, 2.811829068737871307, -12.37346575716765962 ) ) ;
#50995 = CARTESIAN_POINT ( 'NONE',  ( 10.82949413291699869, -3.087070836781100169, 7.916546720849799712 ) ) ;
#50996 = CARTESIAN_POINT ( 'NONE',  ( 9.170323341230000480, 5.558938731259999599, 6.272977177425000050 ) ) ;
#50997 = EDGE_CURVE ( 'NONE', #49024, #23104, #26033, .T. ) ;
#50998 = ORIENTED_EDGE ( 'NONE', *, *, #25478, .F. ) ;
#50999 = CARTESIAN_POINT ( 'NONE',  ( 7.669816860518959167, 2.954814231707052929, 8.376417257409977779 ) ) ;
#51000 = EDGE_CURVE ( 'NONE', #59964, #14358, #35893, .T. ) ;
#51001 = CARTESIAN_POINT ( 'NONE',  ( 8.662855646795000197, -2.741638482234999952, 6.457327039244000311 ) ) ;
#51002 = CARTESIAN_POINT ( 'NONE',  ( 24.96666885018256821, -2.078227441565727140, 11.31065739473216070 ) ) ;
#51003 = ORIENTED_EDGE ( 'NONE', *, *, #56145, .T. ) ;
#51004 = CARTESIAN_POINT ( 'NONE',  ( 12.44904482565497794, -1.853472941501686400, -12.46293187093603017 ) ) ;
#51005 = CARTESIAN_POINT ( 'NONE',  ( 11.70379573085659786, 5.106255642043000087, 7.308581953418300081 ) ) ;
#51006 = CARTESIAN_POINT ( 'NONE',  ( 10.81188185321000006, -4.614147550108000928, -5.930138617968999881 ) ) ;
#51007 = CARTESIAN_POINT ( 'NONE',  ( 6.325859839683334762, 1.460959015002472494, 0.3926218265389232465 ) ) ;
#51008 = CARTESIAN_POINT ( 'NONE',  ( 17.95534550153200115, -3.277905616156999713, -11.84067279748999901 ) ) ;
#51009 = CARTESIAN_POINT ( 'NONE',  ( 9.824751812578400134, 5.732824308054384588, -7.158329579245652496 ) ) ;
#51010 = CARTESIAN_POINT ( 'NONE',  ( 12.27346860450520261, -2.829323760734076210, -13.59803440778111572 ) ) ;
#51011 = CARTESIAN_POINT ( 'NONE',  ( 11.50705667793316778, 4.601576474242010661, -8.661791977777625107 ) ) ;
#51012 = SURFACE_STYLE_USAGE ( .BOTH. , #53838 ) ;
#51013 = CARTESIAN_POINT ( 'NONE',  ( 11.03502897915239878, -3.672866099873000056, -8.735435061820998826 ) ) ;
#51014 = LINE ( 'NONE', #20222, #51192 ) ;
#51015 = ORIENTED_EDGE ( 'NONE', *, *, #65564, .T. ) ;
#51016 = ORIENTED_EDGE ( 'NONE', *, *, #52410, .F. ) ;
#51017 = SHAPE_REPRESENTATION_RELATIONSHIP ( 'NONE' , 'NONE' ,  #30050, #42688 ) ;
#51018 = AXIS2_PLACEMENT_3D ( 'NONE', #27106, #5429, #52983 ) ;
#51019 = DIRECTION ( 'NONE',  ( 0.000000000000000000, -0.4739929102870218958, 0.8805286599524397850 ) ) ;
#51020 = CARTESIAN_POINT ( 'NONE',  ( 18.16776742079087725, 2.623333169980955670, 13.64647547701603614 ) ) ;
#51021 = CARTESIAN_POINT ( 'NONE',  ( 24.45387357698500352, -3.540473908871999864, 12.31800308314999981 ) ) ;
#51022 = ADVANCED_FACE ( 'NONE', ( #3384 ), #8977, .T. ) ;
#51023 = CARTESIAN_POINT ( 'NONE',  ( 6.999999085428000534, -11.95749330617000084, 3.642574904853999929 ) ) ;
#51024 = CARTESIAN_POINT ( 'NONE',  ( 17.91037351677406875, 3.107515944418832277, 12.21078942061118511 ) ) ;
#51025 = DIRECTION ( 'NONE',  ( 0.000000000000000000, -0.8660254037844288266, 0.5000000000000169864 ) ) ;
#51026 = CARTESIAN_POINT ( 'NONE',  ( 9.352253013669001191, 2.817757427878999632, 6.388459691516000127 ) ) ;
#51027 = AXIS2_PLACEMENT_3D ( 'NONE', #43497, #47365, #37896 ) ;
#51028 = CARTESIAN_POINT ( 'NONE',  ( 11.36486084871759950, -5.207010770456999893, -7.825000000000000178 ) ) ;
#51029 = ORIENTED_EDGE ( 'NONE', *, *, #50273, .F. ) ;
#51030 = CARTESIAN_POINT ( 'NONE',  ( 12.18012697958979906, -2.522451323245133548, 12.44635604318887623 ) ) ;
#51031 = CARTESIAN_POINT ( 'NONE',  ( 9.351063610504999346, -3.588011994494999968, -8.416028484082099581 ) ) ;
#51032 = CARTESIAN_POINT ( 'NONE',  ( 11.27765994926999937, 3.273804980682999854, 6.368305648407000419 ) ) ;
#51033 = CARTESIAN_POINT ( 'NONE',  ( 11.42968717260509948, -4.687649763627899979, 6.377637058250999580 ) ) ;
#51034 = VECTOR ( 'NONE', #8919, 1000.000000000000000 ) ;
#51035 = CARTESIAN_POINT ( 'NONE',  ( 11.33041235500449950, 3.057642534728299832, -6.636704692336500067 ) ) ;
#51036 = CARTESIAN_POINT ( 'NONE',  ( 12.29127437512780396, 0.3560396104572040588, 12.69328656575055980 ) ) ;
#51037 = CARTESIAN_POINT ( 'NONE',  ( 7.352704719590999360, 4.773081973066999772, 8.927402469597002010 ) ) ;
#51038 = CARTESIAN_POINT ( 'NONE',  ( 9.352253013669001191, 2.817757427878999632, 6.388459691516000127 ) ) ;
#51039 = AXIS2_PLACEMENT_3D ( 'NONE', #13943, #62842, #63181 ) ;
#51040 = CARTESIAN_POINT ( 'NONE',  ( 12.27169925567829623, 2.173540117687664086, 12.52166307684904112 ) ) ;
#51041 = EDGE_LOOP ( 'NONE', ( #1042, #57087, #44505, #3617 ) ) ;
#51042 = CARTESIAN_POINT ( 'NONE',  ( 9.942214158770999788, 3.986577607995999806, -9.280166295424001177 ) ) ;
#51043 = CARTESIAN_POINT ( 'NONE',  ( 10.96118313518939935, 3.207251432249800249, -8.502430091786999711 ) ) ;
#51044 = CARTESIAN_POINT ( 'NONE',  ( 5.366518311043334322, 1.085476820253131081, 1.060886400888860326 ) ) ;
#51046 = DIRECTION ( 'NONE',  ( 0.8480635683784329970, -0.3746919961710145075, 0.3746919961710145075 ) ) ;
#51045 = CARTESIAN_POINT ( 'NONE',  ( 8.946004440379999423, -5.458705123429999695, 7.456451825584000659 ) ) ;
#51047 = CARTESIAN_POINT ( 'NONE',  ( 9.982684229509999341, -4.708027397558999461, 8.212418068717900255 ) ) ;
#51048 = CARTESIAN_POINT ( 'NONE',  ( 11.24025954179439957, -3.228187097503200320, -8.141292208271599051 ) ) ;
#51049 = ORIENTED_EDGE ( 'NONE', *, *, #20204, .T. ) ;
#51050 = CARTESIAN_POINT ( 'NONE',  ( 1.729838003972999916, -3.006852806188000216, -1.965371480138999871 ) ) ;
#51051 = CARTESIAN_POINT ( 'NONE',  ( 18.14735902876271467, -0.1997594609313395053, -12.69789023917851090 ) ) ;
#51052 = CARTESIAN_POINT ( 'NONE',  ( 25.26998262954836250, 11.52971071118044577, 2.996572855046998995 ) ) ;
#51053 = CARTESIAN_POINT ( 'NONE',  ( 18.40015514469800095, 2.597921877622999464E-14, 2.051692149506999743E-13 ) ) ;
#51054 = ADVANCED_FACE ( 'NONE', ( #51963 ), #43287, .T. ) ;
#51055 = EDGE_CURVE ( 'NONE', #42427, #29053, #12752, .T. ) ;
#51056 = DIRECTION ( 'NONE',  ( 0.000000000000000000, 1.000000000000000000, 0.000000000000000000 ) ) ;
#51057 = CARTESIAN_POINT ( 'NONE',  ( 16.07905395910120916, 8.470000438687089073, 7.998963526368290111 ) ) ;
#51058 = CARTESIAN_POINT ( 'NONE',  ( 8.216851002544000693, -2.832432432432000269, 6.822293592207000934 ) ) ;
#51059 = FACE_OUTER_BOUND ( 'NONE', #21496, .T. ) ;
#51060 = CARTESIAN_POINT ( 'NONE',  ( 8.502043146794999728, -3.869396851328000153, 5.695656592546999519 ) ) ;
#51061 = ORIENTED_EDGE ( 'NONE', *, *, #24106, .T. ) ;
#51062 = EDGE_CURVE ( 'NONE', #37575, #48333, #56668, .T. ) ;
#51063 = CARTESIAN_POINT ( 'NONE',  ( 7.635857780409000206, 2.466388272391000225, 6.935562100014999842 ) ) ;
#51064 = LINE ( 'NONE', #46164, #47424 ) ;
#51065 = CARTESIAN_POINT ( 'NONE',  ( 7.410149690637857667, -2.473805498145990711, 8.336998697800455105 ) ) ;
#51066 = CARTESIAN_POINT ( 'NONE',  ( 11.54684497800060150, 3.023157657667436826, -7.824998645711865208 ) ) ;
#51067 = CARTESIAN_POINT ( 'NONE',  ( 1.795703038681999875, -2.202566789350000054, 2.837701071685999832 ) ) ;
#51068 = VERTEX_POINT ( 'NONE', #3043 ) ;
#51069 = CARTESIAN_POINT ( 'NONE',  ( 1.334048900806262150, 2.473082949858750101, 2.189141735302758462 ) ) ;
#51070 = CARTESIAN_POINT ( 'NONE',  ( 9.411640687504601033, 2.873222873814825995, -6.752018918871659281 ) ) ;
#51071 = CARTESIAN_POINT ( 'NONE',  ( 10.86578724599310775, -5.674343923958758751, -8.061244989951715567 ) ) ;
#51072 = CARTESIAN_POINT ( 'NONE',  ( 10.64872393945999995, 2.614781729644000130, 6.717281948314999696 ) ) ;
#51073 = MECHANICAL_DESIGN_GEOMETRIC_PRESENTATION_REPRESENTATION (  '', ( #4139 ), #10837 ) ;
#51074 = CARTESIAN_POINT ( 'NONE',  ( 11.73256516821459883, 4.706297556651700020, 6.787191910456499500 ) ) ;
#51075 = CARTESIAN_POINT ( 'NONE',  ( 10.42499241036559532, -5.349775919985432004, 7.500001834605715345 ) ) ;
#51076 = CARTESIAN_POINT ( 'NONE',  ( 10.31152944037999930, -2.716820959546999870, -7.950167805575999225 ) ) ;
#51077 = CONICAL_SURFACE ( 'NONE', #34316, 10.65000781019999998, 0.7853981633972997312 ) ;
#51078 = CARTESIAN_POINT ( 'NONE',  ( 17.93599053679682243, 0.4959091552601219144, -13.88809952003718173 ) ) ;
#51079 = CARTESIAN_POINT ( 'NONE',  ( 10.35685100253999913, 2.832432432432000269, -6.822293592207000934 ) ) ;
#51080 = CARTESIAN_POINT ( 'NONE',  ( 12.72076653475835428, -3.120601141703879922, 12.28508997180244755 ) ) ;
#51081 = CARTESIAN_POINT ( 'NONE',  ( 7.553107481192300909, 3.493056710060427061, 5.802405665999490481 ) ) ;
#51082 = ORIENTED_EDGE ( 'NONE', *, *, #19050, .F. ) ;
#51083 = VECTOR ( 'NONE', #38478, 1000.000000000000000 ) ;
#51084 = CARTESIAN_POINT ( 'NONE',  ( 18.03491643637242348, -3.065379368238255964, 13.66028979695642853 ) ) ;
#51085 = DIRECTION ( 'NONE',  ( 0.000000000000000000, 0.8514543052404082157, -0.5244287998266055073 ) ) ;
#51086 = VERTEX_POINT ( 'NONE', #51625 ) ;
#51087 = CARTESIAN_POINT ( 'NONE',  ( 8.962844625895410644, -5.333198074240036668, 7.284253336463978989 ) ) ;
#51088 = CARTESIAN_POINT ( 'NONE',  ( 10.61257802013489737, 3.108115747127599970, 7.520762592984879369 ) ) ;
#51089 = CARTESIAN_POINT ( 'NONE',  ( 5.340524985724223406, -1.123086320356926793, -0.1487314272998045972 ) ) ;
#51090 = CARTESIAN_POINT ( 'NONE',  ( 23.56695564235076290, 13.34701990426062501, -4.193234373864223485 ) ) ;
#51091 = CARTESIAN_POINT ( 'NONE',  ( 9.124700695083998170, 4.778663323155000420, 8.799742559280000265 ) ) ;
#51092 = CARTESIAN_POINT ( 'NONE',  ( 9.976690600124999975, 4.172224310749999887, -6.147156451669999910 ) ) ;
#51093 = CARTESIAN_POINT ( 'NONE',  ( 9.201570984676626708, -4.444002162597382011, -8.253919324947762703 ) ) ;
#51094 = CARTESIAN_POINT ( 'NONE',  ( 10.01532628870999986, -4.946995631616999844, 8.559221361189001342 ) ) ;
#51095 = CARTESIAN_POINT ( 'NONE',  ( 18.17115522622104606, -0.3798658283128687474, -12.59428767283705319 ) ) ;
#51096 = CIRCLE ( 'NONE', #828, 11.50000000000000178 ) ;
#51097 = CARTESIAN_POINT ( 'NONE',  ( 25.59997327719300131, 11.07537871057999901, 3.096068926251000164 ) ) ;
#51098 = CARTESIAN_POINT ( 'NONE',  ( 10.89979975933730039, -3.180925410802600162, -7.218192605361100078 ) ) ;
#51099 = CARTESIAN_POINT ( 'NONE',  ( 6.932475402859345159, 1.100779672715244351, 1.004415898055839973 ) ) ;
#51100 = VERTEX_POINT ( 'NONE', #56533 ) ;
#51101 = CARTESIAN_POINT ( 'NONE',  ( 11.07128162083999889, -5.551565104116000349, -5.077697045197999692 ) ) ;
#51102 = FILL_AREA_STYLE ('',( #60902 ) ) ;
#51103 = CARTESIAN_POINT ( 'NONE',  ( 24.71428570498787280, 8.651876458988047247, 8.603903068042686897 ) ) ;
#51104 = ADVANCED_FACE ( 'NONE', ( #41147 ), #19817, .F. ) ;
#51105 = CARTESIAN_POINT ( 'NONE',  ( 10.90000000000000036, -4.000000000000000000, 7.500000000000000000 ) ) ;
#51106 = CARTESIAN_POINT ( 'NONE',  ( 9.253772138682000659, 3.523984281974800403, -6.312652778810999621 ) ) ;
#51107 = CARTESIAN_POINT ( 'NONE',  ( 12.17639632831536467, 2.882401473261805069, 13.70008095139100135 ) ) ;
#51108 = CARTESIAN_POINT ( 'NONE',  ( 10.59303089732000025, -2.436232726560000117, 7.793465286118999913 ) ) ;
#51109 = VERTEX_POINT ( 'NONE', #41484 ) ;
#51110 = CARTESIAN_POINT ( 'NONE',  ( 12.28050398187715153, -0.3399395272364318932, -12.69387965975802146 ) ) ;
#51111 = CARTESIAN_POINT ( 'NONE',  ( 11.09999999999999964, 2.649999999999999911, -7.500000000000000000 ) ) ;
#51112 = VERTEX_POINT ( 'NONE', #9312 ) ;
#51113 = DIRECTION ( 'NONE',  ( 1.000000000000000000, 0.000000000000000000, 0.000000000000000000 ) ) ;
#51114 = CARTESIAN_POINT ( 'NONE',  ( 24.44496482743900145, 12.03536723905999928, -3.224852005146999989 ) ) ;
#51115 = CARTESIAN_POINT ( 'NONE',  ( 15.57784398236293022, 9.457709274034840519, 8.211421075710344297 ) ) ;
#51116 = DIRECTION ( 'NONE',  ( 0.000000000000000000, -0.8648648648648720183, 0.5020047465136825426 ) ) ;
#51117 = COLOUR_RGB ( '', 0.09019608, 0.27058824, 0.51372549) ;
#51118 = AXIS2_PLACEMENT_3D ( 'NONE', #2720, #65306, #50619 ) ;
#51119 = CARTESIAN_POINT ( 'NONE',  ( 7.307500000000000107, 0.2500000000000000000, 3.149999999999999911 ) ) ;
#51120 = CARTESIAN_POINT ( 'NONE',  ( 10.89393020684959978, -5.250000000000000000, -7.500000000000000000 ) ) ;
#51121 = B_SPLINE_CURVE_WITH_KNOTS ( 'NONE', 1,
 ( #27786, #11005 ),
 .UNSPECIFIED., .F., .F.,
 ( 2, 2 ),
 ( 0.000000000000000000, 1.000000000000000000 ),
 .UNSPECIFIED. ) ;
#51122 = CARTESIAN_POINT ( 'NONE',  ( 8.091573680993445095, 3.319738643651897636, 8.680038712423343128 ) ) ;
#51123 = CIRCLE ( 'NONE', #8707, 11.84999999999999964 ) ;
#51124 = CARTESIAN_POINT ( 'NONE',  ( 12.75685601902876343, 3.198499228556002105, 12.18727240180921179 ) ) ;
#51125 = CARTESIAN_POINT ( 'NONE',  ( 9.262725409949998934, -4.818302824158000597, -8.808202952968999355 ) ) ;
#51126 = CARTESIAN_POINT ( 'NONE',  ( 10.53057053952199951, 3.659587858614300249, -6.703496287302799672 ) ) ;
#51127 = CARTESIAN_POINT ( 'NONE',  ( 8.500392882431995645, 2.902640497153002652, -6.605631719337000440 ) ) ;
#51128 = CARTESIAN_POINT ( 'NONE',  ( 10.98632665877000036, 3.015084670878999784, -9.064442106213000727 ) ) ;
#51129 = CARTESIAN_POINT ( 'NONE',  ( 9.202051052051999136, 5.120555153167999585, -7.719295683256799379 ) ) ;
#51131 = CARTESIAN_POINT ( 'NONE',  ( 12.09999999999999964, -4.000000000000000000, 7.500000000000000000 ) ) ;
#51130 = CARTESIAN_POINT ( 'NONE',  ( 15.86087891924500148, -8.502609378008999741, -8.308114605954999732 ) ) ;
#51132 = CARTESIAN_POINT ( 'NONE',  ( 8.200000304434999165, -12.49999969551000056, 3.568585274154000017E-10 ) ) ;
#51133 = VERTEX_POINT ( 'NONE', #62456 ) ;
#51134 = AXIS2_PLACEMENT_3D ( 'NONE', #13585, #34219, #23715 ) ;
#51135 = B_SPLINE_CURVE_WITH_KNOTS ( 'NONE', 3,
 ( #58320, #20921, #10079, #47845, #63560, #53767, #48178, #31764 ),
 .UNSPECIFIED., .F., .F.,
 ( 4, 2, 2, 4 ),
 ( 0.000000000000000000, 0.2499999999999974465, 0.4999999999999948930, 1.000000000000000000 ),
 .UNSPECIFIED. ) ;
#51136 = CARTESIAN_POINT ( 'NONE',  ( 11.23589666366019912, 3.960399224793059947, 6.608753462694600067 ) ) ;
#51137 = CARTESIAN_POINT ( 'NONE',  ( 10.34521071928999980, -2.724119865955000108, 6.497322598008000050 ) ) ;
#51138 = CARTESIAN_POINT ( 'NONE',  ( 9.857646554150999663, 4.486270025758400060, 6.621146336197599958 ) ) ;
#51139 = CARTESIAN_POINT ( 'NONE',  ( 9.051550650638001017, -2.899999999999999911, 6.227445478845999638 ) ) ;
#51140 = EDGE_CURVE ( 'NONE', #6955, #48764, #62793, .T. ) ;
#51141 = EDGE_CURVE ( 'NONE', #57880, #1963, #40447, .T. ) ;
#51142 = CARTESIAN_POINT ( 'NONE',  ( 23.89320776801300283, 11.54071136931999852, -2.936967729253997295 ) ) ;
#51143 = DIRECTION ( 'NONE',  ( 1.000000000000000000, 0.000000000000000000, 0.000000000000000000 ) ) ;
#51144 = CARTESIAN_POINT ( 'NONE',  ( 9.332537864288001472, -2.899999999999999911, 6.571291218949999902 ) ) ;
#51145 = VERTEX_POINT ( 'NONE', #67015 ) ;
#51146 = EDGE_CURVE ( 'NONE', #55873, #23381, #31004, .T. ) ;
#51147 = ADVANCED_FACE ( 'NONE', ( #50947 ), #12787, .T. ) ;
#51148 = CARTESIAN_POINT ( 'NONE',  ( 9.303367640780999537, -3.461752753411900141, -6.493012239633999982 ) ) ;
#51149 = CARTESIAN_POINT ( 'NONE',  ( 10.46536477495381590, -4.887125000223165650, -4.987012270671904446 ) ) ;
#51150 = CARTESIAN_POINT ( 'NONE',  ( 11.18546886766499959, -4.566506264294200257, 8.529286361367999447 ) ) ;
#51151 = PRODUCT_DEFINITION_SHAPE ( 'NONE', 'NONE',  #38090 ) ;
#51152 = CARTESIAN_POINT ( 'NONE',  ( 17.72222400754427696, 1.779821952440179045, -12.47366250980180702 ) ) ;
#51153 = CARTESIAN_POINT ( 'NONE',  ( 2.636390132542666631, -0.4581489286485235790, 3.499999999999998224 ) ) ;
#51154 = CARTESIAN_POINT ( 'NONE',  ( 24.63002439619599926, 0.000000000000000000, 0.000000000000000000 ) ) ;
#51155 = CARTESIAN_POINT ( 'NONE',  ( 12.24837323144403278, 2.784344744724901677, -13.60903177733648306 ) ) ;
#51156 = CARTESIAN_POINT ( 'NONE',  ( 9.790745838555999114, -4.301175052434000001, -8.935144319903001175 ) ) ;
#51157 = CARTESIAN_POINT ( 'NONE',  ( 10.11094409420000062, -5.100000000000000533, -6.571291218949999902 ) ) ;
#51158 = ORIENTED_EDGE ( 'NONE', *, *, #63288, .F. ) ;
#51159 = CARTESIAN_POINT ( 'NONE',  ( 17.92254446305189575, 3.154612309636608547, -13.64000973911191217 ) ) ;
#51160 = LINE ( 'NONE', #67221, #9635 ) ;
#51161 = CARTESIAN_POINT ( 'NONE',  ( 5.000000000000000000, 0.000000000000000000, 0.000000000000000000 ) ) ;
#51162 = CARTESIAN_POINT ( 'NONE',  ( 18.10163077481709237, -2.185641740717685799, -13.73537224937313184 ) ) ;
#51163 = B_SPLINE_CURVE_WITH_KNOTS ( 'NONE', 3,
 ( #12729, #7130, #12029, #17631, #50134, #33365, #54327, #44560, #12379, #1200, #39295, #23553, #17273, #29162, #55030, #6426, #28468, #33711, #66197, #49782, #22508 ),
 .UNSPECIFIED., .F., .F.,
 ( 4, 2, 2, 2, 1, 2, 2, 1, 1, 2, 2, 4 ),
 ( 0.000000000000000000, 0.1249999999999764355, 0.1874999999999669154, 0.2499999999999574229, 0.3124999999999479305, 0.3437499999999464873, 0.3749999999999449884, 0.4374999999999377165, 0.4687499999999341083, 0.4843749999999329425, 0.4999999999999318323, 1.000000000000000000 ),
 .UNSPECIFIED. ) ;
#51164 = CARTESIAN_POINT ( 'NONE',  ( 25.60000000000000142, -9.517611874540000017, -8.103398312166000039 ) ) ;
#51165 = EDGE_CURVE ( 'NONE', #40269, #20353, #65556, .T. ) ;
#51166 = CARTESIAN_POINT ( 'NONE',  ( 9.269689158774999882, 3.135494838036999798, -8.598037907310999373 ) ) ;
#51167 = CARTESIAN_POINT ( 'NONE',  ( 11.91672066707849886, -3.258843737379200078, 7.948314604624900248 ) ) ;
#51168 = VERTEX_POINT ( 'NONE', #27830 ) ;
#51169 = CARTESIAN_POINT ( 'NONE',  ( 4.000000000000000000, -1.878475312369306982, 1.082895748632574762 ) ) ;
#51170 = CARTESIAN_POINT ( 'NONE',  ( 18.02597764372132971, 3.073197451853422191, -13.65853278380549263 ) ) ;
#51171 = VERTEX_POINT ( 'NONE', #49135 ) ;
#51172 = CARTESIAN_POINT ( 'NONE',  ( 10.71924205624999971, -4.310927436352299580, 6.690659495528099576 ) ) ;
#51173 = CARTESIAN_POINT ( 'NONE',  ( 2.634306799210667016, 1.762666431298139713, 3.058252359239908458 ) ) ;
#51174 = CARTESIAN_POINT ( 'NONE',  ( 9.699495280410998177, 5.048004622677000341, -6.120508709481000231 ) ) ;
#51175 = CARTESIAN_POINT ( 'NONE',  ( 7.000000000000000000, 6.255435840762999966, 3.000000000000000000 ) ) ;
#51176 = CARTESIAN_POINT ( 'NONE',  ( 10.89324174884020024, -4.032306468273969990, -8.674442868902998427 ) ) ;
#51177 = FACE_OUTER_BOUND ( 'NONE', #54805, .T. ) ;
#51178 = VECTOR ( 'NONE', #63042, 1000.000000000000000 ) ;
#51179 = DIRECTION ( 'NONE',  ( 1.000000000000000000, 0.000000000000000000, 0.000000000000000000 ) ) ;
#51180 = VERTEX_POINT ( 'NONE', #65206 ) ;
#51181 = CARTESIAN_POINT ( 'NONE',  ( 7.614999999996999946, 5.349999999999999645, -7.500000000000000000 ) ) ;
#51182 = FACE_OUTER_BOUND ( 'NONE', #49634, .T. ) ;
#51183 = CARTESIAN_POINT ( 'NONE',  ( 9.079170280414000871, 4.815598936798999752, -8.835641302565999666 ) ) ;
#51184 = ORIENTED_EDGE ( 'NONE', *, *, #24388, .F. ) ;
#51185 = AXIS2_PLACEMENT_3D ( 'NONE', #5147, #251, #32081 ) ;
#51186 = CARTESIAN_POINT ( 'NONE',  ( 10.79839886931999970, 5.269366011605000288, -6.148705891248999578 ) ) ;
#51187 = VERTEX_POINT ( 'NONE', #50866 ) ;
#51188 = CARTESIAN_POINT ( 'NONE',  ( 9.911267173156000254, 3.130949526459800403, 8.240598219300300897 ) ) ;
#51189 = CARTESIAN_POINT ( 'NONE',  ( 17.87014202174174926, -1.960141137139741252, -12.56108054050352685 ) ) ;
#51190 = EDGE_CURVE ( 'NONE', #66190, #44139, #29489, .T. ) ;
#51191 = CARTESIAN_POINT ( 'NONE',  ( 8.731616107288068918, -3.999997736744774546, -8.381579007094499545 ) ) ;
#51192 = VECTOR ( 'NONE', #62183, 1000.000000000000000 ) ;
#51193 = ADVANCED_FACE ( 'NONE', ( #8899 ), #57918, .F. ) ;
#51194 = CARTESIAN_POINT ( 'NONE',  ( 24.56046482271400322, -12.50678080147000060, -2.996392338889999785 ) ) ;
#51195 = FACE_OUTER_BOUND ( 'NONE', #68454, .T. ) ;
#51196 = ORIENTED_EDGE ( 'NONE', *, *, #53955, .T. ) ;
#51197 = CARTESIAN_POINT ( 'NONE',  ( 11.59999999999999787, 3.707964997157290110, 6.463642954493290738 ) ) ;
#51198 = CARTESIAN_POINT ( 'NONE',  ( 11.33382334123000135, 2.642405149457999869, -7.577896731332000257 ) ) ;
#51199 = CARTESIAN_POINT ( 'NONE',  ( 11.04647262364999882, -5.245405433888000069, -5.117543298298000032 ) ) ;
#51200 = CARTESIAN_POINT ( 'NONE',  ( 12.33301873031881613, 1.963679441452095720, -13.86160245617593212 ) ) ;
#51201 = CARTESIAN_POINT ( 'NONE',  ( 9.684367640780997988, -3.396982508013000501, -6.371835875489000323 ) ) ;
#51202 = CARTESIAN_POINT ( 'NONE',  ( 18.18297552798360783, 0.3652063536484332906, 13.99523956222174270 ) ) ;
#51203 = CARTESIAN_POINT ( 'NONE',  ( 7.842433916446627684, 5.025786930142569275, 6.559111426468311024 ) ) ;
#51204 = ORIENTED_EDGE ( 'NONE', *, *, #13546, .F. ) ;
#51205 = VERTEX_POINT ( 'NONE', #46309 ) ;
#51206 = CARTESIAN_POINT ( 'NONE',  ( 9.476970280414001024, 5.511689883260999956, -7.095113581311000672 ) ) ;
#51207 = CARTESIAN_POINT ( 'NONE',  ( 9.243873111163818379, 5.510384933080038294, 8.414177276375912840 ) ) ;
#51208 = CARTESIAN_POINT ( 'NONE',  ( 12.22115613549653546, -2.722964197143763254, 13.62363865713189526 ) ) ;
#51209 = DIRECTION ( 'NONE',  ( -1.000000000000000000, 0.000000000000000000, 2.893429392099000104E-14 ) ) ;
#51210 = CARTESIAN_POINT ( 'NONE',  ( 24.03127491216000067, 9.408387437348000759, -9.735706541027999705 ) ) ;
#51211 = CARTESIAN_POINT ( 'NONE',  ( 18.05609597790000009, -3.343430715100999873, -11.12052764821000039 ) ) ;
#51213 = DIRECTION ( 'NONE',  ( -1.000000000000000000, 0.000000000000000000, 0.000000000000000000 ) ) ;
#51212 = CARTESIAN_POINT ( 'NONE',  ( 9.449822372493999367, -4.367693913457399546, 6.297150255604999636 ) ) ;
#51214 = LINE ( 'NONE', #62715, #57593 ) ;
#51215 = ORIENTED_EDGE ( 'NONE', *, *, #55265, .T. ) ;
#51216 = DIRECTION ( 'NONE',  ( -1.000000000000000000, 0.000000000000000000, 0.000000000000000000 ) ) ;
#51217 = CARTESIAN_POINT ( 'NONE',  ( 7.915025373318000490, 3.368995052637000054, -6.306487705577000114 ) ) ;
#51218 = CARTESIAN_POINT ( 'NONE',  ( 9.881157842586999251, -5.290169207169999943, -8.858081286661999343 ) ) ;
#51219 = CARTESIAN_POINT ( 'NONE',  ( 7.949652217634350926, 4.891777316758940231, 6.381786135468885846 ) ) ;
#51220 = AXIS2_PLACEMENT_3D ( 'NONE', #42621, #63930, #52765 ) ;
#51221 = CARTESIAN_POINT ( 'NONE',  ( 11.49977531252999974, 12.43119799159999950, 1.530013559959999991 ) ) ;
#51222 = CARTESIAN_POINT ( 'NONE',  ( 11.04678944127999962, -5.235596213805000509, -5.039805523473999571 ) ) ;
#51223 = CARTESIAN_POINT ( 'NONE',  ( 9.541460841232000334, 2.824732249080000202, -8.992748220058999209 ) ) ;
#51224 = EDGE_CURVE ( 'NONE', #8893, #66228, #51123, .T. ) ;
#51225 = EDGE_CURVE ( 'NONE', #37494, #21235, #1844, .T. ) ;
#51226 = CARTESIAN_POINT ( 'NONE',  ( 10.49349279008999858, 3.667611644732699627, 6.265968249244999733 ) ) ;
#51227 = CARTESIAN_POINT ( 'NONE',  ( 8.099999999999999645, 0.000000000000000000, 11.84999999999999964 ) ) ;
#51228 = CARTESIAN_POINT ( 'NONE',  ( 11.09999999999999964, 2.649999999999999911, 7.500000000000000000 ) ) ;
#51229 = CARTESIAN_POINT ( 'NONE',  ( 3.300975217870999678, 3.258359658149000193, 0.06617378549577000724 ) ) ;
#51230 = VERTEX_POINT ( 'NONE', #57817 ) ;
#51231 = CARTESIAN_POINT ( 'NONE',  ( 12.47306973639847349, 0.6395598188657407590, -12.58375915074078577 ) ) ;
#51232 = DIRECTION ( 'NONE',  ( 0.000000000000000000, -0.9916377111174247139, 0.1290528957048031888 ) ) ;
#51233 = CARTESIAN_POINT ( 'NONE',  ( 16.09997386696500143, 6.963621661623434989, 9.386500412226205015 ) ) ;
#51234 = CYLINDRICAL_SURFACE ( 'NONE', #8873, 1.250000000000000222 ) ;
#51235 = CARTESIAN_POINT ( 'NONE',  ( 17.92913687483821406, -3.216295279492294767, -11.40344415251901289 ) ) ;
#51236 = EDGE_LOOP ( 'NONE', ( #36666, #20732, #20372, #4312 ) ) ;
#51237 = CARTESIAN_POINT ( 'NONE',  ( 5.550217628333999897, -0.9612325616298000863, -1.110208802542000051 ) ) ;
#51238 = PRODUCT_CONTEXT ( 'NONE', #21734, 'mechanical' ) ;
#51239 = DIRECTION ( 'NONE',  ( 4.129963865151999738E-10, 4.129962357295999768E-10, -1.000000000000000000 ) ) ;
#51240 = ADVANCED_FACE ( 'NONE', ( #10610 ), #47339, .T. ) ;
#51241 = B_SPLINE_CURVE_WITH_KNOTS ( 'NONE', 3,
 ( #34295, #2468, #8747, #23793, #66090, #28707, #30092, #44788, #45127, #3492, #66435, #44448, #18557, #39185, #61203, #29405, #65745, #60509, #12616, #33947, #13658, #55269, #50713, #50024, #2131, #23451, #18209, #2809, #24137, #4175, #36696, #58017, #68838, #9418, #51734, #56982, #15021, #25853, #52769, #47184, #15368, #41591, #25513, #10119, #20956, #20263, #46155, #10455, #31450, #58353, #15710 ),
 .UNSPECIFIED., .F., .F.,
 ( 4, 2, 2, 2, 2, 2, 2, 2, 2, 2, 2, 2, 2, 1, 2, 2, 2, 2, 2, 2, 2, 2, 2, 2, 2, 4 ),
 ( 0.000000000000000000, 0.06261444088629199156, 0.1252288817725839831, 0.1565361022157301107, 0.1878433226588762384, 0.2191505431020223937, 0.2348041533235934453, 0.2504577635451644690, 0.2817649839883067386, 0.2974185942098764301, 0.3130722044314461217, 0.3287258146530158687, 0.3443794248745855602, 0.3600330350961553072, 0.3678598402069396256, 0.3756866453177239440, 0.3913402555392901383, 0.3991670606500741791, 0.4069938657608581645, 0.4226474759824261351, 0.4304742810932104535, 0.4343876836486003645, 0.4383010862039902755, 0.4539546964255526396, 0.4696083066471148926, 0.5009155270902391210 ),
 .UNSPECIFIED. ) ;
#51242 = CARTESIAN_POINT ( 'NONE',  ( 9.573148997458000409, -5.167567567567999731, -6.822293592207000934 ) ) ;
#51243 = CARTESIAN_POINT ( 'NONE',  ( 1.636390132540125109, -0.4581489286485235790, 3.499999999999998224 ) ) ;
#51244 = CARTESIAN_POINT ( 'NONE',  ( 10.85679632507500081, 4.490665650747399873, -8.409605917786398877 ) ) ;
#51245 = ORIENTED_EDGE ( 'NONE', *, *, #16578, .F. ) ;
#51246 = CARTESIAN_POINT ( 'NONE',  ( 9.423521818475000700, -4.993993578306000103, 8.578110568283999982 ) ) ;
#51247 = VERTEX_POINT ( 'NONE', #48361 ) ;
#51248 = CARTESIAN_POINT ( 'NONE',  ( 9.424850088744616272, -5.349972419855331118, 7.500009359253513530 ) ) ;
#51249 = CARTESIAN_POINT ( 'NONE',  ( 8.560879440379000727, -4.228293421747000735, 8.941387937291999322 ) ) ;
#51250 = CARTESIAN_POINT ( 'NONE',  ( 18.28003411566973924, -0.02431279293012689191, -13.99999914078080110 ) ) ;
#51251 = ORIENTED_EDGE ( 'NONE', *, *, #63369, .F. ) ;
#51252 = CARTESIAN_POINT ( 'NONE',  ( 10.90512994902607602, 9.806150973310261421, -5.715962064497588813 ) ) ;
#51253 = CARTESIAN_POINT ( 'NONE',  ( 10.99570321855803456, -5.445259508076158106, -7.243346639202360215 ) ) ;
#51254 = B_SPLINE_CURVE_WITH_KNOTS ( 'NONE', 3,
 ( #43064, #64370, #16493, #10906 ),
 .UNSPECIFIED., .F., .F.,
 ( 4, 4 ),
 ( 0.000000000000000000, 1.000000000000000000 ),
 .UNSPECIFIED. ) ;
#51255 = CARTESIAN_POINT ( 'NONE',  ( -0.2999999999999999889, 0.000000000000000000, 0.000000000000000000 ) ) ;
#51256 = CARTESIAN_POINT ( 'NONE',  ( 4.400000000000000355, 0.000000000000000000, 0.000000000000000000 ) ) ;
#51257 = CARTESIAN_POINT ( 'NONE',  ( 17.63847140750532461, -3.120744938285826109, 12.28504437646398806 ) ) ;
#51258 = VERTEX_POINT ( 'NONE', #64082 ) ;
#51259 = CARTESIAN_POINT ( 'NONE',  ( 2.053056799206542049, 2.798833948393625537, 2.150913519912209360 ) ) ;
#51260 = CARTESIAN_POINT ( 'NONE',  ( 11.59999999999999609, 4.247874375640066091, 8.548800951397311110 ) ) ;
#51261 = CARTESIAN_POINT ( 'NONE',  ( 5.532109839683624131, -0.9218200799623775810, 1.199500263597266247 ) ) ;
#51262 = CARTESIAN_POINT ( 'NONE',  ( 9.643930206848999376, 5.250000000000000000, 7.500000000000000000 ) ) ;
#51263 = CARTESIAN_POINT ( 'NONE',  ( 12.43804048104135163, -3.154843637310955629, 13.63995574169148917 ) ) ;
#51264 = ORIENTED_EDGE ( 'NONE', *, *, #44335, .F. ) ;
#51265 = CARTESIAN_POINT ( 'NONE',  ( 17.91195221639529933, 0.5131987758830273139, -13.88724801698936062 ) ) ;
#51266 = CARTESIAN_POINT ( 'NONE',  ( 10.95823604978370547, -2.826496578562578854, -6.686434942404212656 ) ) ;
#51267 = CARTESIAN_POINT ( 'NONE',  ( 23.91319693356835430, -3.340393349183891747, -12.90999628518435038 ) ) ;
#51268 = CARTESIAN_POINT ( 'NONE',  ( 10.90987533632539730, 5.099994864246352400, -5.097495378088114926 ) ) ;
#51269 = AXIS2_PLACEMENT_3D ( 'NONE', #53024, #32054, #48468 ) ;
#51270 = ADVANCED_FACE ( 'NONE', ( #37875 ), #52573, .T. ) ;
#51271 = CARTESIAN_POINT ( 'NONE',  ( 12.19601928331639051, -0.1418539764880159537, -13.89904537328360945 ) ) ;
#51272 = CARTESIAN_POINT ( 'NONE',  ( 18.16486442019682102, -2.361571392960267968, 12.48278654574965607 ) ) ;
#51273 = ORIENTED_EDGE ( 'NONE', *, *, #32739, .T. ) ;
#51274 = CARTESIAN_POINT ( 'NONE',  ( 10.85679632507500081, -3.509334349252600127, -8.409605917786398877 ) ) ;
#51275 = ORIENTED_EDGE ( 'NONE', *, *, #65253, .T. ) ;
#51276 = CARTESIAN_POINT ( 'NONE',  ( 10.64872393945999995, 2.614781729644000130, 6.717281948314999696 ) ) ;
#51277 = CARTESIAN_POINT ( 'NONE',  ( 12.80505043854144276, -0.6250000000000001110, -12.67928921589118652 ) ) ;
#51278 = CARTESIAN_POINT ( 'NONE',  ( 9.725595280412999699, 2.495531372253999791, -7.930944806125000746 ) ) ;
#51279 = CARTESIAN_POINT ( 'NONE',  ( 3.271177333949000232, -3.705085452251000167, 0.1482300145088999987 ) ) ;
#51280 = CARTESIAN_POINT ( 'NONE',  ( 10.75911128370000114, -4.477561100530000004, -5.708582007447000173 ) ) ;
#51281 = CARTESIAN_POINT ( 'NONE',  ( 10.31021345716899873, 4.636538040886300394, -8.078719053813800954 ) ) ;
#51282 = CARTESIAN_POINT ( 'NONE',  ( 25.30000327618300204, -10.36736154742122018, 5.168041346173460227 ) ) ;
#51283 = EDGE_LOOP ( 'NONE', ( #33017, #46080, #48117 ) ) ;
#51284 = CARTESIAN_POINT ( 'NONE',  ( 10.94841638348500013, -5.108333310975999630, 7.769976643522699788 ) ) ;
#51285 = CARTESIAN_POINT ( 'NONE',  ( 10.71756692516999898, 3.040224182812999665, 8.808452309630000698 ) ) ;
#51286 = CARTESIAN_POINT ( 'NONE',  ( 15.39403162610500075, 9.133592062008998980, 8.216350050208999889 ) ) ;
#51287 = CARTESIAN_POINT ( 'NONE',  ( 18.29991931957795259, -1.031823913341759950E-13, -12.32514597914127563 ) ) ;
#51289 = CARTESIAN_POINT ( 'NONE',  ( 12.80505043854144276, -5.963111948670274387E-16, -25.00000000000000000 ) ) ;
#51288 = CARTESIAN_POINT ( 'NONE',  ( 11.15982925107999968, 5.578232410510000072, 8.067793621926998782 ) ) ;
#51290 = CARTESIAN_POINT ( 'NONE',  ( 10.89564560330029863, 4.307504762655200103, -6.544808043482999160 ) ) ;
#51291 = CARTESIAN_POINT ( 'NONE',  ( 25.46375152665800101, -2.879425814940999917, -11.30951176145000048 ) ) ;
#51292 = B_SPLINE_CURVE_WITH_KNOTS ( 'NONE', 3,
 ( #29177, #40007, #35445, #2586 ),
 .UNSPECIFIED., .F., .F.,
 ( 4, 4 ),
 ( 0.000000000000000000, 1.000000000000000000 ),
 .UNSPECIFIED. ) ;
#51293 = CARTESIAN_POINT ( 'NONE',  ( 9.148430433047000321, 3.145249924879699677, -6.972511033848699746 ) ) ;
#51294 = CARTESIAN_POINT ( 'NONE',  ( 18.15103067362389311, -0.4097539338085443017, 12.59333942654355631 ) ) ;
#51295 = CARTESIAN_POINT ( 'NONE',  ( 24.62773497368900166, 3.462213745051000213, 12.08749688049000071 ) ) ;
#51296 = CARTESIAN_POINT ( 'NONE',  ( 8.736413463905998711, 4.084156314540369870, 6.617590440947399344 ) ) ;
#51297 = DIRECTION ( 'NONE',  ( 0.000000000000000000, 1.000000000000000000, 0.000000000000000000 ) ) ;
#51298 = VERTEX_POINT ( 'NONE', #5707 ) ;
#51299 = CARTESIAN_POINT ( 'NONE',  ( 7.833769353207999941, -2.583664704444999849, 6.684748541034000624 ) ) ;
#51300 = EDGE_CURVE ( 'NONE', #36930, #59297, #22632, .T. ) ;
#51301 = ADVANCED_FACE ( 'NONE', ( #64423 ), #47319, .F. ) ;
#51302 = CARTESIAN_POINT ( 'NONE',  ( 4.000000000000000000, 1.321078631445433471, -1.719326598155805685 ) ) ;
#51303 = DIRECTION ( 'NONE',  ( 1.000000000000000000, 0.000000000000000000, 0.000000000000000000 ) ) ;
#51304 = CARTESIAN_POINT ( 'NONE',  ( 10.09964828895399869, -2.878385131502000149, -8.112615456209400833 ) ) ;
#51305 = ORIENTED_EDGE ( 'NONE', *, *, #45145, .T. ) ;
#51306 = CARTESIAN_POINT ( 'NONE',  ( 8.641801658773999861, 2.933833973450999721, 8.496479443567000800 ) ) ;
#51308 = CARTESIAN_POINT ( 'NONE',  ( 11.18923293495519822, 2.967327562101000016, 7.541513160549049744 ) ) ;
#51307 = CARTESIAN_POINT ( 'NONE',  ( 8.724822372493999723, -4.249211653873900651, -8.315254653915399530 ) ) ;
#51309 = CARTESIAN_POINT ( 'NONE',  ( 11.07691721959000120, 3.101894630379999906, -8.926552937604000704 ) ) ;
#51310 = EDGE_LOOP ( 'NONE', ( #67031, #18780, #25705, #11067, #35948, #8834, #39239 ) ) ;
#51311 = B_SPLINE_CURVE_WITH_KNOTS ( 'NONE', 3,
 ( #42616, #36686, #54393, #37030, #41581, #57651, #22574, #58009, #10445, #31107, #10791, #33427, #16035, #33079, #31441, #37365 ),
 .UNSPECIFIED., .F., .F.,
 ( 4, 2, 2, 2, 2, 2, 2, 4 ),
 ( 0.1254285313929423273, 0.2190720462666236046, 0.3127155611403048541, 0.4063590760139861313, 0.5000025908876674086, 0.6872896206350299630, 0.7809331355087112403, 0.8745766503823925175 ),
 .UNSPECIFIED. ) ;
#51312 = B_SPLINE_CURVE_WITH_KNOTS ( 'NONE', 3,
 ( #4251, #15782, #47947, #36769, #37112, #58426, #25589, #63316, #31871, #21367 ),
 .UNSPECIFIED., .F., .F.,
 ( 4, 2, 2, 2, 4 ),
 ( 0.5015528379108959989, 0.6261646284331719992, 0.7507764189554479994, 0.8753882094777239997, 1.000000000000000000 ),
 .UNSPECIFIED. ) ;
#51313 = DIRECTION ( 'NONE',  ( 0.7070979648104197546, 0.000000000000000000, -0.7071155974527518762 ) ) ;
#51314 = CARTESIAN_POINT ( 'NONE',  ( 17.77834352330038215, -3.212755074437998015, -13.62637949436378015 ) ) ;
#51315 = CARTESIAN_POINT ( 'NONE',  ( 10.91610672858429965, 3.088399709291500095, 8.185766014210599906 ) ) ;
#51316 = CARTESIAN_POINT ( 'NONE',  ( 17.10000000000000142, -3.470217030164000072, -11.92928724693999953 ) ) ;
#51317 = CARTESIAN_POINT ( 'NONE',  ( 11.09999999999999964, -5.299999999999999822, -5.157071272631999825 ) ) ;
#51318 = EDGE_LOOP ( 'NONE', ( #57231, #51949, #54331, #9603 ) ) ;
#51319 = FACE_OUTER_BOUND ( 'NONE', #1240, .T. ) ;
#51320 = CARTESIAN_POINT ( 'NONE',  ( 11.35905860703999970, -2.719090443614000208, -7.157642341559000698 ) ) ;
#51321 = EDGE_CURVE ( 'NONE', #56658, #1963, #25989, .T. ) ;
#51322 = CARTESIAN_POINT ( 'NONE',  ( 8.233317044961992792, -5.585056236752896197, 8.216725689016870504 ) ) ;
#51323 = CARTESIAN_POINT ( 'NONE',  ( 10.85168717260509830, -4.613789146762799831, -8.501809683958001074 ) ) ;
#51324 = CARTESIAN_POINT ( 'NONE',  ( 10.43458376188599956, -5.078750111091999919, 6.812480849273599759 ) ) ;
#51325 = ORIENTED_EDGE ( 'NONE', *, *, #14154, .F. ) ;
#51326 = FACE_OUTER_BOUND ( 'NONE', #8538, .T. ) ;
#51327 = CARTESIAN_POINT ( 'NONE',  ( 10.57503300763299947, -3.118110956362800223, 6.575021251017499679 ) ) ;
#51328 = ORIENTED_EDGE ( 'NONE', *, *, #17671, .T. ) ;
#51329 = ADVANCED_FACE ( 'NONE', ( #39958 ), #16473, .T. ) ;
#51330 = CARTESIAN_POINT ( 'NONE',  ( 9.022188178962252891, 3.408865106546500989, 6.476088678109181984 ) ) ;
#51331 = VERTEX_POINT ( 'NONE', #56375 ) ;
#51332 = CARTESIAN_POINT ( 'NONE',  ( 9.235799540957000175, -4.950980172046000050, -5.959730545597000884 ) ) ;
#51333 = DIRECTION ( 'NONE',  ( 0.000000000000000000, 1.000000000000000000, 0.000000000000000000 ) ) ;
#51334 = CARTESIAN_POINT ( 'NONE',  ( 11.42834208742529967, 3.293478249981899975, -8.610579932818998472 ) ) ;
#51335 = CARTESIAN_POINT ( 'NONE',  ( 8.320275434042544660, 5.099114858442474585, 6.576956779799525421 ) ) ;
#51336 = CARTESIAN_POINT ( 'NONE',  ( 12.24230779986659101, 2.227307356672650673, -12.51097363402014118 ) ) ;
#51337 = CARTESIAN_POINT ( 'NONE',  ( 11.21918447801630059, -2.859536135895000442, 7.525145395936648995 ) ) ;
#51338 = CARTESIAN_POINT ( 'NONE',  ( 7.308885841229000313, 4.847807297114000491, 9.065373753110998578 ) ) ;
#51339 = ORIENTED_EDGE ( 'NONE', *, *, #10561, .F. ) ;
#51340 = CARTESIAN_POINT ( 'NONE',  ( 9.604346873516666605, 5.250000000000001776, 7.663624617374461323 ) ) ;
#51341 = B_SPLINE_CURVE_WITH_KNOTS ( 'NONE', 3,
 ( #52425, #36350, #4522, #42299 ),
 .UNSPECIFIED., .F., .F.,
 ( 4, 4 ),
 ( 0.000000000000000000, 1.000000000000000000 ),
 .UNSPECIFIED. ) ;
#51342 = CARTESIAN_POINT ( 'NONE',  ( 8.470293146793999028, -4.255646685191999623, 9.114089645792999406 ) ) ;
#51343 = CARTESIAN_POINT ( 'NONE',  ( 7.000000000000000000, 0.6646153846154000400, 2.616923076922999858 ) ) ;
#51344 = ORIENTED_EDGE ( 'NONE', *, *, #40108, .F. ) ;
#51345 = B_SPLINE_SURFACE_WITH_KNOTS ( 'NONE', 3, 3, ( 
 ( #11496, #27943, #60096, #38419, #59744, #12895, #34224, #49253, #1362, #55543, #677, #22680, #44024, #21988, #16742, #67386, #46078, #50297, #19508, #24065, #8674, #66362, #13927, #9010, #24753, #56226, #15553, #61131, #23719, #40156, #2739, #40826, #62151, #14269, #35597 ),
 ( #56911, #45055, #3079, #7641, #2395, #29679, #24412, #35254, #4698, #26044, #56570, #42124, #30021, #29326, #30351, #63432, #68676, #45740, #47371, #52605, #13248, #18483, #28989, #51323, #67050, #50639, #20794, #19159, #61472, #40483, #36881, #3418, #39809, #34573, #13591 ),
 ( #55889, #45400, #7993, #66709, #61810, #18830, #34911, #8335, #50982, #69028, #32666, #15886, #27418, #17269, #22163, #500, #53977, #49084, #65148, #38243, #48394, #155, #10641, #37217, #63775, #33008, #42808, #58534, #21141, #58197, #16230, #48054, #16576, #48743, #53298 ),
 ( #31985, #42466, #37554, #21816, #5401, #21473, #6081, #59223, #26737, #58885, #27774, #43149, #64115, #10989, #64454, #32329, #846, #43503, #31634, #64801, #53640, #11325, #47716, #37901, #59570, #16912, #5736, #10299, #27077, #5052, #11668, #54323, #6422, #1195, #22504 ) ),
 .UNSPECIFIED., .F., .F., .F.,
 ( 4, 4 ),
 ( 4, 1, 1, 1, 1, 1, 1, 1, 1, 1, 1, 1, 1, 1, 1, 1, 1, 1, 1, 1, 1, 1, 1, 1, 1, 1, 1, 1, 1, 1, 1, 1, 4 ),
 ( -0.02000000000000000042, 1.020000000000000018 ),
 ( 0.1633025096610999927, 0.1899619885200000136, 0.2166214673788000034, 0.2432809462376999965, 0.2699404250964999585, 0.2965999039553000038, 0.3232593828141999692, 0.3499188616730000145, 0.3765783405318000043, 0.4032378193906999697, 0.4298972982494999595, 0.4565567771083000048, 0.4832162559671999702, 0.5098757348260000155, 0.5365352136848999809, 0.5631946925437000262, 0.5898541714025000715, 0.6165136502614000369, 0.6431731291201999712, 0.6698326079790000165, 0.6964920868378999819, 0.7231515656967000272, 0.7498110445554999615, 0.7764705234143999268, 0.8031300022731999722, 0.8297894811320000175, 0.8564489599908999828, 0.8831084388497000282, 0.9097679177085999935, 0.9364273965674000388, 0.9630868754261999731, 0.9897463542851000495, 1.016405833144000015 ),
 .UNSPECIFIED. ) ;
#51346 = CARTESIAN_POINT ( 'NONE',  ( 12.12451730110975134, -2.231694252990107152, -12.40079297172317929 ) ) ;
#51347 = CARTESIAN_POINT ( 'NONE',  ( 11.20733594839949809, 4.840266102192999575, 8.462948211532999920 ) ) ;
#51348 = CARTESIAN_POINT ( 'NONE',  ( 10.90246814679000131, -4.554787328265999413, -6.081873034041000103 ) ) ;
#51349 = CARTESIAN_POINT ( 'NONE',  ( 7.000000000000000000, 7.526486366024999874, 3.526486366024999874 ) ) ;
#51350 = CARTESIAN_POINT ( 'NONE',  ( 18.44495723965300016, -2.860707309908000262, -12.13834028902000028 ) ) ;
#51351 = CARTESIAN_POINT ( 'NONE',  ( 9.303275160948496492, 2.900329483618105719, -6.884602962369688051 ) ) ;
#51352 = CARTESIAN_POINT ( 'NONE',  ( 12.25689739436622716, -2.199570998105317088, -13.73255685804838500 ) ) ;
#51353 = FACE_OUTER_BOUND ( 'NONE', #56412, .T. ) ;
#51354 = CARTESIAN_POINT ( 'NONE',  ( 10.73964560330029983, -3.608363763633400279, -6.283473206644000442 ) ) ;
#51355 = DIRECTION ( 'NONE',  ( 0.000000000000000000, 1.000000000000000000, 0.000000000000000000 ) ) ;
#51356 = EDGE_LOOP ( 'NONE', ( #65680, #38709, #58159, #19983 ) ) ;
#51357 = ORIENTED_EDGE ( 'NONE', *, *, #43836, .F. ) ;
#51358 = CARTESIAN_POINT ( 'NONE',  ( 10.33235660140000078, -4.841932061664000031, 4.868350078553000060 ) ) ;
#51359 = DIRECTION ( 'NONE',  ( -1.000000000000000000, 0.000000000000000000, 0.000000000000000000 ) ) ;
#51360 = CARTESIAN_POINT ( 'NONE',  ( 17.59614113505323729, 3.124999999999999556, 13.52078631348661908 ) ) ;
#51361 = CARTESIAN_POINT ( 'NONE',  ( 10.73506130198999919, 5.202496273738000276, -8.441412224440000500 ) ) ;
#51362 = CARTESIAN_POINT ( 'NONE',  ( 8.668193840844024223, 5.051241208858799681, 6.199741807410033445 ) ) ;
#51363 = CARTESIAN_POINT ( 'NONE',  ( 18.15128053492057703, 2.312280642761794347, 12.49331763295500508 ) ) ;
#51364 = PLANE ( 'NONE',  #41752 ) ;
#51365 = ADVANCED_FACE ( 'NONE', ( #50436 ), #21090, .T. ) ;
#51366 = CARTESIAN_POINT ( 'NONE',  ( 9.476372460169001144, 5.098395626600999542, 6.305536056092000408 ) ) ;
#51367 = CARTESIAN_POINT ( 'NONE',  ( 9.321633776942626071, -3.275060658047592277, 7.010106850326409678 ) ) ;
#51368 = VERTEX_POINT ( 'NONE', #7967 ) ;
#51369 = CARTESIAN_POINT ( 'NONE',  ( 12.18465059688365848, -2.421662038956231999, 12.46951891513069732 ) ) ;
#51370 = CARTESIAN_POINT ( 'NONE',  ( 9.452380199233999747, -3.003429752324399793, -7.374740103075099640 ) ) ;
#51371 = CARTESIAN_POINT ( 'NONE',  ( 10.48165121391000021, 4.022873529486999722, 9.090897232145000117 ) ) ;
#51372 = CARTESIAN_POINT ( 'NONE',  ( 11.01925056272500036, -2.825232917634000085, 7.482589369563879877 ) ) ;
#51373 = CARTESIAN_POINT ( 'NONE',  ( 8.581920280410001212, 4.769017407621999993, -8.862909124839001507 ) ) ;
#51374 = CARTESIAN_POINT ( 'NONE',  ( 10.59195391537400077, 5.057233422790000432, -8.218034727798299244 ) ) ;
#51375 = CARTESIAN_POINT ( 'NONE',  ( 12.44117949531284317, 0.5082598251325830541, 12.68630931495243352 ) ) ;
#51376 = CARTESIAN_POINT ( 'NONE',  ( 7.903989158771000056, 2.095715612964000218, 8.056490963156001328 ) ) ;
#51377 = CARTESIAN_POINT ( 'NONE',  ( 9.848730799670999403, 2.769737997918999994, 6.441853401936000090 ) ) ;
#51378 = CARTESIAN_POINT ( 'NONE',  ( 12.29407742813162940, 2.139519579705956076, 12.52828553530646793 ) ) ;
#51379 = ORIENTED_EDGE ( 'NONE', *, *, #5592, .F. ) ;
#51380 = CARTESIAN_POINT ( 'NONE',  ( 9.965360841230999966, 4.034680274230000308, -6.102912434217000026 ) ) ;
#51381 = CARTESIAN_POINT ( 'NONE',  ( 7.293613499430000147, 1.437192322347000006, 0.3816175901828000039 ) ) ;
#51382 = EDGE_CURVE ( 'NONE', #25292, #15838, #47660, .T. ) ;
#51383 = ADVANCED_FACE ( 'NONE', ( #45375 ), #40133, .F. ) ;
#51384 = CARTESIAN_POINT ( 'NONE',  ( 10.62947109217999930, -5.100000000000000533, 6.152188490330000370 ) ) ;
#51386 = CARTESIAN_POINT ( 'NONE',  ( 10.13559687351566829, 5.092232985442826099, 8.129523725463617012 ) ) ;
#51385 = CARTESIAN_POINT ( 'NONE',  ( 8.881816940380000247, -4.977917894183000236, 6.416767031887000705 ) ) ;
#51387 = CARTESIAN_POINT ( 'NONE',  ( 12.10000000000000142, -4.531190383827668811, 8.305884920888427558 ) ) ;
#51388 = CIRCLE ( 'NONE', #67003, 1.000000000000000000 ) ;
#51389 = CARTESIAN_POINT ( 'NONE',  ( 10.52641638348499953, -4.974961480482700260, -7.262511127784999410 ) ) ;
#51390 = EDGE_LOOP ( 'NONE', ( #69050, #35168, #64472, #23255 ) ) ;
#51391 = B_SPLINE_CURVE_WITH_KNOTS ( 'NONE', 3,
 ( #22694, #44037, #54863, #49615 ),
 .UNSPECIFIED., .F., .F.,
 ( 4, 4 ),
 ( 0.000000000000000000, 1.000000000000000000 ),
 .UNSPECIFIED. ) ;
#51392 = EDGE_CURVE ( 'NONE', #10760, #4735, #5179, .T. ) ;
#51393 = CARTESIAN_POINT ( 'NONE',  ( 1.295927120944000199, -3.621562729233000599, -1.006310721376000084 ) ) ;
#51394 = CARTESIAN_POINT ( 'NONE',  ( 17.82925890471818064, -0.5617199691364276326, -12.68327559334252008 ) ) ;
#51396 = CARTESIAN_POINT ( 'NONE',  ( 13.64731601457200050, -9.647116713587001513, -7.903424745186999445 ) ) ;
#51395 = CARTESIAN_POINT ( 'NONE',  ( 8.722714158775000115, 3.892978337449999771, -8.893414073324001023 ) ) ;
#51397 = CARTESIAN_POINT ( 'NONE',  ( 7.000000000000000000, -7.356391799243646723, 3.356391799243647167 ) ) ;
#51398 = CARTESIAN_POINT ( 'NONE',  ( 15.49269116706029514, 8.815195450845969560, 7.616746626196044367 ) ) ;
#51399 = LINE ( 'NONE', #28710, #58757 ) ;
#51400 = CARTESIAN_POINT ( 'NONE',  ( 2.050973465875999935, 3.500000000000000000, 0.000000000000000000 ) ) ;
#51401 = CARTESIAN_POINT ( 'NONE',  ( 8.207504440379000954, -5.944572422272999646, 7.106845737860000511 ) ) ;
#51402 = ORIENTED_EDGE ( 'NONE', *, *, #50855, .F. ) ;
#51403 = CARTESIAN_POINT ( 'NONE',  ( 7.507482780409000078, 3.501518846194999757, 9.055971388486000251 ) ) ;
#51404 = CARTESIAN_POINT ( 'NONE',  ( 23.59999468372399889, -2.915558691838999739, 13.58549495651999983 ) ) ;
#51405 = CARTESIAN_POINT ( 'NONE',  ( 7.332307259148439726, -3.827065593140268174, 9.239363644322621028 ) ) ;
#51406 = CARTESIAN_POINT ( 'NONE',  ( 10.49640421544676983, -5.348966112464561995, 7.853238477522131333 ) ) ;
#51407 = CARTESIAN_POINT ( 'NONE',  ( 1.171064357889000096, 3.048238319583999711, -1.563029678068999839 ) ) ;
#51408 = ORIENTED_EDGE ( 'NONE', *, *, #18509, .F. ) ;
#51409 = CARTESIAN_POINT ( 'NONE',  ( 1.524776698570021516, -3.302120733362293947, 0.06692889220319675481 ) ) ;
#51410 = CARTESIAN_POINT ( 'NONE',  ( 11.44487616594229884, -4.303437140848100029, 8.456491899811199531 ) ) ;
#51411 = ADVANCED_FACE ( 'NONE', ( #67025, #46401 ), #62126, .F. ) ;
#51412 = CARTESIAN_POINT ( 'NONE',  ( 10.27427173614549716, -4.712533253186579785, 4.944156917096328208 ) ) ;
#51413 = CARTESIAN_POINT ( 'NONE',  ( 10.48165121391000021, 4.022873529486999722, 9.090897232145000117 ) ) ;
#51414 = CARTESIAN_POINT ( 'NONE',  ( 11.19102897915239936, 4.256858847510399890, 6.529961657816500065 ) ) ;
#51415 = DIRECTION ( 'NONE',  ( -1.000000000000000000, 0.000000000000000000, 0.000000000000000000 ) ) ;
#51416 = CARTESIAN_POINT ( 'NONE',  ( 9.160535748954998780, 2.900115872948000106, -6.152093930328999427 ) ) ;
#51417 = LINE ( 'NONE', #10825, #47622 ) ;
#51418 = CARTESIAN_POINT ( 'NONE',  ( 12.21825390183959392, -2.283832253985284666, 12.49935200980254812 ) ) ;
#51419 = B_SPLINE_CURVE_WITH_KNOTS ( 'NONE', 3,
 ( #54844, #55187, #66011, #32491, #7291, #6940 ),
 .UNSPECIFIED., .F., .F.,
 ( 4, 1, 1, 4 ),
 ( 0.000000000000000000, 0.2305484669808168796, 0.8346924774243514866, 1.000000000000000000 ),
 .UNSPECIFIED. ) ;
#51420 = CARTESIAN_POINT ( 'NONE',  ( 8.196909354935570491, 5.767095180863751835, 7.402880174889286735 ) ) ;
#51421 = ORIENTED_EDGE ( 'NONE', *, *, #65073, .T. ) ;
#51422 = CARTESIAN_POINT ( 'NONE',  ( 17.85663772380318903, -3.182036958951517835, 13.63358608099387581 ) ) ;
#51423 = CARTESIAN_POINT ( 'NONE',  ( 11.41486084871699802, -5.207010770456999893, -7.825000000000000178 ) ) ;
#51424 = ORIENTED_EDGE ( 'NONE', *, *, #32363, .T. ) ;
#51425 = ORIENTED_EDGE ( 'NONE', *, *, #50499, .F. ) ;
#51426 = CARTESIAN_POINT ( 'NONE',  ( 25.05004217274195000, -2.896626469317051811, -11.52364839812445396 ) ) ;
#51427 = CARTESIAN_POINT ( 'NONE',  ( 9.802263540183334456, 2.907767014557178786, -6.870476274536374994 ) ) ;
#51428 = AXIS2_PLACEMENT_3D ( 'NONE', #36487, #28597, #57808 ) ;
#51429 = CARTESIAN_POINT ( 'NONE',  ( 11.41672066707849886, 4.741156262620799922, 7.948314604624900248 ) ) ;
#51430 = CARTESIAN_POINT ( 'NONE',  ( 10.87021720923999979, 2.226038107033000202, 7.782753921296999167 ) ) ;
#51431 = CARTESIAN_POINT ( 'NONE',  ( 9.675534850247000662, 4.656736118461000551, -8.653212384786000300 ) ) ;
#51432 = CARTESIAN_POINT ( 'NONE',  ( 9.733483075504627990, -4.114479073428862321, -8.367425391989351979 ) ) ;
#51433 = CARTESIAN_POINT ( 'NONE',  ( 9.959635380193999410, -5.406637819064000539, 7.700301345050000634 ) ) ;
#51434 = CARTESIAN_POINT ( 'NONE',  ( 17.93788416347131331, 0.6112845611542863100, -12.58516990776526967 ) ) ;
#51435 = CARTESIAN_POINT ( 'NONE',  ( 6.899999692065000190, -12.99045401431999913, 1.690592943268000026 ) ) ;
#51436 = CARTESIAN_POINT ( 'NONE',  ( 10.45672469555900008, -3.566534988568399900, -6.750062220519700062 ) ) ;
#51437 = CARTESIAN_POINT ( 'NONE',  ( 7.854823341228001077, 4.561643343497000735, 6.153061759127000485 ) ) ;
#51438 = VERTEX_POINT ( 'NONE', #36247 ) ;
#51439 = AXIS2_PLACEMENT_3D ( 'NONE', #30761, #26205, #68487 ) ;
#51440 = CARTESIAN_POINT ( 'NONE',  ( 10.96256856629999987, -5.431962315094999383, -4.905456409002999507 ) ) ;
#51441 = PRESENTATION_STYLE_ASSIGNMENT (( #56695 ) ) ;
#51442 = CARTESIAN_POINT ( 'NONE',  ( 10.60000000000016662, 3.353329715112616238, -4.756097560975664607 ) ) ;
#51443 = CARTESIAN_POINT ( 'NONE',  ( 11.09999999999999964, -4.000000000000000000, 7.500000000000000000 ) ) ;
#51444 = CARTESIAN_POINT ( 'NONE',  ( 9.481734463323000739, 4.133249246727800141, -8.772253522581999974 ) ) ;
#51445 = EDGE_CURVE ( 'NONE', #53853, #50471, #36889, .T. ) ;
#51446 = CARTESIAN_POINT ( 'NONE',  ( 12.40968101568426007, 3.130119464836095933, 13.64559997174501049 ) ) ;
#51447 = EDGE_CURVE ( 'NONE', #20805, #35599, #40457, .T. ) ;
#51448 = CARTESIAN_POINT ( 'NONE',  ( 10.24478558459999888, -5.265199116477000452, 8.959495174640998982 ) ) ;
#51449 = ORIENTED_EDGE ( 'NONE', *, *, #22606, .T. ) ;
#51450 = CARTESIAN_POINT ( 'NONE',  ( 12.31001894287360265, -0.3816018583990969937, -12.69228475097292375 ) ) ;
#51451 = CARTESIAN_POINT ( 'NONE',  ( 12.39267642948476755, -0.6007076874295131930, 13.98710814480368292 ) ) ;
#51452 = ORIENTED_EDGE ( 'NONE', *, *, #24999, .T. ) ;
#51453 = CYLINDRICAL_SURFACE ( 'NONE', #63320, 1.250000000000000222 ) ;
#51454 = LINE ( 'NONE', #29468, #27036 ) ;
#51455 = CARTESIAN_POINT ( 'NONE',  ( 13.99999999308669629, 9.069400206872137105, 8.107642827045808076 ) ) ;
#51456 = CARTESIAN_POINT ( 'NONE',  ( 8.409459851179015288, 2.941725506722952854, 6.357402555654233289 ) ) ;
#51457 = CARTESIAN_POINT ( 'NONE',  ( 9.520528907821001141, 2.899999999999999911, 6.152188490330000370 ) ) ;
#51458 = CARTESIAN_POINT ( 'NONE',  ( -0.1370230224197999946, -1.720643726402999896, -3.153834707638000001 ) ) ;
#51459 = DIRECTION ( 'NONE',  ( -1.000000000000000000, 0.000000000000000000, 0.000000000000000000 ) ) ;
#51460 = FACE_OUTER_BOUND ( 'NONE', #31565, .T. ) ;
#51461 = DIRECTION ( 'NONE',  ( 0.000000000000000000, -0.2461538461537955691, -0.9692307692307821076 ) ) ;
#51462 = AXIS2_PLACEMENT_3D ( 'NONE', #58177, #69006, #15865 ) ;
#51463 = CARTESIAN_POINT ( 'NONE',  ( 10.69872335273220010, 4.349306362047499874, -8.440710326446700051 ) ) ;
#51464 = DIRECTION ( 'NONE',  ( 1.000000000000000000, 4.438568037851000240E-10, 1.557552607591000152E-09 ) ) ;
#51465 = CARTESIAN_POINT ( 'NONE',  ( 10.56983915876999980, 2.152856944368999770, -7.425100664021000441 ) ) ;
#51466 = CARTESIAN_POINT ( 'NONE',  ( 9.657975701332999208, 4.837683410033799980, -8.275900091855099561 ) ) ;
#51468 = CARTESIAN_POINT ( 'NONE',  ( 12.18236035866429390, 2.554391060822402970, 12.43872824571935176 ) ) ;
#51467 = DIRECTION ( 'NONE',  ( -1.000000000000000000, 0.000000000000000000, -1.233561263588000078E-14 ) ) ;
#51469 = CARTESIAN_POINT ( 'NONE',  ( 23.61968394240093616, -13.40114650748445335, 3.921251161824122367 ) ) ;
#51470 = ORIENTED_EDGE ( 'NONE', *, *, #17941, .T. ) ;
#51471 = EDGE_CURVE ( 'NONE', #68067, #59819, #14360, .T. ) ;
#51472 = CIRCLE ( 'NONE', #4548, 1.600000000000000089 ) ;
#51473 = CARTESIAN_POINT ( 'NONE',  ( 10.82035090130999855, 4.758726914843000699, 7.030721746772699454 ) ) ;
#51474 = CARTESIAN_POINT ( 'NONE',  ( 10.77962878203999963, -2.397503436487000261, 7.755423856053000442 ) ) ;
#51475 = CARTESIAN_POINT ( 'NONE',  ( 9.832317406968998696, 4.186809223719299311, 6.513113677132300161 ) ) ;
#51476 = CARTESIAN_POINT ( 'NONE',  ( 10.91080643070914213, -2.803404389956826392, -6.850777194059048725 ) ) ;
#51477 = CARTESIAN_POINT ( 'NONE',  ( 9.587239738464759853, -5.286462772564067158, -7.027016876574450954 ) ) ;
#51478 = CARTESIAN_POINT ( 'NONE',  ( 12.80505043854146940, -2.500000000000000444, -25.00000000000000000 ) ) ;
#51479 = CARTESIAN_POINT ( 'NONE',  ( 7.011490480521701762, -1.352039016092809298, -0.3642379411497885799 ) ) ;
#51480 = ORIENTED_EDGE ( 'NONE', *, *, #53493, .F. ) ;
#51481 = CARTESIAN_POINT ( 'NONE',  ( 9.379355082327998971, -4.511005581663400044, -6.478918346312998899 ) ) ;
#51482 = FACE_OUTER_BOUND ( 'NONE', #57890, .T. ) ;
#51483 = CARTESIAN_POINT ( 'NONE',  ( 12.02166954483529970, -3.437903757373499847, 8.367285821793199574 ) ) ;
#51484 = ADVANCED_FACE ( 'NONE', ( #36595 ), #25412, .T. ) ;
#51485 = CARTESIAN_POINT ( 'NONE',  ( 18.26928656998117972, 2.355301763765361045, -12.37791135143290866 ) ) ;
#51486 = CARTESIAN_POINT ( 'NONE',  ( 8.288959924527002698, -3.489898988435000238, -6.767656065023998302 ) ) ;
#51487 = DIRECTION ( 'NONE',  ( -0.6684585169941805738, -0.6684585169941805738, -0.3260773253629903334 ) ) ;
#51488 = CIRCLE ( 'NONE', #21343, 0.8000000000000000444 ) ;
#51489 = CARTESIAN_POINT ( 'NONE',  ( 12.23181585139621674, 2.749296767756840509, -13.61742212736085378 ) ) ;
#51490 = CARTESIAN_POINT ( 'NONE',  ( 9.570737326637999587, -4.261100936929000049, -5.979198511086000423 ) ) ;
#51491 = DIRECTION ( 'NONE',  ( 0.000000000000000000, 1.000000000000000000, 0.000000000000000000 ) ) ;
#51492 = CARTESIAN_POINT ( 'NONE',  ( 9.725191424783300675, -2.649754699899359522, 7.500009801425228773 ) ) ;
#51493 = CARTESIAN_POINT ( 'NONE',  ( 8.679055905797000037, -2.899999999999999911, 6.571291218949999902 ) ) ;
#51494 = CARTESIAN_POINT ( 'NONE',  ( 23.61768885478876356, 13.40073015714643923, 3.927800159012043490 ) ) ;
#51495 = CARTESIAN_POINT ( 'NONE',  ( 12.80505043854143388, 3.124999999999999556, 12.28373071562070074 ) ) ;
#51496 = CARTESIAN_POINT ( 'NONE',  ( 3.030140132544667519, 3.408904368339106483, -0.9161175952574748260 ) ) ;
#51497 = CARTESIAN_POINT ( 'NONE',  ( 9.807804719590000886, 3.988943694240999704, -8.966360307350999648 ) ) ;
#51498 = CARTESIAN_POINT ( 'NONE',  ( 6.555026506349999948, -1.500000000000000000, 0.000000000000000000 ) ) ;
#51499 = ORIENTED_EDGE ( 'NONE', *, *, #3726, .T. ) ;
#51500 = CARTESIAN_POINT ( 'NONE',  ( 9.281707361444031079, -3.320047962278884768, -8.679668831483224878 ) ) ;
#51501 = CARTESIAN_POINT ( 'NONE',  ( 18.18506112704242383, 2.156549459697482352, -13.83291014715494427 ) ) ;
#51502 = EDGE_LOOP ( 'NONE', ( #33190, #331, #25514, #42651 ) ) ;
#51503 = CARTESIAN_POINT ( 'NONE',  ( 10.82055864497999842, -3.317414799430800088, 6.965412239408199646 ) ) ;
#51504 = CARTESIAN_POINT ( 'NONE',  ( 2.592640132543833520, 3.058252359239899132, 1.762666431298155034 ) ) ;
#51505 = CARTESIAN_POINT ( 'NONE',  ( 8.447510841229000533, 4.933589693325000525, -9.154576215408999573 ) ) ;
#51506 = CARTESIAN_POINT ( 'NONE',  ( 9.934999999999998721, 4.640430492595999823, -9.117542781427999898 ) ) ;
#51507 = CARTESIAN_POINT ( 'NONE',  ( 10.47769598648999967, -2.990523684589000197, -8.101059042556599366 ) ) ;
#51508 = DIRECTION ( 'NONE',  ( 0.000000000000000000, 0.8648648648648720183, 0.5020047465136825426 ) ) ;
#51509 = CARTESIAN_POINT ( 'NONE',  ( 11.35393384239835690, -12.19578912391865444, -1.764073091440432561 ) ) ;
#51510 = ORIENTED_EDGE ( 'NONE', *, *, #45479, .F. ) ;
#51511 = CARTESIAN_POINT ( 'NONE',  ( 8.817462135714999150, 5.100000000000000533, 6.571291218949999902 ) ) ;
#51512 = CARTESIAN_POINT ( 'NONE',  ( 5.699994923231000321, 12.50864296698000011, 2.924709704137000266 ) ) ;
#51513 = CARTESIAN_POINT ( 'NONE',  ( 10.03280471959000231, 3.987760651117999711, -9.123263301387000368 ) ) ;
#51514 = VERTEX_POINT ( 'NONE', #57921 ) ;
#51515 = CARTESIAN_POINT ( 'NONE',  ( 10.55068356942999941, 2.412177153420000053, -6.919581319869999803 ) ) ;
#51516 = B_SPLINE_CURVE_WITH_KNOTS ( 'NONE', 3,
 ( #31213, #52517, #62659, #31547 ),
 .UNSPECIFIED., .F., .F.,
 ( 4, 4 ),
 ( 0.000000000000000000, 0.8163836489557126930 ),
 .UNSPECIFIED. ) ;
#51517 = ORIENTED_EDGE ( 'NONE', *, *, #28841, .T. ) ;
#51518 = CARTESIAN_POINT ( 'NONE',  ( 8.999417874593998334, 2.949199072237000063, 7.053287723251499663 ) ) ;
#51519 = CARTESIAN_POINT ( 'NONE',  ( 17.96242084756264390, -2.025889508701483432, -12.54946620628462917 ) ) ;
#51520 = DIRECTION ( 'NONE',  ( 0.000000000000000000, 0.000000000000000000, -1.000000000000000000 ) ) ;
#51521 = ADVANCED_FACE ( 'NONE', ( #25413 ), #10478, .F. ) ;
#51522 = EDGE_CURVE ( 'NONE', #62590, #11166, #21537, .T. ) ;
#51523 = VECTOR ( 'NONE', #27716, 1000.000000000000000 ) ;
#51524 = CARTESIAN_POINT ( 'NONE',  ( 10.90000000000000036, -8.091320520030999219, -7.077643127633000297 ) ) ;
#51525 = EDGE_CURVE ( 'NONE', #48366, #23094, #37617, .T. ) ;
#51526 = ADVANCED_FACE ( 'NONE', ( #53019 ), #15951, .T. ) ;
#51527 = CARTESIAN_POINT ( 'NONE',  ( 13.99999999231800096, -8.833253877201999060, -7.896562762484000686 ) ) ;
#51528 = ORIENTED_EDGE ( 'NONE', *, *, #57474, .T. ) ;
#51529 = DIRECTION ( 'NONE',  ( 0.8843050095428980351, 0.1786785984225995050, -0.4313682980505990638 ) ) ;
#51530 = CARTESIAN_POINT ( 'NONE',  ( 7.174999999999994493, 4.000000000000000000, 8.979903810567671840 ) ) ;
#51531 = FACE_OUTER_BOUND ( 'NONE', #8337, .T. ) ;
#51532 = CARTESIAN_POINT ( 'NONE',  ( 12.12494527865623972, 2.264899384641845259, -13.81558393673957141 ) ) ;
#51533 = CARTESIAN_POINT ( 'NONE',  ( 11.07299956498199833, 5.207010770456999893, 7.174999999999999822 ) ) ;
#51534 = CARTESIAN_POINT ( 'NONE',  ( 17.79229341877100268, 3.377812583009999869, 11.11021646535000151 ) ) ;
#51535 = VECTOR ( 'NONE', #27018, 1000.000000000000000 ) ;
#51536 = CARTESIAN_POINT ( 'NONE',  ( 18.17483763484055004, -2.416937413759673969, 12.47057468849341078 ) ) ;
#51537 = ORIENTED_EDGE ( 'NONE', *, *, #29143, .T. ) ;
#51538 = ORIENTED_EDGE ( 'NONE', *, *, #48129, .F. ) ;
#51539 = CARTESIAN_POINT ( 'NONE',  ( 9.974220280410998285, 5.496789211521000418, -7.043125396300999874 ) ) ;
#51540 = CARTESIAN_POINT ( 'NONE',  ( 5.966666563597951445, 12.43894384121852248, 2.828928431917153485 ) ) ;
#51541 = CARTESIAN_POINT ( 'NONE',  ( 7.350695902300781626, -3.999976678040469746, 6.116819565496747657 ) ) ;
#51542 = CARTESIAN_POINT ( 'NONE',  ( 24.98216315915700036, 8.515971576431999424, -8.483917917255999086 ) ) ;
#51543 = CARTESIAN_POINT ( 'NONE',  ( 24.25866889917200098, 8.929925749802000823, -8.812657214412999096 ) ) ;
#51544 = CARTESIAN_POINT ( 'NONE',  ( 18.35481756226800343, -2.723642650930000020, -11.47750709399999991 ) ) ;
#51546 = CARTESIAN_POINT ( 'NONE',  ( 7.810832536737804865, 4.190757782081667493, 6.135062409754994839 ) ) ;
#51545 = CARTESIAN_POINT ( 'NONE',  ( 10.08103849359899939, -3.173653894988100355, 8.287963554181398962 ) ) ;
#51547 = CARTESIAN_POINT ( 'NONE',  ( 8.507487536397000838, -5.082459883441999615, -6.579846171250996356 ) ) ;
#51548 = ORIENTED_EDGE ( 'NONE', *, *, #60533, .F. ) ;
#51549 = CARTESIAN_POINT ( 'NONE',  ( 11.59999999999999964, 4.000000000000000000, 7.500000000000000000 ) ) ;
#51550 = CARTESIAN_POINT ( 'NONE',  ( 10.49684650188000035, -3.093163888438999809, -5.046887178931999784 ) ) ;
#51551 = CARTESIAN_POINT ( 'NONE',  ( 9.326385834542001874, -4.867164667115999599, -6.095483598963999938 ) ) ;
#51552 = CARTESIAN_POINT ( 'NONE',  ( 7.954939691786412581, 5.004658466033554021, 6.485426177601712361 ) ) ;
#51553 = CARTESIAN_POINT ( 'NONE',  ( 1.699999999999999956, 0.000000000000000000, 0.000000000000000000 ) ) ;
#51554 = CARTESIAN_POINT ( 'NONE',  ( 11.04426809015000011, -5.244714960646999380, 5.175279275819000269 ) ) ;
#51555 = CARTESIAN_POINT ( 'NONE',  ( 25.59997384872700010, 11.07537887597999848, -3.096069522331000190 ) ) ;
#51556 = CARTESIAN_POINT ( 'NONE',  ( 7.780759508074995168, -4.599947829706001912, 6.384407252255998699 ) ) ;
#51557 = VECTOR ( 'NONE', #65337, 1000.000000000000000 ) ;
#51558 = CARTESIAN_POINT ( 'NONE',  ( 6.563702397401000255, 1.130384497037000058, -0.3246714051208999807 ) ) ;
#51559 = ADVANCED_FACE ( 'NONE', ( #36944 ), #16638, .F. ) ;
#51560 = CARTESIAN_POINT ( 'NONE',  ( 0.2813751657999145617, 0.8596862427041435106, 3.195618825391118190 ) ) ;
#51561 = CARTESIAN_POINT ( 'NONE',  ( 3.205611318989000313, 1.247253500342999866, -3.010921006634000197 ) ) ;
#51562 = ORIENTED_EDGE ( 'NONE', *, *, #6691, .F. ) ;
#51563 = CARTESIAN_POINT ( 'NONE',  ( 12.78440276244763574, -0.6249994333735316987, -12.67928921956170818 ) ) ;
#51564 = B_SPLINE_CURVE_WITH_KNOTS ( 'NONE', 3,
 ( #59041, #52764, #64615, #47179, #31790, #16040, #68482, #53108, #42961, #38052, #42286, #4857, #11143, #20952, #59377, #20605, #63588, #26200, #48204, #37034, #21626 ),
 .UNSPECIFIED., .F., .F.,
 ( 4, 2, 2, 2, 1, 2, 2, 1, 1, 2, 2, 4 ),
 ( 0.000000000000000000, 0.1249999999999983902, 0.1875000000000058009, 0.2500000000000132117, 0.3125000000000205946, 0.3437500000000301981, 0.3750000000000398015, 0.4375000000000550671, 0.4687500000000596745, 0.4843750000000524580, 0.5000000000000451861, 1.000000000000000000 ),
 .UNSPECIFIED. ) ;
#51565 = CARTESIAN_POINT ( 'NONE',  ( 12.33520056820728072, -2.912263648500925672, -12.34589992753920740 ) ) ;
#51566 = EDGE_CURVE ( 'NONE', #60441, #29347, #45190, .T. ) ;
#51567 = DIRECTION ( 'NONE',  ( -1.000000000000000000, 0.000000000000000000, 0.000000000000000000 ) ) ;
#51568 = CARTESIAN_POINT ( 'NONE',  ( 7.614801658771000348, 3.326263523254000098, 8.794511546544999447 ) ) ;
#51569 = CARTESIAN_POINT ( 'NONE',  ( 11.59999999999999964, 4.000000000000000000, -7.500000000000000000 ) ) ;
#51570 = ORIENTED_EDGE ( 'NONE', *, *, #19255, .T. ) ;
#51571 = DIRECTION ( 'NONE',  ( 1.000000000000000000, 0.000000000000000000, 0.000000000000000000 ) ) ;
#51572 = B_SPLINE_CURVE_WITH_KNOTS ( 'NONE', 3,
 ( #51079, #19254, #15042, #57681 ),
 .UNSPECIFIED., .F., .F.,
 ( 4, 4 ),
 ( 0.000000000000000000, 1.000000000000000000 ),
 .UNSPECIFIED. ) ;
#51573 = PRODUCT_CONTEXT ( 'NONE', #32885, 'mechanical' ) ;
#51574 = CARTESIAN_POINT ( 'NONE',  ( 0.5839156351703003178, 1.786861044915114549, 3.043887924358878561 ) ) ;
#51575 = CARTESIAN_POINT ( 'NONE',  ( 13.32922381500400100, -11.63215034022999994, -1.960198572322999988 ) ) ;
#51576 = CARTESIAN_POINT ( 'NONE',  ( 10.29657053952199952, 3.497746311184500190, 8.675184076076000395 ) ) ;
#51577 = CARTESIAN_POINT ( 'NONE',  ( 11.05946005378019947, 5.036385109519999403, -6.946587256304699309 ) ) ;
#51578 = VERTEX_POINT ( 'NONE', #20856 ) ;
#51579 = CARTESIAN_POINT ( 'NONE',  ( 10.14750362918999826, -2.602959084636999876, 6.738575912023000214 ) ) ;
#51580 = EDGE_LOOP ( 'NONE', ( #54013, #61301, #1474 ) ) ;
#51581 = CARTESIAN_POINT ( 'NONE',  ( 12.04292372906209430, -2.967457464456210836, 6.730835578941808173 ) ) ;
#51582 = CARTESIAN_POINT ( 'NONE',  ( 8.625066940379999991, -3.117370956513999758, 8.662188901935000018 ) ) ;
#51583 = AXIS2_PLACEMENT_3D ( 'NONE', #64676, #52826, #43719 ) ;
#51584 = CARTESIAN_POINT ( 'NONE',  ( 18.27863135987958287, 0.04720351400547010551, -13.99992551180917211 ) ) ;
#51585 = ORIENTED_EDGE ( 'NONE', *, *, #45927, .F. ) ;
#51586 = CARTESIAN_POINT ( 'NONE',  ( 23.57244473461747702, 10.28737204536955119, 9.478197202474877514 ) ) ;
#51587 = CARTESIAN_POINT ( 'NONE',  ( 10.90000668870999867, 0.2999999999999999889, -9.776630298829998011 ) ) ;
#51588 = CARTESIAN_POINT ( 'NONE',  ( 7.482204719588999353, 2.733910551100999786, -6.580132171107999639 ) ) ;
#51589 = CARTESIAN_POINT ( 'NONE',  ( 16.39999997324030900, -3.261216865579173341, -11.32142606715090416 ) ) ;
#51590 = CARTESIAN_POINT ( 'NONE',  ( 8.167796732633897605, -2.954779252209375873, 6.459714628853201468 ) ) ;
#51591 = ORIENTED_EDGE ( 'NONE', *, *, #53434, .F. ) ;
#51592 = CARTESIAN_POINT ( 'NONE',  ( 11.08492081570999943, -3.668392767032000013, 5.558160538745999801 ) ) ;
#51593 = DIRECTION ( 'NONE',  ( -1.000000000000000000, 0.000000000000000000, 0.000000000000000000 ) ) ;
#51594 = FACE_BOUND ( 'NONE', #26032, .T. ) ;
#51595 = CARTESIAN_POINT ( 'NONE',  ( 10.68375832677999959, -4.547311397465000127, -8.749131152219000285 ) ) ;
#51596 = CARTESIAN_POINT ( 'NONE',  ( 10.90000000011000125, 2.899999999889000257, -6.571291220762999430 ) ) ;
#51597 = B_SPLINE_CURVE_WITH_KNOTS ( 'NONE', 3,
 ( #47205, #54415, #4535, #8247 ),
 .UNSPECIFIED., .F., .F.,
 ( 4, 4 ),
 ( 0.000000000000000000, 0.1253746098019370980 ),
 .UNSPECIFIED. ) ;
#51598 = EDGE_LOOP ( 'NONE', ( #18061, #2728, #46989, #7530 ) ) ;
#51599 = CARTESIAN_POINT ( 'NONE',  ( 10.75765839980110528, 5.312263182874568557, 8.656084424456086168 ) ) ;
#51600 = CARTESIAN_POINT ( 'NONE',  ( 25.46373185538400463, 11.23406899464000119, 3.161078463958999496 ) ) ;
#51601 = CARTESIAN_POINT ( 'NONE',  ( 10.43314899746000002, -5.167567567567999731, 6.822293592207000934 ) ) ;
#51602 = CARTESIAN_POINT ( 'NONE',  ( 3.042640132543832809, 3.058252359239899132, 1.762666431298154146 ) ) ;
#51603 = ADVANCED_FACE ( 'NONE', ( #6142 ), #4763, .T. ) ;
#51604 = CARTESIAN_POINT ( 'NONE',  ( 12.25867852505488997, 0.3036576181174169831, -13.89554011873102546 ) ) ;
#51605 = EDGE_CURVE ( 'NONE', #13349, #12119, #56082, .T. ) ;
#51607 = EDGE_CURVE ( 'NONE', #2983, #31596, #68976, .T. ) ;
#51606 = CARTESIAN_POINT ( 'NONE',  ( 18.17062868725396640, -2.391413364859044766, 12.47623124499065028 ) ) ;
#51608 = EDGE_LOOP ( 'NONE', ( #12671, #8315, #58215, #37660, #49513, #12829 ) ) ;
#51609 = CARTESIAN_POINT ( 'NONE',  ( 8.079287380335998137, -4.920039154826996608, 6.237958006931995314 ) ) ;
#51610 = ORIENTED_EDGE ( 'NONE', *, *, #53455, .T. ) ;
#51611 = CARTESIAN_POINT ( 'NONE',  ( 10.34947814066000049, 4.457562099971999814, 6.154877938302999674 ) ) ;
#51612 = B_SPLINE_CURVE_WITH_KNOTS ( 'NONE', 3,
 ( #44841, #65095, #12326, #66147 ),
 .UNSPECIFIED., .F., .F.,
 ( 4, 4 ),
 ( 0.000000000000000000, 1.000000000000000000 ),
 .UNSPECIFIED. ) ;
#51613 = CARTESIAN_POINT ( 'NONE',  ( 23.60000000000000142, -9.305479840184000651, -8.315530346521999405 ) ) ;
#51614 = CARTESIAN_POINT ( 'NONE',  ( 8.839404719593998649, 5.140767546012999567, -6.196177269779999719 ) ) ;
#51615 = CARTESIAN_POINT ( 'NONE',  ( 2.509915357491000254, 2.041422993037000033, 2.896642013889999756 ) ) ;
#51616 = CARTESIAN_POINT ( 'NONE',  ( 10.60198654464000079, -2.164987663130000239, -7.764523632348000248 ) ) ;
#51617 = PLANE ( 'NONE',  #19424 ) ;
#51618 = CARTESIAN_POINT ( 'NONE',  ( 25.30000327618300204, -9.659335867304687184, 6.394377797198702140 ) ) ;
#51619 = ORIENTED_EDGE ( 'NONE', *, *, #35996, .T. ) ;
#51620 = CARTESIAN_POINT ( 'NONE',  ( 12.17918044953561996, -2.988516238873000219, 6.972563939641199582 ) ) ;
#51621 = B_SPLINE_CURVE_WITH_KNOTS ( 'NONE', 3,
 ( #11133, #9750, #68131, #20249 ),
 .UNSPECIFIED., .F., .F.,
 ( 4, 4 ),
 ( 0.000000000000000000, 1.000000000000000000 ),
 .UNSPECIFIED. ) ;
#51622 = B_SPLINE_CURVE_WITH_KNOTS ( 'NONE', 3,
 ( #61073, #34166, #55484, #13191, #34521, #24698 ),
 .UNSPECIFIED., .F., .F.,
 ( 4, 1, 1, 4 ),
 ( 0.000000000000000000, 0.1550125199478044891, 0.7488612388459089386, 1.000000000000000000 ),
 .UNSPECIFIED. ) ;
#51623 = CARTESIAN_POINT ( 'NONE',  ( 16.04718133169100014, 8.956716759973000208, 8.677900031540000114 ) ) ;
#51624 = EDGE_CURVE ( 'NONE', #50591, #52043, #27732, .T. ) ;
#51625 = CARTESIAN_POINT ( 'NONE',  ( 10.90000154029999990, -11.35000000000000142, 0.000000000000000000 ) ) ;
#51627 = CARTESIAN_POINT ( 'NONE',  ( 12.61587921998065021, 3.224448188370961255, -13.62362021573479431 ) ) ;
#51626 = CARTESIAN_POINT ( 'NONE',  ( 9.476372460169001144, 5.098395626600999542, 6.305536056092000408 ) ) ;
#51628 = CIRCLE ( 'NONE', #39361, 2.000000000000001332 ) ;
#51629 = CARTESIAN_POINT ( 'NONE',  ( 10.94487616594229884, 3.696562859151900415, -6.543508100188799581 ) ) ;
#51630 = FACE_OUTER_BOUND ( 'NONE', #1115, .T. ) ;
#51631 = VECTOR ( 'NONE', #13555, 1000.000000000000114 ) ;
#51632 = CARTESIAN_POINT ( 'NONE',  ( 10.36422949779699820, 4.557226039164599563, -8.335668797826500054 ) ) ;
#51633 = CARTESIAN_POINT ( 'NONE',  ( 18.05961319350868166, 0.5166535389540052314, 12.58940585649086508 ) ) ;
#51634 = CARTESIAN_POINT ( 'NONE',  ( 24.70869262301700076, 3.610540981815000272, 12.15034266584999934 ) ) ;
#51635 = CARTESIAN_POINT ( 'NONE',  ( 11.75203632436369894, 2.890282938442000127, 7.759151359668400083 ) ) ;
#51636 = CARTESIAN_POINT ( 'NONE',  ( 23.73963774284500161, 9.840645693113000192, 9.517990711560001316 ) ) ;
#51637 = ORIENTED_EDGE ( 'NONE', *, *, #5284, .T. ) ;
#51638 = CARTESIAN_POINT ( 'NONE',  ( 7.743183059623000020, -2.735207418315000361, 6.771977475428999860 ) ) ;
#51639 = PLANE ( 'NONE',  #61744 ) ;
#51640 = CARTESIAN_POINT ( 'NONE',  ( 8.654403730149667240, 2.899999999999999911, 6.499666959930667787 ) ) ;
#51641 = CARTESIAN_POINT ( 'NONE',  ( 10.04193802597399987, 3.549239910423600097, 8.240623579255899500 ) ) ;
#51642 = ORIENTED_EDGE ( 'NONE', *, *, #26275, .F. ) ;
#51643 = B_SPLINE_CURVE_WITH_KNOTS ( 'NONE', 3,
 ( #17195, #57020, #45847, #35703 ),
 .UNSPECIFIED., .F., .F.,
 ( 4, 4 ),
 ( 0.000000000000000000, 1.000000000000000000 ),
 .UNSPECIFIED. ) ;
#51644 = CARTESIAN_POINT ( 'NONE',  ( 0.1976626962874999949, 2.474918916286999782, -2.043501580946999852 ) ) ;
#51645 = CARTESIAN_POINT ( 'NONE',  ( 11.60477869730532774, 3.532552483170099844, 8.421761806503198500 ) ) ;
#51646 = CARTESIAN_POINT ( 'NONE',  ( 10.09249221959000131, 2.841614569232000065, -8.724659027040001291 ) ) ;
#51647 = ORIENTED_EDGE ( 'NONE', *, *, #26268, .T. ) ;
#51648 = CARTESIAN_POINT ( 'NONE',  ( 5.096693173016665135, -1.310679582531386389, -0.7554284705563492075 ) ) ;
#51649 = CARTESIAN_POINT ( 'NONE',  ( 17.55505043854144276, 0.6250000000000001110, -13.88107975066922428 ) ) ;
#51650 = CARTESIAN_POINT ( 'NONE',  ( 11.47810404293059960, 3.436653965247300047, 6.352848032645000309 ) ) ;
#51651 = EDGE_CURVE ( 'NONE', #9931, #14587, #52209, .T. ) ;
#51652 = CARTESIAN_POINT ( 'NONE',  ( 10.63462194421999918, -5.668721490782999695, 6.527259573254000635 ) ) ;
#51653 = DIRECTION ( 'NONE',  ( 0.000000000000000000, -0.9979288589194759140, 0.06432723012591848311 ) ) ;
#51654 = ORIENTED_EDGE ( 'NONE', *, *, #65124, .F. ) ;
#51655 = DIRECTION ( 'NONE',  ( 0.4384236320213992233, -0.6355252626312997144, -0.6355252626312997144 ) ) ;
#51656 = CARTESIAN_POINT ( 'NONE',  ( 7.865239158766999417, 5.556101987819999977, -8.589999141415001205 ) ) ;
#51657 = APPLICATION_CONTEXT ( 'automotive_design' ) ;
#51658 = CARTESIAN_POINT ( 'NONE',  ( 8.219916112706140865, -5.679804218022393769, 7.950509028919302779 ) ) ;
#51659 = CARTESIAN_POINT ( 'NONE',  ( 10.61188779216199940, -2.816792857868000155, 7.073306690476799830 ) ) ;
#51660 = ORIENTED_EDGE ( 'NONE', *, *, #65478, .T. ) ;
#51662 = CARTESIAN_POINT ( 'NONE',  ( 2.803056799209541872, -2.798833948393629978, -2.150913519912204031 ) ) ;
#51661 = AXIS2_PLACEMENT_3D ( 'NONE', #30411, #57305, #36685 ) ;
#51663 = CARTESIAN_POINT ( 'NONE',  ( 17.55505043854144631, -0.7192913403693119712, -12.57945229203838267 ) ) ;
#51664 = VERTEX_POINT ( 'NONE', #6840 ) ;
#51665 = CARTESIAN_POINT ( 'NONE',  ( 9.998096873515667227, -4.327184855449103473, 6.282534154164607365 ) ) ;
#51666 = ORIENTED_EDGE ( 'NONE', *, *, #2690, .F. ) ;
#51667 = CARTESIAN_POINT ( 'NONE',  ( 9.888906509039999904, -2.890602650755999647, -6.682694598879999504 ) ) ;
#51668 = PLANE ( 'NONE',  #63894 ) ;
#51669 = CARTESIAN_POINT ( 'NONE',  ( 10.47769598648999967, 5.009476315410999803, -8.101059042556599366 ) ) ;
#51670 = CARTESIAN_POINT ( 'NONE',  ( 12.13611496860034933, -2.828587461987000395, 8.100294210499798808 ) ) ;
#51671 = CARTESIAN_POINT ( 'NONE',  ( 12.43829333464978859, 1.993817424706644914, -12.55522976296196980 ) ) ;
#51672 = CARTESIAN_POINT ( 'NONE',  ( 11.46533729122639933, -5.140346530769000388, 7.529998433785960010 ) ) ;
#51673 = CARTESIAN_POINT ( 'NONE',  ( 7.822385841228999048, 4.636729845879000500, 9.378977473003999421 ) ) ;
#51674 = ORIENTED_EDGE ( 'NONE', *, *, #18065, .T. ) ;
#51675 = CARTESIAN_POINT ( 'NONE',  ( 9.448096873516666605, 3.672815144550898303, -8.717465845835395299 ) ) ;
#51676 = CIRCLE ( 'NONE', #34982, 11.29999999999999538 ) ;
#51677 = CARTESIAN_POINT ( 'NONE',  ( 8.417495559623999313, -2.029110377978999846, 7.726994002375999315 ) ) ;
#51678 = CARTESIAN_POINT ( 'NONE',  ( 9.843930206850000530, 2.750000000000000000, 7.500000000000000000 ) ) ;
#51679 = EDGE_LOOP ( 'NONE', ( #62139, #38618, #43939, #32295 ) ) ;
#51680 = CARTESIAN_POINT ( 'NONE',  ( 12.43906710990146003, -3.006741445058540574, -12.31893827218669557 ) ) ;
#51681 = CARTESIAN_POINT ( 'NONE',  ( 11.57656516821460890, 4.899536366368299589, 6.592171857671999646 ) ) ;
#51682 = CARTESIAN_POINT ( 'NONE',  ( 10.37239314679000124, -3.992345679293999972, -5.977234595428000397 ) ) ;
#51683 = CARTESIAN_POINT ( 'NONE',  ( 10.84254308255000154, 9.576923094808998727, -6.615458963921999391 ) ) ;
#51684 = CARTESIAN_POINT ( 'NONE',  ( 17.79165415090800195, -3.528207907415000122, -11.96069611418000100 ) ) ;
#51685 = CARTESIAN_POINT ( 'NONE',  ( 24.43231275843600159, -8.806084858358998346, 8.751970408574999638 ) ) ;
#51686 = CARTESIAN_POINT ( 'NONE',  ( 12.23404092485631267, -2.245077680571258671, -13.72419654341781126 ) ) ;
#51687 = CARTESIAN_POINT ( 'NONE',  ( 11.68748876160954886, -4.600381688599499697, -8.124372018288600117 ) ) ;
#51688 = CARTESIAN_POINT ( 'NONE',  ( 11.35502763632549872, -5.160433036184000066, -6.964545474268299508 ) ) ;
#51689 = EDGE_CURVE ( 'NONE', #32483, #11912, #66846, .T. ) ;
#51691 = ADVANCED_FACE ( 'NONE', ( #56466 ), #4341, .T. ) ;
#51690 = CARTESIAN_POINT ( 'NONE',  ( 10.12947109217999930, 5.100000000000000533, 6.152188490330000370 ) ) ;
#51692 = EDGE_LOOP ( 'NONE', ( #30145, #13962, #33597, #7648 ) ) ;
#51693 = EDGE_LOOP ( 'NONE', ( #20603, #392, #4629, #55896, #60881, #13853, #16352, #55800, #48832, #50057, #66691, #8383, #1835 ) ) ;
#51694 = CARTESIAN_POINT ( 'NONE',  ( 12.35913878030157598, 0.5835546239762330334, -13.98799446467094221 ) ) ;
#51695 = SURFACE_STYLE_USAGE ( .BOTH. , #8712 ) ;
#51696 = CARTESIAN_POINT ( 'NONE',  ( 23.50387503050299998, 0.000000000000000000, 0.000000000000000000 ) ) ;
#51697 = CARTESIAN_POINT ( 'NONE',  ( 18.11601457969558737, 2.775767521728004006, 13.61104273367227258 ) ) ;
#51698 = CARTESIAN_POINT ( 'NONE',  ( 10.94349541711000029, 3.081616890687000065, -8.919380927961000793 ) ) ;
#51699 = DIRECTION ( 'NONE',  ( 0.000000000000000000, 1.000000000000000000, 0.000000000000000000 ) ) ;
#51700 = CARTESIAN_POINT ( 'NONE',  ( 18.09708155689161657, 2.811828937043456822, 12.37344130164188627 ) ) ;
#51701 = CARTESIAN_POINT ( 'NONE',  ( 25.55308368780314510, 2.866379683385739785, -11.19759676586897257 ) ) ;
#51702 = CARTESIAN_POINT ( 'NONE',  ( 10.87021720923999979, 2.226038107033000202, 7.782753921296999167 ) ) ;
#51703 = CARTESIAN_POINT ( 'NONE',  ( 10.18795867446420722, -4.829522773136136315, -8.579479308275068661 ) ) ;
#51704 = B_SPLINE_CURVE_WITH_KNOTS ( 'NONE', 3,
 ( #28426, #55333, #33323, #39252, #49049 ),
 .UNSPECIFIED., .F., .F.,
 ( 4, 1, 4 ),
 ( 0.000000000000000000, 0.5000000000000000000, 1.000000000000000000 ),
 .UNSPECIFIED. ) ;
#51705 = ORIENTED_EDGE ( 'NONE', *, *, #65698, .T. ) ;
#51706 = CARTESIAN_POINT ( 'NONE',  ( 12.70142344966306602, -3.116692473072852021, 12.28627407840914643 ) ) ;
#51707 = CARTESIAN_POINT ( 'NONE',  ( 8.969113844317998741, -3.781046324972699768, -6.661091642253600398 ) ) ;
#51708 = CARTESIAN_POINT ( 'NONE',  ( 9.479214860607999782, 4.071727169861000029, 9.089299483126000112 ) ) ;
#51709 = EDGE_CURVE ( 'NONE', #54265, #46886, #30582, .T. ) ;
#51710 = CARTESIAN_POINT ( 'NONE',  ( 11.55435090131019926, -2.880552878538999995, 6.807613609764599616 ) ) ;
#51711 = CARTESIAN_POINT ( 'NONE',  ( 9.219485841232998524, 3.892978337449999771, -8.893414073324001023 ) ) ;
#51712 = AXIS2_PLACEMENT_3D ( 'NONE', #41930, #26546, #4510 ) ;
#51713 = PRODUCT ( 'Negative Post', 'Negative Post', '', ( #68327 ) ) ;
#51714 = EDGE_CURVE ( 'NONE', #63300, #12790, #48523, .T. ) ;
#51715 = CARTESIAN_POINT ( 'NONE',  ( 24.95781766713999872, 8.510855470215000551, 8.989990260059000704 ) ) ;
#51716 = CARTESIAN_POINT ( 'NONE',  ( 12.20137806200446029, 0.1622035078961257260, 12.69861136640059129 ) ) ;
#51717 = CARTESIAN_POINT ( 'NONE',  ( 8.160739158772001289, 5.944584532500000407, 7.106843289410999631 ) ) ;
#51718 = CARTESIAN_POINT ( 'NONE',  ( 9.786671076420999427, 2.381202181614999525, 7.612749448318000489 ) ) ;
#51719 = CARTESIAN_POINT ( 'NONE',  ( 11.31919037786000182, -3.456300244116000453, 11.37193521011000108 ) ) ;
#51720 = ORIENTED_EDGE ( 'NONE', *, *, #17671, .F. ) ;
#51721 = CARTESIAN_POINT ( 'NONE',  ( 9.775320280412000074, 2.527713920559999661, -6.969421869128999525 ) ) ;
#51722 = CARTESIAN_POINT ( 'NONE',  ( 7.094364705359000212, -0.9274734728647999749, -1.162302709265000011 ) ) ;
#51723 = CARTESIAN_POINT ( 'NONE',  ( 24.37808886002350306, -12.29705476218489046, 3.189923891270713074 ) ) ;
#51724 = CARTESIAN_POINT ( 'NONE',  ( 4.599999999999999645, 0.7192913403693119712, -12.57945229203838267 ) ) ;
#51725 = CARTESIAN_POINT ( 'NONE',  ( 10.32309687351566652, 2.782534154164606921, -7.172815144550894750 ) ) ;
#51726 = CARTESIAN_POINT ( 'NONE',  ( 11.19102897915239936, -3.743141152489600110, -8.470038342183499935 ) ) ;
#51727 = EDGE_LOOP ( 'NONE', ( #23426, #45057, #27220, #2083 ) ) ;
#51728 = AXIS2_PLACEMENT_3D ( 'NONE', #58223, #5430, #16605 ) ;
#51729 = CARTESIAN_POINT ( 'NONE',  ( 1.920565801736000111, 3.542864650996000453, -0.5932612529451999350 ) ) ;
#51730 = CARTESIAN_POINT ( 'NONE',  ( 17.63677106500005465, -0.6210356003259921431, -12.67955509032280403 ) ) ;
#51731 = CIRCLE ( 'NONE', #59518, 13.10000000000000320 ) ;
#51733 = CARTESIAN_POINT ( 'NONE',  ( 14.04809435262700035, -9.134678144910999720, -8.215103563399999587 ) ) ;
#51732 = CARTESIAN_POINT ( 'NONE',  ( 8.772439158776000667, 3.098073081301000009, -8.567513114264999174 ) ) ;
#51734 = CARTESIAN_POINT ( 'NONE',  ( 18.15002510833730653, -2.691473085186385727, 13.63098399825532070 ) ) ;
#51735 = DIRECTION ( 'NONE',  ( 1.000000000000000000, 0.000000000000000000, 0.000000000000000000 ) ) ;
#51736 = CARTESIAN_POINT ( 'NONE',  ( 12.75695158412492880, -3.246897126047502358, 13.61828421767944164 ) ) ;
#51737 = CARTESIAN_POINT ( 'NONE',  ( 10.62903166480609940, 3.135947233695900227, 7.439078678739090122 ) ) ;
#51738 = CYLINDRICAL_SURFACE ( 'NONE', #19873, 0.4999999999999998335 ) ;
#51739 = CARTESIAN_POINT ( 'NONE',  ( 8.116918146793999256, -5.773185758034999893, 7.141496747382000798 ) ) ;
#51740 = VERTEX_POINT ( 'NONE', #51221 ) ;
#51741 = CARTESIAN_POINT ( 'NONE',  ( 8.406107780410998487, 5.342170561818999630, 8.432311822615000452 ) ) ;
#51742 =( BOUNDED_SURFACE ( )  B_SPLINE_SURFACE ( 3, 3, ( 
 ( #40051, #66599, #50187, #45970 ),
 ( #29217, #56810, #55433, #40378 ),
 ( #3313, #62046, #19051, #8566 ),
 ( #67279, #45637, #56463, #13482 ) ),
 .UNSPECIFIED., .F., .F., .T. ) 
 B_SPLINE_SURFACE_WITH_KNOTS ( ( 4, 4 ),
 ( 4, 4 ),
 ( 0.000000000000000000, 1.000000000000000000 ),
 ( 0.000000000000000000, 1.000000000000000000 ),
 .UNSPECIFIED. ) 
 GEOMETRIC_REPRESENTATION_ITEM ( )  RATIONAL_B_SPLINE_SURFACE ( (
 ( 1.512182578520000042, 1.160176301760999840, 1.160176301760999840, 1.512182578520000042),
 ( 1.111288591041000196, 0.8526025270081000196, 0.8526025270081000196, 1.111288591041000196),
 ( 1.111288591041000196, 0.8526025270081000196, 0.8526025270081000196, 1.111288591041000196),
 ( 1.512182578520000042, 1.160176301760999840, 1.160176301760999840, 1.512182578520000042) ) ) 
 REPRESENTATION_ITEM ( '' )  SURFACE ( )  );
#51744 = CARTESIAN_POINT ( 'NONE',  ( 10.90760155002999987, 5.030021895791999320, 4.934359348414000479 ) ) ;
#51743 = CARTESIAN_POINT ( 'NONE',  ( 5.469792710280000136, 0.08722338096737999869, 1.612367018429999854 ) ) ;
#51745 = CARTESIAN_POINT ( 'NONE',  ( 7.576913711449058120, -4.062718167131674996, 5.761938145506621645 ) ) ;
#51746 = CARTESIAN_POINT ( 'NONE',  ( 18.06968158351558884, -0.3547715225555931884, 13.89390930605073393 ) ) ;
#51747 = CARTESIAN_POINT ( 'NONE',  ( 1.457156054533999878, -3.424908732075000017, 0.06941761548046999908 ) ) ;
#51748 = EDGE_LOOP ( 'NONE', ( #52680, #54973, #13845, #41717, #6164 ) ) ;
#51749 = CARTESIAN_POINT ( 'NONE',  ( 1.000275254720587315, -3.126551503801492604, 1.064497837873157327 ) ) ;
#51750 = CARTESIAN_POINT ( 'NONE',  ( 11.10441638348510018, -4.841589649988700117, 7.705001100909899314 ) ) ;
#51751 = CARTESIAN_POINT ( 'NONE',  ( 10.32671362595031006, -4.830823584655211889, 4.959879567452830429 ) ) ;
#51752 = CARTESIAN_POINT ( 'NONE',  ( 10.16829701902000060, 4.567214950372999738, 5.832525041908999341 ) ) ;
#51753 = CARTESIAN_POINT ( 'NONE',  ( 11.50687348028854906, 2.996540789803000315, 6.957450711802899868 ) ) ;
#51754 = PRODUCT_DEFINITION ( 'UNKNOWN', '', #1666, #312 ) ;
#51755 = CARTESIAN_POINT ( 'NONE',  ( 9.817462135711998883, 5.100000000000000533, 6.571291218949999902 ) ) ;
#51756 = CARTESIAN_POINT ( 'NONE',  ( 17.97872601847937801, 3.578425380680016588, -12.00298730842260930 ) ) ;
#51757 = CARTESIAN_POINT ( 'NONE',  ( 12.34388784977539899, -5.255745690988000263, 7.571757098260779806 ) ) ;
#51758 = CARTESIAN_POINT ( 'NONE',  ( 7.739871862179882989, 5.559621021845134514, 8.354610903474103623 ) ) ;
#51759 = ORIENTED_EDGE ( 'NONE', *, *, #7477, .T. ) ;
#51760 = CIRCLE ( 'NONE', #21612, 11.50000000000000533 ) ;
#51761 = CARTESIAN_POINT ( 'NONE',  ( 17.79021264935889945, -3.209040350003993236, 13.62725621160039502 ) ) ;
#51762 = LINE ( 'NONE', #51423, #20466 ) ;
#51763 = VERTEX_POINT ( 'NONE', #40721 ) ;
#51764 = VERTEX_POINT ( 'NONE', #34806 ) ;
#51765 = DIRECTION ( 'NONE',  ( 0.000000000000000000, 0.2588190451024934835, -0.9659258262890757507 ) ) ;
#51766 = VERTEX_POINT ( 'NONE', #36166 ) ;
#51767 = CARTESIAN_POINT ( 'NONE',  ( 8.428055354833562163, 3.943840852781273387, 6.010070386527693209 ) ) ;
#51768 = CARTESIAN_POINT ( 'NONE',  ( 11.39210538575740017, 4.842454415653899780, 7.701417844014099678 ) ) ;
#51769 = CARTESIAN_POINT ( 'NONE',  ( 10.65550720192000078, 4.237674045823999869, 9.105219676299999065 ) ) ;
#51770 = DIRECTION ( 'NONE',  ( -0.9999999999999987788, 4.835295647719984237E-08, -1.472971858110998225E-08 ) ) ;
#51771 = CARTESIAN_POINT ( 'NONE',  ( 10.31021345716899873, -3.363461959113699606, -8.078719053813800954 ) ) ;
#51772 = CARTESIAN_POINT ( 'NONE',  ( 9.980430903642000473, -4.047223565251000466, 9.090364706348999846 ) ) ;
#51773 = CARTESIAN_POINT ( 'NONE',  ( 18.16427545049632286, 0.3901114995139649544, -12.59396323349877989 ) ) ;
#51774 = CARTESIAN_POINT ( 'NONE',  ( 10.20917469696999902, -3.334764780022000163, -5.769478358936999562 ) ) ;
#51775 = CARTESIAN_POINT ( 'NONE',  ( 10.67826222744820086, -4.668580868411999596, -8.050725169876500331 ) ) ;
#51776 = EDGE_CURVE ( 'NONE', #30122, #43332, #57478, .T. ) ;
#51778 = EDGE_CURVE ( 'NONE', #13432, #59076, #60166, .T. ) ;
#51777 = CARTESIAN_POINT ( 'NONE',  ( 7.029903297284646690, 0.4289550007897103834, 1.323513554004721149 ) ) ;
#51779 = ORIENTED_EDGE ( 'NONE', *, *, #33486, .T. ) ;
#51780 = CIRCLE ( 'NONE', #28383, 1.300165623000000270 ) ;
#51781 = CARTESIAN_POINT ( 'NONE',  ( 9.482564767455610166, -5.103418008754404767, 7.204352198296668064 ) ) ;
#51782 = CARTESIAN_POINT ( 'NONE',  ( 10.31746213571000048, -5.100000000000000533, 6.571291218949999902 ) ) ;
#51783 = CARTESIAN_POINT ( 'NONE',  ( 24.94500410606760710, 8.558268712512990817, 8.385800952028061417 ) ) ;
#51784 = CIRCLE ( 'NONE', #32819, 1.250000000000000888 ) ;
#51785 = CARTESIAN_POINT ( 'NONE',  ( 11.88093429839001658, 9.756630077891992769, 5.709945283618997003 ) ) ;
#51786 = CARTESIAN_POINT ( 'NONE',  ( 12.29903578917715379, 3.040996334883330210, 13.66573881806045598 ) ) ;
#51787 = DIRECTION ( 'NONE',  ( 1.000000000000000000, 0.000000000000000000, 0.000000000000000000 ) ) ;
#51788 = ORIENTED_EDGE ( 'NONE', *, *, #64570, .T. ) ;
#51789 = CARTESIAN_POINT ( 'NONE',  ( 12.25734197677224202, -0.3012394091496986559, -12.69519438487131069 ) ) ;
#51790 = CARTESIAN_POINT ( 'NONE',  ( 12.14438218221665267, -0.3016537271415141164, 13.99676704218776990 ) ) ;
#51791 = ORIENTED_EDGE ( 'NONE', *, *, #58641, .T. ) ;
#51792 = CARTESIAN_POINT ( 'NONE',  ( 6.105026506350000659, -1.500000000000000000, 0.000000000000000000 ) ) ;
#51793 = CARTESIAN_POINT ( 'NONE',  ( 23.59999172237900211, -2.915589696762999949, -13.58550518520000061 ) ) ;
#51794 = CARTESIAN_POINT ( 'NONE',  ( 10.72934687351609817, -4.163624617374463099, -6.249999999999998224 ) ) ;
#51795 = CARTESIAN_POINT ( 'NONE',  ( 11.79364426047339975, -3.533902447304699823, 6.769896129503799820 ) ) ;
#51796 = EDGE_CURVE ( 'NONE', #65786, #36471, #58903, .T. ) ;
#51797 = CARTESIAN_POINT ( 'NONE',  ( 10.59393020684899867, 5.250000000000000000, 7.500000000000000000 ) ) ;
#51798 = CARTESIAN_POINT ( 'NONE',  ( 17.60000000649198171, -11.44336891997908090, 3.156190330102982333 ) ) ;
#51799 = CARTESIAN_POINT ( 'NONE',  ( 11.25361999289386539, 3.455907502640804374, 8.657883396625686956 ) ) ;
#51800 = CARTESIAN_POINT ( 'NONE',  ( 11.59999999999999964, 3.182579051151299687, 7.825000000000000178 ) ) ;
#51801 = CARTESIAN_POINT ( 'NONE',  ( 7.307500000000000107, -0.2999999999999999889, 3.149999999999999911 ) ) ;
#51802 = CARTESIAN_POINT ( 'NONE',  ( 11.68333460557258796, 4.162011815820000571, -8.490304555719900392 ) ) ;
#51803 = CARTESIAN_POINT ( 'NONE',  ( 9.860260465798509344, 4.592567190355682172, -8.996616293939812437 ) ) ;
#51804 = CARTESIAN_POINT ( 'NONE',  ( 10.82035090130999855, 4.758726914843000699, -7.969278253227299658 ) ) ;
#51805 = CARTESIAN_POINT ( 'NONE',  ( 9.250696787962999323, 4.219671260427300119, -6.239790126677999815 ) ) ;
#51807 = CARTESIAN_POINT ( 'NONE',  ( 12.19170508189790425, 2.620143503867971901, 12.42276098599301548 ) ) ;
#51806 = CARTESIAN_POINT ( 'NONE',  ( 10.20000030442999872, -12.49999969551000056, 3.568610900609000272E-10 ) ) ;
#51808 = CARTESIAN_POINT ( 'NONE',  ( 23.57258086761195415, -13.35170972070031681, 4.170319815648626083 ) ) ;
#51809 = ORIENTED_EDGE ( 'NONE', *, *, #24869, .F. ) ;
#51810 = AXIS2_PLACEMENT_3D ( 'NONE', #6744, #23522, #28084 ) ;
#51811 = PLANE ( 'NONE',  #19929 ) ;
#51812 = CARTESIAN_POINT ( 'NONE',  ( 11.09999999999999964, -4.000000000000000000, 7.500000000000000000 ) ) ;
#51813 = CARTESIAN_POINT ( 'NONE',  ( 9.551684229509998403, 3.388828644390000200, 8.114961396014498618 ) ) ;
#51814 = CARTESIAN_POINT ( 'NONE',  ( 9.252229279041625176, 4.091138914130668880, -8.370187317335780364 ) ) ;
#51815 = CARTESIAN_POINT ( 'NONE',  ( 7.000000000000000000, 0.000000000000000000, 0.000000000000000000 ) ) ;
#51816 = DIRECTION ( 'NONE',  ( 0.000000000000000000, 0.000000000000000000, 1.000000000000000000 ) ) ;
#51817 = DIRECTION ( 'NONE',  ( -0.9999999999999613642, 3.249250440393876213E-08, 2.763724548567895895E-07 ) ) ;
#51818 = CARTESIAN_POINT ( 'NONE',  ( 24.30001122380595291, 3.256147833935072899, 12.15210915319683060 ) ) ;
#51819 = ORIENTED_EDGE ( 'NONE', *, *, #44078, .F. ) ;
#51820 = CARTESIAN_POINT ( 'NONE',  ( 5.037467514214999831, 1.016370699457000093, -0.5038814123657998634 ) ) ;
#51821 = CARTESIAN_POINT ( 'NONE',  ( 9.352013376692999813, -5.140392946802999852, -6.920441276178300072 ) ) ;
#51822 = DIRECTION ( 'NONE',  ( 0.7071068207016518725, 0.000000000000000000, -0.7071067416714409415 ) ) ;
#51823 = CARTESIAN_POINT ( 'NONE',  ( 11.56967835872019990, -4.754733798270200928, 7.975673736933100777 ) ) ;
#51824 = CARTESIAN_POINT ( 'NONE',  ( 18.21784200350676741, 2.188139590168312498, -12.40855205325248356 ) ) ;
#51825 = CARTESIAN_POINT ( 'NONE',  ( 10.95279684016000132, -2.845132595845000001, 5.182798816160999245 ) ) ;
#51826 = VECTOR ( 'NONE', #47117, 1000.000000000000114 ) ;
#51827 = DIRECTION ( 'NONE',  ( 0.000000000000000000, -1.000000000000000000, 0.000000000000000000 ) ) ;
#51828 = EDGE_CURVE ( 'NONE', #23381, #49108, #3316, .T. ) ;
#51829 = EDGE_CURVE ( 'NONE', #25486, #7230, #32168, .T. ) ;
#51830 = CARTESIAN_POINT ( 'NONE',  ( 12.48673873072914020, 3.044366353191839458, -13.54286685750310504 ) ) ;
#51831 = CARTESIAN_POINT ( 'NONE',  ( 11.55336220499919975, -4.965402920923000174, 7.174999999999999822 ) ) ;
#51832 = CARTESIAN_POINT ( 'NONE',  ( 11.08729972629000038, -2.258669075224000178, -7.034582301298999418 ) ) ;
#51833 = CARTESIAN_POINT ( 'NONE',  ( 8.965984360231558981, -5.205022649008422597, 8.206117015345352428 ) ) ;
#51834 = CIRCLE ( 'NONE', #7176, 1.000000000000000666 ) ;
#51835 = CARTESIAN_POINT ( 'NONE',  ( 12.25981791760051109, 0.4818816852691563124, -13.99171642476390076 ) ) ;
#51836 = CARTESIAN_POINT ( 'NONE',  ( 13.55563472374800149, -9.144188282469000839, -7.452974878633000344 ) ) ;
#51837 = LINE ( 'NONE', #14786, #36507 ) ;
#51838 = CARTESIAN_POINT ( 'NONE',  ( 2.404534975661500429, 1.236092914997090064, -3.291825510064177784 ) ) ;
#51839 = CARTESIAN_POINT ( 'NONE',  ( 8.921614158776000281, 3.251172436837000301, -6.320036569851000152 ) ) ;
#51840 = CARTESIAN_POINT ( 'NONE',  ( 12.23671932425159881, -4.127012898954600217, 6.643164954553199664 ) ) ;
#51841 = EDGE_LOOP ( 'NONE', ( #17274, #12631, #18299, #20799 ) ) ;
#51842 = CARTESIAN_POINT ( 'NONE',  ( 8.497376085219370268, -4.829144488946368163, 8.579037299257766591 ) ) ;
#51843 = CARTESIAN_POINT ( 'NONE',  ( 18.20740272079781619, 2.198619098391829230, -13.82629845589066342 ) ) ;
#51844 = ORIENTED_EDGE ( 'NONE', *, *, #2360, .T. ) ;
#51845 = CARTESIAN_POINT ( 'NONE',  ( 10.66858376188599955, -4.731143729777899765, 7.034020612385399218 ) ) ;
#51846 = CARTESIAN_POINT ( 'NONE',  ( 10.97124174884019965, 3.963805917081910213, 6.184229974648999928 ) ) ;
#51847 = CARTESIAN_POINT ( 'NONE',  ( 4.600000127571202135, 3.375077994860000042E-14, 13.89999852642010403 ) ) ;
#51848 = CARTESIAN_POINT ( 'NONE',  ( 9.865041550948095761, 2.650034642413356512, -7.500002425457249267 ) ) ;
#51849 = CARTESIAN_POINT ( 'NONE',  ( 11.06456920625009843, -3.962850971080120299, -6.467161360063999886 ) ) ;
#51850 = CARTESIAN_POINT ( 'NONE',  ( 11.60000000000000320, -2.860800829850470794, -7.074412716661199418 ) ) ;
#51851 = CARTESIAN_POINT ( 'NONE',  ( 11.79999999771000141, -12.39026187696000036, -1.832249219479999969 ) ) ;
#51852 = ORIENTED_EDGE ( 'NONE', *, *, #61507, .F. ) ;
#51853 = CARTESIAN_POINT ( 'NONE',  ( 9.925810748568999031, 2.827416853083249304, -8.000243450341617546 ) ) ;
#51855 = EDGE_CURVE ( 'NONE', #18634, #33492, #11861, .T. ) ;
#51854 = CARTESIAN_POINT ( 'NONE',  ( 9.833904719592002408, 5.048004622677000341, -6.120508709481000231 ) ) ;
#51856 = ORIENTED_EDGE ( 'NONE', *, *, #46199, .F. ) ;
#51857 = VECTOR ( 'NONE', #30684, 1000.000000000000227 ) ;
#51858 = CARTESIAN_POINT ( 'NONE',  ( 10.44486820642000069, 4.964088085664999817, -9.083609801695999408 ) ) ;
#51859 = EDGE_CURVE ( 'NONE', #66543, #17007, #58543, .T. ) ;
#51860 = VERTEX_POINT ( 'NONE', #45641 ) ;
#51861 = CARTESIAN_POINT ( 'NONE',  ( 8.898101285863999621, 3.264788442324599860, 8.373612278672599274 ) ) ;
#51862 = CARTESIAN_POINT ( 'NONE',  ( 17.88769455523112484, -1.970775861831701947, -12.55923393539036148 ) ) ;
#51863 = CARTESIAN_POINT ( 'NONE',  ( 16.24418116638901921, 3.625803901486591929, 11.98884806668391256 ) ) ;
#51864 = FACE_OUTER_BOUND ( 'NONE', #19084, .T. ) ;
#51865 = CARTESIAN_POINT ( 'NONE',  ( 9.817462135711998883, 5.100000000000000533, 6.571291218949999902 ) ) ;
#51866 = EDGE_LOOP ( 'NONE', ( #21301, #24731, #42899, #29910 ) ) ;
#51867 = CARTESIAN_POINT ( 'NONE',  ( 11.53828694957233481, 4.309606737214646266, 6.264939056470322676 ) ) ;
#51868 = CARTESIAN_POINT ( 'NONE',  ( 10.38726084123000071, 2.888676266723000374, -6.716337836090000124 ) ) ;
#51869 = VECTOR ( 'NONE', #14407, 1000.000000000000000 ) ;
#51870 = CYLINDRICAL_SURFACE ( 'NONE', #11773, 0.6250000000000005551 ) ;
#51871 = DIRECTION ( 'NONE',  ( -1.000000000000000000, 0.000000000000000000, -4.629487027253999916E-14 ) ) ;
#51872 = ADVANCED_FACE ( 'NONE', ( #46322 ), #46667, .T. ) ;
#51873 = CARTESIAN_POINT ( 'NONE',  ( 18.00570828977289040, 0.5721320424853906239, 13.98830666644471954 ) ) ;
#51874 = CARTESIAN_POINT ( 'NONE',  ( 18.04399228544049905, 11.57290723012127032, -4.790145353825725927 ) ) ;
#51875 = CARTESIAN_POINT ( 'NONE',  ( 9.870877370727999534, -2.904359058094999835, -8.563874348197000330 ) ) ;
#51876 = ORIENTED_EDGE ( 'NONE', *, *, #35531, .T. ) ;
#51877 = ORIENTED_EDGE ( 'NONE', *, *, #60224, .F. ) ;
#51878 = CARTESIAN_POINT ( 'NONE',  ( 10.01508584123000034, 4.845406482350000488, -6.387189183984999907 ) ) ;
#51879 = FACE_OUTER_BOUND ( 'NONE', #64814, .T. ) ;
#51880 = CARTESIAN_POINT ( 'NONE',  ( 8.296584958550784705, -4.202842144468573515, 6.085974855212024082 ) ) ;
#51881 = CARTESIAN_POINT ( 'NONE',  ( 24.95401031917199930, 8.513686805178998895, -8.994139667403999283 ) ) ;
#51882 = CARTESIAN_POINT ( 'NONE',  ( 9.099999999999999645, 0.000000000000000000, 0.000000000000000000 ) ) ;
#51884 = VECTOR ( 'NONE', #47824, 1000.000000000000000 ) ;
#51883 = CARTESIAN_POINT ( 'NONE',  ( 5.200000002332999749, 0.2500000023327000331, -3.149999979209999967 ) ) ;
#51886 = CARTESIAN_POINT ( 'NONE',  ( 8.802452061267722172, 4.497572718073743481, 9.205822469557245924 ) ) ;
#51885 = CARTESIAN_POINT ( 'NONE',  ( 9.576468108405999047, -2.769196120524999749, 7.151422676278199830 ) ) ;
#51887 = FACE_OUTER_BOUND ( 'NONE', #18703, .T. ) ;
#51888 = EDGE_LOOP ( 'NONE', ( #10731, #42212, #60705, #35605 ) ) ;
#51889 = B_SPLINE_CURVE_WITH_KNOTS ( 'NONE', 3,
 ( #59540, #42432, #47337, #63743, #27047, #68643, #37524, #63399, #121, #15853 ),
 .UNSPECIFIED., .F., .F.,
 ( 4, 2, 2, 2, 4 ),
 ( 0.4999999999999994449, 0.6249999999999995559, 0.7499999999999997780, 0.8749999999999998890, 1.000000000000000000 ),
 .UNSPECIFIED. ) ;
#51890 = CARTESIAN_POINT ( 'NONE',  ( 9.727263540182331525, 4.629523725463627670, -6.407767014557179230 ) ) ;
#51891 = CARTESIAN_POINT ( 'NONE',  ( 11.09999999999999964, 2.700000000000000178, 5.160242713806000303 ) ) ;
#51892 = CARTESIAN_POINT ( 'NONE',  ( 9.839739029020998728, -5.130141620686999637, -6.219151643305999677 ) ) ;
#51893 = CARTESIAN_POINT ( 'NONE',  ( 7.909880988579637950, 4.709301544937013695, 6.316488363215514212 ) ) ;
#51894 = CARTESIAN_POINT ( 'NONE',  ( 11.79999998109720849, 11.63601885445003425, 1.847750289993329131 ) ) ;
#51895 = CARTESIAN_POINT ( 'NONE',  ( 11.13353229228999908, -5.335146187777999316, 5.116023372597999774 ) ) ;
#51896 = CARTESIAN_POINT ( 'NONE',  ( 9.640910841231999484, 2.212639797530000063, -6.855876382544999537 ) ) ;
#51897 = CARTESIAN_POINT ( 'NONE',  ( 13.73869549901200315, 8.889050979574999900, 7.612322772148999661 ) ) ;
#51898 = CARTESIAN_POINT ( 'NONE',  ( 7.980579959020838388, 3.019615321986244716, -6.448822506946575217 ) ) ;
#51899 = CARTESIAN_POINT ( 'NONE',  ( 6.009144881614999711, 0.6694104981402000387, -0.9669902716602000181 ) ) ;
#51900 = B_SPLINE_SURFACE_WITH_KNOTS ( 'NONE', 3, 3, ( 
 ( #4488, #47158, #57990, #30397, #19899, #21269, #20929, #31425, #42598, #52741, #63569, #3802, #15681, #37015, #63910, #46471, #62536, #54463, #16703, #38380, #43638, #54809, #49561, #58674, #1672, #32119, #6563, #38731, #22989, #17048, #53435, #27551, #6908, #38031, #16363 ),
 ( #289, #49215, #64934, #59706, #22640, #21949, #27906, #37693, #5531, #5871, #28243, #33495, #54114, #44338, #65635, #1323, #987, #21608, #33148, #59022, #43984, #17762, #65290, #22298, #17407, #10773, #26871, #60059, #48880, #640, #11125, #32457, #64249, #48187, #43289 ),
 ( #11807, #12164, #53774, #42941, #27209, #48534, #64594, #59358, #11459, #32800, #6213, #50601, #2023, #28954, #13554, #40120, #60742, #66324, #8635, #2703, #23341, #44685, #45362, #34187, #55503, #60403, #49910, #51285, #29642, #7951, #19121, #18446, #3041, #39080, #7605 ),
 ( #29984, #67349, #34871, #39772, #18792, #24028, #35218, #3381, #12507, #24717, #33840, #56189, #40445, #46042, #66670, #55154, #29290, #56531, #61090, #65977, #61770, #7259, #28599, #61434, #50945, #12857, #8296, #45703, #18104, #50257, #13891, #24374, #13211, #2362, #67012 ) ),
 .UNSPECIFIED., .F., .F., .F.,
 ( 4, 4 ),
 ( 4, 1, 1, 1, 1, 1, 1, 1, 1, 1, 1, 1, 1, 1, 1, 1, 1, 1, 1, 1, 1, 1, 1, 1, 1, 1, 1, 1, 1, 1, 1, 1, 4 ),
 ( -0.1039370721279000015, 1.103937072127999963 ),
 ( -0.01933701211302999920, 0.01208563257065999909, 0.04350827725433999843, 0.07493092193802000645, 0.1063535666217000075, 0.1377762113054000204, 0.1691988559891000055, 0.2006215006727000150, 0.2320441453564000001, 0.2634667900400999851, 0.2948894347238000258, 0.3263120794074999553, 0.3577347240911999959, 0.3891573687748000054, 0.4205800134584999905, 0.4520026581421999756, 0.4834253028259000162, 0.5148479475096000568, 0.5462705921932000663, 0.5776932368768999959, 0.6091158815606000365, 0.6405385262443000771, 0.6719611709280000067, 0.7033838156117000473, 0.7348064602953000568, 0.7662291049789999864, 0.7976517496627000270, 0.8290743943464000676, 0.8604970390300999972, 0.8919196837138000378, 0.9233423283974000473, 0.9547649730810999769, 0.9861876177648000175 ),
 .UNSPECIFIED. ) ;
#51901 = CARTESIAN_POINT ( 'NONE',  ( 0.2153359931920000025, 3.215315751876999695, 1.126573897625000029E-09 ) ) ;
#51902 = DIRECTION ( 'NONE',  ( 0.000000000000000000, 1.000000000000000000, 0.000000000000000000 ) ) ;
#51903 = ORIENTED_EDGE ( 'NONE', *, *, #20743, .F. ) ;
#51904 = ADVANCED_FACE ( 'NONE', ( #61705 ), #13822, .F. ) ;
#51905 = ADVANCED_FACE ( 'NONE', ( #67973 ), #58486, .T. ) ;
#51906 = CARTESIAN_POINT ( 'NONE',  ( 12.41256632787946756, -0.4864235087029714633, -12.68745975172791240 ) ) ;
#51907 = CARTESIAN_POINT ( 'NONE',  ( 12.24249432806117888, -2.226917153383584758, -12.51101585362955859 ) ) ;
#51908 = DIRECTION ( 'NONE',  ( 0.000000000000000000, -1.000000000000000000, 0.000000000000000000 ) ) ;
#51909 = CARTESIAN_POINT ( 'NONE',  ( 1.284778341492999868E-07, 0.000000000000000000, 0.000000000000000000 ) ) ;
#51910 = CARTESIAN_POINT ( 'NONE',  ( 3.500000000000000000, -1.789730407083999886, 2.652709005895000249 ) ) ;
#51911 = EDGE_LOOP ( 'NONE', ( #12772, #45102, #19195, #65945 ) ) ;
#51912 = CARTESIAN_POINT ( 'NONE',  ( 5.341892472960999783, -1.146783406111000048, -0.2608682635935000160 ) ) ;
#51913 = EDGE_CURVE ( 'NONE', #31596, #27235, #29835, .T. ) ;
#51914 = DIRECTION ( 'NONE',  ( 1.000000000000000000, 0.000000000000000000, 0.000000000000000000 ) ) ;
#51915 = CARTESIAN_POINT ( 'NONE',  ( 0.6466687473056148550, -0.8995628260960769618, 3.414327399381721584 ) ) ;
#51916 = CARTESIAN_POINT ( 'NONE',  ( 10.90000000164000049, 5.100000000007000267, 5.160242739040000082 ) ) ;
#51917 = CARTESIAN_POINT ( 'NONE',  ( 10.07503300763299947, 4.881889043637199777, 6.575021251017499679 ) ) ;
#51918 = CARTESIAN_POINT ( 'NONE',  ( 11.48011496860029901, 4.919769165942200040, -7.028661263734299780 ) ) ;
#51919 = ORIENTED_EDGE ( 'NONE', *, *, #27187, .F. ) ;
#51920 = CARTESIAN_POINT ( 'NONE',  ( 10.42595817177000050, -5.042180160032999403, 8.702227297563000619 ) ) ;
#51921 = ORIENTED_EDGE ( 'NONE', *, *, #2157, .T. ) ;
#51922 = CARTESIAN_POINT ( 'NONE',  ( 7.550000000000000711, -4.000000000000000000, 8.849999999999999645 ) ) ;
#51923 = CARTESIAN_POINT ( 'NONE',  ( 8.946004440379999423, -5.458705123429999695, 7.456451825584000659 ) ) ;
#51924 = CONICAL_SURFACE ( 'NONE', #30729, 2.624999810206000372, 0.7853980665166908626 ) ;
#51925 = CARTESIAN_POINT ( 'NONE',  ( 10.64393020684969926, -2.750000000000000000, -7.500000000000000000 ) ) ;
#51926 = VERTEX_POINT ( 'NONE', #24218 ) ;
#51927 = CARTESIAN_POINT ( 'NONE',  ( 7.100000000000000533, 12.03770622561999915, -3.722046322334000124 ) ) ;
#51928 = DIRECTION ( 'NONE',  ( 1.000000000000000000, 0.000000000000000000, 0.000000000000000000 ) ) ;
#51929 = CARTESIAN_POINT ( 'NONE',  ( 8.020320280406000535, 2.268410489563000176, -7.553872882963998947 ) ) ;
#51930 = CARTESIAN_POINT ( 'NONE',  ( 11.09999999999999964, -5.350000000000000533, 7.500000000000000000 ) ) ;
#51931 = CARTESIAN_POINT ( 'NONE',  ( 17.88880419370420327, -3.028786488652052800, 12.31252201556900339 ) ) ;
#51932 = ORIENTED_EDGE ( 'NONE', *, *, #2357, .F. ) ;
#51933 = CARTESIAN_POINT ( 'NONE',  ( 10.02990552045999983, -2.506467134554999809, 6.215414506835998942 ) ) ;
#51934 = CARTESIAN_POINT ( 'NONE',  ( 12.19254401039981772, -2.624350118461198367, -13.64624664190003500 ) ) ;
#51935 = DIRECTION ( 'NONE',  ( 5.839779914975694033E-06, 0.7070792670853635054, -0.7071342941930635062 ) ) ;
#51936 = ORIENTED_EDGE ( 'NONE', *, *, #35845, .T. ) ;
#51937 = CARTESIAN_POINT ( 'NONE',  ( 9.858853446676000942, -2.668079545448999834, -7.206971019603000350 ) ) ;
#51938 = CARTESIAN_POINT ( 'NONE',  ( 10.86123236735334530, -5.100000000000000533, -6.348362623949493688 ) ) ;
#51939 = ORIENTED_EDGE ( 'NONE', *, *, #56908, .F. ) ;
#51940 = CARTESIAN_POINT ( 'NONE',  ( 10.76566879297876511, 5.188023026155113016, 8.781755977163156146 ) ) ;
#51941 = DIRECTION ( 'NONE',  ( 0.7071067617951957152, 0.000000000000000000, -0.7071068005778986532 ) ) ;
#51942 = DIRECTION ( 'NONE',  ( -1.000000000000000000, 0.000000000000000000, -2.609704304917999919E-14 ) ) ;
#51943 = DIRECTION ( 'NONE',  ( 1.000000000000000000, 0.000000000000000000, 0.000000000000000000 ) ) ;
#51944 = CARTESIAN_POINT ( 'NONE',  ( 12.37622832409308238, 2.954798090471128624, 13.56635979911537859 ) ) ;
#51945 = CIRCLE ( 'NONE', #63114, 0.5000000000000000000 ) ;
#51946 = CARTESIAN_POINT ( 'NONE',  ( 17.87083331331565006, -1.960545027353535863, 12.56104967893681845 ) ) ;
#51947 = ORIENTED_EDGE ( 'NONE', *, *, #11044, .T. ) ;
#51948 = CARTESIAN_POINT ( 'NONE',  ( 8.434756776051003158, -5.098765216145000778, 6.624660916390000764 ) ) ;
#51949 = ORIENTED_EDGE ( 'NONE', *, *, #19086, .F. ) ;
#51950 = CARTESIAN_POINT ( 'NONE',  ( 9.681187238460999822, 2.612249048987000055, 7.804677627401999551 ) ) ;
#51951 = DIRECTION ( 'NONE',  ( -3.759177529598868022E-06, -0.7070924869988756134, -0.7071210750752756624 ) ) ;
#51952 = FACE_OUTER_BOUND ( 'NONE', #18863, .T. ) ;
#51953 = CARTESIAN_POINT ( 'NONE',  ( 2.356219824740000135, 1.924171680976999976, -2.845918095194999609 ) ) ;
#51954 = CARTESIAN_POINT ( 'NONE',  ( 10.28773706650000008, -5.077599250153999932, -5.991350640809000261 ) ) ;
#51955 = EDGE_CURVE ( 'NONE', #51763, #64065, #50801, .T. ) ;
#51956 = CARTESIAN_POINT ( 'NONE',  ( 15.90000000000000036, 8.729799320959164888, 8.474717466972236934 ) ) ;
#51957 = CARTESIAN_POINT ( 'NONE',  ( 23.61707908624700281, 13.18052050803000164, 4.240820030121000173 ) ) ;
#51958 = VERTEX_POINT ( 'NONE', #45893 ) ;
#51959 = EDGE_CURVE ( 'NONE', #53716, #42472, #24907, .T. ) ;
#51960 = CARTESIAN_POINT ( 'NONE',  ( 10.75564828895399927, -3.119330945648699949, 7.018986873610899124 ) ) ;
#51961 = CARTESIAN_POINT ( 'NONE',  ( 5.200000000000000178, -11.29999999999999893, 0.000000000000000000 ) ) ;
#51962 = FACE_OUTER_BOUND ( 'NONE', #68822, .T. ) ;
#51963 = FACE_OUTER_BOUND ( 'NONE', #27929, .T. ) ;
#51965 = DIRECTION ( 'NONE',  ( 1.000000000000000000, 0.000000000000000000, 0.000000000000000000 ) ) ;
#51964 = CARTESIAN_POINT ( 'NONE',  ( 11.02286749330999882, 2.398743616553999924, 6.352468982205000891 ) ) ;
#51966 = CARTESIAN_POINT ( 'NONE',  ( 11.40841235500449891, 3.158861363519000154, -6.729431436870699557 ) ) ;
#51967 = CARTESIAN_POINT ( 'NONE',  ( 8.731616107288068918, -3.999997736744774546, -8.381579007094499545 ) ) ;
#51968 = CARTESIAN_POINT ( 'NONE',  ( 9.399709346416997846, 4.783195203880800328, -7.128095150442700145 ) ) ;
#51969 = CARTESIAN_POINT ( 'NONE',  ( 18.19734990864320778, 0.3336735144251340435, 12.59558214381612551 ) ) ;
#51970 = CARTESIAN_POINT ( 'NONE',  ( 6.774531911923999949, -0.7882360144965000481, 0.7672747788395000157 ) ) ;
#51971 = B_SPLINE_CURVE_WITH_KNOTS ( 'NONE', 3,
 ( #38170, #31915, #43779, #21746 ),
 .UNSPECIFIED., .F., .F.,
 ( 4, 4 ),
 ( 0.000000000000000000, 1.000000000000000000 ),
 .UNSPECIFIED. ) ;
#51972 = CARTESIAN_POINT ( 'NONE',  ( 11.71922412107039868, 4.069539071394910223, 8.814426450544999625 ) ) ;
#51973 = CARTESIAN_POINT ( 'NONE',  ( 0.3288139673412197039, 2.029848442696892796, -2.674009039041026270 ) ) ;
#51974 = ORIENTED_EDGE ( 'NONE', *, *, #55444, .T. ) ;
#51975 = CARTESIAN_POINT ( 'NONE',  ( 9.117519353207999444, -4.954907757874000396, 8.825780921426000347 ) ) ;
#51976 = CARTESIAN_POINT ( 'NONE',  ( 17.82352195865853872, 3.196339915866913906, 13.63023968027431465 ) ) ;
#51977 = CARTESIAN_POINT ( 'NONE',  ( 6.954847353040172209, -0.9689943386775232703, 1.116583658536274948 ) ) ;
#51978 = EDGE_LOOP ( 'NONE', ( #33396, #13987, #45277, #15962, #66969 ) ) ;
#51979 = CARTESIAN_POINT ( 'NONE',  ( 0.1648568235610000099, -2.003871238023999801, -2.529037764236000019 ) ) ;
#51980 = CARTESIAN_POINT ( 'NONE',  ( 11.39700581613019992, 4.869652672166700391, 6.941573685175900010 ) ) ;
#51981 = CARTESIAN_POINT ( 'NONE',  ( 10.82674528040999995, 3.167160000746000126, -6.225151413000000744 ) ) ;
#51982 = ORIENTED_EDGE ( 'NONE', *, *, #9709, .T. ) ;
#51983 = EDGE_CURVE ( 'NONE', #50721, #44355, #16808, .T. ) ;
#51984 = CARTESIAN_POINT ( 'NONE',  ( 11.57273594314529142, -2.871094011463778184, 7.824979517142727659 ) ) ;
#51985 = CARTESIAN_POINT ( 'NONE',  ( 17.74460677683594767, -3.176355914694789284, 12.19306589750932623 ) ) ;
#51986 = CARTESIAN_POINT ( 'NONE',  ( 10.76426088462129904, 4.002719309691810778, 8.778009775371000245 ) ) ;
#51987 = DIRECTION ( 'NONE',  ( -3.936133611084978447E-08, 0.7071067676227968946, -0.7071067947502968076 ) ) ;
#51988 = CARTESIAN_POINT ( 'NONE',  ( 7.911791375976998886, 3.505433841991000499, 6.324291089890995643 ) ) ;
#51989 = EDGE_LOOP ( 'NONE', ( #43254, #43943, #29666, #66758, #37724 ) ) ;
#51990 = DIRECTION ( 'NONE',  ( 1.000000000000000000, 0.000000000000000000, 0.000000000000000000 ) ) ;
#51991 = ADVANCED_FACE ( 'NONE', ( #14768, #36085 ), #45561, .T. ) ;
#51992 = EDGE_CURVE ( 'NONE', #26661, #46967, #67545, .T. ) ;
#51993 = CARTESIAN_POINT ( 'NONE',  ( 7.666339158767000228, 3.406663518590999917, -5.695144508491999602 ) ) ;
#51994 = CARTESIAN_POINT ( 'NONE',  ( 8.128451618207334306, -5.085822230759275087, 6.140894674361986993 ) ) ;
#51995 = AXIS2_PLACEMENT_3D ( 'NONE', #12233, #48947, #54180 ) ;
#51996 = CARTESIAN_POINT ( 'NONE',  ( 9.271455549953000030, -3.111370763671500228, 8.216988513669100769 ) ) ;
#51997 = ORIENTED_EDGE ( 'NONE', *, *, #15801, .T. ) ;
#51998 = CARTESIAN_POINT ( 'NONE',  ( 9.299999999999998934, -4.537600397704999899, 9.154563893594000135 ) ) ;
#51999 = CARTESIAN_POINT ( 'NONE',  ( 11.59999999999999964, -4.000000000000000000, -7.500000000000000000 ) ) ;
#52000 = ORIENTED_EDGE ( 'NONE', *, *, #50668, .F. ) ;
#52001 = CARTESIAN_POINT ( 'NONE',  ( 10.00851354018233152, -4.163624617374471093, 6.250000000000000888 ) ) ;
#52002 = AXIS2_PLACEMENT_3D ( 'NONE', #22139, #821, #59198 ) ;
#52003 = ORIENTED_EDGE ( 'NONE', *, *, #6066, .F. ) ;
#52004 = FACE_OUTER_BOUND ( 'NONE', #16408, .T. ) ;
#52005 = CARTESIAN_POINT ( 'NONE',  ( 8.696135841231001251, 3.038023536984999939, -5.861661709981000001 ) ) ;
#52006 = CARTESIAN_POINT ( 'NONE',  ( 11.30878751119029957, 2.958974835389999836, -8.044634158732998586 ) ) ;
#52007 = CARTESIAN_POINT ( 'NONE',  ( 11.01414141025500015, -3.384226587288500010, 6.403245959303999868 ) ) ;
#52008 = CARTESIAN_POINT ( 'NONE',  ( 12.33224723617686891, 2.090732662878786563, -12.53759506087954456 ) ) ;
#52009 = CARTESIAN_POINT ( 'NONE',  ( 12.02733460557258915, -3.793662715184400014, 6.238754009183999472 ) ) ;
#52010 = CARTESIAN_POINT ( 'NONE',  ( 7.603420280409000753, 5.687206835507000235, 6.847268999608999707 ) ) ;
#52011 = EDGE_CURVE ( 'NONE', #28416, #18264, #48878, .T. ) ;
#52012 = VERTEX_POINT ( 'NONE', #25247 ) ;
#52013 = CARTESIAN_POINT ( 'NONE',  ( 9.479346873516668381, 4.163624617374466652, -8.749999999999998224 ) ) ;
#52014 = CIRCLE ( 'NONE', #21873, 13.98989063587000281 ) ;
#52015 = CARTESIAN_POINT ( 'NONE',  ( 17.64998052282863839, -0.7146386402724677067, 12.57972080578535312 ) ) ;
#52016 = CARTESIAN_POINT ( 'NONE',  ( 9.896013540183126622, 3.000416447002273834, 6.731816600031358178 ) ) ;
#52017 = VERTEX_POINT ( 'NONE', #61973 ) ;
#52018 = CARTESIAN_POINT ( 'NONE',  ( 12.72250989631414164, -3.119868145445779728, -12.28529260172211224 ) ) ;
#52020 = CARTESIAN_POINT ( 'NONE',  ( 10.49764694612699856, 2.940513484064000149, 7.077178005756699974 ) ) ;
#52019 = AXIS2_PLACEMENT_3D ( 'NONE', #64228, #53414, #4816 ) ;
#52021 = CARTESIAN_POINT ( 'NONE',  ( 9.991527686541001430, -4.805948463426999773, -8.932428271061001013 ) ) ;
#52022 = LINE ( 'NONE', #4123, #43325 ) ;
#52023 = CARTESIAN_POINT ( 'NONE',  ( 18.35309301929700254, -2.844470671424999875, -12.04740840676999802 ) ) ;
#52024 = CARTESIAN_POINT ( 'NONE',  ( 21.59999987243000064, 13.89999852641999922, 0.000000000000000000 ) ) ;
#52025 = CARTESIAN_POINT ( 'NONE',  ( 12.80505043854146940, -1.875000000000000444, -13.78627172894481667 ) ) ;
#52026 = CARTESIAN_POINT ( 'NONE',  ( 11.36333594839950045, -3.340240242524600056, -6.743912759487099784 ) ) ;
#52027 = DIRECTION ( 'NONE',  ( 0.000000000000000000, -0.9905022095861402143, 0.1374968101629056305 ) ) ;
#52028 = CARTESIAN_POINT ( 'NONE',  ( 9.356851002546999752, 2.832432432432000269, -6.822293592207000934 ) ) ;
#52029 = VERTEX_POINT ( 'NONE', #9505 ) ;
#52030 = EDGE_LOOP ( 'NONE', ( #26065, #6866, #63749, #48518 ) ) ;
#52031 = CARTESIAN_POINT ( 'NONE',  ( 12.35923975629391514, -0.5837697427702301933, -13.98798827747872053 ) ) ;
#52032 = DIRECTION ( 'NONE',  ( 0.000000000000000000, -0.1218274111675001214, 0.9925512993736016476 ) ) ;
#52033 = CARTESIAN_POINT ( 'NONE',  ( 18.03215848269747568, 2.904634633594406434, 13.57923905310747337 ) ) ;
#52034 = CARTESIAN_POINT ( 'NONE',  ( 10.89218604104999955, 2.661903984162000469, -8.236033286991000679 ) ) ;
#52035 = CARTESIAN_POINT ( 'NONE',  ( 8.695634021592812957, 5.082571230934349593, 6.279975830437711792 ) ) ;
#52036 = EDGE_CURVE ( 'NONE', #38268, #28175, #29349, .T. ) ;
#52037 = CARTESIAN_POINT ( 'NONE',  ( 18.15975285618098312, 2.341680162859185010, 12.48703895936063013 ) ) ;
#52038 = CARTESIAN_POINT ( 'NONE',  ( 23.61990947728800094, -13.19621614317000002, 4.178973957053000454 ) ) ;
#52039 = CARTESIAN_POINT ( 'NONE',  ( 9.199602729599000384, 2.551394566582000145, 7.536605852160000119 ) ) ;
#52040 = VERTEX_POINT ( 'NONE', #19668 ) ;
#52041 = ADVANCED_FACE ( 'NONE', ( #30847 ), #56652, .F. ) ;
#52042 = DIRECTION ( 'NONE',  ( 0.000000000000000000, 0.000000000000000000, -1.000000000000000000 ) ) ;
#52043 = VERTEX_POINT ( 'NONE', #57745 ) ;
#52044 = CARTESIAN_POINT ( 'NONE',  ( 12.66109513597121605, -3.108543426238435714, 12.28874474902926650 ) ) ;
#52045 = CARTESIAN_POINT ( 'NONE',  ( 13.50007192468515704, 9.074936576711696290, 7.617865797329646860 ) ) ;
#52046 = CARTESIAN_POINT ( 'NONE',  ( 10.39106065309000115, 4.025321035224999733, 9.261125884460000179 ) ) ;
#52047 = CARTESIAN_POINT ( 'NONE',  ( 12.17403632436368888, -4.976178716761900489, 7.727966254184200245 ) ) ;
#52048 = CARTESIAN_POINT ( 'NONE',  ( 7.167854234552727632, 1.232145303795026292, 0.2729883214974913597 ) ) ;
#52049 = CARTESIAN_POINT ( 'NONE',  ( 10.96245927184000024, 7.417218077776000840, -6.111351059656000118 ) ) ;
#52050 = CARTESIAN_POINT ( 'NONE',  ( 10.73964560330029983, 4.391636236366600166, -6.283473206644000442 ) ) ;
#52051 = CARTESIAN_POINT ( 'NONE',  ( 10.96233853605644093, 4.057274665987934625, -9.264935003284213266 ) ) ;
#52052 = VECTOR ( 'NONE', #12489, 1000.000000000000000 ) ;
#52053 = CARTESIAN_POINT ( 'NONE',  ( 5.606877745312729644, -12.12699005521680817, -3.748526802952889980 ) ) ;
#52054 = CARTESIAN_POINT ( 'NONE',  ( 10.96580581817999978, 4.930645553951000792, 6.170542400361000546 ) ) ;
#52055 = CARTESIAN_POINT ( 'NONE',  ( 9.218906055667105193, -2.654017316073122856, 7.603682184084918028 ) ) ;
#52056 = ORIENTED_EDGE ( 'NONE', *, *, #11389, .F. ) ;
#52057 = CARTESIAN_POINT ( 'NONE',  ( 8.979720280412999855, 5.524776413195999325, -7.147585171405999915 ) ) ;
#52058 = CARTESIAN_POINT ( 'NONE',  ( 23.60000000000000142, -2.548720605937000006, -12.21654710926000220 ) ) ;
#52059 = CARTESIAN_POINT ( 'NONE',  ( 3.800000448357999883, 0.000000000000000000, 0.000000000000000000 ) ) ;
#52060 = CARTESIAN_POINT ( 'NONE',  ( 10.33351354018233081, 2.750000000000000000, 7.663624617374469317 ) ) ;
#52061 = CARTESIAN_POINT ( 'NONE',  ( 10.91079984269360637, 5.053022793955669556, 4.907707240338313071 ) ) ;
#52062 = CARTESIAN_POINT ( 'NONE',  ( 10.42795525820099911, -4.094749303624469761, -6.501013802764199490 ) ) ;
#52063 = ORIENTED_EDGE ( 'NONE', *, *, #2319, .T. ) ;
#52064 = AXIS2_PLACEMENT_3D ( 'NONE', #3796, #40869, #4480 ) ;
#52065 = B_SPLINE_CURVE_WITH_KNOTS ( 'NONE', 3,
 ( #26384, #27071, #38236, #16907 ),
 .UNSPECIFIED., .F., .F.,
 ( 4, 4 ),
 ( 0.000000000000000000, 1.000000000000000000 ),
 .UNSPECIFIED. ) ;
#52066 = CARTESIAN_POINT ( 'NONE',  ( 1.725064665911000050, -3.060375075103999976, 2.182311086106999642 ) ) ;
#52067 = CARTESIAN_POINT ( 'NONE',  ( 7.330281674562000305, 4.426928431836000044, 9.293321981113999541 ) ) ;
#52070 = CARTESIAN_POINT ( 'NONE',  ( 11.35564217374000329, 3.878722322503999731, -11.75620894677000017 ) ) ;
#52069 = CARTESIAN_POINT ( 'NONE',  ( 9.629471092178999214, 5.100000000000000533, 6.152188490330000370 ) ) ;
#52068 = PRODUCT_DEFINITION_CONTEXT ( 'detailed design', #305, 'design' ) ;
#52071 = DIRECTION ( 'NONE',  ( 1.000000000000000000, 0.000000000000000000, 0.000000000000000000 ) ) ;
#52072 = ORIENTED_EDGE ( 'NONE', *, *, #28097, .F. ) ;
#52073 = CYLINDRICAL_SURFACE ( 'NONE', #33926, 1.250000000000000222 ) ;
#52074 = CARTESIAN_POINT ( 'NONE',  ( 18.15125141007965226, -2.312191647150520613, -13.71145324559126877 ) ) ;
#52075 = CARTESIAN_POINT ( 'NONE',  ( 11.58902763632552002, 3.213494089586499847, 7.862914650060299770 ) ) ;
#52076 = DIRECTION ( 'NONE',  ( 0.000000000000000000, 0.8648648648648720183, 0.5020047465136825426 ) ) ;
#52077 = CARTESIAN_POINT ( 'NONE',  ( 9.234504440379000201, -5.964711531933999389, 7.776478361891000723 ) ) ;
#52078 = VERTEX_POINT ( 'NONE', #15790 ) ;
#52079 = CARTESIAN_POINT ( 'NONE',  ( 8.481676658773000810, 2.472348777564000066, 6.234194744024999402 ) ) ;
#52080 = EDGE_CURVE ( 'NONE', #19987, #4, #63675, .T. ) ;
#52081 = EDGE_CURVE ( 'NONE', #64580, #30607, #35156, .T. ) ;
#52083 = CARTESIAN_POINT ( 'NONE',  ( 10.90000000000000036, 0.2500000000000000000, 9.776630298829998011 ) ) ;
#52082 = CARTESIAN_POINT ( 'NONE',  ( 10.62452888361057113, 3.128042445605609512, -7.561478660064198110 ) ) ;
#52084 = CARTESIAN_POINT ( 'NONE',  ( 7.645530094557493328, -5.359336832227764802, 6.415087437494591427 ) ) ;
#52085 = CARTESIAN_POINT ( 'NONE',  ( 18.14736049945578245, -0.1997550941145084524, 13.89807248760369518 ) ) ;
#52086 = CARTESIAN_POINT ( 'NONE',  ( 0.9755632220631000884, -1.955279592509000075, 2.607329530612999768 ) ) ;
#52087 = ORIENTED_EDGE ( 'NONE', *, *, #40963, .T. ) ;
#52088 = CARTESIAN_POINT ( 'NONE',  ( 1.715504496333042583, 2.382347238673330203, -2.287553813110801748 ) ) ;
#52089 = CARTESIAN_POINT ( 'NONE',  ( 11.00595525820100029, -4.081787880721680750, 8.362327856951900173 ) ) ;
#52090 = CARTESIAN_POINT ( 'NONE',  ( 10.21609109105999913, 5.961715741921000067, 7.319666990313999477 ) ) ;
#52091 = CARTESIAN_POINT ( 'NONE',  ( 10.14750576281000072, 2.602962605360999770, 6.738577830910999822 ) ) ;
#52092 = CARTESIAN_POINT ( 'NONE',  ( 10.76841504065829902, 4.914510326623699576, 8.181880472491098288 ) ) ;
#52093 = CARTESIAN_POINT ( 'NONE',  ( 24.30000000000000071, -9.517611874540000017, 8.103398312166998352 ) ) ;
#52094 = DIRECTION ( 'NONE',  ( 0.000000000000000000, 0.000000000000000000, -1.000000000000000000 ) ) ;
#52095 = FACE_OUTER_BOUND ( 'NONE', #61136, .T. ) ;
#52096 = EDGE_CURVE ( 'NONE', #46284, #48412, #13492, .T. ) ;
#52097 = CARTESIAN_POINT ( 'NONE',  ( 9.975298369746534277, -5.350379160513648813, 7.499985214262776978 ) ) ;
#52098 = VECTOR ( 'NONE', #29952, 1000.000000000000000 ) ;
#52099 = CARTESIAN_POINT ( 'NONE',  ( 24.51039984485900192, -12.36383375972000209, -3.075091620974999884 ) ) ;
#52100 = CARTESIAN_POINT ( 'NONE',  ( 11.61486084871780022, -2.792989229543000107, 7.825000000000000178 ) ) ;
#52101 = ORIENTED_EDGE ( 'NONE', *, *, #1524, .F. ) ;
#52102 = CARTESIAN_POINT ( 'NONE',  ( 8.709622771139999386, -5.146410603519000482, -6.783155613812000162 ) ) ;
#52103 = EDGE_CURVE ( 'NONE', #11762, #62789, #57798, .T. ) ;
#52104 = CARTESIAN_POINT ( 'NONE',  ( 11.40010796094000334, 0.000000000000000000, -5.373479439185999994E-14 ) ) ;
#52105 = EDGE_LOOP ( 'NONE', ( #36826, #66398, #10469, #25785, #21982 ) ) ;
#52106 = FILL_AREA_STYLE_COLOUR ( '', #30482 ) ;
#52107 = CARTESIAN_POINT ( 'NONE',  ( 11.73671932425159881, 3.872987101045399783, 6.643164954553199664 ) ) ;
#52108 = CIRCLE ( 'NONE', #66635, 2.000000000000000444 ) ;
#52109 = CARTESIAN_POINT ( 'NONE',  ( 9.724611353170001138, 2.928305163963000446, 8.718478150869000132 ) ) ;
#52110 = CARTESIAN_POINT ( 'NONE',  ( 10.49937419337999955, 2.985313722448000195, -6.358656051156999389 ) ) ;
#52111 = CARTESIAN_POINT ( 'NONE',  ( 9.632166486775625813, -4.862862160676565182, -7.644917771834661480 ) ) ;
#52112 = CARTESIAN_POINT ( 'NONE',  ( 9.646285452541999206, -2.591464128784999765, 6.760053199270999791 ) ) ;
#52113 = CARTESIAN_POINT ( 'NONE',  ( 18.23387849499156133, -0.2528603812084161406, -12.59746735456353051 ) ) ;
#52114 = CARTESIAN_POINT ( 'NONE',  ( 9.061840824070779732, 4.635339463665918203, 8.712817598784141637 ) ) ;
#52115 = CARTESIAN_POINT ( 'NONE',  ( 11.26902897915239876, -3.778278678798900447, -8.337339982364900592 ) ) ;
#52116 = CARTESIAN_POINT ( 'NONE',  ( 7.159807156518384730, -0.4668129303315028400, 1.167714605286940488 ) ) ;
#52117 = ORIENTED_EDGE ( 'NONE', *, *, #52522, .T. ) ;
#52118 = AXIS2_PLACEMENT_3D ( 'NONE', #61036, #50206, #65923 ) ;
#52119 = CARTESIAN_POINT ( 'NONE',  ( 11.12486982654999856, -6.581651479209999600, -5.643180424050000532 ) ) ;
#52120 = CARTESIAN_POINT ( 'NONE',  ( 24.95270871331634410, -2.977372476727536466, 11.59851889212190024 ) ) ;
#52121 = CARTESIAN_POINT ( 'NONE',  ( 24.67921321731900264, -3.567517257907000250, -12.13750614118000115 ) ) ;
#52122 = CARTESIAN_POINT ( 'NONE',  ( 8.524970964081628466, 2.900000000000001688, -6.445556248366430374 ) ) ;
#52123 = CARTESIAN_POINT ( 'NONE',  ( 7.254703680423997270, 9.104289213269002090, 5.358377883862995184 ) ) ;
#52124 = CARTESIAN_POINT ( 'NONE',  ( 12.38020518697565286, 1.926193139504584373, 13.86686096623706810 ) ) ;
#52125 = CARTESIAN_POINT ( 'NONE',  ( 9.465112865370999273, -2.290047720994000002, 6.601709978349000529 ) ) ;
#52126 = VERTEX_POINT ( 'NONE', #47615 ) ;
#52127 = CIRCLE ( 'NONE', #6358, 0.3000000000000000444 ) ;
#52128 = ADVANCED_FACE ( 'NONE', ( #63325 ), #31200, .T. ) ;
#52129 = CARTESIAN_POINT ( 'NONE',  ( 9.246653663635285625, -2.697134473482441841, 7.146693063513369637 ) ) ;
#52130 = CARTESIAN_POINT ( 'NONE',  ( 12.08123665194308138, -0.04806343339258901948, 13.99993753789458850 ) ) ;
#52131 = ORIENTED_EDGE ( 'NONE', *, *, #32364, .T. ) ;
#52132 = CARTESIAN_POINT ( 'NONE',  ( 12.18657262959521326, -2.104614846739868206, 12.42298765743896816 ) ) ;
#52133 = CARTESIAN_POINT ( 'NONE',  ( 10.57314899745999881, -5.167567567567999731, -6.822293592207000934 ) ) ;
#52134 = CARTESIAN_POINT ( 'NONE',  ( 9.538434317036999843, -5.620900626097999897, 7.423100105894999245 ) ) ;
#52135 = DIRECTION ( 'NONE',  ( 0.000000000000000000, 1.000000000000000000, 0.000000000000000000 ) ) ;
#52136 = CARTESIAN_POINT ( 'NONE',  ( 11.62133729122639991, -4.865898216891100247, 7.522778681411049995 ) ) ;
#52137 = CARTESIAN_POINT ( 'NONE',  ( 9.332537864288001472, 2.899999999999999911, 6.571291218949999902 ) ) ;
#52138 = CARTESIAN_POINT ( 'NONE',  ( 0.6062974075931000240, 0.9423624982842000453, -3.239329654985999785 ) ) ;
#52139 = LINE ( 'NONE', #24892, #25933 ) ;
#52140 = CARTESIAN_POINT ( 'NONE',  ( 12.13061620557590992, 2.744764576889032970, 12.29741386912397338 ) ) ;
#52141 = CARTESIAN_POINT ( 'NONE',  ( 10.11094409420000062, -5.100000000000000533, -6.571291218949999902 ) ) ;
#52142 = CARTESIAN_POINT ( 'NONE',  ( 10.32949413291699869, 4.912929163218899831, -7.083453279150199400 ) ) ;
#52143 = LINE ( 'NONE', #62300, #32503 ) ;
#52144 = B_SPLINE_CURVE_WITH_KNOTS ( 'NONE', 3,
 ( #31899, #53212, #26655, #47972, #37472, #21391, #64029, #58800, #5651, #69, #26992, #48308, #415, #43422, #65417, #35009, #13342, #39208 ),
 .UNSPECIFIED., .F., .F.,
 ( 4, 2, 2, 2, 2, 2, 2, 2, 4 ),
 ( 0.000000000000000000, 0.1250000000000000000, 0.2500000000000000000, 0.3750000000000000000, 0.5000000000000000000, 0.6250000000000000000, 0.7500000000000000000, 0.8750000000000000000, 1.000000000000000000 ),
 .UNSPECIFIED. ) ;
#52145 = CARTESIAN_POINT ( 'NONE',  ( 11.11477971959000044, 2.548217283716999848, -8.356742414746999970 ) ) ;
#52146 = CARTESIAN_POINT ( 'NONE',  ( 9.377342523874999003, 2.735516931877000513, -7.306436165809000016 ) ) ;
#52148 = FACE_OUTER_BOUND ( 'NONE', #30121, .T. ) ;
#52147 = DIRECTION ( 'NONE',  ( -1.000000000000000000, 0.000000000000000000, 0.000000000000000000 ) ) ;
#52149 = CARTESIAN_POINT ( 'NONE',  ( 8.819055905797000605, 2.899999999999999911, -6.571291218949999902 ) ) ;
#52150 = VERTEX_POINT ( 'NONE', #68572 ) ;
#52151 = B_SPLINE_CURVE_WITH_KNOTS ( 'NONE', 3,
 ( #68971, #52897, #22103, #42749, #42411, #43788, #64743, #65085, #58482, #17207, #16857, #10586, #31924, #43092, #4995, #53237, #5337, #26682 ),
 .UNSPECIFIED., .F., .F.,
 ( 4, 2, 2, 2, 2, 2, 2, 2, 4 ),
 ( 0.000000000000000000, 0.1250000000000000000, 0.2500000000000000000, 0.3750000000000000000, 0.5000000000000000000, 0.6250000000000000000, 0.7500000000000000000, 0.8750000000000000000, 1.000000000000000000 ),
 .UNSPECIFIED. ) ;
#52152 = DIRECTION ( 'NONE',  ( 1.000000000000000000, 0.000000000000000000, 0.000000000000000000 ) ) ;
#52153 = CARTESIAN_POINT ( 'NONE',  ( 10.32101354018304207, 3.231816600031359510, 8.499583552997727054 ) ) ;
#52154 =( GEOMETRIC_REPRESENTATION_CONTEXT ( 3 ) GLOBAL_UNCERTAINTY_ASSIGNED_CONTEXT ( ( #66520 ) ) GLOBAL_UNIT_ASSIGNED_CONTEXT ( ( #11964, #43447, #53238 ) ) REPRESENTATION_CONTEXT ( 'NONE', 'WORKASPACE' ) );
#52155 = CARTESIAN_POINT ( 'NONE',  ( 11.50000000000000000, -5.058572498595999889, 7.174999999999999822 ) ) ;
#52156 = CARTESIAN_POINT ( 'NONE',  ( 9.627671671056999614, 3.144964309357700216, 7.356396684460199786 ) ) ;
#52157 = CARTESIAN_POINT ( 'NONE',  ( 9.328216720588626387, 4.762939826712631941, -7.928316576537355331 ) ) ;
#52158 = CARTESIAN_POINT ( 'NONE',  ( 11.49999144015000319, 3.886253129992999877, -11.90689313971000018 ) ) ;
#52160 = CARTESIAN_POINT ( 'NONE',  ( 12.64218892536046646, -3.103760129324341754, 13.52669845179788943 ) ) ;
#52159 = CIRCLE ( 'NONE', #23119, 7.720759220056002903 ) ;
#52161 = CARTESIAN_POINT ( 'NONE',  ( 23.61661350339327115, -3.308521622829082354, 13.56940557538989545 ) ) ;
#52162 = CARTESIAN_POINT ( 'NONE',  ( 23.55339688456600200, 3.057948053973999603, -13.69581934054999905 ) ) ;
#52163 = ORIENTED_EDGE ( 'NONE', *, *, #41655, .F. ) ;
#52164 = EDGE_CURVE ( 'NONE', #18264, #16502, #47269, .T. ) ;
#52165 = ADVANCED_FACE ( 'NONE', ( #31534 ), #15455, .T. ) ;
#52166 = CARTESIAN_POINT ( 'NONE',  ( 4.319063347543000475, -1.132153191583000096, 0.07165796951064999643 ) ) ;
#52167 = CARTESIAN_POINT ( 'NONE',  ( 9.833267173155999075, -4.973628086880700572, -6.670281532133299329 ) ) ;
#52168 = VECTOR ( 'NONE', #17428, 1000.000000000000000 ) ;
#52169 = ADVANCED_FACE ( 'NONE', ( #68925 ), #45543, .F. ) ;
#52170 = CARTESIAN_POINT ( 'NONE',  ( 10.49914019022526901, -4.925950642208848151, -4.998102050154486165 ) ) ;
#52171 = CARTESIAN_POINT ( 'NONE',  ( 11.44501463001509833, -3.527519786474400121, 8.256737112932800216 ) ) ;
#52172 = CARTESIAN_POINT ( 'NONE',  ( 17.80580762821592344, 3.072583274995464464, -12.29955455495395711 ) ) ;
#52173 = CARTESIAN_POINT ( 'NONE',  ( 2.573890132542666187, 2.150913519912194705, 2.798833948393636639 ) ) ;
#52174 = CARTESIAN_POINT ( 'NONE',  ( 18.13957898666327750, 2.721486385479426229, 12.39720401453807419 ) ) ;
#52176 = CIRCLE ( 'NONE', #37704, 0.9999997023190999590 ) ;
#52175 = CARTESIAN_POINT ( 'NONE',  ( 12.20205663599317703, 2.664445668530659006, -13.63720455689867350 ) ) ;
#52177 = CARTESIAN_POINT ( 'NONE',  ( 12.79999999975700042, -11.86189249994999884, 3.298671769835999967 ) ) ;
#52178 = CARTESIAN_POINT ( 'NONE',  ( 10.72129555961999792, -4.673507771948999689, -5.778404201896999659 ) ) ;
#52179 = DIRECTION ( 'NONE',  ( 0.000000000000000000, 0.000000000000000000, -1.000000000000000000 ) ) ;
#52180 = CARTESIAN_POINT ( 'NONE',  ( 12.38296256657291039, 0.5938246120522370219, -13.98740230410798091 ) ) ;
#52181 = CARTESIAN_POINT ( 'NONE',  ( 13.60249209530700121, -8.943624754334001281, -7.827978252961999672 ) ) ;
#52182 = CARTESIAN_POINT ( 'NONE',  ( 8.287602349183067929, -2.892084057926692431, 6.689538224764139507 ) ) ;
#52183 = CARTESIAN_POINT ( 'NONE',  ( 2.967640132544666631, 1.762666431298152148, -3.058252359239900908 ) ) ;
#52184 = EDGE_CURVE ( 'NONE', #5164, #1057, #63488, .T. ) ;
#52185 = CARTESIAN_POINT ( 'NONE',  ( 8.912754719595000097, 2.481540185810000132, -7.878707153279001396 ) ) ;
#52186 = CARTESIAN_POINT ( 'NONE',  ( 6.713407900711241716, 0.6189880680375690059, -1.392846009744216573 ) ) ;
#52187 = EDGE_LOOP ( 'NONE', ( #17316, #58202, #67299, #29828 ) ) ;
#52188 = CARTESIAN_POINT ( 'NONE',  ( 13.63045347340495539, 12.32568024774173310, 2.226002549926721308 ) ) ;
#52189 = CARTESIAN_POINT ( 'NONE',  ( 18.21736474454386823, 2.220153890850322664, -13.82285830752081068 ) ) ;
#52190 = ORIENTED_EDGE ( 'NONE', *, *, #66523, .T. ) ;
#52191 = ADVANCED_FACE ( 'NONE', ( #21436 ), #57814, .F. ) ;
#52192 = CARTESIAN_POINT ( 'NONE',  ( 8.632946129846658323, 2.796778970782894724, 8.203843119991381272 ) ) ;
#52193 = CARTESIAN_POINT ( 'NONE',  ( 11.64122412107036908, 4.062069863985690255, 8.673243607771999208 ) ) ;
#52194 = CARTESIAN_POINT ( 'NONE',  ( 4.149992563292001613, -0.5234817089163702475, -1.947893036340041517 ) ) ;
#52195 = CARTESIAN_POINT ( 'NONE',  ( 17.80000000009400196, 3.216307036143000175, -11.40341376487999980 ) ) ;
#52196 = CARTESIAN_POINT ( 'NONE',  ( 0.2500098862125000321, 0.000000000000000000, 0.000000000000000000 ) ) ;
#52197 = CARTESIAN_POINT ( 'NONE',  ( 11.60000000000000142, -3.133991299512490336, -6.727195615969564280 ) ) ;
#52198 = CARTESIAN_POINT ( 'NONE',  ( 8.856495485442710702, -3.650546589001255171, -8.453238005838597857 ) ) ;
#52199 = VERTEX_POINT ( 'NONE', #58502 ) ;
#52200 = CARTESIAN_POINT ( 'NONE',  ( 13.89309513285500230, 9.135233488911998379, 8.214486393748998694 ) ) ;
#52201 = CARTESIAN_POINT ( 'NONE',  ( 9.427245280414000561, 4.989193221215000307, -6.287302145481000082 ) ) ;
#52202 = VERTEX_POINT ( 'NONE', #46992 ) ;
#52203 = AXIS2_PLACEMENT_3D ( 'NONE', #45233, #7126, #55370 ) ;
#52204 = CARTESIAN_POINT ( 'NONE',  ( 9.792312867577999569, 4.284154069364999984, -9.000485152170000447 ) ) ;
#52205 = ORIENTED_EDGE ( 'NONE', *, *, #55168, .T. ) ;
#52206 = CARTESIAN_POINT ( 'NONE',  ( 9.048063610504998522, 4.524705472883399970, 6.333351572150998976 ) ) ;
#52207 = CARTESIAN_POINT ( 'NONE',  ( 18.07135403277173324, -2.147634186626016017, -12.52670565379013112 ) ) ;
#52208 = CARTESIAN_POINT ( 'NONE',  ( 11.44750515593000095, -11.62256912479000093, -1.379235499629000161 ) ) ;
#52209 = CIRCLE ( 'NONE', #34367, 1.649999999999999911 ) ;
#52210 = CARTESIAN_POINT ( 'NONE',  ( 24.51327040776200050, -12.11106229541000090, -3.153269560843000363 ) ) ;
#52211 = CARTESIAN_POINT ( 'NONE',  ( 24.30000000000000071, -3.224868684338999980, 12.03537377768999939 ) ) ;
#52212 = ORIENTED_EDGE ( 'NONE', *, *, #40024, .T. ) ;
#52213 = CARTESIAN_POINT ( 'NONE',  ( 12.52995381683800247, 11.92229088141000126, -3.300664210127000064 ) ) ;
#52214 = DIRECTION ( 'NONE',  ( 0.000000000000000000, -0.8897496663235402448, 0.4564488265700210046 ) ) ;
#52215 = CARTESIAN_POINT ( 'NONE',  ( 8.039443364739078390, -4.176885327615397436, 8.849067469250744722 ) ) ;
#52216 = AXIS2_PLACEMENT_3D ( 'NONE', #43137, #59212, #48734 ) ;
#52217 = CYLINDRICAL_SURFACE ( 'NONE', #49486, 1.350000000000000533 ) ;
#52218 = CARTESIAN_POINT ( 'NONE',  ( 18.26375728754768701, 0.1544074001203936397, 13.99915345895492180 ) ) ;
#52219 = CARTESIAN_POINT ( 'NONE',  ( 17.79421883851900077, 3.253172350820999981, 11.33701189166999868 ) ) ;
#52220 = CARTESIAN_POINT ( 'NONE',  ( 10.65650106607000147, -5.448187878199999723, -7.015213573792999036 ) ) ;
#52221 = ADVANCED_FACE ( 'NONE', ( #26354 ), #36845, .T. ) ;
#52222 = ORIENTED_EDGE ( 'NONE', *, *, #22330, .F. ) ;
#52223 = VERTEX_POINT ( 'NONE', #26702 ) ;
#52224 = AXIS2_PLACEMENT_3D ( 'NONE', #4043, #30298, #36218 ) ;
#52225 = CARTESIAN_POINT ( 'NONE',  ( 9.269210841233000764, 3.098073081301000009, -8.567513114264999174 ) ) ;
#52226 = CARTESIAN_POINT ( 'NONE',  ( 10.58728840301827923, 2.899999999999999911, -6.305985889763610963 ) ) ;
#52227 = DIRECTION ( 'NONE',  ( 0.000000000000000000, 4.343333852296999816E-12, -1.000000000000000000 ) ) ;
#52228 = CARTESIAN_POINT ( 'NONE',  ( 25.29571535093799994, 8.389559371064001070, -8.302794996009000172 ) ) ;
#52229 = CARTESIAN_POINT ( 'NONE',  ( 10.80502344389999791, 2.874741265256000489, -6.817099149379099110 ) ) ;
#52230 = CARTESIAN_POINT ( 'NONE',  ( 9.991279731608999626, 4.077800926195140008, -6.636486849903699969 ) ) ;
#52232 = CARTESIAN_POINT ( 'NONE',  ( 2.210247277619000084, 2.108360286353999413, -2.286637680308000409 ) ) ;
#52231 = CARTESIAN_POINT ( 'NONE',  ( 9.371822372493999964, -4.328199826929600036, 6.426348619097999482 ) ) ;
#52233 = CARTESIAN_POINT ( 'NONE',  ( 7.782975328289005290, -3.196931270636999667, 6.293200827887002191 ) ) ;
#52234 = ORIENTED_EDGE ( 'NONE', *, *, #29481, .T. ) ;
#52235 = CARTESIAN_POINT ( 'NONE',  ( 9.664763540182335078, 5.217465845835396188, -7.172815144550905408 ) ) ;
#52236 = CARTESIAN_POINT ( 'NONE',  ( 8.149001627428001271, -3.121156835630000348, 6.130053226229998486 ) ) ;
#52237 = CARTESIAN_POINT ( 'NONE',  ( 10.44424205625099944, 3.541248877825399877, 6.305876158747000026 ) ) ;
#52238 = CARTESIAN_POINT ( 'NONE',  ( 12.80505043854143388, 3.124999999999999556, 13.52078605991414939 ) ) ;
#52239 = B_SPLINE_CURVE_WITH_KNOTS ( 'NONE', 3,
 ( #38727, #28594, #55149, #27902 ),
 .UNSPECIFIED., .F., .F.,
 ( 4, 4 ),
 ( 0.000000000000000000, 1.000000000000000000 ),
 .UNSPECIFIED. ) ;
#52240 = CARTESIAN_POINT ( 'NONE',  ( 4.900006121741999010, 2.000000000000000000, 0.000000000000000000 ) ) ;
#52241 = CARTESIAN_POINT ( 'NONE',  ( 17.59622528265708041, 3.124999999999999112, -12.28374666422326555 ) ) ;
#52242 = CARTESIAN_POINT ( 'NONE',  ( 10.01721296880961631, 5.205658458020796964, 8.206277775804023733 ) ) ;
#52243 = AXIS2_PLACEMENT_3D ( 'NONE', #6706, #54956, #7058 ) ;
#52244 = EDGE_CURVE ( 'NONE', #62424, #24059, #65226, .T. ) ;
#52245 = ADVANCED_FACE ( 'NONE', ( #14829 ), #9571, .T. ) ;
#52246 = FACE_OUTER_BOUND ( 'NONE', #67997, .T. ) ;
#52247 = CARTESIAN_POINT ( 'NONE',  ( 8.244326721667006197, -4.955553483043997787, 6.175174249266997428 ) ) ;
#52248 = B_SPLINE_CURVE_WITH_KNOTS ( 'NONE', 3,
 ( #31395, #4806, #4115, #47131 ),
 .UNSPECIFIED., .F., .F.,
 ( 4, 4 ),
 ( 0.000000000000000000, 0.1254181127249429095 ),
 .UNSPECIFIED. ) ;
#52249 = ADVANCED_FACE ( 'NONE', ( #20413 ), #62708, .T. ) ;
#52250 = CARTESIAN_POINT ( 'NONE',  ( 6.765359675869000000, -0.7428381837956999911, 0.9117187782023999931 ) ) ;
#52251 = CIRCLE ( 'NONE', #14295, 1.500000000000000000 ) ;
#52252 = CARTESIAN_POINT ( 'NONE',  ( 25.46372189163300348, -2.879475976718999686, 11.30953721564000070 ) ) ;
#52253 = CARTESIAN_POINT ( 'NONE',  ( 18.00302879685015967, 3.053770323291399080, 12.22453350001232586 ) ) ;
#52254 = CARTESIAN_POINT ( 'NONE',  ( 3.110247420108000149, -2.350685999463999920, -2.257335140124000272 ) ) ;
#52255 = ORIENTED_EDGE ( 'NONE', *, *, #36615, .F. ) ;
#52256 = CARTESIAN_POINT ( 'NONE',  ( 12.24435292127285635, 0.2761699508452409857, -12.69595998167825357 ) ) ;
#52257 = CARTESIAN_POINT ( 'NONE',  ( 12.22445834447965041, -2.731426566108815734, -12.39462880883199603 ) ) ;
#52258 = FACE_OUTER_BOUND ( 'NONE', #975, .T. ) ;
#52260 = CARTESIAN_POINT ( 'NONE',  ( 24.44496487975900223, 3.224879802562000464, -12.03535984693000138 ) ) ;
#52259 = CIRCLE ( 'NONE', #24425, 0.6999999999999992895 ) ;
#52261 = CARTESIAN_POINT ( 'NONE',  ( 9.214598350284001427, -2.899999999999999911, -6.571291218949999902 ) ) ;
#52262 = ORIENTED_EDGE ( 'NONE', *, *, #21853, .T. ) ;
#52263 = CARTESIAN_POINT ( 'NONE',  ( 10.90000000296000060, 5.100000000009000445, -5.160242730682999657 ) ) ;
#52264 = CARTESIAN_POINT ( 'NONE',  ( 17.97862686867181026, 0.4596875349763956398, 12.68880368814833304 ) ) ;
#52265 = DIRECTION ( 'NONE',  ( -0.7071067811865713315, 0.6115518083850753905, -0.3549709645321856843 ) ) ;
#52266 = CARTESIAN_POINT ( 'NONE',  ( 10.67320712186517362, 2.921171224854686166, 8.329102901498840694 ) ) ;
#52267 = CARTESIAN_POINT ( 'NONE',  ( 10.85168717260509830, 3.386210853237200169, -8.501809683958001074 ) ) ;
#52268 = EDGE_LOOP ( 'NONE', ( #27445, #56186, #67936, #15598, #37743, #63211, #32273, #21158 ) ) ;
#52269 = CARTESIAN_POINT ( 'NONE',  ( 9.332935524889000689, -5.100347267927999972, 8.693464469215999912 ) ) ;
#52270 = ORIENTED_EDGE ( 'NONE', *, *, #4184, .F. ) ;
#52271 = EDGE_CURVE ( 'NONE', #45997, #15587, #30215, .T. ) ;
#52272 = CARTESIAN_POINT ( 'NONE',  ( 11.92394752546313796, -4.702246198360438889, 6.396140797112706444 ) ) ;
#52273 = CARTESIAN_POINT ( 'NONE',  ( 8.122956853208000538, -3.566638198986999964, 5.743608852252999775 ) ) ;
#52274 = CARTESIAN_POINT ( 'NONE',  ( 4.149992563291999836, 4.286198015044692593E-16, -1.999973142472143861 ) ) ;
#52275 = ORIENTED_EDGE ( 'NONE', *, *, #39639, .T. ) ;
#52276 = CARTESIAN_POINT ( 'NONE',  ( 23.60453139207830375, 10.14142216786711259, 9.612068792943430751 ) ) ;
#52277 = FACE_OUTER_BOUND ( 'NONE', #41442, .T. ) ;
#52278 = CIRCLE ( 'NONE', #13222, 0.7499999936418002555 ) ;
#52279 = CARTESIAN_POINT ( 'NONE',  ( 7.771695280404999906, 5.732261791031000087, -7.476053406707000804 ) ) ;
#52280 = CARTESIAN_POINT ( 'NONE',  ( 4.999999999955999641, -1.352284261683000199, -11.01731942327999825 ) ) ;
#52281 = CARTESIAN_POINT ( 'NONE',  ( 8.155831921393041029, -3.033675026350174608, 6.347534157511051767 ) ) ;
#52282 = ORIENTED_EDGE ( 'NONE', *, *, #10392, .T. ) ;
#52283 = FACE_OUTER_BOUND ( 'NONE', #37907, .T. ) ;
#52284 = CARTESIAN_POINT ( 'NONE',  ( 12.17999101424757846, -2.480063841750759668, -13.67763837794374204 ) ) ;
#52285 = FACE_OUTER_BOUND ( 'NONE', #28720, .T. ) ;
#52286 = ORIENTED_EDGE ( 'NONE', *, *, #58665, .F. ) ;
#52287 = CARTESIAN_POINT ( 'NONE',  ( 10.97075054419999951, -2.648517896406999750, -6.788869136079999755 ) ) ;
#52288 = DIRECTION ( 'NONE',  ( 1.000000000000000000, 0.000000000000000000, 0.000000000000000000 ) ) ;
#52289 = ORIENTED_EDGE ( 'NONE', *, *, #35285, .F. ) ;
#52290 = CARTESIAN_POINT ( 'NONE',  ( 23.60224675149267881, -10.14893003115017223, 9.606056460203635794 ) ) ;
#52291 = CARTESIAN_POINT ( 'NONE',  ( 17.71608705221678903, 0.6042412280260501811, -13.88231902342887736 ) ) ;
#52292 = CARTESIAN_POINT ( 'NONE',  ( 17.63732991102260783, -0.6196453797482965875, -12.67964297675818308 ) ) ;
#52293 = DIRECTION ( 'NONE',  ( 1.000000000000000000, 0.000000000000000000, 0.000000000000000000 ) ) ;
#52294 = DIRECTION ( 'NONE',  ( 0.000000000000000000, 0.000000000000000000, -1.000000000000000000 ) ) ;
#52295 = CARTESIAN_POINT ( 'NONE',  ( 7.000000000000000000, 0.2708497377871000311, -3.000000000000000000 ) ) ;
#52296 = CARTESIAN_POINT ( 'NONE',  ( 12.34730967147302039, 2.925678532231710705, 13.57385403034849425 ) ) ;
#52297 = CARTESIAN_POINT ( 'NONE',  ( 17.60707724214346115, -1.877081947552195151, 12.57511531410870020 ) ) ;
#52298 = ORIENTED_EDGE ( 'NONE', *, *, #25835, .T. ) ;
#52299 = CARTESIAN_POINT ( 'NONE',  ( 3.439766623689833658, 0.6157310107295393964, -3.489820053897106700 ) ) ;
#52300 = VERTEX_POINT ( 'NONE', #64078 ) ;
#52301 = CARTESIAN_POINT ( 'NONE',  ( 10.79500540879000070, 3.503955365545999623, 6.168588659884999714 ) ) ;
#52302 = CARTESIAN_POINT ( 'NONE',  ( 11.18114303127866727, -4.620698129841968260, -8.119425260350672247 ) ) ;
#52303 = CARTESIAN_POINT ( 'NONE',  ( 12.23000334607946016, 2.254948878044618521, -13.72238900567161579 ) ) ;
#52304 = CARTESIAN_POINT ( 'NONE',  ( 2.600505918310000109, 2.136089819110000398, 3.030967877105000152 ) ) ;
#52305 = CARTESIAN_POINT ( 'NONE',  ( 7.000000000000000000, 6.255435840762999966, -3.000000000000000000 ) ) ;
#52306 = CARTESIAN_POINT ( 'NONE',  ( 17.55505043854147118, -3.125000000000000000, -25.00000000000000000 ) ) ;
#52307 = AXIS2_PLACEMENT_3D ( 'NONE', #30472, #10173, #62281 ) ;
#52308 = CARTESIAN_POINT ( 'NONE',  ( 18.09811766390441079, 0.3100353841908372599, 13.89536095208713284 ) ) ;
#52309 = EDGE_CURVE ( 'NONE', #23656, #29419, #23507, .T. ) ;
#52310 = EDGE_CURVE ( 'NONE', #13624, #48769, #47682, .T. ) ;
#52311 = B_SPLINE_CURVE_WITH_KNOTS ( 'NONE', 3,
 ( #50238, #56860, #67330, #2342 ),
 .UNSPECIFIED., .F., .F.,
 ( 4, 4 ),
 ( 0.000000000000000000, 1.000000000000000000 ),
 .UNSPECIFIED. ) ;
#52312 = EDGE_LOOP ( 'NONE', ( #6800, #48698, #44409, #58526 ) ) ;
#52313 = CIRCLE ( 'NONE', #69077, 12.42499880353999941 ) ;
#52314 = CARTESIAN_POINT ( 'NONE',  ( 12.47605349747044201, 0.5315089155327396009, 13.88632137824158441 ) ) ;
#52315 = CARTESIAN_POINT ( 'NONE',  ( 11.48579841651039857, -4.449968941611500028, 6.303820944768999901 ) ) ;
#52316 = CARTESIAN_POINT ( 'NONE',  ( 3.155140132544248743, 0.9161175952574702741, 3.408904368339106927 ) ) ;
#52317 = CARTESIAN_POINT ( 'NONE',  ( 15.64816728597000228, 9.503848651356001653, 8.217120907884000403 ) ) ;
#52318 = DIRECTION ( 'NONE',  ( 0.9999999999999997780, 1.340555680669999710E-09, 2.196395946400999623E-08 ) ) ;
#52320 = CARTESIAN_POINT ( 'NONE',  ( 12.35647036339751637, 1.936369888824708285, -13.86561402904834139 ) ) ;
#52319 = CARTESIAN_POINT ( 'NONE',  ( 10.31667774810000004, 3.819530253758000260, 6.062195927068000145 ) ) ;
#52321 = CARTESIAN_POINT ( 'NONE',  ( 11.16225954179439839, 4.877394611789299894, -8.229019074832200076 ) ) ;
#52322 = CARTESIAN_POINT ( 'NONE',  ( 24.98632742932199946, -11.60054869656999976, 3.134150456063999890 ) ) ;
#52323 = CARTESIAN_POINT ( 'NONE',  ( 9.855633995697999694, 4.861719613449499988, -7.595641268826199166 ) ) ;
#52324 = CARTESIAN_POINT ( 'NONE',  ( 17.87637886473324755, 0.6448943924266568040, 12.58348668657565916 ) ) ;
#52325 = CARTESIAN_POINT ( 'NONE',  ( 7.048326796653999970, 0.08385301782618000133, 1.411478992815000000 ) ) ;
#52326 = CARTESIAN_POINT ( 'NONE',  ( 24.30000000000000071, -9.289189189551001036, -7.908916752675001050 ) ) ;
#52327 = CARTESIAN_POINT ( 'NONE',  ( 0.3777305576672876919, 2.683931128707652825, -2.096468434807130077 ) ) ;
#52328 = ORIENTED_EDGE ( 'NONE', *, *, #59302, .T. ) ;
#52329 = CARTESIAN_POINT ( 'NONE',  ( 9.250897313459001126, -4.135077143711000325, 9.175520401071999288 ) ) ;
#52330 = CARTESIAN_POINT ( 'NONE',  ( 17.96944589180082019, 3.117220005880602329, 13.64855254614797886 ) ) ;
#52331 = CARTESIAN_POINT ( 'NONE',  ( 5.000030787343001215, -0.5496608443529845678, -2.045306479342562156 ) ) ;
#52332 = ORIENTED_EDGE ( 'NONE', *, *, #57512, .F. ) ;
#52333 = AXIS2_PLACEMENT_3D ( 'NONE', #9381, #19889, #57625 ) ;
#52334 = EDGE_CURVE ( 'NONE', #34244, #28326, #65685, .T. ) ;
#52335 = CARTESIAN_POINT ( 'NONE',  ( 0.5678519969244000265, -2.189299194929000159, -2.346944523683000217 ) ) ;
#52336 = CARTESIAN_POINT ( 'NONE',  ( 10.68035971519489813, 4.678140486081599825, 8.628134814664999652 ) ) ;
#52337 = CARTESIAN_POINT ( 'NONE',  ( 11.26847444708000090, 2.565620268983000329, -7.116623294300999270 ) ) ;
#52338 = ORIENTED_EDGE ( 'NONE', *, *, #56460, .F. ) ;
#52339 = CARTESIAN_POINT ( 'NONE',  ( 1.321806799207333460, -3.408904368339104263, -0.9161175952574813763 ) ) ;
#52340 = DIRECTION ( 'NONE',  ( 1.000000000000000000, 0.000000000000000000, 0.000000000000000000 ) ) ;
#52341 = CARTESIAN_POINT ( 'NONE',  ( 10.41964694612699915, 2.813019656517000477, 7.026297514493899499 ) ) ;
#52342 = DIRECTION ( 'NONE',  ( 0.000000000000000000, 0.4815106998112011483, -0.8764402124317022258 ) ) ;
#52343 = CARTESIAN_POINT ( 'NONE',  ( 9.106135841230999617, 4.192919163547999872, 5.525472271700999194 ) ) ;
#52344 = ORIENTED_EDGE ( 'NONE', *, *, #52081, .F. ) ;
#52345 = CARTESIAN_POINT ( 'NONE',  ( 24.84554778200963909, -12.09423845806785103, -2.925021800096165414 ) ) ;
#52346 = CARTESIAN_POINT ( 'NONE',  ( 15.89999719559887659, 8.538166969133406781, 8.218914602276583992 ) ) ;
#52347 = CARTESIAN_POINT ( 'NONE',  ( 8.219858292491261764, -5.680146748682262547, 7.949319526458594964 ) ) ;
#52348 = CARTESIAN_POINT ( 'NONE',  ( 9.448759580228999866, -5.110528875107000601, 7.765443149353999708 ) ) ;
#52349 = ORIENTED_EDGE ( 'NONE', *, *, #49797, .T. ) ;
#52350 = CARTESIAN_POINT ( 'NONE',  ( 2.980140132543583231, 3.408904368339106927, -0.9161175952574746040 ) ) ;
#52351 = CARTESIAN_POINT ( 'NONE',  ( 10.94426222744800015, -4.986443098259000450, 6.687444528363699625 ) ) ;
#52352 = ORIENTED_EDGE ( 'NONE', *, *, #46005, .F. ) ;
#52353 = EDGE_CURVE ( 'NONE', #18634, #63477, #20900, .T. ) ;
#52354 = CARTESIAN_POINT ( 'NONE',  ( 16.09997386696500143, -6.963621661623434100, -9.386500412226212120 ) ) ;
#52355 = CARTESIAN_POINT ( 'NONE',  ( 6.999999691988000095, 12.11716380430000051, 3.069905306952999791 ) ) ;
#52356 = ORIENTED_EDGE ( 'NONE', *, *, #2692, .F. ) ;
#52357 = CARTESIAN_POINT ( 'NONE',  ( 9.580894592352999339, -5.371875912611999482, -7.370590366721999409 ) ) ;
#52358 = DIRECTION ( 'NONE',  ( 0.4384236320214023319, 0.000000000000000000, 0.8987684456439056779 ) ) ;
#52359 = CIRCLE ( 'NONE', #16624, 1.250000000000000000 ) ;
#52360 = CARTESIAN_POINT ( 'NONE',  ( 10.89324174884020024, 3.967693531726030010, -8.674442868902998427 ) ) ;
#52361 = CARTESIAN_POINT ( 'NONE',  ( 11.89189666366029918, -4.052152326617509459, 6.326270943800999191 ) ) ;
#52362 = DIRECTION ( 'NONE',  ( -1.000000000000000000, 0.000000000000000000, 0.000000000000000000 ) ) ;
#52363 = CARTESIAN_POINT ( 'NONE',  ( 12.00271932425157040, -4.187398418774900044, 6.235801371442999397 ) ) ;
#52364 = CARTESIAN_POINT ( 'NONE',  ( 8.245295280410999794, 4.283000592898000392, 9.286795422009001655 ) ) ;
#52365 = ORIENTED_EDGE ( 'NONE', *, *, #34550, .F. ) ;
#52366 = CARTESIAN_POINT ( 'NONE',  ( 9.343930206849998754, 2.750000000000000000, -7.500000000000000000 ) ) ;
#52367 = CARTESIAN_POINT ( 'NONE',  ( 9.149956853208999874, -4.175914961544999748, 5.699510287082000026 ) ) ;
#52368 = CARTESIAN_POINT ( 'NONE',  ( 10.01059687351599692, 4.629523725463622341, 6.407767014557176566 ) ) ;
#52369 = VERTEX_POINT ( 'NONE', #47335 ) ;
#52370 = CARTESIAN_POINT ( 'NONE',  ( 12.24387941792144474, -2.775899267521871217, -12.38300827451277897 ) ) ;
#52371 = CARTESIAN_POINT ( 'NONE',  ( 18.46714228074024078, 2.893782244576861729, 11.28496185859599699 ) ) ;
#52372 = CARTESIAN_POINT ( 'NONE',  ( 23.56666365135700403, -8.673757318211000822, 7.881093921744994901 ) ) ;
#52373 = CARTESIAN_POINT ( 'NONE',  ( 10.69601354018300832, 4.999583552997727054, 8.268183399968641822 ) ) ;
#52374 = CARTESIAN_POINT ( 'NONE',  ( 12.72263738247862008, -1.880115814278897846, -13.78550660562619434 ) ) ;
#52375 = CARTESIAN_POINT ( 'NONE',  ( 11.24025954179439957, -3.228187097503200320, -8.141292208271599051 ) ) ;
#52376 = CARTESIAN_POINT ( 'NONE',  ( 11.43114108301961629, 4.620688244309836712, -6.880598518631706462 ) ) ;
#52377 = CARTESIAN_POINT ( 'NONE',  ( 18.22954180134192015, -2.744780546098131158, 12.29741030561552506 ) ) ;
#52378 = EDGE_LOOP ( 'NONE', ( #28038, #51619, #19942, #21618 ) ) ;
#52379 = ORIENTED_EDGE ( 'NONE', *, *, #36707, .F. ) ;
#52380 = CARTESIAN_POINT ( 'NONE',  ( 12.43999839845094790, 0.6380582630481954620, -13.98550026811281910 ) ) ;
#52381 =( NAMED_UNIT ( * ) PLANE_ANGLE_UNIT ( ) SI_UNIT ( $, .RADIAN. ) );
#52382 = FACE_OUTER_BOUND ( 'NONE', #26839, .T. ) ;
#52383 = CARTESIAN_POINT ( 'NONE',  ( 12.03828694957233303, -3.690393262785353734, 6.264939056470321788 ) ) ;
#52384 = CARTESIAN_POINT ( 'NONE',  ( 10.14584353048000054, 5.370502454907000178, -6.826221644974000746 ) ) ;
#52385 = CARTESIAN_POINT ( 'NONE',  ( 3.500000000000000000, 0.000000000000000000, 0.000000000000000000 ) ) ;
#52386 = CARTESIAN_POINT ( 'NONE',  ( 17.57591570971901618, 3.124999463061048921, 12.28373083832239132 ) ) ;
#52387 = CARTESIAN_POINT ( 'NONE',  ( 24.13682939974800234, -12.33401113332000065, 3.394273003449000292 ) ) ;
#52388 = ADVANCED_FACE ( 'NONE', ( #48017 ), #52570, .F. ) ;
#52390 = EDGE_CURVE ( 'NONE', #63466, #16664, #118, .T. ) ;
#52389 = CARTESIAN_POINT ( 'NONE',  ( 10.71756692516999898, 3.040224182812999665, 8.808452309630000698 ) ) ;
#52391 = ORIENTED_EDGE ( 'NONE', *, *, #26616, .T. ) ;
#52392 = CARTESIAN_POINT ( 'NONE',  ( 8.996000993494989828, 3.322909228140538129, -9.141577125681626725 ) ) ;
#52393 = EDGE_CURVE ( 'NONE', #51763, #64582, #6045, .T. ) ;
#52394 = EDGE_CURVE ( 'NONE', #12823, #16567, #11633, .T. ) ;
#52395 = ORIENTED_EDGE ( 'NONE', *, *, #41840, .T. ) ;
#52396 = CARTESIAN_POINT ( 'NONE',  ( 12.80505043854146940, -3.125000000000000444, 12.28374638332999780 ) ) ;
#52397 = CARTESIAN_POINT ( 'NONE',  ( 9.703659112603999048, -4.376739491155700712, -8.280881105104999307 ) ) ;
#52398 = CARTESIAN_POINT ( 'NONE',  ( 10.78089701270000056, 5.735299658853000082, 7.801561896854000366 ) ) ;
#52399 = CARTESIAN_POINT ( 'NONE',  ( 11.14391429142989942, -3.977620450637519678, 8.674673860548999471 ) ) ;
#52400 = DIRECTION ( 'NONE',  ( 1.000000000000000000, -8.605781653910000390E-10, 6.242650264219000041E-09 ) ) ;
#52401 = CARTESIAN_POINT ( 'NONE',  ( 7.966901574931999797, 4.609574279519000228, -6.276317554486000816 ) ) ;
#52402 = CARTESIAN_POINT ( 'NONE',  ( 11.09999999999999964, 4.000000000000000000, -7.500000000000000000 ) ) ;
#52403 = CARTESIAN_POINT ( 'NONE',  ( 12.35550214789977552, -0.4343244881883143171, 12.69000555157926868 ) ) ;
#52404 = CARTESIAN_POINT ( 'NONE',  ( 9.294718325437999695, 4.148133901461999784, 9.337478696773001019 ) ) ;
#52405 = CARTESIAN_POINT ( 'NONE',  ( 10.00637913184999839, 5.119263020957999899, 8.420380450036001108 ) ) ;
#52406 = CARTESIAN_POINT ( 'NONE',  ( 9.180279526884143948, -2.858231322599188662, 8.226333960650446642 ) ) ;
#52407 = ORIENTED_EDGE ( 'NONE', *, *, #50106, .F. ) ;
#52408 = CARTESIAN_POINT ( 'NONE',  ( 9.029445280412998542, 5.442817578555000146, -8.106149115450000053 ) ) ;
#52409 = CARTESIAN_POINT ( 'NONE',  ( 7.169256274120936467, 0.2500000000000000000, 3.082564036157276366 ) ) ;
#52410 = EDGE_CURVE ( 'NONE', #52012, #8057, #28782, .T. ) ;
#52411 = CARTESIAN_POINT ( 'NONE',  ( 17.88807090798125543, 1.970716457409874778, 13.77152834881607113 ) ) ;
#52412 = CARTESIAN_POINT ( 'NONE',  ( 12.80505043854146940, -3.199698446519381179, -12.18695736643652516 ) ) ;
#52413 = CARTESIAN_POINT ( 'NONE',  ( 10.13559687351566829, 5.092232985442826099, -6.870476274536379435 ) ) ;
#52414 = CARTESIAN_POINT ( 'NONE',  ( 10.76841504065829902, -3.085489673376300424, -6.818119527508899935 ) ) ;
#52415 = VERTEX_POINT ( 'NONE', #49389 ) ;
#52416 = DIRECTION ( 'NONE',  ( 1.000000000000000000, 0.000000000000000000, 0.000000000000000000 ) ) ;
#52417 = CARTESIAN_POINT ( 'NONE',  ( 11.36660992314014784, -3.674321412135250764, 11.19575788941673444 ) ) ;
#52419 = CARTESIAN_POINT ( 'NONE',  ( 13.99944283128300171, -9.262889243704000464, -8.209791536961999370 ) ) ;
#52418 = CARTESIAN_POINT ( 'NONE',  ( 9.700639158771000581, 4.262870449202000422, -8.811513791423999820 ) ) ;
#52420 = DIRECTION ( 'NONE',  ( 0.000000000000000000, 0.000000000000000000, -1.000000000000000000 ) ) ;
#52421 = ORIENTED_EDGE ( 'NONE', *, *, #60777, .F. ) ;
#52422 = CARTESIAN_POINT ( 'NONE',  ( 9.569805421428000614, 4.064052243276000453, 8.919241792616000808 ) ) ;
#52423 = CARTESIAN_POINT ( 'NONE',  ( 18.13009756288984420, -2.254948952832146247, -13.72233930590318884 ) ) ;
#52424 = CARTESIAN_POINT ( 'NONE',  ( 10.45672469555900008, 4.433465011431599656, 8.249937779480299938 ) ) ;
#52425 = CARTESIAN_POINT ( 'NONE',  ( 11.09999999999999964, -5.538898460221000519, 7.685179721164000277 ) ) ;
#52426 = CARTESIAN_POINT ( 'NONE',  ( 7.641206853206999661, -4.524489047957000132, 9.047757046927999980 ) ) ;
#52427 = VERTEX_POINT ( 'NONE', #6389 ) ;
#52428 = CARTESIAN_POINT ( 'NONE',  ( 8.995176658772999545, 2.707986230053999854, 5.994446745591000436 ) ) ;
#52430 = DIRECTION ( 'NONE',  ( 1.000000000000000000, 0.000000000000000000, 0.000000000000000000 ) ) ;
#52429 = CARTESIAN_POINT ( 'NONE',  ( 11.59999999999999964, 4.000000000000000000, 7.500000000000000000 ) ) ;
#52431 = VECTOR ( 'NONE', #46940, 1000.000000000000000 ) ;
#52432 = CARTESIAN_POINT ( 'NONE',  ( 7.612036250381388314, -4.782439721774751185, 5.946226314582684580 ) ) ;
#52433 = CARTESIAN_POINT ( 'NONE',  ( 18.17506427777800937, -0.08141198786016999589, 13.89969880262531632 ) ) ;
#52434 = CARTESIAN_POINT ( 'NONE',  ( 1.738474413115999928, 2.350777309937000403, -2.257240049571999752 ) ) ;
#52435 = ORIENTED_EDGE ( 'NONE', *, *, #61237, .F. ) ;
#52436 = LINE ( 'NONE', #4532, #37758 ) ;
#52437 = CARTESIAN_POINT ( 'NONE',  ( 11.54333729122640051, -5.003122373830000136, 7.526388557597149642 ) ) ;
#52438 = CARTESIAN_POINT ( 'NONE',  ( 10.09197164456000095, 3.841384681542000301, 5.536408945990000774 ) ) ;
#52439 = CARTESIAN_POINT ( 'NONE',  ( 11.79999999771000141, 12.39026187696000036, 1.832249219479999969 ) ) ;
#52440 = EDGE_CURVE ( 'NONE', #50331, #1476, #1502, .T. ) ;
#52441 = CARTESIAN_POINT ( 'NONE',  ( 11.40841235500449891, 3.158861363519000154, 8.270568563129298667 ) ) ;
#52442 = ORIENTED_EDGE ( 'NONE', *, *, #49706, .F. ) ;
#52443 = CARTESIAN_POINT ( 'NONE',  ( 23.99446449805473947, -3.345746341642283017, 12.75763603700710291 ) ) ;
#52444 = ADVANCED_FACE ( 'NONE', ( #11987 ), #27739, .F. ) ;
#52445 = CARTESIAN_POINT ( 'NONE',  ( 12.47072553654362714, 1.841758158201594942, -12.46466843114749068 ) ) ;
#52446 = CARTESIAN_POINT ( 'NONE',  ( 10.97884673417783041, -5.207210053465712640, 6.723535013421952478 ) ) ;
#52447 = CARTESIAN_POINT ( 'NONE',  ( 25.57778428390800229, -2.768507693251000212, -11.23374941714000030 ) ) ;
#52448 = CARTESIAN_POINT ( 'NONE',  ( 17.78989870834646680, -1.827084948615278481, 13.88026577095109815 ) ) ;
#52449 = CARTESIAN_POINT ( 'NONE',  ( 18.15002510837776128, 2.691473085059168824, -13.63098399828460927 ) ) ;
#52450 = ORIENTED_EDGE ( 'NONE', *, *, #9730, .F. ) ;
#52451 = MANIFOLD_SOLID_BREP ( 'Stock-MAS-678-1', #36975 ) ;
#52452 = LINE ( 'NONE', #20295, #54833 ) ;
#52453 = CARTESIAN_POINT ( 'NONE',  ( 0.2000000000000000389, 0.000000000000000000, 0.000000000000000000 ) ) ;
#52454 = ORIENTED_EDGE ( 'NONE', *, *, #26589, .T. ) ;
#52455 = CARTESIAN_POINT ( 'NONE',  ( 10.74708275169999894, -5.262360166711999909, 4.827842598592000378 ) ) ;
#52456 = CARTESIAN_POINT ( 'NONE',  ( 10.89979975933730039, 4.819074589197400726, 7.781807394638899922 ) ) ;
#52457 = CARTESIAN_POINT ( 'NONE',  ( 10.46932803217000085, 4.988495740890000363, 6.213106455073000411 ) ) ;
#52458 = CARTESIAN_POINT ( 'NONE',  ( 9.882903428397000312, 4.314559027837000293, -9.161039561412001930 ) ) ;
#52459 = CARTESIAN_POINT ( 'NONE',  ( 9.986774547327625484, -3.921486932049647489, -6.628582782427464792 ) ) ;
#52460 = CARTESIAN_POINT ( 'NONE',  ( 10.07771285905000092, -4.622037501707999319, 5.671359981946999973 ) ) ;
#52461 = CARTESIAN_POINT ( 'NONE',  ( 18.20545956023470779, -0.3178346465811165422, -12.59599179195193663 ) ) ;
#52462 = CARTESIAN_POINT ( 'NONE',  ( 8.975133055567869889, 5.349981391149201571, 7.499992565666659949 ) ) ;
#52463 = CARTESIAN_POINT ( 'NONE',  ( 10.60026222744819790, -4.774534945026900346, -8.138001937130599828 ) ) ;
#52464 = CARTESIAN_POINT ( 'NONE',  ( 7.533885841228999958, 4.623631324973000112, 8.651459902566999816 ) ) ;
#52465 = ORIENTED_EDGE ( 'NONE', *, *, #35553, .T. ) ;
#52466 =( NAMED_UNIT ( * ) SI_UNIT ( $, .STERADIAN. ) SOLID_ANGLE_UNIT ( ) );
#52467 = CARTESIAN_POINT ( 'NONE',  ( 10.93210843320491676, 2.862311695598936723, 6.901605483505059979 ) ) ;
#52468 = DIRECTION ( 'NONE',  ( 1.000000000000000000, 0.000000000000000000, 0.000000000000000000 ) ) ;
#52469 = CARTESIAN_POINT ( 'NONE',  ( 8.668369459057998938, 3.037916315484999963, -6.050520490110999461 ) ) ;
#52470 = B_SPLINE_CURVE_WITH_KNOTS ( 'NONE', 3,
 ( #48815, #48471, #37625, #924, #59991, #12101 ),
 .UNSPECIFIED., .F., .F.,
 ( 4, 2, 4 ),
 ( 0.000000000000000000, 0.5000000000000000000, 1.000000000000000000 ),
 .UNSPECIFIED. ) ;
#52471 = DIRECTION ( 'NONE',  ( 0.000000000000000000, 1.000000000000000000, 0.000000000000000000 ) ) ;
#52472 = CARTESIAN_POINT ( 'NONE',  ( 12.38032181885347960, 3.110191202103290031, 13.65016103957348825 ) ) ;
#52473 = CARTESIAN_POINT ( 'NONE',  ( 11.09648096125000016, -3.099777420064000033, 6.097103007060000301 ) ) ;
#52474 = CARTESIAN_POINT ( 'NONE',  ( 12.76469316428371847, -0.6250000000000007772, -12.67928922306547257 ) ) ;
#52475 = EDGE_CURVE ( 'NONE', #55564, #25719, #15084, .T. ) ;
#52476 = CARTESIAN_POINT ( 'NONE',  ( 12.36383866360284856, -0.5795518042670544379, 13.98800095993141390 ) ) ;
#52477 = EDGE_CURVE ( 'NONE', #23303, #10085, #57847, .T. ) ;
#52478 = VERTEX_POINT ( 'NONE', #50093 ) ;
#52479 = CARTESIAN_POINT ( 'NONE',  ( 12.58121427537368398, -1.795950320080881069, 12.47134981075813265 ) ) ;
#52480 = CARTESIAN_POINT ( 'NONE',  ( 10.21426717315699939, -4.869050473540199597, -6.759401780699699103 ) ) ;
#52481 = DIRECTION ( 'NONE',  ( 1.000000000000000000, 0.000000000000000000, 0.000000000000000000 ) ) ;
#52482 = CARTESIAN_POINT ( 'NONE',  ( 9.104016254283999743, -5.045864843302999780, 8.527867871227000407 ) ) ;
#52483 = CARTESIAN_POINT ( 'NONE',  ( 10.60434687351569494, -2.749999999999998224, -7.336375382625535124 ) ) ;
#52484 = CARTESIAN_POINT ( 'NONE',  ( 12.35979573085659844, -3.159987984332300215, 7.354650721737899133 ) ) ;
#52485 = B_SPLINE_SURFACE_WITH_KNOTS ( 'NONE', 3, 3, ( 
 ( #3203, #24873, #9465, #21255 ),
 ( #63892, #30806, #46201, #51440 ),
 ( #10761, #51101, #40952, #62274 ),
 ( #32104, #18943, #46549, #67852 ),
 ( #19976, #53421, #41297, #45857 ),
 ( #62606, #40271, #61588, #35034 ),
 ( #13704, #14729, #56348, #3536 ),
 ( #8454, #8794, #14392, #67166 ),
 ( #52119, #42584, #36044, #19279 ) ),
 .UNSPECIFIED., .F., .F., .F.,
 ( 4, 1, 1, 1, 1, 1, 4 ),
 ( 4, 4 ),
 ( -0.01830387170766999833, 0.000000000000000000, 0.2500000000000000000, 0.5000000000000000000, 0.7500000000000000000, 1.000000000000000000, 1.018541916426999983 ),
 ( -0.2206046696922999983, 1.220604669692000099 ),
 .UNSPECIFIED. ) ;
#52486 = CARTESIAN_POINT ( 'NONE',  ( 12.18940205905205332, 0.3800566752825982886, 12.59427093624936411 ) ) ;
#52487 = CARTESIAN_POINT ( 'NONE',  ( 7.555281674562000838, 4.314040636970999820, 8.819134391732999845 ) ) ;
#52488 = DIRECTION ( 'NONE',  ( 0.000000000000000000, 0.000000000000000000, -1.000000000000000000 ) ) ;
#52489 = CARTESIAN_POINT ( 'NONE',  ( 12.56929374240175612, 1.799893664886381250, 12.47078182885977782 ) ) ;
#52490 = CARTESIAN_POINT ( 'NONE',  ( 9.531901401888999814, -3.025808284870999731, -9.100010361367001366 ) ) ;
#52491 = CARTESIAN_POINT ( 'NONE',  ( 10.96949144726329806, 3.419793223320000131, -6.681274802424499448 ) ) ;
#52492 = CARTESIAN_POINT ( 'NONE',  ( 7.920378813398999185, 2.912874113511002783, -6.463705393502997332 ) ) ;
#52493 = B_SPLINE_CURVE_WITH_KNOTS ( 'NONE', 3,
 ( #27675, #59471, #33612, #22411, #64357, #1101, #22063, #59131, #11234, #32914 ),
 .UNSPECIFIED., .F., .F.,
 ( 4, 2, 2, 2, 4 ),
 ( 0.000000000000000000, 0.1249999999532679928, 0.2499999999065359857, 0.3749999998598039785, 0.4999999998130725265 ),
 .UNSPECIFIED. ) ;
#52494 = CARTESIAN_POINT ( 'NONE',  ( 10.97819528041000048, 5.476824759564999923, -7.128718425160999850 ) ) ;
#52495 = EDGE_CURVE ( 'NONE', #35879, #49285, #33308, .T. ) ;
#52496 = CARTESIAN_POINT ( 'NONE',  ( 9.655963142879999239, 5.251703735191999733, -7.236139910592400248 ) ) ;
#52498 = CARTESIAN_POINT ( 'NONE',  ( 12.26360295038370651, 2.812350523778595512, 12.37328769146724561 ) ) ;
#52497 = DIRECTION ( 'NONE',  ( 1.000000000000000000, 0.000000000000000000, 0.000000000000000000 ) ) ;
#52499 = CARTESIAN_POINT ( 'NONE',  ( 11.30000000000000071, -11.91995122273334751, -1.454135469681903547 ) ) ;
#52500 = ORIENTED_EDGE ( 'NONE', *, *, #44289, .F. ) ;
#52501 = CARTESIAN_POINT ( 'NONE',  ( 12.50368198906695127, -0.5476376384638111938, 12.68410501633232279 ) ) ;
#52502 = CARTESIAN_POINT ( 'NONE',  ( 9.030800552329955266, 2.902287361240370345, 6.174410955706410853 ) ) ;
#52503 = CARTESIAN_POINT ( 'NONE',  ( 10.68904248846000016, -2.568964727443000307, 7.728094434513999467 ) ) ;
#52504 = CARTESIAN_POINT ( 'NONE',  ( 10.21024205624999937, 3.689072563647699976, 6.690659495528099576 ) ) ;
#52505 = CARTESIAN_POINT ( 'NONE',  ( -15.86200481174999943, -11.00717859340000082, -1.432487142323000118 ) ) ;
#52506 = CARTESIAN_POINT ( 'NONE',  ( 12.21987570834416559, -2.720459983100028900, 13.62424277487875202 ) ) ;
#52507 = CARTESIAN_POINT ( 'NONE',  ( 12.63953418767183834, 1.875000000000000444, 13.78627077332620665 ) ) ;
#52508 = CYLINDRICAL_SURFACE ( 'NONE', #55615, 12.50000000000000000 ) ;
#52509 = EDGE_LOOP ( 'NONE', ( #27178, #51215, #13805, #1136 ) ) ;
#52510 = CARTESIAN_POINT ( 'NONE',  ( 4.226970154309000804, 0.7404484344845000399, 0.9906202336981998480 ) ) ;
#52511 = CARTESIAN_POINT ( 'NONE',  ( 8.820101285864000218, -4.823683599683300294, -6.521261160937499746 ) ) ;
#52512 = CARTESIAN_POINT ( 'NONE',  ( 9.731599613776074520, -3.320020895154290663, -8.679702885126729939 ) ) ;
#52513 = CARTESIAN_POINT ( 'NONE',  ( 11.94366954483529852, -3.514796851401900124, 8.248643701125299543 ) ) ;
#52514 = AXIS2_PLACEMENT_3D ( 'NONE', #60909, #7074, #49037 ) ;
#52515 = CARTESIAN_POINT ( 'NONE',  ( 18.16584637247983736, 2.632875908479945792, -12.41964751440798054 ) ) ;
#52516 = CARTESIAN_POINT ( 'NONE',  ( 11.50001436749000128, 11.64999275565999959, 4.104571566060999824E-10 ) ) ;
#52517 = CARTESIAN_POINT ( 'NONE',  ( 8.736820887142258130, -4.253281749927233513, -8.358484985884542695 ) ) ;
#52518 = B_SPLINE_CURVE_WITH_KNOTS ( 'NONE', 3,
 ( #61461, #35245, #8666, #66353 ),
 .UNSPECIFIED., .F., .F.,
 ( 4, 4 ),
 ( 0.000000000000000000, 1.000000000000000000 ),
 .UNSPECIFIED. ) ;
#52519 = CARTESIAN_POINT ( 'NONE',  ( 7.470056312015993960, 3.527048554922000090, 6.623442700707995456 ) ) ;
#52520 = CARTESIAN_POINT ( 'NONE',  ( 9.531901401888999814, -3.025808284870999731, -9.100010361367001366 ) ) ;
#52521 = LINE ( 'NONE', #15123, #58365 ) ;
#52522 = EDGE_CURVE ( 'NONE', #13791, #22723, #11292, .T. ) ;
#52523 = LINE ( 'NONE', #35426, #13216 ) ;
#52524 = CARTESIAN_POINT ( 'NONE',  ( 12.09897931881620181, 0.1662062226620488470, -13.99901824074930978 ) ) ;
#52525 = CARTESIAN_POINT ( 'NONE',  ( 13.46222979673600051, -9.132942286732999904, -7.608635239113000104 ) ) ;
#52526 = CARTESIAN_POINT ( 'NONE',  ( 9.216851002545999094, -2.832432432432000269, 6.822293592207000934 ) ) ;
#52527 = CARTESIAN_POINT ( 'NONE',  ( 11.00000000000000000, -2.799999999999999822, -5.864181267619000160 ) ) ;
#52528 = CIRCLE ( 'NONE', #50294, 13.89999856298999958 ) ;
#52529 = ORIENTED_EDGE ( 'NONE', *, *, #33418, .T. ) ;
#52530 = CARTESIAN_POINT ( 'NONE',  ( 8.713854719593998155, 5.442817578555000146, -8.106149115450000053 ) ) ;
#52531 = CARTESIAN_POINT ( 'NONE',  ( 11.52287616594230002, -4.261927842557799551, 8.325646653015098764 ) ) ;
#52532 = ORIENTED_EDGE ( 'NONE', *, *, #27406, .F. ) ;
#52533 = CARTESIAN_POINT ( 'NONE',  ( 13.60806600682073153, 12.33328427344333811, 2.183404734281086501 ) ) ;
#52534 = CARTESIAN_POINT ( 'NONE',  ( 18.08710802279906105, 2.021458498708241347, -13.85330284862005890 ) ) ;
#52535 = VERTEX_POINT ( 'NONE', #54643 ) ;
#52536 = CARTESIAN_POINT ( 'NONE',  ( 11.30878751119029957, 2.958974835389999836, 6.955365841266999638 ) ) ;
#52537 = CARTESIAN_POINT ( 'NONE',  ( 17.84632887396263001, 3.351233551899029717, -11.15758637348134208 ) ) ;
#52538 = LINE ( 'NONE', #51175, #65529 ) ;
#52539 = CARTESIAN_POINT ( 'NONE',  ( 10.28014141025500017, -3.582647672488299850, -8.243346240911998635 ) ) ;
#52540 = CARTESIAN_POINT ( 'NONE',  ( 12.22418139218991051, 0.2308705899911544235, -13.89742331311149393 ) ) ;
#52541 = CARTESIAN_POINT ( 'NONE',  ( 5.500000000000000000, 0.000000000000000000, 0.000000000000000000 ) ) ;
#52542 = CARTESIAN_POINT ( 'NONE',  ( 11.09999999999999964, 6.066544595402000084, 5.234304349664999911 ) ) ;
#52543 = ORIENTED_EDGE ( 'NONE', *, *, #66482, .T. ) ;
#52544 = CARTESIAN_POINT ( 'NONE',  ( 6.899999692186000289, 12.99045401582999837, -1.690592930688000095 ) ) ;
#52545 = CARTESIAN_POINT ( 'NONE',  ( 8.789679719592999874, 4.162493982103000256, -5.775210092227999858 ) ) ;
#52546 = ORIENTED_EDGE ( 'NONE', *, *, #34689, .F. ) ;
#52547 = CARTESIAN_POINT ( 'NONE',  ( 11.11264834745999863, 2.146077493652999824, -7.517188756437000130 ) ) ;
#52548 =( NAMED_UNIT ( * ) PLANE_ANGLE_UNIT ( ) SI_UNIT ( $, .RADIAN. ) );
#52549 = ORIENTED_EDGE ( 'NONE', *, *, #66686, .T. ) ;
#52550 = CARTESIAN_POINT ( 'NONE',  ( 8.870759580228998686, 2.755835090116000696, 7.797385380423699885 ) ) ;
#52551 = CARTESIAN_POINT ( 'NONE',  ( 18.13782450322841910, -2.273941707540254153, -12.50136077393157308 ) ) ;
#52552 = DIRECTION ( 'NONE',  ( -1.000000000000000000, 0.000000000000000000, 0.000000000000000000 ) ) ;
#52553 = CARTESIAN_POINT ( 'NONE',  ( 24.35365242081699932, -8.885108761891000739, -7.331500822262997374 ) ) ;
#52554 = EDGE_CURVE ( 'NONE', #63466, #36772, #39234, .T. ) ;
#52555 = CARTESIAN_POINT ( 'NONE',  ( 8.627615234342979278, 2.900000000000000799, 6.423404582975466681 ) ) ;
#52556 = EDGE_CURVE ( 'NONE', #34720, #26471, #813, .T. ) ;
#52557 = ORIENTED_EDGE ( 'NONE', *, *, #60490, .F. ) ;
#52558 = CARTESIAN_POINT ( 'NONE',  ( 12.83560584653800163, 12.04942283913000090, -3.198386977700000244 ) ) ;
#52559 = CARTESIAN_POINT ( 'NONE',  ( 18.22487142087599921, 11.55078329699999884, -4.188961560869000067 ) ) ;
#52560 = FACE_OUTER_BOUND ( 'NONE', #843, .T. ) ;
#52561 = DIRECTION ( 'NONE',  ( 1.000000000000000000, 0.000000000000000000, 0.000000000000000000 ) ) ;
#52562 = AXIS2_PLACEMENT_3D ( 'NONE', #6985, #23062, #11191 ) ;
#52563 = CARTESIAN_POINT ( 'NONE',  ( 12.09999922233642522, -11.66744139996562701, 3.971920075675145156 ) ) ;
#52564 = CARTESIAN_POINT ( 'NONE',  ( 18.26004861284300063, -2.925574202914999589, 11.93524904697000011 ) ) ;
#52565 = CARTESIAN_POINT ( 'NONE',  ( 10.49937632700000023, -2.985311165300999825, -6.358653174814000053 ) ) ;
#52566 = ORIENTED_EDGE ( 'NONE', *, *, #22358, .T. ) ;
#52567 = VERTEX_POINT ( 'NONE', #40623 ) ;
#52568 = AXIS2_PLACEMENT_3D ( 'NONE', #29649, #56883, #40128 ) ;
#52569 = CARTESIAN_POINT ( 'NONE',  ( 10.16426084122999995, 4.808846957865000604, -8.639578604182998944 ) ) ;
#52570 = PLANE ( 'NONE',  #69022 ) ;
#52571 = DIRECTION ( 'NONE',  ( 1.000000000000000000, 0.000000000000000000, -1.924386576027000187E-14 ) ) ;
#52572 = CARTESIAN_POINT ( 'NONE',  ( 24.15442797605639669, 3.324447313803516213, 12.46602381067075527 ) ) ;
#52573 = CYLINDRICAL_SURFACE ( 'NONE', #5347, 0.5000000000000002220 ) ;
#52574 = EDGE_CURVE ( 'NONE', #57654, #12746, #26620, .T. ) ;
#52575 = CARTESIAN_POINT ( 'NONE',  ( 9.155417874594000693, 3.202096358337300330, -7.839201596587598964 ) ) ;
#52577 = CARTESIAN_POINT ( 'NONE',  ( 7.752051012050213075, 3.239139382392606681, 6.375725454493062827 ) ) ;
#52576 = CARTESIAN_POINT ( 'NONE',  ( 10.23100081823899998, -4.888721525563999748, 7.032008172796599510 ) ) ;
#52578 = CARTESIAN_POINT ( 'NONE',  ( 7.555544676565999040, -2.930005555947998275, 6.552699291324001862 ) ) ;
#52579 = EDGE_LOOP ( 'NONE', ( #15301, #50976, #58633, #69118, #35249 ) ) ;
#52580 = EDGE_CURVE ( 'NONE', #2109, #48162, #65089, .T. ) ;
#52581 = DIRECTION ( 'NONE',  ( 1.000000000000000000, 1.776356839457000172E-14, -1.776356839457000172E-14 ) ) ;
#52582 = CARTESIAN_POINT ( 'NONE',  ( 7.540373275913000661, -2.929987504175003199, 6.557984262489997995 ) ) ;
#52583 = CARTESIAN_POINT ( 'NONE',  ( 10.36825461470400001, 2.760277452415999644, 7.184607557167700165 ) ) ;
#52584 = CARTESIAN_POINT ( 'NONE',  ( 6.999999691988000095, -12.11716380430000051, -3.069905306952999791 ) ) ;
#52585 = CARTESIAN_POINT ( 'NONE',  ( 9.595487457706001422, -3.928425191288000384, 5.531324308465000783 ) ) ;
#52586 = CARTESIAN_POINT ( 'NONE',  ( 17.94531445437959150, 2.988940031718388290, -12.32413547815658283 ) ) ;
#52587 = CARTESIAN_POINT ( 'NONE',  ( 10.52314899745999988, 5.167567567567999731, -6.822293592207000934 ) ) ;
#52588 = CARTESIAN_POINT ( 'NONE',  ( 13.73849254682300192, 8.874722368053999944, 7.906926164786999500 ) ) ;
#52589 = CARTESIAN_POINT ( 'NONE',  ( 8.057875016312998184, -4.641725571029997610, 6.225038937488997171 ) ) ;
#52590 = CARTESIAN_POINT ( 'NONE',  ( 9.965950584426998660, -3.655872208659600275, -6.704208565179699875 ) ) ;
#52591 = CARTESIAN_POINT ( 'NONE',  ( 17.80000000001300009, -3.351264566333000072, 11.15757590352999884 ) ) ;
#52592 = CARTESIAN_POINT ( 'NONE',  ( 11.05068303964748111, -4.571908710946855692, 8.161067340483363353 ) ) ;
#52593 = LINE ( 'NONE', #42113, #23895 ) ;
#52594 = CARTESIAN_POINT ( 'NONE',  ( 2.824155723461999390, 3.102089502169999680, 0.9991633116965998873 ) ) ;
#52595 = VERTEX_POINT ( 'NONE', #23861 ) ;
#52596 = CARTESIAN_POINT ( 'NONE',  ( 12.18832871607759927, -0.1019009512359513453, -12.69945530929772559 ) ) ;
#52597 = CARTESIAN_POINT ( 'NONE',  ( 12.18582115247814990, -2.585797660396002673, -12.43116941335174808 ) ) ;
#52598 = CARTESIAN_POINT ( 'NONE',  ( 8.225195096046167720, 2.649880853682612614, 7.500010424662513664 ) ) ;
#52599 = CARTESIAN_POINT ( 'NONE',  ( 25.60000000000000142, 0.000000000000000000, 0.000000000000000000 ) ) ;
#52600 = CARTESIAN_POINT ( 'NONE',  ( 8.646755198799242592, -2.839843517792559613, -6.809530303469401247 ) ) ;
#52601 = ORIENTED_EDGE ( 'NONE', *, *, #9295, .F. ) ;
#52602 = CARTESIAN_POINT ( 'NONE',  ( 10.84999882987999875, 0.000000000000000000, 0.000000000000000000 ) ) ;
#52603 = CIRCLE ( 'NONE', #15734, 14.00000000000000000 ) ;
#52604 = APPLICATION_PROTOCOL_DEFINITION ( 'draft international standard', 'automotive_design', 1998, #65019 ) ;
#52605 = CARTESIAN_POINT ( 'NONE',  ( 11.01790547754519878, -2.825704134258000266, -7.537269019642879542 ) ) ;
#52606 = CARTESIAN_POINT ( 'NONE',  ( 17.86534717979584030, 0.5429181308642001547, 12.68438171063677089 ) ) ;
#52607 = CARTESIAN_POINT ( 'NONE',  ( 13.08018231457700153, -11.57028798436999928, -1.758177683552999859 ) ) ;
#52608 = CARTESIAN_POINT ( 'NONE',  ( 7.577152171347006693, 5.350137026785319883, -7.706116878973872097 ) ) ;
#52609 = CARTESIAN_POINT ( 'NONE',  ( 27.64127793187000037, 5.599999999999999645, -6.571291218949999902 ) ) ;
#52610 = ORIENTED_EDGE ( 'NONE', *, *, #58253, .T. ) ;
#52611 = CARTESIAN_POINT ( 'NONE',  ( 10.74600376124999990, -5.242711034443999552, 8.978690688221998784 ) ) ;
#52612 = ORIENTED_EDGE ( 'NONE', *, *, #62825, .T. ) ;
#52613 = CARTESIAN_POINT ( 'NONE',  ( 12.00705667793316245, -3.398423525757989339, 6.338208022222376670 ) ) ;
#52614 = CARTESIAN_POINT ( 'NONE',  ( 7.866206853207000194, -4.580607464247000493, 9.213361409141999303 ) ) ;
#52615 = CARTESIAN_POINT ( 'NONE',  ( 16.13712493497300215, 8.294738329384999886, 8.125890082391000746 ) ) ;
#52616 = PRODUCT_RELATED_PRODUCT_CATEGORY ( 'part', '', ( #51713 ) ) ;
#52617 = ORIENTED_EDGE ( 'NONE', *, *, #60611, .T. ) ;
#52618 = CARTESIAN_POINT ( 'NONE',  ( 23.61131147273417241, 10.12055327194686427, 9.627973054067471281 ) ) ;
#52619 = VECTOR ( 'NONE', #65882, 1000.000000000000000 ) ;
#52620 = CARTESIAN_POINT ( 'NONE',  ( 7.880004719587999418, 2.759821810153000321, -8.454514188070000102 ) ) ;
#52621 = DIRECTION ( 'NONE',  ( 0.000000000000000000, -0.9659258262890757507, 0.2588190451024934835 ) ) ;
#52622 = CARTESIAN_POINT ( 'NONE',  ( 17.98439275848210173, -2.954313498893242684, 12.33404747595917783 ) ) ;
#52623 = ORIENTED_EDGE ( 'NONE', *, *, #24966, .T. ) ;
#52624 = CARTESIAN_POINT ( 'NONE',  ( 10.12549839661999940, -5.788806995403000144, 7.335561828691000485 ) ) ;
#52625 = CARTESIAN_POINT ( 'NONE',  ( 11.60000000000000142, 3.468809616172331634, 8.305884920888427558 ) ) ;
#52626 = CARTESIAN_POINT ( 'NONE',  ( 5.407109839684124175, 1.199500263597268246, 0.9218200799623752495 ) ) ;
#52627 = ORIENTED_EDGE ( 'NONE', *, *, #55803, .T. ) ;
#52628 = CARTESIAN_POINT ( 'NONE',  ( 9.688891943909794691, -2.651205815582408754, 7.263338752445791080 ) ) ;
#52629 = ORIENTED_EDGE ( 'NONE', *, *, #58389, .T. ) ;
#52630 = CARTESIAN_POINT ( 'NONE',  ( 23.60956155030027759, -10.12579905328778374, 9.624114175715389408 ) ) ;
#52631 = CARTESIAN_POINT ( 'NONE',  ( 10.92587665653180551, 2.333614391320864456, 8.028595212472627196 ) ) ;
#52632 = CARTESIAN_POINT ( 'NONE',  ( 4.932236545624000712, 0.07284287022823998647, 1.555811222638000091 ) ) ;
#52633 = CONICAL_SURFACE ( 'NONE', #15761, 13.04999927352999833, 0.7853981075146502233 ) ;
#52634 = CARTESIAN_POINT ( 'NONE',  ( 11.79999999771000141, -12.39026187696000036, -1.832249219479999969 ) ) ;
#52635 = LINE ( 'NONE', #53333, #63189 ) ;
#52636 = DIRECTION ( 'NONE',  ( 1.000000000000000000, 0.000000000000000000, 0.000000000000000000 ) ) ;
#52637 = CARTESIAN_POINT ( 'NONE',  ( 12.27346860450516708, 2.829323760734074433, 13.59803440778111572 ) ) ;
#52638 = CARTESIAN_POINT ( 'NONE',  ( 11.07345355053000091, -3.998673159585000025, 8.920828114954002075 ) ) ;
#52639 = ORIENTED_EDGE ( 'NONE', *, *, #26802, .F. ) ;
#52640 = EDGE_CURVE ( 'NONE', #43427, #12913, #61607, .T. ) ;
#52641 = CARTESIAN_POINT ( 'NONE',  ( 10.73724174883999893, -4.024531238983009906, -8.391788556008700439 ) ) ;
#52642 = ADVANCED_FACE ( 'NONE', ( #39600 ), #66162, .T. ) ;
#52643 = ORIENTED_EDGE ( 'NONE', *, *, #47435, .F. ) ;
#52644 = CARTESIAN_POINT ( 'NONE',  ( 9.332933391271998502, 5.100349772922000646, 8.693467186193998941 ) ) ;
#52645 = FACE_OUTER_BOUND ( 'NONE', #68061, .T. ) ;
#52646 = CARTESIAN_POINT ( 'NONE',  ( 12.70155625791296572, 1.883284863834661760, -13.78507964965114674 ) ) ;
#52647 = ADVANCED_FACE ( 'NONE', ( #66850 ), #60924, .F. ) ;
#52648 = DIRECTION ( 'NONE',  ( 0.000000000000000000, 1.000000000000000000, 0.000000000000000000 ) ) ;
#52649 = CARTESIAN_POINT ( 'NONE',  ( 6.999999999999999112, 7.162151381622562596, -3.226150686063063322 ) ) ;
#52650 = CARTESIAN_POINT ( 'NONE',  ( 23.50387503050299998, 0.000000000000000000, 0.000000000000000000 ) ) ;
#52651 = CARTESIAN_POINT ( 'NONE',  ( 9.442390274284505836, -4.489521974667288973, -9.208960678577202685 ) ) ;
#52652 = B_SPLINE_CURVE_WITH_KNOTS ( 'NONE', 3,
 ( #55607, #8396, #29741, #23441 ),
 .UNSPECIFIED., .F., .F.,
 ( 4, 4 ),
 ( 0.000000000000000000, 1.000000000000000000 ),
 .UNSPECIFIED. ) ;
#52653 = ORIENTED_EDGE ( 'NONE', *, *, #63158, .F. ) ;
#52654 = CARTESIAN_POINT ( 'NONE',  ( 7.100000000000000533, 13.17499999999999893, 0.000000000000000000 ) ) ;
#52655 = CARTESIAN_POINT ( 'NONE',  ( 11.85502763632550050, -5.160433036184000066, 8.035454525731699604 ) ) ;
#52656 = CARTESIAN_POINT ( 'NONE',  ( 3.248890132543875264, -2.798833948393641080, 2.150913519912190708 ) ) ;
#52657 = CARTESIAN_POINT ( 'NONE',  ( 15.47616489729399980, 9.395071224208001226, 8.199988963223999505 ) ) ;
#52658 = CARTESIAN_POINT ( 'NONE',  ( 8.822980646795000936, -2.678334737187000325, 8.735278777293000729 ) ) ;
#52660 = DIRECTION ( 'NONE',  ( 1.000000000000000000, -1.507841021312999948E-09, -1.100585032007000091E-11 ) ) ;
#52659 = CARTESIAN_POINT ( 'NONE',  ( 10.84168637167000071, 2.681011538858999899, 6.554754637093000547 ) ) ;
#52661 = CARTESIAN_POINT ( 'NONE',  ( 11.18272066707849888, 5.093522884867000222, -6.838543969064300398 ) ) ;
#52662 = ADVANCED_FACE ( 'NONE', ( #51460 ), #69090, .T. ) ;
#52663 = CARTESIAN_POINT ( 'NONE',  ( 25.58980682296600051, -11.09071036895000084, 3.239368791882000220 ) ) ;
#52664 = CARTESIAN_POINT ( 'NONE',  ( 9.754317406968999293, 4.161254277581000416, -8.351883209406098629 ) ) ;
#52665 = CARTESIAN_POINT ( 'NONE',  ( 18.07652645701807970, 0.4998493492226911417, 12.59008424712975227 ) ) ;
#52666 = CARTESIAN_POINT ( 'NONE',  ( 6.969371378776000547, 0.09220185020346000071, 1.552013010797000048 ) ) ;
#52667 = VECTOR ( 'NONE', #20317, 1000.000000000000000 ) ;
#52668 = DIRECTION ( 'NONE',  ( -1.000000000000000000, 0.000000000000000000, -2.523982353566999962E-12 ) ) ;
#52669 = CARTESIAN_POINT ( 'NONE',  ( 24.45366905783700062, 8.897659148319000622, 9.225340520377001141 ) ) ;
#52670 = VERTEX_POINT ( 'NONE', #50007 ) ;
#52671 = CARTESIAN_POINT ( 'NONE',  ( 7.390495559621999888, -2.216884807317999861, 8.370075800106999253 ) ) ;
#52672 = CARTESIAN_POINT ( 'NONE',  ( 8.126014158770999529, 5.189036231907000030, -8.048606212067999977 ) ) ;
#52673 = LINE ( 'NONE', #26109, #65066 ) ;
#52674 = DIRECTION ( 'NONE',  ( 0.000000000000000000, -0.2588190451024934280, 0.9659258262890756397 ) ) ;
#52675 = ORIENTED_EDGE ( 'NONE', *, *, #52556, .F. ) ;
#52676 = CARTESIAN_POINT ( 'NONE',  ( 18.26005557146100244, 2.925549590147000334, 11.93525498079000080 ) ) ;
#52677 = CARTESIAN_POINT ( 'NONE',  ( 10.64391429142989765, 4.022379549362480766, 8.674673860548999471 ) ) ;
#52678 = AXIS2_PLACEMENT_3D ( 'NONE', #33816, #56506, #61412 ) ;
#52679 = CARTESIAN_POINT ( 'NONE',  ( 10.18308278041000037, 2.953582937013000009, -8.606284720264998356 ) ) ;
#52680 = ORIENTED_EDGE ( 'NONE', *, *, #44074, .F. ) ;
#52681 = CARTESIAN_POINT ( 'NONE',  ( 12.48426296206727670, -0.6451567829544542221, -12.58347320810648107 ) ) ;
#52682 = DIRECTION ( 'NONE',  ( 1.000000000000000000, 0.000000000000000000, 0.000000000000000000 ) ) ;
#52683 = CARTESIAN_POINT ( 'NONE',  ( 10.71503032197929883, 4.743378537856500543, 8.539569492647999027 ) ) ;
#52684 = DIRECTION ( 'NONE',  ( 1.000000000000000000, 0.000000000000000000, 0.000000000000000000 ) ) ;
#52685 = CARTESIAN_POINT ( 'NONE',  ( 8.528448341230999930, 2.472348777564000066, 6.234194744024999402 ) ) ;
#52686 = ORIENTED_EDGE ( 'NONE', *, *, #6555, .F. ) ;
#52687 = CARTESIAN_POINT ( 'NONE',  ( 11.35194303199000032, -3.840151595817999919, 11.76830449990999838 ) ) ;
#52688 = CARTESIAN_POINT ( 'NONE',  ( 6.837589158771000264, 5.757004663580000070, -7.968612095259000050 ) ) ;
#52689 = CARTESIAN_POINT ( 'NONE',  ( 8.234515473452628243, -5.574618550199808453, 8.239559727061074312 ) ) ;
#52690 = CARTESIAN_POINT ( 'NONE',  ( 11.03775575519999919, -8.050335494570999728, 6.914609630061999468 ) ) ;
#52691 = ORIENTED_EDGE ( 'NONE', *, *, #57177, .F. ) ;
#52692 = CARTESIAN_POINT ( 'NONE',  ( 16.29309513285500088, -3.300500509464999954, -11.83372189959999865 ) ) ;
#52693 = CARTESIAN_POINT ( 'NONE',  ( 6.240443173016666734, 0.1963495408493638184, -1.499999999999999778 ) ) ;
#52694 = ORIENTED_EDGE ( 'NONE', *, *, #1041, .F. ) ;
#52695 = CARTESIAN_POINT ( 'NONE',  ( 8.736413463905998711, 4.084156314540369870, 6.617590440947399344 ) ) ;
#52696 = CARTESIAN_POINT ( 'NONE',  ( 9.090417628846997999, 10.34502497667999954, -4.677911246888999841 ) ) ;
#52697 = ORIENTED_EDGE ( 'NONE', *, *, #68611, .F. ) ;
#52698 = CARTESIAN_POINT ( 'NONE',  ( 13.50000000000000178, 0.000000000000000000, 0.000000000000000000 ) ) ;
#52699 = EDGE_CURVE ( 'NONE', #15904, #17545, #61764, .T. ) ;
#52700 = EDGE_CURVE ( 'NONE', #23313, #53841, #12954, .T. ) ;
#52701 = CARTESIAN_POINT ( 'NONE',  ( 9.492891187585001944, -4.474581801608000120, -6.279517683005999551 ) ) ;
#52702 = CARTESIAN_POINT ( 'NONE',  ( 8.895035841232999729, 5.751585344281000545, -8.235867044345999588 ) ) ;
#52703 = CARTESIAN_POINT ( 'NONE',  ( 10.55569598648999907, 5.130952141044000214, -8.173387776112500447 ) ) ;
#52704 = B_SPLINE_CURVE_WITH_KNOTS ( 'NONE', 3,
 ( #1304, #61072, #60032, #12486, #11786, #55483, #6190, #18429, #1650, #34165, #22619, #33821, #48858, #22278, #43963, #64914, #17028, #33472, #65269, #7239, #1999, #38361, #28576, #49891, #33125, #12142, #54788, #66991, #29270, #3024, #34520, #61416, #7934, #40101, #24353 ),
 .UNSPECIFIED., .F., .F.,
 ( 4, 1, 1, 1, 1, 1, 1, 1, 1, 1, 1, 1, 1, 1, 1, 1, 1, 1, 1, 1, 1, 1, 1, 1, 1, 1, 1, 1, 1, 1, 1, 1, 4 ),
 ( 0.000000000000000000, 0.01250563797078715726, 0.04500523735960059585, 0.07750483674842403858, 0.1100044361372474744, 0.1425040355260709102, 0.1750036349148943460, 0.2075032343037177818, 0.2400028336925412453, 0.2725024330813646811, 0.3050020324701880892, 0.3375016318590116082, 0.3700012312478350163, 0.4025008306366584798, 0.4350004300254818879, 0.4675000294143053514, 0.4999996288031287039, 0.5324992281919521675, 0.5649988275807755755, 0.5974984269695990946, 0.6299980263584225026, 0.6624976257472459107, 0.6949972251360693187, 0.7274968245248928378, 0.7599964239137162458, 0.7924960233025396539, 0.8249956226913630619, 0.8574952220801865810, 0.8899948214690099890, 0.9224944208578333971, 0.9549940202466568051, 0.9874936196354803242, 1.000000000000000000 ),
 .UNSPECIFIED. ) ;
#52705 = CARTESIAN_POINT ( 'NONE',  ( 12.22433327354039889, -4.983220429128399687, 8.143111181492699302 ) ) ;
#52706 = CARTESIAN_POINT ( 'NONE',  ( 12.55891702277097011, 3.074517471785632949, -12.29897628258782660 ) ) ;
#52707 = CARTESIAN_POINT ( 'NONE',  ( 11.80995122972050027, -3.547233695387300045, 8.547040013405998948 ) ) ;
#52708 = CARTESIAN_POINT ( 'NONE',  ( 8.630420280412000267, 5.808262417891000062, 7.446016144116000213 ) ) ;
#52709 = ORIENTED_EDGE ( 'NONE', *, *, #27224, .F. ) ;
#52710 = CARTESIAN_POINT ( 'NONE',  ( 9.185590450029501142, -2.907727159402500039, -6.870462550877413754 ) ) ;
#52711 = VECTOR ( 'NONE', #46275, 1000.000000000000000 ) ;
#52712 = CARTESIAN_POINT ( 'NONE',  ( 8.160745559622998968, -5.944572422272999646, 7.106845737860000511 ) ) ;
#52713 = CARTESIAN_POINT ( 'NONE',  ( 9.832537864288001472, 2.899999999999999911, 6.571291218949999902 ) ) ;
#52714 = ORIENTED_EDGE ( 'NONE', *, *, #65124, .T. ) ;
#52715 = CARTESIAN_POINT ( 'NONE',  ( 12.23528344688402036, -2.757674802278839099, -12.38780605717374250 ) ) ;
#52716 = CARTESIAN_POINT ( 'NONE',  ( 10.62954538377999647, 10.07873972128999895, -5.168771492221002184 ) ) ;
#52717 = CARTESIAN_POINT ( 'NONE',  ( 5.700000000000000178, -1.300000000000000044, -10.66294468575716969 ) ) ;
#52718 = CARTESIAN_POINT ( 'NONE',  ( 10.78976354018297634, 3.672815144550904076, 8.717465845835395299 ) ) ;
#52719 = CARTESIAN_POINT ( 'NONE',  ( 12.50345261626383220, -3.182071724319532890, -13.63357796689960111 ) ) ;
#52720 = B_SPLINE_CURVE_WITH_KNOTS ( 'NONE', 3,
 ( #7846, #13782, #17995, #29181, #55394 ),
 .UNSPECIFIED., .F., .F.,
 ( 4, 1, 4 ),
 ( 0.000000000000000000, 0.5000000000000000000, 1.000000000000000000 ),
 .UNSPECIFIED. ) ;
#52721 = CARTESIAN_POINT ( 'NONE',  ( 11.09256785386839894, -4.832509746210599921, -8.060248494254899754 ) ) ;
#52722 = DIRECTION ( 'NONE',  ( 0.000000000000000000, 1.000000000000000000, 0.000000000000000000 ) ) ;
#52723 = CARTESIAN_POINT ( 'NONE',  ( 18.05312913029198896, -3.003720153666145531, 12.23674614497118007 ) ) ;
#52724 = VERTEX_POINT ( 'NONE', #35983 ) ;
#52725 = ADVANCED_FACE ( 'NONE', ( #58336 ), #62547, .F. ) ;
#52726 = ORIENTED_EDGE ( 'NONE', *, *, #50997, .T. ) ;
#52727 = AXIS2_PLACEMENT_3D ( 'NONE', #13723, #61606, #29474 ) ;
#52728 = DIRECTION ( 'NONE',  ( 1.000000000000000000, 0.000000000000000000, 0.000000000000000000 ) ) ;
#52729 = CARTESIAN_POINT ( 'NONE',  ( 11.75158531382729699, -3.727547057523674212, 8.749999999999996447 ) ) ;
#52730 = CARTESIAN_POINT ( 'NONE',  ( 11.91486084871699802, -5.207010770456999893, 7.174999999999999822 ) ) ;
#52731 = EDGE_CURVE ( 'NONE', #4160, #48090, #11727, .T. ) ;
#52732 = CARTESIAN_POINT ( 'NONE',  ( 10.77434248675000106, 4.612886656332999991, -8.898793847069001117 ) ) ;
#52733 = CARTESIAN_POINT ( 'NONE',  ( 10.52663358771999924, -4.933730002636999679, -6.506004698255999585 ) ) ;
#52734 = CARTESIAN_POINT ( 'NONE',  ( 18.17259031544350023, 2.401600790900606519, 12.47395980848747321 ) ) ;
#52735 = AXIS2_PLACEMENT_3D ( 'NONE', #1067, #47589, #68894 ) ;
#52736 = CARTESIAN_POINT ( 'NONE',  ( 23.91179595127900015, -12.75400041561000108, 3.592921910965999999 ) ) ;
#52737 = CARTESIAN_POINT ( 'NONE',  ( 10.99933470386000067, 5.081013421858999735, 8.239043921879998678 ) ) ;
#52738 = EDGE_LOOP ( 'NONE', ( #41470, #44647, #61421, #62806, #55492 ) ) ;
#52739 = CARTESIAN_POINT ( 'NONE',  ( 10.90157398350000051, -5.294378252237999405, -4.903209430186000084 ) ) ;
#52740 = ORIENTED_EDGE ( 'NONE', *, *, #47519, .T. ) ;
#52741 = CARTESIAN_POINT ( 'NONE',  ( 9.781673028307999118, 5.464749740720999505, 8.817329433105999925 ) ) ;
#52742 = CARTESIAN_POINT ( 'NONE',  ( 9.171747021775997766, -4.651672637235799712, -8.071865996877098937 ) ) ;
#52743 = CARTESIAN_POINT ( 'NONE',  ( 10.66951519566999806, 4.592673277375999952, 5.841403042559999648 ) ) ;
#52744 = CARTESIAN_POINT ( 'NONE',  ( 11.86056039236529891, -3.108928759355700233, 7.456633480985620288 ) ) ;
#52745 = CARTESIAN_POINT ( 'NONE',  ( 9.318935841232999451, 2.644017913812000131, -7.838184857420000817 ) ) ;
#52746 = CARTESIAN_POINT ( 'NONE',  ( 10.95087244768999923, 9.916146810440000792, -5.627651682437000424 ) ) ;
#52747 = CARTESIAN_POINT ( 'NONE',  ( 24.85114852451900092, 8.568860018262000722, 8.855052040836000060 ) ) ;
#52748 = EDGE_CURVE ( 'NONE', #47074, #3245, #15354, .T. ) ;
#52749 = CARTESIAN_POINT ( 'NONE',  ( 12.61341903040855783, -0.5949840079737210852, 12.68123264482375490 ) ) ;
#52750 = CARTESIAN_POINT ( 'NONE',  ( 5.518321182375771627, -12.20777697081100932, -3.787023466231959734 ) ) ;
#52751 = CARTESIAN_POINT ( 'NONE',  ( 10.81315553411000074, 3.756074350075000012, 6.071610008629000355 ) ) ;
#52752 = CARTESIAN_POINT ( 'NONE',  ( 9.148111568353531453, -3.223588768401370874, 8.615646755131677992 ) ) ;
#52753 = ORIENTED_EDGE ( 'NONE', *, *, #6797, .T. ) ;
#52754 = CARTESIAN_POINT ( 'NONE',  ( 8.988579719593998263, 4.902869380824999901, -8.978557145469999057 ) ) ;
#52755 = CARTESIAN_POINT ( 'NONE',  ( 10.09964828895399869, 5.121614868497999851, -8.112615456209400833 ) ) ;
#52756 = B_SPLINE_CURVE_WITH_KNOTS ( 'NONE', 3,
 ( #35002, #22846, #60262, #59908, #28103, #64793 ),
 .UNSPECIFIED., .F., .F.,
 ( 4, 2, 4 ),
 ( 0.000000000000000000, 0.5000000000000000000, 1.000000000000000000 ),
 .UNSPECIFIED. ) ;
#52757 = B_SPLINE_CURVE_WITH_KNOTS ( 'NONE', 3,
 ( #25298, #24955, #14130, #51191 ),
 .UNSPECIFIED., .F., .F.,
 ( 4, 4 ),
 ( 0.000000000000000000, 0.1836163425310833319 ),
 .UNSPECIFIED. ) ;
#52758 = DIRECTION ( 'NONE',  ( -1.000000000000000000, 0.000000000000000000, 0.000000000000000000 ) ) ;
#52759 = CARTESIAN_POINT ( 'NONE',  ( 9.099999999999999645, 0.000000000000000000, 0.000000000000000000 ) ) ;
#52760 = CARTESIAN_POINT ( 'NONE',  ( 12.10000000000000142, -2.860800829850470350, 7.925587283338803246 ) ) ;
#52761 = CARTESIAN_POINT ( 'NONE',  ( 11.69559063708295987, -2.913481137622000006, -7.805482129094999166 ) ) ;
#52762 = EDGE_LOOP ( 'NONE', ( #23330, #67309, #16613, #68024 ) ) ;
#52763 = CIRCLE ( 'NONE', #21459, 11.85002173638999778 ) ;
#52764 = CARTESIAN_POINT ( 'NONE',  ( 5.695116968502542676, -12.04237015855036219, 3.723491068767540657 ) ) ;
#52765 = DIRECTION ( 'NONE',  ( -1.000000000000000000, 0.000000000000000000, 0.000000000000000000 ) ) ;
#52768 = CARTESIAN_POINT ( 'NONE',  ( 14.02341781689399980, -9.526752659074999130, -8.190681853965998016 ) ) ;
#52767 = UNCERTAINTY_MEASURE_WITH_UNIT (LENGTH_MEASURE( 1.000000000000000082E-05 ), #60580, 'distance_accuracy_value', 'NONE');
#52766 = DIRECTION ( 'NONE',  ( 0.000000000000000000, 1.000000000000000000, 0.000000000000000000 ) ) ;
#52769 = CARTESIAN_POINT ( 'NONE',  ( 18.16582246987730187, -2.632686762925362967, 13.64442020621638818 ) ) ;
#52770 = ORIENTED_EDGE ( 'NONE', *, *, #51983, .T. ) ;
#52771 = CARTESIAN_POINT ( 'NONE',  ( 10.25888757983999966, 4.512388525173999909, 5.993701490107000929 ) ) ;
#52772 = CARTESIAN_POINT ( 'NONE',  ( 18.05358084703149757, -2.122495591609769860, -13.74627451715324078 ) ) ;
#52773 = CARTESIAN_POINT ( 'NONE',  ( 11.02287616594229824, 3.738072157442200005, 8.325646653015098764 ) ) ;
#52774 = CARTESIAN_POINT ( 'NONE',  ( 24.70910065716694959, -11.78226157761774751, 3.190800174812568724 ) ) ;
#52775 = CARTESIAN_POINT ( 'NONE',  ( 8.668206853210000062, -3.979464503892999439, 9.134080454305001595 ) ) ;
#52776 = VERTEX_POINT ( 'NONE', #26535 ) ;
#52777 = CARTESIAN_POINT ( 'NONE',  ( 8.251329719592000345, 5.773189794777000117, 7.141495931231999883 ) ) ;
#52779 = DIRECTION ( 'NONE',  ( 0.7071067811865180408, 0.1740571194759044926, 0.6853496327859179837 ) ) ;
#52778 = CARTESIAN_POINT ( 'NONE',  ( 10.67375944625267614, 3.325302618462734561, -8.055763479958521600 ) ) ;
#52780 = CARTESIAN_POINT ( 'NONE',  ( 7.608564460558524090, -4.712693663111584996, 5.912577119032927264 ) ) ;
#52781 = CIRCLE ( 'NONE', #20390, 12.50000000000000000 ) ;
#52782 = CARTESIAN_POINT ( 'NONE',  ( 18.13610176148302600, -0.2304125752445602970, 13.89743363615726501 ) ) ;
#52783 = CARTESIAN_POINT ( 'NONE',  ( 23.74058065684300090, 3.323266457502000115, 13.27946843520000009 ) ) ;
#52784 = ORIENTED_EDGE ( 'NONE', *, *, #7137, .T. ) ;
#52785 = CARTESIAN_POINT ( 'NONE',  ( 23.66004879239100234, 13.39256428908000096, 3.813547978107000080 ) ) ;
#52786 = CARTESIAN_POINT ( 'NONE',  ( 11.81410538575740077, -3.024036709177600368, 7.733337754805098996 ) ) ;
#52787 = CARTESIAN_POINT ( 'NONE',  ( 9.409314688805999083, 2.634692233435000031, 8.920311306029999443 ) ) ;
#52788 = CARTESIAN_POINT ( 'NONE',  ( 11.53154451118193258, 12.41096832478124057, 1.687237643085517158 ) ) ;
#52789 = CARTESIAN_POINT ( 'NONE',  ( 10.94072200990529886, 2.922907051630999842, 7.875713849677398848 ) ) ;
#52790 = ORIENTED_EDGE ( 'NONE', *, *, #36299, .T. ) ;
#52791 = EDGE_CURVE ( 'NONE', #39266, #58368, #65968, .T. ) ;
#52792 = EDGE_CURVE ( 'NONE', #7236, #33164, #23273, .T. ) ;
#52793 = B_SPLINE_CURVE_WITH_KNOTS ( 'NONE', 3,
 ( #26641, #25941, #52161, #10204, #46928, #53198 ),
 .UNSPECIFIED., .F., .F.,
 ( 4, 2, 4 ),
 ( 0.000000000000000000, 0.5000000000000000000, 1.000000000000000000 ),
 .UNSPECIFIED. ) ;
#52794 = CARTESIAN_POINT ( 'NONE',  ( 23.60000336544893074, -2.996612530978001843, 13.56986086524380930 ) ) ;
#52795 = ADVANCED_FACE ( 'NONE', ( #36331 ), #26687, .F. ) ;
#52796 = CARTESIAN_POINT ( 'NONE',  ( 12.08118961495425836, 2.529460273524981151, -12.34351656561901400 ) ) ;
#52797 = DIRECTION ( 'NONE',  ( 1.000000000000000000, 0.000000000000000000, 0.000000000000000000 ) ) ;
#52798 = CARTESIAN_POINT ( 'NONE',  ( 17.55505043854147118, -3.199751711897561801, 12.18694338143115452 ) ) ;
#52799 = CARTESIAN_POINT ( 'NONE',  ( 17.88876975676777192, -1.869670916578588526, 13.87459417580158316 ) ) ;
#52800 = CARTESIAN_POINT ( 'NONE',  ( 18.16657332772220101, 2.629115783231108949, -13.64522528429649029 ) ) ;
#52801 = ORIENTED_EDGE ( 'NONE', *, *, #46367, .T. ) ;
#52802 = MANIFOLD_SOLID_BREP ( 'Stock-MAS-678-1', #12421 ) ;
#52803 = CARTESIAN_POINT ( 'NONE',  ( 9.704564187634398209, 2.648431596117105435, 7.852956029643507918 ) ) ;
#52804 = CARTESIAN_POINT ( 'NONE',  ( 13.00000000005200107, -12.15994572112000149, -2.000334444851999738 ) ) ;
#52805 = VERTEX_POINT ( 'NONE', #1332 ) ;
#52806 = DIRECTION ( 'NONE',  ( -0.000000000000000000, 0.5895247755844827964, 0.8077502949377767250 ) ) ;
#52807 = CARTESIAN_POINT ( 'NONE',  ( 15.90003771078200145, 3.695138809391000034, 11.25918926437999978 ) ) ;
#52808 = CARTESIAN_POINT ( 'NONE',  ( 7.100000000000000533, -12.50865771883999855, 2.924687089724999911 ) ) ;
#52809 = CARTESIAN_POINT ( 'NONE',  ( 10.30296826955000000, 4.081263352980999848, -9.025008366823000117 ) ) ;
#52810 = CARTESIAN_POINT ( 'NONE',  ( 25.59994555223600088, 0.6783951095376320461, -11.19994871957817573 ) ) ;
#52811 = CARTESIAN_POINT ( 'NONE',  ( 10.00122642709000154, -2.274091010763000131, 7.851325450887000734 ) ) ;
#52812 = CARTESIAN_POINT ( 'NONE',  ( 17.88703114068441380, -0.6395598188657377614, -12.58375915074078577 ) ) ;
#52813 = LINE ( 'NONE', #41632, #17377 ) ;
#52814 = CARTESIAN_POINT ( 'NONE',  ( 11.53148876160955005, -4.790673964186999534, -8.322268080792200706 ) ) ;
#52815 = CARTESIAN_POINT ( 'NONE',  ( 8.213545280409999094, 3.608525622520999843, 5.913376237674000002 ) ) ;
#52816 = ORIENTED_EDGE ( 'NONE', *, *, #48721, .T. ) ;
#52817 = VECTOR ( 'NONE', #46406, 1000.000000000000114 ) ;
#52818 = CARTESIAN_POINT ( 'NONE',  ( 7.550000000000000711, 4.000000000000000000, 8.849999999999999645 ) ) ;
#52819 = B_SPLINE_CURVE_WITH_KNOTS ( 'NONE', 3,
 ( #64206, #16666, #38337, #48836, #53048, #17364, #37990, #26828, #6521, #27510, #69119, #11417, #11083, #6169, #63865, #15979, #54072, #5493, #32759, #16321, #48146 ),
 .UNSPECIFIED., .F., .F.,
 ( 4, 2, 2, 1, 1, 2, 2, 2, 1, 2, 2, 4 ),
 ( 0.000000000000000000, 0.1249999999999699685, 0.1874999999999563127, 0.2187499999999506228, 0.2343749999999491240, 0.2421874999999520106, 0.2499999999999548694, 0.3749999999999629186, 0.4374999999999693023, 0.4687499999999714118, 0.4999999999999735767, 1.000000000000000000 ),
 .UNSPECIFIED. ) ;
#52820 = CARTESIAN_POINT ( 'NONE',  ( 11.96021572556889012, -5.045751188959975764, 7.824997386306807634 ) ) ;
#52821 = CARTESIAN_POINT ( 'NONE',  ( 8.593644002494778888, 2.940065707283205043, -6.265224637780645978 ) ) ;
#52822 = CARTESIAN_POINT ( 'NONE',  ( 6.543367680740003856, 10.50330513573999269, 4.576010683979003346 ) ) ;
#52823 = CARTESIAN_POINT ( 'NONE',  ( 12.43994760172710023, 1.886699913279277885, 13.87229234465171501 ) ) ;
#52824 = CARTESIAN_POINT ( 'NONE',  ( 10.96418140149000031, 7.492203170189000616, 6.189237391497999674 ) ) ;
#52825 = CARTESIAN_POINT ( 'NONE',  ( 9.254609482145166766, -2.734579386017075286, 7.018993749219657019 ) ) ;
#52826 = DIRECTION ( 'NONE',  ( -1.000000000000000000, 0.000000000000000000, 0.000000000000000000 ) ) ;
#52827 = ORIENTED_EDGE ( 'NONE', *, *, #38801, .F. ) ;
#52828 = CARTESIAN_POINT ( 'NONE',  ( 24.72545694048200104, 8.702406706990998941, 9.187175443698999189 ) ) ;
#52829 = CARTESIAN_POINT ( 'NONE',  ( 9.304430433046999127, -5.088604610742000212, -6.828193190755800224 ) ) ;
#52830 = DIRECTION ( 'NONE',  ( 0.000000000000000000, 1.000000000000000000, 0.000000000000000000 ) ) ;
#52831 = CARTESIAN_POINT ( 'NONE',  ( 9.724613486786999772, -2.928302463146000179, 8.718481221599999387 ) ) ;
#52832 = CARTESIAN_POINT ( 'NONE',  ( 12.06441235500451015, -4.638700978900200056, 8.085115074060599483 ) ) ;
#52833 = AXIS2_PLACEMENT_3D ( 'NONE', #46873, #5, #21327 ) ;
#52834 = EDGE_CURVE ( 'NONE', #20902, #67055, #8402, .T. ) ;
#52835 = CARTESIAN_POINT ( 'NONE',  ( 12.10479047996948943, 0.1866745257715813344, 12.59862229962904046 ) ) ;
#52836 = LINE ( 'NONE', #58761, #6381 ) ;
#52837 = CARTESIAN_POINT ( 'NONE',  ( 4.490838406521878490, 0.5240408911627599808, -1.077889606989799409 ) ) ;
#52838 = EDGE_CURVE ( 'NONE', #25280, #56515, #43299, .T. ) ;
#52839 = CARTESIAN_POINT ( 'NONE',  ( 12.09642313398529190, 2.633248533341329356, 12.32177498806536953 ) ) ;
#52840 = CARTESIAN_POINT ( 'NONE',  ( 25.29987654162099986, -9.517611874540000017, -8.103398312166000039 ) ) ;
#52841 = CARTESIAN_POINT ( 'NONE',  ( 10.89564560330029863, 4.307504762655200103, -6.544808043482999160 ) ) ;
#52842 = CARTESIAN_POINT ( 'NONE',  ( 12.57536348657924385, 11.53887048480315691, -4.871543742293567902 ) ) ;
#52843 = CARTESIAN_POINT ( 'NONE',  ( 11.07691721959000120, 3.101894630379999906, -8.926552937604000704 ) ) ;
#52844 = CARTESIAN_POINT ( 'NONE',  ( 10.10344474310099905, 5.137935629024000583, -8.052229793103100164 ) ) ;
#52846 = CARTESIAN_POINT ( 'NONE',  ( 12.23179573719470348, 2.749250018103629234, 12.38999654616027790 ) ) ;
#52845 = CARTESIAN_POINT ( 'NONE',  ( 9.091433907306445406, -3.054280487670652189, -8.331756427597948544 ) ) ;
#52847 = B_SPLINE_CURVE_WITH_KNOTS ( 'NONE', 3,
 ( #53335, #21849, #68708, #16264 ),
 .UNSPECIFIED., .F., .F.,
 ( 4, 4 ),
 ( 0.000000000000000000, 1.000000000000000000 ),
 .UNSPECIFIED. ) ;
#52848 = CARTESIAN_POINT ( 'NONE',  ( 11.30565467195989093, -5.136173005413446013, -6.911917091190548312 ) ) ;
#52849 = VERTEX_POINT ( 'NONE', #16712 ) ;
#52850 = CARTESIAN_POINT ( 'NONE',  ( 0.7380637418424000895, 3.204751743350000126, -0.5916681129576000231 ) ) ;
#52851 = CARTESIAN_POINT ( 'NONE',  ( 10.37309687351658383, 2.782534154164606921, 7.827184855449101697 ) ) ;
#52852 = FACE_OUTER_BOUND ( 'NONE', #43649, .T. ) ;
#52853 = CARTESIAN_POINT ( 'NONE',  ( 10.03293802597399953, 3.549239910423600097, 8.240623579255899500 ) ) ;
#52854 = DIRECTION ( 'NONE',  ( 0.000000000000000000, -0.06400262754467088422, -0.9979497300302145879 ) ) ;
#52855 = CARTESIAN_POINT ( 'NONE',  ( 12.20884949286986831, -2.312191565065524035, 13.71150332431687424 ) ) ;
#52856 = CARTESIAN_POINT ( 'NONE',  ( 12.26374059927404403, 2.812587984009075726, 13.60212386631915571 ) ) ;
#52857 = CARTESIAN_POINT ( 'NONE',  ( 23.68244710019300214, 3.146849026561000073, -13.35211358126000114 ) ) ;
#52858 = ORIENTED_EDGE ( 'NONE', *, *, #28453, .T. ) ;
#52859 = CIRCLE ( 'NONE', #39436, 1.249999999999999778 ) ;
#52860 = CARTESIAN_POINT ( 'NONE',  ( 4.945374320980000071, -1.099255157290000007, -0.6468487824790000174 ) ) ;
#52861 = CARTESIAN_POINT ( 'NONE',  ( 8.541480666858999982, -3.573487373903700082, -8.706015266875999359 ) ) ;
#52862 = AXIS2_PLACEMENT_3D ( 'NONE', #64864, #39014, #16977 ) ;
#52863 = CARTESIAN_POINT ( 'NONE',  ( 23.60000000000000142, -9.289189189551001036, -7.908916752675001050 ) ) ;
#52864 = CARTESIAN_POINT ( 'NONE',  ( 17.78683280784126097, 3.080523647204255866, -12.29718062304645798 ) ) ;
#52865 = CARTESIAN_POINT ( 'NONE',  ( 25.60000000000000142, 8.527654132752997995, -7.260537518969999660 ) ) ;
#52866 = CARTESIAN_POINT ( 'NONE',  ( 18.17813913393023384, 2.550022942068608689, 12.43977370304579644 ) ) ;
#52867 = EDGE_CURVE ( 'NONE', #41725, #26079, #11467, .T. ) ;
#52868 = CARTESIAN_POINT ( 'NONE',  ( 10.90000000000000036, -2.832432432432000269, -6.822293592207000934 ) ) ;
#52869 = DIRECTION ( 'NONE',  ( -0.8660254037844968833, 0.000000000000000000, 0.4999999999998989142 ) ) ;
#52870 = CARTESIAN_POINT ( 'NONE',  ( 8.433148997460000018, 5.167567567567999731, 6.822293592207000934 ) ) ;
#52871 = CYLINDRICAL_SURFACE ( 'NONE', #61215, 1.999999999999999556 ) ;
#52872 = EDGE_CURVE ( 'NONE', #22245, #61548, #48927, .T. ) ;
#52873 = DIRECTION ( 'NONE',  ( -0.7071069400700297214, 0.7071066223030297859, 2.150916229665089677E-09 ) ) ;
#52874 = EDGE_CURVE ( 'NONE', #28855, #29023, #17058, .T. ) ;
#52875 = CARTESIAN_POINT ( 'NONE',  ( 24.03569645326925297, 9.310050201079944188, -9.237031074784450624 ) ) ;
#52876 = CARTESIAN_POINT ( 'NONE',  ( 11.32299956498189886, -5.207010770456999893, -7.174999999999999822 ) ) ;
#52877 = CARTESIAN_POINT ( 'NONE',  ( 23.58681904253500150, 13.29342458620000045, -4.187351535191000451 ) ) ;
#52878 = ORIENTED_EDGE ( 'NONE', *, *, #68898, .T. ) ;
#52879 = CARTESIAN_POINT ( 'NONE',  ( 8.813304719595000947, 3.880154689736000417, -9.060377011187000562 ) ) ;
#52880 = CARTESIAN_POINT ( 'NONE',  ( 11.42441504065829960, -3.305585767322499979, 8.017771632862299214 ) ) ;
#52881 = ORIENTED_EDGE ( 'NONE', *, *, #52872, .T. ) ;
#52882 = CARTESIAN_POINT ( 'NONE',  ( 24.96666885024123417, 10.83443035737135851, -3.855530940255541772 ) ) ;
#52883 = CARTESIAN_POINT ( 'NONE',  ( 10.69456919669529960, -2.906008650422999828, -7.823222900359999343 ) ) ;
#52884 = ORIENTED_EDGE ( 'NONE', *, *, #46056, .T. ) ;
#52885 = DIRECTION ( 'NONE',  ( 1.000000000000000000, 0.000000000000000000, 0.000000000000000000 ) ) ;
#52886 = CARTESIAN_POINT ( 'NONE',  ( 8.646410841231000788, 2.261390688294000029, -6.733978371730000134 ) ) ;
#52887 = CARTESIAN_POINT ( 'NONE',  ( 17.79319863334400154, -3.315493116453000155, 11.22361396466000016 ) ) ;
#52888 = CARTESIAN_POINT ( 'NONE',  ( 10.44125056272499918, -2.966599088466999934, -7.515315513715298934 ) ) ;
#52889 = CARTESIAN_POINT ( 'NONE',  ( 9.852263540182327972, -5.092232985442820770, -6.870476274536370553 ) ) ;
#52890 = CARTESIAN_POINT ( 'NONE',  ( 7.000000000000000000, -7.356634010774431687, -3.356634010774432575 ) ) ;
#52891 = CARTESIAN_POINT ( 'NONE',  ( 12.97447410014400226, 11.72278459482000024, 1.967342116188999679 ) ) ;
#52892 = VERTEX_POINT ( 'NONE', #22307 ) ;
#52894 = CARTESIAN_POINT ( 'NONE',  ( 10.11094409420000062, 5.100000000000000533, -6.571291218949999902 ) ) ;
#52893 = B_SPLINE_CURVE_WITH_KNOTS ( 'NONE', 3,
 ( #51755, #46863, #9105, #3849 ),
 .UNSPECIFIED., .F., .F.,
 ( 4, 4 ),
 ( 0.000000000000000000, 1.000000000000000000 ),
 .UNSPECIFIED. ) ;
#52895 = ORIENTED_EDGE ( 'NONE', *, *, #3546, .F. ) ;
#52896 = EDGE_CURVE ( 'NONE', #18236, #14432, #834, .T. ) ;
#52897 = CARTESIAN_POINT ( 'NONE',  ( 10.88351354018293904, 2.750000000000000000, -7.336375382625530683 ) ) ;
#52898 =( LENGTH_UNIT ( ) NAMED_UNIT ( * ) SI_UNIT ( .MILLI., .METRE. ) );
#52899 = ORIENTED_EDGE ( 'NONE', *, *, #41458, .T. ) ;
#52900 = CARTESIAN_POINT ( 'NONE',  ( 9.706621437244999484, 4.849675135054999586, 8.456261759323901117 ) ) ;
#52901 = B_SPLINE_CURVE_WITH_KNOTS ( 'NONE', 3,
 ( #68978, #14815, #62361, #40690, #26340, #25992, #4652, #31247, #57112, #62020, #52555, #36138 ),
 .UNSPECIFIED., .F., .F.,
 ( 4, 2, 2, 2, 2, 4 ),
 ( 0.000000000000000000, 0.2500000000000010547, 0.3750000000000015543, 0.5000000000000021094, 0.7500000000000009992, 1.000000000000000000 ),
 .UNSPECIFIED. ) ;
#52902 = CARTESIAN_POINT ( 'NONE',  ( 18.05239999627277214, -2.879049404332130191, -12.35514073459315654 ) ) ;
#52903 = CARTESIAN_POINT ( 'NONE',  ( 18.30002258771995471, 11.69706282806914288, -3.884923957652766102 ) ) ;
#52904 = B_SPLINE_SURFACE_WITH_KNOTS ( 'NONE', 3, 3, ( 
 ( #33507, #45032, #2718, #12521, #60756, #17418, #39784, #50616, #28254, #43996, #1684, #33852, #28611, #13226, #12871, #1334, #7620, #2375, #24042, #55166, #6922, #12177, #49227, #7271, #39091, #28966, #22651, #7969, #34199, #50271, #29305, #45377, #60416, #13567, #23698 ),
 ( #49925, #23354, #18117, #2036, #18808, #40135, #66337, #66684, #23001, #34887, #65303, #44696, #18461, #38744, #65991, #61106, #56203, #39435, #44350, #34553, #8311, #54823, #60073, #55863, #65649, #61449, #49574, #17773, #35906, #41496, #62128, #24732, #36598, #52329, #19831 ),
 ( #62807, #67704, #30667, #8988, #3735, #50958, #63147, #4424, #9669, #14926, #19137, #67362, #51299, #3395, #46059, #19485, #25762, #8651, #40459, #46749, #61786, #45718, #15274, #36249, #40806, #35233, #68054, #47092, #57924, #24387, #68392, #20168, #51975, #20512, #14248 ),
 ( #13905, #57569, #56545, #67027, #29657, #31020, #35575, #29999, #41838, #3056, #56891, #30330, #51638, #25069, #4077, #46403, #41162, #62468, #14588, #57221, #25415, #9323, #53366, #47433, #16297, #48119, #27486, #10705, #20859, #920, #223, #21884, #32050, #21200, #21540 ) ),
 .UNSPECIFIED., .F., .F., .F.,
 ( 4, 4 ),
 ( 4, 1, 1, 1, 1, 1, 1, 1, 1, 1, 1, 1, 1, 1, 1, 1, 1, 1, 1, 1, 1, 1, 1, 1, 1, 1, 1, 1, 1, 1, 1, 1, 4 ),
 ( -0.1039086239011999951, 1.103908623900999864 ),
 ( -0.02000000000000000042, 0.01250000000000000069, 0.04499999999999999833, 0.07749999999999999944, 0.1100000000000000006, 0.1424999999999999878, 0.1749999999999999889, 0.2074999999999999900, 0.2399999999999999911, 0.2725000000000000200, 0.3049999999999999933, 0.3375000000000000222, 0.3699999999999999956, 0.4025000000000000244, 0.4349999999999999978, 0.4675000000000000266, 0.5000000000000000000, 0.5324999999999999734, 0.5649999999999999467, 0.5975000000000000311, 0.6300000000000000044, 0.6624999999999999778, 0.6949999999999999512, 0.7275000000000000355, 0.7600000000000000089, 0.7924999999999999822, 0.8249999999999999556, 0.8575000000000000400, 0.8900000000000000133, 0.9224999999999999867, 0.9549999999999999600, 0.9875000000000000444, 1.020000000000000018 ),
 .UNSPECIFIED. ) ;
#52905 = CARTESIAN_POINT ( 'NONE',  ( 8.447783767286816570, -5.285582108569009563, 7.027722483016056287 ) ) ;
#52906 = CARTESIAN_POINT ( 'NONE',  ( 10.44608131895000191, -8.241816726637999579, -6.830402593584000925 ) ) ;
#52907 = CONICAL_SURFACE ( 'NONE', #31701, 12.42518024156999878, 0.7854126340177727261 ) ;
#52908 = ORIENTED_EDGE ( 'NONE', *, *, #47610, .F. ) ;
#52909 = CARTESIAN_POINT ( 'NONE',  ( 12.13343030045100157, 11.60886806805999960, -4.031065632098000506 ) ) ;
#52910 = CARTESIAN_POINT ( 'NONE',  ( 17.61515110739400214, 11.44262809724999919, -4.698133467368000638 ) ) ;
#52911 = CARTESIAN_POINT ( 'NONE',  ( 17.55505043854147118, -1.760910691117812954, -12.47634535983622861 ) ) ;
#52912 = CARTESIAN_POINT ( 'NONE',  ( 11.00000000000000000, -4.968589424331200100, -7.174999999999999822 ) ) ;
#52913 = AXIS2_PLACEMENT_3D ( 'NONE', #35470, #56792, #61684 ) ;
#52914 = CARTESIAN_POINT ( 'NONE',  ( 9.942214158770999788, 3.986577607995999806, -9.280166295424001177 ) ) ;
#52915 = CARTESIAN_POINT ( 'NONE',  ( 18.17677363193000062, -3.419785592864999835, 11.99291007725999947 ) ) ;
#52916 = CARTESIAN_POINT ( 'NONE',  ( 10.40879003340999986, -3.093879171920000282, -6.480773124728999690 ) ) ;
#52917 = EDGE_LOOP ( 'NONE', ( #48898, #2188, #24774, #44147, #28610, #38340, #5502 ) ) ;
#52918 = VERTEX_POINT ( 'NONE', #33505 ) ;
#52919 = DIRECTION ( 'NONE',  ( 0.000000000000000000, 1.000000000000000000, 0.000000000000000000 ) ) ;
#52920 = EDGE_CURVE ( 'NONE', #43147, #35517, #45594, .T. ) ;
#52921 = DIRECTION ( 'NONE',  ( 1.000000000000000000, 0.000000000000000000, 0.000000000000000000 ) ) ;
#52922 = CARTESIAN_POINT ( 'NONE',  ( 12.34854013679586160, -2.926988005537949800, 13.57357535316058694 ) ) ;
#52923 = CARTESIAN_POINT ( 'NONE',  ( 6.032109839683332808, -0.9218200799623775810, 1.199500263597266247 ) ) ;
#52924 = CARTESIAN_POINT ( 'NONE',  ( 11.51656039236534923, 5.173498198882000132, -7.557111631074219460 ) ) ;
#52925 = CARTESIAN_POINT ( 'NONE',  ( 9.130088727410999638, 3.136022381937999981, -7.572461161969050281 ) ) ;
#52927 = CARTESIAN_POINT ( 'NONE',  ( 10.26106145044999884, -3.441494892447000353, 4.532186341712000299 ) ) ;
#52926 = CARTESIAN_POINT ( 'NONE',  ( 9.673759580228999511, -4.976892840331100132, 7.733500918284399894 ) ) ;
#52928 = CARTESIAN_POINT ( 'NONE',  ( 7.790168786842999182, -2.923571394339999685, 6.474157094959999803 ) ) ;
#52929 = ORIENTED_EDGE ( 'NONE', *, *, #29463, .F. ) ;
#52930 = CARTESIAN_POINT ( 'NONE',  ( 9.821013540182335078, 3.231816600031359510, -6.500416447002272946 ) ) ;
#52931 = AXIS2_PLACEMENT_3D ( 'NONE', #34918, #2745, #19166 ) ;
#52932 = CARTESIAN_POINT ( 'NONE',  ( 7.861945368778997079, -2.855203060631998024, 6.787771340568003353 ) ) ;
#52933 = CARTESIAN_POINT ( 'NONE',  ( 9.800903104272999045, -2.772050158355999994, -8.125211791007998841 ) ) ;
#52934 = CARTESIAN_POINT ( 'NONE',  ( 11.91486084871699802, -5.207010770456999893, 7.174999999999999822 ) ) ;
#52935 = CARTESIAN_POINT ( 'NONE',  ( 9.905786073958001481, -2.698967003257000119, 8.979227319929000473 ) ) ;
#52936 = CARTESIAN_POINT ( 'NONE',  ( 10.86209373942999967, -5.065348428249999202, 5.178139088298999937 ) ) ;
#52937 = CARTESIAN_POINT ( 'NONE',  ( 16.00249209530700156, -3.346223412964000055, -11.40475585647000045 ) ) ;
#52938 = CIRCLE ( 'NONE', #64159, 2.725000000000000089 ) ;
#52939 = CARTESIAN_POINT ( 'NONE',  ( 25.59994555223599733, 10.55174472786000095, -3.754934689065000164 ) ) ;
#52940 = CARTESIAN_POINT ( 'NONE',  ( 7.976952457388438944, 3.338438528537961858, -6.270514789011116363 ) ) ;
#52941 = CARTESIAN_POINT ( 'NONE',  ( 9.991279731608999626, -3.922199073804859992, -6.636486849903699969 ) ) ;
#52942 = CARTESIAN_POINT ( 'NONE',  ( 10.89393020684999946, -5.250000000000000000, 7.500000000000000000 ) ) ;
#52943 = DIRECTION ( 'NONE',  ( 2.186552006505935969E-10, 0.9979498542811704453, -0.06400069015401811667 ) ) ;
#52944 = CARTESIAN_POINT ( 'NONE',  ( 5.534341696747668848, 12.89488364838971712, -2.703816490859269894 ) ) ;
#52945 = CARTESIAN_POINT ( 'NONE',  ( 11.79999999771000141, 12.39026187696000036, 1.832249219479999969 ) ) ;
#52946 = ORIENTED_EDGE ( 'NONE', *, *, #52309, .F. ) ;
#52947 = CARTESIAN_POINT ( 'NONE',  ( 12.35550214789977908, 0.4343244881883154274, -12.69000555157927757 ) ) ;
#52948 = CARTESIAN_POINT ( 'NONE',  ( 12.21857308197977687, -2.283092344262311002, -12.49946922047021225 ) ) ;
#52949 = DIRECTION ( 'NONE',  ( -1.000000000000000000, 0.000000000000000000, 0.000000000000000000 ) ) ;
#52950 = CARTESIAN_POINT ( 'NONE',  ( 5.199999999795999805, 0.2499999997964000020, -9.776630293835998131 ) ) ;
#52951 = CARTESIAN_POINT ( 'NONE',  ( 1.592640132540833253, 3.058252359239899132, 1.762666431298155034 ) ) ;
#52952 = ORIENTED_EDGE ( 'NONE', *, *, #60387, .T. ) ;
#52953 = FACE_OUTER_BOUND ( 'NONE', #27115, .T. ) ;
#52954 = CONTEXT_DEPENDENT_SHAPE_REPRESENTATION ( #36043, #24350 ) ;
#52955 = EDGE_CURVE ( 'NONE', #38520, #2626, #29996, .T. ) ;
#52956 = CARTESIAN_POINT ( 'NONE',  ( 17.55505043854143565, 1.875000000000000000, 13.78627172894481667 ) ) ;
#52957 = CARTESIAN_POINT ( 'NONE',  ( 18.17506407532043866, 0.08141364314609686459, 12.69967032936880713 ) ) ;
#52958 = DIRECTION ( 'NONE',  ( 0.3139086814191160424, 2.556637375876062946E-07, -0.9494531793246292484 ) ) ;
#52959 = CARTESIAN_POINT ( 'NONE',  ( 7.723040328487922324, 3.449924197545608084, -8.750316711071878473 ) ) ;
#52960 = CARTESIAN_POINT ( 'NONE',  ( 10.52435971519499880, 4.532462039660099862, -6.614211617270199461 ) ) ;
#52961 = VERTEX_POINT ( 'NONE', #51296 ) ;
#52962 = AXIS2_PLACEMENT_3D ( 'NONE', #64859, #48110, #42520 ) ;
#52963 = CARTESIAN_POINT ( 'NONE',  ( 25.60000000000000142, 9.517611874540000017, -8.103398312166000039 ) ) ;
#52964 = CARTESIAN_POINT ( 'NONE',  ( 18.05225003025148922, 2.879247418710621176, -13.58568546892325557 ) ) ;
#52965 = ORIENTED_EDGE ( 'NONE', *, *, #21601, .T. ) ;
#52966 = CARTESIAN_POINT ( 'NONE',  ( 13.09269116697131885, 11.52576810756814751, 1.696811579065023556 ) ) ;
#52967 = CARTESIAN_POINT ( 'NONE',  ( 8.508081853209001011, -2.202816532622999812, 7.706987678916999762 ) ) ;
#52968 = CARTESIAN_POINT ( 'NONE',  ( 15.95296092448800174, 8.433319028468000411, 8.247373098099998856 ) ) ;
#52969 = ORIENTED_EDGE ( 'NONE', *, *, #42796, .T. ) ;
#52970 = CARTESIAN_POINT ( 'NONE',  ( 16.39999999347100257, 3.345256695718999751, 11.86066175541999890 ) ) ;
#52971 = CARTESIAN_POINT ( 'NONE',  ( 6.736329719590999687, 5.216734614776999734, -8.484106667489999865 ) ) ;
#52972 = CARTESIAN_POINT ( 'NONE',  ( 23.56665676678700194, 0.000000000000000000, -3.819167204710999951E-13 ) ) ;
#52973 = CARTESIAN_POINT ( 'NONE',  ( 9.464429763972951548, 5.182499815101167862, 8.153205832973403844 ) ) ;
#52974 = ORIENTED_EDGE ( 'NONE', *, *, #37341, .T. ) ;
#52975 = CARTESIAN_POINT ( 'NONE',  ( 9.724613486786999772, -2.928302463146000179, 8.718481221599999387 ) ) ;
#52976 = CARTESIAN_POINT ( 'NONE',  ( 25.08549704953700044, 11.33427520304999980, -3.320998664874999839 ) ) ;
#52977 = DIRECTION ( 'NONE',  ( 1.000000000000000000, 0.000000000000000000, 0.000000000000000000 ) ) ;
#52978 = EDGE_LOOP ( 'NONE', ( #4711, #55120, #51548, #27891 ) ) ;
#52979 = EDGE_CURVE ( 'NONE', #47790, #53063, #56200, .T. ) ;
#52980 = CIRCLE ( 'NONE', #28436, 12.50000000000000000 ) ;
#52981 = CYLINDRICAL_SURFACE ( 'NONE', #67154, 10.75000000000000000 ) ;
#52982 = ORIENTED_EDGE ( 'NONE', *, *, #61176, .F. ) ;
#52983 = DIRECTION ( 'NONE',  ( 0.000000000000000000, -1.000000000000000000, 0.000000000000000000 ) ) ;
#52984 = CARTESIAN_POINT ( 'NONE',  ( 18.17506427775392197, 0.08141198804361876595, -13.89969880262316337 ) ) ;
#52985 = EDGE_CURVE ( 'NONE', #46630, #9447, #13223, .T. ) ;
#52986 = CARTESIAN_POINT ( 'NONE',  ( 11.54292372906209074, 5.032542535543790052, -8.269164421058194492 ) ) ;
#52987 = CONICAL_SURFACE ( 'NONE', #22832, 2.050034397132999953, 0.7853981633972997312 ) ;
#52988 = CARTESIAN_POINT ( 'NONE',  ( 5.271693173017333756, 0.7554284705563509839, -1.310679582531385945 ) ) ;
#52989 = DIRECTION ( 'NONE',  ( -0.000000000000000000, -0.000000000000000000, 1.000000000000000000 ) ) ;
#52990 = CARTESIAN_POINT ( 'NONE',  ( 24.03543903504724355, 12.65494737823116012, 3.444447339656595553 ) ) ;
#52991 = CARTESIAN_POINT ( 'NONE',  ( 7.000000000000000000, 3.640000000000000124, -3.000000000000000000 ) ) ;
#52992 = EDGE_LOOP ( 'NONE', ( #55922, #31410, #4132 ) ) ;
#52993 = CARTESIAN_POINT ( 'NONE',  ( 10.32169598648999909, -3.233475335853099875, -7.956401575444799867 ) ) ;
#52994 = ORIENTED_EDGE ( 'NONE', *, *, #67430, .F. ) ;
#52995 = CARTESIAN_POINT ( 'NONE',  ( 11.11504246380000005, 3.456610836627000083, 5.970339330302000036 ) ) ;
#52996 = DIRECTION ( 'NONE',  ( 1.000000000000000000, 0.000000000000000000, 0.000000000000000000 ) ) ;
#52997 = AXIS2_PLACEMENT_3D ( 'NONE', #67743, #62506, #15653 ) ;
#52998 = LINE ( 'NONE', #51613, #44526 ) ;
#52999 = CARTESIAN_POINT ( 'NONE',  ( 9.667010841233000917, 4.769103072373000352, -8.666849124598000387 ) ) ;
#53000 = DIRECTION ( 'NONE',  ( -1.000000000000000000, 0.000000000000000000, 0.000000000000000000 ) ) ;
#53001 = CARTESIAN_POINT ( 'NONE',  ( 25.52346828417099900, 2.888732412976000141, 11.27716578594000119 ) ) ;
#53002 = CARTESIAN_POINT ( 'NONE',  ( 17.57569743819256658, -0.6249994633519876386, 13.88107975068473365 ) ) ;
#53003 = CARTESIAN_POINT ( 'NONE',  ( 9.258050732556000639, -4.895927245463000510, -6.008721945297999412 ) ) ;
#53004 = ORIENTED_EDGE ( 'NONE', *, *, #45065, .T. ) ;
#53005 = CARTESIAN_POINT ( 'NONE',  ( 12.41700012676155218, 0.4899485149124510608, 13.88837626668677316 ) ) ;
#53006 = CARTESIAN_POINT ( 'NONE',  ( 12.11759063708296047, -2.782734359457999851, 7.157757529645699890 ) ) ;
#53007 = CARTESIAN_POINT ( 'NONE',  ( 11.51961669203094196, -2.969723712172476215, -7.175016092226064401 ) ) ;
#53008 = CARTESIAN_POINT ( 'NONE',  ( 18.09811766381520215, -0.3100353843471406190, -13.89536095208329236 ) ) ;
#53009 = CARTESIAN_POINT ( 'NONE',  ( 7.127706853208000126, -4.698358408974000255, 8.789434435623999065 ) ) ;
#53011 = CARTESIAN_POINT ( 'NONE',  ( 10.27164068752446902, -2.873222873891751572, 6.752018918739129738 ) ) ;
#53010 = DIRECTION ( 'NONE',  ( 0.000000000000000000, -0.1218274111675001353, 0.9925512993736016476 ) ) ;
#53012 = AXIS2_PLACEMENT_3D ( 'NONE', #28347, #11909, #22740 ) ;
#53013 = CARTESIAN_POINT ( 'NONE',  ( 10.34995525820099971, 3.892289273474800471, -6.364355462479999836 ) ) ;
#53014 = CARTESIAN_POINT ( 'NONE',  ( 15.40000000001299973, -8.815237407733999220, -7.616696375847999967 ) ) ;
#53015 = PRODUCT_DEFINITION_FORMATION_WITH_SPECIFIED_SOURCE ( 'ANY', '', #35538, .NOT_KNOWN. ) ;
#53016 = CARTESIAN_POINT ( 'NONE',  ( 8.869809814040998219, 4.614409247670200109, -8.294571108394100278 ) ) ;
#53017 = CARTESIAN_POINT ( 'NONE',  ( 18.13088395572279410, 0.4376617689587105064, 12.59240970319242869 ) ) ;
#53018 = CARTESIAN_POINT ( 'NONE',  ( 7.015118664308999996, 0.6487287962077999959, 1.256367379015999930 ) ) ;
#53019 = FACE_OUTER_BOUND ( 'NONE', #60129, .T. ) ;
#53020 = ORIENTED_EDGE ( 'NONE', *, *, #27794, .T. ) ;
#53021 = CARTESIAN_POINT ( 'NONE',  ( 9.304730646793998972, -5.284133759825000887, 6.489273023403000273 ) ) ;
#53022 = CARTESIAN_POINT ( 'NONE',  ( 9.617764158771999305, 5.322769172805999816, -7.951018786192998178 ) ) ;
#53023 = CARTESIAN_POINT ( 'NONE',  ( 21.72233714749290101, 0.000000000000000000, 0.000000000000000000 ) ) ;
#53024 = CARTESIAN_POINT ( 'NONE',  ( 4.600001223043999943, 0.000000000000000000, 0.000000000000000000 ) ) ;
#53025 = ORIENTED_EDGE ( 'NONE', *, *, #16665, .F. ) ;
#53026 = B_SPLINE_CURVE_WITH_KNOTS ( 'NONE', 3,
 ( #17734, #66300, #35194, #18077, #34159, #51263, #66649, #45339, #18768, #39399, #8269, #40097, #3359, #39055, #13529, #60376, #29266, #2337 ),
 .UNSPECIFIED., .F., .F.,
 ( 4, 2, 2, 2, 2, 2, 2, 2, 4 ),
 ( 0.000000000000000000, 0.06250000000000112410, 0.1250000000000022482, 0.2500000000000026090, 0.5000000000000021094, 0.7500000000000015543, 0.8750000000000019984, 0.9375000000000009992, 1.000000000000000000 ),
 .UNSPECIFIED. ) ;
#53027 = CARTESIAN_POINT ( 'NONE',  ( 10.67905590578999941, 2.899999999999999911, 6.571291218949999902 ) ) ;
#53028 = CIRCLE ( 'NONE', #54170, 11.65000000000000036 ) ;
#53029 = CARTESIAN_POINT ( 'NONE',  ( 11.48522412107029922, 4.047131449166419870, 8.390877922225699947 ) ) ;
#53030 = CARTESIAN_POINT ( 'NONE',  ( 10.42512334122999995, 3.371064118627999928, -6.294343971198999910 ) ) ;
#53031 = ORIENTED_EDGE ( 'NONE', *, *, #6613, .T. ) ;
#53032 = CARTESIAN_POINT ( 'NONE',  ( 8.912651967921339846, 2.899999999999999911, 6.383937126463831824 ) ) ;
#53033 = CARTESIAN_POINT ( 'NONE',  ( 24.30000564989370204, 3.240508264636430713, -12.09374148597397891 ) ) ;
#53034 = CARTESIAN_POINT ( 'NONE',  ( 10.25149413291699929, 5.037815157227999663, 7.973529073237199505 ) ) ;
#53035 = CARTESIAN_POINT ( 'NONE',  ( 7.121419741036552509, -3.646617224772007670, 8.816373456089998228 ) ) ;
#53036 = CARTESIAN_POINT ( 'NONE',  ( 8.271698341229999585, 5.629399530851999955, 8.631829656822000985 ) ) ;
#53037 = VERTEX_POINT ( 'NONE', #24384 ) ;
#53038 = CARTESIAN_POINT ( 'NONE',  ( 7.844724262280000637, -4.719412258162999585, 6.357657668295000342 ) ) ;
#53039 = EDGE_CURVE ( 'NONE', #8953, #47157, #12092, .T. ) ;
#53040 = EDGE_CURVE ( 'NONE', #5919, #60348, #17689, .T. ) ;
#53041 = CARTESIAN_POINT ( 'NONE',  ( 7.748070280408000166, 2.435036720175999925, -7.494591853605999887 ) ) ;
#53042 = CARTESIAN_POINT ( 'NONE',  ( 8.414467752718078231, -2.422965004064780103, 8.233303954855905715 ) ) ;
#53043 = CARTESIAN_POINT ( 'NONE',  ( 9.446747021775999897, -4.961496216383199709, 6.656252755052399550 ) ) ;
#53044 = VERTEX_POINT ( 'NONE', #45715 ) ;
#53045 = DIRECTION ( 'NONE',  ( -0.7660444387781886189, 2.249698893085964329E-11, -0.6427876148596907147 ) ) ;
#53046 = CARTESIAN_POINT ( 'NONE',  ( 11.82333928233100018, 11.49420271256999904, 1.652349626741000055 ) ) ;
#53047 = ORIENTED_EDGE ( 'NONE', *, *, #32770, .T. ) ;
#53048 = CARTESIAN_POINT ( 'NONE',  ( 24.65659773182258974, 3.152267499950374141, -11.84443715742482084 ) ) ;
#53049 = CARTESIAN_POINT ( 'NONE',  ( 16.39999999347100257, -3.345256695718999751, -11.86066175541999890 ) ) ;
#53050 = CARTESIAN_POINT ( 'NONE',  ( 7.800894438721999613, -3.218815632501999868, 6.398977300879999497 ) ) ;
#53051 = CARTESIAN_POINT ( 'NONE',  ( 9.932908211424001266, -3.485164486501000081, -6.221839249167999242 ) ) ;
#53052 = CARTESIAN_POINT ( 'NONE',  ( 9.733249152250484926, -4.120954265945523609, -8.873128867233456063 ) ) ;
#53053 = CARTESIAN_POINT ( 'NONE',  ( 10.72702344389999851, 2.995605560827999891, -6.890449684422599752 ) ) ;
#53054 = CARTESIAN_POINT ( 'NONE',  ( 12.01145123989533126, -3.394760891061399999, 6.331134574721999364 ) ) ;
#53055 = CARTESIAN_POINT ( 'NONE',  ( 8.835539685685773748, -3.765107182069276526, 9.264007590920439128 ) ) ;
#53056 = CARTESIAN_POINT ( 'NONE',  ( 11.65810538575740019, -2.757018958839999812, 7.797177576385699638 ) ) ;
#53057 = VERTEX_POINT ( 'NONE', #8308 ) ;
#53058 = CARTESIAN_POINT ( 'NONE',  ( 7.512829719590000010, 5.524123123935000379, 6.910361319981999095 ) ) ;
#53059 = VERTEX_POINT ( 'NONE', #50955 ) ;
#53060 = LINE ( 'NONE', #58298, #30685 ) ;
#53061 = CARTESIAN_POINT ( 'NONE',  ( 8.924662153698969647, 5.350575487761837223, 7.500021879703680838 ) ) ;
#53062 = CARTESIAN_POINT ( 'NONE',  ( 11.12487846393999824, 5.426360382733999899, -5.164845216807000483 ) ) ;
#53063 = VERTEX_POINT ( 'NONE', #24039 ) ;
#53064 = B_SPLINE_SURFACE_WITH_KNOTS ( 'NONE', 3, 3, ( 
 ( #30354, #3082, #57588, #35931 ),
 ( #9696, #40487, #8338, #50985 ),
 ( #24415, #31042, #35600, #25096 ),
 ( #3421, #62829, #2742, #34915 ),
 ( #3757, #36273, #13930, #24068 ),
 ( #24756, #19853, #41182, #19162 ),
 ( #41518, #67729, #45403, #46082 ),
 ( #56914, #66712, #19511, #40829 ),
 ( #56229, #62154, #14613, #30689 ),
 ( #57244, #61813, #14272, #67389 ),
 ( #18833, #13594, #9013, #9345 ) ),
 .UNSPECIFIED., .F., .F., .F.,
 ( 4, 1, 1, 1, 1, 1, 1, 1, 4 ),
 ( 4, 4 ),
 ( -0.01375657147579999878, 0.000000000000000000, 0.06250000000000000000, 0.1250000000000000000, 0.1875000000000000000, 0.2500000000000000000, 0.3125000000000000000, 0.3750000000000000000, 0.4325988669058000169 ),
 ( -0.1687363430499000116, 1.168634397496999933 ),
 .UNSPECIFIED. ) ;
#53065 = CARTESIAN_POINT ( 'NONE',  ( 12.18425839594608995, -2.573099938722084534, -12.43423733299712985 ) ) ;
#53066 = EDGE_CURVE ( 'NONE', #30735, #4878, #4170, .T. ) ;
#53067 = CARTESIAN_POINT ( 'NONE',  ( 17.89269116643086122, 3.351202196788891197, 11.15759579123215950 ) ) ;
#53068 = CARTESIAN_POINT ( 'NONE',  ( 11.09999999999999964, -4.000000000000000000, -7.500000000000000000 ) ) ;
#53069 = PLANE ( 'NONE',  #33072 ) ;
#53070 = CARTESIAN_POINT ( 'NONE',  ( 12.16922513814163054, -2.166987123599049436, -13.83127908232058267 ) ) ;
#53071 = CARTESIAN_POINT ( 'NONE',  ( 11.75718044953559804, -3.110233631466100324, -7.963966784336999005 ) ) ;
#53072 = DIRECTION ( 'NONE',  ( 0.000000000000000000, 1.000000000000000000, 0.000000000000000000 ) ) ;
#53073 = CARTESIAN_POINT ( 'NONE',  ( 18.20778913885557415, -2.166651812353031392, 12.41232206190563048 ) ) ;
#53074 = VERTEX_POINT ( 'NONE', #29302 ) ;
#53075 = EDGE_LOOP ( 'NONE', ( #28911, #19409, #35799, #21850 ) ) ;
#53076 = DIRECTION ( 'NONE',  ( 1.000000000000000000, 0.000000000000000000, 0.000000000000000000 ) ) ;
#53077 = DIRECTION ( 'NONE',  ( 0.000000000000000000, 1.000000000000000000, 0.000000000000000000 ) ) ;
#53078 = LINE ( 'NONE', #36659, #31623 ) ;
#53079 = CARTESIAN_POINT ( 'NONE',  ( 10.13061872827999998, 2.189311095934999951, -7.101639631284999865 ) ) ;
#53080 = LINE ( 'NONE', #5863, #35459 ) ;
#53081 = VECTOR ( 'NONE', #55968, 1000.000000000000114 ) ;
#53082 = CARTESIAN_POINT ( 'NONE',  ( 18.14748133480223302, 2.299853946629115686, -12.49599191558583655 ) ) ;
#53083 = CARTESIAN_POINT ( 'NONE',  ( 8.168244718249995984, 3.088031253505000961, -6.162676582372005996 ) ) ;
#53084 = CARTESIAN_POINT ( 'NONE',  ( 8.811649685568998080, 4.101356036306899711, -8.457700632733599733 ) ) ;
#53085 = EDGE_LOOP ( 'NONE', ( #40151, #26146, #56544, #26479, #50343 ) ) ;
#53086 = DIRECTION ( 'NONE',  ( -1.000000000000000000, 0.000000000000000000, 0.000000000000000000 ) ) ;
#53087 = CARTESIAN_POINT ( 'NONE',  ( 12.39876276414171485, -2.975035832937171776, 12.32812070139215521 ) ) ;
#53088 = CYLINDRICAL_SURFACE ( 'NONE', #18111, 14.00000000000000000 ) ;
#53089 = CARTESIAN_POINT ( 'NONE',  ( 10.52323372634000087, 3.325642821414999784, 5.689987891230000372 ) ) ;
#53090 = CARTESIAN_POINT ( 'NONE',  ( 10.94635971519499940, -3.540377183549800133, 8.264615166761799969 ) ) ;
#53091 = CARTESIAN_POINT ( 'NONE',  ( 7.234321569752399483, 0.04198228903204147960, 1.193235013897578245 ) ) ;
#53092 = CARTESIAN_POINT ( 'NONE',  ( 11.73671932425159881, 3.872987101045399783, -8.356835045446798560 ) ) ;
#53093 = CARTESIAN_POINT ( 'NONE',  ( 11.07253275740080234, 2.278112260258351007, -7.888934961064568263 ) ) ;
#53094 = EDGE_CURVE ( 'NONE', #40232, #52776, #18440, .T. ) ;
#53095 = EDGE_CURVE ( 'NONE', #59582, #14991, #13209, .T. ) ;
#53096 = CARTESIAN_POINT ( 'NONE',  ( 8.195614351789243912, 4.733557677076899672, -8.663326391184606123 ) ) ;
#53097 = CARTESIAN_POINT ( 'NONE',  ( 18.43329219593509549, -2.701919656448346974, -11.40083085748004876 ) ) ;
#53098 = CARTESIAN_POINT ( 'NONE',  ( 9.213774118050919171, -2.663711227152621763, 7.691546656787776826 ) ) ;
#53099 = ORIENTED_EDGE ( 'NONE', *, *, #25252, .T. ) ;
#53100 = DIRECTION ( 'NONE',  ( 0.000000000000000000, -1.000000000000000000, 0.000000000000000000 ) ) ;
#53101 = CARTESIAN_POINT ( 'NONE',  ( 6.862290055324999472, -1.004440062237000220, -0.5229138879281000074 ) ) ;
#53102 = CARTESIAN_POINT ( 'NONE',  ( 17.71877800696617200, 1.896477791912290378, 13.78304299653506781 ) ) ;
#53103 = CARTESIAN_POINT ( 'NONE',  ( 17.60000000798000386, 11.41069016990000051, -4.623987642516999230 ) ) ;
#53104 = CARTESIAN_POINT ( 'NONE',  ( 10.79967784532818698, 4.987751806468194715, 4.853501387964938907 ) ) ;
#53105 = CARTESIAN_POINT ( 'NONE',  ( 10.62072335273219892, -3.602909566644000083, -8.569396700949999612 ) ) ;
#53106 = EDGE_LOOP ( 'NONE', ( #61725, #49606, #48344, #7826 ) ) ;
#53107 = VECTOR ( 'NONE', #24178, 1000.000000000000114 ) ;
#53108 = CARTESIAN_POINT ( 'NONE',  ( 5.647168941336192738, -12.08810193142197242, 3.737902345523164360 ) ) ;
#53109 = CARTESIAN_POINT ( 'NONE',  ( 8.143323341229999457, 5.061727314042999915, 5.824077473724000420 ) ) ;
#53110 = AXIS2_PLACEMENT_3D ( 'NONE', #38485, #53871, #54913 ) ;
#53112 = CARTESIAN_POINT ( 'NONE',  ( 10.57314899745999881, 5.167567567567999731, -6.822293592207000934 ) ) ;
#53111 = CARTESIAN_POINT ( 'NONE',  ( 8.614404719593999005, 5.030502105212999453, -6.322203460290999999 ) ) ;
#53113 = FACE_OUTER_BOUND ( 'NONE', #30065, .T. ) ;
#53114 = ORIENTED_EDGE ( 'NONE', *, *, #58433, .F. ) ;
#53115 = CARTESIAN_POINT ( 'NONE',  ( 10.31457848836000046, 5.362142879234999882, 6.677781064327999339 ) ) ;
#53116 = CARTESIAN_POINT ( 'NONE',  ( 18.06560877808663079, -2.138932497554039802, -13.74340275081395291 ) ) ;
#53117 = CARTESIAN_POINT ( 'NONE',  ( 10.87518447801629939, 4.865987311498500389, 7.519093628927509876 ) ) ;
#53118 = CARTESIAN_POINT ( 'NONE',  ( 10.31457635473999979, -5.362146312020000138, 6.677778992223999843 ) ) ;
#53119 = CARTESIAN_POINT ( 'NONE',  ( 7.614808059621999803, -3.326257819185999942, 8.794522506294001118 ) ) ;
#53120 = VERTEX_POINT ( 'NONE', #10016 ) ;
#53121 = CARTESIAN_POINT ( 'NONE',  ( 8.508079719592000600, 2.202812441249000219, 7.706988150133999405 ) ) ;
#53122 = EDGE_CURVE ( 'NONE', #57489, #25637, #32544, .T. ) ;
#53124 = CARTESIAN_POINT ( 'NONE',  ( 10.11549555961999936, -2.489199523559999960, -6.434642413229999747 ) ) ;
#53123 = CARTESIAN_POINT ( 'NONE',  ( 10.05882936267868466, -4.704418606475396558, 8.703716202581736283 ) ) ;
#53125 = CARTESIAN_POINT ( 'NONE',  ( 7.611706454504995278, -4.775798000191374904, 5.942893401888585281 ) ) ;
#53126 = CARTESIAN_POINT ( 'NONE',  ( 18.18005043824477696, -1.062925945863725942E-10, 13.90000000153292881 ) ) ;
#53128 = CARTESIAN_POINT ( 'NONE',  ( 1.261654918708000173, 2.900008637959000435, -1.487022697228999935 ) ) ;
#53127 = CIRCLE ( 'NONE', #45303, 1.349999999999999867 ) ;
#53129 = ORIENTED_EDGE ( 'NONE', *, *, #2276, .T. ) ;
#53130 = CARTESIAN_POINT ( 'NONE',  ( 25.60000000000000142, 0.000000000000000000, 0.000000000000000000 ) ) ;
#53131 = EDGE_CURVE ( 'NONE', #12705, #10297, #52259, .T. ) ;
#53132 = CARTESIAN_POINT ( 'NONE',  ( 11.58841369783139896, -4.057552111898620417, 6.360711682373000109 ) ) ;
#53133 = CARTESIAN_POINT ( 'NONE',  ( 11.02445190299000011, 3.404087387974999768, 5.822483872269000216 ) ) ;
#53134 = AXIS2_PLACEMENT_3D ( 'NONE', #57532, #9637, #30984 ) ;
#53135 = CARTESIAN_POINT ( 'NONE',  ( 11.67918044953561996, 5.011483761127000669, 6.972563939641199582 ) ) ;
#53136 = VERTEX_POINT ( 'NONE', #25066 ) ;
#53137 = CARTESIAN_POINT ( 'NONE',  ( 9.410004719593999312, 2.495531372253999791, -7.930944806125000746 ) ) ;
#53138 = CARTESIAN_POINT ( 'NONE',  ( 12.35083548769875250, 1.919332845685024935, -12.45296032288162813 ) ) ;
#53139 = CARTESIAN_POINT ( 'NONE',  ( 11.01414141025500015, -3.384226587288500010, 6.403245959303999868 ) ) ;
#53140 = CARTESIAN_POINT ( 'NONE',  ( 25.59037377391700119, -2.738633770010999502, -11.22408586312000089 ) ) ;
#53141 = CARTESIAN_POINT ( 'NONE',  ( 18.17602379430283932, 2.571655014618306812, -13.65800652342106325 ) ) ;
#53142 = EDGE_LOOP ( 'NONE', ( #34431, #69058, #59144, #32771 ) ) ;
#53143 = CARTESIAN_POINT ( 'NONE',  ( 3.500000000000000000, 1.140396268832999827, -3.309002319436000317 ) ) ;
#53144 = CARTESIAN_POINT ( 'NONE',  ( 5.499999999550999163, -0.5000000004493000416, -9.662944680110001627 ) ) ;
#53145 = ORIENTED_EDGE ( 'NONE', *, *, #58642, .F. ) ;
#53146 = CARTESIAN_POINT ( 'NONE',  ( 9.448096873516666605, 3.672815144550898303, 6.282534154164604701 ) ) ;
#53147 = EDGE_CURVE ( 'NONE', #24689, #65709, #16552, .T. ) ;
#53148 = CARTESIAN_POINT ( 'NONE',  ( 10.53057053952199951, 3.659587858614300249, 8.296503712697200328 ) ) ;
#53149 = CARTESIAN_POINT ( 'NONE',  ( 10.37873747135000002, 4.882725050998000249, 6.350806206758999650 ) ) ;
#53150 = CARTESIAN_POINT ( 'NONE',  ( 10.14584353048000054, 5.370502454907000178, -6.826221644974000746 ) ) ;
#53151 = CARTESIAN_POINT ( 'NONE',  ( 8.436984272513997851, 5.098716299041000433, 6.624027315230001101 ) ) ;
#53152 = CARTESIAN_POINT ( 'NONE',  ( 9.910640133503999749, -2.107273866476999657, 7.885282692430999774 ) ) ;
#53153 = CARTESIAN_POINT ( 'NONE',  ( 17.88507951091366621, 0.5311517451680620727, -12.68505220952107493 ) ) ;
#53154 = CARTESIAN_POINT ( 'NONE',  ( 8.991737455307951876, 5.328242699075392608, 7.781227856390141362 ) ) ;
#53155 = CARTESIAN_POINT ( 'NONE',  ( 11.26487482311540056, -3.069598554678400149, -7.875904247640098887 ) ) ;
#53156 = CARTESIAN_POINT ( 'NONE',  ( 8.432510841230001830, 5.430400319332999715, 7.210801214872999410 ) ) ;
#53157 = ORIENTED_EDGE ( 'NONE', *, *, #42775, .T. ) ;
#53158 = B_SPLINE_CURVE_WITH_KNOTS ( 'NONE', 3,
 ( #63856, #62823, #10380, #41511, #52345, #25432 ),
 .UNSPECIFIED., .F., .F.,
 ( 4, 2, 4 ),
 ( 0.000000000000000000, 0.5000000000000000000, 1.000000000000000000 ),
 .UNSPECIFIED. ) ;
#53159 =( LENGTH_UNIT ( ) NAMED_UNIT ( * ) SI_UNIT ( .MILLI., .METRE. ) );
#53160 = CARTESIAN_POINT ( 'NONE',  ( 10.97028665956023197, 3.257584962274628904, 6.450604656432374462 ) ) ;
#53161 = CARTESIAN_POINT ( 'NONE',  ( 9.237254889805134539, 2.665102389433001928, 7.298797478834294417 ) ) ;
#53162 = CARTESIAN_POINT ( 'NONE',  ( 8.716851002545999094, 2.832432432432000269, 6.822293592207000934 ) ) ;
#53163 = CARTESIAN_POINT ( 'NONE',  ( 18.24542859620200019, 2.700577031380341886, 12.30719352326003779 ) ) ;
#53164 = CARTESIAN_POINT ( 'NONE',  ( 12.48191940168456604, 1.864230036291395720, 13.87532606992096795 ) ) ;
#53165 = CARTESIAN_POINT ( 'NONE',  ( 10.96428034375000138, 7.885731839849998259, 6.436515532732999922 ) ) ;
#53166 = CARTESIAN_POINT ( 'NONE',  ( 12.38151466856633220, -0.4597251445480311505, -12.68880184500082819 ) ) ;
#53167 = DIRECTION ( 'NONE',  ( 0.000000000000000000, 0.000000000000000000, -1.000000000000000000 ) ) ;
#53168 = ORIENTED_EDGE ( 'NONE', *, *, #32364, .F. ) ;
#53169 = CARTESIAN_POINT ( 'NONE',  ( 12.38926598778393995, -1.890730539229764862, 12.45733450583996671 ) ) ;
#53170 = CARTESIAN_POINT ( 'NONE',  ( 9.507063610504999929, -3.475294527116599586, -8.666648427848999248 ) ) ;
#53171 = DIRECTION ( 'NONE',  ( 0.000000000000000000, -0.1333333333333049375, 0.9910712498212376209 ) ) ;
#53172 = CARTESIAN_POINT ( 'NONE',  ( 10.97865453029000093, -5.273142482194999481, 7.958032781726000593 ) ) ;
#53173 = CARTESIAN_POINT ( 'NONE',  ( 11.98641235500450009, -4.739919807690899489, 8.177841818594698609 ) ) ;
#53174 = AXIS2_PLACEMENT_3D ( 'NONE', #45130, #14347, #3495 ) ;
#53175 = CARTESIAN_POINT ( 'NONE',  ( 12.17126533935444499, 0.3494793053307373998, 12.59515668824706580 ) ) ;
#53176 = EDGE_CURVE ( 'NONE', #57519, #5439, #56813, .T. ) ;
#53177 = ADVANCED_FACE ( 'NONE', ( #64430 ), #63144, .F. ) ;
#53178 = CARTESIAN_POINT ( 'NONE',  ( 0.3183723959866999742, 0.6486458134353999538, 3.310649237188999727 ) ) ;
#53179 = B_SPLINE_CURVE_WITH_KNOTS ( 'NONE', 3,
 ( #51601, #24011, #3699, #25037 ),
 .UNSPECIFIED., .F., .F.,
 ( 4, 4 ),
 ( 0.000000000000000000, 0.1254754252289749794 ),
 .UNSPECIFIED. ) ;
#53180 = CARTESIAN_POINT ( 'NONE',  ( 0.000000000000000000, -5.100000000000000533, -7.500000000000000000 ) ) ;
#53181 = CARTESIAN_POINT ( 'NONE',  ( 12.11850681454232515, 2.712075317534401897, 12.30466467946555831 ) ) ;
#53183 = DIRECTION ( 'NONE',  ( 0.000000000000000000, -1.000000000000000000, 0.000000000000000000 ) ) ;
#53182 = CARTESIAN_POINT ( 'NONE',  ( 9.530380199233999150, 5.132898093246000215, -7.357604921762999517 ) ) ;
#53184 = ADVANCED_FACE ( 'NONE', ( #30663 ), #5464, .F. ) ;
#53185 = CARTESIAN_POINT ( 'NONE',  ( 11.65456516821461008, 4.802916961510000249, -8.310318115935698913 ) ) ;
#53186 = CARTESIAN_POINT ( 'NONE',  ( 12.49459120399991896, 12.10614746208231551, -3.212001293532309454 ) ) ;
#53187 = CARTESIAN_POINT ( 'NONE',  ( 10.13035471959000056, 2.409325917207000511, -8.058043919563999680 ) ) ;
#53188 = CARTESIAN_POINT ( 'NONE',  ( 9.579975701332999805, 4.938486452461599896, -8.369268408503399925 ) ) ;
#53190 = CARTESIAN_POINT ( 'NONE',  ( 12.20125275681506238, 2.661451430635814575, 12.41248063365286924 ) ) ;
#53189 = CARTESIAN_POINT ( 'NONE',  ( 15.37447410014400084, -8.836271409840000146, -7.950749727554001112 ) ) ;
#53191 = CARTESIAN_POINT ( 'NONE',  ( 11.29996927726999978, -12.23272628844000032, -1.505586261403999870 ) ) ;
#53192 = ORIENTED_EDGE ( 'NONE', *, *, #13975, .T. ) ;
#53193 = CARTESIAN_POINT ( 'NONE',  ( 0.7062757755484999622, 2.610614231003999919, -1.727479700733000056 ) ) ;
#53194 = FACE_OUTER_BOUND ( 'NONE', #14886, .T. ) ;
#53195 = CARTESIAN_POINT ( 'NONE',  ( 17.78895972989507257, 0.6824382159868358499, -12.58151825845973271 ) ) ;
#53196 = CARTESIAN_POINT ( 'NONE',  ( 9.754317406968999293, 4.161254277581000416, 6.648116790593900483 ) ) ;
#53197 = CARTESIAN_POINT ( 'NONE',  ( 12.43942356506269142, -3.006998533878517676, 13.55276137517231838 ) ) ;
#53198 = CARTESIAN_POINT ( 'NONE',  ( 23.56665676678100141, -2.935523947847999970, 13.67844066972000050 ) ) ;
#53199 = CARTESIAN_POINT ( 'NONE',  ( 8.154250713371753889, 3.097976385119930232, 6.283652888193028474 ) ) ;
#53200 = EDGE_LOOP ( 'NONE', ( #34231, #46213, #58705, #45123 ) ) ;
#53201 = CARTESIAN_POINT ( 'NONE',  ( 4.866418903102999849, -0.9777056432663999708, -0.5753238461295000494 ) ) ;
#53202 = CARTESIAN_POINT ( 'NONE',  ( 9.985242056249999720, -4.458751122174599679, -8.694123841252999085 ) ) ;
#53203 = CARTESIAN_POINT ( 'NONE',  ( 25.00266768346542889, 3.413762979258133878, 11.76148390993455628 ) ) ;
#53204 = CARTESIAN_POINT ( 'NONE',  ( 24.63002439619599926, 0.000000000000000000, 0.000000000000000000 ) ) ;
#53205 = CARTESIAN_POINT ( 'NONE',  ( 18.08682736286118597, 2.829024318083993794, -12.36883279713289951 ) ) ;
#53206 = CARTESIAN_POINT ( 'NONE',  ( 9.843930206850000530, -5.250000000000000000, 7.500000000000000000 ) ) ;
#53207 = PRESENTATION_LAYER_ASSIGNMENT (  '', '', ( #14143 ) ) ;
#53208 = CARTESIAN_POINT ( 'NONE',  ( 18.17603698666708212, 2.571536872321186440, 12.43461505415530866 ) ) ;
#53209 = CARTESIAN_POINT ( 'NONE',  ( 9.267891187585000523, -4.645169647889000331, -5.840816811670999975 ) ) ;
#53210 = CARTESIAN_POINT ( 'NONE',  ( 10.19122055961999962, -3.990707710465999813, -5.651373900265999950 ) ) ;
#53211 = AXIS2_PLACEMENT_3D ( 'NONE', #25342, #51567, #25002 ) ;
#53212 = CARTESIAN_POINT ( 'NONE',  ( 4.844609839683289287, 1.500000000000000888, -0.1963495408493590444 ) ) ;
#53213 = CARTESIAN_POINT ( 'NONE',  ( 24.30000564890097081, 8.853233220944831672, 8.853233220944831672 ) ) ;
#53214 = CARTESIAN_POINT ( 'NONE',  ( 24.15442946601968188, 9.133667536019347111, -9.112066069742461139 ) ) ;
#53215 = CARTESIAN_POINT ( 'NONE',  ( 9.422953957969571803, 5.349869638328708099, 7.471018043992390112 ) ) ;
#53216 = CARTESIAN_POINT ( 'NONE',  ( 24.51195772155200103, 12.36179148984999898, -3.074600399797000172 ) ) ;
#53217 = B_SPLINE_CURVE_WITH_KNOTS ( 'NONE', 3,
 ( #60065, #1678, #6572, #53779 ),
 .UNSPECIFIED., .F., .F.,
 ( 4, 4 ),
 ( 0.000000000000000000, 1.000000000000000000 ),
 .UNSPECIFIED. ) ;
#53218 = ORIENTED_EDGE ( 'NONE', *, *, #23301, .F. ) ;
#53219 = CARTESIAN_POINT ( 'NONE',  ( 9.988985841228000595, 3.986577607995999806, -9.280166295424001177 ) ) ;
#53220 = CARTESIAN_POINT ( 'NONE',  ( 11.98641235500450009, -4.739919807690899489, 8.177841818594698609 ) ) ;
#53221 = EDGE_LOOP ( 'NONE', ( #67929, #52557, #18973, #27601 ) ) ;
#53222 = AXIS2_PLACEMENT_3D ( 'NONE', #52402, #20246, #9064 ) ;
#53223 = FACE_OUTER_BOUND ( 'NONE', #31804, .T. ) ;
#53224 = CARTESIAN_POINT ( 'NONE',  ( 10.22687885159599830, -2.867290578374000365, -7.364871923548499844 ) ) ;
#53225 = ORIENTED_EDGE ( 'NONE', *, *, #1823, .T. ) ;
#53226 = DIRECTION ( 'NONE',  ( 0.000000000000000000, -0.1807154286440006141, -0.9835354258236025382 ) ) ;
#53227 = ADVANCED_FACE ( 'NONE', ( #34722 ), #32268, .T. ) ;
#53228 = CARTESIAN_POINT ( 'NONE',  ( 24.17206213204222820, 3.320420788054297745, -12.43428578304583354 ) ) ;
#53229 = CARTESIAN_POINT ( 'NONE',  ( 17.96012107570599881, -3.168891391480999520, 11.45723209283999999 ) ) ;
#53230 = CARTESIAN_POINT ( 'NONE',  ( 10.32169598648999909, -3.233475335853099875, -7.956401575444799867 ) ) ;
#53231 = CARTESIAN_POINT ( 'NONE',  ( 12.55587196706169095, 0.5732793990000022433, -13.88408420575383850 ) ) ;
#53232 = CARTESIAN_POINT ( 'NONE',  ( 11.59999999999999787, -4.794859953698266786, -7.075514291626550545 ) ) ;
#53233 = CARTESIAN_POINT ( 'NONE',  ( 10.15000066238999921, -1.190159082397999942E-13, -12.44999944941012160 ) ) ;
#53234 = ORIENTED_EDGE ( 'NONE', *, *, #26372, .F. ) ;
#53235 = CARTESIAN_POINT ( 'NONE',  ( 9.368660841232999914, 2.702406276695999754, -6.981052078638000147 ) ) ;
#53236 = ORIENTED_EDGE ( 'NONE', *, *, #14830, .F. ) ;
#53237 = CARTESIAN_POINT ( 'NONE',  ( 10.66476354018302608, 5.217465845835396188, -7.172815144550905408 ) ) ;
#53238 =( NAMED_UNIT ( * ) SI_UNIT ( $, .STERADIAN. ) SOLID_ANGLE_UNIT ( ) );
#53239 = ORIENTED_EDGE ( 'NONE', *, *, #64786, .T. ) ;
#53240 = CARTESIAN_POINT ( 'NONE',  ( 9.478659112603999404, 3.444147913214900214, 6.347865960448999090 ) ) ;
#53241 = CARTESIAN_POINT ( 'NONE',  ( 17.55505043854147118, -3.125000000000000000, -12.28373071562069896 ) ) ;
#53242 = DIRECTION ( 'NONE',  ( 0.4384236320213994453, -0.6355252626312994924, 0.6355252626312996034 ) ) ;
#53243 = CARTESIAN_POINT ( 'NONE',  ( 17.72046959778183961, -1.874999999999999556, -12.57541560742024345 ) ) ;
#53244 = CARTESIAN_POINT ( 'NONE',  ( 12.20137680394560142, -0.1621987986621315492, 13.89873133405097327 ) ) ;
#53245 = ORIENTED_EDGE ( 'NONE', *, *, #40592, .T. ) ;
#53246 = CARTESIAN_POINT ( 'NONE',  ( 11.60000000000000142, 4.325863785438847309, 6.377063228063085454 ) ) ;
#53247 = CARTESIAN_POINT ( 'NONE',  ( 17.72554598058900055, 11.44503420830000096, -4.692817581925999626 ) ) ;
#53248 = CARTESIAN_POINT ( 'NONE',  ( 9.556179045228626379, 3.383234358265068575, 8.120590373834733811 ) ) ;
#53249 = CARTESIAN_POINT ( 'NONE',  ( 18.30003129334700063, -2.732683817159999862, 11.53064095410000078 ) ) ;
#53250 = CIRCLE ( 'NONE', #30954, 0.4999999999999995559 ) ;
#53251 = B_SPLINE_CURVE_WITH_KNOTS ( 'NONE', 3,
 ( #14735, #36054, #30814, #5267 ),
 .UNSPECIFIED., .F., .F.,
 ( 4, 4 ),
 ( 0.000000000000000000, 1.000000000000000000 ),
 .UNSPECIFIED. ) ;
#53252 = CARTESIAN_POINT ( 'NONE',  ( 9.643864158774000828, 2.927176851028000293, -5.932007155957999878 ) ) ;
#53253 = CARTESIAN_POINT ( 'NONE',  ( 18.14390421667115305, 12.07230385407727447, -3.337096842113823847 ) ) ;
#53254 = CARTESIAN_POINT ( 'NONE',  ( 10.18512684885999953, -5.526147823900999789, -7.556025229989000280 ) ) ;
#53255 = ADVANCED_FACE ( 'NONE', ( #8825 ), #43387, .F. ) ;
#53256 = EDGE_CURVE ( 'NONE', #66718, #63209, #15491, .T. ) ;
#53257 = EDGE_LOOP ( 'NONE', ( #36566, #12845, #56500, #33440 ) ) ;
#53258 = ORIENTED_EDGE ( 'NONE', *, *, #16211, .T. ) ;
#53259 = DIRECTION ( 'NONE',  ( 0.000000000000000000, 0.000000000000000000, -1.000000000000000000 ) ) ;
#53260 = VECTOR ( 'NONE', #4828, 1000.000000000000000 ) ;
#53261 = DIRECTION ( 'NONE',  ( 1.000000000000000000, 0.000000000000000000, 0.000000000000000000 ) ) ;
#53262 = CARTESIAN_POINT ( 'NONE',  ( 8.616332382228000242, -2.832433105983000132, -6.822293595522999965 ) ) ;
#53263 = ADVANCED_FACE ( 'NONE', ( #46234 ), #51811, .F. ) ;
#53264 = EDGE_CURVE ( 'NONE', #11189, #57248, #14763, .T. ) ;
#53265 = CARTESIAN_POINT ( 'NONE',  ( 12.32889761174919485, -2.904977411726858527, 13.57918629439492442 ) ) ;
#53266 = LINE ( 'NONE', #48020, #28860 ) ;
#53267 = CARTESIAN_POINT ( 'NONE',  ( 11.01279632507519857, 4.624908853805600906, -8.658468685623999406 ) ) ;
#53268 = CARTESIAN_POINT ( 'NONE',  ( 10.21924205624999971, 3.689072563647699976, -8.309340504471899536 ) ) ;
#53270 = DIRECTION ( 'NONE',  ( 0.000000000000000000, 1.000000000000000000, 0.000000000000000000 ) ) ;
#53269 = CARTESIAN_POINT ( 'NONE',  ( 10.02836764078099918, -3.526522998810799781, 8.385811396220899994 ) ) ;
#53271 = CARTESIAN_POINT ( 'NONE',  ( 4.805026506350000837, 1.500000000000000000, 0.000000000000000000 ) ) ;
#53272 = VERTEX_POINT ( 'NONE', #2545 ) ;
#53273 = CIRCLE ( 'NONE', #13116, 12.52500000000000036 ) ;
#53274 = CARTESIAN_POINT ( 'NONE',  ( 10.35826357027499789, -3.149486845331399998, -7.664090691848299386 ) ) ;
#53275 = CARTESIAN_POINT ( 'NONE',  ( 7.602716214150000873, -2.929796814311000919, 6.536389039862005035 ) ) ;
#53276 = FACE_OUTER_BOUND ( 'NONE', #30670, .T. ) ;
#53277 = CARTESIAN_POINT ( 'NONE',  ( 12.09999999999999964, -4.000000000000000000, 7.500000000000000000 ) ) ;
#53278 = AXIS2_PLACEMENT_3D ( 'NONE', #64822, #49102, #65169 ) ;
#53279 = CARTESIAN_POINT ( 'NONE',  ( 10.83668192271000130, -4.288535286065000562, 9.448729895547000268 ) ) ;
#53280 = CARTESIAN_POINT ( 'NONE',  ( 17.75789140671455968, 3.091531401869214157, -12.29387995131248346 ) ) ;
#53281 = CARTESIAN_POINT ( 'NONE',  ( 15.99015267864900203, -3.493241607194999876, -11.26524960718000123 ) ) ;
#53282 = EDGE_CURVE ( 'NONE', #2520, #37807, #57546, .T. ) ;
#53283 = CARTESIAN_POINT ( 'NONE',  ( 19.89999890908300273, 0.000000000000000000, 0.000000000000000000 ) ) ;
#53284 = CARTESIAN_POINT ( 'NONE',  ( 7.573333333330499073, 5.179611624278248172, -6.820114376499284425 ) ) ;
#53285 = CARTESIAN_POINT ( 'NONE',  ( 9.915292290062998504, -3.250213325543700016, -7.064651992867799990 ) ) ;
#53286 = CARTESIAN_POINT ( 'NONE',  ( 6.182261061822000414, -0.7806768893493000183, 1.067248597240000096 ) ) ;
#53287 = CARTESIAN_POINT ( 'NONE',  ( 4.500000125099000492, 12.99999867215000116, 0.000000000000000000 ) ) ;
#53288 = CARTESIAN_POINT ( 'NONE',  ( 17.74468889437551766, 1.784327658738282363, 12.47302143557446996 ) ) ;
#53289 = ORIENTED_EDGE ( 'NONE', *, *, #35747, .T. ) ;
#53290 = CARTESIAN_POINT ( 'NONE',  ( 12.24897804304629290, 0.2853680816562786937, -12.69568625917504257 ) ) ;
#53291 = CARTESIAN_POINT ( 'NONE',  ( 11.76133460557259980, 4.139849081322200419, -8.354833838171700222 ) ) ;
#53292 = FACE_OUTER_BOUND ( 'NONE', #50450, .T. ) ;
#53293 = DIRECTION ( 'NONE',  ( -1.644739578229999948E-10, -1.644740771478999934E-10, 1.000000000000000000 ) ) ;
#53294 = CARTESIAN_POINT ( 'NONE',  ( 1.550973465874000201, 3.500000000000000000, 0.000000000000000000 ) ) ;
#53295 = ORIENTED_EDGE ( 'NONE', *, *, #10584, .F. ) ;
#53296 = CARTESIAN_POINT ( 'NONE',  ( 25.57779415553899938, -11.11294835904000067, -3.219291969928999908 ) ) ;
#53297 = SHAPE_DEFINITION_REPRESENTATION ( #29383, #24587 ) ;
#53298 = CARTESIAN_POINT ( 'NONE',  ( 10.35814141025499957, -3.516507310755200066, -8.361148840840000318 ) ) ;
#53299 = DIRECTION ( 'NONE',  ( 0.9999999999977496890, 1.824801334886089481E-06, -1.081901619956053515E-06 ) ) ;
#53300 = CARTESIAN_POINT ( 'NONE',  ( 8.470944094208999076, 5.100000000000000533, 6.571291218949999902 ) ) ;
#53301 = CARTESIAN_POINT ( 'NONE',  ( 7.883148997456999929, 5.167567567567999731, 6.822293592207000934 ) ) ;
#53302 = CARTESIAN_POINT ( 'NONE',  ( 12.97415039705200179, 12.11604096695999999, 2.033011318524000188 ) ) ;
#53303 = EDGE_LOOP ( 'NONE', ( #18850, #20538 ) ) ;
#53304 = CIRCLE ( 'NONE', #62238, 0.9999997023190999590 ) ;
#53305 = CARTESIAN_POINT ( 'NONE',  ( 10.33537187819000103, -5.153689638257000105, 8.830861236101000600 ) ) ;
#53306 = CARTESIAN_POINT ( 'NONE',  ( 17.99129208686611392, 2.947687251868547520, -13.56825406139790680 ) ) ;
#53307 = VERTEX_POINT ( 'NONE', #45210 ) ;
#53308 = CARTESIAN_POINT ( 'NONE',  ( 10.02052890782000105, -2.899999999999999911, 6.152188490330000370 ) ) ;
#53309 = CARTESIAN_POINT ( 'NONE',  ( 7.545269353206999874, -2.302293129340000188, 6.875167727519000849 ) ) ;
#53310 = EDGE_CURVE ( 'NONE', #95, #2054, #62389, .T. ) ;
#53311 = CARTESIAN_POINT ( 'NONE',  ( 16.04382898362900178, 8.457859886528000359, 8.090718092504999959 ) ) ;
#53312 = ORIENTED_EDGE ( 'NONE', *, *, #31966, .T. ) ;
#53313 = CARTESIAN_POINT ( 'NONE',  ( 17.55505043854147118, -1.787797342887044172, -13.88538010501570774 ) ) ;
#53314 = B_SPLINE_CURVE_WITH_KNOTS ( 'NONE', 3,
 ( #28528, #59637, #49840, #1951, #48461, #569, #54389, #11733, #23272 ),
 .UNSPECIFIED., .F., .F.,
 ( 4, 1, 2, 2, 4 ),
 ( 0.000000000000000000, 0.2500000000000015543, 0.3750000000000009992, 0.5000000000000004441, 1.000000000000000000 ),
 .UNSPECIFIED. ) ;
#53315 = CARTESIAN_POINT ( 'NONE',  ( 6.777195280410000855, 5.620828677136000096, -7.589710348707000342 ) ) ;
#53316 = EDGE_CURVE ( 'NONE', #68518, #27264, #40969, .T. ) ;
#53317 = AXIS2_PLACEMENT_3D ( 'NONE', #26865, #63899, #69154 ) ;
#53318 = CARTESIAN_POINT ( 'NONE',  ( 10.90000000536000080, -2.899999999941999640, -5.157071284930999866 ) ) ;
#53319 = CARTESIAN_POINT ( 'NONE',  ( 7.100000000000000533, -5.349999999999999645, -7.500000000000000000 ) ) ;
#53320 = ORIENTED_EDGE ( 'NONE', *, *, #37970, .F. ) ;
#53321 = CARTESIAN_POINT ( 'NONE',  ( 10.59344961228999971, -5.297755890367000120, 8.474197994416998725 ) ) ;
#53322 = CARTESIAN_POINT ( 'NONE',  ( 21.60000012424471194, 3.970157536060000036E-13, 1.776356839399999796E-13 ) ) ;
#53323 = CARTESIAN_POINT ( 'NONE',  ( 6.899999691988000450, 0.000000000000000000, 0.000000000000000000 ) ) ;
#53324 = ORIENTED_EDGE ( 'NONE', *, *, #7337, .T. ) ;
#53325 = VECTOR ( 'NONE', #1020, 1000.000000000000000 ) ;
#53326 = CARTESIAN_POINT ( 'NONE',  ( 11.79999999471800010, -3.216299622513999701, 11.40340969442000052 ) ) ;
#53327 = CARTESIAN_POINT ( 'NONE',  ( 11.14450444037999866, -5.035425715994000129, -8.381528062715000615 ) ) ;
#53328 = VERTEX_POINT ( 'NONE', #36081 ) ;
#53329 = CARTESIAN_POINT ( 'NONE',  ( 23.58407651006106676, -10.21953228476464837, 9.544199785307510453 ) ) ;
#53330 = CARTESIAN_POINT ( 'NONE',  ( 18.14038165173105099, 0.2193642558646157759, -13.89767506191630098 ) ) ;
#53331 = CARTESIAN_POINT ( 'NONE',  ( 5.195378349970999565, 1.269083497910999947, -0.6291676704954000110 ) ) ;
#53332 = CARTESIAN_POINT ( 'NONE',  ( 8.080472934640001270, 5.120350537135998081, -6.726184732097004293 ) ) ;
#53333 = CARTESIAN_POINT ( 'NONE',  ( 21.47500033997000202, -1.509903313490000218E-14, 12.72499970925004398 ) ) ;
#53334 = CARTESIAN_POINT ( 'NONE',  ( 0.000000000000000000, 2.899999999999999911, -7.500000000000000000 ) ) ;
#53335 = CARTESIAN_POINT ( 'NONE',  ( 9.251496707488000126, -3.918323994020610268, 6.643597378104299622 ) ) ;
#53336 = B_SPLINE_SURFACE_WITH_KNOTS ( 'NONE', 3, 3, ( 
 ( #53982, #31638, #31299, #53302 ),
 ( #47720, #69033, #6084, #42471 ),
 ( #22168, #63082, #36533, #15207 ),
 ( #57858, #6778, #11673, #7469 ),
 ( #59920, #18319, #64805, #1893 ),
 ( #27778, #23212, #65152, #2239 ),
 ( #54680, #7825, #39642, #55725 ),
 ( #17976, #16916, #44209, #34059 ),
 ( #38957, #44893, #49088, #60274 ),
 ( #38247, #59574, #43851, #38597 ) ),
 .UNSPECIFIED., .F., .F., .F.,
 ( 4, 1, 1, 1, 1, 1, 1, 4 ),
 ( 4, 4 ),
 ( 0.07203983506772999867, 0.1428571428570999946, 0.2857142857143000203, 0.4285714285713999594, 0.5714285714286000406, 0.7142857142856999797, 0.8571428571429000609, 0.9589780836993999635 ),
 ( -0.1900620218102000158, 1.190128522698000069 ),
 .UNSPECIFIED. ) ;
#53337 = ORIENTED_EDGE ( 'NONE', *, *, #59530, .T. ) ;
#53338 = CARTESIAN_POINT ( 'NONE',  ( 8.712681907068999365, 3.774194491866800227, -8.364514367444298770 ) ) ;
#53339 = ORIENTED_EDGE ( 'NONE', *, *, #44161, .F. ) ;
#53340 = CARTESIAN_POINT ( 'NONE',  ( 10.27967883605999866, 5.739712809045000697, 7.774963411801000923 ) ) ;
#53341 = CARTESIAN_POINT ( 'NONE',  ( 10.30480165877000154, 5.828331171948000211, -7.226590957700000928 ) ) ;
#53342 = CARTESIAN_POINT ( 'NONE',  ( 18.32080262064242504, -12.02611605606520584, 3.500834971663305595 ) ) ;
#53343 = CARTESIAN_POINT ( 'NONE',  ( 12.43812277102952635, 1.993632728549933786, -13.76791003216515286 ) ) ;
#53344 = CARTESIAN_POINT ( 'NONE',  ( 24.67921321864300310, 12.29514728640000065, 2.979192498689000157 ) ) ;
#53345 = B_SPLINE_CURVE_WITH_KNOTS ( 'NONE', 3,
 ( #25595, #47612, #21036, #4257 ),
 .UNSPECIFIED., .F., .F.,
 ( 4, 4 ),
 ( 0.000000000000000000, 1.000000000000000000 ),
 .UNSPECIFIED. ) ;
#53346 = CARTESIAN_POINT ( 'NONE',  ( 18.12459203954894349, 0.2581888431706754750, 13.89679013629345228 ) ) ;
#53347 = CARTESIAN_POINT ( 'NONE',  ( 18.00676300520316886, 0.4321619634324096459, 13.89096157872187298 ) ) ;
#53348 = ORIENTED_EDGE ( 'NONE', *, *, #33142, .T. ) ;
#53349 = CARTESIAN_POINT ( 'NONE',  ( 14.30000961100051704, 12.52500000000000036, 1.148724466519551595E-10 ) ) ;
#53350 = ADVANCED_FACE ( 'NONE', ( #47953 ), #15787, .F. ) ;
#53351 = CARTESIAN_POINT ( 'NONE',  ( 11.38733729122639993, -5.277570687708000641, 7.533608309972310124 ) ) ;
#53352 = EDGE_CURVE ( 'NONE', #33283, #43200, #50138, .T. ) ;
#53353 = CARTESIAN_POINT ( 'NONE',  ( 18.05194946914436471, -0.3792369706354827286, -13.89303997535758661 ) ) ;
#53354 = CARTESIAN_POINT ( 'NONE',  ( 8.951355646795001064, -2.821866379289000193, 6.127148604720000336 ) ) ;
#53356 = DIRECTION ( 'NONE',  ( 0.000000000000000000, 0.000000000000000000, 1.000000000000000000 ) ) ;
#53355 = FACE_OUTER_BOUND ( 'NONE', #29155, .T. ) ;
#53357 = CARTESIAN_POINT ( 'NONE',  ( 10.71918447801630059, 5.140463864104999558, -7.474854604063350116 ) ) ;
#53358 = CARTESIAN_POINT ( 'NONE',  ( 7.100000000000000533, -5.349999999999999645, 7.500000000000000000 ) ) ;
#53359 = AXIS2_PLACEMENT_3D ( 'NONE', #19932, #46847, #36006 ) ;
#53360 = CARTESIAN_POINT ( 'NONE',  ( 9.678329965421998082, 3.397808798486600335, -8.123757726465999696 ) ) ;
#53361 = CARTESIAN_POINT ( 'NONE',  ( 18.11564574962621066, -0.2765170649790819057, 12.69595318831093778 ) ) ;
#53362 = CARTESIAN_POINT ( 'NONE',  ( 6.728784626390999613, -1.193958516581999918, 0.4421009869154999827 ) ) ;
#53363 = CARTESIAN_POINT ( 'NONE',  ( 24.21998667016800155, 9.186813646192000249, 9.646745715273000954 ) ) ;
#53364 = ORIENTED_EDGE ( 'NONE', *, *, #14099, .F. ) ;
#53365 = CARTESIAN_POINT ( 'NONE',  ( 9.240543146793999796, -4.158911960977000000, 5.873536005760000123 ) ) ;
#53366 = CARTESIAN_POINT ( 'NONE',  ( 8.385058059625000837, -4.977917894183000236, 6.416767031887000705 ) ) ;
#53367 = B_SPLINE_CURVE_WITH_KNOTS ( 'NONE', 3,
 ( #750, #10893, #48299, #65407, #32239, #1791, #5640, #60179, #22760, #403 ),
 .UNSPECIFIED., .F., .F.,
 ( 4, 2, 2, 2, 4 ),
 ( 0.000000000000000000, 0.2499999999999997780, 0.4999999999999995559, 0.7499999999999997780, 1.000000000000000000 ),
 .UNSPECIFIED. ) ;
#53368 = DIRECTION ( 'NONE',  ( 1.000000000000000000, 0.000000000000000000, -3.552713678656000544E-14 ) ) ;
#53369 = EDGE_CURVE ( 'NONE', #61815, #8371, #59004, .T. ) ;
#53370 = DIRECTION ( 'NONE',  ( -1.000000000000000000, 0.000000000000000000, 0.000000000000000000 ) ) ;
#53371 = ORIENTED_EDGE ( 'NONE', *, *, #46266, .T. ) ;
#53372 = VECTOR ( 'NONE', #55023, 1000.000000000000000 ) ;
#53373 = CARTESIAN_POINT ( 'NONE',  ( 0.8229711358043999558, 3.123219710863000209, -0.8105742342224000474 ) ) ;
#53374 = CARTESIAN_POINT ( 'NONE',  ( 11.06967835872019812, 3.245266201729799960, 7.975673736933100777 ) ) ;
#53375 = CARTESIAN_POINT ( 'NONE',  ( 2.123246496035999797, 1.354718277511999913, 3.506157399516999895 ) ) ;
#53376 = ORIENTED_EDGE ( 'NONE', *, *, #51714, .F. ) ;
#53377 = CARTESIAN_POINT ( 'NONE',  ( 12.61757266016683232, -0.6952251598378732522, -12.58080715426406293 ) ) ;
#53378 = AXIS2_PLACEMENT_3D ( 'NONE', #17882, #25529, #61557 ) ;
#53379 = CARTESIAN_POINT ( 'NONE',  ( 10.90437023801000116, -5.099522774867000230, 5.132565236215000049 ) ) ;
#53380 = CARTESIAN_POINT ( 'NONE',  ( 17.87828936854284478, 3.124432504806127220, -12.20647160316251245 ) ) ;
#53381 = CARTESIAN_POINT ( 'NONE',  ( 7.954938716748859662, -4.949324164348111843, 6.428079711092701487 ) ) ;
#53382 = CARTESIAN_POINT ( 'NONE',  ( 9.234510841229999656, 5.964723767581000757, 7.776480083716999836 ) ) ;
#53383 = ORIENTED_EDGE ( 'NONE', *, *, #7911, .T. ) ;
#53384 = CARTESIAN_POINT ( 'NONE',  ( 7.835819183419109102, -4.957498340680790427, 6.488970330265980024 ) ) ;
#53385 = CARTESIAN_POINT ( 'NONE',  ( 7.201095280410000576, 2.696863807693000048, -8.366590973307999946 ) ) ;
#53386 = CARTESIAN_POINT ( 'NONE',  ( 8.418727353860353091, -2.386268681369533962, 8.150113380672019403 ) ) ;
#53387 = CARTESIAN_POINT ( 'NONE',  ( 9.345430433046999497, -5.088604610742000212, 8.171806809244198888 ) ) ;
#53389 = ORIENTED_EDGE ( 'NONE', *, *, #24000, .T. ) ;
#53388 = AXIS2_PLACEMENT_3D ( 'NONE', #11636, #816, #37184 ) ;
#53390 = CARTESIAN_POINT ( 'NONE',  ( 15.95458079702100029, -3.771493919207000278, -11.78965436225000118 ) ) ;
#53391 = B_SPLINE_CURVE_WITH_KNOTS ( 'NONE', 3,
 ( #41634, #46885, #35709, #30134, #9814 ),
 .UNSPECIFIED., .F., .F.,
 ( 4, 1, 4 ),
 ( 0.000000000000000000, 0.5000000000000000000, 1.000000000000000000 ),
 .UNSPECIFIED. ) ;
#53392 = CARTESIAN_POINT ( 'NONE',  ( 8.356851002541000994, 2.832432432432000269, -6.822293592207000934 ) ) ;
#53393 = ORIENTED_EDGE ( 'NONE', *, *, #63113, .T. ) ;
#53394 = DIRECTION ( 'NONE',  ( -2.359070754062999948E-09, 7.431742730979001170E-12, 1.000000000000000000 ) ) ;
#53395 = CARTESIAN_POINT ( 'NONE',  ( 24.63612635734461875, -8.692478787479979374, -8.668777295098667679 ) ) ;
#53396 = CARTESIAN_POINT ( 'NONE',  ( 11.59999999999999964, -2.820501972398000046, -7.174999999999999822 ) ) ;
#53397 = ORIENTED_EDGE ( 'NONE', *, *, #68833, .T. ) ;
#53398 = LINE ( 'NONE', #22949, #29788 ) ;
#53399 = CARTESIAN_POINT ( 'NONE',  ( 5.500000000000000000, -11.06886219213000011, 1.536526853569999851 ) ) ;
#53400 = CARTESIAN_POINT ( 'NONE',  ( 10.17726354018333090, -3.370476274536371442, 8.592232985442818105 ) ) ;
#53401 = EDGE_CURVE ( 'NONE', #25637, #16938, #39977, .T. ) ;
#53402 = CARTESIAN_POINT ( 'NONE',  ( 12.76336819523226929, 3.123957167202322971, -12.28406425424631365 ) ) ;
#53403 = CARTESIAN_POINT ( 'NONE',  ( 11.14118447801630118, -2.722297859592000435, 7.528171279442569919 ) ) ;
#53404 = ORIENTED_EDGE ( 'NONE', *, *, #47772, .T. ) ;
#53405 = CARTESIAN_POINT ( 'NONE',  ( 8.026329719592000700, 5.601795057054999916, 7.176148573050999957 ) ) ;
#53406 = ORIENTED_EDGE ( 'NONE', *, *, #34631, .T. ) ;
#53407 = CARTESIAN_POINT ( 'NONE',  ( 9.843930206850000530, -5.250000000000000000, 7.500000000000000000 ) ) ;
#53408 = CARTESIAN_POINT ( 'NONE',  ( 15.76350100824699929, -9.023747925888001120, -8.341981946770999912 ) ) ;
#53409 = CARTESIAN_POINT ( 'NONE',  ( 11.09999999999999964, -5.350000000000000533, 7.500000000000000000 ) ) ;
#53410 = VERTEX_POINT ( 'NONE', #10883 ) ;
#53411 = CARTESIAN_POINT ( 'NONE',  ( 5.000000000000000000, 0.2999999999999999889, 3.149999999999999911 ) ) ;
#53412 = CARTESIAN_POINT ( 'NONE',  ( 10.27427156480999848, -4.600000212792999754, 4.944156960788000710 ) ) ;
#53413 = CARTESIAN_POINT ( 'NONE',  ( 23.60000000000000497, 0.9826074340704106236, 13.89473237476927459 ) ) ;
#53414 = DIRECTION ( 'NONE',  ( 1.000000000000000000, 0.000000000000000000, 0.000000000000000000 ) ) ;
#53415 = CARTESIAN_POINT ( 'NONE',  ( 12.27409806343529652, -3.015283977741793020, -13.67143535301651447 ) ) ;
#53416 = AXIS2_PLACEMENT_3D ( 'NONE', #57645, #25840, #14670 ) ;
#53417 = CARTESIAN_POINT ( 'NONE',  ( 11.16641369783139837, -4.050626550392200542, -8.502191501283999031 ) ) ;
#53418 = CARTESIAN_POINT ( 'NONE',  ( 11.55670819615736455, 3.379350336066780702, -6.880644002891321165 ) ) ;
#53419 = CARTESIAN_POINT ( 'NONE',  ( 18.03569330394761039, -3.019535577993367692, 12.23285103262380424 ) ) ;
#53420 = ORIENTED_EDGE ( 'NONE', *, *, #12706, .T. ) ;
#53421 = CARTESIAN_POINT ( 'NONE',  ( 11.07242469412000041, -6.093414471448999947, -5.195953259728000262 ) ) ;
#53422 = ORIENTED_EDGE ( 'NONE', *, *, #9052, .F. ) ;
#53423 = CIRCLE ( 'NONE', #67933, 11.35000000000000675 ) ;
#53424 = DIRECTION ( 'NONE',  ( -1.000000000000000000, 0.000000000000000000, 0.000000000000000000 ) ) ;
#53425 = CARTESIAN_POINT ( 'NONE',  ( 7.000000000000000000, 0.2708497377871000311, -3.000000000000000000 ) ) ;
#53426 = CARTESIAN_POINT ( 'NONE',  ( 10.56271176071999918, 2.509373760909999973, -8.602415192333999983 ) ) ;
#53427 = CARTESIAN_POINT ( 'NONE',  ( 23.57774090764768005, -10.35460453196024311, -9.360197169778087911 ) ) ;
#53428 = CARTESIAN_POINT ( 'NONE',  ( 9.073148997461000675, 5.167567567567999731, -6.822293592207000934 ) ) ;
#53429 = CARTESIAN_POINT ( 'NONE',  ( 15.90003771078200145, 3.695138809391000034, 11.25918926437999978 ) ) ;
#53430 = VECTOR ( 'NONE', #25125, 1000.000000000000000 ) ;
#53431 = CARTESIAN_POINT ( 'NONE',  ( 8.755786719645998417, 3.934709392726489785, -8.402920843186199917 ) ) ;
#53432 = VERTEX_POINT ( 'NONE', #57396 ) ;
#53433 = CARTESIAN_POINT ( 'NONE',  ( 11.50962052873067698, -4.169679534937900556, -6.639752069194234885 ) ) ;
#53434 = EDGE_CURVE ( 'NONE', #34256, #2379, #30810, .T. ) ;
#53435 = CARTESIAN_POINT ( 'NONE',  ( 11.08492721656000057, 3.668390701878999849, 5.558148445539999649 ) ) ;
#53436 = EDGE_CURVE ( 'NONE', #28950, #33864, #28883, .T. ) ;
#53437 = CARTESIAN_POINT ( 'NONE',  ( 10.90000000000000036, 4.000000000000000000, -7.500000000000000000 ) ) ;
#53438 = CARTESIAN_POINT ( 'NONE',  ( 11.39835090130999973, -3.121033016283800254, 6.956352367771000189 ) ) ;
#53439 = CARTESIAN_POINT ( 'NONE',  ( 18.35295676019000055, 2.690485605734000085, -11.48482900035000043 ) ) ;
#53440 = CARTESIAN_POINT ( 'NONE',  ( 11.24441369783139777, 3.956299011112040187, -8.365094684940499903 ) ) ;
#53441 = CARTESIAN_POINT ( 'NONE',  ( 12.60374982967590185, -0.5917829749564905706, 12.68143435689271215 ) ) ;
#53442 = CARTESIAN_POINT ( 'NONE',  ( 8.365056901398830291, 2.650139792115765669, -7.500003826568613086 ) ) ;
#53443 = DIRECTION ( 'NONE',  ( -1.000000000000000000, 0.000000000000000000, 0.000000000000000000 ) ) ;
#53444 = CARTESIAN_POINT ( 'NONE',  ( 11.83178351958400043, -3.316209711830000018, 11.22342786695999983 ) ) ;
#53445 = ORIENTED_EDGE ( 'NONE', *, *, #30125, .F. ) ;
#53446 = DIRECTION ( 'NONE',  ( 0.000000000000000000, -0.9466492601157000530, 0.3222656952305000266 ) ) ;
#53447 = CARTESIAN_POINT ( 'NONE',  ( 7.061538849395999407, 1.118341376545999966, -0.1779135255794999926 ) ) ;
#53448 = CARTESIAN_POINT ( 'NONE',  ( 17.77689708618907005, 3.084393760937525375, 13.53193451522998103 ) ) ;
#53449 = EDGE_CURVE ( 'NONE', #64300, #16312, #47527, .T. ) ;
#53450 = CARTESIAN_POINT ( 'NONE',  ( 10.68942872719545001, 4.875347057626597369, 4.799721330339216330 ) ) ;
#53451 = B_SPLINE_CURVE_WITH_KNOTS ( 'NONE', 3,
 ( #30123, #18589, #39564, #60888, #24169, #35020 ),
 .UNSPECIFIED., .F., .F.,
 ( 4, 2, 4 ),
 ( 0.000000000000000000, 0.5000000000000000000, 1.000000000000000000 ),
 .UNSPECIFIED. ) ;
#53452 = CARTESIAN_POINT ( 'NONE',  ( 10.23103300763299828, -3.307558760216100069, -8.226274395107198600 ) ) ;
#53453 = ORIENTED_EDGE ( 'NONE', *, *, #20682, .F. ) ;
#53454 = CARTESIAN_POINT ( 'NONE',  ( 10.98768538770000092, -2.700669876604000041, 4.945210823433001224 ) ) ;
#53455 = EDGE_CURVE ( 'NONE', #29277, #23594, #4948, .T. ) ;
#53456 = CARTESIAN_POINT ( 'NONE',  ( 9.266851002542999538, -2.832432432432000269, 6.822293592207000934 ) ) ;
#53459 = DIRECTION ( 'NONE',  ( -1.000000000000000000, 0.000000000000000000, 0.000000000000000000 ) ) ;
#53458 = CARTESIAN_POINT ( 'NONE',  ( 9.003345280414000840, 2.319062457810000311, -7.919229449146000022 ) ) ;
#53457 = UNCERTAINTY_MEASURE_WITH_UNIT (LENGTH_MEASURE( 1.000000000000000082E-05 ), #64053, 'distance_accuracy_value', 'NONE');
#53460 = CARTESIAN_POINT ( 'NONE',  ( 2.645785826631131155, -0.2223228057201264707, -3.250327251304248044 ) ) ;
#53461 = EDGE_LOOP ( 'NONE', ( #6115, #7309, #27281, #29166 ) ) ;
#53462 = CARTESIAN_POINT ( 'NONE',  ( 9.423523952092001110, 4.993991073313000406, 8.578107851305000864 ) ) ;
#53464 = CARTESIAN_POINT ( 'NONE',  ( 17.57587588171171689, -3.124999410540973521, -13.52078618842887181 ) ) ;
#53463 = VECTOR ( 'NONE', #6150, 1000.000000000000000 ) ;
#53465 = CARTESIAN_POINT ( 'NONE',  ( 11.65871932425156920, 3.852858594438699935, 6.507377093516500288 ) ) ;
#53466 = CARTESIAN_POINT ( 'NONE',  ( 9.980430903642000473, -4.047223565251000466, 9.090364706348999846 ) ) ;
#53467 = CARTESIAN_POINT ( 'NONE',  ( 7.037120559622001004, -4.623636604834999275, 8.651469651195000665 ) ) ;
#53468 = ORIENTED_EDGE ( 'NONE', *, *, #466, .T. ) ;
#53469 = CARTESIAN_POINT ( 'NONE',  ( 9.021579719592999425, 2.193665972875999959, 7.400591513898000073 ) ) ;
#53471 = CARTESIAN_POINT ( 'NONE',  ( 10.05463185321000097, -3.531218470783999752, -9.119231780812000920 ) ) ;
#53470 = CARTESIAN_POINT ( 'NONE',  ( 11.04298866606778162, 3.494581883632823516, -6.786808489985508785 ) ) ;
#53472 = CARTESIAN_POINT ( 'NONE',  ( 7.790883244326107793, -4.713827597390799262, 9.089417837454107030 ) ) ;
#53473 = CARTESIAN_POINT ( 'NONE',  ( 10.00137895011999944, -3.855365288061999962, 5.709482985498999241 ) ) ;
#53474 = CARTESIAN_POINT ( 'NONE',  ( 1.452382716471000146, -1.124102084663000101, 3.059032707631999859 ) ) ;
#53475 = VERTEX_POINT ( 'NONE', #42369 ) ;
#53476 = CARTESIAN_POINT ( 'NONE',  ( 9.477263540182331525, 3.370476274536374106, -8.592232985442821658 ) ) ;
#53477 = CARTESIAN_POINT ( 'NONE',  ( 11.98225819896750011, -5.120994791668000090, 7.288668995979000087 ) ) ;
#53478 = CARTESIAN_POINT ( 'NONE',  ( 10.25149413291699929, 5.037815157227999663, 7.973529073237199505 ) ) ;
#53479 = ORIENTED_EDGE ( 'NONE', *, *, #16800, .T. ) ;
#53480 = B_SPLINE_SURFACE_WITH_KNOTS ( 'NONE', 3, 3, ( 
 ( #63840, #5802, #26806, #53022, #26454, #5118, #42875, #47787, #11060, #69096, #37620, #15954, #64868, #53709, #27145, #37284, #31700, #48465, #16641, #58261, #54047, #573, #64523, #42531, #37968, #16981, #59288, #11393, #32732, #6145, #38313, #10020, #58604, #31358, #52672 ),
 ( #4766, #68742, #42197, #15617, #63497, #36947, #10365, #65914, #7890, #60679, #29224, #6844, #12793, #18042, #7197, #34122, #33775, #28888, #18383, #34474, #33428, #55440, #22922, #50536, #12443, #28178, #23616, #27844, #55090, #59641, #54394, #28533, #49846, #39358, #55785 ),
 ( #33080, #6497, #7533, #12097, #44274, #39019, #44958, #23278, #11737, #50197, #2297, #2638, #65571, #17337, #22575, #49149, #17694, #49494, #66262, #1260, #39705, #44620, #61027, #13144, #23965, #1605, #45299, #66606, #60337, #1956, #43918, #18724, #54745, #38666, #65222 ),
 ( #59985, #61707, #4343, #56120, #40723, #24990, #8232, #62051, #51896, #47009, #51223, #13824, #62393, #25676, #45644, #29579, #3318, #35153, #57144, #9242, #68310, #46324, #3994, #24653, #56468, #40059, #62723, #30252, #41417, #14508, #25330, #8912, #41072, #19402, #14168 ) ),
 .UNSPECIFIED., .F., .F., .F.,
 ( 4, 4 ),
 ( 4, 1, 1, 1, 1, 1, 1, 1, 1, 1, 1, 1, 1, 1, 1, 1, 1, 1, 1, 1, 1, 1, 1, 1, 1, 1, 1, 1, 1, 1, 1, 1, 4 ),
 ( -0.1039370721279000015, 1.103937072127999963 ),
 ( -0.02000000000000000042, 0.01250000000000000069, 0.04499999999999999833, 0.07749999999999999944, 0.1100000000000000006, 0.1424999999999999878, 0.1749999999999999889, 0.2074999999999999900, 0.2399999999999999911, 0.2725000000000000200, 0.3049999999999999933, 0.3375000000000000222, 0.3699999999999999956, 0.4025000000000000244, 0.4349999999999999978, 0.4675000000000000266, 0.5000000000000000000, 0.5324999999999999734, 0.5649999999999999467, 0.5975000000000000311, 0.6300000000000000044, 0.6624999999999999778, 0.6949999999999999512, 0.7275000000000000355, 0.7600000000000000089, 0.7924999999999999822, 0.8249999999999999556, 0.8575000000000000400, 0.8900000000000000133, 0.9224999999999999867, 0.9549999999999999600, 0.9875000000000000444, 1.020000000000000018 ),
 .UNSPECIFIED. ) ;
#53481 = CARTESIAN_POINT ( 'NONE',  ( 8.564679719593000229, 4.146787477634999775, -5.941926545671999627 ) ) ;
#53482 = CARTESIAN_POINT ( 'NONE',  ( 12.68566995881735870, 1.770266656024989116, -12.47502217142794478 ) ) ;
#53483 = CARTESIAN_POINT ( 'NONE',  ( 11.76723293495529887, -5.173938955706000264, 7.547192037433419820 ) ) ;
#53484 = B_SPLINE_CURVE_WITH_KNOTS ( 'NONE', 3,
 ( #64670, #11193, #10850, #12241, #33566 ),
 .UNSPECIFIED., .F., .F.,
 ( 4, 1, 4 ),
 ( 0.000000000000000000, 0.5000000000000000000, 1.000000000000000000 ),
 .UNSPECIFIED. ) ;
#53485 = FACE_OUTER_BOUND ( 'NONE', #58296, .T. ) ;
#53486 = CARTESIAN_POINT ( 'NONE',  ( 18.16762906240600017, 2.624018810214213460, -13.64637396502920019 ) ) ;
#53487 = ORIENTED_EDGE ( 'NONE', *, *, #34379, .T. ) ;
#53488 = DIRECTION ( 'NONE',  ( 0.000000000000000000, 1.000000000000000000, 0.000000000000000000 ) ) ;
#53489 = CARTESIAN_POINT ( 'NONE',  ( 9.303275160948496492, -5.099670516381894281, -6.884602962369688051 ) ) ;
#53490 = EDGE_LOOP ( 'NONE', ( #20171, #14087, #64138, #57103, #49101, #20801, #66998, #47408, #31723, #66310 ) ) ;
#53491 = CARTESIAN_POINT ( 'NONE',  ( 12.39015342239249762, -3.070413439580835568, -12.22017215029075032 ) ) ;
#53492 = CARTESIAN_POINT ( 'NONE',  ( 10.40749413291699987, 4.788043169210699723, 7.859564368461399830 ) ) ;
#53493 = EDGE_CURVE ( 'NONE', #68077, #6526, #53345, .T. ) ;
#53494 = CARTESIAN_POINT ( 'NONE',  ( 24.30000000000000071, -8.756202924575998026, 7.455126447192999883 ) ) ;
#53495 = ADVANCED_FACE ( 'NONE', ( #53194 ), #46920, .F. ) ;
#53496 = CARTESIAN_POINT ( 'NONE',  ( 10.15787172175999942, 4.213497149090000171, -5.822953133183999874 ) ) ;
#53497 = CARTESIAN_POINT ( 'NONE',  ( 7.643735281411005111, 4.861037469149006363, 6.423817941563998879 ) ) ;
#53498 = CARTESIAN_POINT ( 'NONE',  ( 11.05935368890999904, -2.480241580537000168, 6.610077204591000566 ) ) ;
#53499 = CARTESIAN_POINT ( 'NONE',  ( 17.56702613447739481, -0.7192913015564690316, -12.57945229205062354 ) ) ;
#53500 = CARTESIAN_POINT ( 'NONE',  ( 9.004750526303645586, 5.259872394538027685, 7.984454890150045614 ) ) ;
#53501 = CARTESIAN_POINT ( 'NONE',  ( 10.72333863405319931, -3.380905141010200232, -8.289729326049599223 ) ) ;
#53503 = CARTESIAN_POINT ( 'NONE',  ( 8.534482780410998615, 3.011620138462000273, 8.801434747080000065 ) ) ;
#53502 = B_SPLINE_CURVE_WITH_KNOTS ( 'NONE', 3,
 ( #13659, #66787, #54576, #44449 ),
 .UNSPECIFIED., .F., .F.,
 ( 4, 4 ),
 ( 0.000000000000000000, 1.000000000000000000 ),
 .UNSPECIFIED. ) ;
#53505 = VERTEX_POINT ( 'NONE', #12272 ) ;
#53504 = B_SPLINE_CURVE_WITH_KNOTS ( 'NONE', 3,
 ( #43911, #6489, #33768, #59978, #64516, #17330, #43562, #27480 ),
 .UNSPECIFIED., .F., .F.,
 ( 4, 2, 2, 4 ),
 ( 0.000000000000000000, 0.2500000000000018319, 0.5000000000000036637, 1.000000000000000000 ),
 .UNSPECIFIED. ) ;
#53506 = LINE ( 'NONE', #46888, #6803 ) ;
#53507 = DIRECTION ( 'NONE',  ( 1.000000000000000000, 0.000000000000000000, 0.000000000000000000 ) ) ;
#53508 = DIRECTION ( 'NONE',  ( 0.7660444431190069903, 0.000000000000000000, 0.6427876096865049460 ) ) ;
#53509 = B_SPLINE_CURVE_WITH_KNOTS ( 'NONE', 3,
 ( #36165, #9584, #43484, #52934 ),
 .UNSPECIFIED., .F., .F.,
 ( 4, 4 ),
 ( 0.000000000000000000, 1.000000000000000000 ),
 .UNSPECIFIED. ) ;
#53510 = CARTESIAN_POINT ( 'NONE',  ( 18.22068658462131197, 2.765866853816869142, 12.29268492208001540 ) ) ;
#53511 = DIRECTION ( 'NONE',  ( 0.000000000000000000, -1.000000000000000000, 0.000000000000000000 ) ) ;
#53512 = CARTESIAN_POINT ( 'NONE',  ( 11.01861045693000030, 7.589698685664999722, 6.381113859002999433 ) ) ;
#53513 = DIRECTION ( 'NONE',  ( 1.000000000000000000, 0.000000000000000000, 0.000000000000000000 ) ) ;
#53514 = CARTESIAN_POINT ( 'NONE',  ( 12.80505043854146940, -1.845938772038641318, 13.81933890150171074 ) ) ;
#53515 = EDGE_CURVE ( 'NONE', #57153, #38028, #38843, .T. ) ;
#53516 = EDGE_LOOP ( 'NONE', ( #57012, #19523, #22773, #44886, #27260 ) ) ;
#53517 = CARTESIAN_POINT ( 'NONE',  ( 12.20599951553718832, -2.074681531931807488, 12.42802467457380367 ) ) ;
#53518 = EDGE_CURVE ( 'NONE', #43577, #25042, #41703, .T. ) ;
#53519 = CARTESIAN_POINT ( 'NONE',  ( 10.16159632033899918, -4.929952350555500296, -7.120485934352199564 ) ) ;
#53520 = CARTESIAN_POINT ( 'NONE',  ( 11.36669567114815749, 11.69740569349575843, 1.420376822756192592 ) ) ;
#53521 = CARTESIAN_POINT ( 'NONE',  ( 10.99934110471000004, -5.081022574063999819, 8.239050178861999640 ) ) ;
#53522 = CARTESIAN_POINT ( 'NONE',  ( 11.32179975933729921, -3.051121678931899783, 7.826467126457498757 ) ) ;
#53523 = EDGE_CURVE ( 'NONE', #66927, #30301, #68303, .T. ) ;
#53524 = CARTESIAN_POINT ( 'NONE',  ( 11.45764291764649911, 2.867875922590999771, -7.360052904210999891 ) ) ;
#53525 = CARTESIAN_POINT ( 'NONE',  ( 12.54953071380263196, 0.6732419856523105262, 12.58200148172923960 ) ) ;
#53526 = CARTESIAN_POINT ( 'NONE',  ( 0.1949759624410999925, 3.323048643578999872, -0.5818070024050000510 ) ) ;
#53527 = CARTESIAN_POINT ( 'NONE',  ( 9.814910518647794291, 2.650130971540564317, -7.499994893876710478 ) ) ;
#53528 = CARTESIAN_POINT ( 'NONE',  ( 12.80505043854143388, 1.760910691117812510, 12.47634535983623394 ) ) ;
#53530 = CARTESIAN_POINT ( 'NONE',  ( 9.115118560745049336, 5.349923934101355805, -7.499992884230159973 ) ) ;
#53529 = CARTESIAN_POINT ( 'NONE',  ( 9.353076168957999315, 3.420574098817999786, -8.483869947211399420 ) ) ;
#53531 = CARTESIAN_POINT ( 'NONE',  ( 11.18687482311539938, 5.057677595549000316, -7.927326830586499007 ) ) ;
#53532 = CARTESIAN_POINT ( 'NONE',  ( 12.74229120054512343, 12.11986439831269635, -3.159827838237255992 ) ) ;
#53533 = CARTESIAN_POINT ( 'NONE',  ( 10.19121415877000203, 3.990707652596999555, -5.651362387566000400 ) ) ;
#53534 = CARTESIAN_POINT ( 'NONE',  ( 11.25962254157670905, 4.169672662336058266, 6.639751609450684100 ) ) ;
#53536 = CARTESIAN_POINT ( 'NONE',  ( 12.22445834451951541, 2.731426566208313922, 12.39462880880582318 ) ) ;
#53535 = CARTESIAN_POINT ( 'NONE',  ( 12.65361178023557009, 10.78680294140104046, -4.401676341640982315 ) ) ;
#53537 = AXIS2_PLACEMENT_3D ( 'NONE', #51909, #4006, #57848 ) ;
#53538 = CARTESIAN_POINT ( 'NONE',  ( 8.800594747508441174, 2.899999999999999911, -6.515385012870885895 ) ) ;
#53539 = ORIENTED_EDGE ( 'NONE', *, *, #31188, .T. ) ;
#53540 = CARTESIAN_POINT ( 'NONE',  ( 12.54858945031608997, 0.5700410258791628326, 12.68277524907516884 ) ) ;
#53541 = EDGE_CURVE ( 'NONE', #62494, #24573, #23096, .T. ) ;
#53542 = CARTESIAN_POINT ( 'NONE',  ( 15.90000000000360991, 3.781197540827905712, 11.56430939782970668 ) ) ;
#53543 = CYLINDRICAL_SURFACE ( 'NONE', #58609, 1.350000000000000533 ) ;
#53544 = CARTESIAN_POINT ( 'NONE',  ( 8.741151519676998660, 4.018750234858180725, 6.633192605878799775 ) ) ;
#53545 = CARTESIAN_POINT ( 'NONE',  ( 12.18118526251765665, -2.542711865659281756, 13.66432766657963960 ) ) ;
#53546 = CARTESIAN_POINT ( 'NONE',  ( 12.22105292102199137, 2.722876829147647282, 13.62360956004511792 ) ) ;
#53547 = CARTESIAN_POINT ( 'NONE',  ( 24.45366336996499967, 3.540551434415999843, -12.31827634870000132 ) ) ;
#53548 = ORIENTED_EDGE ( 'NONE', *, *, #31349, .F. ) ;
#53549 = DIRECTION ( 'NONE',  ( 0.7071067617951957152, 0.000000000000000000, -0.7071068005778986532 ) ) ;
#53550 = DIRECTION ( 'NONE',  ( -1.000000000000000000, 0.000000000000000000, 0.000000000000000000 ) ) ;
#53551 = DIRECTION ( 'NONE',  ( -1.000000000000000000, 0.000000000000000000, 0.000000000000000000 ) ) ;
#53552 = CARTESIAN_POINT ( 'NONE',  ( 10.96126252468000040, 5.100438257636001005, -4.932323065253000571 ) ) ;
#53553 = CARTESIAN_POINT ( 'NONE',  ( 18.02645743154359081, 2.910866584900387188, -12.34632125423082982 ) ) ;
#53554 = CARTESIAN_POINT ( 'NONE',  ( 17.60000000000000142, -11.23412379136000006, 3.084957477885999833 ) ) ;
#53555 = CARTESIAN_POINT ( 'NONE',  ( 8.356851002541000994, 2.832432432432000269, -6.822293592207000934 ) ) ;
#53556 = CARTESIAN_POINT ( 'NONE',  ( 5.449999267937000624, 6.217248937900999058E-14, 3.708144902247999495E-14 ) ) ;
#53557 = CARTESIAN_POINT ( 'NONE',  ( 10.69829435321000055, -2.534030585780999711, -6.667788699001999220 ) ) ;
#53558 = PLANE ( 'NONE',  #12050 ) ;
#53559 = CARTESIAN_POINT ( 'NONE',  ( 9.520528907821001141, -2.899999999999999911, 6.152188490330000370 ) ) ;
#53560 = CARTESIAN_POINT ( 'NONE',  ( 24.56500367226799852, 12.27494567759000077, 3.065703875465999761 ) ) ;
#53561 = CARTESIAN_POINT ( 'NONE',  ( 0.8009734658753000502, -3.500000000000000000, 0.000000000000000000 ) ) ;
#53562 = ORIENTED_EDGE ( 'NONE', *, *, #22869, .F. ) ;
#53563 = CARTESIAN_POINT ( 'NONE',  ( 8.704995280412999747, 5.140767546012999567, -6.196177269779999719 ) ) ;
#53564 = CARTESIAN_POINT ( 'NONE',  ( 11.84287482311539996, -3.196874704906699893, 7.175518335304800210 ) ) ;
#53565 = ORIENTED_EDGE ( 'NONE', *, *, #5393, .T. ) ;
#53566 = CARTESIAN_POINT ( 'NONE',  ( 13.55676532396020484, 12.34669046015806337, 2.106274408591566338 ) ) ;
#53567 = CARTESIAN_POINT ( 'NONE',  ( 11.57656516821460890, -3.100463633631699967, -8.407828142327998577 ) ) ;
#53568 = VERTEX_POINT ( 'NONE', #59811 ) ;
#53569 = CARTESIAN_POINT ( 'NONE',  ( 10.44999293566599974, 4.720032669050099550, 6.616719557880299085 ) ) ;
#53570 = DIRECTION ( 'NONE',  ( 0.4384236320214023319, 0.000000000000000000, 0.8987684456439056779 ) ) ;
#53571 = CARTESIAN_POINT ( 'NONE',  ( 23.67740124563481174, 3.195736743838564209, -13.38333689704936091 ) ) ;
#53572 = EDGE_CURVE ( 'NONE', #53921, #32830, #34160, .T. ) ;
#53573 = CARTESIAN_POINT ( 'NONE',  ( 18.38722619340700248, -3.117741388420999904, 11.18549237633000004 ) ) ;
#53574 = EDGE_CURVE ( 'NONE', #66683, #22688, #48640, .T. ) ;
#53575 = CARTESIAN_POINT ( 'NONE',  ( 9.356463691918067482, -5.100000000000000533, 6.665341197419115460 ) ) ;
#53576 = CARTESIAN_POINT ( 'NONE',  ( 12.47664075733698219, 0.5322329922976065664, -13.88628950328449285 ) ) ;
#53577 = CARTESIAN_POINT ( 'NONE',  ( 7.133860169640499294, 0.8910540846543333338, 0.7159253625619631523 ) ) ;
#53578 = DIRECTION ( 'NONE',  ( -1.000000000000000000, 0.000000000000000000, 0.000000000000000000 ) ) ;
#53579 = CARTESIAN_POINT ( 'NONE',  ( 13.19211270977099915, 11.64284154253999937, 1.888701237101999997 ) ) ;
#53580 = ORIENTED_EDGE ( 'NONE', *, *, #31205, .T. ) ;
#53581 = CARTESIAN_POINT ( 'NONE',  ( 8.631645280409999899, 3.826300099041999747, -9.055335252254000267 ) ) ;
#53582 = ORIENTED_EDGE ( 'NONE', *, *, #5292, .F. ) ;
#53583 = CIRCLE ( 'NONE', #15652, 6.772075922005999615 ) ;
#53584 = CARTESIAN_POINT ( 'NONE',  ( 24.54174074949149897, -12.46120270595140234, 3.023779783212969363 ) ) ;
#53585 = FILL_AREA_STYLE_COLOUR ( '', #22008 ) ;
#53586 = VERTEX_POINT ( 'NONE', #740 ) ;
#53587 = CARTESIAN_POINT ( 'NONE',  ( 8.769442991499998286, 3.919472480837189909, 8.776675254768999679 ) ) ;
#53588 = CARTESIAN_POINT ( 'NONE',  ( 18.14695621644404611, -2.700933560328190985, -12.40248159148175944 ) ) ;
#53589 = CARTESIAN_POINT ( 'NONE',  ( 24.77780260647635657, -8.621837834250825949, 8.548044453014501443 ) ) ;
#53590 = CARTESIAN_POINT ( 'NONE',  ( 10.25851354018279160, 4.163624617374472869, -6.250000000000000888 ) ) ;
#53591 = FACE_OUTER_BOUND ( 'NONE', #6020, .T. ) ;
#53592 = CARTESIAN_POINT ( 'NONE',  ( 12.39257741226468390, 0.4700078255514595904, 13.88931146942756811 ) ) ;
#53593 = ORIENTED_EDGE ( 'NONE', *, *, #31763, .T. ) ;
#53594 = CARTESIAN_POINT ( 'NONE',  ( 12.27593309678900191, 11.75515418280000013, -3.561236062516000000 ) ) ;
#53595 = CARTESIAN_POINT ( 'NONE',  ( 17.56813469587400434, 11.44347843772000139, -4.696234928490000904 ) ) ;
#53596 = CARTESIAN_POINT ( 'NONE',  ( 9.581508192411627434, 3.220001783077621305, 7.896402636871828307 ) ) ;
#53597 = CARTESIAN_POINT ( 'NONE',  ( 4.407312471546000587, -0.7071374513468999812, -0.8783066828273999871 ) ) ;
#53598 = EDGE_CURVE ( 'NONE', #56839, #66643, #8270, .T. ) ;
#53599 = CARTESIAN_POINT ( 'NONE',  ( 11.48513281071060277, 2.915426916004881353, 7.175000865651856685 ) ) ;
#53600 = CARTESIAN_POINT ( 'NONE',  ( 18.04816728597000264, -3.610133590554000182, 12.03375048192000207 ) ) ;
#53601 = CARTESIAN_POINT ( 'NONE',  ( 10.60198654464000079, -2.164987663130000239, -7.764523632348000248 ) ) ;
#53602 = ORIENTED_EDGE ( 'NONE', *, *, #23607, .F. ) ;
#53603 = EDGE_LOOP ( 'NONE', ( #32663, #37843, #34807, #37880 ) ) ;
#53604 = CARTESIAN_POINT ( 'NONE',  ( 17.55505043854144276, 0.6250000000000001110, -13.88107975066922428 ) ) ;
#53605 = CARTESIAN_POINT ( 'NONE',  ( 10.90000000000000036, -5.100000000000000533, -6.436740704805999691 ) ) ;
#53606 = CARTESIAN_POINT ( 'NONE',  ( 18.20361801365685750, -2.140066979970441263, 13.83614404522478480 ) ) ;
#53607 = CARTESIAN_POINT ( 'NONE',  ( 7.000000000000000000, -9.735955015381000166, 5.735955015381000166 ) ) ;
#53608 = CARTESIAN_POINT ( 'NONE',  ( 6.021693173016668510, -0.7554284705563544255, 1.310679582531384169 ) ) ;
#53609 = CARTESIAN_POINT ( 'NONE',  ( -15.86200481174999943, -5.599999999999999645, -6.571291218949999902 ) ) ;
#53610 = CARTESIAN_POINT ( 'NONE',  ( 9.256734463322999318, 4.090312251411050148, -8.362294405496898619 ) ) ;
#53612 = CARTESIAN_POINT ( 'NONE',  ( 8.341525531978778218, 4.649628395467509279, -6.060028403045727430 ) ) ;
#53611 = CARTESIAN_POINT ( 'NONE',  ( 10.73758376188599861, -4.847012523549299345, 6.960174024681499816 ) ) ;
#53613 = B_SPLINE_CURVE_WITH_KNOTS ( 'NONE', 3,
 ( #47345, #57823, #57138, #19743 ),
 .UNSPECIFIED., .F., .F.,
 ( 4, 4 ),
 ( 0.000000000000000000, 1.000000000000000000 ),
 .UNSPECIFIED. ) ;
#53614 = CARTESIAN_POINT ( 'NONE',  ( 8.166819129144998968, -2.890362633264002667, 6.359808956951005676 ) ) ;
#53615 = ORIENTED_EDGE ( 'NONE', *, *, #2157, .F. ) ;
#53616 = ADVANCED_FACE ( 'NONE', ( #43744 ), #65041, .T. ) ;
#53617 = CARTESIAN_POINT ( 'NONE',  ( 10.89874164595999950, -2.834836218627000193, 9.088455567997000273 ) ) ;
#53618 = CARTESIAN_POINT ( 'NONE',  ( 9.834329965421998665, 3.206942993865000258, 6.678540912152799436 ) ) ;
#53619 = CARTESIAN_POINT ( 'NONE',  ( 5.700000000000000178, -13.04986661130000059, 1.811520473896000016 ) ) ;
#53620 = CARTESIAN_POINT ( 'NONE',  ( 9.781666627457001439, -5.464740618746000145, 8.817321229216000589 ) ) ;
#53621 = CARTESIAN_POINT ( 'NONE',  ( 18.07108758010737048, 2.852736468701840611, -12.36237742790534533 ) ) ;
#53622 = CARTESIAN_POINT ( 'NONE',  ( 11.00000000000000000, -3.008232475376599879, -7.174999999999999822 ) ) ;
#53623 = B_SPLINE_CURVE_WITH_KNOTS ( 'NONE', 3,
 ( #9451, #41624, #9116, #68522 ),
 .UNSPECIFIED., .F., .F.,
 ( 4, 4 ),
 ( 0.000000000000000000, 1.000000000000000000 ),
 .UNSPECIFIED. ) ;
#53624 = B_SPLINE_CURVE_WITH_KNOTS ( 'NONE', 3,
 ( #9974, #30619, #3353, #4027 ),
 .UNSPECIFIED., .F., .F.,
 ( 4, 4 ),
 ( 0.000000000000000000, 1.000000000000000000 ),
 .UNSPECIFIED. ) ;
#53625 = AXIS2_PLACEMENT_3D ( 'NONE', #36170, #4682, #24992 ) ;
#53626 = CARTESIAN_POINT ( 'NONE',  ( 10.46029575260939026, -3.171266584307757874, -8.253465265694870823 ) ) ;
#53627 = CARTESIAN_POINT ( 'NONE',  ( 9.231405316140000039, -4.184077495686000958, -8.347244604637999998 ) ) ;
#53628 = CARTESIAN_POINT ( 'NONE',  ( 5.778946504885999147, -1.272350122907000003, -0.3600015818555999947 ) ) ;
#53629 = B_SPLINE_SURFACE_WITH_KNOTS ( 'NONE', 3, 3, ( 
 ( #9925, #20415, #9573, #24291 ),
 ( #3977, #62710, #35138, #62378 ),
 ( #56451, #62035, #29904, #40709 ),
 ( #8556, #35480, #52228, #8898 ),
 ( #30237, #51542, #41057, #25317 ),
 ( #57131, #41743, #9228, #51881 ),
 ( #30567, #63044, #46653, #59193 ),
 ( #27385, #10960, #48713, #58165 ) ),
 .UNSPECIFIED., .F., .F., .F.,
 ( 4, 1, 1, 1, 1, 4 ),
 ( 4, 4 ),
 ( 0.7452945369162999878, 0.7647058823529000460, 0.8235294117646999590, 0.8823529411764999830, 0.9411764705882000870, 0.9905759319504999771 ),
 ( -0.1831087563478999980, 1.182948900798000080 ),
 .UNSPECIFIED. ) ;
#53630 = CARTESIAN_POINT ( 'NONE',  ( 11.39529697814177744, -3.173432105636238454, 7.784385510031588851 ) ) ;
#53631 = DIRECTION ( 'NONE',  ( 0.000000000000000000, -0.9553735099700838562, 0.2954005017724949944 ) ) ;
#53632 = ORIENTED_EDGE ( 'NONE', *, *, #8103, .T. ) ;
#53633 = CARTESIAN_POINT ( 'NONE',  ( 12.47441792805236815, 0.5304820368560160260, -12.68508456201359991 ) ) ;
#53634 = CARTESIAN_POINT ( 'NONE',  ( 11.63825819896753977, 3.148796120250299868, -7.660469764776300039 ) ) ;
#53635 = CARTESIAN_POINT ( 'NONE',  ( 9.447682302133550536, -5.285671839984060760, 7.027659275301481046 ) ) ;
#53636 = DIRECTION ( 'NONE',  ( 0.000000000000000000, 1.000000000000000000, 0.000000000000000000 ) ) ;
#53637 = DIRECTION ( 'NONE',  ( 1.000000000000000000, 0.000000000000000000, 0.000000000000000000 ) ) ;
#53638 = ORIENTED_EDGE ( 'NONE', *, *, #10640, .F. ) ;
#53639 = CARTESIAN_POINT ( 'NONE',  ( 25.18910272528800220, -11.36135965050999985, -3.216800270569000197 ) ) ;
#53640 = CARTESIAN_POINT ( 'NONE',  ( 10.82035090130999855, -3.241273085157000189, -7.969278253227299658 ) ) ;
#53641 = CARTESIAN_POINT ( 'NONE',  ( 18.11727294764897067, 0.2737714783216526060, 12.69604447593775198 ) ) ;
#53642 = CARTESIAN_POINT ( 'NONE',  ( 10.38559687351649963, -5.092232985442824322, 6.870476274536375882 ) ) ;
#53643 = CARTESIAN_POINT ( 'NONE',  ( 11.49999672495000524, -7.851643750443679792, 8.692270414123820288 ) ) ;
#53644 = CARTESIAN_POINT ( 'NONE',  ( 10.57102344389999971, 3.237334151971200225, -7.037150754511299233 ) ) ;
#53645 = ORIENTED_EDGE ( 'NONE', *, *, #64851, .F. ) ;
#53646 = CARTESIAN_POINT ( 'NONE',  ( 9.910640133503999749, -2.107273866476999657, 7.885282692430999774 ) ) ;
#53647 = CARTESIAN_POINT ( 'NONE',  ( 17.75779383521792099, 3.091556742956585779, -13.53003950643005204 ) ) ;
#53648 = ORIENTED_EDGE ( 'NONE', *, *, #61441, .F. ) ;
#53649 = LINE ( 'NONE', #63785, #32874 ) ;
#53650 = CARTESIAN_POINT ( 'NONE',  ( 8.791230646795000325, -5.095088356574999366, 6.286978111459999852 ) ) ;
#53651 = CARTESIAN_POINT ( 'NONE',  ( 15.48018231457700189, 8.819832297131000587, 7.692419064155999742 ) ) ;
#53652 = EDGE_CURVE ( 'NONE', #35693, #59934, #46662, .T. ) ;
#53653 = ORIENTED_EDGE ( 'NONE', *, *, #59426, .F. ) ;
#53654 = DIRECTION ( 'NONE',  ( -0.8987684456439055669, 0.000000000000000000, -0.4384236320214022764 ) ) ;
#53656 = EDGE_CURVE ( 'NONE', #60101, #26192, #52313, .T. ) ;
#53655 = B_SPLINE_CURVE_WITH_KNOTS ( 'NONE', 3,
 ( #61305, #13425, #28112, #34746, #56055, #49424, #1537, #44206, #61645, #19690, #24241, #18996, #46262, #41011, #51838, #20370, #41694, #30524 ),
 .UNSPECIFIED., .F., .F.,
 ( 4, 2, 2, 2, 2, 2, 2, 2, 4 ),
 ( 0.000000000000000000, 0.1250000000000000000, 0.2500000000000000000, 0.3750000000000000000, 0.5000000000000000000, 0.6250000000000000000, 0.7500000000000000000, 0.8750000000000000000, 1.000000000000000000 ),
 .UNSPECIFIED. ) ;
#53657 = B_SPLINE_CURVE_WITH_KNOTS ( 'NONE', 3,
 ( #50384, #8767, #2483, #7731, #46518, #24845, #50730, #66452, #30109, #9102, #19945, #55632, #51751, #51412, #14016 ),
 .UNSPECIFIED., .F., .F.,
 ( 4, 2, 2, 1, 2, 2, 2, 4 ),
 ( 0.000000000000000000, 0.1250000000000078271, 0.1875000000000136280, 0.2187500000000169031, 0.2343750000000154321, 0.2500000000000139333, 0.5000000000000107692, 1.000000000000000000 ),
 .UNSPECIFIED. ) ;
#53658 = CARTESIAN_POINT ( 'NONE',  ( 7.812560841224999386, 5.525377065333000104, -6.367402836891999485 ) ) ;
#53659 = CARTESIAN_POINT ( 'NONE',  ( 8.753190465598311931, 3.015364744815148601, -8.459884657046686129 ) ) ;
#53660 = EDGE_CURVE ( 'NONE', #8893, #66228, #38947, .T. ) ;
#53661 = CARTESIAN_POINT ( 'NONE',  ( 7.100000000000000533, -12.50865771883999855, 2.924687089724999911 ) ) ;
#53662 = ORIENTED_EDGE ( 'NONE', *, *, #16250, .T. ) ;
#53663 = CARTESIAN_POINT ( 'NONE',  ( 9.290195424034999760, -2.377814350880000038, 7.540992175424999999 ) ) ;
#53664 = EDGE_CURVE ( 'NONE', #15952, #1219, #49123, .T. ) ;
#53665 = CARTESIAN_POINT ( 'NONE',  ( 8.299720885770000223, 3.399999999999999911, -6.084164326786999588 ) ) ;
#53666 = CARTESIAN_POINT ( 'NONE',  ( 11.28830977893787768, 3.023401864784706738, -6.673569913327193959 ) ) ;
#53667 = VERTEX_POINT ( 'NONE', #24484 ) ;
#53668 = CARTESIAN_POINT ( 'NONE',  ( 6.263359839683333874, 1.310679582531388387, -0.7554284705563470981 ) ) ;
#53669 = CARTESIAN_POINT ( 'NONE',  ( 11.50001258332000020, 11.56502147876000031, 1.404302031979000054 ) ) ;
#53670 = VERTEX_POINT ( 'NONE', #39530 ) ;
#53671 = CARTESIAN_POINT ( 'NONE',  ( 24.39664234077866567, 3.224866613683543992, 12.03536604998859083 ) ) ;
#53672 = CARTESIAN_POINT ( 'NONE',  ( 18.06968158350326092, 0.3547715225740352696, -13.89390930605025787 ) ) ;
#53673 = CARTESIAN_POINT ( 'NONE',  ( 4.579603349966000714, -0.4781559447700999832, -1.333338567780000039 ) ) ;
#53674 = CARTESIAN_POINT ( 'NONE',  ( 7.724132149008994475, 4.510524588886997144, -6.436036822971000326 ) ) ;
#53675 = CARTESIAN_POINT ( 'NONE',  ( 16.22798078375900133, 3.564332247067999671, 11.94996243427999971 ) ) ;
#53676 = DIRECTION ( 'NONE',  ( 0.000000000000000000, -1.000000000000000000, 0.000000000000000000 ) ) ;
#53677 = CARTESIAN_POINT ( 'NONE',  ( 3.240556799211292027, -3.500000000000003109, 0.4581489286484972667 ) ) ;
#53678 = AXIS2_PLACEMENT_3D ( 'NONE', #61603, #46564, #25579 ) ;
#53679 = ORIENTED_EDGE ( 'NONE', *, *, #58412, .T. ) ;
#53680 = CARTESIAN_POINT ( 'NONE',  ( 9.308000177250203677, -4.364660356823166332, 9.210564710512558761 ) ) ;
#53681 = VERTEX_POINT ( 'NONE', #30420 ) ;
#53682 = CARTESIAN_POINT ( 'NONE',  ( 10.24477918374999952, 5.265206995764999398, 8.959504263949002123 ) ) ;
#53683 = CARTESIAN_POINT ( 'NONE',  ( 10.98632665877000036, 3.015084670878999784, -9.064442106213000727 ) ) ;
#53684 = CIRCLE ( 'NONE', #35816, 12.59999999999999964 ) ;
#53685 = DIRECTION ( 'NONE',  ( 0.000000000000000000, -0.1218274111675000937, 0.9925512993736016476 ) ) ;
#53686 = CARTESIAN_POINT ( 'NONE',  ( 12.52680909801648390, 3.059742249080376286, -13.53867541207075220 ) ) ;
#53687 = DIRECTION ( 'NONE',  ( 0.000000000000000000, -1.000000000000000000, 0.000000000000000000 ) ) ;
#53688 = CARTESIAN_POINT ( 'NONE',  ( 7.000000000000000000, 7.356391799243646723, -3.356391799243647167 ) ) ;
#53689 = CARTESIAN_POINT ( 'NONE',  ( 18.17477505917495151, 0.08167545936615694391, 13.89968205666727386 ) ) ;
#53690 = LINE ( 'NONE', #37603, #10452 ) ;
#53691 = VERTEX_POINT ( 'NONE', #30089 ) ;
#53692 = CARTESIAN_POINT ( 'NONE',  ( 12.34511315269135778, 0.4233056299066624839, 13.89132630015666514 ) ) ;
#53693 = CARTESIAN_POINT ( 'NONE',  ( 11.53502897915239878, -3.672866099873000056, 6.264564938179000286 ) ) ;
#53694 = CARTESIAN_POINT ( 'NONE',  ( 10.19256470245000123, -2.560274838243000062, 7.664550593243999899 ) ) ;
#53695 = CARTESIAN_POINT ( 'NONE',  ( 18.06844887846742154, -0.3566139488127487156, -13.89384732036045023 ) ) ;
#53696 = CARTESIAN_POINT ( 'NONE',  ( 7.346668146792000087, -2.374041291348000016, 8.293390875797999939 ) ) ;
#53698 = CARTESIAN_POINT ( 'NONE',  ( 12.71479700542668922, -11.41062399033360819, 4.624005385416206870 ) ) ;
#53697 = CARTESIAN_POINT ( 'NONE',  ( 10.15902941591999920, 4.166415211384999040, 9.114163806478000396 ) ) ;
#53699 = CARTESIAN_POINT ( 'NONE',  ( 10.79303032197930001, 4.663532080728800544, -6.572090902022299730 ) ) ;
#53700 = CARTESIAN_POINT ( 'NONE',  ( 24.53003472522700434, -8.771519074185000875, -8.897032352648000852 ) ) ;
#53701 = EDGE_CURVE ( 'NONE', #32730, #65648, #37484, .T. ) ;
#53702 = FACE_OUTER_BOUND ( 'NONE', #20339, .T. ) ;
#53703 = CARTESIAN_POINT ( 'NONE',  ( 18.17180462559269571, 0.1017072266180434337, 12.69945743039634856 ) ) ;
#53704 = CARTESIAN_POINT ( 'NONE',  ( 6.933458400913999675, -12.41496613996999976, -2.805592698698999854 ) ) ;
#53705 = EDGE_CURVE ( 'NONE', #33649, #45386, #43309, .T. ) ;
#53706 = CARTESIAN_POINT ( 'NONE',  ( 24.02042701938200153, 9.295092309749000137, 9.129993563720001148 ) ) ;
#53707 = ORIENTED_EDGE ( 'NONE', *, *, #49303, .F. ) ;
#53708 = CARTESIAN_POINT ( 'NONE',  ( 8.893206853209999707, -3.977267280662000193, 9.308921106447000327 ) ) ;
#53709 = CARTESIAN_POINT ( 'NONE',  ( 9.120514158775000269, 5.306366356490000769, -7.996450761531000317 ) ) ;
#53710 = AXIS2_PLACEMENT_3D ( 'NONE', #19667, #30502, #18978 ) ;
#53711 = DIRECTION ( 'NONE',  ( 0.000000000000000000, -0.9466492601157001641, 0.3222656952305000266 ) ) ;
#53712 = CARTESIAN_POINT ( 'NONE',  ( 25.46372779695100164, -11.23407511953000082, -3.161075425950000017 ) ) ;
#53713 = CARTESIAN_POINT ( 'NONE',  ( 0.2965795288954000131, -0.5398464557615000325, -3.496157131901000081 ) ) ;
#53714 = CARTESIAN_POINT ( 'NONE',  ( 10.61257802013489737, 3.108115747127599970, 7.520762592984879369 ) ) ;
#53715 = CARTESIAN_POINT ( 'NONE',  ( 10.27367334122999942, 3.065551304793999510, -8.487910413489000661 ) ) ;
#53716 = VERTEX_POINT ( 'NONE', #30758 ) ;
#53717 = DIRECTION ( 'NONE',  ( 0.000000000000000000, 0.000000000000000000, -1.000000000000000000 ) ) ;
#53719 = AXIS2_PLACEMENT_3D ( 'NONE', #24724, #29297, #13218 ) ;
#53718 = CARTESIAN_POINT ( 'NONE',  ( 9.940795537695766626, 5.100000000000000533, 6.662590550604607031 ) ) ;
#53720 = CARTESIAN_POINT ( 'NONE',  ( 17.57925688241711626, 3.199751027636638323, -12.18694352263475444 ) ) ;
#53721 = CARTESIAN_POINT ( 'NONE',  ( 15.89999719559888369, -8.538166969133412110, -8.218914602276569781 ) ) ;
#53722 = CARTESIAN_POINT ( 'NONE',  ( 11.00000000058999916, -1.300000000000000044, -10.56294468516420082 ) ) ;
#53723 = EDGE_LOOP ( 'NONE', ( #22287, #33033, #1981, #50525 ) ) ;
#53724 = CARTESIAN_POINT ( 'NONE',  ( 7.023969222280999958, -1.381912473529000041, 0.6877288610791999490 ) ) ;
#53725 = CARTESIAN_POINT ( 'NONE',  ( 7.806654719586000546, 4.523949137149999800, -5.848703038986000635 ) ) ;
#53726 = CARTESIAN_POINT ( 'NONE',  ( 8.392827495614858080, -2.685109840479763754, 8.639376818827626536 ) ) ;
#53727 = CARTESIAN_POINT ( 'NONE',  ( 9.674709346416999978, -2.844451673749999632, 8.048718920009699573 ) ) ;
#53728 = EDGE_LOOP ( 'NONE', ( #11268, #32679, #34849, #41197, #52222 ) ) ;
#53729 = CARTESIAN_POINT ( 'NONE',  ( 16.15930817923600316, -3.787151970053999950, -11.97924296128000066 ) ) ;
#53730 = CARTESIAN_POINT ( 'NONE',  ( 11.61719580513100247, 11.50344080059000085, 1.587150035090999722 ) ) ;
#53731 = VERTEX_POINT ( 'NONE', #26548 ) ;
#53732 = CARTESIAN_POINT ( 'NONE',  ( 11.09999999999999432, 2.853660941539340357, -8.651758704407463085 ) ) ;
#53733 = CARTESIAN_POINT ( 'NONE',  ( 27.64127793187000037, 2.399999999999999911, 6.571291218949999902 ) ) ;
#53734 = CLOSED_SHELL ( 'NONE', ( #37186, #41973, #43968, #5143, #54039, #47354, #9054, #2710, #8405, #32604, #52245, #48581, #12665, #435, #61701, #2440, #26222, #16026, #31655, #42607, #7091, #22976, #60106, #9173, #32136, #1423, #26041, #9135, #14367, #52191, #59658 ) ) ;
#53735 = CARTESIAN_POINT ( 'NONE',  ( 17.74610569661007631, -0.5951713840684283996, -13.88284414672551392 ) ) ;
#53736 = ORIENTED_EDGE ( 'NONE', *, *, #62265, .T. ) ;
#53737 = CARTESIAN_POINT ( 'NONE',  ( 10.99458782869000117, -8.059061327796998242, 7.168112971386999988 ) ) ;
#53738 =( NAMED_UNIT ( * ) PLANE_ANGLE_UNIT ( ) SI_UNIT ( $, .RADIAN. ) );
#53739 = CARTESIAN_POINT ( 'NONE',  ( 10.69057802013490033, 2.966773425016000054, -7.475947032624040034 ) ) ;
#53740 = DIRECTION ( 'NONE',  ( 1.000000000000000000, 0.000000000000000000, 0.000000000000000000 ) ) ;
#53741 = ADVANCED_FACE ( 'NONE', ( #63589 ), #4858, .T. ) ;
#53742 = CARTESIAN_POINT ( 'NONE',  ( 11.55964426047339977, -3.312306505177499805, 6.422784126663999338 ) ) ;
#53743 = ORIENTED_EDGE ( 'NONE', *, *, #59217, .T. ) ;
#53744 = CARTESIAN_POINT ( 'NONE',  ( 8.090517219592001652, 5.342170561818999630, 8.432311822615000452 ) ) ;
#53745 = EDGE_CURVE ( 'NONE', #683, #18643, #63356, .T. ) ;
#53746 = VERTEX_POINT ( 'NONE', #36691 ) ;
#53747 = CARTESIAN_POINT ( 'NONE',  ( 8.554774139323296112, 5.012966070311602351, -8.578716361322166861 ) ) ;
#53748 = DIRECTION ( 'NONE',  ( 0.000000000000000000, 1.000000000000000000, 0.000000000000000000 ) ) ;
#53749 = CARTESIAN_POINT ( 'NONE',  ( 5.500000000000000000, 0.8000000000000000444, 3.149999999999999911 ) ) ;
#53750 = ORIENTED_EDGE ( 'NONE', *, *, #53401, .F. ) ;
#53751 = CARTESIAN_POINT ( 'NONE',  ( 12.23381074371948429, -2.246196888878375209, -12.50707970526073609 ) ) ;
#53752 = CARTESIAN_POINT ( 'NONE',  ( 10.64601354018249957, 4.999583552997728830, -6.731816600031361730 ) ) ;
#53753 = CARTESIAN_POINT ( 'NONE',  ( 23.60205915885299888, -9.223492163361996177, 8.025915643364996299 ) ) ;
#53754 = CARTESIAN_POINT ( 'NONE',  ( 25.60000000000000142, 0.000000000000000000, 0.000000000000000000 ) ) ;
#53755 = CARTESIAN_POINT ( 'NONE',  ( 12.21346991607045496, -2.095738610141145486, -13.84225324474580354 ) ) ;
#53756 = CARTESIAN_POINT ( 'NONE',  ( 10.30487885159599770, -3.003595720052600448, -7.381132626649399064 ) ) ;
#53757 = CARTESIAN_POINT ( 'NONE',  ( 13.69997185827400266, -11.40547114375999982, -2.374390024598000082 ) ) ;
#53758 = CARTESIAN_POINT ( 'NONE',  ( 18.26928656998121525, -2.355301763765359713, 12.37791135143290866 ) ) ;
#53759 = ORIENTED_EDGE ( 'NONE', *, *, #29507, .F. ) ;
#53760 = CARTESIAN_POINT ( 'NONE',  ( 11.51656039236534923, -2.826501801118000312, -7.557111631074219460 ) ) ;
#53761 = B_SPLINE_CURVE_WITH_KNOTS ( 'NONE', 3,
 ( #26228, #57005, #15393, #19606 ),
 .UNSPECIFIED., .F., .F.,
 ( 4, 4 ),
 ( 0.000000000000000000, 1.000000000000000000 ),
 .UNSPECIFIED. ) ;
#53762 = ORIENTED_EDGE ( 'NONE', *, *, #28203, .T. ) ;
#53763 = EDGE_CURVE ( 'NONE', #15051, #66838, #9131, .T. ) ;
#53764 = CARTESIAN_POINT ( 'NONE',  ( 25.29989948031900227, 2.596966625103000137, -11.35305524894999962 ) ) ;
#53765 = CARTESIAN_POINT ( 'NONE',  ( 4.900006121742001675, -1.229093439949829447, 1.599333684796361732 ) ) ;
#53766 = CARTESIAN_POINT ( 'NONE',  ( 9.610944094206999466, 5.100000000000000533, -6.571291218949999902 ) ) ;
#53767 = CARTESIAN_POINT ( 'NONE',  ( 18.05828166255868084, 3.296090596061254541, -11.87625419658844983 ) ) ;
#53768 = DIRECTION ( 'NONE',  ( -0.7071067783159971087, 0.7071067840570971486, -3.025403634578990376E-08 ) ) ;
#53769 = CARTESIAN_POINT ( 'NONE',  ( 8.339994183033994091, 2.871570486036998382, -6.342248726812004911 ) ) ;
#53770 = CARTESIAN_POINT ( 'NONE',  ( 9.944319408602000365, 5.443001719280999851, 7.367350382395000175 ) ) ;
#53771 = VECTOR ( 'NONE', #1744, 1000.000000000000000 ) ;
#53772 = ORIENTED_EDGE ( 'NONE', *, *, #44922, .T. ) ;
#53773 = CARTESIAN_POINT ( 'NONE',  ( 18.26087891924500184, 2.716433685251999908, 11.57325030293000090 ) ) ;
#53774 = CARTESIAN_POINT ( 'NONE',  ( 9.166073843917999397, 4.023333628930999772, 9.122276991855001071 ) ) ;
#53775 = DIRECTION ( 'NONE',  ( 1.000000000000000000, 0.000000000000000000, 0.000000000000000000 ) ) ;
#53776 = CARTESIAN_POINT ( 'NONE',  ( 10.98280513895999988, -3.096689368913399854, 8.002155910165599906 ) ) ;
#53777 = CARTESIAN_POINT ( 'NONE',  ( 18.31802873821099809, 2.927761598026000112, -11.42873208727000112 ) ) ;
#53778 = CARTESIAN_POINT ( 'NONE',  ( 11.21979841651039855, 3.695024856201900132, -8.310733465454200442 ) ) ;
#53779 = CARTESIAN_POINT ( 'NONE',  ( 11.09999999999999964, 5.538898460221000519, 7.685179721164000277 ) ) ;
#53780 = CONICAL_SURFACE ( 'NONE', #62703, 11.34994642770999818, 0.7853934433896081480 ) ;
#53781 = CARTESIAN_POINT ( 'NONE',  ( 6.778816671981999775, -0.8882170986559999593, 0.6661914818925001036 ) ) ;
#53782 = B_SPLINE_CURVE_WITH_KNOTS ( 'NONE', 3,
 ( #1789, #44106, #50031, #53284, #65405, #17524, #58521, #5384, #2138, #38854, #39194, #60177, #12283, #26723, #7029, #23105, #60516, #23458 ),
 .UNSPECIFIED., .F., .F.,
 ( 4, 2, 2, 2, 2, 2, 2, 2, 4 ),
 ( 0.000000000000000000, 0.1250000000000000000, 0.2500000000000000000, 0.3750000000000000000, 0.5000000000000000000, 0.6250000000000000000, 0.7500000000000000000, 0.8750000000000000000, 1.000000000000000000 ),
 .UNSPECIFIED. ) ;
#53783 = CARTESIAN_POINT ( 'NONE',  ( 19.89999890908300273, 0.000000000000000000, -12.52499975980204816 ) ) ;
#53784 = EDGE_CURVE ( 'NONE', #55729, #33287, #13368, .T. ) ;
#53785 = ORIENTED_EDGE ( 'NONE', *, *, #32381, .T. ) ;
#53786 = CARTESIAN_POINT ( 'NONE',  ( 3.400000000000000355, 0.000000000000000000, 0.000000000000000000 ) ) ;
#53787 = CARTESIAN_POINT ( 'NONE',  ( 7.260532792544999836, 1.067048968730999858, 0.8573300240319000620 ) ) ;
#53788 = CARTESIAN_POINT ( 'NONE',  ( 18.17997055489863811, 2.522561811188517300, 13.66861645680632797 ) ) ;
#53789 = CARTESIAN_POINT ( 'NONE',  ( 24.46275371508600216, 8.882876217567000410, -9.187943390846999847 ) ) ;
#53790 = CARTESIAN_POINT ( 'NONE',  ( 11.60533460557258323, -3.815825449682300086, -8.625775273268001087 ) ) ;
#53791 = EDGE_LOOP ( 'NONE', ( #60630, #62780, #3211, #4662, #9859 ) ) ;
#53792 = CARTESIAN_POINT ( 'NONE',  ( -2.444943969992999916E-05, -2.899969545325999931, 0.000000000000000000 ) ) ;
#53793 = CARTESIAN_POINT ( 'NONE',  ( 7.833767219591000419, 2.583668273793999770, 6.684750595573999199 ) ) ;
#53795 = CARTESIAN_POINT ( 'NONE',  ( 9.766851002543001314, -2.832432432432000269, 6.822293592207000934 ) ) ;
#53794 = CARTESIAN_POINT ( 'NONE',  ( 8.142589158771000868, 5.074768364528000397, -8.296267706722000312 ) ) ;
#53796 = CARTESIAN_POINT ( 'NONE',  ( 2.561951899676131461, -2.934981565945976367, -1.414191605408132935 ) ) ;
#53797 = ORIENTED_EDGE ( 'NONE', *, *, #25480, .T. ) ;
#53798 = CARTESIAN_POINT ( 'NONE',  ( 10.20319667131999886, 3.421760346951000287, 6.017732782098999422 ) ) ;
#53799 = CARTESIAN_POINT ( 'NONE',  ( 18.26224557552280103, -2.355566563843558558, -13.80042983216602437 ) ) ;
#53800 = CARTESIAN_POINT ( 'NONE',  ( 10.47718582084299932, 3.343463760027599818, 8.258888014436699621 ) ) ;
#53801 = CARTESIAN_POINT ( 'NONE',  ( 10.73930809942999964, -2.762991917822000154, 6.801028165221000066 ) ) ;
#53802 = CARTESIAN_POINT ( 'NONE',  ( 7.871558059623000148, -4.780993534312999671, 6.267212032957000467 ) ) ;
#53803 = EDGE_LOOP ( 'NONE', ( #19100, #29871, #20552, #38555 ) ) ;
#53804 = CARTESIAN_POINT ( 'NONE',  ( 8.455992358796999397, 5.100000000000000533, 6.571291218954000257 ) ) ;
#53806 = CARTESIAN_POINT ( 'NONE',  ( 10.24394435321000074, -3.220344030624999743, -6.005416930865999703 ) ) ;
#53805 = CARTESIAN_POINT ( 'NONE',  ( 12.46445792838400024, -11.52135921566999954, 4.763665720747999544 ) ) ;
#53807 = CARTESIAN_POINT ( 'NONE',  ( 7.892384426797941721, -2.680859579914350199, 8.636688153635477150 ) ) ;
#53808 = CARTESIAN_POINT ( 'NONE',  ( 7.000000000000000000, 7.526486366024999874, -3.526486366024999874 ) ) ;
#53809 = CARTESIAN_POINT ( 'NONE',  ( 24.51040166152899857, 3.518808723585000298, 12.24493758046000025 ) ) ;
#53810 = EDGE_LOOP ( 'NONE', ( #19194, #36806, #62831, #13243 ) ) ;
#53812 = CARTESIAN_POINT ( 'NONE',  ( 24.32158544041289261, 12.72716532455095972, 3.095239629920860214 ) ) ;
#53811 = AXIS2_PLACEMENT_3D ( 'NONE', #55722, #12725, #39638 ) ;
#53813 = B_SPLINE_CURVE_WITH_KNOTS ( 'NONE', 3,
 ( #37043, #68151, #31122, #9423, #4180, #24832, #63597, #52774, #31456, #36702, #19588, #67808, #3832, #4869, #46159, #62231, #62905, #9089, #35672, #47191, #56986 ),
 .UNSPECIFIED., .F., .F.,
 ( 4, 2, 2, 1, 1, 2, 2, 2, 1, 2, 2, 4 ),
 ( 0.000000000000000000, 0.1250000000000654754, 0.1875000000000969225, 0.2187500000001172396, 0.2343750000001220968, 0.2421875000001264266, 0.2500000000001307288, 0.3750000000001184608, 0.4375000000001083578, 0.4687500000001048051, 0.5000000000001012523, 1.000000000000000000 ),
 .UNSPECIFIED. ) ;
#53814 = CARTESIAN_POINT ( 'NONE',  ( 10.75564828895399927, -3.119330945648699949, 7.018986873610899124 ) ) ;
#53815 = CARTESIAN_POINT ( 'NONE',  ( 10.46887750876899936, 3.307728619566300043, 6.425720373262999274 ) ) ;
#53816 = ORIENTED_EDGE ( 'NONE', *, *, #32163, .T. ) ;
#53817 = CARTESIAN_POINT ( 'NONE',  ( 9.568039158772000619, 5.336630274082000192, -7.092011739486999922 ) ) ;
#53818 = CARTESIAN_POINT ( 'NONE',  ( 24.34833249973733516, 12.15210535428998284, 3.256146816021051382 ) ) ;
#53819 = ADVANCED_FACE ( 'NONE', ( #10797 ), #32282, .F. ) ;
#53820 = CARTESIAN_POINT ( 'NONE',  ( 11.22702344389999851, -5.004394439171999664, 8.109550315577399360 ) ) ;
#53821 = ADVANCED_FACE ( 'NONE', ( #19143 ), #21651, .F. ) ;
#53822 = EDGE_LOOP ( 'NONE', ( #9783, #62184, #17073, #61233 ) ) ;
#53823 = CARTESIAN_POINT ( 'NONE',  ( 7.947810405765513231, 4.792115117880548780, -6.324572600310053971 ) ) ;
#53824 = DIRECTION ( 'NONE',  ( 1.000000000000000000, 0.000000000000000000, 0.000000000000000000 ) ) ;
#53825 = ORIENTED_EDGE ( 'NONE', *, *, #50358, .T. ) ;
#53826 = CARTESIAN_POINT ( 'NONE',  ( 8.111566940377999302, -3.326257819185999942, 8.794522506294001118 ) ) ;
#53827 = DIRECTION ( 'NONE',  ( 0.000000000000000000, 0.8684118855788046654, -0.4958435206650028126 ) ) ;
#53828 = ORIENTED_EDGE ( 'NONE', *, *, #2992, .F. ) ;
#53829 = CARTESIAN_POINT ( 'NONE',  ( 12.56995090575623308, -3.160862399908569209, -12.19708787818173867 ) ) ;
#53830 = CARTESIAN_POINT ( 'NONE',  ( 11.68333460557258796, 4.162011815820000571, 6.509695444280099608 ) ) ;
#53831 = AXIS2_PLACEMENT_3D ( 'NONE', #60060, #16705, #38033 ) ;
#53832 = CARTESIAN_POINT ( 'NONE',  ( 10.56491664109999995, 4.212242527248999835, 8.933458498617000032 ) ) ;
#53833 = CARTESIAN_POINT ( 'NONE',  ( 10.05205635875000070, 2.669891600604999748, -8.791543746052999708 ) ) ;
#53834 = CARTESIAN_POINT ( 'NONE',  ( 8.060004013849999538, 5.097451875645002239, 6.450907456765003545 ) ) ;
#53835 = CARTESIAN_POINT ( 'NONE',  ( 9.465112865370999273, -2.290047720994000002, 6.601709978349000529 ) ) ;
#53836 = CARTESIAN_POINT ( 'NONE',  ( 13.99944283128300171, 9.262889243704000464, 8.209791536961999370 ) ) ;
#53837 = CARTESIAN_POINT ( 'NONE',  ( 17.69686089611048985, 0.6090396975623089126, -12.68033511803396252 ) ) ;
#53838 = SURFACE_SIDE_STYLE ('',( #1054 ) ) ;
#53839 = CARTESIAN_POINT ( 'NONE',  ( 10.20641772631199906, -3.568446272909699957, -8.388315195900499788 ) ) ;
#53840 = CARTESIAN_POINT ( 'NONE',  ( 9.459510841229999301, 5.445214367171999470, 7.703373622193999459 ) ) ;
#53841 = VERTEX_POINT ( 'NONE', #19836 ) ;
#53842 = ADVANCED_FACE ( 'NONE', ( #63503 ), #41844, .T. ) ;
#53843 = B_SPLINE_CURVE_WITH_KNOTS ( 'NONE', 3,
 ( #35699, #4547, #46531, #67838, #19959, #68178, #31151, #62930, #57691, #9802, #68520, #20642, #15405, #48238, #53489, #11512, #22355, #49270 ),
 .UNSPECIFIED., .F., .F.,
 ( 4, 2, 2, 2, 2, 2, 2, 2, 4 ),
 ( 0.000000000000000000, 0.1250000000000000000, 0.2500000000000000000, 0.3750000000000000000, 0.5000000000000000000, 0.6250000000000000000, 0.7500000000000000000, 0.8750000000000000000, 1.000000000000000000 ),
 .UNSPECIFIED. ) ;
#53844 = CARTESIAN_POINT ( 'NONE',  ( 7.100000000000000533, 5.221516520829000640, -8.074802043613001246 ) ) ;
#53845 = CARTESIAN_POINT ( 'NONE',  ( 9.241226895148511034, 2.676623112219036482, 7.234156217801734456 ) ) ;
#53846 = DIRECTION ( 'NONE',  ( -0.7071134747947538379, 0.000000000000000000, -0.7071000875149777709 ) ) ;
#53847 = EDGE_CURVE ( 'NONE', #8734, #10646, #59151, .T. ) ;
#53848 = CARTESIAN_POINT ( 'NONE',  ( 18.00922683609308095, 1.919385048924809656, 12.45295227646844616 ) ) ;
#53849 = CARTESIAN_POINT ( 'NONE',  ( 12.53635786351535053, 1.839692799137174095, 13.87860051966028152 ) ) ;
#53850 = CARTESIAN_POINT ( 'NONE',  ( 10.86291173059000137, 9.763630752138000801, 5.703239193002999308 ) ) ;
#53851 = FACE_OUTER_BOUND ( 'NONE', #16856, .T. ) ;
#53852 = CARTESIAN_POINT ( 'NONE',  ( 12.80505043854146940, -1.787816316115923287, 13.88537766212463076 ) ) ;
#53853 = VERTEX_POINT ( 'NONE', #57573 ) ;
#53854 = CARTESIAN_POINT ( 'NONE',  ( 12.51946955736931422, -3.141640009352832941, 12.20205326030422199 ) ) ;
#53855 = CARTESIAN_POINT ( 'NONE',  ( 9.958963142879998287, -3.017187828228399926, -7.292822454528599785 ) ) ;
#53856 = CARTESIAN_POINT ( 'NONE',  ( 9.299999999999998934, -4.537600397704999899, 9.154563893594000135 ) ) ;
#53857 = CARTESIAN_POINT ( 'NONE',  ( 10.37874387220000116, -4.882732524430000609, 6.350796477317000921 ) ) ;
#53858 = CONICAL_SURFACE ( 'NONE', #4741, 1.200857723089999940, 0.7853979760808852406 ) ;
#53859 = CARTESIAN_POINT ( 'NONE',  ( 11.23610538575739959, 5.109472165990999848, -7.234742334405199315 ) ) ;
#53860 = CARTESIAN_POINT ( 'NONE',  ( 12.13986395842897537, 0.2863297863804566412, 12.59675086341328409 ) ) ;
#53861 = CARTESIAN_POINT ( 'NONE',  ( 8.855420280411999912, 5.633477595780999714, 7.451234169193000412 ) ) ;
#53862 = CARTESIAN_POINT ( 'NONE',  ( 24.30000000000000071, -10.83443035398000021, -3.855530949778000149 ) ) ;
#53863 = CARTESIAN_POINT ( 'NONE',  ( 12.76350962112086407, 3.123958135104669243, 12.28404825260450117 ) ) ;
#53864 = CARTESIAN_POINT ( 'NONE',  ( 18.49997192701553317, -2.999031289802028155, -12.16100995559911446 ) ) ;
#53865 = CARTESIAN_POINT ( 'NONE',  ( 11.08841369783139896, 3.942447888101379583, -8.639288317626999003 ) ) ;
#53866 = CARTESIAN_POINT ( 'NONE',  ( 8.061825939490002924, 3.419144686567003877, -6.221559872366999144 ) ) ;
#53867 = CARTESIAN_POINT ( 'NONE',  ( 10.65229834123000074, 4.944334466443999432, -8.478467788338001299 ) ) ;
#53868 = CARTESIAN_POINT ( 'NONE',  ( 8.642797255587998606, 5.278067516796999925, -7.445890648716809501 ) ) ;
#53870 = CARTESIAN_POINT ( 'NONE',  ( 12.30934879320328079, 2.881204795976714639, 12.35454860660065890 ) ) ;
#53869 = CARTESIAN_POINT ( 'NONE',  ( 8.187982051047001164, 4.942702676859997979, 6.196150354213001421 ) ) ;
#53871 = DIRECTION ( 'NONE',  ( -1.000000000000000000, 0.000000000000000000, 0.000000000000000000 ) ) ;
#53872 = ORIENTED_EDGE ( 'NONE', *, *, #7883, .F. ) ;
#53873 = AXIS2_PLACEMENT_3D ( 'NONE', #58652, #10753, #59000 ) ;
#53874 = CARTESIAN_POINT ( 'NONE',  ( 12.31001894270039720, 0.3816018581758214845, 12.69228475098156395 ) ) ;
#53875 = CARTESIAN_POINT ( 'NONE',  ( 1.500973465873999935, 3.500000000000000000, 0.000000000000000000 ) ) ;
#53876 = CARTESIAN_POINT ( 'NONE',  ( 18.00096484323668022, 0.5748214922193798371, -12.58705572532864991 ) ) ;
#53877 = CARTESIAN_POINT ( 'NONE',  ( 8.893126402770997530, 4.811247217215600003, 7.805918119494599239 ) ) ;
#53878 = CARTESIAN_POINT ( 'NONE',  ( 12.08107629042319253, -2.473358331846541525, 13.77980712931821827 ) ) ;
#53879 = CARTESIAN_POINT ( 'NONE',  ( 10.86079987841999994, 2.936792838704000097, 5.172914090879999982 ) ) ;
#53880 = PLANE ( 'NONE',  #57839 ) ;
#53881 = EDGE_LOOP ( 'NONE', ( #52529, #2176, #17094, #65153 ) ) ;
#53882 = B_SPLINE_CURVE_WITH_KNOTS ( 'NONE', 3,
 ( #56669, #10735, #21229, #51416 ),
 .UNSPECIFIED., .F., .F.,
 ( 4, 4 ),
 ( 0.000000000000000000, 1.000000000000000000 ),
 .UNSPECIFIED. ) ;
#53883 = CARTESIAN_POINT ( 'NONE',  ( 10.10000000000000142, 0.000000000000000000, 0.000000000000000000 ) ) ;
#53884 = CARTESIAN_POINT ( 'NONE',  ( 9.828775684073081109, 2.650411012611820105, -7.263174729041424804 ) ) ;
#53885 = CARTESIAN_POINT ( 'NONE',  ( 9.648264191885376206, -4.679965170704055488, -8.679680463610704777 ) ) ;
#53886 = CARTESIAN_POINT ( 'NONE',  ( 18.43276988671243544, -2.975106096554608559, 11.26378872113905238 ) ) ;
#53887 = CARTESIAN_POINT ( 'NONE',  ( 7.307500000000000107, -0.2999999999999999889, 3.149999999999999911 ) ) ;
#53888 = CARTESIAN_POINT ( 'NONE',  ( 9.701637546194749717, -3.727464796005204750, 8.730330573913894554 ) ) ;
#53889 = CARTESIAN_POINT ( 'NONE',  ( 11.34287482311539996, 4.803125295093300551, 7.175518335304800210 ) ) ;
#53890 = CARTESIAN_POINT ( 'NONE',  ( 21.60000000000000142, -12.52500000000000036, 0.000000000000000000 ) ) ;
#53891 = CARTESIAN_POINT ( 'NONE',  ( 10.96333185321000059, -5.283547384770999500, -8.592770849731000027 ) ) ;
#53892 = CARTESIAN_POINT ( 'NONE',  ( 9.099999952505998024, -4.000000000000000000, 7.500000000000000000 ) ) ;
#53893 = B_SPLINE_SURFACE_WITH_KNOTS ( 'NONE', 3, 3, ( 
 ( #21939, #43277, #54106, #27543, #54453, #65966, #64585, #1662, #54798, #38022, #49549, #49207, #44327, #50248, #60733, #22979, #43630, #28234, #33137, #64924, #23332, #55494, #6554, #65625, #22290, #11451, #7594, #7248, #22630, #17750, #43975, #48869, #18092, #39070, #60392 ),
 ( #12496, #1314, #33831, #28589, #38372, #59696, #49901, #39413, #28943, #16694, #17040, #32790, #6201, #977, #11798, #38723, #27897, #60045, #34862, #19460, #13543, #24019, #39764, #19114, #35211, #51614, #40781, #57199, #62446, #9302, #3710, #23672, #41135, #62105, #61762 ),
 ( #46033, #30643, #14224, #25047, #40113, #50936, #67339, #45010, #66314, #51278, #14567, #24710, #35551, #56869, #2350, #35884, #18438, #8967, #61082, #13202, #30306, #56178, #34530, #55839, #46379, #7943, #67681, #19807, #18782, #61427, #3373, #29279, #50594, #2695, #45354 ),
 ( #66663, #8289, #29633, #3034, #24365, #45696, #67005, #40435, #29976, #13880, #56522, #8627, #52999, #57896, #68370, #10341, #5095, #64161, #5445, #4740, #15929, #20490, #25738, #41815, #26431, #58931, #63816, #32031, #63122, #31334, #47761, #25388, #46726, #31677, #21516 ) ),
 .UNSPECIFIED., .F., .F., .F.,
 ( 4, 4 ),
 ( 4, 1, 1, 1, 1, 1, 1, 1, 1, 1, 1, 1, 1, 1, 1, 1, 1, 1, 1, 1, 1, 1, 1, 1, 1, 1, 1, 1, 1, 1, 1, 1, 4 ),
 ( -0.1039370721279000015, 1.103937072127999963 ),
 ( -0.02000000000000000042, 0.01250000000000000069, 0.04499999999999999833, 0.07749999999999999944, 0.1100000000000000006, 0.1424999999999999878, 0.1749999999999999889, 0.2074999999999999900, 0.2399999999999999911, 0.2725000000000000200, 0.3049999999999999933, 0.3375000000000000222, 0.3699999999999999956, 0.4025000000000000244, 0.4349999999999999978, 0.4675000000000000266, 0.5000000000000000000, 0.5324999999999999734, 0.5649999999999999467, 0.5975000000000000311, 0.6300000000000000044, 0.6624999999999999778, 0.6949999999999999512, 0.7275000000000000355, 0.7600000000000000089, 0.7924999999999999822, 0.8249999999999999556, 0.8575000000000000400, 0.8900000000000000133, 0.9224999999999999867, 0.9549999999999999600, 0.9875000000000000444, 1.020000000000000018 ),
 .UNSPECIFIED. ) ;
#53894 = CARTESIAN_POINT ( 'NONE',  ( 11.09999999999999964, 6.593648130222000248, -5.598803514566000672 ) ) ;
#53895 = CARTESIAN_POINT ( 'NONE',  ( 24.16198684513495110, 9.122969203443838992, -9.103568285634533908 ) ) ;
#53896 = ADVANCED_FACE ( 'NONE', ( #47793 ), #447, .F. ) ;
#53897 = CARTESIAN_POINT ( 'NONE',  ( 9.416236906464300560, 5.342733096692782624, 7.360698289850908793 ) ) ;
#53898 = EDGE_CURVE ( 'NONE', #19784, #47809, #21545, .T. ) ;
#53899 = ORIENTED_EDGE ( 'NONE', *, *, #65670, .F. ) ;
#53900 = CARTESIAN_POINT ( 'NONE',  ( 11.09999999999999964, -5.299999998610999796, 5.148506132424000015 ) ) ;
#53901 = CARTESIAN_POINT ( 'NONE',  ( 12.08071932425156980, -4.167269912168199753, 6.371589232479998977 ) ) ;
#53902 = EDGE_LOOP ( 'NONE', ( #23111, #43871, #24613, #35710 ) ) ;
#53903 = CONICAL_SURFACE ( 'NONE', #63928, 0.8999999993723004632, 0.7853981633972997312 ) ;
#53904 = CARTESIAN_POINT ( 'NONE',  ( 18.05294241905986041, -2.122066809870763571, 13.74638883949612023 ) ) ;
#53905 = CARTESIAN_POINT ( 'NONE',  ( 10.91610672858429965, -4.911600290708499905, -6.814233985789400094 ) ) ;
#53906 = ORIENTED_EDGE ( 'NONE', *, *, #31493, .F. ) ;
#53907 = CARTESIAN_POINT ( 'NONE',  ( 10.56591429142999949, 4.019686495353769651, 8.533318907609000803 ) ) ;
#53908 = CARTESIAN_POINT ( 'NONE',  ( 5.679855442506180907, 0.3526799806875357546, 1.076168297469421553 ) ) ;
#53909 = FACE_OUTER_BOUND ( 'NONE', #50394, .T. ) ;
#53910 = AXIS2_PLACEMENT_3D ( 'NONE', #66506, #54646, #39957 ) ;
#53911 = CARTESIAN_POINT ( 'NONE',  ( 18.53574650668400281, -2.786976374009999535, 11.27236326136999978 ) ) ;
#53912 = CYLINDRICAL_SURFACE ( 'NONE', #67861, 1.350000000000000533 ) ;
#53913 = CARTESIAN_POINT ( 'NONE',  ( 12.32101708576682064, 0.3953980351523287418, -13.89243073565737241 ) ) ;
#53914 = CARTESIAN_POINT ( 'NONE',  ( 6.786452000648069749, -0.9523218012055599813, 0.5806051447938145316 ) ) ;
#53915 = DIRECTION ( 'NONE',  ( 0.000000000000000000, 1.099932324123999872E-09, -1.000000000000000000 ) ) ;
#53916 = CARTESIAN_POINT ( 'NONE',  ( 0.1499996298882999846, 2.250000000000000000, 0.000000000000000000 ) ) ;
#53917 = EDGE_LOOP ( 'NONE', ( #39480, #58660, #33122, #28229 ) ) ;
#53918 = CARTESIAN_POINT ( 'NONE',  ( 9.716735841232001292, 3.941185585667000169, -8.896279800194999865 ) ) ;
#53919 = VERTEX_POINT ( 'NONE', #64187 ) ;
#53920 = CARTESIAN_POINT ( 'NONE',  ( 24.62620337148488048, -12.35920179360042681, 2.996409964397301451 ) ) ;
#53921 = VERTEX_POINT ( 'NONE', #27490 ) ;
#53922 = DIRECTION ( 'NONE',  ( -1.000000000000000000, 0.000000000000000000, 0.000000000000000000 ) ) ;
#53923 = CARTESIAN_POINT ( 'NONE',  ( 18.12468263438044147, -2.757387671472311119, -12.38786642819431982 ) ) ;
#53924 = EDGE_CURVE ( 'NONE', #60029, #31626, #52470, .T. ) ;
#53925 = CARTESIAN_POINT ( 'NONE',  ( 24.92847981667748769, -8.562973297442058040, 8.403437224533664818 ) ) ;
#53926 = CARTESIAN_POINT ( 'NONE',  ( 18.30000077768849565, 11.66744147158535405, -3.971919865264926575 ) ) ;
#53927 = CARTESIAN_POINT ( 'NONE',  ( 9.681180837610000367, -2.612237299844000216, 7.804680206899999639 ) ) ;
#53928 = CARTESIAN_POINT ( 'NONE',  ( 17.55505043854147118, -1.875000000000000000, -12.57541666120755863 ) ) ;
#53929 = CARTESIAN_POINT ( 'NONE',  ( 12.24422661137779400, -0.2766185922798731212, 13.89631150889696798 ) ) ;
#53930 = VERTEX_POINT ( 'NONE', #22236 ) ;
#53931 = CARTESIAN_POINT ( 'NONE',  ( 7.196271682457999752, 4.719833207100999850, -8.789699670502999496 ) ) ;
#53932 = CARTESIAN_POINT ( 'NONE',  ( 17.93529619513299878, 12.15408297959000095, -3.184072412108000183 ) ) ;
#53933 = CARTESIAN_POINT ( 'NONE',  ( 4.600001223043999943, 0.000000000000000000, 0.000000000000000000 ) ) ;
#53934 = CARTESIAN_POINT ( 'NONE',  ( 4.930797932093000213, 1.481278897913000048, 0.05118800434419999712 ) ) ;
#53935 = MANIFOLD_SOLID_BREP ( 'Stock-MAS-678-1', #9066 ) ;
#53936 = CARTESIAN_POINT ( 'NONE',  ( 9.152446624286001864, 2.899999999999999911, -6.169193161299999950 ) ) ;
#53937 = CARTESIAN_POINT ( 'NONE',  ( 18.35499787466299892, -2.879071536379000040, 12.03968120189999880 ) ) ;
#53938 = CARTESIAN_POINT ( 'NONE',  ( 9.961463664312999455, -2.787129471086000176, -8.677705025472000955 ) ) ;
#53939 = ORIENTED_EDGE ( 'NONE', *, *, #19735, .F. ) ;
#53940 = PLANE ( 'NONE',  #5807 ) ;
#53941 = DIRECTION ( 'NONE',  ( -0.000000000000000000, -0.000000000000000000, 1.000000000000000000 ) ) ;
#53942 = DIRECTION ( 'NONE',  ( -1.000000000000000000, 0.000000000000000000, 0.000000000000000000 ) ) ;
#53943 = CARTESIAN_POINT ( 'NONE',  ( 8.611367277397988573, -2.905107992438832110, 6.370216274085540142 ) ) ;
#53944 = LINE ( 'NONE', #42773, #5375 ) ;
#53945 = AXIS2_PLACEMENT_3D ( 'NONE', #41456, #10322, #19440 ) ;
#53946 = CARTESIAN_POINT ( 'NONE',  ( 10.39969598649000027, 4.888000489779200208, -8.028730309000598808 ) ) ;
#53947 = CARTESIAN_POINT ( 'NONE',  ( 9.077417874593999514, 3.075647715286899953, -7.892956936667999912 ) ) ;
#53949 = CARTESIAN_POINT ( 'NONE',  ( 8.440751497925912616, 5.098238174920831867, -6.529850537739550376 ) ) ;
#53948 = CARTESIAN_POINT ( 'NONE',  ( 9.597772138681998300, -4.373757805842100055, 8.432280753260499750 ) ) ;
#53950 = CARTESIAN_POINT ( 'NONE',  ( 6.899999691988000450, 12.20988339176000004, -3.111064831549000154 ) ) ;
#53951 = ORIENTED_EDGE ( 'NONE', *, *, #42442, .F. ) ;
#53952 = CARTESIAN_POINT ( 'NONE',  ( 10.88813259637009878, 2.844182332072999753, 6.870201387206400057 ) ) ;
#53953 = CARTESIAN_POINT ( 'NONE',  ( 9.305875415870998424, -4.945293979885000191, 9.077881967919999795 ) ) ;
#53954 = EDGE_CURVE ( 'NONE', #15615, #49620, #64953, .T. ) ;
#53955 = EDGE_CURVE ( 'NONE', #42349, #57892, #61710, .T. ) ;
#53956 = CARTESIAN_POINT ( 'NONE',  ( 9.253772138682000659, 3.523984281974800403, 8.687347221188998603 ) ) ;
#53957 = CARTESIAN_POINT ( 'NONE',  ( 17.60000001994400165, -11.53041320601000130, 4.891397783926000109 ) ) ;
#53958 = CARTESIAN_POINT ( 'NONE',  ( 10.34020413671000149, -4.202027362542999356, 9.459588031742001135 ) ) ;
#53959 = CARTESIAN_POINT ( 'NONE',  ( 9.905947954862410754, -2.481286724714716563, 8.418981899270745473 ) ) ;
#53960 = CARTESIAN_POINT ( 'NONE',  ( 16.32975648157900039, -3.316681689484000106, -11.22330675696999869 ) ) ;
#53961 = CONICAL_SURFACE ( 'NONE', #55129, 11.75016914289000169, 0.7854125553233202162 ) ;
#53962 = CARTESIAN_POINT ( 'NONE',  ( 8.925442991499998868, -4.063228561016970275, -6.497580701799000380 ) ) ;
#53963 = CARTESIAN_POINT ( 'NONE',  ( 6.557034520496999974, -0.07351275584480999881, 1.466703212027999914 ) ) ;
#53964 = CARTESIAN_POINT ( 'NONE',  ( 11.49375810342577608, -3.998140074039970848, 8.374120210831636157 ) ) ;
#53965 = AXIS2_PLACEMENT_3D ( 'NONE', #60988, #19631, #49809 ) ;
#53966 = CARTESIAN_POINT ( 'NONE',  ( 24.36453968238300050, -3.372832729159999765, 12.24475767785000002 ) ) ;
#53967 = ORIENTED_EDGE ( 'NONE', *, *, #53256, .T. ) ;
#53968 = CARTESIAN_POINT ( 'NONE',  ( 12.78441639972301758, 0.6247443594537122058, -12.67930618256806419 ) ) ;
#53969 = CARTESIAN_POINT ( 'NONE',  ( 11.31825954179440075, 4.666231193203100425, -8.053565341712399572 ) ) ;
#53970 = CARTESIAN_POINT ( 'NONE',  ( 9.424850088744616272, -5.349972419855331118, 7.500009359253513530 ) ) ;
#53971 = CARTESIAN_POINT ( 'NONE',  ( 24.59181004102800117, -8.769933227510000151, 9.082960305682000524 ) ) ;
#53972 = CARTESIAN_POINT ( 'NONE',  ( 12.07911454975265642, 2.296549521726467091, 12.39040777275211624 ) ) ;
#53973 = ORIENTED_EDGE ( 'NONE', *, *, #18087, .F. ) ;
#53974 = CARTESIAN_POINT ( 'NONE',  ( 24.63407836964800168, -11.78083276143999925, -3.229000863272000199 ) ) ;
#53975 = PRODUCT_CONTEXT ( 'NONE', #26660, 'mechanical' ) ;
#53977 = CARTESIAN_POINT ( 'NONE',  ( 11.06456920625009843, -3.962850971080120299, -6.467161360063999886 ) ) ;
#53976 = SHAPE_REPRESENTATION ( 'Terminal Screw 1', ( #9676 ), #756 ) ;
#53978 = EDGE_CURVE ( 'NONE', #5660, #27749, #33780, .T. ) ;
#53979 = CARTESIAN_POINT ( 'NONE',  ( 18.05193840056092114, 0.3791517837227010856, 12.69238281682775416 ) ) ;
#53980 = CARTESIAN_POINT ( 'NONE',  ( 23.50387503050299998, 3.715991115242999921E-06, -13.79999999999999893 ) ) ;
#53981 = CARTESIAN_POINT ( 'NONE',  ( 7.000000000000000000, 10.57888183308256735, 3.948561346722022414 ) ) ;
#53982 = CARTESIAN_POINT ( 'NONE',  ( 12.95870478550200211, 12.43384127863000010, 1.801469962976000039 ) ) ;
#53983 = EDGE_LOOP ( 'NONE', ( #60195, #33313, #33216, #19613, #16858 ) ) ;
#53984 = B_SPLINE_CURVE_WITH_KNOTS ( 'NONE', 3,
 ( #48384, #16220, #63418, #9593, #37542, #5389, #15193, #57841, #58525, #26727 ),
 .UNSPECIFIED., .F., .F.,
 ( 4, 2, 2, 2, 4 ),
 ( 0.000000000000000000, 0.1249999999999998335, 0.2499999999999996669, 0.3749999999999995559, 0.4999999999999994449 ),
 .UNSPECIFIED. ) ;
#53985 = ADVANCED_FACE ( 'NONE', ( #7202 ), #9895, .T. ) ;
#53986 = CARTESIAN_POINT ( 'NONE',  ( 10.96876739532000045, -2.333349849211999949, 6.524062020538999640 ) ) ;
#53987 = CARTESIAN_POINT ( 'NONE',  ( 17.93750432894411517, 2.994741171281513736, -13.55599983589036484 ) ) ;
#53988 = VERTEX_POINT ( 'NONE', #49850 ) ;
#53989 = CARTESIAN_POINT ( 'NONE',  ( 16.00000000429200142, 11.53036813819577411, -4.891445144093894193 ) ) ;
#53990 = CARTESIAN_POINT ( 'NONE',  ( 25.21376180238323528, 8.515659051923003986, -8.063054907511679303 ) ) ;
#53991 = CARTESIAN_POINT ( 'NONE',  ( 15.39325612864500137, 8.820489328074000213, 7.691617095226000345 ) ) ;
#53992 = ORIENTED_EDGE ( 'NONE', *, *, #52334, .T. ) ;
#53993 = CARTESIAN_POINT ( 'NONE',  ( 23.67741840186891622, -13.18815814536682751, 3.924039949733880928 ) ) ;
#53994 = CARTESIAN_POINT ( 'NONE',  ( 8.210360841226998829, 3.344658122371999998, -5.716722540613000447 ) ) ;
#53995 = CARTESIAN_POINT ( 'NONE',  ( 7.400000000000000355, 0.000000000000000000, 0.5999999999999999778 ) ) ;
#53996 = CARTESIAN_POINT ( 'NONE',  ( 7.936333771302000351, 5.123034328734999754, 6.721303713258000023 ) ) ;
#53997 = ORIENTED_EDGE ( 'NONE', *, *, #13972, .T. ) ;
#53998 = CARTESIAN_POINT ( 'NONE',  ( 9.972852379787999766, -5.044471434015000533, 6.258101649750000384 ) ) ;
#53999 = CARTESIAN_POINT ( 'NONE',  ( 11.60000000000000142, 3.745359844992759868, 8.477868186285956398 ) ) ;
#54000 = ORIENTED_EDGE ( 'NONE', *, *, #34269, .F. ) ;
#54001 = VECTOR ( 'NONE', #13206, 1000.000000000000000 ) ;
#54002 = DIRECTION ( 'NONE',  ( -1.000000000000000000, 0.000000000000000000, 0.000000000000000000 ) ) ;
#54003 = CARTESIAN_POINT ( 'NONE',  ( 10.42511694037999881, -3.371058793856000158, -6.294333763729999198 ) ) ;
#54004 = ORIENTED_EDGE ( 'NONE', *, *, #33105, .F. ) ;
#54005 = CARTESIAN_POINT ( 'NONE',  ( 9.432025935145999185, 3.854158361175799907, 8.493766832166899761 ) ) ;
#54006 = CARTESIAN_POINT ( 'NONE',  ( 24.30001683613300045, -12.21047198529999989, -3.271805531187999883 ) ) ;
#54007 = CARTESIAN_POINT ( 'NONE',  ( 4.305925572186999339, 0.8223230991370998888, 1.100157502810999999 ) ) ;
#54008 = EDGE_CURVE ( 'NONE', #21149, #7230, #39712, .T. ) ;
#54009 = CARTESIAN_POINT ( 'NONE',  ( 11.59999999999999787, 3.745359844992758092, -6.522131813714044490 ) ) ;
#54010 = CARTESIAN_POINT ( 'NONE',  ( 24.69607688207488749, 11.79509585809828742, -3.190917141363150744 ) ) ;
#54011 = CARTESIAN_POINT ( 'NONE',  ( 9.379129085676606081, 2.650412078218661538, -7.263196332420141843 ) ) ;
#54012 = CARTESIAN_POINT ( 'NONE',  ( 8.741072744221000335, 3.937347817007940343, -8.366433385397499478 ) ) ;
#54013 = ORIENTED_EDGE ( 'NONE', *, *, #25089, .T. ) ;
#54014 = CARTESIAN_POINT ( 'NONE',  ( 9.351497027444999333, 4.821940693094999730, 8.950154065657999425 ) ) ;
#54015 = CARTESIAN_POINT ( 'NONE',  ( 4.417085542195750669, 1.094284481885183125, 1.075295689758499318 ) ) ;
#54016 = CIRCLE ( 'NONE', #24980, 1.000000000000000666 ) ;
#54017 = CARTESIAN_POINT ( 'NONE',  ( 24.30000000000000071, 9.305479840184000651, 8.315530346521999405 ) ) ;
#54018 = CARTESIAN_POINT ( 'NONE',  ( 12.70875935989986338, 1.793877008111237403, -13.88459618876652968 ) ) ;
#54019 = CARTESIAN_POINT ( 'NONE',  ( 3.648430005244999830, 0.04330141671533999093, 3.707787403725999908 ) ) ;
#54020 = CARTESIAN_POINT ( 'NONE',  ( 10.27814441345999974, -5.521593622715999850, 8.751220666652999469 ) ) ;
#54021 = CARTESIAN_POINT ( 'NONE',  ( 18.12461517476719308, -0.2575405707509137443, 13.89679341043304994 ) ) ;
#54022 = AXIS2_PLACEMENT_3D ( 'NONE', #18617, #24547, #28772 ) ;
#54023 = CARTESIAN_POINT ( 'NONE',  ( 7.717918984469999799, -2.852331559125000027, 6.784354950350999225 ) ) ;
#54024 = VERTEX_POINT ( 'NONE', #17701 ) ;
#54025 = ORIENTED_EDGE ( 'NONE', *, *, #51624, .F. ) ;
#54026 = CARTESIAN_POINT ( 'NONE',  ( 12.20957190031489503, -0.1900921648596720082, 13.89825464817906564 ) ) ;
#54027 = VECTOR ( 'NONE', #47375, 1000.000000000000114 ) ;
#54028 = CARTESIAN_POINT ( 'NONE',  ( 12.53086501631639393, -0.5620205155227050442, -13.88470856849332513 ) ) ;
#54029 = CARTESIAN_POINT ( 'NONE',  ( 10.47094409420000005, 5.100000000000000533, 6.571291218949999902 ) ) ;
#54030 = CARTESIAN_POINT ( 'NONE',  ( 17.96218347282713879, -0.4743995195315680591, -13.88910611340119772 ) ) ;
#54031 = CARTESIAN_POINT ( 'NONE',  ( 7.282480646792000023, -3.448181789123000218, 9.222458996124998976 ) ) ;
#54032 = FACE_OUTER_BOUND ( 'NONE', #54082, .T. ) ;
#54034 = CYLINDRICAL_SURFACE ( 'NONE', #18339, 0.6999999999999992895 ) ;
#54033 = CARTESIAN_POINT ( 'NONE',  ( 10.51364655415099847, -3.380689388027600106, 6.380697202105999999 ) ) ;
#54035 = CARTESIAN_POINT ( 'NONE',  ( 10.71503032197929883, 4.743378537856500543, -6.460430507351999196 ) ) ;
#54036 = DIRECTION ( 'NONE',  ( 1.000000000000000000, 0.000000000000000000, 0.000000000000000000 ) ) ;
#54037 = CARTESIAN_POINT ( 'NONE',  ( 8.994442991499997930, 3.945420918055940085, -6.634708680083400090 ) ) ;
#54038 = EDGE_CURVE ( 'NONE', #13996, #18320, #18840, .T. ) ;
#54039 = ADVANCED_FACE ( 'NONE', ( #1960 ), #26677, .T. ) ;
#54040 = CARTESIAN_POINT ( 'NONE',  ( 18.15913468976203404, 0.1616215023347959134, 12.69863621249087871 ) ) ;
#54041 = B_SPLINE_SURFACE_WITH_KNOTS ( 'NONE', 3, 3, ( 
 ( #48201, #38049, #64265, #306 ),
 ( #59374, #11823, #42283, #21622 ),
 ( #37710, #33162, #16036, #27568 ),
 ( #37031, #11474, #63925, #59038 ),
 ( #10446, #31786, #53789, #5204 ),
 ( #27226, #32814, #6228, #61109 ) ),
 .UNSPECIFIED., .F., .F., .F.,
 ( 4, 1, 1, 4 ),
 ( 4, 4 ),
 ( 0.1423941366080999915, 0.3333333333333000081, 0.6666666666667000474, 0.8219462302419999755 ),
 ( -0.1256563615234000120, 1.125656361508000192 ),
 .UNSPECIFIED. ) ;
#54042 = CARTESIAN_POINT ( 'NONE',  ( 3.899999681170999821, 0.000000000000000000, -2.624999810206000372 ) ) ;
#54043 = B_SPLINE_CURVE_WITH_KNOTS ( 'NONE', 3,
 ( #6457, #37933, #59252, #59603, #54354, #11359, #54010, #11702, #6112, #43876, #64835, #27451, #883, #16944, #65182, #12058, #14393, #66568, #36047, #25562, #45263 ),
 .UNSPECIFIED., .F., .F.,
 ( 4, 2, 2, 1, 1, 2, 2, 2, 1, 2, 2, 4 ),
 ( 0.000000000000000000, 0.1249999999999492073, 0.1874999999999213685, 0.2187499999999089617, 0.2343749999999027445, 0.2421874999999015232, 0.2499999999999003575, 0.3749999999999252265, 0.4374999999999350520, 0.4687499999999401035, 0.4999999999999450440, 1.000000000000000000 ),
 .UNSPECIFIED. ) ;
#54044 = CARTESIAN_POINT ( 'NONE',  ( 24.63805661103100064, 8.801154613476001032, 9.346935862444000875 ) ) ;
#54045 = EDGE_LOOP ( 'NONE', ( #53245, #11558, #31561, #17479 ) ) ;
#54046 = CARTESIAN_POINT ( 'NONE',  ( 9.047980646795000581, -2.806079842068999852, 8.615883328687999665 ) ) ;
#54047 = CARTESIAN_POINT ( 'NONE',  ( 8.772439158776000667, 3.098073081301000009, -8.567513114264999174 ) ) ;
#54048 = B_SPLINE_CURVE_WITH_KNOTS ( 'NONE', 3,
 ( #3513, #24851, #40927, #62249 ),
 .UNSPECIFIED., .F., .F.,
 ( 4, 4 ),
 ( 0.000000000000000000, 1.000000000000000000 ),
 .UNSPECIFIED. ) ;
#54049 = ADVANCED_FACE ( 'NONE', ( #65917 ), #50884, .F. ) ;
#54050 = FACE_OUTER_BOUND ( 'NONE', #34510, .T. ) ;
#54051 = CARTESIAN_POINT ( 'NONE',  ( 0.9790647364571333222, 3.399126080497532953, -0.9633645835950521708 ) ) ;
#54052 = VECTOR ( 'NONE', #51965, 1000.000000000000000 ) ;
#54053 = CARTESIAN_POINT ( 'NONE',  ( 0.7407068467740000051, 0.9423624982842000453, -3.239329654985999785 ) ) ;
#54054 = CARTESIAN_POINT ( 'NONE',  ( 10.81524174883999834, 3.971581146373189597, 6.466884287543999577 ) ) ;
#54055 = CARTESIAN_POINT ( 'NONE',  ( 2.170928445476999702, -0.8586646638686999955, 3.659381217151000065 ) ) ;
#54056 = ORIENTED_EDGE ( 'NONE', *, *, #57313, .T. ) ;
#54057 = CARTESIAN_POINT ( 'NONE',  ( 9.321001730958840881, 3.231794228473278352, -6.500403846372135419 ) ) ;
#54058 = CARTESIAN_POINT ( 'NONE',  ( 7.000000000000000000, 0.5292307692307999245, 2.083846153846000249 ) ) ;
#54059 = CARTESIAN_POINT ( 'NONE',  ( 18.03569330394757131, 3.019535577993371689, -12.23285103262380957 ) ) ;
#54060 = CARTESIAN_POINT ( 'NONE',  ( 7.183954769576917698, -2.819171138525097930, 8.180672465553621819 ) ) ;
#54061 = CARTESIAN_POINT ( 'NONE',  ( 9.117517219591000810, 4.954905351382000944, 8.825777580285999235 ) ) ;
#54062 = ORIENTED_EDGE ( 'NONE', *, *, #67828, .F. ) ;
#54063 = CARTESIAN_POINT ( 'NONE',  ( 5.852703546036000404, 0.07932534654106999927, 1.466367974616999748 ) ) ;
#54064 = CARTESIAN_POINT ( 'NONE',  ( 8.344770280407999508, 3.460181152982999997, -6.031076961652000357 ) ) ;
#54065 = CARTESIAN_POINT ( 'NONE',  ( 8.374455264001134935, -2.988149489109947599, 8.916437303143837312 ) ) ;
#54066 = COLOUR_RGB ( '', 0.72549020, 0.75294118, 0.79215686) ;
#54067 = CARTESIAN_POINT ( 'NONE',  ( 9.269442991500000062, -4.080527519162810535, 8.776675254768999679 ) ) ;
#54068 = VERTEX_POINT ( 'NONE', #60682 ) ;
#54069 = DIRECTION ( 'NONE',  ( 1.000000000000000000, 0.000000000000000000, 0.000000000000000000 ) ) ;
#54070 = CARTESIAN_POINT ( 'NONE',  ( 11.53970701685000222, 11.52114570934000071, 1.450082077858000140 ) ) ;
#54071 = VERTEX_POINT ( 'NONE', #34478 ) ;
#54072 = CARTESIAN_POINT ( 'NONE',  ( 24.94501239293118644, 2.983176329050218012, -11.60457232061659205 ) ) ;
#54073 = CARTESIAN_POINT ( 'NONE',  ( 16.44832727683000329, 3.192413998985999868, 11.44999110620999794 ) ) ;
#54074 = AXIS2_PLACEMENT_3D ( 'NONE', #46695, #15211, #30958 ) ;
#54075 = CARTESIAN_POINT ( 'NONE',  ( 17.55505043854144276, -0.6250000000000001110, -13.88107975066922428 ) ) ;
#54076 = EDGE_LOOP ( 'NONE', ( #14890, #27505, #20817, #49716 ) ) ;
#54077 = CARTESIAN_POINT ( 'NONE',  ( 10.39973737267491138, -5.293988795193000030, -8.716508489687221584 ) ) ;
#54078 = CARTESIAN_POINT ( 'NONE',  ( 24.30001682246400208, -8.938702682732001747, -8.938676171235998780 ) ) ;
#54079 = CARTESIAN_POINT ( 'NONE',  ( 11.19434208742519843, 3.521141233577200325, -8.252717006421999457 ) ) ;
#54080 = CARTESIAN_POINT ( 'NONE',  ( 7.100000000000000533, 0.000000000000000000, 0.000000000000000000 ) ) ;
#54081 = DIRECTION ( 'NONE',  ( -1.000000000000000000, 0.000000000000000000, 0.000000000000000000 ) ) ;
#54082 = EDGE_LOOP ( 'NONE', ( #55431, #18507, #28583, #14612 ) ) ;
#54083 = CARTESIAN_POINT ( 'NONE',  ( 8.924954719592001595, 4.158911560497999815, 5.873540104660999184 ) ) ;
#54084 = CARTESIAN_POINT ( 'NONE',  ( 18.18506112704245581, -2.156549459697490345, 13.83291014715494072 ) ) ;
#54085 = EDGE_LOOP ( 'NONE', ( #32275, #67083, #33301, #37383 ) ) ;
#54086 = FILL_AREA_STYLE_COLOUR ( '', #25092 ) ;
#54087 = CARTESIAN_POINT ( 'NONE',  ( 18.00086602813224701, 0.5750310236279777554, 12.58704914195693192 ) ) ;
#54088 = CARTESIAN_POINT ( 'NONE',  ( 10.96255537160999971, 6.761658444318999983, -5.456360451353000407 ) ) ;
#54089 = ORIENTED_EDGE ( 'NONE', *, *, #30312, .F. ) ;
#54090 = CARTESIAN_POINT ( 'NONE',  ( 12.22206196700521375, -2.274492675301823752, -12.50124639636504220 ) ) ;
#54091 = EDGE_CURVE ( 'NONE', #9579, #10089, #20768, .T. ) ;
#54092 = CARTESIAN_POINT ( 'NONE',  ( 7.100000000000000533, 0.000000000000000000, 0.000000000000000000 ) ) ;
#54093 = DIRECTION ( 'NONE',  ( -5.691941604301808236E-06, -0.9659358920123676251, 0.2587814763267914375 ) ) ;
#54094 = CARTESIAN_POINT ( 'NONE',  ( 17.55505043854144276, 0.000000000000000000, -25.00000000000000000 ) ) ;
#54095 = CARTESIAN_POINT ( 'NONE',  ( 12.15443728026463965, -2.840296387118483867, -13.70885984368922372 ) ) ;
#54096 = ADVANCED_FACE ( 'NONE', ( #7538 ), #2302, .F. ) ;
#54097 = CARTESIAN_POINT ( 'NONE',  ( 10.55103166480599874, -5.000984463463999496, -7.570575893572789816 ) ) ;
#54098 = CARTESIAN_POINT ( 'NONE',  ( 12.43699713708037891, -3.107380776419843560, 12.21088077983946363 ) ) ;
#54100 = CARTESIAN_POINT ( 'NONE',  ( 17.93748940951491022, -2.994360127459124943, 12.32254798267195106 ) ) ;
#54099 = B_SPLINE_CURVE_WITH_KNOTS ( 'NONE', 1,
 ( #11900, #11548 ),
 .UNSPECIFIED., .F., .F.,
 ( 2, 2 ),
 ( 0.000000000000000000, 1.000000000000000000 ),
 .UNSPECIFIED. ) ;
#54101 = ORIENTED_EDGE ( 'NONE', *, *, #37167, .T. ) ;
#54102 = CARTESIAN_POINT ( 'NONE',  ( 11.14256920625030034, -3.957769094421040190, -6.325872106312999676 ) ) ;
#54103 = ORIENTED_EDGE ( 'NONE', *, *, #5201, .F. ) ;
#54104 = AXIS2_PLACEMENT_3D ( 'NONE', #52759, #42281, #58687 ) ;
#54105 = DIRECTION ( 'NONE',  ( 0.9999999999999998890, 1.582250227828999695E-08, -5.275446505821999214E-09 ) ) ;
#54106 = CARTESIAN_POINT ( 'NONE',  ( 9.892489158770999325, 5.099602161831000124, -9.049221499261999924 ) ) ;
#54107 = CARTESIAN_POINT ( 'NONE',  ( 10.15787172175999942, 4.213497149090000171, -5.822953133183999874 ) ) ;
#54108 = DIRECTION ( 'NONE',  ( -1.000000000000000000, 0.000000000000000000, 0.000000000000000000 ) ) ;
#54109 = CARTESIAN_POINT ( 'NONE',  ( 23.73952188783414741, -13.33635550666453540, -3.648248442822538351 ) ) ;
#54110 = CARTESIAN_POINT ( 'NONE',  ( 7.612465007326000510, 3.179383379803001564, -6.407107007521996245 ) ) ;
#54111 = DIRECTION ( 'NONE',  ( -0.7071067811865474617, -0.7071067811865474617, -1.029446549002069181E-08 ) ) ;
#54112 = VERTEX_POINT ( 'NONE', #55788 ) ;
#54113 = CARTESIAN_POINT ( 'NONE',  ( 11.39975833414730033, 4.796537143354000499, -7.174999999999999822 ) ) ;
#54114 = CARTESIAN_POINT ( 'NONE',  ( 9.877261637240000169, 2.207988120125000009, 7.624813826992999921 ) ) ;
#54115 = CARTESIAN_POINT ( 'NONE',  ( 10.08079553768663672, -5.100000000000000533, -6.662590550639031939 ) ) ;
#54116 = CARTESIAN_POINT ( 'NONE',  ( 11.11257802013489915, -4.891884252872400474, 7.520762592984879369 ) ) ;
#54117 = CARTESIAN_POINT ( 'NONE',  ( 17.79416955086200147, 3.253172910778000304, -11.33701170283999993 ) ) ;
#54118 = AXIS2_PLACEMENT_3D ( 'NONE', #66918, #36141, #57451 ) ;
#54119 = CARTESIAN_POINT ( 'NONE',  ( 11.04951995735000025, 9.925864394642001542, -5.806870034355000598 ) ) ;
#54120 = LINE ( 'NONE', #993, #39205 ) ;
#54121 = AXIS2_PLACEMENT_3D ( 'NONE', #66899, #24605, #8523 ) ;
#54122 = CARTESIAN_POINT ( 'NONE',  ( 23.61814126825800031, -10.28285508195000020, -9.267271738533999326 ) ) ;
#54123 = EDGE_CURVE ( 'NONE', #21968, #24059, #29230, .T. ) ;
#54124 = CARTESIAN_POINT ( 'NONE',  ( 24.22012566761399910, -8.984033207697999401, 8.868613826359998953 ) ) ;
#54125 = ORIENTED_EDGE ( 'NONE', *, *, #42342, .T. ) ;
#54126 = CARTESIAN_POINT ( 'NONE',  ( 8.921135841230999119, 3.292387953886000140, -6.294868737226000377 ) ) ;
#54127 = CARTESIAN_POINT ( 'NONE',  ( 6.994867733785000041, -1.214120350334000120, -0.6320739451511001583 ) ) ;
#54128 = EDGE_CURVE ( 'NONE', #43538, #55462, #33286, .T. ) ;
#54129 = EDGE_CURVE ( 'NONE', #63173, #12318, #57150, .T. ) ;
#54130 = CARTESIAN_POINT ( 'NONE',  ( 18.17537806675982637, 2.421014888063410808, 13.68986186821173767 ) ) ;
#54131 = LINE ( 'NONE', #5546, #1014 ) ;
#54132 = CARTESIAN_POINT ( 'NONE',  ( 11.60118044953561878, -2.866798846279000390, -8.090905336380599167 ) ) ;
#54133 = ORIENTED_EDGE ( 'NONE', *, *, #62642, .F. ) ;
#54134 = CARTESIAN_POINT ( 'NONE',  ( 25.41799978389900261, 2.807552223335999741, -11.31775031636999884 ) ) ;
#54135 = CARTESIAN_POINT ( 'NONE',  ( 9.170323341230000480, 5.558938731259999599, 6.272977177425000050 ) ) ;
#54137 = FACE_OUTER_BOUND ( 'NONE', #62339, .T. ) ;
#54136 = CARTESIAN_POINT ( 'NONE',  ( 8.704995280412999747, 5.140767546012999567, -6.196177269779999719 ) ) ;
#54138 = CARTESIAN_POINT ( 'NONE',  ( 3.316457242269348349, 2.850256168064621232, 1.578002730033648993 ) ) ;
#54139 = ORIENTED_EDGE ( 'NONE', *, *, #16779, .F. ) ;
#54140 = CARTESIAN_POINT ( 'NONE',  ( 9.924742128742000347, 5.060458431729999873, 8.686130311522999747 ) ) ;
#54141 = CARTESIAN_POINT ( 'NONE',  ( 18.17327101506966969, -2.135860178445234236, -13.83613041148202605 ) ) ;
#54142 = CARTESIAN_POINT ( 'NONE',  ( 11.21564426047340035, 4.539962866738299851, 6.654192128557399499 ) ) ;
#54143 = CARTESIAN_POINT ( 'NONE',  ( 11.29621718459000057, -3.561654022787999807, 6.266039799355000106 ) ) ;
#54144 = CARTESIAN_POINT ( 'NONE',  ( 7.544198296194000619, 2.929983868333001951, 6.556648683638004016 ) ) ;
#54145 = EDGE_LOOP ( 'NONE', ( #19381, #55392 ) ) ;
#54146 = CARTESIAN_POINT ( 'NONE',  ( 8.832537864289999874, 2.899999999999999911, 6.571291218949999902 ) ) ;
#54147 = EDGE_CURVE ( 'NONE', #10337, #21003, #41420, .T. ) ;
#54149 = CARTESIAN_POINT ( 'NONE',  ( 11.12964314679000033, -3.869080819553999628, -9.017146989745999264 ) ) ;
#54148 = CARTESIAN_POINT ( 'NONE',  ( 12.70688507812400125, -11.81408563393000044, 3.326099274546999940 ) ) ;
#54150 = CARTESIAN_POINT ( 'NONE',  ( 7.896885084209208649, -2.621122013384412419, 8.559930520408130405 ) ) ;
#54151 = CARTESIAN_POINT ( 'NONE',  ( 10.40226385995999969, -2.765692573780999641, 9.035345396600000356 ) ) ;
#54152 = DIRECTION ( 'NONE',  ( 1.000000000000000000, 0.000000000000000000, 0.000000000000000000 ) ) ;
#54153 = ORIENTED_EDGE ( 'NONE', *, *, #29066, .F. ) ;
#54154 = CARTESIAN_POINT ( 'NONE',  ( 9.539763540182331525, 4.327184855449099921, -8.717465845835397076 ) ) ;
#54155 = CARTESIAN_POINT ( 'NONE',  ( 11.10026222744819790, -4.774534945026900346, 6.861998062869400172 ) ) ;
#54156 = CARTESIAN_POINT ( 'NONE',  ( 7.428092358015002006, 3.524408735919001501, 6.653372890553997721 ) ) ;
#54157 = CARTESIAN_POINT ( 'NONE',  ( 11.18272066707849888, 5.093522884867000222, 8.161456030935699602 ) ) ;
#54158 = PRODUCT_DEFINITION_FORMATION_WITH_SPECIFIED_SOURCE ( 'ANY', '', #46133, .NOT_KNOWN. ) ;
#54159 = ORIENTED_EDGE ( 'NONE', *, *, #21267, .T. ) ;
#54160 = CARTESIAN_POINT ( 'NONE',  ( 9.700639158771000581, 4.262870449202000422, -8.811513791423999820 ) ) ;
#54161 = CARTESIAN_POINT ( 'NONE',  ( 12.29866314003339589, 2.995318252715385654, -12.23879431495722514 ) ) ;
#54162 = CARTESIAN_POINT ( 'NONE',  ( 11.93345123989529988, -3.459769760840400110, 6.456682674800999777 ) ) ;
#54163 = CARTESIAN_POINT ( 'NONE',  ( 9.137709786520556321, 4.829499945559576624, -8.579760339927545942 ) ) ;
#54164 = DIRECTION ( 'NONE',  ( 1.000000000000000000, 0.000000000000000000, 0.000000000000000000 ) ) ;
#54165 = ORIENTED_EDGE ( 'NONE', *, *, #17923, .T. ) ;
#54166 = CARTESIAN_POINT ( 'NONE',  ( 7.598066940377999678, -3.554853390786000045, 8.889491623367000273 ) ) ;
#54167 = CARTESIAN_POINT ( 'NONE',  ( 5.565443173016707767, -1.500000000000000222, -0.1963495408493622363 ) ) ;
#54168 = ORIENTED_EDGE ( 'NONE', *, *, #40190, .T. ) ;
#54169 = CARTESIAN_POINT ( 'NONE',  ( 12.40985643288215812, -3.083578315866618347, -12.21685683184791138 ) ) ;
#54171 = CARTESIAN_POINT ( 'NONE',  ( 10.45672469555900008, 4.433465011431599656, 8.249937779480299938 ) ) ;
#54170 = AXIS2_PLACEMENT_3D ( 'NONE', #68305, #14503, #26715 ) ;
#54172 = EDGE_CURVE ( 'NONE', #51180, #17467, #60028, .T. ) ;
#54173 = CARTESIAN_POINT ( 'NONE',  ( 9.571961069101000419, 4.084683332033999470, 8.946609345378000455 ) ) ;
#54174 = CARTESIAN_POINT ( 'NONE',  ( 10.89212517796999968, 2.946919582117999870, -5.013248949648000163 ) ) ;
#54175 = CARTESIAN_POINT ( 'NONE',  ( 7.948904172952001801, 4.897346594336003278, 6.290771953639007208 ) ) ;
#54176 = CARTESIAN_POINT ( 'NONE',  ( 10.80169466977000070, -3.998196228428999355, 9.431543037543999475 ) ) ;
#54177 = CYLINDRICAL_SURFACE ( 'NONE', #66698, 1.250000000000000222 ) ;
#54178 = CARTESIAN_POINT ( 'NONE',  ( 17.67403227923241005, -0.7096370184368607781, -12.58000072970462924 ) ) ;
#54179 = EDGE_CURVE ( 'NONE', #67539, #40612, #56697, .T. ) ;
#54180 = DIRECTION ( 'NONE',  ( 1.000000000000000000, 0.000000000000000000, 0.000000000000000000 ) ) ;
#54181 = CARTESIAN_POINT ( 'NONE',  ( 10.57149279008999798, -4.296686446741600385, -8.601484120896000007 ) ) ;
#54182 = CARTESIAN_POINT ( 'NONE',  ( 7.892607780408998686, 5.480308727866000318, 8.192324747680999053 ) ) ;
#54183 = EDGE_LOOP ( 'NONE', ( #505, #65580, #50313, #30079 ) ) ;
#54184 = CARTESIAN_POINT ( 'NONE',  ( 23.60205915885299888, -11.72032963058999400, 3.891881970957998593 ) ) ;
#54185 = CARTESIAN_POINT ( 'NONE',  ( 9.652931135702420562, 5.100000000000000533, -6.444141223381762096 ) ) ;
#54186 = CARTESIAN_POINT ( 'NONE',  ( 11.48828127163000268, 12.23964378314000001, 1.839251152677999990 ) ) ;
#54187 = CARTESIAN_POINT ( 'NONE',  ( 18.22966818124860211, 2.744306698987324822, 12.29751612260396954 ) ) ;
#54188 = CARTESIAN_POINT ( 'NONE',  ( 12.54752909501214297, 1.835309592424127834, 13.87918066653183224 ) ) ;
#54189 = CARTESIAN_POINT ( 'NONE',  ( 11.00094363691999888, 8.784914713122999430, 6.555567193519999947 ) ) ;
#54190 = DIRECTION ( 'NONE',  ( 0.000000000000000000, -0.9439966912222074180, -0.3299549165591025846 ) ) ;
#54191 = CARTESIAN_POINT ( 'NONE',  ( 25.46372189163300348, -2.879475976718999686, 11.30953721564000070 ) ) ;
#54192 = ORIENTED_EDGE ( 'NONE', *, *, #61008, .F. ) ;
#54193 = CARTESIAN_POINT ( 'NONE',  ( 12.75668783919150151, -3.198551280946745567, 12.18725874734143844 ) ) ;
#54194 = CARTESIAN_POINT ( 'NONE',  ( 10.31357120343299982, -4.048688523195909994, -8.503230697164999796 ) ) ;
#54195 = CARTESIAN_POINT ( 'NONE',  ( 10.40516904918000129, 5.216391323504000255, 6.765759859247999941 ) ) ;
#54196 = CARTESIAN_POINT ( 'NONE',  ( 8.290071854142535557, 2.941495930016484461, -6.434443241224298227 ) ) ;
#54197 = B_SPLINE_SURFACE_WITH_KNOTS ( 'NONE', 3, 3, ( 
 ( #55926, #18867, #40195, #29368, #45437, #23419, #17835, #7331, #61511, #49990, #19200, #60133, #44754, #2102, #12242, #54886, #66058, #28318, #18178, #39499, #45096, #66402, #39847, #14648, #8715, #68112, #25474, #10078, #41896, #19891, #4826, #20571, #4479, #40522, #56950 ),
 ( #30059, #63204, #35294, #15332, #52034, #31416, #20229, #52732, #51361, #3455, #24793, #40868, #46119, #46806, #57627, #67425, #61849, #62191, #26169, #36660, #47148, #35637, #68799, #52384, #57981, #3795, #14312, #41218, #19549, #56609, #9048, #62528, #30388, #35964, #30726 ),
 ( #46464, #31078, #47493, #14983, #13965, #51698, #57279, #25131, #25819, #67764, #9383, #36308, #4137, #41555, #68449, #62865, #9728, #6556, #37684, #27544, #27202, #38023, #33138, #21260, #27898, #54107, #58319, #49208, #58664, #26513, #47844, #63559, #54454, #42590, #20920 ),
 ( #5178, #15674, #6202, #48871, #21941, #16013, #978, #32791, #64241, #10766, #59697, #42256, #37003, #69153, #38373, #16695, #11799, #53426, #43278, #10421, #32109, #42934, #63898, #26864, #11452, #22291, #64586, #31762, #53079, #21595, #37342, #43631, #5524, #48177, #59350 ) ),
 .UNSPECIFIED., .F., .F., .F.,
 ( 4, 4 ),
 ( 4, 1, 1, 1, 1, 1, 1, 1, 1, 1, 1, 1, 1, 1, 1, 1, 1, 1, 1, 1, 1, 1, 1, 1, 1, 1, 1, 1, 1, 1, 1, 1, 4 ),
 ( -0.1039370721279000015, 1.103937072127999963 ),
 ( 0.1942321073450000157, 0.2199060843169000079, 0.2455800612886999967, 0.2712540382605999612, 0.2969280152323999777, 0.3226019922043000254, 0.3482759691761000420, 0.3739499461479999787, 0.3996239231197999953, 0.4252979000916999874, 0.4509718770635000040, 0.4766458540353999962, 0.5023198310072000128, 0.5279938079791000050, 0.5536677849509000771, 0.5793417619227999582, 0.6050157388945999193, 0.6306897158665000225, 0.6563636928382999836, 0.6820376698101999757, 0.7077116467820000478, 0.7333856237539000400, 0.7590596007256998901, 0.7847335776975999933, 0.8104075546693999543, 0.8360815316413000575, 0.8617555086131000186, 0.8874294855850000108, 0.9131034625568000829, 0.9387774395286999640, 0.9644514165004999251, 0.9901253934722999972, 1.015799370444000038 ),
 .UNSPECIFIED. ) ;
#54198 = CARTESIAN_POINT ( 'NONE',  ( 10.64949279009019989, 3.739015461786900030, -8.468936491037499792 ) ) ;
#54199 = CARTESIAN_POINT ( 'NONE',  ( 12.25943167926923749, -0.4738025322793273930, 12.59109159930368627 ) ) ;
#54200 = CARTESIAN_POINT ( 'NONE',  ( 8.496698341230001006, 5.198556077301000222, 8.332552905512999430 ) ) ;
#54201 = CARTESIAN_POINT ( 'NONE',  ( 9.691082467489000152, 5.335647408863999352, 8.701220655673999715 ) ) ;
#54202 = CARTESIAN_POINT ( 'NONE',  ( 12.18551697106545717, 2.583096739011645493, 12.43182067874258578 ) ) ;
#54203 = ORIENTED_EDGE ( 'NONE', *, *, #33056, .T. ) ;
#54204 = CARTESIAN_POINT ( 'NONE',  ( 11.00000000058999916, -1.300000000000000044, -9.662944685757000940 ) ) ;
#54205 = CARTESIAN_POINT ( 'NONE',  ( 11.48225819896749833, 2.879005208331999910, -7.711331004020999913 ) ) ;
#54206 = CARTESIAN_POINT ( 'NONE',  ( 18.17069881803083220, -0.3800566752825981776, 12.59427093624936234 ) ) ;
#54207 = ADVANCED_FACE ( 'NONE', ( #47358 ), #63377, .F. ) ;
#54208 = EDGE_CURVE ( 'NONE', #32603, #69137, #38355, .T. ) ;
#54209 = CARTESIAN_POINT ( 'NONE',  ( 10.29667028040999988, 2.755514216060999999, -6.622437150225000124 ) ) ;
#54210 = FACE_OUTER_BOUND ( 'NONE', #64989, .T. ) ;
#54212 = CARTESIAN_POINT ( 'NONE',  ( 18.00675905399072363, -0.4321659192889827916, 12.69010673283423429 ) ) ;
#54211 = CARTESIAN_POINT ( 'NONE',  ( 7.875072778631000858, 5.143389081112999861, 6.784077933858997156 ) ) ;
#54213 = CARTESIAN_POINT ( 'NONE',  ( 11.66883611569390489, 12.15999240567520268, 2.000270994069734964 ) ) ;
#54214 = VERTEX_POINT ( 'NONE', #52591 ) ;
#54215 = VECTOR ( 'NONE', #9156, 1000.000000000000114 ) ;
#54216 = FACE_OUTER_BOUND ( 'NONE', #4549, .T. ) ;
#54217 = CARTESIAN_POINT ( 'NONE',  ( 18.29983863915591158, 0.9627070266348703997, 12.32514598389175831 ) ) ;
#54218 = AXIS2_PLACEMENT_3D ( 'NONE', #66624, #22938, #50212 ) ;
#54219 = CARTESIAN_POINT ( 'NONE',  ( 17.65223863466379228, -0.7192245859875955327, -12.57945610904468658 ) ) ;
#54220 = FACE_OUTER_BOUND ( 'NONE', #52509, .T. ) ;
#54221 = CARTESIAN_POINT ( 'NONE',  ( 12.17076609166790746, -2.871707895891081108, 13.70231394784453371 ) ) ;
#54222 = CARTESIAN_POINT ( 'NONE',  ( 10.90769129028899798, -4.889436474118636689, 6.586710612921465646 ) ) ;
#54223 = CARTESIAN_POINT ( 'NONE',  ( 24.42335332038400253, 3.752413731090000315, -12.53707314549000174 ) ) ;
#54224 = ORIENTED_EDGE ( 'NONE', *, *, #52475, .F. ) ;
#54225 = ADVANCED_FACE ( 'NONE', ( #35496 ), #37851, .F. ) ;
#54226 = CARTESIAN_POINT ( 'NONE',  ( 12.10000669845703847, 11.02846243759400124, -3.754394857303852362 ) ) ;
#54227 = DIRECTION ( 'NONE',  ( 0.000000000000000000, 0.2461538461537955413, -0.9692307692307821076 ) ) ;
#54228 = CARTESIAN_POINT ( 'NONE',  ( 7.100000000000000533, -12.03770622561999915, 3.722046322334000124 ) ) ;
#54229 = CARTESIAN_POINT ( 'NONE',  ( 10.62947109217999930, -5.100000000000000533, 6.152188490330000370 ) ) ;
#54230 = DIRECTION ( 'NONE',  ( 1.000000000000000000, 0.000000000000000000, 0.000000000000000000 ) ) ;
#54231 = CARTESIAN_POINT ( 'NONE',  ( 17.78721996965301955, 1.919630126996079600, -12.56804012644223612 ) ) ;
#54232 = CARTESIAN_POINT ( 'NONE',  ( 9.532678149083000818, 4.663044775770000427, 8.669813205957000335 ) ) ;
#54233 = CARTESIAN_POINT ( 'NONE',  ( 11.44133594839949986, 4.569506585117100173, 8.152656755002400502 ) ) ;
#54234 = CARTESIAN_POINT ( 'NONE',  ( 11.58810207955109917, -4.796537143354000499, -7.174999999999999822 ) ) ;
#54235 = CARTESIAN_POINT ( 'NONE',  ( 10.54684435321000002, -3.691674321452999674, -9.157280075569998345 ) ) ;
#54236 = CARTESIAN_POINT ( 'NONE',  ( 12.80505043854144276, -0.6250000000000001110, 12.67928921589117586 ) ) ;
#54237 = DIRECTION ( 'NONE',  ( 1.000000000000000000, 0.000000000000000000, 0.000000000000000000 ) ) ;
#54238 = CARTESIAN_POINT ( 'NONE',  ( 24.31006797060300073, 12.13011445653000031, 3.289861759914999517 ) ) ;
#54239 = CARTESIAN_POINT ( 'NONE',  ( 5.599958567364899942, -11.06886219213000011, 1.536526853569999851 ) ) ;
#54240 = ORIENTED_EDGE ( 'NONE', *, *, #29774, .T. ) ;
#54241 = CARTESIAN_POINT ( 'NONE',  ( 7.477183612850018868, 2.357857793230528465, 6.915030216468147195 ) ) ;
#54242 = CARTESIAN_POINT ( 'NONE',  ( 10.70641772631199906, -3.568446272909699957, 6.611684804099500212 ) ) ;
#54243 = ORIENTED_EDGE ( 'NONE', *, *, #42695, .F. ) ;
#54244 = B_SPLINE_CURVE_WITH_KNOTS ( 'NONE', 3,
 ( #11432, #17733, #33814, #56159, #28927, #28569 ),
 .UNSPECIFIED., .F., .F.,
 ( 4, 2, 4 ),
 ( 0.000000000000000000, 0.5000000000000000000, 1.000000000000000000 ),
 .UNSPECIFIED. ) ;
#54245 = CARTESIAN_POINT ( 'NONE',  ( 17.96105691736160637, -2.975276276409919873, 13.56109295189183150 ) ) ;
#54246 = CARTESIAN_POINT ( 'NONE',  ( 10.34995525820099971, -4.107710726525199973, -6.364355462479999836 ) ) ;
#54247 = ORIENTED_EDGE ( 'NONE', *, *, #58785, .F. ) ;
#54248 = CARTESIAN_POINT ( 'NONE',  ( 10.56080513895999928, 5.026880838510000338, 8.070849345005600028 ) ) ;
#54249 = CARTESIAN_POINT ( 'NONE',  ( 5.534428103885884020, 0.9514691251117015636, -0.6142997976039359376 ) ) ;
#54250 = CARTESIAN_POINT ( 'NONE',  ( 8.410398127216504705, 5.351350780489198655, 7.263115598813870477 ) ) ;
#54251 = AXIS2_PLACEMENT_3D ( 'NONE', #10196, #25931, #26282 ) ;
#54252 = CARTESIAN_POINT ( 'NONE',  ( 17.77441288034700051, -3.189751316310999840, 11.45074679932000095 ) ) ;
#54253 = CARTESIAN_POINT ( 'NONE',  ( 12.07956470885932987, -2.330212498096153606, -13.80606232674627520 ) ) ;
#54254 = DIRECTION ( 'NONE',  ( -1.000000000000000000, 0.000000000000000000, 0.000000000000000000 ) ) ;
#54255 = CARTESIAN_POINT ( 'NONE',  ( 6.934611375570498559, -0.2896425330593513925, -1.105727683284202678 ) ) ;
#54256 = EDGE_CURVE ( 'NONE', #19885, #47743, #55672, .T. ) ;
#54257 = CARTESIAN_POINT ( 'NONE',  ( 9.753033816428001046, -4.922930220739999641, -8.639537379291999386 ) ) ;
#54258 = DIRECTION ( 'NONE',  ( -1.000000000000000000, 0.000000000000000000, 0.000000000000000000 ) ) ;
#54259 = ORIENTED_EDGE ( 'NONE', *, *, #60451, .T. ) ;
#54260 = CARTESIAN_POINT ( 'NONE',  ( 8.771960841230001193, 3.061731693614000438, -8.535706278603999664 ) ) ;
#54261 = ORIENTED_EDGE ( 'NONE', *, *, #12878, .T. ) ;
#54262 = CIRCLE ( 'NONE', #45353, 12.39999890530000037 ) ;
#54263 = CARTESIAN_POINT ( 'NONE',  ( 10.05205635875000070, 2.669891600604999748, -8.791543746052999708 ) ) ;
#54264 = SURFACE_STYLE_USAGE ( .BOTH. , #37845 ) ;
#54265 = VERTEX_POINT ( 'NONE', #33694 ) ;
#54266 = CARTESIAN_POINT ( 'NONE',  ( 9.600000000000001421, 0.000000000000000000, 0.000000000000000000 ) ) ;
#54267 = CARTESIAN_POINT ( 'NONE',  ( 18.01300802853351968, -2.925445001331292705, -12.34219835790438502 ) ) ;
#54268 = AXIS2_PLACEMENT_3D ( 'NONE', #4730, #21169, #58228 ) ;
#54269 = CARTESIAN_POINT ( 'NONE',  ( 10.63214998050358773, -2.955201170656483800, 5.051157783803637891 ) ) ;
#54270 = CARTESIAN_POINT ( 'NONE',  ( 10.37309687351658383, 2.782534154164606921, -7.172815144550898303 ) ) ;
#54271 = CARTESIAN_POINT ( 'NONE',  ( 12.49912319420860030, 3.045104416349984522, 13.54255671968480357 ) ) ;
#54272 = CARTESIAN_POINT ( 'NONE',  ( 9.532671748231999587, -4.663050389319001177, 8.669823109968998409 ) ) ;
#54273 = CARTESIAN_POINT ( 'NONE',  ( 10.27164068750306569, 2.873222873834239799, 6.752018918838213146 ) ) ;
#54274 = CARTESIAN_POINT ( 'NONE',  ( 12.78440343889028874, 0.6249994633519863063, 13.88107975068473365 ) ) ;
#54275 = ORIENTED_EDGE ( 'NONE', *, *, #10088, .T. ) ;
#54276 = CARTESIAN_POINT ( 'NONE',  ( 7.132090560819000835, 2.788803157567000035, -8.345558963038001821 ) ) ;
#54277 = CARTESIAN_POINT ( 'NONE',  ( 18.30003129332100187, 2.732683818840999646, 11.53064095373000164 ) ) ;
#54278 = CARTESIAN_POINT ( 'NONE',  ( 9.606837339593626623, 3.135127465292355087, 7.632392475727677095 ) ) ;
#54279 = CARTESIAN_POINT ( 'NONE',  ( 4.995294366068000258, -0.4131193957761999935, 1.492006182730000186 ) ) ;
#54280 = CARTESIAN_POINT ( 'NONE',  ( 8.830545280412000153, 3.207599814920999659, -6.150466394809999571 ) ) ;
#54281 = CARTESIAN_POINT ( 'NONE',  ( 10.97807333593999957, 5.235090452703000885, -6.783100406990000053 ) ) ;
#54282 = CARTESIAN_POINT ( 'NONE',  ( 10.24845588172999911, -4.234132110154000372, -5.660862927546999934 ) ) ;
#54283 = ORIENTED_EDGE ( 'NONE', *, *, #5982, .F. ) ;
#54284 = DIRECTION ( 'NONE',  ( -1.000000000000000000, 0.000000000000000000, 0.000000000000000000 ) ) ;
#54285 = CARTESIAN_POINT ( 'NONE',  ( 11.05568736158000043, 5.199900061860000200, -4.877315744757000360 ) ) ;
#54286 = CARTESIAN_POINT ( 'NONE',  ( 4.412918875529167728, 0.3262666342505332051, 1.484200010477007226 ) ) ;
#54287 = CARTESIAN_POINT ( 'NONE',  ( 8.767879976495999372, -3.394455611366999914, -6.293427637271999942 ) ) ;
#54288 = DIRECTION ( 'NONE',  ( 1.000000000000000000, 0.000000000000000000, 0.000000000000000000 ) ) ;
#54289 = DIRECTION ( 'NONE',  ( -0.8660254017593186360, 3.394428858350072688E-12, -0.5000000035076106464 ) ) ;
#54290 = EDGE_CURVE ( 'NONE', #42842, #27465, #65836, .T. ) ;
#54291 = ADVANCED_FACE ( 'NONE', ( #44543 ), #37729, .T. ) ;
#54292 = CARTESIAN_POINT ( 'NONE',  ( 11.43345123989529810, 4.540230239159599890, -8.543317325199000223 ) ) ;
#54293 = CARTESIAN_POINT ( 'NONE',  ( 10.25944474310099785, 4.893483781708200198, -7.933599538786499039 ) ) ;
#54295 = CARTESIAN_POINT ( 'NONE',  ( 8.455555256449757806, 5.100005072561971886, -6.567582415677733820 ) ) ;
#54294 = CARTESIAN_POINT ( 'NONE',  ( 9.471126402771000485, -3.060189502158800146, 7.854398824525599565 ) ) ;
#54296 = CARTESIAN_POINT ( 'NONE',  ( 7.925467018026002286, -3.503349646405999884, 6.315515750141001305 ) ) ;
#54297 = ORIENTED_EDGE ( 'NONE', *, *, #24051, .T. ) ;
#54298 = VECTOR ( 'NONE', #54429, 1000.000000000000000 ) ;
#54299 = CARTESIAN_POINT ( 'NONE',  ( 10.85168717260509830, 3.386210853237200169, 6.498190316041999814 ) ) ;
#54300 = AXIS2_PLACEMENT_3D ( 'NONE', #67314, #63446, #30963 ) ;
#54301 = CARTESIAN_POINT ( 'NONE',  ( 7.925467018026002286, -3.503349646405999884, 6.315515750141001305 ) ) ;
#54302 = CARTESIAN_POINT ( 'NONE',  ( 9.454392757686999715, 4.770706668257700400, 6.657535947657399866 ) ) ;
#54303 = CARTESIAN_POINT ( 'NONE',  ( 5.700000000000000178, -13.04986661130000059, -1.811520473896000016 ) ) ;
#54304 = CARTESIAN_POINT ( 'NONE',  ( 9.075489683949001574, -4.020837068201999820, 8.948702918089999514 ) ) ;
#54305 = CARTESIAN_POINT ( 'NONE',  ( 24.45625626939792951, 12.38367859507303415, 3.108175842103299669 ) ) ;
#54306 = CARTESIAN_POINT ( 'NONE',  ( 11.74249537357300177, 3.528133194209999601, -11.96072866431000037 ) ) ;
#54307 = B_SPLINE_CURVE_WITH_KNOTS ( 'NONE', 3,
 ( #64227, #16344, #15661, #47482 ),
 .UNSPECIFIED., .F., .F.,
 ( 4, 4 ),
 ( 0.000000000000000000, 1.000000000000000000 ),
 .UNSPECIFIED. ) ;
#54308 = APPLICATION_CONTEXT ( 'automotive_design' ) ;
#54309 = EDGE_CURVE ( 'NONE', #8973, #22792, #28332, .T. ) ;
#54310 = CARTESIAN_POINT ( 'NONE',  ( 9.330709346416998784, -3.092687088662700035, -7.069157126958599768 ) ) ;
#54311 = CARTESIAN_POINT ( 'NONE',  ( 5.505001685446000437, 0.6181797131151999247, -1.000516987031000005 ) ) ;
#54312 = EDGE_CURVE ( 'NONE', #62750, #26055, #38219, .T. ) ;
#54313 = CARTESIAN_POINT ( 'NONE',  ( 7.000000000000000000, 6.255435840762999966, 3.000000000000000000 ) ) ;
#54314 = CARTESIAN_POINT ( 'NONE',  ( 9.906851002540999929, 2.832432432432000269, -6.822293592207000934 ) ) ;
#54315 = CARTESIAN_POINT ( 'NONE',  ( 12.26133460557259980, -3.860150918677800025, 6.645166161828299778 ) ) ;
#54316 = CARTESIAN_POINT ( 'NONE',  ( 9.933148997456999751, -5.167567567567999731, 6.822293592207000934 ) ) ;
#54317 = CARTESIAN_POINT ( 'NONE',  ( 6.433333127195900225, 12.43895222601181771, -2.828919834973015579 ) ) ;
#54318 = CARTESIAN_POINT ( 'NONE',  ( 25.08881512370800237, -8.444445702635000828, 8.588598710570000350 ) ) ;
#54319 = CARTESIAN_POINT ( 'NONE',  ( 12.75601868328677213, 3.199663661910121526, 12.18696649917219332 ) ) ;
#54320 = ORIENTED_EDGE ( 'NONE', *, *, #18274, .F. ) ;
#54321 = CARTESIAN_POINT ( 'NONE',  ( 25.59994555223600088, 9.407310119912997592, -6.227539428020409495 ) ) ;
#54322 = ITEM_DEFINED_TRANSFORMATION ( 'NONE', 'NONE', #56368,  #9676 ) ;
#54323 = CARTESIAN_POINT ( 'NONE',  ( 10.36325056272499978, -3.107965259299500183, -7.513220396995270001 ) ) ;
#54324 = FACE_OUTER_BOUND ( 'NONE', #28485, .T. ) ;
#54325 = CARTESIAN_POINT ( 'NONE',  ( 17.60000003185799855, -12.11983897296999935, 3.159727888982000188 ) ) ;
#54326 = CARTESIAN_POINT ( 'NONE',  ( 7.000000000000000000, 9.782049358651168092, 4.603971795490571672 ) ) ;
#54327 = CARTESIAN_POINT ( 'NONE',  ( 5.655092287088755221, 12.08052032219111815, -3.735600122825968317 ) ) ;
#54328 = ORIENTED_EDGE ( 'NONE', *, *, #55535, .F. ) ;
#54329 = CARTESIAN_POINT ( 'NONE',  ( 24.35365242081699932, 8.885108761891000739, 7.331500822262997374 ) ) ;
#54330 = CARTESIAN_POINT ( 'NONE',  ( 17.84291783703835677, 3.054853729147657848, -13.53999333998545573 ) ) ;
#54331 = ORIENTED_EDGE ( 'NONE', *, *, #23517, .T. ) ;
#54332 = DIRECTION ( 'NONE',  ( 1.000000000000000000, 0.000000000000000000, 0.000000000000000000 ) ) ;
#54333 = CARTESIAN_POINT ( 'NONE',  ( 24.66912214958201233, 8.674026130943369495, -8.642841412892551034 ) ) ;
#54334 = CARTESIAN_POINT ( 'NONE',  ( 9.459729719592999686, 2.527713920559999661, -6.969421869128999525 ) ) ;
#54335 = VERTEX_POINT ( 'NONE', #62909 ) ;
#54336 = DIRECTION ( 'NONE',  ( -1.000000000000000000, 0.000000000000000000, 0.000000000000000000 ) ) ;
#54337 = CARTESIAN_POINT ( 'NONE',  ( 11.76077869730539938, -4.595338376575799799, -6.326049646822999861 ) ) ;
#54338 = CARTESIAN_POINT ( 'NONE',  ( 7.613660841224000109, 2.100129367691999871, -7.493434492293999938 ) ) ;
#54339 = FACE_OUTER_BOUND ( 'NONE', #52312, .T. ) ;
#54340 = CARTESIAN_POINT ( 'NONE',  ( 9.450685262603977677, 5.278039455209302844, 7.934618797907818433 ) ) ;
#54341 = ORIENTED_EDGE ( 'NONE', *, *, #38048, .F. ) ;
#54342 = CARTESIAN_POINT ( 'NONE',  ( 10.06844525594999951, -4.148609764890999863, 8.941457795715999524 ) ) ;
#54343 = CARTESIAN_POINT ( 'NONE',  ( 17.86920599196271198, -3.040695425050457867, -13.54374392799785198 ) ) ;
#54344 = DIRECTION ( 'NONE',  ( 1.000000000000000000, 0.000000000000000000, 5.921189464682000602E-14 ) ) ;
#54345 = ORIENTED_EDGE ( 'NONE', *, *, #34544, .F. ) ;
#54346 = CARTESIAN_POINT ( 'NONE',  ( 10.91943903453000075, 3.268382602297999817, -6.413946631105000407 ) ) ;
#54347 = CARTESIAN_POINT ( 'NONE',  ( 10.16007944038000055, -4.812966563646999596, -8.526591612524001107 ) ) ;
#54348 = VERTEX_POINT ( 'NONE', #42975 ) ;
#54349 = CARTESIAN_POINT ( 'NONE',  ( 8.748138961223999033, 4.832207374954999857, 6.937618199889199033 ) ) ;
#54350 = DIRECTION ( 'NONE',  ( 0.000000000000000000, 0.2461538461537955413, -0.9692307692307821076 ) ) ;
#54351 = CARTESIAN_POINT ( 'NONE',  ( 4.750651961078999896, 1.377769485253000248, 0.3289013390324999619 ) ) ;
#54352 = CARTESIAN_POINT ( 'NONE',  ( 7.857643339617994549, 5.082727619679005215, -6.471061634085996772 ) ) ;
#54353 = EDGE_CURVE ( 'NONE', #5840, #49573, #15687, .T. ) ;
#54354 = CARTESIAN_POINT ( 'NONE',  ( 24.65657919783774332, 11.83373535527700504, -3.192275918523050482 ) ) ;
#54355 = CARTESIAN_POINT ( 'NONE',  ( 7.279117636432513194, 2.756047754360720692, -8.107296174373129105 ) ) ;
#54356 = AXIS2_PLACEMENT_3D ( 'NONE', #29237, #60346, #55103 ) ;
#54357 = CARTESIAN_POINT ( 'NONE',  ( 9.940621437244999470, 4.575883738927100097, 8.148124882831599081 ) ) ;
#54358 = DIRECTION ( 'NONE',  ( 1.000000000000000000, 0.000000000000000000, 0.000000000000000000 ) ) ;
#54359 = B_SPLINE_CURVE_WITH_KNOTS ( 'NONE', 3,
 ( #8750, #25515, #47188, #9086 ),
 .UNSPECIFIED., .F., .F.,
 ( 4, 4 ),
 ( 0.000000000000000000, 1.000000000000000000 ),
 .UNSPECIFIED. ) ;
#54360 = B_SPLINE_CURVE_WITH_KNOTS ( 'NONE', 3,
 ( #19013, #67580, #51509, #57436, #62346, #40337 ),
 .UNSPECIFIED., .F., .F.,
 ( 4, 2, 4 ),
 ( 0.000000000000000000, 0.5000000000000000000, 1.000000000000000000 ),
 .UNSPECIFIED. ) ;
#54361 = VERTEX_POINT ( 'NONE', #10128 ) ;
#54362 = FACE_OUTER_BOUND ( 'NONE', #38218, .T. ) ;
#54363 = CARTESIAN_POINT ( 'NONE',  ( 11.05392028041000074, 5.159483628325999938, -8.487146968478000986 ) ) ;
#54364 = CARTESIAN_POINT ( 'NONE',  ( 13.39991752512754530, 12.13029446165148961, 2.190571078338882760 ) ) ;
#54365 = CARTESIAN_POINT ( 'NONE',  ( 12.20418674196358388, 2.672312675674151095, -13.63540648336421413 ) ) ;
#54366 = CARTESIAN_POINT ( 'NONE',  ( 10.24160887879199855, -4.289688213680199702, -6.254020414961999563 ) ) ;
#54367 = CARTESIAN_POINT ( 'NONE',  ( 24.98214774730800158, 3.089314405311999856, 11.61702339075000090 ) ) ;
#54368 = CARTESIAN_POINT ( 'NONE',  ( 18.14493363608988474, -0.4251989115648892592, 13.99355557726514654 ) ) ;
#54369 = CARTESIAN_POINT ( 'NONE',  ( 1.699999999999999956, -2.250000000000000000, 0.000000000000000000 ) ) ;
#54370 = VERTEX_POINT ( 'NONE', #31460 ) ;
#54371 = ORIENTED_EDGE ( 'NONE', *, *, #3137, .F. ) ;
#54372 = AXIS2_PLACEMENT_3D ( 'NONE', #15043, #19608, #68513 ) ;
#54373 = CARTESIAN_POINT ( 'NONE',  ( 9.799251915619999309, 4.057329420971000467, 9.430703183047999261 ) ) ;
#54374 = CARTESIAN_POINT ( 'NONE',  ( 12.20071588506785254, -0.1606973241710302203, 13.89876784138693289 ) ) ;
#54375 = CARTESIAN_POINT ( 'NONE',  ( 12.29146891699357091, -0.3563501258530247240, -13.89385640120244325 ) ) ;
#54376 = DIRECTION ( 'NONE',  ( 0.000000000000000000, -1.000000000000000000, -0.000000000000000000 ) ) ;
#54377 = CARTESIAN_POINT ( 'NONE',  ( 17.55505043854144276, 0.6250000000000001110, -25.00000000000000000 ) ) ;
#54378 = ADVANCED_FACE ( 'NONE', ( #4873 ), #26215, .T. ) ;
#54379 = EDGE_CURVE ( 'NONE', #11630, #25798, #27245, .T. ) ;
#54380 = CARTESIAN_POINT ( 'NONE',  ( 9.091120559621998609, -3.762710033898000184, 8.787827024292999667 ) ) ;
#54381 = DIRECTION ( 'NONE',  ( 1.000000000000000000, 0.000000000000000000, 0.000000000000000000 ) ) ;
#54383 = CARTESIAN_POINT ( 'NONE',  ( 12.80000000000000071, -43.96540072520999587, 14.96704326274999985 ) ) ;
#54382 = CARTESIAN_POINT ( 'NONE',  ( 9.753772138682000659, -4.476015718025199597, 8.687347221188998603 ) ) ;
#54384 = CARTESIAN_POINT ( 'NONE',  ( 10.17349413291699811, 5.162701151235999930, -6.969488574374499201 ) ) ;
#54385 = ADVANCED_FACE ( 'NONE', ( #60092 ), #6028, .F. ) ;
#54386 = CARTESIAN_POINT ( 'NONE',  ( 7.492075307187761268, 4.829186685176425797, -6.421019192411952403 ) ) ;
#54387 = CARTESIAN_POINT ( 'NONE',  ( 8.725683545309856015, 2.905353685799620500, -6.303952321520784885 ) ) ;
#54388 = CARTESIAN_POINT ( 'NONE',  ( 18.02507753857511474, -0.4124490627810481480, 12.69099791225215235 ) ) ;
#54389 = CARTESIAN_POINT ( 'NONE',  ( 11.10000000000000320, -5.584402864533258182, 7.269764875316957919 ) ) ;
#54390 = CARTESIAN_POINT ( 'NONE',  ( 18.02583793287565683, -2.911580782555497127, -12.34610277261805855 ) ) ;
#54391 = ORIENTED_EDGE ( 'NONE', *, *, #2991, .T. ) ;
#54393 = CARTESIAN_POINT ( 'NONE',  ( 9.136065740934069979, 5.315322084245146961, -7.853657639600751139 ) ) ;
#54392 = CARTESIAN_POINT ( 'NONE',  ( 8.545870559624999530, -3.856773448568000084, 5.521258396339000285 ) ) ;
#54394 = CARTESIAN_POINT ( 'NONE',  ( 8.365779719592000063, 2.949305648881000330, -8.659807625323999503 ) ) ;
#54395 =( BOUNDED_SURFACE ( )  B_SPLINE_SURFACE ( 3, 3, ( 
 ( #4815, #38012, #11102, #47138 ),
 ( #20905, #5511, #41885, #26852 ),
 ( #68439, #48165, #52372, #53753 ),
 ( #27190, #26157, #269, #31750 ) ),
 .UNSPECIFIED., .F., .F., .T. ) 
 B_SPLINE_SURFACE_WITH_KNOTS ( ( 4, 4 ),
 ( 4, 4 ),
 ( 0.000000000000000000, 1.000000000000000000 ),
 ( 0.000000000000000000, 1.000000000000000000 ),
 .UNSPECIFIED. ) 
 GEOMETRIC_REPRESENTATION_ITEM ( )  RATIONAL_B_SPLINE_SURFACE ( (
 ( 1.512182578520000042, 1.160176301760999840, 1.160176301760999840, 1.512182578520000042),
 ( 1.111288591041000196, 0.8526025270081000196, 0.8526025270081000196, 1.111288591041000196),
 ( 1.111288591041000196, 0.8526025270081000196, 0.8526025270081000196, 1.111288591041000196),
 ( 1.512182578520000042, 1.160176301760999840, 1.160176301760999840, 1.512182578520000042) ) ) 
 REPRESENTATION_ITEM ( '' )  SURFACE ( )  );
#54396 = FACE_OUTER_BOUND ( 'NONE', #50930, .T. ) ;
#54397 = CARTESIAN_POINT ( 'NONE',  ( 9.447288403127886980, -2.899999999999999911, 6.305985889523069154 ) ) ;
#54398 = CONICAL_SURFACE ( 'NONE', #24262, 11.34994642770999818, 0.7853934433896081480 ) ;
#54399 = CARTESIAN_POINT ( 'NONE',  ( 0.7162272458363000416, -2.757152670777000214, 2.469952924947999673 ) ) ;
#54400 = EDGE_CURVE ( 'NONE', #7379, #28950, #44063, .T. ) ;
#54401 = PRESENTATION_LAYER_ASSIGNMENT (  '', '', ( #30960 ) ) ;
#54402 = CARTESIAN_POINT ( 'NONE',  ( 10.44635971519499940, 4.459622816450200311, 8.264615166761799969 ) ) ;
#54403 = CARTESIAN_POINT ( 'NONE',  ( 10.06949528041000086, 4.910370880657999315, -8.649591080567999413 ) ) ;
#54404 = ORIENTED_EDGE ( 'NONE', *, *, #14492, .F. ) ;
#54405 = CARTESIAN_POINT ( 'NONE',  ( 12.10479047996948232, -0.1866745257715890227, -12.59862229962904223 ) ) ;
#54406 = CARTESIAN_POINT ( 'NONE',  ( 24.30001685126999789, 8.938702716825000394, -8.938676159935001309 ) ) ;
#54407 = CARTESIAN_POINT ( 'NONE',  ( 17.79586754331421972, 3.158948767300548965, -12.19758365745370021 ) ) ;
#54408 = CARTESIAN_POINT ( 'NONE',  ( 5.569720047906554505, 12.16229356903371794, 3.760137167885124754 ) ) ;
#54410 = CARTESIAN_POINT ( 'NONE',  ( 8.951357780412001475, 2.821863697211000055, 6.127145479358000024 ) ) ;
#54409 = VECTOR ( 'NONE', #50693, 1000.000000000000227 ) ;
#54411 = ORIENTED_EDGE ( 'NONE', *, *, #15312, .T. ) ;
#54412 = CARTESIAN_POINT ( 'NONE',  ( 6.687873758168000116, 0.03883618666160999766, -1.614257485795999925 ) ) ;
#54413 = CARTESIAN_POINT ( 'NONE',  ( 8.543670280408999673, 5.311932732455999506, -8.353077699453999472 ) ) ;
#54415 = CARTESIAN_POINT ( 'NONE',  ( 10.39709268726349300, 5.286023823538134714, 7.026709681657270501 ) ) ;
#54414 = CARTESIAN_POINT ( 'NONE',  ( 8.513685092916551511, -2.802204424339387767, 6.226699829290962995 ) ) ;
#54416 = AXIS2_PLACEMENT_3D ( 'NONE', #22394, #16456, #32216 ) ;
#54417 = CARTESIAN_POINT ( 'NONE',  ( 10.50145247700547557, -4.082536117276985621, -6.629783135293719099 ) ) ;
#54418 = VERTEX_POINT ( 'NONE', #57905 ) ;
#54419 = FACE_OUTER_BOUND ( 'NONE', #25744, .T. ) ;
#54420 = ORIENTED_EDGE ( 'NONE', *, *, #32993, .T. ) ;
#54421 = CARTESIAN_POINT ( 'NONE',  ( 12.75601781082312947, 1.760880198315114553, -12.47634966360018005 ) ) ;
#54422 = CARTESIAN_POINT ( 'NONE',  ( 25.29996559941400136, -2.596925179230000325, -11.35302181744000016 ) ) ;
#54423 = CARTESIAN_POINT ( 'NONE',  ( 17.78863088638136247, 0.6916885356983994981, -13.98290438115173906 ) ) ;
#54424 = EDGE_LOOP ( 'NONE', ( #40035, #53638, #56480 ) ) ;
#54425 = CARTESIAN_POINT ( 'NONE',  ( 10.43232984631212013, -4.711432589314514807, -9.126745072100195699 ) ) ;
#54426 = CARTESIAN_POINT ( 'NONE',  ( 17.60000002360358096, -11.94788428419862747, 3.252375034948150390 ) ) ;
#54427 = AXIS2_PLACEMENT_3D ( 'NONE', #44665, #43965, #49540 ) ;
#54428 = CARTESIAN_POINT ( 'NONE',  ( 10.29399293566599916, 4.546741702992100009, -8.170700474995699736 ) ) ;
#54429 = DIRECTION ( 'NONE',  ( 0.9999999999999682476, -2.518940175903920502E-07, 2.686332970438915230E-09 ) ) ;
#54430 = CARTESIAN_POINT ( 'NONE',  ( 10.91964694612699915, -5.186980343482999523, 7.026297514493899499 ) ) ;
#54431 = ORIENTED_EDGE ( 'NONE', *, *, #34097, .F. ) ;
#54432 = CARTESIAN_POINT ( 'NONE',  ( 8.192489158772998437, 2.550241116032999855, 7.666973618349000041 ) ) ;
#54433 = CARTESIAN_POINT ( 'NONE',  ( 10.98768503802999952, -8.067884818888000353, -6.818830313157000056 ) ) ;
#54434 = DIRECTION ( 'NONE',  ( 1.000000000000000000, 0.000000000000000000, 7.549516567300000767E-14 ) ) ;
#54435 = CARTESIAN_POINT ( 'NONE',  ( 15.98069952315600162, -9.346107076637000688, -8.395568570714997847 ) ) ;
#54436 = CARTESIAN_POINT ( 'NONE',  ( 11.07128326594000001, 5.551436772566000322, -5.077701490514000326 ) ) ;
#54437 = VERTEX_POINT ( 'NONE', #15599 ) ;
#54438 = CARTESIAN_POINT ( 'NONE',  ( 12.51634965191645499, -1.945578265428328457, -12.56358890505709880 ) ) ;
#54439 = CARTESIAN_POINT ( 'NONE',  ( 16.10004050617000004, -5.773856762095680217, -11.16084031980687108 ) ) ;
#54440 = DIRECTION ( 'NONE',  ( -0.000000000000000000, 0.6194815870790952861, 0.7850111867164476509 ) ) ;
#54441 = EDGE_CURVE ( 'NONE', #32174, #6933, #37949, .T. ) ;
#54442 = DIRECTION ( 'NONE',  ( 1.000000000000000000, 0.000000000000000000, 0.000000000000000000 ) ) ;
#54443 = CARTESIAN_POINT ( 'NONE',  ( 12.11816748453751913, -2.752694035764604141, -13.72673318081622718 ) ) ;
#54444 = EDGE_CURVE ( 'NONE', #61665, #41305, #14821, .T. ) ;
#54445 = CARTESIAN_POINT ( 'NONE',  ( 10.74795391537419853, -3.169881940022800215, -8.063786182297898009 ) ) ;
#54446 = CARTESIAN_POINT ( 'NONE',  ( 12.08055032392415207, -2.669683454855332094, 12.31540075205091966 ) ) ;
#54447 = CARTESIAN_POINT ( 'NONE',  ( 18.08807463888095057, -1.992345594299827161, 12.44148860874184592 ) ) ;
#54448 = ORIENTED_EDGE ( 'NONE', *, *, #14195, .T. ) ;
#54449 = CARTESIAN_POINT ( 'NONE',  ( 11.80233327354039830, -5.101536739857000846, -6.779499720266399798 ) ) ;
#54450 = ORIENTED_EDGE ( 'NONE', *, *, #6168, .F. ) ;
#54451 = B_SPLINE_CURVE_WITH_KNOTS ( 'NONE', 3,
 ( #21389, #759, #38866, #16489, #12292, #58797, #43420, #48998 ),
 .UNSPECIFIED., .F., .F.,
 ( 4, 2, 2, 4 ),
 ( 0.000000000000000000, 0.4999999999999953371, 0.7499999999999976685, 1.000000000000000000 ),
 .UNSPECIFIED. ) ;
#54452 = CARTESIAN_POINT ( 'NONE',  ( 11.80727443316700231, -12.22191286342000005, -1.956148154176999832 ) ) ;
#54453 = CARTESIAN_POINT ( 'NONE',  ( 9.793039158772000263, 5.817107086401000160, -6.945352709928000579 ) ) ;
#54454 = CARTESIAN_POINT ( 'NONE',  ( 9.882903428397000312, 4.314559027837000293, -9.161039561412001930 ) ) ;
#54455 = CARTESIAN_POINT ( 'NONE',  ( 10.62924380535000068, -3.609488729914999805, -5.855142811286000004 ) ) ;
#54456 = AXIS2_PLACEMENT_3D ( 'NONE', #27148, #31704, #21202 ) ;
#54457 = CARTESIAN_POINT ( 'NONE',  ( 11.04384236319999957, 7.001054331151000731, -5.879104662970000561 ) ) ;
#54458 = CARTESIAN_POINT ( 'NONE',  ( 5.500000000000000000, -12.43893545635000031, 2.828937028792000152 ) ) ;
#54459 = CARTESIAN_POINT ( 'NONE',  ( 8.720712484379999907, 3.780467314030099946, -8.340498368324299250 ) ) ;
#54460 = VERTEX_POINT ( 'NONE', #52654 ) ;
#54461 = AXIS2_PLACEMENT_3D ( 'NONE', #68993, #36493, #5365 ) ;
#54462 = FACE_OUTER_BOUND ( 'NONE', #26077, .T. ) ;
#54463 = CARTESIAN_POINT ( 'NONE',  ( 10.27815081430999911, 5.521603098753999461, 8.751228458888000716 ) ) ;
#54464 = FACE_OUTER_BOUND ( 'NONE', #28220, .T. ) ;
#54465 = CARTESIAN_POINT ( 'NONE',  ( 18.30003129334700063, -2.732683817159999862, 11.53064095410000078 ) ) ;
#54466 = CARTESIAN_POINT ( 'NONE',  ( 18.38722619340700248, 3.117741388420999904, -11.18549237633000004 ) ) ;
#54467 = VECTOR ( 'NONE', #57940, 1000.000000000000114 ) ;
#54468 = CARTESIAN_POINT ( 'NONE',  ( 11.65871932425156920, 3.852858594438699935, -8.492622906483498824 ) ) ;
#54469 = EDGE_CURVE ( 'NONE', #24573, #35849, #32415, .T. ) ;
#54470 = DIRECTION ( 'NONE',  ( 1.000000000000000000, 0.000000000000000000, 0.000000000000000000 ) ) ;
#54471 = CARTESIAN_POINT ( 'NONE',  ( 23.55359760295800342, -10.33014718151000189, -9.497754714104001295 ) ) ;
#54472 = CARTESIAN_POINT ( 'NONE',  ( 24.02992999001800101, -9.410060158574999889, 9.736248058902001290 ) ) ;
#54473 = CIRCLE ( 'NONE', #33274, 13.98989069973999477 ) ;
#54474 = CARTESIAN_POINT ( 'NONE',  ( 11.68610928851700237, -3.397019518052000198, 11.10441497445000003 ) ) ;
#54475 = ORIENTED_EDGE ( 'NONE', *, *, #33330, .F. ) ;
#54476 = CARTESIAN_POINT ( 'NONE',  ( 8.970860841232001448, 4.131080973160000447, -6.108642999115999395 ) ) ;
#54477 = CARTESIAN_POINT ( 'NONE',  ( 7.061283998474999990, -0.3468507372608000128, -1.324123422434000164 ) ) ;
#54478 = CARTESIAN_POINT ( 'NONE',  ( 18.09841665128858779, 2.190490658128017021, 13.73421521058127759 ) ) ;
#54479 = CARTESIAN_POINT ( 'NONE',  ( 11.09999999999999964, 5.299999999999999822, -5.160242713806000303 ) ) ;
#54480 = CARTESIAN_POINT ( 'NONE',  ( 11.52733460557258915, -3.793662715184400014, -8.761245990815998752 ) ) ;
#54481 = ORIENTED_EDGE ( 'NONE', *, *, #15162, .T. ) ;
#54482 = CARTESIAN_POINT ( 'NONE',  ( 24.56892813840100231, 3.303732449835000029, -12.00214075350999821 ) ) ;
#54483 = CARTESIAN_POINT ( 'NONE',  ( 7.410857780409000561, 2.302289264429000504, 6.875166305059000393 ) ) ;
#54484 = EDGE_CURVE ( 'NONE', #26882, #59889, #7175, .T. ) ;
#54486 = CARTESIAN_POINT ( 'NONE',  ( 11.45284386393252696, 4.902679577238613362, 7.824986766837089824 ) ) ;
#54485 = CARTESIAN_POINT ( 'NONE',  ( 9.649770280412001355, 4.042991257420999851, -5.768106221333000327 ) ) ;
#54487 = CARTESIAN_POINT ( 'NONE',  ( 10.81499708368651369, -2.650004840405617124, -7.499999822193714749 ) ) ;
#54488 = ORIENTED_EDGE ( 'NONE', *, *, #31012, .F. ) ;
#54489 = CARTESIAN_POINT ( 'NONE',  ( 10.39106065309000115, 4.025321035224999733, 9.261125884460000179 ) ) ;
#54490 = CARTESIAN_POINT ( 'NONE',  ( 18.23381869303825553, -2.775531333002572598, -13.72213247881302856 ) ) ;
#54491 = CARTESIAN_POINT ( 'NONE',  ( 10.30903300763299946, 4.597717337857299746, 6.873077781830399857 ) ) ;
#54492 = CARTESIAN_POINT ( 'NONE',  ( 10.09181272066999924, -2.440908155048000516, 7.817368209339999652 ) ) ;
#54493 = CARTESIAN_POINT ( 'NONE',  ( 7.654876518126000562, 2.928962009306002479, 6.518628166992000317 ) ) ;
#54494 = VERTEX_POINT ( 'NONE', #1939 ) ;
#54495 = CARTESIAN_POINT ( 'NONE',  ( 24.56351374471499938, 12.27674503263999917, -3.066186501856999591 ) ) ;
#54496 = B_SPLINE_CURVE_WITH_KNOTS ( 'NONE', 3,
 ( #15973, #48831, #58624, #4786, #42895, #939, #47455, #64201, #21222, #68760, #37645, #20880, #36966, #58280, #31722, #13167, #45321, #49512, #7556, #40080, #44975, #1978, #34141, #12462, #7216, #54417, #66627, #55808, #34496, #66279, #22595, #1626, #54761, #7909, #49169 ),
 .UNSPECIFIED., .F., .F.,
 ( 4, 1, 1, 1, 1, 1, 1, 1, 1, 1, 1, 1, 1, 1, 1, 1, 1, 1, 1, 1, 1, 1, 1, 1, 1, 1, 1, 1, 1, 1, 1, 1, 4 ),
 ( 0.000000000000000000, 0.02634724210002164710, 0.05799096732718461711, 0.08963469255434758365, 0.1212784177813103353, 0.1529221430084733158, 0.1845658682354360536, 0.2162095934625990201, 0.2478533186897620144, 0.2794970439167247522, 0.3111407691438877188, 0.3427844943710506853, 0.3744282195980134231, 0.4060719448251764452, 0.4377156700521391830, 0.4693593952793021495, 0.5010031205064651161, 0.5326468457334281315, 0.5642905709605910980, 0.5959342961875535583, 0.6275780214147167468, 0.6592217466418797134, 0.6908654718688422847, 0.7225091970960054732, 0.7541529223229680445, 0.7857966475501312331, 0.8174403727772941997, 0.8490840980042566599, 0.8807278232314198485, 0.9123715484585828150, 0.9440152736855453863, 0.9756589989127085749, 1.000000000000000000 ),
 .UNSPECIFIED. ) ;
#54498 = CARTESIAN_POINT ( 'NONE',  ( 10.66043185321000131, -2.315667072036000196, -7.431702410656999547 ) ) ;
#54497 = CARTESIAN_POINT ( 'NONE',  ( 12.03709034744600181, -11.69601057336999972, 4.586677359659000253 ) ) ;
#54499 = CARTESIAN_POINT ( 'NONE',  ( 7.749273516063919232, -5.411483081375795479, 8.518382685781334729 ) ) ;
#54500 = CARTESIAN_POINT ( 'NONE',  ( 11.14698053895999941, -5.129799765052999838, 5.886044098803999702 ) ) ;
#54501 = CARTESIAN_POINT ( 'NONE',  ( 10.14577693501968803, -2.689538146648244421, 7.995535515817278949 ) ) ;
#54502 = VERTEX_POINT ( 'NONE', #23258 ) ;
#54503 = CARTESIAN_POINT ( 'NONE',  ( 24.19055608310253191, -9.082956471743646176, 9.070969611592573756 ) ) ;
#54504 = B_SPLINE_CURVE_WITH_KNOTS ( 'NONE', 3,
 ( #18709, #18026, #13128, #60320, #7516, #23598, #44941, #49478, #55770, #7872, #40040, #61353, #29208, #8213 ),
 .UNSPECIFIED., .F., .F.,
 ( 4, 2, 2, 2, 2, 2, 4 ),
 ( 0.000000000000000000, 0.1249999999999997224, 0.2499999999999994449, 0.4999999999999991118, 0.7499999999999987788, 0.8749999999999993339, 1.000000000000000000 ),
 .UNSPECIFIED. ) ;
#54505 = CARTESIAN_POINT ( 'NONE',  ( 11.61302897915239818, -3.708003626182200030, 6.397263297997000109 ) ) ;
#54506 = FACE_OUTER_BOUND ( 'NONE', #65656, .T. ) ;
#54507 = CARTESIAN_POINT ( 'NONE',  ( 10.42380110216399913, 3.026453990125600235, 8.094557215852098864 ) ) ;
#54508 = ORIENTED_EDGE ( 'NONE', *, *, #45395, .T. ) ;
#54509 = B_SPLINE_CURVE_WITH_KNOTS ( 'NONE', 3,
 ( #52818, #68535, #5260, #41983 ),
 .UNSPECIFIED., .F., .F.,
 ( 4, 4 ),
 ( 0.000000000000000000, 1.000000000000000000 ),
 .UNSPECIFIED. ) ;
#54510 = CARTESIAN_POINT ( 'NONE',  ( 8.324914158772999784, 2.633142096252999664, -7.791134854666999843 ) ) ;
#54511 = AXIS2_PLACEMENT_3D ( 'NONE', #60236, #49052, #34020 ) ;
#54512 = DIRECTION ( 'NONE',  ( 1.000000000000000000, 0.000000000000000000, 0.000000000000000000 ) ) ;
#54513 = CARTESIAN_POINT ( 'NONE',  ( 12.36094932703097093, 3.049537035394463746, -12.22540636754321319 ) ) ;
#54514 = CARTESIAN_POINT ( 'NONE',  ( 11.81900581613029999, -3.249313226592100534, 7.017964743997199939 ) ) ;
#54515 = ORIENTED_EDGE ( 'NONE', *, *, #25137, .F. ) ;
#54516 = CARTESIAN_POINT ( 'NONE',  ( 23.56664676942400050, 2.935522432666999748, 13.67843419499999946 ) ) ;
#54517 = AXIS2_PLACEMENT_3D ( 'NONE', #47815, #24850, #10390 ) ;
#54518 = CARTESIAN_POINT ( 'NONE',  ( 4.400000000000000355, 0.000000000000000000, 0.000000000000000000 ) ) ;
#54519 = ORIENTED_EDGE ( 'NONE', *, *, #26611, .T. ) ;
#54520 = CARTESIAN_POINT ( 'NONE',  ( 23.89320776801300283, 12.21745654481001075, 3.256241354617000816 ) ) ;
#54521 = CARTESIAN_POINT ( 'NONE',  ( 5.669609839683792174, -0.1963495408493606265, -1.500000000000000222 ) ) ;
#54522 = ORIENTED_EDGE ( 'NONE', *, *, #58059, .T. ) ;
#54523 = CARTESIAN_POINT ( 'NONE',  ( 12.75685601902880073, -3.198499228556006990, -12.18727240180921179 ) ) ;
#54524 = CARTESIAN_POINT ( 'NONE',  ( 11.14179841651039915, 3.646693590264900031, 6.560784671286499226 ) ) ;
#54525 = CARTESIAN_POINT ( 'NONE',  ( 10.00190805961999807, -2.729654112791000120, -8.843024969850999284 ) ) ;
#54526 = CARTESIAN_POINT ( 'NONE',  ( 10.64601354018249957, 4.999583552997728830, 8.268183399968640046 ) ) ;
#54527 = CARTESIAN_POINT ( 'NONE',  ( 18.39711792013700276, -11.90291294758000085, 3.720230460285999907 ) ) ;
#54528 = EDGE_CURVE ( 'NONE', #8090, #31317, #34893, .T. ) ;
#54529 = CARTESIAN_POINT ( 'NONE',  ( 12.79999999038796510, 11.45060587895086002, -4.713120762395663910 ) ) ;
#54530 = CARTESIAN_POINT ( 'NONE',  ( 13.78326532032400031, 9.295717737520000412, 8.172239456948000580 ) ) ;
#54531 = EDGE_CURVE ( 'NONE', #52043, #51187, #34032, .T. ) ;
#54532 = CARTESIAN_POINT ( 'NONE',  ( 17.86819591275963148, -0.5409888710114163501, -12.68448745112149645 ) ) ;
#54533 = CARTESIAN_POINT ( 'NONE',  ( 12.18822406274264658, 2.601257609780446067, -12.42743042557257915 ) ) ;
#54534 = CARTESIAN_POINT ( 'NONE',  ( 11.50271932425157040, -4.187398418774900044, -8.764198628556998827 ) ) ;
#54535 = EDGE_CURVE ( 'NONE', #6526, #10927, #4036, .T. ) ;
#54536 = EDGE_CURVE ( 'NONE', #3005, #25668, #56551, .T. ) ;
#54537 = CARTESIAN_POINT ( 'NONE',  ( 8.508079719592000600, 2.202812441249000219, 7.706988150133999405 ) ) ;
#54538 = ORIENTED_EDGE ( 'NONE', *, *, #43349, .T. ) ;
#54539 = FILL_AREA_STYLE ('',( #12931 ) ) ;
#54540 = DIRECTION ( 'NONE',  ( 0.000000000000000000, -1.000000000000000000, 0.000000000000000000 ) ) ;
#54541 = CARTESIAN_POINT ( 'NONE',  ( 7.131839088562530016, 3.481695193657420084, 8.754754956630815599 ) ) ;
#54542 = CARTESIAN_POINT ( 'NONE',  ( 11.60578299225600141, 12.22760809526000081, 1.919009911369000010 ) ) ;
#54543 = CARTESIAN_POINT ( 'NONE',  ( 17.98055108453612760, 1.897673117161885248, 12.45627908894455338 ) ) ;
#54544 = CARTESIAN_POINT ( 'NONE',  ( 13.00000000009400303, 11.69118001589999878, 1.923222888683999932 ) ) ;
#54545 = CARTESIAN_POINT ( 'NONE',  ( 9.442843574488000158, 2.691255504502000129, 6.269523028052000235 ) ) ;
#54546 = CARTESIAN_POINT ( 'NONE',  ( 9.676241837494625742, -4.657637647145090654, 6.922899494040819945 ) ) ;
#54547 = CARTESIAN_POINT ( 'NONE',  ( 8.741501215035997419, 3.771222299067000350, 6.624106355763400344 ) ) ;
#54548 = VERTEX_POINT ( 'NONE', #66929 ) ;
#54549 = CARTESIAN_POINT ( 'NONE',  ( 12.11326330726104139, -2.264210275637939418, 12.39489744172470687 ) ) ;
#54550 = CARTESIAN_POINT ( 'NONE',  ( 9.150442991499998513, -4.071878040089889517, -6.360452723514999462 ) ) ;
#54551 = FACE_OUTER_BOUND ( 'NONE', #27570, .T. ) ;
#54552 = EDGE_CURVE ( 'NONE', #56890, #57674, #29560, .T. ) ;
#54553 = CARTESIAN_POINT ( 'NONE',  ( 10.44080359545000114, -5.435731278187999393, 7.303630150377999009 ) ) ;
#54554 = B_SPLINE_CURVE_WITH_KNOTS ( 'NONE', 3,
 ( #33536, #54855, #1368, #50988 ),
 .UNSPECIFIED., .F., .F.,
 ( 4, 4 ),
 ( 0.000000000000000000, 1.000000000000000000 ),
 .UNSPECIFIED. ) ;
#54555 = CARTESIAN_POINT ( 'NONE',  ( 10.21462282008599942, 4.523146351753199568, -8.343818446627699004 ) ) ;
#54556 = CARTESIAN_POINT ( 'NONE',  ( 12.80505043854144276, -0.7192913403693028673, 12.57945229203838444 ) ) ;
#54557 = CARTESIAN_POINT ( 'NONE',  ( 9.433107780409999421, 4.954905351382000944, 8.825777580285999235 ) ) ;
#54558 = DIRECTION ( 'NONE',  ( -0.7071067811865474617, -0.7071067811865474617, -7.650295924916503855E-09 ) ) ;
#54559 = AXIS2_PLACEMENT_3D ( 'NONE', #35404, #3569, #24903 ) ;
#54560 = CARTESIAN_POINT ( 'NONE',  ( 12.66194203315988709, 3.108482559131307443, 12.28874639354599196 ) ) ;
#54561 = ORIENTED_EDGE ( 'NONE', *, *, #19798, .F. ) ;
#54562 = CARTESIAN_POINT ( 'NONE',  ( 8.239948341229000661, 2.735218126362000124, 6.771983639047999937 ) ) ;
#54563 = CARTESIAN_POINT ( 'NONE',  ( 11.01456785386839954, 3.053605396817899997, -8.136888821800198457 ) ) ;
#54564 = CARTESIAN_POINT ( 'NONE',  ( 18.24150829797649109, -0.2316996085785957560, 12.59787430930301433 ) ) ;
#54565 = DIRECTION ( 'NONE',  ( 0.000000000000000000, 0.000000000000000000, 1.000000000000000000 ) ) ;
#54567 = LINE ( 'NONE', #11556, #60746 ) ;
#54566 = CARTESIAN_POINT ( 'NONE',  ( 8.298061260823001106, 5.118905885020002877, 6.382684838875003486 ) ) ;
#54568 = CARTESIAN_POINT ( 'NONE',  ( 11.17056785386839834, -4.718624889240500053, -7.983608166707499620 ) ) ;
#54569 = DIRECTION ( 'NONE',  ( 0.000000000000000000, 0.000000000000000000, -1.000000000000000000 ) ) ;
#54570 = EDGE_LOOP ( 'NONE', ( #43812, #22061, #8484, #30676 ) ) ;
#54571 = CARTESIAN_POINT ( 'NONE',  ( 2.211430836446000026, -0.2901351235585999944, -3.413359411422000278 ) ) ;
#54572 = DIRECTION ( 'NONE',  ( 1.000000000000000000, 0.000000000000000000, 7.697546303983999388E-14 ) ) ;
#54573 = ADVANCED_FACE ( 'NONE', ( #7870 ), #46651, .T. ) ;
#54574 = CARTESIAN_POINT ( 'NONE',  ( 11.00000000000000000, -3.008232475376599879, -7.174999999999999822 ) ) ;
#54575 = CARTESIAN_POINT ( 'NONE',  ( 9.298392757686999133, 4.585219941293100732, 6.860292594369099106 ) ) ;
#54576 = CARTESIAN_POINT ( 'NONE',  ( 10.01835931249159906, 5.126777126174925314, -6.752018918854003182 ) ) ;
#54577 = EDGE_CURVE ( 'NONE', #58602, #6078, #26602, .T. ) ;
#54578 = CARTESIAN_POINT ( 'NONE',  ( 12.23619509270001160, -2.970722878206530471, 13.68118758531137757 ) ) ;
#54579 = CARTESIAN_POINT ( 'NONE',  ( 10.84393020684900044, -5.250000000000000000, 7.500000000000000000 ) ) ;
#54580 = CARTESIAN_POINT ( 'NONE',  ( 18.90826270587400160, 11.65000000000000036, 0.000000000000000000 ) ) ;
#54581 = CARTESIAN_POINT ( 'NONE',  ( 12.96900185986900134, -12.22197440418000092, -1.955830866674999946 ) ) ;
#54582 = ORIENTED_EDGE ( 'NONE', *, *, #12901, .T. ) ;
#54583 = AXIS2_PLACEMENT_3D ( 'NONE', #47411, #46725, #15248 ) ;
#54584 = DIRECTION ( 'NONE',  ( 0.000000000000000000, 1.000000000000000000, 0.000000000000000000 ) ) ;
#54585 = CARTESIAN_POINT ( 'NONE',  ( 10.45746213570999927, 5.100000000000000533, -6.571291218949999902 ) ) ;
#54586 = CARTESIAN_POINT ( 'NONE',  ( 0.7514734890462999584, -3.558193753575999985, 1.211459191638999844 ) ) ;
#54587 = CARTESIAN_POINT ( 'NONE',  ( 9.972537864286000087, -2.899999999999999911, -6.571291218949999902 ) ) ;
#54588 = CARTESIAN_POINT ( 'NONE',  ( 17.98541303540591940, 2.046657644932490250, -12.54573712159720777 ) ) ;
#54589 = CARTESIAN_POINT ( 'NONE',  ( 9.716839207166817260, -3.231820996160967407, 8.499566091636109988 ) ) ;
#54590 = CARTESIAN_POINT ( 'NONE',  ( 10.87518447801629939, 4.865987311498500389, 7.519093628927509876 ) ) ;
#54592 = DIRECTION ( 'NONE',  ( 1.000000000000000000, 0.000000000000000000, 0.000000000000000000 ) ) ;
#54591 = B_SPLINE_CURVE_WITH_KNOTS ( 'NONE', 3,
 ( #24423, #1112, #22425, #29689 ),
 .UNSPECIFIED., .F., .F.,
 ( 4, 4 ),
 ( 0.000000000000000000, 1.000000000000000000 ),
 .UNSPECIFIED. ) ;
#54593 = CARTESIAN_POINT ( 'NONE',  ( 11.03905685320999908, -3.855072944465999907, -9.179476187420998912 ) ) ;
#54594 = FACE_OUTER_BOUND ( 'NONE', #45527, .T. ) ;
#54595 = CARTESIAN_POINT ( 'NONE',  ( 10.90000004630000063, 9.856474695503001371, 5.627825000517000298 ) ) ;
#54596 = DIRECTION ( 'NONE',  ( 1.000000000000000000, 0.000000000000000000, 0.000000000000000000 ) ) ;
#54597 = ORIENTED_EDGE ( 'NONE', *, *, #43652, .F. ) ;
#54598 = CARTESIAN_POINT ( 'NONE',  ( 8.546960841229999772, 2.724453559418999582, -8.908010318766001134 ) ) ;
#54599 = EDGE_LOOP ( 'NONE', ( #9004, #54345, #56807, #6939 ) ) ;
#54600 = CARTESIAN_POINT ( 'NONE',  ( 18.17895306041987880, -2.542296241241987165, 13.66441818551904852 ) ) ;
#54601 = CARTESIAN_POINT ( 'NONE',  ( 10.59195391537400077, -2.942766577210000012, -8.218034727798299244 ) ) ;
#54602 = ORIENTED_EDGE ( 'NONE', *, *, #66716, .T. ) ;
#54603 = CARTESIAN_POINT ( 'NONE',  ( 11.05946005378019947, 5.036385109519999403, 8.053412743695298914 ) ) ;
#54604 = LINE ( 'NONE', #33289, #26025 ) ;
#54605 = CARTESIAN_POINT ( 'NONE',  ( 23.72388938462524877, 3.247317956399220051, -13.28503071072038288 ) ) ;
#54606 = CARTESIAN_POINT ( 'NONE',  ( 9.347254965556000883, 4.028327103212000715, 9.469449669541999626 ) ) ;
#54607 = CARTESIAN_POINT ( 'NONE',  ( 10.90000000000000036, -1.433333333332999837, 10.65401593558000037 ) ) ;
#54608 = CARTESIAN_POINT ( 'NONE',  ( 17.80000000005199823, -3.345268251980999974, -11.86064071431999878 ) ) ;
#54609 = CARTESIAN_POINT ( 'NONE',  ( 11.42387073792000152, 3.325692027085000113, -11.41083924281000073 ) ) ;
#54610 = AXIS2_PLACEMENT_3D ( 'NONE', #52429, #57669, #10464 ) ;
#54611 = CARTESIAN_POINT ( 'NONE',  ( 11.19120431613999855, -3.005395205805000192, -6.023553580263000029 ) ) ;
#54612 = CARTESIAN_POINT ( 'NONE',  ( 10.08492069073747466, -4.544768192061120260, -8.875938726815583379 ) ) ;
#54613 = ORIENTED_EDGE ( 'NONE', *, *, #61960, .T. ) ;
#54614 = EDGE_CURVE ( 'NONE', #4517, #56617, #46777, .T. ) ;
#54615 = EDGE_CURVE ( 'NONE', #59469, #33299, #48256, .T. ) ;
#54616 = CARTESIAN_POINT ( 'NONE',  ( 10.71937333909091450, -2.934588105059417362, -5.069903530434454630 ) ) ;
#54617 = ORIENTED_EDGE ( 'NONE', *, *, #65099, .T. ) ;
#54618 = CARTESIAN_POINT ( 'NONE',  ( 4.600000207916515649, 0.000000000000000000, -9.325873406851000657E-14 ) ) ;
#54619 =( NAMED_UNIT ( * ) SI_UNIT ( $, .STERADIAN. ) SOLID_ANGLE_UNIT ( ) );
#54620 = ORIENTED_EDGE ( 'NONE', *, *, #35220, .F. ) ;
#54621 = PLANE ( 'NONE',  #62644 ) ;
#54622 = CARTESIAN_POINT ( 'NONE',  ( 17.33333333083533390, 3.216308279608388609, 11.40341444610950461 ) ) ;
#54623 = CYLINDRICAL_SURFACE ( 'NONE', #60874, 1.350000000000000089 ) ;
#54624 = CARTESIAN_POINT ( 'NONE',  ( 12.57340716663134295, 1.919420395509098043, 13.77954053360031850 ) ) ;
#54625 = B_SPLINE_SURFACE_WITH_KNOTS ( 'NONE', 3, 3, ( 
 ( #32831, #28275, #11490, #64967 ),
 ( #21983, #6244, #48567, #65669 ),
 ( #59737, #48912, #12197, #11838 ),
 ( #1703, #33178, #54495, #37725 ),
 ( #27937, #39110, #33525, #12541 ),
 ( #43324, #64628, #6596, #44370 ) ),
 .UNSPECIFIED., .F., .F., .F.,
 ( 4, 1, 1, 4 ),
 ( 4, 4 ),
 ( 0.1811037619699999990, 0.3333333333333000081, 0.6666666666667000474, 0.8725156331704999602 ),
 ( -0.1256563615239000009, 1.125656361510000147 ),
 .UNSPECIFIED. ) ;
#54626 = CARTESIAN_POINT ( 'NONE',  ( 17.63816080826980226, -1.880463790428644533, 12.57456020225082050 ) ) ;
#54627 = CARTESIAN_POINT ( 'NONE',  ( 23.56666365135700403, -8.694246338441999455, -8.392498551189996547 ) ) ;
#54628 = CARTESIAN_POINT ( 'NONE',  ( 12.42411034028606309, 0.4959091552601215813, 13.88809952003718173 ) ) ;
#54629 = ORIENTED_EDGE ( 'NONE', *, *, #10000, .T. ) ;
#54630 = CARTESIAN_POINT ( 'NONE',  ( 7.223909439180999037, 5.321245676936000812, -7.068438969505000280 ) ) ;
#54631 = CARTESIAN_POINT ( 'NONE',  ( 10.67008478491585066, -2.650321919618085609, 7.583525828155321058 ) ) ;
#54632 = ADVANCED_FACE ( 'NONE', ( #51879 ), #42188, .F. ) ;
#54633 = CARTESIAN_POINT ( 'NONE',  ( 10.08809113605762597, 3.189914598996232975, 7.830596297620237678 ) ) ;
#54634 = CARTESIAN_POINT ( 'NONE',  ( 4.769414598756999801, -0.6079694192054000412, -1.351744651493000049 ) ) ;
#54635 = B_SPLINE_CURVE_WITH_KNOTS ( 'NONE', 3,
 ( #26950, #16783, #5951, #54191 ),
 .UNSPECIFIED., .F., .F.,
 ( 4, 4 ),
 ( 0.000000000000000000, 1.000000000000000000 ),
 .UNSPECIFIED. ) ;
#54636 = B_SPLINE_SURFACE_WITH_KNOTS ( 'NONE', 3, 3, ( 
 ( #34547, #55859, #3052, #47782, #14922, #15613, #10361, #32046, #47087, #20855, #41491, #21196, #42871, #26450, #42527, #41834, #69091, #36245, #51970 ),
 ( #63836, #36592, #62803, #42191, #15950, #10701, #57564, #4073, #31015, #63143, #57919, #37280, #63493, #30662, #36943, #31696, #53362, #15268, #9665 ),
 ( #9319, #10015, #68388, #58257, #52325, #53018, #5114, #26801, #58600, #5465, #20508, #64179, #4420, #25758, #48115, #25410, #16293, #218, #21536 ),
 ( #4762, #37616, #31353, #26104, #52666, #47429, #46745, #68050, #20164, #68738, #6141, #59980, #49144, #5798, #43913, #58948, #28173, #17688, #33770 ) ),
 .UNSPECIFIED., .F., .F., .F.,
 ( 4, 4 ),
 ( 4, 1, 1, 1, 1, 1, 1, 1, 1, 1, 1, 1, 1, 1, 1, 1, 4 ),
 ( -0.02636945251836000231, 1.026369452518000047 ),
 ( 0.6640607743075999103, 0.6854686661408999626, 0.7068765579742000149, 0.7282844498075999873, 0.7496923416409000396, 0.7711002334743000119, 0.7925081253075999532, 0.8139160171409000055, 0.8353239089742999779, 0.8567318008076000302, 0.8781396926410000026, 0.8995475844743000549, 0.9209554763077000272, 0.9423633681409999685, 0.9637712599743000208, 0.9851791518076999932, 1.006587043640999823 ),
 .UNSPECIFIED. ) ;
#54637 = CARTESIAN_POINT ( 'NONE',  ( 9.088029719595001055, 2.881930053949999682, -8.823338183322999129 ) ) ;
#54638 = CARTESIAN_POINT ( 'NONE',  ( 25.29986325275000070, 2.078227429405999693, 11.31065739696999906 ) ) ;
#54639 = CARTESIAN_POINT ( 'NONE',  ( 10.35427551197999918, -4.879111827962000270, -8.944027914303999793 ) ) ;
#54640 = B_SPLINE_CURVE_WITH_KNOTS ( 'NONE', 3,
 ( #44224, #38970, #33726, #55043, #44574, #28838 ),
 .UNSPECIFIED., .F., .F.,
 ( 4, 2, 4 ),
 ( 0.000000000000000000, 0.5000000000000000000, 1.000000000000000000 ),
 .UNSPECIFIED. ) ;
#54641 = CARTESIAN_POINT ( 'NONE',  ( 10.17500046684972936, -2.650307855384914202, 7.500001770945068813 ) ) ;
#54642 = CARTESIAN_POINT ( 'NONE',  ( 24.32155075627094831, 3.683040026163987957, 12.56970858062822849 ) ) ;
#54643 = CARTESIAN_POINT ( 'NONE',  ( 24.30001680216799897, -3.271769318036999774, 12.21048166890999909 ) ) ;
#54644 = CARTESIAN_POINT ( 'NONE',  ( 17.74431590772262979, -1.811500042934492072, 13.88231098337033131 ) ) ;
#54645 = DIRECTION ( 'NONE',  ( -1.000000000000000000, 0.000000000000000000, 0.000000000000000000 ) ) ;
#54646 = DIRECTION ( 'NONE',  ( 1.000000000000000000, 0.000000000000000000, 0.000000000000000000 ) ) ;
#54647 = CARTESIAN_POINT ( 'NONE',  ( 11.68788784977535933, 3.014014167207800465, -7.443657794094239222 ) ) ;
#54648 = CARTESIAN_POINT ( 'NONE',  ( 8.672151519676999598, 4.021721698617580110, -8.504175633905001419 ) ) ;
#54650 = PLANE ( 'NONE',  #51810 ) ;
#54649 = CARTESIAN_POINT ( 'NONE',  ( 10.63425461470299993, -4.840245908677600184, 7.286236678332599581 ) ) ;
#54651 = DIRECTION ( 'NONE',  ( 0.000000000000000000, -1.000000000000000000, 0.000000000000000000 ) ) ;
#54652 = ORIENTED_EDGE ( 'NONE', *, *, #1845, .T. ) ;
#54653 = CARTESIAN_POINT ( 'NONE',  ( 10.44125056272499918, 5.033400911533000510, 7.484684486284700178 ) ) ;
#54654 = CARTESIAN_POINT ( 'NONE',  ( 9.566960887370999700, -5.215923019114000247, 6.177729435798999802 ) ) ;
#54655 = CARTESIAN_POINT ( 'NONE',  ( 10.13827973160999818, 4.102460098134500299, 8.637205511891998810 ) ) ;
#54656 = CARTESIAN_POINT ( 'NONE',  ( 9.632166486775625813, 3.137137839323436594, -7.644917771834661480 ) ) ;
#54657 = CARTESIAN_POINT ( 'NONE',  ( 11.05639424537999993, -5.030223832177999732, 6.028291574375000295 ) ) ;
#54658 = EDGE_CURVE ( 'NONE', #61556, #30450, #24469, .T. ) ;
#54659 = CARTESIAN_POINT ( 'NONE',  ( 13.50003721581400029, 9.159934378815998812, 7.517910889891000537 ) ) ;
#54660 = CARTESIAN_POINT ( 'NONE',  ( 9.099999931440999390, 5.064317881551000156, -8.155535999783198875 ) ) ;
#54661 = ORIENTED_EDGE ( 'NONE', *, *, #22950, .T. ) ;
#54662 = CARTESIAN_POINT ( 'NONE',  ( 9.710646554150999421, -3.513729974241599940, -8.378853663802400931 ) ) ;
#54663 = CARTESIAN_POINT ( 'NONE',  ( 7.100000000000000533, 0.000000000000000000, 0.000000000000000000 ) ) ;
#54664 = CARTESIAN_POINT ( 'NONE',  ( 6.405791561646000609, 1.411445953971000034, -0.4053984660343999957 ) ) ;
#54665 = CARTESIAN_POINT ( 'NONE',  ( 6.999998782146999332, 11.95749337870000062, 3.642574926947999892 ) ) ;
#54666 = CARTESIAN_POINT ( 'NONE',  ( 10.94076550314999885, 5.140765503144999471, -6.571291218949999902 ) ) ;
#54667 = CARTESIAN_POINT ( 'NONE',  ( 24.44496351116800170, 3.224881296174999967, 12.03535797436000010 ) ) ;
#54668 = CARTESIAN_POINT ( 'NONE',  ( 11.21564426047340035, 4.539962866738299851, -8.345807871442598724 ) ) ;
#54669 = CARTESIAN_POINT ( 'NONE',  ( 7.770167153117901293, -2.851532783649957548, 6.786996034065015948 ) ) ;
#54670 = DIRECTION ( 'NONE',  ( -0.7071068207016518725, 0.000000000000000000, -0.7071067416714409415 ) ) ;
#54671 = CARTESIAN_POINT ( 'NONE',  ( 12.61270316626370125, 1.780234759031155134, 12.47365767676520854 ) ) ;
#54672 = ORIENTED_EDGE ( 'NONE', *, *, #55712, .T. ) ;
#54673 = CARTESIAN_POINT ( 'NONE',  ( 25.59037099084400069, -11.08966619523999952, -3.240309866392999893 ) ) ;
#54674 = CARTESIAN_POINT ( 'NONE',  ( 12.11457335221577303, -0.2229649748661372555, -13.99822903660538564 ) ) ;
#54675 = DIRECTION ( 'NONE',  ( 0.000000000000000000, 1.000000000000000000, 0.000000000000000000 ) ) ;
#54676 = CARTESIAN_POINT ( 'NONE',  ( 9.928197172112565028, -5.125396288433639036, 6.749639981095324259 ) ) ;
#54677 = VECTOR ( 'NONE', #31897, 1000.000000000000114 ) ;
#54678 = CARTESIAN_POINT ( 'NONE',  ( 13.69586690835513565, -11.42311322218530556, -2.288407577486363920 ) ) ;
#54679 = CARTESIAN_POINT ( 'NONE',  ( 10.49640421544308211, 5.348966112464498934, 7.853238477522235250 ) ) ;
#54680 = CARTESIAN_POINT ( 'NONE',  ( 13.68724299200000161, 12.36060503258000054, 2.247042498203000171 ) ) ;
#54681 = ORIENTED_EDGE ( 'NONE', *, *, #36607, .F. ) ;
#54682 = FACE_OUTER_BOUND ( 'NONE', #62362, .T. ) ;
#54683 = CARTESIAN_POINT ( 'NONE',  ( 18.12605992003768307, 2.245077608621426357, -13.72424617901693544 ) ) ;
#54684 = VERTEX_POINT ( 'NONE', #62376 ) ;
#54685 = DIRECTION ( 'NONE',  ( 1.000000000000000000, 0.000000000000000000, 0.000000000000000000 ) ) ;
#54686 = CARTESIAN_POINT ( 'NONE',  ( 9.294724726289000927, -4.148132978932999926, 9.337467253566000380 ) ) ;
#54687 = CARTESIAN_POINT ( 'NONE',  ( 9.700639158771000581, 4.262870449202000422, -8.811513791423999820 ) ) ;
#54688 = CARTESIAN_POINT ( 'NONE',  ( 6.553816671982000130, -1.199981415667000118, 0.9000247785775999931 ) ) ;
#54689 = CARTESIAN_POINT ( 'NONE',  ( 8.766851002546001581, 2.832432432432000269, 6.822293592207000934 ) ) ;
#54690 = CARTESIAN_POINT ( 'NONE',  ( 18.18005043855006875, 0.04052604707540623935, -12.70000016496744522 ) ) ;
#54691 = DIRECTION ( 'NONE',  ( -1.000000000000000000, 0.000000000000000000, 0.000000000000000000 ) ) ;
#54692 = CARTESIAN_POINT ( 'NONE',  ( 4.909193173016666911, 0.3926218265389159745, 1.460959015002474493 ) ) ;
#54693 = ORIENTED_EDGE ( 'NONE', *, *, #30875, .T. ) ;
#54694 = CARTESIAN_POINT ( 'NONE',  ( 10.97865453029000093, -5.273142482194999481, 7.958032781726000593 ) ) ;
#54695 = EDGE_CURVE ( 'NONE', #51171, #3171, #65713, .T. ) ;
#54696 = EDGE_CURVE ( 'NONE', #26192, #60622, #37838, .T. ) ;
#54697 = CARTESIAN_POINT ( 'NONE',  ( 18.16759718505687005, -2.624144390823405892, -13.64629239165651953 ) ) ;
#54698 = CARTESIAN_POINT ( 'NONE',  ( 25.55274092379240258, 8.264541415825529924, -8.081433428414696252 ) ) ;
#54699 = ORIENTED_EDGE ( 'NONE', *, *, #63956, .F. ) ;
#54700 = CARTESIAN_POINT ( 'NONE',  ( 13.69997185827400266, 11.40547114375999982, 2.374390024598000082 ) ) ;
#54701 = CARTESIAN_POINT ( 'NONE',  ( 10.76587944038000089, -3.166536971515000243, -8.574494061818999313 ) ) ;
#54702 = EDGE_LOOP ( 'NONE', ( #41750, #2689, #48848, #43915, #6437, #43526, #6855, #7844, #35208 ) ) ;
#54703 = CARTESIAN_POINT ( 'NONE',  ( 8.950772138681999834, 3.626242194157900389, 8.432280753260499750 ) ) ;
#54704 = CARTESIAN_POINT ( 'NONE',  ( 18.08635919897133704, -2.970004615628412559, -12.24496439055023522 ) ) ;
#54705 = CARTESIAN_POINT ( 'NONE',  ( 8.005461299830001209, 5.128003005022999439, -6.747396629211001695 ) ) ;
#54706 = CARTESIAN_POINT ( 'NONE',  ( 16.13732479921000262, 3.901986904155000158, 11.94169104666999992 ) ) ;
#54707 = PLANE ( 'NONE',  #12864 ) ;
#54708 = B_SPLINE_CURVE_WITH_KNOTS ( 'NONE', 3,
 ( #47216, #26235, #58727, #5580, #15741, #52102, #14712, #67837 ),
 .UNSPECIFIED., .F., .F.,
 ( 4, 1, 1, 1, 1, 4 ),
 ( 0.000000000000000000, 0.2000000000000000111, 0.4000000000000000222, 0.5999999999999999778, 0.8000000000000000444, 1.000000000000000000 ),
 .UNSPECIFIED. ) ;
#54709 = CARTESIAN_POINT ( 'NONE',  ( 9.889963142879999225, 4.848366390061300102, 7.678836273503299559 ) ) ;
#54710 = FACE_OUTER_BOUND ( 'NONE', #5700, .T. ) ;
#54711 = ORIENTED_EDGE ( 'NONE', *, *, #16561, .F. ) ;
#54712 = CARTESIAN_POINT ( 'NONE',  ( 8.229423500915721945, -4.864029983609895247, 6.209053182952776417 ) ) ;
#54713 = CARTESIAN_POINT ( 'NONE',  ( 10.18308278041000037, 2.953582937013000009, -8.606284720264998356 ) ) ;
#54714 = ADVANCED_FACE ( 'NONE', ( #34454 ), #29206, .F. ) ;
#54715 = DIRECTION ( 'NONE',  ( 0.000000000000000000, -0.1807154286440003366, -0.9835354258236024272 ) ) ;
#54716 = CARTESIAN_POINT ( 'NONE',  ( 12.19422188688372266, 2.632730885462788883, -13.64441700900758292 ) ) ;
#54717 = CARTESIAN_POINT ( 'NONE',  ( 11.30226354018299872, -5.092232985442821658, 8.129523725463625894 ) ) ;
#54718 = EDGE_CURVE ( 'NONE', #24435, #11483, #49866, .T. ) ;
#54719 = CARTESIAN_POINT ( 'NONE',  ( 9.905786073958001481, -2.698967003257000119, 8.979227319929000473 ) ) ;
#54720 = CARTESIAN_POINT ( 'NONE',  ( 18.26152657770007082, -0.1657344298535245175, 13.99903850390422910 ) ) ;
#54721 = CARTESIAN_POINT ( 'NONE',  ( 25.20468240883799993, -2.650152599392000319, 11.40088862747000142 ) ) ;
#54722 = VERTEX_POINT ( 'NONE', #24820 ) ;
#54723 = ORIENTED_EDGE ( 'NONE', *, *, #56776, .T. ) ;
#54724 = B_SPLINE_CURVE_WITH_KNOTS ( 'NONE', 3,
 ( #61001, #29200, #18360, #46302 ),
 .UNSPECIFIED., .F., .F.,
 ( 4, 4 ),
 ( 0.000000000000000000, 1.000000000000000000 ),
 .UNSPECIFIED. ) ;
#54725 = CARTESIAN_POINT ( 'NONE',  ( 9.494689158774999527, 2.824732249080000202, -8.992748220058999209 ) ) ;
#54726 = CARTESIAN_POINT ( 'NONE',  ( 12.21279768065092952, -0.1999278271778355542, 13.89806912752932710 ) ) ;
#54727 = CARTESIAN_POINT ( 'NONE',  ( 12.46489557886510191, -0.5244061151917449592, -13.88668399598972947 ) ) ;
#54728 = CARTESIAN_POINT ( 'NONE',  ( 9.648858509738902356, -2.900412407185302577, -6.176298919794867004 ) ) ;
#54729 = CARTESIAN_POINT ( 'NONE',  ( 4.599999651764306030, -13.27499965161999818, 2.617290972024999914E-09 ) ) ;
#54730 = CARTESIAN_POINT ( 'NONE',  ( 8.834370559623998531, -4.141908960411000429, 6.047561724438000219 ) ) ;
#54732 = TOROIDAL_SURFACE ( 'NONE', #36864, 1.649999999999999911, 0.5000000000000000000 ) ;
#54731 = CARTESIAN_POINT ( 'NONE',  ( 25.46373024410000241, -11.23407150414000100, 3.161076981347000103 ) ) ;
#54734 = CARTESIAN_POINT ( 'NONE',  ( 11.12483846379999974, -5.434435013714999485, 5.164704272902999271 ) ) ;
#54733 = CARTESIAN_POINT ( 'NONE',  ( 10.69095058442700008, -3.492264136285500253, 8.674133161175999973 ) ) ;
#54735 = CARTESIAN_POINT ( 'NONE',  ( 10.37041638348499895, 2.758294858530000226, -7.197535585171899619 ) ) ;
#54736 = B_SPLINE_CURVE_WITH_KNOTS ( 'NONE', 3,
 ( #59757, #23042, #33197, #54516 ),
 .UNSPECIFIED., .F., .F.,
 ( 4, 4 ),
 ( 0.000000000000000000, 1.000000000000000000 ),
 .UNSPECIFIED. ) ;
#54737 = CARTESIAN_POINT ( 'NONE',  ( 24.56351374471499938, -8.793767919668001198, -9.098879823118998900 ) ) ;
#54738 = CARTESIAN_POINT ( 'NONE',  ( 8.585340200126335475, 5.100000000000000533, -6.496871349812457730 ) ) ;
#54739 = CARTESIAN_POINT ( 'NONE',  ( 17.98240372392063335, -0.4561785182478259038, 12.68897339690746762 ) ) ;
#54740 = CARTESIAN_POINT ( 'NONE',  ( 6.899999691988000450, -12.43893545635000031, -2.828937028792000152 ) ) ;
#54741 = CARTESIAN_POINT ( 'NONE',  ( 18.11161644829667949, -2.784507902030457505, -12.38071508487800010 ) ) ;
#54742 = ORIENTED_EDGE ( 'NONE', *, *, #11258, .F. ) ;
#54744 = CARTESIAN_POINT ( 'NONE',  ( 18.01246087681401775, 10.82907928505076711, -4.296547899031908813 ) ) ;
#54743 = DIRECTION ( 'NONE',  ( 1.000000000000000000, 0.000000000000000000, 0.000000000000000000 ) ) ;
#54745 = CARTESIAN_POINT ( 'NONE',  ( 8.356920280409999791, 4.851303550474000303, -9.008742670124000540 ) ) ;
#54746 = CARTESIAN_POINT ( 'NONE',  ( 8.849999778957998942, -4.000000000000000000, -7.500000000000000000 ) ) ;
#54747 = CARTESIAN_POINT ( 'NONE',  ( 10.16000000000000014, -4.496968146123999865, -8.755198255949000696 ) ) ;
#54748 = CARTESIAN_POINT ( 'NONE',  ( 0.3705175461371000289, 3.176450105220999909, 1.136354878726999917 ) ) ;
#54749 = CARTESIAN_POINT ( 'NONE',  ( 12.80505043854143388, 3.124999999999999556, -25.00000000000000000 ) ) ;
#54750 = CARTESIAN_POINT ( 'NONE',  ( 3.167476045672999785, 2.924661563963000255, 2.085714127773000470 ) ) ;
#54751 = VERTEX_POINT ( 'NONE', #14676 ) ;
#54752 = CARTESIAN_POINT ( 'NONE',  ( 12.15464131684816884, 0.3178346465811170418, -12.59599179195193486 ) ) ;
#54753 = DIRECTION ( 'NONE',  ( 0.000000000000000000, -0.1333333333333049098, 0.9910712498212373989 ) ) ;
#54754 = CARTESIAN_POINT ( 'NONE',  ( 24.17809223743226710, -12.41828058357439346, -3.338452890154027575 ) ) ;
#54755 = CARTESIAN_POINT ( 'NONE',  ( 7.229676658770999964, 2.630487280353000390, 6.995957894972000268 ) ) ;
#54756 = ORIENTED_EDGE ( 'NONE', *, *, #49962, .T. ) ;
#54757 = CARTESIAN_POINT ( 'NONE',  ( 6.911404257992000311, -0.9275392149503000061, 1.138410677097999812 ) ) ;
#54758 = CARTESIAN_POINT ( 'NONE',  ( 8.534810841228001266, 5.092576903264999899, -6.628615687103999399 ) ) ;
#54760 = CARTESIAN_POINT ( 'NONE',  ( 4.600001223043999943, 13.10000000000000142, 0.000000000000000000 ) ) ;
#54759 = FACE_OUTER_BOUND ( 'NONE', #42768, .T. ) ;
#54761 = CARTESIAN_POINT ( 'NONE',  ( 10.33103907547007694, -3.225837863097586133, -7.899515915943056577 ) ) ;
#54762 = ORIENTED_EDGE ( 'NONE', *, *, #51522, .F. ) ;
#54763 = CARTESIAN_POINT ( 'NONE',  ( 23.60000000000000142, 0.000000000000000000, 0.000000000000000000 ) ) ;
#54764 = CARTESIAN_POINT ( 'NONE',  ( 17.80000000009400196, 3.216307036143000175, 11.40341376487999980 ) ) ;
#54765 = VERTEX_POINT ( 'NONE', #14337 ) ;
#54766 = CARTESIAN_POINT ( 'NONE',  ( 5.355026506350999860, 1.500000000000000000, 0.000000000000000000 ) ) ;
#54768 = CARTESIAN_POINT ( 'NONE',  ( 15.99015267864900203, 3.493241607194999876, 11.26524960718000123 ) ) ;
#54767 = AXIS2_PLACEMENT_3D ( 'NONE', #37853, #59177, #36475 ) ;
#54769 = CARTESIAN_POINT ( 'NONE',  ( 18.17477505917495151, -0.08167545936615620839, -13.89968205666727386 ) ) ;
#54770 = ORIENTED_EDGE ( 'NONE', *, *, #10559, .T. ) ;
#54771 = CARTESIAN_POINT ( 'NONE',  ( 15.40000000001299973, -8.815237407733999220, -7.616696375847999967 ) ) ;
#54772 = DIRECTION ( 'NONE',  ( 0.000000000000000000, 0.000000000000000000, -1.000000000000000000 ) ) ;
#54773 = CARTESIAN_POINT ( 'NONE',  ( 10.28014141025500017, 4.417352327511700594, -8.243346240911998635 ) ) ;
#54774 = CARTESIAN_POINT ( 'NONE',  ( 9.470944094206000585, -5.100000000000000533, 6.571291218949999902 ) ) ;
#54775 = CARTESIAN_POINT ( 'NONE',  ( 11.03776785110999903, 5.237767851104999650, 6.571291218949999902 ) ) ;
#54776 = ORIENTED_EDGE ( 'NONE', *, *, #23404, .T. ) ;
#54777 = FACE_OUTER_BOUND ( 'NONE', #30629, .T. ) ;
#54778 = EDGE_CURVE ( 'NONE', #8057, #36962, #52359, .T. ) ;
#54779 = EDGE_CURVE ( 'NONE', #23104, #63538, #69057, .T. ) ;
#54780 = CARTESIAN_POINT ( 'NONE',  ( 12.27940634383494789, -2.838250353068023646, -13.59582428665004450 ) ) ;
#54781 = AXIS2_PLACEMENT_3D ( 'NONE', #15358, #47171, #25843 ) ;
#54782 = CARTESIAN_POINT ( 'NONE',  ( 10.08079553769483461, 5.100000000000000533, -6.662590550628426200 ) ) ;
#54783 = CARTESIAN_POINT ( 'NONE',  ( 15.86005557146100209, -8.873324881979000267, -8.501367972259000538 ) ) ;
#54784 = ORIENTED_EDGE ( 'NONE', *, *, #32579, .F. ) ;
#54785 = B_SPLINE_SURFACE_WITH_KNOTS ( 'NONE', 3, 3, ( 
 ( #46388, #20846, #57908, #10006 ),
 ( #14914, #35892, #57208, #51286 ),
 ( #68040, #52657, #31343, #9310 ),
 ( #52317, #19469, #3383, #35219 ),
 ( #24718, #4753, #8636, #26095 ),
 ( #67350, #56877, #68728, #46043 ),
 ( #40792, #14233, #62114, #20156 ),
 ( #35561, #56532, #30316, #13892 ),
 ( #20500, #51623, #29986, #25749 ),
 ( #67692, #3719, #4063, #25057 ) ),
 .UNSPECIFIED., .F., .F., .F.,
 ( 4, 1, 1, 1, 1, 1, 1, 4 ),
 ( 4, 4 ),
 ( 0.07203983506773999068, 0.1428571428570999946, 0.2857142857143000203, 0.4285714285713999594, 0.5714285714286000406, 0.7142857142856999797, 0.8571428571429000609, 0.9589780836993999635 ),
 ( -0.1900620218102000158, 1.190128522698000069 ),
 .UNSPECIFIED. ) ;
#54786 = CARTESIAN_POINT ( 'NONE',  ( 12.42127013197883656, -2.006280959398177632, -12.55298695860706992 ) ) ;
#54787 = CARTESIAN_POINT ( 'NONE',  ( 10.80226354018299872, 2.907767014557178786, -6.870476274536374994 ) ) ;
#54788 = CARTESIAN_POINT ( 'NONE',  ( 7.192747165043829938, 3.481309508196248181, -5.716746811592346766 ) ) ;
#54789 = CARTESIAN_POINT ( 'NONE',  ( 12.01961669203094196, -2.969723712172476215, 7.824983907773938263 ) ) ;
#54790 = CARTESIAN_POINT ( 'NONE',  ( 12.80505043854146940, -1.787797342887048169, -13.88538010501570952 ) ) ;
#54791 = CARTESIAN_POINT ( 'NONE',  ( 11.55610404293055993, -4.502836909561000134, -8.523936114709998790 ) ) ;
#54792 = CARTESIAN_POINT ( 'NONE',  ( 5.909193173017250444, 0.3926218265389159745, 1.460959015002474493 ) ) ;
#54793 = CARTESIAN_POINT ( 'NONE',  ( 17.87931509819279441, -1.836668601340719187, 12.46541920085823918 ) ) ;
#54794 = VERTEX_POINT ( 'NONE', #40897 ) ;
#54795 = CARTESIAN_POINT ( 'NONE',  ( 11.43345123989529810, -3.459769760840400110, -8.543317325199000223 ) ) ;
#54796 = ORIENTED_EDGE ( 'NONE', *, *, #4416, .F. ) ;
#54797 = CARTESIAN_POINT ( 'NONE',  ( 11.26395919764000197, -12.20155262497000059, -1.453968487665999954 ) ) ;
#54798 = CARTESIAN_POINT ( 'NONE',  ( 9.594139158774000364, 2.212639797530000063, -6.855876382544999537 ) ) ;
#54799 = CARTESIAN_POINT ( 'NONE',  ( 3.173830139264999683, -1.787327779986999987, -2.868047506627999788 ) ) ;
#54800 = EDGE_CURVE ( 'NONE', #46101, #60944, #40698, .T. ) ;
#54801 = CARTESIAN_POINT ( 'NONE',  ( 10.14584566409999944, -5.370505908760000224, -6.826219946961000318 ) ) ;
#54802 = CARTESIAN_POINT ( 'NONE',  ( 24.63332959156760182, -8.756202931479764473, -7.455126439085038470 ) ) ;
#54803 = CARTESIAN_POINT ( 'NONE',  ( 24.22012832183300191, 12.17245628853000028, 3.346092709831000267 ) ) ;
#54804 = CARTESIAN_POINT ( 'NONE',  ( 11.50705667793316778, 4.601576474242010661, 6.338208022222376670 ) ) ;
#54805 = EDGE_LOOP ( 'NONE', ( #21256, #40158, #57950, #1241, #23328, #16126, #50872 ) ) ;
#54806 = CARTESIAN_POINT ( 'NONE',  ( 18.53712493497300073, 2.638811780578999677, 11.30793729956000071 ) ) ;
#54807 = AXIS2_PLACEMENT_3D ( 'NONE', #57828, #41414, #31273 ) ;
#54808 = CARTESIAN_POINT ( 'NONE',  ( 11.64179841651039915, -4.353306409735099969, 6.560784671286499226 ) ) ;
#54809 = CARTESIAN_POINT ( 'NONE',  ( 10.52638970730999901, 2.451081172664000274, 6.282749363171999946 ) ) ;
#54810 = CARTESIAN_POINT ( 'NONE',  ( 18.49996808500599954, -0.9036517542723243590, -11.65000000000000213 ) ) ;
#54811 = CARTESIAN_POINT ( 'NONE',  ( 8.896432056425105372, -5.285622111567716885, 7.027794277398525580 ) ) ;
#54812 = CARTESIAN_POINT ( 'NONE',  ( 18.35481935287100086, 2.723593151845999927, -11.47751840123000022 ) ) ;
#54813 = CARTESIAN_POINT ( 'NONE',  ( 11.36333594839950045, 4.659759757475400832, -6.743912759487099784 ) ) ;
#54814 = B_SPLINE_CURVE_WITH_KNOTS ( 'NONE', 3,
 ( #2813, #24143, #25519, #30096 ),
 .UNSPECIFIED., .F., .F.,
 ( 4, 4 ),
 ( 0.000000000000000000, 1.000000000000000000 ),
 .UNSPECIFIED. ) ;
#54815 = CONICAL_SURFACE ( 'NONE', #48124, 1.949999999867999767, 0.7853981633972997312 ) ;
#54816 = CARTESIAN_POINT ( 'NONE',  ( 8.616332382228000242, -2.832433105983000132, -6.822293595522999965 ) ) ;
#54817 = CARTESIAN_POINT ( 'NONE',  ( 9.884988259786998910, 3.850604015305000072, -8.631996151823999597 ) ) ;
#54818 = CARTESIAN_POINT ( 'NONE',  ( 23.83659698888000023, -9.655115511098998127, -9.481980187101999746 ) ) ;
#54819 = CARTESIAN_POINT ( 'NONE',  ( 23.73946058743000265, -9.841007807744000857, 9.518031540355998743 ) ) ;
#54820 = AXIS2_PLACEMENT_3D ( 'NONE', #56461, #29216, #8565 ) ;
#54821 = CARTESIAN_POINT ( 'NONE',  ( 25.60000000000000142, 0.000000000000000000, 0.000000000000000000 ) ) ;
#54822 = VERTEX_POINT ( 'NONE', #4167 ) ;
#54823 = CARTESIAN_POINT ( 'NONE',  ( 8.502043146794999728, -3.869396851328000153, 5.695656592546999519 ) ) ;
#54824 = CARTESIAN_POINT ( 'NONE',  ( 10.01574583856000089, -4.333399685216000385, -9.088699530815999239 ) ) ;
#54825 = CARTESIAN_POINT ( 'NONE',  ( 18.17186084707618576, 2.602861751209118779, 13.65107289232777177 ) ) ;
#54826 = CARTESIAN_POINT ( 'NONE',  ( 24.35365242081700288, -3.193712117489998281, 11.49150331539999215 ) ) ;
#54827 = CARTESIAN_POINT ( 'NONE',  ( 11.23195122972050086, -3.492749840905900349, -6.326963915009999440 ) ) ;
#54828 = ORIENTED_EDGE ( 'NONE', *, *, #24191, .T. ) ;
#54829 = CARTESIAN_POINT ( 'NONE',  ( 24.30000565690453840, -8.853233224111329847, 8.853233224111329847 ) ) ;
#54830 = CARTESIAN_POINT ( 'NONE',  ( 7.127704719590999716, 4.698356649019999942, 8.789431186081998248 ) ) ;
#54832 = CARTESIAN_POINT ( 'NONE',  ( 11.38678751119029897, 2.833702563575000166, 6.889827023674499173 ) ) ;
#54831 = CARTESIAN_POINT ( 'NONE',  ( 9.740360841231000322, 4.047146749018000200, -5.600703114891000034 ) ) ;
#54833 = VECTOR ( 'NONE', #62929, 1000.000000000000000 ) ;
#54834 = DIRECTION ( 'NONE',  ( -1.000000000000000000, -0.000000000000000000, -0.000000000000000000 ) ) ;
#54835 = EDGE_CURVE ( 'NONE', #33013, #2243, #21499, .T. ) ;
#54836 = VERTEX_POINT ( 'NONE', #10792 ) ;
#54837 = EDGE_CURVE ( 'NONE', #25728, #55564, #69125, .T. ) ;
#54838 = PLANE ( 'NONE',  #14945 ) ;
#54839 = CARTESIAN_POINT ( 'NONE',  ( 18.27904986288418243, -2.473365887482168901, -13.77980577478706969 ) ) ;
#54840 = CARTESIAN_POINT ( 'NONE',  ( 10.60026222744819790, 3.225465054973100099, 6.861998062869400172 ) ) ;
#54841 = CARTESIAN_POINT ( 'NONE',  ( 9.632185590920999019, -5.638162562978999759, 6.476633609657000079 ) ) ;
#54842 = CARTESIAN_POINT ( 'NONE',  ( 8.186785374738994037, 2.888678623336002005, 6.695956381329003726 ) ) ;
#54843 = ORIENTED_EDGE ( 'NONE', *, *, #33144, .F. ) ;
#54844 = CARTESIAN_POINT ( 'NONE',  ( 24.67921321864300310, 12.29514728640000065, 2.979192498689000157 ) ) ;
#54846 = CARTESIAN_POINT ( 'NONE',  ( 10.56170564679000101, -5.057490041178001050, -8.595713413570999606 ) ) ;
#54845 = CARTESIAN_POINT ( 'NONE',  ( 12.27593309678900191, -11.75515418280000013, 3.561236062516000000 ) ) ;
#54847 = CARTESIAN_POINT ( 'NONE',  ( 7.745598420978331511, -5.458216742540686894, 8.448484368435345004 ) ) ;
#54848 = CARTESIAN_POINT ( 'NONE',  ( 9.753140057121997941, -4.104977100659999323, 9.293279163877999238 ) ) ;
#54849 = CARTESIAN_POINT ( 'NONE',  ( 23.51693421199300360, 2.933245738859999729, 13.82474819291000045 ) ) ;
#54850 = CARTESIAN_POINT ( 'NONE',  ( 9.577417874593999514, -4.924352284713100047, 7.107043063332000088 ) ) ;
#54851 = EDGE_LOOP ( 'NONE', ( #16195, #67759, #41052, #63799, #59547 ) ) ;
#54852 = CARTESIAN_POINT ( 'NONE',  ( 23.80953379775873557, -9.702200433909665023, 9.418729782999628597 ) ) ;
#54853 = CARTESIAN_POINT ( 'NONE',  ( 11.95348876160960039, -4.885820101980599794, 6.578783887955899523 ) ) ;
#54854 = ORIENTED_EDGE ( 'NONE', *, *, #17611, .F. ) ;
#54855 = CARTESIAN_POINT ( 'NONE',  ( 17.60000000266004960, 10.99220013531737372, -4.481500379774075782 ) ) ;
#54856 = ORIENTED_EDGE ( 'NONE', *, *, #58556, .F. ) ;
#54857 = CARTESIAN_POINT ( 'NONE',  ( 9.649770280412001355, 4.042991257420999851, -5.768106221333000327 ) ) ;
#54858 = CARTESIAN_POINT ( 'NONE',  ( 23.51508276455100344, 13.45797239394999956, -4.320681590166000063 ) ) ;
#54859 = CARTESIAN_POINT ( 'NONE',  ( 12.80505043854143388, 3.199751711897557804, -12.18694338143115630 ) ) ;
#54860 = CARTESIAN_POINT ( 'NONE',  ( 12.14633327354034797, -4.864904118400500188, 8.065722083251399610 ) ) ;
#54861 = EDGE_CURVE ( 'NONE', #23416, #3150, #54131, .T. ) ;
#54862 = VERTEX_POINT ( 'NONE', #21966 ) ;
#54863 = CARTESIAN_POINT ( 'NONE',  ( 8.869959105252339882, -2.899999999999999911, 6.481052078534832006 ) ) ;
#54864 = B_SPLINE_CURVE_WITH_KNOTS ( 'NONE', 3,
 ( #17630, #34408, #13760, #34747, #41360, #35771, #67566, #46263, #14106, #8167 ),
 .UNSPECIFIED., .F., .F.,
 ( 4, 2, 2, 2, 4 ),
 ( 0.4999999998130725265, 0.6249999998598043671, 0.7499999999065363188, 0.8749999999532681594, 1.000000000000000000 ),
 .UNSPECIFIED. ) ;
#54865 = EDGE_CURVE ( 'NONE', #48385, #63101, #43305, .T. ) ;
#54866 = VERTEX_POINT ( 'NONE', #11140 ) ;
#54867 = CARTESIAN_POINT ( 'NONE',  ( 7.533879440377999614, -4.623636604834999275, 8.651469651195000665 ) ) ;
#54868 = CARTESIAN_POINT ( 'NONE',  ( 23.60000648950287427, 10.25354916021784746, 9.380079597658479429 ) ) ;
#54869 = EDGE_LOOP ( 'NONE', ( #8330, #15363, #29084, #1583, #60657 ) ) ;
#54870 = CARTESIAN_POINT ( 'NONE',  ( 12.51412939328312390, -3.139365204187050118, -12.20263940233110311 ) ) ;
#54871 = CARTESIAN_POINT ( 'NONE',  ( 10.79303032197930001, 4.663532080728800544, 8.427909097977700270 ) ) ;
#54872 = CARTESIAN_POINT ( 'NONE',  ( 10.68343305961999867, -3.810133104029999718, -5.661126601970999594 ) ) ;
#54873 = CARTESIAN_POINT ( 'NONE',  ( 10.24846228258000025, 4.234133568259999869, -5.660851473941000300 ) ) ;
#54874 = CARTESIAN_POINT ( 'NONE',  ( 18.35889944991900435, -11.74562277640000119, 3.912379265303000508 ) ) ;
#54875 = CARTESIAN_POINT ( 'NONE',  ( 8.017297003156455659, -5.179978819780794552, 8.180934229233972843 ) ) ;
#54876 = CARTESIAN_POINT ( 'NONE',  ( 12.64146116164748435, -3.103558470340185949, -13.52669597090169340 ) ) ;
#54877 = CARTESIAN_POINT ( 'NONE',  ( 17.83205770179218774, -0.5603556898929438201, -12.68335562943301476 ) ) ;
#54878 = AXIS2_PLACEMENT_3D ( 'NONE', #19370, #3965, #35124 ) ;
#54879 = CARTESIAN_POINT ( 'NONE',  ( 12.19252377751849536, 2.624242476089503118, -12.42177825695367943 ) ) ;
#54880 = CARTESIAN_POINT ( 'NONE',  ( 11.43302763632549990, -5.035790660926999784, -7.022058766158599141 ) ) ;
#54881 = CARTESIAN_POINT ( 'NONE',  ( 7.390489158771000433, 2.216873702600000051, 8.370081218683999680 ) ) ;
#54882 = ORIENTED_EDGE ( 'NONE', *, *, #17719, .T. ) ;
#54883 = CARTESIAN_POINT ( 'NONE',  ( 24.35365242081699932, -12.20235406293000935, 3.288253180433003298 ) ) ;
#54884 = FACE_OUTER_BOUND ( 'NONE', #26746, .T. ) ;
#54885 = DIRECTION ( 'NONE',  ( -1.264998825433999916E-10, -1.265000103913999927E-10, 1.000000000000000000 ) ) ;
#54886 = CARTESIAN_POINT ( 'NONE',  ( 10.36950244779999863, 2.719131864236000062, -7.031786688683999920 ) ) ;
#54887 = ADVANCED_FACE ( 'NONE', ( #32474 ), #21285, .T. ) ;
#54888 = CARTESIAN_POINT ( 'NONE',  ( 17.88769455523108931, 1.970775861831701947, 12.55923393539035970 ) ) ;
#54889 = AXIS2_PLACEMENT_3D ( 'NONE', #32774, #32431, #53748 ) ;
#54890 = CARTESIAN_POINT ( 'NONE',  ( 18.53935907712300235, 2.923447147946000246, -12.21821814482000157 ) ) ;
#54891 = CARTESIAN_POINT ( 'NONE',  ( 9.905792474809000936, 2.698958900805999761, 8.979236532123000103 ) ) ;
#54892 = CARTESIAN_POINT ( 'NONE',  ( 10.76539516633362581, -3.766791217824746241, 6.656705459454948404 ) ) ;
#54893 = CARTESIAN_POINT ( 'NONE',  ( 8.790860954911998704, 4.097566467530549872, 6.578106533244199916 ) ) ;
#54894 = ORIENTED_EDGE ( 'NONE', *, *, #19972, .T. ) ;
#54895 = CARTESIAN_POINT ( 'NONE',  ( 12.17614882354827621, -2.839252809666454880, 12.27595571488803827 ) ) ;
#54896 = CARTESIAN_POINT ( 'NONE',  ( 9.277088727410998104, -5.137817193984000497, -7.595427884080399927 ) ) ;
#54897 = CARTESIAN_POINT ( 'NONE',  ( 24.44917776433500123, -3.519943607436000210, -12.30316564740000196 ) ) ;
#54898 = DIRECTION ( 'NONE',  ( 0.7071058580587948894, 0.7071077043130949979, -4.007479631938970195E-09 ) ) ;
#54899 = CARTESIAN_POINT ( 'NONE',  ( 10.94487616594229884, 3.696562859151900415, -6.543508100188799581 ) ) ;
#54900 = EDGE_LOOP ( 'NONE', ( #33435, #56409, #459 ) ) ;
#54901 = CARTESIAN_POINT ( 'NONE',  ( 12.47306973639847882, -0.6395598188657312111, 12.58375915074078577 ) ) ;
#54902 = CARTESIAN_POINT ( 'NONE',  ( 8.341920280410999311, 5.601795057054999916, 7.176148573050999957 ) ) ;
#54903 = CARTESIAN_POINT ( 'NONE',  ( 10.27815081430999911, 5.521603098753999461, 8.751228458888000716 ) ) ;
#54904 = CARTESIAN_POINT ( 'NONE',  ( 12.34719455185577885, 2.925915912524184925, 12.34207449233261933 ) ) ;
#54905 = EDGE_LOOP ( 'NONE', ( #44681, #32592, #29981, #32513 ) ) ;
#54906 = CARTESIAN_POINT ( 'NONE',  ( 25.31133098161000206, 8.473030475148000562, 8.042931544829999169 ) ) ;
#54907 = CARTESIAN_POINT ( 'NONE',  ( 11.05964426047339799, 4.687693494822500639, -8.577215873335999774 ) ) ;
#54908 = CARTESIAN_POINT ( 'NONE',  ( 9.674960421382234443, 2.650268802166420024, 7.499999178247376719 ) ) ;
#54910 = DIRECTION ( 'NONE',  ( -1.000000000000000000, 0.000000000000000000, 0.000000000000000000 ) ) ;
#54909 = CARTESIAN_POINT ( 'NONE',  ( 7.822787301102997581, 4.879242518472000967, 6.344068876191006012 ) ) ;
#54911 = CARTESIAN_POINT ( 'NONE',  ( 9.402126402770999647, -3.188752782784400441, 7.805918119494599239 ) ) ;
#54912 = CARTESIAN_POINT ( 'NONE',  ( 11.68748876160954886, -4.600381688599499697, -8.124372018288600117 ) ) ;
#54913 = DIRECTION ( 'NONE',  ( 0.000000000000000000, 0.000000000000000000, -1.000000000000000000 ) ) ;
#54914 = ORIENTED_EDGE ( 'NONE', *, *, #42149, .F. ) ;
#54915 = AXIS2_PLACEMENT_3D ( 'NONE', #24426, #62161, #45750 ) ;
#54916 = CARTESIAN_POINT ( 'NONE',  ( 1.210109898187999855, -0.3467249428283000201, -3.408020022541999872 ) ) ;
#54917 = CARTESIAN_POINT ( 'NONE',  ( 23.94495875478589753, -9.457063741204379426, -9.320448346922830751 ) ) ;
#54918 = CARTESIAN_POINT ( 'NONE',  ( 9.396714042595458949, -4.136150106425177775, 8.546714100015048388 ) ) ;
#54919 = CARTESIAN_POINT ( 'NONE',  ( 7.000000000000000000, 7.526486366024999874, -3.526486366024999874 ) ) ;
#54920 = EDGE_CURVE ( 'NONE', #4653, #38352, #67438, .T. ) ;
#54921 = EDGE_CURVE ( 'NONE', #64347, #35994, #26543, .T. ) ;
#54922 = CARTESIAN_POINT ( 'NONE',  ( 24.56351374521100439, -12.27674503203999912, 3.066186501695999933 ) ) ;
#54923 = CARTESIAN_POINT ( 'NONE',  ( 12.08891106753600830, -2.402099963521321602, 13.79240636836165024 ) ) ;
#54924 = DIRECTION ( 'NONE',  ( -0.7071060865236062920, -0.7071074758488062884, -8.141935074000071186E-10 ) ) ;
#54925 = CARTESIAN_POINT ( 'NONE',  ( 9.015584277044482064, -4.716917290452846245, -8.431467892494236338 ) ) ;
#54926 = DIRECTION ( 'NONE',  ( 0.000000000000000000, 0.8648648648648717963, -0.5020047465136829867 ) ) ;
#54927 = ORIENTED_EDGE ( 'NONE', *, *, #3959, .T. ) ;
#54928 = ADVANCED_FACE ( 'NONE', ( #47522 ), #54041, .F. ) ;
#54929 = CARTESIAN_POINT ( 'NONE',  ( 7.645552793751999587, 8.186488560794998648, -4.631829788185999774 ) ) ;
#54930 = CARTESIAN_POINT ( 'NONE',  ( 9.523148997461001741, 5.167567567567999731, -6.822293592207000934 ) ) ;
#54931 = FACE_OUTER_BOUND ( 'NONE', #49092, .T. ) ;
#54932 = CIRCLE ( 'NONE', #50488, 12.50000000000000178 ) ;
#54933 = DIRECTION ( 'NONE',  ( -0.9999999999999978906, 6.939020669836964126E-09, -6.650367360942975276E-08 ) ) ;
#54934 = CARTESIAN_POINT ( 'NONE',  ( 0.5130637418424000007, 3.696170276785000208, -0.6823948523853999859 ) ) ;
#54935 = CARTESIAN_POINT ( 'NONE',  ( 10.82336322478654544, 2.820284244472439195, -8.179952785015741412 ) ) ;
#54936 = CARTESIAN_POINT ( 'NONE',  ( 6.899999691988000450, 11.00717859340000082, -1.432487142323000118 ) ) ;
#54937 = CARTESIAN_POINT ( 'NONE',  ( 9.848259964010999568, 4.436917881843999822, 6.148031614254000132 ) ) ;
#54938 = CARTESIAN_POINT ( 'NONE',  ( 11.17056785386839834, 3.281375110759499947, 7.016391833292499491 ) ) ;
#54939 = CIRCLE ( 'NONE', #15846, 1.000000000000000222 ) ;
#54940 = DIRECTION ( 'NONE',  ( 0.000000000000000000, 0.8648648648648717963, 0.5020047465136829867 ) ) ;
#54941 = CARTESIAN_POINT ( 'NONE',  ( 10.37239314679000124, -3.992345679293999972, -5.977234595428000397 ) ) ;
#54942 = CARTESIAN_POINT ( 'NONE',  ( 17.55505043854144276, -0.7302158263239199032, -13.98094363220830871 ) ) ;
#54943 = CARTESIAN_POINT ( 'NONE',  ( 9.615109647822677630, 5.349900357012234764, -7.499993490198826329 ) ) ;
#54944 = CARTESIAN_POINT ( 'NONE',  ( 3.999999173945999686, 0.000000000000000000, -1.825000327748890427 ) ) ;
#54945 = EDGE_LOOP ( 'NONE', ( #17287, #6465, #66084, #3299 ) ) ;
#54946 = CARTESIAN_POINT ( 'NONE',  ( 11.09999999999999964, -5.299771130038000599, 5.136740763824000133 ) ) ;
#54947 = EDGE_LOOP ( 'NONE', ( #48122, #58553, #41376, #42205, #20129 ) ) ;
#54948 = CARTESIAN_POINT ( 'NONE',  ( 18.17181771166727344, -2.603111764601558686, 13.65106951237197386 ) ) ;
#54950 = CARTESIAN_POINT ( 'NONE',  ( 11.15810538575740019, -2.757018958839999812, -7.202822423614300362 ) ) ;
#54949 = B_SPLINE_CURVE_WITH_KNOTS ( 'NONE', 3,
 ( #28807, #18647, #2558, #7456 ),
 .UNSPECIFIED., .F., .F.,
 ( 4, 4 ),
 ( 0.000000000000000000, 1.000000000000000000 ),
 .UNSPECIFIED. ) ;
#54951 = ORIENTED_EDGE ( 'NONE', *, *, #51300, .F. ) ;
#54952 = CARTESIAN_POINT ( 'NONE',  ( 11.18923293495519822, 2.967327562101000016, 7.541513160549049744 ) ) ;
#54953 = CARTESIAN_POINT ( 'NONE',  ( 6.697846812853917697, 0.1022963455632099478, 1.128078040366519597 ) ) ;
#54954 = DIRECTION ( 'NONE',  ( -1.000000000000000000, 0.000000000000000000, 0.000000000000000000 ) ) ;
#54955 = CARTESIAN_POINT ( 'NONE',  ( 9.504903297738000134, 3.934733353759999552, 5.704831249548000471 ) ) ;
#54956 = DIRECTION ( 'NONE',  ( 1.000000000000000000, 0.000000000000000000, 0.000000000000000000 ) ) ;
#54957 = CARTESIAN_POINT ( 'NONE',  ( 10.88351354018329431, -5.249999999999998224, 7.663624617374469317 ) ) ;
#54958 = CARTESIAN_POINT ( 'NONE',  ( 0.7000000000000000666, 0.000000000000000000, 0.000000000000000000 ) ) ;
#54959 = CARTESIAN_POINT ( 'NONE',  ( 9.949439740260999088, -2.508493821066999807, -7.171861383782999866 ) ) ;
#54960 = DIRECTION ( 'NONE',  ( 0.000000000000000000, 0.8648648261949251070, 0.5020048131351152465 ) ) ;
#54961 = SURFACE_STYLE_USAGE ( .BOTH. , #60899 ) ;
#54962 = ORIENTED_EDGE ( 'NONE', *, *, #741, .F. ) ;
#54963 = DIRECTION ( 'NONE',  ( 1.000000000000000000, 0.000000000000000000, 0.000000000000000000 ) ) ;
#54964 = AXIS2_PLACEMENT_3D ( 'NONE', #22441, #65078, #42405 ) ;
#54965 = VERTEX_POINT ( 'NONE', #17421 ) ;
#54966 = CARTESIAN_POINT ( 'NONE',  ( 17.65158693965129899, -1.792693047833532116, -13.88475221912021418 ) ) ;
#54967 =( NAMED_UNIT ( * ) SI_UNIT ( $, .STERADIAN. ) SOLID_ANGLE_UNIT ( ) );
#54968 = ADVANCED_FACE ( 'NONE', ( #45035 ), #1339, .T. ) ;
#54969 = CARTESIAN_POINT ( 'NONE',  ( 25.12926781546009636, -8.519457660519075048, 8.174621111370402815 ) ) ;
#54970 = CARTESIAN_POINT ( 'NONE',  ( 10.03897570133299944, 4.938486452461599896, -8.369268408503399925 ) ) ;
#54971 = CARTESIAN_POINT ( 'NONE',  ( 12.72263738247858456, 1.880115814278896957, 13.78550660562620145 ) ) ;
#54972 = CARTESIAN_POINT ( 'NONE',  ( 9.555699158955999195, -2.440755924888999839, 6.680881588809999272 ) ) ;
#54973 = ORIENTED_EDGE ( 'NONE', *, *, #41319, .F. ) ;
#54974 = EDGE_CURVE ( 'NONE', #15766, #54866, #18177, .T. ) ;
#54975 = CARTESIAN_POINT ( 'NONE',  ( 12.76431688221209981, 0.6240105542978634512, -12.67935574133243470 ) ) ;
#54976 = CARTESIAN_POINT ( 'NONE',  ( 12.37769783401832768, -0.4561791668615506889, 13.88992602861185333 ) ) ;
#54977 = B_SPLINE_CURVE_WITH_KNOTS ( 'NONE', 3,
 ( #59879, #22819, #11985, #30829 ),
 .UNSPECIFIED., .F., .F.,
 ( 4, 4 ),
 ( 0.000000000000000000, 0.1254144463278223376 ),
 .UNSPECIFIED. ) ;
#54978 = VERTEX_POINT ( 'NONE', #33510 ) ;
#54979 = CARTESIAN_POINT ( 'NONE',  ( 7.009409439180999790, 2.534482666265000184, -7.314862106114000007 ) ) ;
#54980 = CARTESIAN_POINT ( 'NONE',  ( 17.56849549447199976, 11.93188800409999928, -3.261574020045000299 ) ) ;
#54981 = CARTESIAN_POINT ( 'NONE',  ( 8.998937807218627682, 3.944921334759000420, 8.373211663664079651 ) ) ;
#54982 = CARTESIAN_POINT ( 'NONE',  ( 4.310425572186999510, -0.9683957735725999827, -0.7692866548104999591 ) ) ;
#54983 = CIRCLE ( 'NONE', #42703, 1.000000000000001332 ) ;
#54984 = CARTESIAN_POINT ( 'NONE',  ( 9.526695280414001488, 5.462898983065000102, -8.055936939571999744 ) ) ;
#54985 = CARTESIAN_POINT ( 'NONE',  ( 9.927263540182998725, 3.370476274536375438, -8.592232985442821658 ) ) ;
#54986 = AXIS2_PLACEMENT_3D ( 'NONE', #57553, #41825, #42180 ) ;
#54987 = CARTESIAN_POINT ( 'NONE',  ( 10.95551720753999980, -4.744041807741999683, -9.198129812222999746 ) ) ;
#54988 = CARTESIAN_POINT ( 'NONE',  ( 8.273285508597860272, 2.795069959664616022, -8.205047406324164072 ) ) ;
#54989 = CYLINDRICAL_SURFACE ( 'NONE', #20340, 1.350000000000000089 ) ;
#54990 = SURFACE_STYLE_FILL_AREA ( #65110 ) ;
#54991 = CARTESIAN_POINT ( 'NONE',  ( 18.30000000000000071, 2.818726571106858980, 11.83569999720589294 ) ) ;
#54992 = DIRECTION ( 'NONE',  ( 0.000000000000000000, -1.000000000000000000, 0.000000000000000000 ) ) ;
#54993 = CARTESIAN_POINT ( 'NONE',  ( 24.53428985175800037, 12.47024902693999948, -3.026245299674999778 ) ) ;
#54994 = CARTESIAN_POINT ( 'NONE',  ( 10.60746886766490071, 3.501664543805500074, -6.594573315824700188 ) ) ;
#54995 = CARTESIAN_POINT ( 'NONE',  ( 9.533342523874999586, 3.007153757386999526, -7.348017636355000270 ) ) ;
#54997 = DIRECTION ( 'NONE',  ( 0.7071068219128313626, 0.000000000000000000, 0.7071067404602613404 ) ) ;
#54996 = CARTESIAN_POINT ( 'NONE',  ( 9.798392757686999133, -3.414780058706900157, 6.860292594369099106 ) ) ;
#54998 = CARTESIAN_POINT ( 'NONE',  ( 11.16476354018302430, -2.782534154164604256, 7.827184855449094592 ) ) ;
#54999 = ORIENTED_EDGE ( 'NONE', *, *, #27138, .F. ) ;
#55000 = CARTESIAN_POINT ( 'NONE',  ( 10.81013259637009938, 2.968328969579000276, 6.937848198857199833 ) ) ;
#55001 = CARTESIAN_POINT ( 'NONE',  ( 10.96080136920999948, -2.054580854576999904, 7.810082699133999995 ) ) ;
#55002 = CARTESIAN_POINT ( 'NONE',  ( 10.23959632033899858, 2.942832934044000037, 7.931430460958599049 ) ) ;
#55003 = CARTESIAN_POINT ( 'NONE',  ( 9.530849898046625412, 3.608426922415753690, -6.717566108970133953 ) ) ;
#55004 = EDGE_CURVE ( 'NONE', #52029, #56220, #46528, .T. ) ;
#55005 = CARTESIAN_POINT ( 'NONE',  ( 9.104016254283999743, -5.045864843302999780, 8.527867871227000407 ) ) ;
#55006 = DIRECTION ( 'NONE',  ( 1.000000000000000000, 0.000000000000000000, 0.000000000000000000 ) ) ;
#55007 = CARTESIAN_POINT ( 'NONE',  ( 10.40434687351665310, 2.750000000000000000, 7.336375382625536901 ) ) ;
#55008 = VERTEX_POINT ( 'NONE', #65994 ) ;
#55009 = EDGE_CURVE ( 'NONE', #28289, #52029, #59028, .T. ) ;
#55010 = EDGE_CURVE ( 'NONE', #62083, #11162, #10729, .T. ) ;
#55011 = CARTESIAN_POINT ( 'NONE',  ( 9.381367640780998940, -3.526522998810799781, -6.614188603779100006 ) ) ;
#55012 = AXIS2_PLACEMENT_3D ( 'NONE', #37969, #59987, #5121 ) ;
#55013 = FACE_OUTER_BOUND ( 'NONE', #34517, .T. ) ;
#55014 = CARTESIAN_POINT ( 'NONE',  ( 9.933148997456999751, -5.167567567567999731, 6.822293592207000934 ) ) ;
#55015 = CARTESIAN_POINT ( 'NONE',  ( 7.000000000000000000, 6.495985883990673670, 3.000000000000000000 ) ) ;
#55016 = CARTESIAN_POINT ( 'NONE',  ( 24.44916829770000177, -3.519946668155999880, 12.30317708153000034 ) ) ;
#55017 = CARTESIAN_POINT ( 'NONE',  ( 12.75354487906747458, 0.6229596466635303198, -12.67942438339646749 ) ) ;
#55018 = CARTESIAN_POINT ( 'NONE',  ( 11.56025819896753859, 3.013900664291200293, -7.685900384398899554 ) ) ;
#55019 = CARTESIAN_POINT ( 'NONE',  ( 10.98768472639999949, 5.139099012905000485, 4.945212061661000469 ) ) ;
#55020 = CARTESIAN_POINT ( 'NONE',  ( 24.95409909025299910, -8.513620944989998662, 8.994042707941998671 ) ) ;
#55021 = DIRECTION ( 'NONE',  ( 0.000000000000000000, -0.7198977633594747516, -0.6940801180771756229 ) ) ;
#55022 = EDGE_LOOP ( 'NONE', ( #11333, #53312, #41029, #2585 ) ) ;
#55023 = DIRECTION ( 'NONE',  ( 1.000000000000000000, 0.000000000000000000, -7.105427357580000488E-14 ) ) ;
#55024 = CARTESIAN_POINT ( 'NONE',  ( 12.80505043854144276, 0.6249999999999995559, -13.88107975066922428 ) ) ;
#55025 = CARTESIAN_POINT ( 'NONE',  ( 8.296584986412122831, 4.202841942069439618, 6.085974839126271796 ) ) ;
#55026 = CARTESIAN_POINT ( 'NONE',  ( 25.31131545028100049, -8.473030824119000215, -8.042950951552001015 ) ) ;
#55027 = EDGE_CURVE ( 'NONE', #26858, #12749, #23359, .T. ) ;
#55028 = CARTESIAN_POINT ( 'NONE',  ( 13.42968832854747241, -11.50414049279774176, -1.837906235105113861 ) ) ;
#55029 = FACE_OUTER_BOUND ( 'NONE', #16161, .T. ) ;
#55030 = CARTESIAN_POINT ( 'NONE',  ( 5.604756202879674909, 12.12903653622838007, -3.749090042450943461 ) ) ;
#55031 = VERTEX_POINT ( 'NONE', #6925 ) ;
#55032 = CARTESIAN_POINT ( 'NONE',  ( 5.600000000706000236, 0.8000000000000000444, -3.149999999999999911 ) ) ;
#55033 = CARTESIAN_POINT ( 'NONE',  ( 17.57920827036996059, 3.248109283636066102, -13.61799489948997888 ) ) ;
#55034 = ORIENTED_EDGE ( 'NONE', *, *, #51190, .F. ) ;
#55035 = FACE_OUTER_BOUND ( 'NONE', #7017, .T. ) ;
#55036 = CARTESIAN_POINT ( 'NONE',  ( 8.224933059623998233, -5.629389383493999865, 8.631822608164000599 ) ) ;
#55037 = CARTESIAN_POINT ( 'NONE',  ( 8.324914158772999784, 2.633142096252999664, -7.791134854666999843 ) ) ;
#55038 = CARTESIAN_POINT ( 'NONE',  ( 11.09999999999999964, -2.289217163982593561, -7.673604523768878138 ) ) ;
#55039 = CARTESIAN_POINT ( 'NONE',  ( 11.07273594314529142, 5.128905988536224037, -7.175020482857276782 ) ) ;
#55040 = DIRECTION ( 'NONE',  ( 1.000000000000000000, 0.000000000000000000, 0.000000000000000000 ) ) ;
#55041 = CARTESIAN_POINT ( 'NONE',  ( 11.08333333333538562, -2.470076941867837217, 7.228155005602529215 ) ) ;
#55042 = ORIENTED_EDGE ( 'NONE', *, *, #9776, .F. ) ;
#55043 = CARTESIAN_POINT ( 'NONE',  ( 8.384365347816494562, 4.198915299351829056, -6.035294823839894462 ) ) ;
#55044 = CARTESIAN_POINT ( 'NONE',  ( 18.16596415355668981, -2.632031932216792658, -13.64451525700246393 ) ) ;
#55045 = CARTESIAN_POINT ( 'NONE',  ( 8.798539158775000146, 5.851083642416999631, -7.072167224702999633 ) ) ;
#55046 = ORIENTED_EDGE ( 'NONE', *, *, #55168, .F. ) ;
#55047 = CARTESIAN_POINT ( 'NONE',  ( 9.675534850247000662, 4.656736118461000551, -8.653212384786000300 ) ) ;
#55048 = CARTESIAN_POINT ( 'NONE',  ( 9.064883232718324635, 5.349954811645839747, -7.500006748065883855 ) ) ;
#55049 = ORIENTED_EDGE ( 'NONE', *, *, #7820, .T. ) ;
#55050 = CARTESIAN_POINT ( 'NONE',  ( 9.634659112603999986, 3.563556310301200014, 6.595367916746299741 ) ) ;
#55051 = CARTESIAN_POINT ( 'NONE',  ( 18.25561427624399613, -2.667326636134559337, -12.31445830791194140 ) ) ;
#55052 = CARTESIAN_POINT ( 'NONE',  ( 9.498096873515667227, 3.672815144550898303, 6.282534154164607365 ) ) ;
#55053 = CARTESIAN_POINT ( 'NONE',  ( 8.406851002545000284, 2.832432432432000269, -6.822293592207000934 ) ) ;
#55054 = CARTESIAN_POINT ( 'NONE',  ( 0.000000000000000000, 0.000000000000000000, 0.000000000000000000 ) ) ;
#55055 = EDGE_CURVE ( 'NONE', #6078, #39994, #45379, .T. ) ;
#55056 = CARTESIAN_POINT ( 'NONE',  ( 8.724822372493999723, 3.750788346126100237, 6.684745346084599582 ) ) ;
#55057 = B_SPLINE_CURVE_WITH_KNOTS ( 'NONE', 3,
 ( #31342, #53007, #19468, #42179 ),
 .UNSPECIFIED., .F., .F.,
 ( 4, 4 ),
 ( 0.000000000000000000, 1.000000000000000000 ),
 .UNSPECIFIED. ) ;
#55058 = CARTESIAN_POINT ( 'NONE',  ( 9.351200703499365829, -3.426673320826296276, 9.142253940106426668 ) ) ;
#55059 = ORIENTED_EDGE ( 'NONE', *, *, #32798, .F. ) ;
#55060 = DIRECTION ( 'NONE',  ( 0.000000000000000000, 0.8514543052404082157, -0.5244287998266055073 ) ) ;
#55061 = CARTESIAN_POINT ( 'NONE',  ( 9.978904719591000116, 5.007782080444000528, -8.772599239991000886 ) ) ;
#55062 = CARTESIAN_POINT ( 'NONE',  ( 24.30000561709021412, 8.853233208361997342, -8.853233208361997342 ) ) ;
#55063 = CARTESIAN_POINT ( 'NONE',  ( 12.20145977811404414, 2.662504703663703065, -13.63765425733092229 ) ) ;
#55064 = AXIS2_PLACEMENT_3D ( 'NONE', #47611, #11559, #63669 ) ;
#55065 = CARTESIAN_POINT ( 'NONE',  ( 16.86666666323366925, -3.595157417866057248, -11.99793599502774200 ) ) ;
#55066 = CARTESIAN_POINT ( 'NONE',  ( 9.442841440870999747, -2.691258483914000355, 6.269525829285999663 ) ) ;
#55067 = CARTESIAN_POINT ( 'NONE',  ( 17.88507584039978937, 0.5311540453515649629, 13.88634387573209139 ) ) ;
#55068 = CARTESIAN_POINT ( 'NONE',  ( 17.77470470800434654, 0.5852235852771162650, 13.88341353704861270 ) ) ;
#55069 = ORIENTED_EDGE ( 'NONE', *, *, #44390, .T. ) ;
#55070 = ORIENTED_EDGE ( 'NONE', *, *, #3137, .T. ) ;
#55071 = CARTESIAN_POINT ( 'NONE',  ( 9.436104719595000745, 5.619431609641999614, -8.115423117607999615 ) ) ;
#55072 = CARTESIAN_POINT ( 'NONE',  ( 12.55587196711313602, -0.5732793990213274071, 13.88408420575303559 ) ) ;
#55073 = CARTESIAN_POINT ( 'NONE',  ( 12.60487368088291582, -0.5921679929136640652, -13.88301795523049087 ) ) ;
#55074 = CARTESIAN_POINT ( 'NONE',  ( 9.261668853699999815, -2.944250413017999612, 6.507387951280999339 ) ) ;
#55075 = LINE ( 'NONE', #19041, #68512 ) ;
#55076 = CARTESIAN_POINT ( 'NONE',  ( 7.807370559623000084, -3.650411072918999800, 6.083135626079000602 ) ) ;
#55077 = PLANE ( 'NONE',  #63879 ) ;
#55079 = CARTESIAN_POINT ( 'NONE',  ( 11.01665855156000084, -6.699723434166000580, 5.516656797456000128 ) ) ;
#55078 = CARTESIAN_POINT ( 'NONE',  ( 9.703113844318000503, -3.676949563211899807, 8.737749087159000894 ) ) ;
#55080 = VECTOR ( 'NONE', #66141, 1000.000000000000114 ) ;
#55081 = CARTESIAN_POINT ( 'NONE',  ( 10.34580110216399973, 2.909301855364999856, -6.833896451085399448 ) ) ;
#55082 = CARTESIAN_POINT ( 'NONE',  ( 12.09999999999999609, -4.745632530848082453, 6.836536274993706641 ) ) ;
#55083 = CARTESIAN_POINT ( 'NONE',  ( 18.02449637307654129, 11.46556595593859562, -4.499409268768501668 ) ) ;
#55084 = CARTESIAN_POINT ( 'NONE',  ( 17.57568447735987149, 0.6247443594537129830, 12.67930618256805886 ) ) ;
#55085 = DIRECTION ( 'NONE',  ( 0.000000000000000000, 1.000000000000000000, 0.000000000000000000 ) ) ;
#55086 = CARTESIAN_POINT ( 'NONE',  ( 18.08152692720914345, -2.836954189429314432, -12.36664858736754447 ) ) ;
#55087 = EDGE_LOOP ( 'NONE', ( #52421, #55984, #35000, #41942, #34838 ) ) ;
#55089 = CARTESIAN_POINT ( 'NONE',  ( 10.84606641549978256, 4.838299037060044938, 7.252322131039115050 ) ) ;
#55088 = CARTESIAN_POINT ( 'NONE',  ( 12.99999999998900080, -12.39025855408000076, -1.832244667012999928 ) ) ;
#55090 = CARTESIAN_POINT ( 'NONE',  ( 8.465229719592999302, 2.567871051582000241, -6.869011921437000012 ) ) ;
#55091 = EDGE_CURVE ( 'NONE', #43802, #23570, #60076, .T. ) ;
#55092 = EDGE_CURVE ( 'NONE', #43147, #62317, #57954, .T. ) ;
#55093 = FACE_OUTER_BOUND ( 'NONE', #48184, .T. ) ;
#55094 = CARTESIAN_POINT ( 'NONE',  ( 23.59999196693599899, 2.915561532799999966, -13.58550759281999909 ) ) ;
#55095 = B_SPLINE_CURVE_WITH_KNOTS ( 'NONE', 3,
 ( #2960, #62034, #13808, #45959 ),
 .UNSPECIFIED., .F., .F.,
 ( 4, 4 ),
 ( 0.000000000000000000, 1.000000000000000000 ),
 .UNSPECIFIED. ) ;
#55096 = CARTESIAN_POINT ( 'NONE',  ( 10.29657053952199952, 3.497746311184500190, 8.675184076076000395 ) ) ;
#55097 = CARTESIAN_POINT ( 'NONE',  ( 8.784678295047998020, 4.000000000000000000, -7.500000000000000000 ) ) ;
#55098 = CARTESIAN_POINT ( 'NONE',  ( 18.28771851938396154, -2.987294196519939327, -11.95930572916780399 ) ) ;
#55099 = CARTESIAN_POINT ( 'NONE',  ( 2.166155107414999836, 2.958863020030999991, 2.036875221550000337 ) ) ;
#55100 = ORIENTED_EDGE ( 'NONE', *, *, #52353, .F. ) ;
#55101 = CARTESIAN_POINT ( 'NONE',  ( 12.25170120909045934, 0.4648927885597781695, -12.59142395508372836 ) ) ;
#55102 = CARTESIAN_POINT ( 'NONE',  ( 7.808998088039303731, -3.043595652559401898, 6.499272882928453399 ) ) ;
#55103 = DIRECTION ( 'NONE',  ( 0.000000000000000000, -1.000000000000000000, 0.000000000000000000 ) ) ;
#55104 = CARTESIAN_POINT ( 'NONE',  ( 8.822982780412001347, 2.678331728353000152, 8.735281589464001684 ) ) ;
#55105 = ORIENTED_EDGE ( 'NONE', *, *, #15214, .F. ) ;
#55106 = CARTESIAN_POINT ( 'NONE',  ( 6.738288077784000407, 0.9869232226998000401, -1.278013103562000152 ) ) ;
#55107 = CARTESIAN_POINT ( 'NONE',  ( 10.94037390526893283, 9.311283358094208040, 6.235718259152663201 ) ) ;
#55108 = ADVANCED_FACE ( 'NONE', ( #39438 ), #63774, .F. ) ;
#55110 = CARTESIAN_POINT ( 'NONE',  ( 24.54223752976283635, -8.848832083081973110, 9.279389144537915968 ) ) ;
#55109 = CARTESIAN_POINT ( 'NONE',  ( 8.576768274605196751, -4.042014915351536786, 5.760874511329109104 ) ) ;
#55111 = CARTESIAN_POINT ( 'NONE',  ( 10.88813259637009878, 2.844182332072999753, -8.129798612793599943 ) ) ;
#55112 = ORIENTED_EDGE ( 'NONE', *, *, #48446, .F. ) ;
#55113 = CIRCLE ( 'NONE', #55064, 0.3000000000000004330 ) ;
#55114 = CARTESIAN_POINT ( 'NONE',  ( 10.29378083128999855, -3.483628580733000302, 6.176326635498999629 ) ) ;
#55115 = VERTEX_POINT ( 'NONE', #67029 ) ;
#55116 = ADVANCED_FACE ( 'NONE', ( #14590, #9325, #67706, #56893 ), #47094, .T. ) ;
#55117 = CARTESIAN_POINT ( 'NONE',  ( 9.406851002546000373, -2.832432432432000269, -6.822293592207000934 ) ) ;
#55118 = CARTESIAN_POINT ( 'NONE',  ( 16.13763077846600069, 3.625006537420000008, 11.03132468648999875 ) ) ;
#55119 = CARTESIAN_POINT ( 'NONE',  ( 18.14706097348721414, -0.2014071429975138050, -13.89805485625563364 ) ) ;
#55120 = ORIENTED_EDGE ( 'NONE', *, *, #37864, .F. ) ;
#55121 = CARTESIAN_POINT ( 'NONE',  ( 9.011117069441999305, -8.696115174831000161, 6.406018931393000493 ) ) ;
#55122 = DIRECTION ( 'NONE',  ( 0.9999999999997695177, 3.376118495992897870E-07, 5.889958325272817302E-07 ) ) ;
#55123 = DIRECTION ( 'NONE',  ( 0.000000000000000000, -0.7507612787780010288, -0.6605736161001442008 ) ) ;
#55124 = CARTESIAN_POINT ( 'NONE',  ( 8.202894943314811727, 2.713916317890099794, 7.026332083725589150 ) ) ;
#55125 = CARTESIAN_POINT ( 'NONE',  ( 18.17055204340471875, -2.609142802259613703, 12.42550174405653962 ) ) ;
#55126 = ORIENTED_EDGE ( 'NONE', *, *, #6941, .T. ) ;
#55127 = CARTESIAN_POINT ( 'NONE',  ( 8.599999952505998024, 3.250000006358199744, 7.500000000000000000 ) ) ;
#55128 = CARTESIAN_POINT ( 'NONE',  ( 23.73547072523399848, -13.39655754821999878, -3.630386468378000053 ) ) ;
#55129 = AXIS2_PLACEMENT_3D ( 'NONE', #40072, #35506, #39721 ) ;
#55130 = FACE_OUTER_BOUND ( 'NONE', #29530, .T. ) ;
#55131 = B_SPLINE_CURVE_WITH_KNOTS ( 'NONE', 3,
 ( #44993, #61743, #3017, #45680, #7234, #13863, #18076, #56505, #7928, #8611, #39746, #45338, #61066, #66298, #18423, #29959, #49885, #51262 ),
 .UNSPECIFIED., .F., .F.,
 ( 4, 2, 2, 2, 2, 2, 2, 2, 4 ),
 ( 0.000000000000000000, 0.1250000000000000000, 0.2500000000000000000, 0.3750000000000000000, 0.5000000000000000000, 0.6250000000000000000, 0.7500000000000000000, 0.8750000000000000000, 1.000000000000000000 ),
 .UNSPECIFIED. ) ;
#55132 = ORIENTED_EDGE ( 'NONE', *, *, #40725, .F. ) ;
#55133 = CARTESIAN_POINT ( 'NONE',  ( 23.76527359064235512, 13.07191039515678987, -3.759479379680037425 ) ) ;
#55134 = AXIS2_PLACEMENT_3D ( 'NONE', #69075, #26435, #20841 ) ;
#55135 = CARTESIAN_POINT ( 'NONE',  ( 10.90000000000000036, 5.167567567567999731, 6.822293592207000934 ) ) ;
#55136 = CARTESIAN_POINT ( 'NONE',  ( 10.91281046606773231, 2.900003320670894169, -5.078864280888942595 ) ) ;
#55137 = CARTESIAN_POINT ( 'NONE',  ( 5.000030787343000327, -1.290525307673963340, 1.679270695423618953 ) ) ;
#55138 = CARTESIAN_POINT ( 'NONE',  ( 11.59999999999999964, 4.000000000000000000, 7.500000000000000000 ) ) ;
#55139 = CARTESIAN_POINT ( 'NONE',  ( 6.002943173016874745, -1.199500263597274241, 0.9218200799623669228 ) ) ;
#55140 = CARTESIAN_POINT ( 'NONE',  ( 17.88706890093973811, -3.029615921040858861, 12.31227368058699412 ) ) ;
#55141 = ORIENTED_EDGE ( 'NONE', *, *, #55505, .F. ) ;
#55142 = CARTESIAN_POINT ( 'NONE',  ( 11.71922412107039868, -3.930460928605089777, -6.185573549454999487 ) ) ;
#55143 = ORIENTED_EDGE ( 'NONE', *, *, #19532, .F. ) ;
#55144 = CARTESIAN_POINT ( 'NONE',  ( 11.83148568236900111, -12.32826180562000040, -1.876276850727000012 ) ) ;
#55145 = CARTESIAN_POINT ( 'NONE',  ( 7.307500000000000107, 0.2500000000000000000, -3.149999999999999911 ) ) ;
#55146 = CARTESIAN_POINT ( 'NONE',  ( 3.509165847083000056, -1.664658919160000083, 2.940974452548000162 ) ) ;
#55147 = CARTESIAN_POINT ( 'NONE',  ( 9.753033816428001046, -4.922930220739999641, -8.639537379291999386 ) ) ;
#55148 = CARTESIAN_POINT ( 'NONE',  ( 10.66052890781999984, 2.899999999999999911, -6.152188490330000370 ) ) ;
#55149 = CARTESIAN_POINT ( 'NONE',  ( 9.580795537697435194, 5.100000000000000533, -6.662590550605531625 ) ) ;
#55150 = LINE ( 'NONE', #59702, #44545 ) ;
#55151 = EDGE_LOOP ( 'NONE', ( #51570, #15145, #13832, #52895 ) ) ;
#55152 = CARTESIAN_POINT ( 'NONE',  ( 1.931500749193666655, 0.2450796643850099987, -3.507702501826547081 ) ) ;
#55153 = CARTESIAN_POINT ( 'NONE',  ( 10.90333997687999990, -3.786145554879500441, 8.480416814141699788 ) ) ;
#55154 = CARTESIAN_POINT ( 'NONE',  ( 9.882259685352000389, 4.932708901218999742, 6.390989635557000170 ) ) ;
#55155 = CARTESIAN_POINT ( 'NONE',  ( 10.90000000164000049, 5.100000000007000267, 5.160242739040000082 ) ) ;
#55156 = TOROIDAL_SURFACE ( 'NONE', #64067, 12.20000000000000107, 0.6999999999999999556 ) ;
#55157 = CARTESIAN_POINT ( 'NONE',  ( 21.60000052036195584, 13.89999947951999992, 2.298222147633000150E-09 ) ) ;
#55158 = LINE ( 'NONE', #65980, #45137 ) ;
#55159 = VECTOR ( 'NONE', #65629, 999.9999999999998863 ) ;
#55160 = CARTESIAN_POINT ( 'NONE',  ( 10.97364560330029981, 4.265439025801100570, -6.675475461903199736 ) ) ;
#55161 = CARTESIAN_POINT ( 'NONE',  ( 10.21106069398042315, 5.731338304127999272, 7.738475558447463598 ) ) ;
#55162 = CARTESIAN_POINT ( 'NONE',  ( 8.975151519677000422, 4.027664626136379766, -8.778912113473998247 ) ) ;
#55163 = CARTESIAN_POINT ( 'NONE',  ( 24.38452337929200198, -8.887488439818000074, 8.991265583227999514 ) ) ;
#55164 = CARTESIAN_POINT ( 'NONE',  ( 8.113036307363870492, 5.051611909519712285, -6.499327669147922037 ) ) ;
#55165 = ORIENTED_EDGE ( 'NONE', *, *, #53784, .T. ) ;
#55166 = CARTESIAN_POINT ( 'NONE',  ( 8.464254440379999522, -2.029110377978999846, 7.726994002375999315 ) ) ;
#55167 = CARTESIAN_POINT ( 'NONE',  ( 9.842321917838999568, -3.423478821957000040, -6.068694811299999436 ) ) ;
#55168 = EDGE_CURVE ( 'NONE', #59694, #67173, #50960, .T. ) ;
#55169 = EDGE_CURVE ( 'NONE', #60390, #46623, #16551, .T. ) ;
#55170 = CARTESIAN_POINT ( 'NONE',  ( 18.27121482242686312, 2.402104771923904369, 13.79240553248645540 ) ) ;
#55171 = CARTESIAN_POINT ( 'NONE',  ( 23.61755490549040459, 3.309897709845488478, 13.56828019137976504 ) ) ;
#55172 = CARTESIAN_POINT ( 'NONE',  ( 10.76426088462129904, -3.997280690308189666, -6.221990224628999755 ) ) ;
#55173 = ORIENTED_EDGE ( 'NONE', *, *, #15611, .F. ) ;
#55174 = CARTESIAN_POINT ( 'NONE',  ( 25.52466892626799932, 2.886236140895999558, -11.27617498557999909 ) ) ;
#55175 = CARTESIAN_POINT ( 'NONE',  ( 9.250899447075999760, 4.135077451221000011, 9.175524215473998879 ) ) ;
#55177 = CARTESIAN_POINT ( 'NONE',  ( 10.97124174884019965, 3.963805917081910213, 6.184229974648999928 ) ) ;
#55176 = CARTESIAN_POINT ( 'NONE',  ( 8.696135841231001251, 3.038023536984999939, -5.861661709981000001 ) ) ;
#55178 = CARTESIAN_POINT ( 'NONE',  ( 3.494875605349273773, -2.878717222751967064, 1.196277934611101879 ) ) ;
#55179 = ORIENTED_EDGE ( 'NONE', *, *, #15101, .F. ) ;
#55180 = CARTESIAN_POINT ( 'NONE',  ( 9.687870098586998324, 5.912263966150999472, 7.772301113561999486 ) ) ;
#55181 = CARTESIAN_POINT ( 'NONE',  ( 18.16514092158340432, -2.912582788079554064, -13.69368340938387973 ) ) ;
#55182 = CARTESIAN_POINT ( 'NONE',  ( 10.25564828895399927, 4.880669054351300495, 7.018986873610899124 ) ) ;
#55183 = CARTESIAN_POINT ( 'NONE',  ( 10.46754921866999943, -2.318350880468999620, 6.549783596838000044 ) ) ;
#55184 = CARTESIAN_POINT ( 'NONE',  ( 7.762706781754004304, 3.200128145701000904, 6.302820412756005020 ) ) ;
#55186 = ORIENTED_EDGE ( 'NONE', *, *, #39002, .T. ) ;
#55185 = CIRCLE ( 'NONE', #42908, 10.80000000000000604 ) ;
#55187 = CARTESIAN_POINT ( 'NONE',  ( 24.66807826201145204, 12.30863159257428485, 2.982840176812266542 ) ) ;
#55188 = B_SPLINE_CURVE_WITH_KNOTS ( 'NONE', 3,
 ( #22180, #43520, #64819, #33027 ),
 .UNSPECIFIED., .F., .F.,
 ( 4, 4 ),
 ( 0.000000000000000000, 1.000000000000000000 ),
 .UNSPECIFIED. ) ;
#55189 = CARTESIAN_POINT ( 'NONE',  ( 10.76587944038000089, -3.166536971515000243, -8.574494061818999313 ) ) ;
#55190 = EDGE_CURVE ( 'NONE', #29277, #34148, #712, .T. ) ;
#55191 = B_SPLINE_CURVE_WITH_KNOTS ( 'NONE', 3,
 ( #10047, #25787, #31384, #37992, #52696, #42901, #31728, #47118 ),
 .UNSPECIFIED., .F., .F.,
 ( 4, 1, 1, 1, 1, 4 ),
 ( 0.000000000000000000, 0.2000000000000000111, 0.4000000000000000222, 0.5999999999999999778, 0.8000000000000000444, 1.000000000000000000 ),
 .UNSPECIFIED. ) ;
#55192 = CARTESIAN_POINT ( 'NONE',  ( 7.966778298513556678, -2.303323755512395543, 7.117734776878376302 ) ) ;
#55193 = CARTESIAN_POINT ( 'NONE',  ( 9.786673210037999837, -2.381198102024000285, 7.612749732462000374 ) ) ;
#55194 = CARTESIAN_POINT ( 'NONE',  ( 23.61708149841600246, 2.918613252417999515, 13.53488618919000075 ) ) ;
#55195 = CARTESIAN_POINT ( 'NONE',  ( 9.980671671056999372, -5.126041103316000047, 7.310881302803900361 ) ) ;
#55196 = EDGE_LOOP ( 'NONE', ( #35433, #14013, #58242, #28996 ) ) ;
#55197 = CARTESIAN_POINT ( 'NONE',  ( 23.71897706907673964, -9.886090438455083174, 9.463268644442225153 ) ) ;
#55198 = CARTESIAN_POINT ( 'NONE',  ( 11.97810404293059960, -4.563346034752700398, 6.352848032645000309 ) ) ;
#55199 = ORIENTED_EDGE ( 'NONE', *, *, #54128, .F. ) ;
#55200 = EDGE_CURVE ( 'NONE', #6243, #56839, #36483, .T. ) ;
#55201 = LINE ( 'NONE', #12553, #61863 ) ;
#55202 = ORIENTED_EDGE ( 'NONE', *, *, #60012, .T. ) ;
#55203 = B_SPLINE_SURFACE_WITH_KNOTS ( 'NONE', 1, 3, ( 
 ( #38677, #53720, #48477, #22587, #37632, #5817, #43580, #6156, #7807, #55709, #59301, #58617, #54407, #584, #32063, #27497, #10716, #53380, #27156, #16309, #17349, #43928, #37978, #48822, #21893, #26816, #64881, #43230, #59998, #54059, #236, #12109, #21213, #69107, #65234, #11404, #16994, #32743, #34393, #42543, #64194, #58966, #38322, #32404, #11070, #33091, #59652, #11749, #6508, #49159, #8840, #24578, #9514, #57073, #2899, #9174, #30512, #61632, #14777, #30179, #51485, #67903, #18646, #50456, #24229, #29500, #3581, #45901, #51824, #56044, #67211, #45568, #45221, #66526, #50807, #66873, #19677, #18985, #13748, #13410, #34732, #40311, #61293, #3922, #24916, #56393, #35080, #46248, #8496, #20020, #3249, #41345, #29844, #25259, #62657, #67554, #46598, #36096, #51152, #40998, #57411, #2557, #56744, #23885, #39980, #62323, #8154, #14437 ),
 ( #19324, #40648, #61982, #14092, #35758, #35418, #58792, #48302, #408, #26649, #46936, #42719, #62989, #9867, #52864, #52172, #30856, #47965, #41684, #10898, #21723, #43058, #64, #68238, #64023, #15118, #31211, #4965, #42033, #64361, #15464, #10211, #53553, #68582, #36790, #53205, #37130, #37814, #16485, #21049, #20360, #16144, #31545, #36437, #58449, #57755, #52515, #58111, #47281, #59135, #5644, #26298, #10551, #47626, #4614, #21386, #68936, #4273, #15802, #25948, #25608, #20705, #63336, #26986, #42381, #31894, #63687, #5307, #37466, #32244, #28722, #38502, #43759, #48652, #44466, #1450, #11238, #59827, #1106, #38862, #54588, #39549, #17883, #32918, #39202, #60524, #22418, #44803, #60183, #12289, #50039, #754, #32575, #54231, #59475, #33617, #6683, #12633, #16825, #28028, #6330, #5989, #27328, #11575, #27680, #49688, #48994, #65053 ) ),
 .UNSPECIFIED., .F., .F., .F.,
 ( 2, 2 ),
 ( 4, 2, 2, 2, 2, 2, 2, 2, 2, 2, 2, 2, 2, 2, 2, 2, 2, 2, 2, 2, 2, 2, 2, 2, 2, 2, 2, 2, 2, 2, 2, 2, 2, 2, 2, 2, 2, 2, 2, 2, 2, 2, 2, 2, 2, 2, 2, 2, 2, 2, 2, 2, 2, 4 ),
 ( 0.000000000000000000, 1.000000000000000000 ),
 ( 0.000000000000000000, 7.157214214794704388E-05, 0.0001431442842958940878, 0.0001789303553698675894, 0.0002147164264438411181, 0.0002326094619808278825, 0.0002505024975178146468, 0.0002862885685917881755, 0.0003220746396657616500, 0.0003578607107397351788, 0.0003936467818137087075, 0.0004294328528876822362, 0.0004652189239616557649, 0.0004831119594986425293, 0.0005010049950356292936, 0.0005725771371835763511, 0.0006441492793315233001, 0.0007157214214794703575, 0.0007872935636274174150, 0.0008588657057753644724, 0.0008946517768493380011, 0.0009304378479233115298, 0.0009662239189972850585, 0.001002009990071258587, 0.001037796061145232224, 0.001073582132219205645, 0.001145154274367152702, 0.001180940345441126339, 0.001216726416515099760, 0.001252512487589073180, 0.001288298558663046600, 0.001359870700810993658, 0.001395656771884967295, 0.001431442842958940715, 0.001467228914032914135, 0.001503014985106887772, 0.001574587127254834830, 0.001646159269402781887, 0.001681945340476755524, 0.001717731411550728945, 0.001753517482624702365, 0.001789303553698676002, 0.001860875695846623060, 0.001896661766920596480, 0.001932447837994570117, 0.001968233909068543754, 0.002004019980142517175, 0.002039806051216491029, 0.002075592122290464449, 0.002147164264438411289, 0.002182950335512384710, 0.002218736406586358130, 0.002254522477660331550, 0.002290308548734305404 ),
 .UNSPECIFIED. ) ;
#55204 = CARTESIAN_POINT ( 'NONE',  ( 9.600045280412000892, 3.021734963141999852, -6.070209284876999511 ) ) ;
#55205 = CARTESIAN_POINT ( 'NONE',  ( 10.97124174884019965, 3.963805917081910213, -8.815770025351000072 ) ) ;
#55206 = DIRECTION ( 'NONE',  ( 0.000000000000000000, 0.9835354258236025382, 0.1807154286440004198 ) ) ;
#55207 = CARTESIAN_POINT ( 'NONE',  ( 12.21409778435354809, 2.897922531322544515, -12.26223633105722044 ) ) ;
#55208 = CARTESIAN_POINT ( 'NONE',  ( 12.09603632436369125, -4.842640371965599932, 7.696781148700499564 ) ) ;
#55209 = CARTESIAN_POINT ( 'NONE',  ( 5.036746727192666029, -1.006919573152100789, 1.157429495210549941 ) ) ;
#55210 = AXIS2_PLACEMENT_3D ( 'NONE', #25590, #24561, #30838 ) ;
#55211 = ORIENTED_EDGE ( 'NONE', *, *, #38430, .T. ) ;
#55212 = DIRECTION ( 'NONE',  ( 0.000000000000000000, -0.8648648648648717963, -0.5020047465136829867 ) ) ;
#55213 = DIRECTION ( 'NONE',  ( -1.000000000000000000, 0.000000000000000000, 0.000000000000000000 ) ) ;
#55214 = ORIENTED_EDGE ( 'NONE', *, *, #35028, .T. ) ;
#55215 = B_SPLINE_SURFACE_WITH_KNOTS ( 'NONE', 1, 3, ( 
 ( #16277, #53002, #22208, #43545, #549, #20840, #37945, #58240, #5098, #201, #37602, #27125, #59267, #10685, #11370, #42852, #47414, #63474, #27462, #42512, #58933, #10345, #32711, #59617, #21861, #54021, #37263, #43198, #26434, #68719, #21181, #64845, #896, #21520, #32374, #26785, #47764, #64500, #6123, #32033, #63819, #11037, #16956, #42174, #53689, #64164, #11713, #33052, #4745, #15933, #26087, #15596, #5448, #53346, #48441, #18358, #50171, #40033, #23942, #27820, #28507, #49468, #49820, #1933, #28154, #1579, #22897, #44595, #44249, #34095, #65545, #55067, #60312, #18700, #12768, #23253, #12420, #6819, #55415, #60999, #33403, #29198, #7508, #55763, #34449, #2273 ),
 ( #23591, #18016, #61345, #50510, #17668, #65888, #39334, #43892, #44934, #60654, #66239, #13120, #38992, #13465, #1238, #7168, #28864, #22550, #39680, #7865, #54368, #33751, #2611, #45275, #66581, #6472, #65194, #49125, #17314, #38638, #59960, #12071, #54720, #8206, #67261, #29895, #41731, #57456, #24967, #36145, #57118, #46644, #3630, #35805, #14142, #8890, #9219, #52218, #50857, #24284, #67951, #45618, #3295, #56444, #20067, #34786, #51202, #14486, #24631, #14822, #25653, #46299, #2951, #20406, #41394, #45950, #40362, #51873, #4318, #63035, #67599, #9565, #46985, #30905, #66924, #3969, #62370, #19034, #19377, #40699, #62027, #8548, #19725, #68286, #62701, #56095 ) ),
 .UNSPECIFIED., .F., .F., .F.,
 ( 2, 2 ),
 ( 4, 2, 2, 2, 2, 2, 2, 2, 2, 2, 2, 2, 2, 2, 2, 2, 2, 2, 2, 2, 2, 2, 2, 2, 2, 2, 2, 2, 2, 2, 2, 2, 2, 2, 2, 2, 2, 2, 2, 2, 2, 2, 4 ),
 ( 0.000000000000000000, 1.000000000000000000 ),
 ( 0.000000000000000000, 7.083094307561030529E-05, 0.0001416618861512206106, 0.0002124928292268309159, 0.0002833237723024412211, 0.0003541547153780515264, 0.0004249856584536618317, 0.0004958166015292721912, 0.0005666475446048824423, 0.0006374784876804926934, 0.0007083094307561030529, 0.0007791403738317134123, 0.0008145558453695185379, 0.0008499713169073236634, 0.0008853867884451287890, 0.0009208022599829340229, 0.0009916332030585443824, 0.001027048674596349508, 0.001062464146134154633, 0.001097879617671959759, 0.001133295089209764885, 0.001204126032285375136, 0.001239541503823180261, 0.001274956975360985387, 0.001310372446898790512, 0.001345787918436595638, 0.001416618861512206106, 0.001487449804587816574, 0.001522865276125621699, 0.001558280747663426825, 0.001629111690739037076, 0.001699942633814647327, 0.001735358105352452452, 0.001770773576890257578, 0.001806189048428062920, 0.001841604519965868046, 0.001912435463041478514, 0.001983266406117088765, 0.002018681877654893674, 0.002054097349192699016, 0.002124928292268309267, 0.002195759235343919518, 0.002266590178419529769 ),
 .UNSPECIFIED. ) ;
#55216 = CARTESIAN_POINT ( 'NONE',  ( 12.28024471298230047, -1.983745382141950397, -12.44286253672009757 ) ) ;
#55217 = CARTESIAN_POINT ( 'NONE',  ( 11.35918179236250047, 3.761636028845500412, 8.615559381441000752 ) ) ;
#55218 = DIRECTION ( 'NONE',  ( -1.000000000000000000, 0.000000000000000000, 0.000000000000000000 ) ) ;
#55219 = CARTESIAN_POINT ( 'NONE',  ( 10.52343057594999998, 3.209665745824000105, -9.177097971982000502 ) ) ;
#55220 = CARTESIAN_POINT ( 'NONE',  ( 18.38280243546500259, -11.68827787447999889, 4.347381705584999700 ) ) ;
#55221 = CARTESIAN_POINT ( 'NONE',  ( 9.099999931440999390, 5.246365646610000155, -7.404749409716440134 ) ) ;
#55222 = CARTESIAN_POINT ( 'NONE',  ( 12.35432851685907707, -2.933105360581562682, -13.57195094675648228 ) ) ;
#55223 = CARTESIAN_POINT ( 'NONE',  ( 18.11801110581809127, -0.2715269968477674323, -12.69609476950841831 ) ) ;
#55224 = CARTESIAN_POINT ( 'NONE',  ( 5.000000000000000000, 0.2999999999999999889, -3.149999999999999911 ) ) ;
#55225 = CARTESIAN_POINT ( 'NONE',  ( 10.79303032197930001, -3.336467919271199900, -6.572090902022299730 ) ) ;
#55226 = CARTESIAN_POINT ( 'NONE',  ( 8.572267219592999865, 2.606995215518000286, 6.345762205468999717 ) ) ;
#55227 = VERTEX_POINT ( 'NONE', #40808 ) ;
#55228 = AXIS2_PLACEMENT_3D ( 'NONE', #53322, #47391, #37573 ) ;
#55229 = CARTESIAN_POINT ( 'NONE',  ( 11.60000000000000142, -4.471166781226291853, -8.438845841270557813 ) ) ;
#55230 = CARTESIAN_POINT ( 'NONE',  ( 4.599999999999999645, 0.000000000000000000, 0.000000000000000000 ) ) ;
#55231 = CARTESIAN_POINT ( 'NONE',  ( 11.24053267693000002, 2.774035422596999645, 6.782113650547000105 ) ) ;
#55232 = CARTESIAN_POINT ( 'NONE',  ( 24.15441502362300241, -3.593679633234999837, 12.72319232787999965 ) ) ;
#55233 = VECTOR ( 'NONE', #36463, 999.9999999999998863 ) ;
#55234 = CARTESIAN_POINT ( 'NONE',  ( 17.86124198984730782, 1.955044089803213536, 12.56196094884553105 ) ) ;
#55235 = EDGE_CURVE ( 'NONE', #42164, #53044, #1448, .T. ) ;
#55236 = CARTESIAN_POINT ( 'NONE',  ( 18.35167777225700192, 2.962063834667000073, -12.02051524900000068 ) ) ;
#55237 = ADVANCED_FACE ( 'NONE', ( #62130 ), #8992, .T. ) ;
#55238 = CARTESIAN_POINT ( 'NONE',  ( 9.305881816721999655, 4.945299866898000829, 9.077891794505999812 ) ) ;
#55239 = CARTESIAN_POINT ( 'NONE',  ( 10.10683733959362662, -4.864872534707646246, 7.632392475727677095 ) ) ;
#55240 = CARTESIAN_POINT ( 'NONE',  ( 8.770072224255999416, 4.093776898754200033, 6.613913699222099041 ) ) ;
#55241 = VERTEX_POINT ( 'NONE', #20516 ) ;
#55242 = CARTESIAN_POINT ( 'NONE',  ( 12.08521996405951171, -2.390121770085883668, 12.37125191860131501 ) ) ;
#55243 = B_SPLINE_CURVE_WITH_KNOTS ( 'NONE', 3,
 ( #38584, #22496, #51070, #44197 ),
 .UNSPECIFIED., .F., .F.,
 ( 4, 4 ),
 ( 0.000000000000000000, 1.000000000000000000 ),
 .UNSPECIFIED. ) ;
#55244 = CARTESIAN_POINT ( 'NONE',  ( 9.781659112603998452, -4.436443689698799986, -8.404632083253700259 ) ) ;
#55245 = CARTESIAN_POINT ( 'NONE',  ( 24.53002386606100060, -3.319300011433999664, -12.04488764000000067 ) ) ;
#55246 = VECTOR ( 'NONE', #59330, 1000.000000000000114 ) ;
#55247 = DIRECTION ( 'NONE',  ( 1.000000000000000000, 0.000000000000000000, 0.000000000000000000 ) ) ;
#55248 = CARTESIAN_POINT ( 'NONE',  ( 10.98579841651039857, 3.550031058388499972, -8.696179055230999211 ) ) ;
#55249 = CARTESIAN_POINT ( 'NONE',  ( 12.61664271790067282, -0.6949735217938508569, 12.58082105808780682 ) ) ;
#55250 = B_SPLINE_CURVE_WITH_KNOTS ( 'NONE', 3,
 ( #32370, #6119, #22545, #33399 ),
 .UNSPECIFIED., .F., .F.,
 ( 4, 4 ),
 ( 0.000000000000000000, 1.000000000000000000 ),
 .UNSPECIFIED. ) ;
#55251 = CARTESIAN_POINT ( 'NONE',  ( 7.892607780408998686, 5.480308727866000318, 8.192324747680999053 ) ) ;
#55252 = CARTESIAN_POINT ( 'NONE',  ( 5.000000000000000000, -1.382741116750999977, 11.26545724788999969 ) ) ;
#55253 = CARTESIAN_POINT ( 'NONE',  ( 12.18778960455903082, 2.401422506651157196, 12.47398279053984460 ) ) ;
#55254 = ORIENTED_EDGE ( 'NONE', *, *, #22214, .T. ) ;
#55255 = CARTESIAN_POINT ( 'NONE',  ( 25.26979906455200009, 8.566782599371000728, 7.890677837420999374 ) ) ;
#55256 = CARTESIAN_POINT ( 'NONE',  ( 11.23195122972050086, 4.507250159094099651, -6.326963915009999440 ) ) ;
#55257 = EDGE_CURVE ( 'NONE', #21413, #26398, #4426, .T. ) ;
#55258 = EDGE_CURVE ( 'NONE', #32335, #16280, #40573, .T. ) ;
#55259 = CARTESIAN_POINT ( 'NONE',  ( 5.428010115736667807, 0.04029576578756271371, 1.517272597181324567 ) ) ;
#55261 = CARTESIAN_POINT ( 'NONE',  ( 17.77470270346956482, -0.5852243768284137726, 12.68184418015406223 ) ) ;
#55260 = CARTESIAN_POINT ( 'NONE',  ( 8.111566940377999302, -3.326257819185999942, 8.794522506294001118 ) ) ;
#55262 = CARTESIAN_POINT ( 'NONE',  ( 9.932025935145999185, -4.145841638824199649, 8.493766832166899761 ) ) ;
#55263 = CARTESIAN_POINT ( 'NONE',  ( 10.43210941423799909, -3.358814833524500276, -6.917608226833099394 ) ) ;
#55264 = EDGE_LOOP ( 'NONE', ( #19290, #41607, #58751, #14739, #63823, #22285 ) ) ;
#55265 = EDGE_CURVE ( 'NONE', #69025, #60711, #12217, .T. ) ;
#55266 = CARTESIAN_POINT ( 'NONE',  ( 1.591565493715000112, -3.424908732075000017, 0.06941761548046999908 ) ) ;
#55267 = CARTESIAN_POINT ( 'NONE',  ( 18.29983863915590803, 1.925365864301426200, 12.21183829863293724 ) ) ;
#55268 = DIRECTION ( 'NONE',  ( 0.000000000000000000, 0.9553735099700839672, 0.2954005017724949389 ) ) ;
#55269 = CARTESIAN_POINT ( 'NONE',  ( 18.08128123659606246, -2.837338021487807893, 13.59610410466120278 ) ) ;
#55270 = B_SPLINE_CURVE_WITH_KNOTS ( 'NONE', 3,
 ( #35003, #2823, #3845, #45488, #40240, #14362, #29421, #66803, #35345, #67136, #67821, #60872, #51071, #29074, #46172, #61558, #23809, #19247 ),
 .UNSPECIFIED., .F., .F.,
 ( 4, 2, 2, 2, 2, 2, 2, 2, 4 ),
 ( 0.000000000000000000, 0.1250000000000000000, 0.2500000000000000000, 0.3750000000000000000, 0.5000000000000000000, 0.6250000000000000000, 0.7500000000000000000, 0.8750000000000000000, 1.000000000000000000 ),
 .UNSPECIFIED. ) ;
#55271 = CARTESIAN_POINT ( 'NONE',  ( 8.717397846562217723, 3.754687009553120181, -8.340771899786949106 ) ) ;
#55272 = CARTESIAN_POINT ( 'NONE',  ( 12.15817878876227809, -2.188143349582273078, 13.82794795582454306 ) ) ;
#55273 = CARTESIAN_POINT ( 'NONE',  ( 10.89182487123000165, 2.946653980248000071, 5.014777219802000197 ) ) ;
#55274 = CARTESIAN_POINT ( 'NONE',  ( 11.09999999999999964, 5.350000000000000533, -7.500000000000000000 ) ) ;
#55275 = CARTESIAN_POINT ( 'NONE',  ( 10.08521345716899908, -3.075109701058799772, -8.340879262988799780 ) ) ;
#55276 = VERTEX_POINT ( 'NONE', #67365 ) ;
#55277 = CARTESIAN_POINT ( 'NONE',  ( 6.992001042874380623, 4.037115771921000018, -6.023232697733999608 ) ) ;
#55278 = LINE ( 'NONE', #40567, #48519 ) ;
#55279 = CARTESIAN_POINT ( 'NONE',  ( 18.11654246898725518, 2.224740281524702823, -13.72801203775192036 ) ) ;
#55280 = LINE ( 'NONE', #52945, #50347 ) ;
#55281 = CARTESIAN_POINT ( 'NONE',  ( 1.895840275625999771, -0.3183524953527000489, -3.745328979271999703 ) ) ;
#55282 = EDGE_LOOP ( 'NONE', ( #57620, #37377, #21658, #16445 ) ) ;
#55283 = FACE_OUTER_BOUND ( 'NONE', #11025, .T. ) ;
#55284 = ADVANCED_FACE ( 'NONE', ( #35578 ), #20170, .F. ) ;
#55285 = DIRECTION ( 'NONE',  ( 0.000000000000000000, 0.9916377111174248249, -0.1290528957048032721 ) ) ;
#55286 = CARTESIAN_POINT ( 'NONE',  ( 9.727255459545908423, -3.370461114521380530, 8.592254274082836929 ) ) ;
#55287 = VECTOR ( 'NONE', #11386, 1000.000000000000000 ) ;
#55288 = CARTESIAN_POINT ( 'NONE',  ( 10.99410672858429905, 3.198097575668700010, 8.103244025831999764 ) ) ;
#55289 = CARTESIAN_POINT ( 'NONE',  ( 18.50001572531400029, -2.908166856580999937, 12.18270046149000052 ) ) ;
#55290 = CARTESIAN_POINT ( 'NONE',  ( 5.500000000595999694, -0.4999999994045000173, 3.150000007847999939 ) ) ;
#55291 = CARTESIAN_POINT ( 'NONE',  ( 21.60000000000000142, 12.52500000000000036, 0.000000000000000000 ) ) ;
#55292 = CARTESIAN_POINT ( 'NONE',  ( 9.432072800716166938, 10.28058112649079803, 4.885051702730572210 ) ) ;
#55293 = CARTESIAN_POINT ( 'NONE',  ( 12.29679984375326285, -2.863892094194480986, 12.35932590994786295 ) ) ;
#55294 = EDGE_LOOP ( 'NONE', ( #23043, #16397, #64697, #52356, #7522, #40964 ) ) ;
#55295 = CARTESIAN_POINT ( 'NONE',  ( 10.98768503802999952, -8.067884818888000353, -6.818830313157000056 ) ) ;
#55296 = EDGE_LOOP ( 'NONE', ( #34003, #9473, #46626, #56390 ) ) ;
#55297 = CARTESIAN_POINT ( 'NONE',  ( 18.09820959019767628, -2.190632709185573290, 13.73422630893085916 ) ) ;
#55298 = CARTESIAN_POINT ( 'NONE',  ( 11.01041369783139956, -4.064477673403060543, -8.776385133971000840 ) ) ;
#55299 = VERTEX_POINT ( 'NONE', #22234 ) ;
#55300 = CARTESIAN_POINT ( 'NONE',  ( 24.83136278930371432, -3.060660479504548892, -11.69612704205236398 ) ) ;
#55301 = CARTESIAN_POINT ( 'NONE',  ( 4.149992563292000725, 1.599290730647370484, -1.229060429538527899 ) ) ;
#55302 = CARTESIAN_POINT ( 'NONE',  ( 8.726967411678998587, -4.064442376558529801, -8.391190439313799487 ) ) ;
#55303 = FACE_OUTER_BOUND ( 'NONE', #33230, .T. ) ;
#55304 = CARTESIAN_POINT ( 'NONE',  ( 12.61333915124458116, -3.228660600416717319, -13.62267210747915058 ) ) ;
#55305 = CARTESIAN_POINT ( 'NONE',  ( 10.87309687351658205, -5.217465845835394411, 7.827184855449101697 ) ) ;
#55306 = DIRECTION ( 'NONE',  ( -1.000000000000000000, 0.000000000000000000, 0.000000000000000000 ) ) ;
#55307 = CARTESIAN_POINT ( 'NONE',  ( 10.94349328348999961, -3.081618981425999770, -8.919377696680001577 ) ) ;
#55308 = CARTESIAN_POINT ( 'NONE',  ( 4.000000000000000000, -0.2816038378556623978, -2.149891155406186805 ) ) ;
#55309 = SURFACE_STYLE_FILL_AREA ( #45518 ) ;
#55310 = ORIENTED_EDGE ( 'NONE', *, *, #27056, .F. ) ;
#55311 = CARTESIAN_POINT ( 'NONE',  ( 11.36486084871759950, 2.792989229543000107, 7.174999999999999822 ) ) ;
#55312 = CARTESIAN_POINT ( 'NONE',  ( 10.90000000011000125, 5.100000000110999743, 6.571291220762999430 ) ) ;
#55313 = CARTESIAN_POINT ( 'NONE',  ( 10.25832651750999958, -4.639457704266000349, 4.530776779397999832 ) ) ;
#55314 = LINE ( 'NONE', #14049, #36144 ) ;
#55315 = CARTESIAN_POINT ( 'NONE',  ( 9.227255459545908423, 4.629538885478623911, 8.592254274082833376 ) ) ;
#55316 = ADVANCED_FACE ( 'NONE', ( #37622 ), #22212, .T. ) ;
#55317 = CARTESIAN_POINT ( 'NONE',  ( 12.58303802678790362, 1.915668549203846993, 13.78011653961192096 ) ) ;
#55318 = EDGE_CURVE ( 'NONE', #36490, #65063, #27489, .T. ) ;
#55319 = CARTESIAN_POINT ( 'NONE',  ( 10.72520823780999955, -5.521647200017000934, 6.612992938078999572 ) ) ;
#55320 = ORIENTED_EDGE ( 'NONE', *, *, #33756, .F. ) ;
#55321 = CARTESIAN_POINT ( 'NONE',  ( 24.35365242081700288, -8.355077740067001102, -8.511587483820997946 ) ) ;
#55322 = EDGE_CURVE ( 'NONE', #47655, #29725, #56427, .T. ) ;
#55323 = CARTESIAN_POINT ( 'NONE',  ( 12.08466087602983841, 0.08309727575450238934, 13.99975851644561864 ) ) ;
#55324 = ORIENTED_EDGE ( 'NONE', *, *, #59174, .F. ) ;
#55325 = CARTESIAN_POINT ( 'NONE',  ( 0.000000000000000000, 0.000000000000000000, 0.000000000000000000 ) ) ;
#55326 = CARTESIAN_POINT ( 'NONE',  ( 18.50003594167399967, 2.686563651857999613, 11.33603604486000016 ) ) ;
#55327 = CARTESIAN_POINT ( 'NONE',  ( 24.42274717983899990, -3.752455261644000117, -12.53779156268999984 ) ) ;
#55328 = DIRECTION ( 'NONE',  ( 1.000000000000000000, 0.000000000000000000, 0.000000000000000000 ) ) ;
#55329 = CARTESIAN_POINT ( 'NONE',  ( 9.029445280412998542, 5.442817578555000146, -8.106149115450000053 ) ) ;
#55330 = AXIS2_PLACEMENT_3D ( 'NONE', #27324, #53550, #43414 ) ;
#55331 = DIRECTION ( 'NONE',  ( -1.000000000000000000, 0.000000000000000000, 0.000000000000000000 ) ) ;
#55332 = CARTESIAN_POINT ( 'NONE',  ( 10.59999999999999964, 4.599999999999999645, -4.756097560976000338 ) ) ;
#55333 = CARTESIAN_POINT ( 'NONE',  ( 6.992190918810999634, -9.194554705909000702, -5.189167530940999917 ) ) ;
#55334 = DIRECTION ( 'NONE',  ( 0.000000000000000000, 0.7455306007789014311, 0.6664713972124013397 ) ) ;
#55335 = SURFACE_STYLE_USAGE ( .BOTH. , #12685 ) ;
#55336 = CARTESIAN_POINT ( 'NONE',  ( 9.749327024990000368, -5.634417356902000407, -7.003562403358999156 ) ) ;
#55337 = CARTESIAN_POINT ( 'NONE',  ( 11.44133594839949986, 4.569506585117100173, -6.847343244997600387 ) ) ;
#55338 = CARTESIAN_POINT ( 'NONE',  ( 1.198890132541874598, -2.798833948393640192, 2.150913519912191152 ) ) ;
#55339 = CARTESIAN_POINT ( 'NONE',  ( 10.43614141025499897, 4.549633050978300730, -8.478951440767898973 ) ) ;
#55340 = CARTESIAN_POINT ( 'NONE',  ( 8.976101285863999024, 3.353260484332500013, -6.731514281717299930 ) ) ;
#55342 = CARTESIAN_POINT ( 'NONE',  ( 11.00478015909000007, -2.938058373007000235, 5.194088448331000585 ) ) ;
#55341 = CARTESIAN_POINT ( 'NONE',  ( 15.91802873821099951, -8.603382153815999800, -8.072764124688998066 ) ) ;
#55343 = CARTESIAN_POINT ( 'NONE',  ( 11.21684687351633869, -3.231816600031351516, 8.499583552997721725 ) ) ;
#55344 = ORIENTED_EDGE ( 'NONE', *, *, #8303, .F. ) ;
#55345 = ADVANCED_FACE ( 'NONE', ( #47789 ), #575, .F. ) ;
#55346 = CARTESIAN_POINT ( 'NONE',  ( 10.76857802013509868, 2.825431102905000103, 7.527343341769989316 ) ) ;
#55347 = CARTESIAN_POINT ( 'NONE',  ( 11.02786767503999954, -5.596230239120999705, 7.209501483790000442 ) ) ;
#55348 = CARTESIAN_POINT ( 'NONE',  ( 9.125113844317997547, 4.288351516201100111, 8.604802177355001191 ) ) ;
#55349 = FACE_OUTER_BOUND ( 'NONE', #13496, .T. ) ;
#55350 = CARTESIAN_POINT ( 'NONE',  ( 9.600494040286998043, -5.206548117663999165, 8.585114612872999373 ) ) ;
#55351 = FACE_OUTER_BOUND ( 'NONE', #16227, .T. ) ;
#55353 = UNCERTAINTY_MEASURE_WITH_UNIT (LENGTH_MEASURE( 1.000000000000000082E-05 ), #65933, 'distance_accuracy_value', 'NONE');
#55352 = CARTESIAN_POINT ( 'NONE',  ( 11.64585080655600002, 3.555558855182999967, -11.95257446901999998 ) ) ;
#55354 = ORIENTED_EDGE ( 'NONE', *, *, #63982, .F. ) ;
#55355 = VECTOR ( 'NONE', #16086, 1000.000000000000000 ) ;
#55356 = CARTESIAN_POINT ( 'NONE',  ( 8.923430433046998900, -4.971677342931100085, -6.900352112302299723 ) ) ;
#55357 = FACE_OUTER_BOUND ( 'NONE', #14539, .T. ) ;
#55358 = CARTESIAN_POINT ( 'NONE',  ( 5.901648365476000357, 1.388436026523999889, -0.4783021510498000062 ) ) ;
#55359 = EDGE_CURVE ( 'NONE', #66683, #37746, #63084, .T. ) ;
#55360 = CARTESIAN_POINT ( 'NONE',  ( 7.000000000000000000, 10.80467228076000019, -3.475853456584999890 ) ) ;
#55361 = VECTOR ( 'NONE', #6666, 1000.000000000000000 ) ;
#55362 = CARTESIAN_POINT ( 'NONE',  ( 11.49999672495000524, 10.70720904779669524, -4.749689352253906982 ) ) ;
#55363 = CARTESIAN_POINT ( 'NONE',  ( 10.50595525820100029, 3.918212119278319694, -6.637672143048099827 ) ) ;
#55364 = CARTESIAN_POINT ( 'NONE',  ( 12.18203530712867177, 2.449198598598032461, -13.68410320367736155 ) ) ;
#55365 = CARTESIAN_POINT ( 'NONE',  ( 9.392147628284998717, -2.890602650755999647, -6.682694598879999504 ) ) ;
#55366 = DIRECTION ( 'NONE',  ( 0.000000000000000000, 1.000000000000000000, 0.000000000000000000 ) ) ;
#55367 = ORIENTED_EDGE ( 'NONE', *, *, #5087, .T. ) ;
#55368 = DIRECTION ( 'NONE',  ( -0.8660254037844974384, 0.000000000000000000, 0.4999999999998981925 ) ) ;
#55369 = CARTESIAN_POINT ( 'NONE',  ( 12.08123665194307073, 0.04806343339260338993, -13.99993753789457962 ) ) ;
#55370 = DIRECTION ( 'NONE',  ( 0.000000000000000000, 0.9421243786071877846, 0.3352635608502961828 ) ) ;
#55371 = CARTESIAN_POINT ( 'NONE',  ( 23.66004879239100234, 0.000000000000000000, 0.000000000000000000 ) ) ;
#55372 = CARTESIAN_POINT ( 'NONE',  ( 13.46547102624232117, -11.49951335169909683, -1.866756745165379483 ) ) ;
#55373 = CARTESIAN_POINT ( 'NONE',  ( 7.100000000000000533, 0.000000000000000000, 0.000000000000000000 ) ) ;
#55374 = FACE_OUTER_BOUND ( 'NONE', #9201, .T. ) ;
#55375 = VERTEX_POINT ( 'NONE', #32397 ) ;
#55376 = AXIS2_PLACEMENT_3D ( 'NONE', #41665, #52147, #10194 ) ;
#55377 = CARTESIAN_POINT ( 'NONE',  ( 18.01376003089016109, 2.074995895013257652, -13.75447352907418974 ) ) ;
#55378 = ORIENTED_EDGE ( 'NONE', *, *, #39223, .F. ) ;
#55379 = CARTESIAN_POINT ( 'NONE',  ( 8.115081613917173087, 5.350113345104855256, -7.499995474391613293 ) ) ;
#55380 = CARTESIAN_POINT ( 'NONE',  ( 8.674245559624999657, -5.983034890242000081, 7.440798487724999966 ) ) ;
#55381 = AXIS2_PLACEMENT_3D ( 'NONE', #49892, #12144, #11439 ) ;
#55382 = CARTESIAN_POINT ( 'NONE',  ( 8.323770280408998801, 5.332332124071999857, -8.487089944253000340 ) ) ;
#55383 = B_SPLINE_CURVE_WITH_KNOTS ( 'NONE', 3,
 ( #60987, #2595, #56084, #57362, #55398, #2939, #44582, #13452, #65530, #23577 ),
 .UNSPECIFIED., .F., .F.,
 ( 4, 2, 2, 2, 4 ),
 ( 0.000000000000000000, 0.2500000000000001665, 0.3750000000000004996, 0.5000000000000007772, 1.000000000000000000 ),
 .UNSPECIFIED. ) ;
#55384 = CARTESIAN_POINT ( 'NONE',  ( 11.60391045180384317, -2.870950512581996961, 6.885461205208885715 ) ) ;
#55385 = CARTESIAN_POINT ( 'NONE',  ( 11.55300581613033906, -2.892415530317000272, -8.211208432468300344 ) ) ;
#55386 = CARTESIAN_POINT ( 'NONE',  ( 9.327567085901730337, -5.070068301512486997, -6.253587086782717464 ) ) ;
#55387 = CARTESIAN_POINT ( 'NONE',  ( 11.30000000000000071, -11.28618258042000022, -10.08934826511999994 ) ) ;
#55388 = ORIENTED_EDGE ( 'NONE', *, *, #12418, .F. ) ;
#55389 = DIRECTION ( 'NONE',  ( 1.000000000000000000, 0.000000000000000000, 0.000000000000000000 ) ) ;
#55390 = DIRECTION ( 'NONE',  ( 0.000000000000000000, -1.000000000000000000, 0.000000000000000000 ) ) ;
#55391 = CARTESIAN_POINT ( 'NONE',  ( 9.146614158775999925, 2.981992329588000423, -5.895876591910999664 ) ) ;
#55392 = ORIENTED_EDGE ( 'NONE', *, *, #55579, .T. ) ;
#55393 = CARTESIAN_POINT ( 'NONE',  ( 10.33022126302999943, 2.650190549566000087, -7.694579890082000162 ) ) ;
#55394 = CARTESIAN_POINT ( 'NONE',  ( 11.03775575519999919, -8.050335494570999728, 6.914609630061999468 ) ) ;
#55395 = ORIENTED_EDGE ( 'NONE', *, *, #22558, .T. ) ;
#55396 = CARTESIAN_POINT ( 'NONE',  ( 9.786633995697998856, 4.998281561686200192, 7.389201877599999690 ) ) ;
#55397 = CARTESIAN_POINT ( 'NONE',  ( 18.27481983568693380, -2.390134998303168778, -12.37124935920179070 ) ) ;
#55398 = CARTESIAN_POINT ( 'NONE',  ( 10.99284065376738795, 5.922215992749499058, -5.009257842713325637 ) ) ;
#55399 = CARTESIAN_POINT ( 'NONE',  ( 19.89999966725400071, 12.52499966719000035, 3.709624234311000015E-10 ) ) ;
#55400 = CARTESIAN_POINT ( 'NONE',  ( 11.83979429613600232, -11.64688653560999931, -1.860528257274000064 ) ) ;
#55401 = ADVANCED_FACE ( 'NONE', ( #64872 ), #63499, .F. ) ;
#55402 = EDGE_CURVE ( 'NONE', #52040, #63838, #48121, .T. ) ;
#55403 = B_SPLINE_CURVE_WITH_KNOTS ( 'NONE', 3,
 ( #13823, #24305, #30251, #40382 ),
 .UNSPECIFIED., .F., .F.,
 ( 4, 4 ),
 ( 0.000000000000000000, 0.1254282067584606419 ),
 .UNSPECIFIED. ) ;
#55404 = CARTESIAN_POINT ( 'NONE',  ( 9.408709346416998187, 4.783195203880800328, 7.871904849557299855 ) ) ;
#55405 = EDGE_CURVE ( 'NONE', #27697, #31394, #21542, .T. ) ;
#55406 = EDGE_CURVE ( 'NONE', #21093, #21223, #13098, .T. ) ;
#55407 = CARTESIAN_POINT ( 'NONE',  ( 9.409668643352913975, -2.474094513855759736, 8.334984523595771577 ) ) ;
#55408 = EDGE_LOOP ( 'NONE', ( #27578, #3888, #2837, #61506, #24857, #18204, #6725, #20223, #16755 ) ) ;
#55409 = CARTESIAN_POINT ( 'NONE',  ( 8.228673373757093401, -4.831901240730346103, 6.190044060663523418 ) ) ;
#55410 = CARTESIAN_POINT ( 'NONE',  ( 10.77401721959000014, 3.826866801954999620, -5.823193568970000733 ) ) ;
#55411 = CARTESIAN_POINT ( 'NONE',  ( 8.789886373836322875, 4.000007821194420110, 6.560153657526067938 ) ) ;
#55412 = CARTESIAN_POINT ( 'NONE',  ( 12.21285350005639536, 2.096151405059777151, -13.84220188050173839 ) ) ;
#55413 = DIRECTION ( 'NONE',  ( 1.000000000000000000, 0.000000000000000000, 0.000000000000000000 ) ) ;
#55414 = CARTESIAN_POINT ( 'NONE',  ( 24.77999297203200157, 3.612935283031999845, 12.08260076442999953 ) ) ;
#55415 = CARTESIAN_POINT ( 'NONE',  ( 17.74610569661007631, 0.5951713840684285106, 13.88284414672552991 ) ) ;
#55416 = CIRCLE ( 'NONE', #18593, 12.35000000006999876 ) ;
#55417 = CARTESIAN_POINT ( 'NONE',  ( 17.69618303683414240, 0.6091729397312527494, 13.88202727520882540 ) ) ;
#55418 = EDGE_LOOP ( 'NONE', ( #52726, #47116, #8464, #62859, #48224 ) ) ;
#55419 = ORIENTED_EDGE ( 'NONE', *, *, #30844, .F. ) ;
#55420 = CARTESIAN_POINT ( 'NONE',  ( 9.693589158772999426, 4.047146749018000200, -5.600703114891000034 ) ) ;
#55421 = CARTESIAN_POINT ( 'NONE',  ( 10.72510394928771227, -2.650147065043205519, 7.500007457243348163 ) ) ;
#55422 = CARTESIAN_POINT ( 'NONE',  ( 12.21427240548824500, -2.704226675393127888, 13.62802533672049954 ) ) ;
#55424 = CARTESIAN_POINT ( 'NONE',  ( 8.348093183609000434, 4.599999999999999645, -6.056236567608999977 ) ) ;
#55423 = SHAPE_REPRESENTATION ( 'Terminal Screw 3', ( #9676 ), #52154 ) ;
#55425 = EDGE_CURVE ( 'NONE', #44911, #31943, #65781, .T. ) ;
#55426 = CARTESIAN_POINT ( 'NONE',  ( 8.732394353210001015, -2.806079842068999852, 8.615883328687999665 ) ) ;
#55427 = LINE ( 'NONE', #44944, #35995 ) ;
#55429 = CARTESIAN_POINT ( 'NONE',  ( 11.12483852207999924, -6.576352438315999471, 5.637707935939000770 ) ) ;
#55428 = CARTESIAN_POINT ( 'NONE',  ( 10.23502593514599823, -4.185743043590700374, 8.765655525501999890 ) ) ;
#55430 = CARTESIAN_POINT ( 'NONE',  ( 10.51810807141099779, 4.059045408506610109, -8.776647962565998995 ) ) ;
#55431 = ORIENTED_EDGE ( 'NONE', *, *, #9311, .T. ) ;
#55432 = CARTESIAN_POINT ( 'NONE',  ( 8.455992358763001704, 3.399999999999999911, -6.571291218977999726 ) ) ;
#55433 = CARTESIAN_POINT ( 'NONE',  ( 23.56666365135700403, -11.61524011585000160, -3.333188920242000197 ) ) ;
#55434 = CARTESIAN_POINT ( 'NONE',  ( 17.86819591275964214, 0.5409888710114112431, 12.68448745112149467 ) ) ;
#55435 = CARTESIAN_POINT ( 'NONE',  ( 25.44994642811700203, 0.000000000000000000, 2.140509991476999645E-13 ) ) ;
#55436 = CARTESIAN_POINT ( 'NONE',  ( 18.13163533201626620, -2.741228481684170770, -12.39208274280229993 ) ) ;
#55437 = EDGE_LOOP ( 'NONE', ( #15014, #54025, #2390, #3644 ) ) ;
#55439 = CARTESIAN_POINT ( 'NONE',  ( 10.99375810342578141, 4.001859925960030928, 8.374120210831636157 ) ) ;
#55438 = CARTESIAN_POINT ( 'NONE',  ( 8.738433059624998833, -5.414909314743000301, 8.890670256079998168 ) ) ;
#55440 = CARTESIAN_POINT ( 'NONE',  ( 8.813304719595000947, 3.880154689736000417, -9.060377011187000562 ) ) ;
#55441 = FACE_BOUND ( 'NONE', #60304, .T. ) ;
#55442 = CARTESIAN_POINT ( 'NONE',  ( 8.354417780085995560, -5.125509315120996057, 6.367236178909004174 ) ) ;
#55443 = CARTESIAN_POINT ( 'NONE',  ( 13.50003721581400029, -9.159934378815998812, -7.517910889891000537 ) ) ;
#55444 = EDGE_CURVE ( 'NONE', #43366, #50721, #15620, .T. ) ;
#55445 = CARTESIAN_POINT ( 'NONE',  ( 9.447419570353266849, 2.249047413870973067, 7.566365124139655229 ) ) ;
#55446 = CARTESIAN_POINT ( 'NONE',  ( 2.447473465997000108, -3.391161957165999663, 0.4846026218182000189 ) ) ;
#55447 = ORIENTED_EDGE ( 'NONE', *, *, #46455, .T. ) ;
#55448 = CARTESIAN_POINT ( 'NONE',  ( 12.17712767754845693, -0.3597466176220747713, -12.59486741915706531 ) ) ;
#55449 = CARTESIAN_POINT ( 'NONE',  ( 7.805362843630345715, -2.998771363040654947, 6.543984068746279803 ) ) ;
#55450 = ADVANCED_FACE ( 'NONE', ( #10023 ), #64525, .F. ) ;
#55451 = CARTESIAN_POINT ( 'NONE',  ( 24.01983190392353151, -12.68029376182448864, -3.458225379361195007 ) ) ;
#55452 = CARTESIAN_POINT ( 'NONE',  ( 8.887170280412000523, 2.193665972875999959, 7.400591513898000073 ) ) ;
#55453 = ORIENTED_EDGE ( 'NONE', *, *, #57884, .T. ) ;
#55454 = CARTESIAN_POINT ( 'NONE',  ( 5.370433571222000602, -1.212815126404999999, 0.5269083208682000530 ) ) ;
#55455 = CARTESIAN_POINT ( 'NONE',  ( 7.092785841229000354, 5.307493345713999666, -7.572367724995999971 ) ) ;
#55457 = DIRECTION ( 'NONE',  ( 0.000000000000000000, -1.000000000000000000, 0.000000000000000000 ) ) ;
#55456 = DIRECTION ( 'NONE',  ( 1.000000000000000000, 0.000000000000000000, 0.000000000000000000 ) ) ;
#55458 = CARTESIAN_POINT ( 'NONE',  ( 11.38678751119029897, 2.833702563575000166, -8.110172976325500827 ) ) ;
#55459 = EDGE_LOOP ( 'NONE', ( #20757, #55186, #20167, #54139 ) ) ;
#55460 = AXIS2_PLACEMENT_3D ( 'NONE', #49526, #43604, #18071 ) ;
#55461 = SURFACE_STYLE_USAGE ( .BOTH. , #6865 ) ;
#55462 = VERTEX_POINT ( 'NONE', #16299 ) ;
#55463 = CARTESIAN_POINT ( 'NONE',  ( 16.39999999485600313, -3.595156957901000094, -11.99794989424000136 ) ) ;
#55464 = CARTESIAN_POINT ( 'NONE',  ( 12.80505043854146940, -3.207098164520926886, -13.58558594083658910 ) ) ;
#55465 = VECTOR ( 'NONE', #48768, 1000.000000000000000 ) ;
#55466 = CARTESIAN_POINT ( 'NONE',  ( 18.23388030753893219, 0.2566959043864865397, -13.99765098363215365 ) ) ;
#55467 = ORIENTED_EDGE ( 'NONE', *, *, #63602, .F. ) ;
#55468 = CARTESIAN_POINT ( 'NONE',  ( 10.92476424391678869, 9.558588620194553798, -6.023462398105898785 ) ) ;
#55469 = CARTESIAN_POINT ( 'NONE',  ( 8.287602312370099256, 2.892084006030188892, 6.689538372556729229 ) ) ;
#55470 = CARTESIAN_POINT ( 'NONE',  ( 8.087764158769999767, 5.395910762051999932, -7.432402852051000153 ) ) ;
#55471 = AXIS2_PLACEMENT_3D ( 'NONE', #25952, #11850, #44029 ) ;
#55472 = CARTESIAN_POINT ( 'NONE',  ( 11.46021572556888657, 2.954248811040025124, -7.175002613693187925 ) ) ;
#55473 = CARTESIAN_POINT ( 'NONE',  ( 24.57937622052009985, 3.599767751968668161, 12.25814915835329266 ) ) ;
#55474 = VERTEX_POINT ( 'NONE', #5471 ) ;
#55475 = PLANE ( 'NONE',  #14214 ) ;
#55476 = CARTESIAN_POINT ( 'NONE',  ( 23.54917057566099814, -13.36598973949000069, -4.292165629430000351 ) ) ;
#55477 = CARTESIAN_POINT ( 'NONE',  ( 10.90000000000000036, 2.399999999999999911, -6.571291218949999902 ) ) ;
#55478 = AXIS2_PLACEMENT_3D ( 'NONE', #27221, #21619, #53100 ) ;
#55479 = DIRECTION ( 'NONE',  ( 0.000000000000000000, 1.000000000000000000, 0.000000000000000000 ) ) ;
#55480 = ORIENTED_EDGE ( 'NONE', *, *, #34292, .F. ) ;
#55481 = CARTESIAN_POINT ( 'NONE',  ( 10.56577346846700038, -5.100000000000000533, 6.304440313576233024 ) ) ;
#55482 = CARTESIAN_POINT ( 'NONE',  ( 10.92292961924958128, 2.909845827876722968, 5.014592305248326554 ) ) ;
#55483 = CARTESIAN_POINT ( 'NONE',  ( 8.236972165045003180, 4.500178187997065038, -5.711464360401827811 ) ) ;
#55484 = CARTESIAN_POINT ( 'NONE',  ( 24.57788509278177003, 12.41755320330292989, -3.012067450446723083 ) ) ;
#55485 = DIRECTION ( 'NONE',  ( -1.000000000000000000, 0.000000000000000000, 0.000000000000000000 ) ) ;
#55486 = CARTESIAN_POINT ( 'NONE',  ( 6.034193173016747735, -1.460959015002474493, 0.3926218265389144757 ) ) ;
#55487 = EDGE_CURVE ( 'NONE', #52776, #3577, #23113, .T. ) ;
#55489 = EDGE_CURVE ( 'NONE', #37319, #41440, #15533, .T. ) ;
#55488 = CARTESIAN_POINT ( 'NONE',  ( 18.02779610229251617, -1.934613261143892426, 12.45059556317631611 ) ) ;
#55490 = ORIENTED_EDGE ( 'NONE', *, *, #37551, .T. ) ;
#55491 = CARTESIAN_POINT ( 'NONE',  ( 11.35545123989519922, -3.524778630617700248, -8.417769225118700405 ) ) ;
#55492 = ORIENTED_EDGE ( 'NONE', *, *, #67383, .T. ) ;
#55493 = CARTESIAN_POINT ( 'NONE',  ( 0.1499942179679999987, -2.199046806507074070, 1.689975037551095127 ) ) ;
#55494 = CARTESIAN_POINT ( 'NONE',  ( 8.947714158774999760, 3.854507394315999758, -9.394302886912999639 ) ) ;
#55495 = CARTESIAN_POINT ( 'NONE',  ( 3.592999774037999750, -3.226682447671000098, 0.007234183023254000221 ) ) ;
#55496 = CARTESIAN_POINT ( 'NONE',  ( 9.949439740260999088, -2.508493821066999807, -7.171861383782999866 ) ) ;
#55497 = CARTESIAN_POINT ( 'NONE',  ( 11.50008140503725329, -2.915874161187789859, 7.632269737612043414 ) ) ;
#55498 = CARTESIAN_POINT ( 'NONE',  ( 11.10000000009000054, -2.699999999911000259, 6.571291220400000022 ) ) ;
#55499 = DIRECTION ( 'NONE',  ( 1.000000000000000000, 0.000000000000000000, 0.000000000000000000 ) ) ;
#55500 = ORIENTED_EDGE ( 'NONE', *, *, #65918, .F. ) ;
#55501 = DIRECTION ( 'NONE',  ( 0.000000000000000000, -0.8648648648648720183, -0.5020047465136825426 ) ) ;
#55502 = CARTESIAN_POINT ( 'NONE',  ( 11.78949010443639978, -2.999324937259999935, 7.425165037173959703 ) ) ;
#55503 = CARTESIAN_POINT ( 'NONE',  ( 10.53138775541999905, 5.607751175212000838, 7.280102404048999887 ) ) ;
#55504 = CARTESIAN_POINT ( 'NONE',  ( 10.78170625604285782, -3.320082702567464850, -8.679590637733081593 ) ) ;
#55505 = EDGE_CURVE ( 'NONE', #67663, #683, #17295, .T. ) ;
#55506 = LINE ( 'NONE', #65637, #28730 ) ;
#55507 = DIRECTION ( 'NONE',  ( 1.000000000000000000, 0.000000000000000000, 1.099503168979000057E-13 ) ) ;
#55508 = CARTESIAN_POINT ( 'NONE',  ( 10.75210807141120029, 4.040019166404060336, -8.365272822098500427 ) ) ;
#55509 = TOROIDAL_SURFACE ( 'NONE', #64410, 1.649999999999999911, 0.5000000000000000000 ) ;
#55510 = B_SPLINE_CURVE_WITH_KNOTS ( 'NONE', 3,
 ( #11351, #33384, #11694, #21840, #58912, #21163, #42490, #58562, #64140, #16255, #64825, #11015, #32352, #38269, #53668, #5760, #43174, #27103 ),
 .UNSPECIFIED., .F., .F.,
 ( 4, 2, 2, 2, 2, 2, 2, 2, 4 ),
 ( 0.000000000000000000, 0.1250000000000000000, 0.2500000000000000000, 0.3750000000000000000, 0.5000000000000000000, 0.6250000000000000000, 0.7500000000000000000, 0.8750000000000000000, 1.000000000000000000 ),
 .UNSPECIFIED. ) ;
#55511 = CARTESIAN_POINT ( 'NONE',  ( 10.96503493446309285, 2.823010900888289765, -6.672616844255583324 ) ) ;
#55512 = CARTESIAN_POINT ( 'NONE',  ( 8.958265421554999719, 3.759926620436100375, -8.741861511046000288 ) ) ;
#55513 = DIRECTION ( 'NONE',  ( 0.000000000000000000, 0.000000000000000000, -1.000000000000000000 ) ) ;
#55514 = CARTESIAN_POINT ( 'NONE',  ( 30.60000000000000142, 0.000000000000000000, 0.000000000000000000 ) ) ;
#55515 = AXIS2_PLACEMENT_3D ( 'NONE', #49564, #7954, #29292 ) ;
#55516 = CARTESIAN_POINT ( 'NONE',  ( 10.34939834122999969, 2.653159779809000085, -7.312415497503999440 ) ) ;
#55517 = EDGE_LOOP ( 'NONE', ( #28556, #18396, #60370, #7831 ) ) ;
#55518 = CARTESIAN_POINT ( 'NONE',  ( 9.957462135714001406, 5.100000000000000533, -6.571291218949999902 ) ) ;
#55519 = CARTESIAN_POINT ( 'NONE',  ( 18.28009623694099162, 2.497067955185368948, 13.77553007214568659 ) ) ;
#55520 = CARTESIAN_POINT ( 'NONE',  ( 15.90018573812067615, -7.083264066697359418, -9.547770387689276106 ) ) ;
#55521 = CARTESIAN_POINT ( 'NONE',  ( 10.37041638348499895, -5.241705141469999774, -7.197535585171899619 ) ) ;
#55522 = VERTEX_POINT ( 'NONE', #10367 ) ;
#55523 = VECTOR ( 'NONE', #38932, 1000.000000000000000 ) ;
#55524 = CARTESIAN_POINT ( 'NONE',  ( 17.79165415090800195, 3.528207907415000122, 11.96069611418000100 ) ) ;
#55526 = CARTESIAN_POINT ( 'NONE',  ( 0.5412046677623798541, 3.514844065040157339, -0.4091116460506022956 ) ) ;
#55525 = CARTESIAN_POINT ( 'NONE',  ( 9.342560841233000346, 5.835196551504000517, -7.008466539623000813 ) ) ;
#55527 = CARTESIAN_POINT ( 'NONE',  ( 16.24412496488759317, 3.380981662632266183, 11.14874627148169672 ) ) ;
#55528 = ORIENTED_EDGE ( 'NONE', *, *, #3297, .F. ) ;
#55529 = B_SPLINE_CURVE_WITH_KNOTS ( 'NONE', 3,
 ( #49059, #56029, #18288, #50439 ),
 .UNSPECIFIED., .F., .F.,
 ( 4, 4 ),
 ( 0.000000000000000000, 1.000000000000000000 ),
 .UNSPECIFIED. ) ;
#55530 = B_SPLINE_CURVE_WITH_KNOTS ( 'NONE', 3,
 ( #59498, #6010, #60201, #38523, #53571, #11951, #54605, #43077, #65430, #32940, #6352, #44132, #87, #31913, #5666, #10919, #27700, #48671, #6703, #37487, #776, #17553, #21405, #49016, #38879, #28044, #38168, #64043, #16846, #53228, #22091, #47985 ),
 .UNSPECIFIED., .F., .F.,
 ( 4, 2, 2, 2, 2, 2, 2, 2, 1, 2, 2, 2, 1, 1, 1, 2, 2, 4 ),
 ( 0.000000000000000000, 0.2500000000000330291, 0.3750000000000466294, 0.4375000000000535683, 0.4687500000000569544, 0.5000000000000602851, 0.6250000000000622835, 0.6875000000000632827, 0.7187500000000637268, 0.7343750000000640599, 0.7500000000000642819, 0.8125000000000637268, 0.8437500000000613953, 0.8593750000000611733, 0.8671875000000591749, 0.8710937500000600631, 0.8750000000000608402, 1.000000000000000000 ),
 .UNSPECIFIED. ) ;
#55531 = CARTESIAN_POINT ( 'NONE',  ( 9.945533384955998812, 2.906048475816000121, 8.880389653997999844 ) ) ;
#55532 = VECTOR ( 'NONE', #31475, 1000.000000000000000 ) ;
#55533 = CARTESIAN_POINT ( 'NONE',  ( 18.05265757431624962, -3.049509720595951823, -13.66384965554843767 ) ) ;
#55534 = CARTESIAN_POINT ( 'NONE',  ( 11.21149010443640037, 5.137564434800999891, 7.414927836855409460 ) ) ;
#55535 = EDGE_CURVE ( 'NONE', #46507, #54548, #60206, .T. ) ;
#55536 = CARTESIAN_POINT ( 'NONE',  ( 10.16829915263999951, -4.567213659083999566, 5.832528837986999726 ) ) ;
#55537 = CARTESIAN_POINT ( 'NONE',  ( 8.325004567511003373, 2.868524053507002236, 6.316175840085996640 ) ) ;
#55538 = ORIENTED_EDGE ( 'NONE', *, *, #53523, .T. ) ;
#55539 = CARTESIAN_POINT ( 'NONE',  ( 11.53943995709000170, -3.847421095330999741, 11.95976051375000004 ) ) ;
#55540 = CARTESIAN_POINT ( 'NONE',  ( 13.99999997735699608, 8.821177874197267954, 7.709989353259445011 ) ) ;
#55541 = CARTESIAN_POINT ( 'NONE',  ( 8.092827459944675894, -4.405392649884461775, 5.808720040846370836 ) ) ;
#55542 = CARTESIAN_POINT ( 'NONE',  ( 11.15982711745999900, -5.578228817597000955, 8.067792329320999656 ) ) ;
#55543 = CARTESIAN_POINT ( 'NONE',  ( 11.51145123989532948, -3.394760891061399999, -8.668865425277999748 ) ) ;
#55544 = CARTESIAN_POINT ( 'NONE',  ( 9.552088727411000235, -5.000897406023000258, 7.416055476975279781 ) ) ;
#55545 = ORIENTED_EDGE ( 'NONE', *, *, #6066, .T. ) ;
#55546 = CARTESIAN_POINT ( 'NONE',  ( 1.746770412757999755E-07, -2.400000174626000238, 7.471644989856000012E-10 ) ) ;
#55547 = CARTESIAN_POINT ( 'NONE',  ( 11.14533863405319991, -3.296214805808900028, 6.602238051205399749 ) ) ;
#55548 = ORIENTED_EDGE ( 'NONE', *, *, #17346, .F. ) ;
#55549 = CARTESIAN_POINT ( 'NONE',  ( 19.99999987597299977, 12.42499880353999941, 0.000000000000000000 ) ) ;
#55550 = ORIENTED_EDGE ( 'NONE', *, *, #28601, .F. ) ;
#55551 = CARTESIAN_POINT ( 'NONE',  ( 9.573145925901000552, -2.133039813254999917, -7.346564890486999566 ) ) ;
#55552 = CARTESIAN_POINT ( 'NONE',  ( 9.839810841229999383, 5.817107086401000160, -6.945352709928000579 ) ) ;
#55553 = CARTESIAN_POINT ( 'NONE',  ( 10.63880513895979973, 5.150451045932999961, -6.860457220153399760 ) ) ;
#55554 = CARTESIAN_POINT ( 'NONE',  ( 13.49994651945300284, 12.07042783918999795, 2.492331243371999960 ) ) ;
#55555 = CARTESIAN_POINT ( 'NONE',  ( 12.76350981947226515, 1.876041592482996290, -12.57528602315340827 ) ) ;
#55556 = CARTESIAN_POINT ( 'NONE',  ( 11.90841235500450068, -4.841138636481000290, 8.270568563129298667 ) ) ;
#55557 = CARTESIAN_POINT ( 'NONE',  ( 11.56967835872019990, -4.754733798270200928, 7.975673736933100777 ) ) ;
#55558 = ORIENTED_EDGE ( 'NONE', *, *, #41187, .T. ) ;
#55559 = CARTESIAN_POINT ( 'NONE',  ( 5.105026506350000659, -1.500000000000000000, 0.000000000000000000 ) ) ;
#55560 = VECTOR ( 'NONE', #66537, 1000.000000000000000 ) ;
#55561 = ORIENTED_EDGE ( 'NONE', *, *, #26944, .F. ) ;
#55562 = CARTESIAN_POINT ( 'NONE',  ( 9.047980646795000581, -2.806079842068999852, 8.615883328687999665 ) ) ;
#55563 = CARTESIAN_POINT ( 'NONE',  ( 18.20121223417782730, 0.3818843736423395696, 13.99543728850611757 ) ) ;
#55564 = VERTEX_POINT ( 'NONE', #12099 ) ;
#55565 = CARTESIAN_POINT ( 'NONE',  ( 12.08198123077154840, -2.425144973324802944, -12.36441727636090349 ) ) ;
#55566 = CARTESIAN_POINT ( 'NONE',  ( 11.48225819896749833, 2.879005208331999910, 7.288668995979000087 ) ) ;
#55567 = MECHANICAL_DESIGN_GEOMETRIC_PRESENTATION_REPRESENTATION (  '', ( #33255 ), #49971 ) ;
#55568 = CARTESIAN_POINT ( 'NONE',  ( 23.60205915885299888, 2.338900754078999444, -12.00073634674999212 ) ) ;
#55569 = CARTESIAN_POINT ( 'NONE',  ( 6.388359839683332098, 0.7554284705563452107, 1.310679582531388609 ) ) ;
#55570 = CARTESIAN_POINT ( 'NONE',  ( 18.12304911038100030, -11.48572971900999917, 4.352322683670000636 ) ) ;
#55571 = CARTESIAN_POINT ( 'NONE',  ( 8.090129597172618148, -4.176673380088065990, 8.851094058678157239 ) ) ;
#55572 = CARTESIAN_POINT ( 'NONE',  ( 12.24414859480286921, -2.775896286417997239, -13.61101139974199548 ) ) ;
#55573 = CARTESIAN_POINT ( 'NONE',  ( 18.17177216100527914, 0.1019009512359512898, -12.69945530929772559 ) ) ;
#55574 = AXIS2_PLACEMENT_3D ( 'NONE', #22229, #43566, #27142 ) ;
#55575 = PRESENTATION_STYLE_ASSIGNMENT (( #51012 ) ) ;
#55576 = CARTESIAN_POINT ( 'NONE',  ( 10.64533863405319991, -3.296214805808900028, -8.397761948794601139 ) ) ;
#55577 = EDGE_CURVE ( 'NONE', #65623, #41499, #38083, .T. ) ;
#55579 = EDGE_CURVE ( 'NONE', #115, #57225, #59048, .T. ) ;
#55578 = CARTESIAN_POINT ( 'NONE',  ( 8.674239158774001979, 5.983047240001000411, 7.440798119034999658 ) ) ;
#55580 = ORIENTED_EDGE ( 'NONE', *, *, #64949, .F. ) ;
#55581 = DIRECTION ( 'NONE',  ( 0.000000000000000000, 0.000000000000000000, -1.000000000000000000 ) ) ;
#55582 = CARTESIAN_POINT ( 'NONE',  ( 7.366321766359212653, 4.272452671693901749, 6.150367080941864018 ) ) ;
#55583 = CARTESIAN_POINT ( 'NONE',  ( 23.73832292375600161, -3.439035004086000047, 13.34772648052000044 ) ) ;
#55584 = CARTESIAN_POINT ( 'NONE',  ( 18.14141836411847208, 2.283433982113741045, 12.49938471124204931 ) ) ;
#55585 = CARTESIAN_POINT ( 'NONE',  ( 18.44330693167099966, 2.998553466420000202, -12.10578145104000036 ) ) ;
#55586 = CARTESIAN_POINT ( 'NONE',  ( 10.15403136780999915, 5.267988602993999514, 5.992335067371000079 ) ) ;
#55587 = CIRCLE ( 'NONE', #35476, 12.39999890530000037 ) ;
#55588 = CARTESIAN_POINT ( 'NONE',  ( 5.700000000000000178, -12.50865771883999855, -2.924687089723999822 ) ) ;
#55589 = CARTESIAN_POINT ( 'NONE',  ( 12.71012035428156928, -0.7146386402780370295, -12.57972080578504404 ) ) ;
#55590 = ORIENTED_EDGE ( 'NONE', *, *, #33330, .T. ) ;
#55591 = CARTESIAN_POINT ( 'NONE',  ( 12.80505043854146940, -1.875000000000000444, 12.57545641911172396 ) ) ;
#55592 = CARTESIAN_POINT ( 'NONE',  ( 10.10892546752099896, -4.864937374655599278, -7.440072690703440017 ) ) ;
#55593 = CARTESIAN_POINT ( 'NONE',  ( 10.62793268324000096, 3.100586971929999880, 8.599896650316999569 ) ) ;
#55594 = ADVANCED_FACE ( 'NONE', ( #1263 ), #16007, .F. ) ;
#55595 = CARTESIAN_POINT ( 'NONE',  ( 9.272783876522375124, 3.210141752053232711, 8.481892410946455740 ) ) ;
#55596 = EDGE_CURVE ( 'NONE', #19885, #24902, #15561, .T. ) ;
#55597 = CARTESIAN_POINT ( 'NONE',  ( 10.39918582084299992, 3.253651555277099927, -6.637298362509499228 ) ) ;
#55598 = CARTESIAN_POINT ( 'NONE',  ( 12.09164653790448440, -0.1286734328892388535, 12.59934825840596595 ) ) ;
#55599 = CARTESIAN_POINT ( 'NONE',  ( 8.058767219590999176, 2.432118421226999949, 6.597517552098000060 ) ) ;
#55600 = CARTESIAN_POINT ( 'NONE',  ( 9.318724127987000116, 2.755029797911999978, 8.795125756257000660 ) ) ;
#55601 = B_SPLINE_CURVE_WITH_KNOTS ( 'NONE', 3,
 ( #62383, #66937, #7878, #45289 ),
 .UNSPECIFIED., .F., .F.,
 ( 4, 4 ),
 ( 0.000000000000000000, 1.000000000000000000 ),
 .UNSPECIFIED. ) ;
#55602 = CARTESIAN_POINT ( 'NONE',  ( 12.22206196700517822, 2.274492675301821976, 12.50124639636504931 ) ) ;
#55603 = ORIENTED_EDGE ( 'NONE', *, *, #62120, .F. ) ;
#55604 = CARTESIAN_POINT ( 'NONE',  ( 9.485829719593997567, 4.953415418491999844, -8.946479654552000227 ) ) ;
#55605 = CARTESIAN_POINT ( 'NONE',  ( 11.40425819896749893, 2.744109752373000255, -7.736761623643599428 ) ) ;
#55606 = VECTOR ( 'NONE', #51770, 999.9999999999998863 ) ;
#55607 = CARTESIAN_POINT ( 'NONE',  ( 11.09999999999999964, 2.646159083949000124, 6.745271721726000536 ) ) ;
#55609 = CARTESIAN_POINT ( 'NONE',  ( 18.01482197265775653, -0.4234835428822800174, 12.69049809666515394 ) ) ;
#55608 = CARTESIAN_POINT ( 'NONE',  ( 8.432504440379000599, -5.430412429559000387, 7.210798766422999329 ) ) ;
#55610 = CARTESIAN_POINT ( 'NONE',  ( 10.76788779216199998, -3.070969952137800441, 7.164969140522200242 ) ) ;
#55611 = CARTESIAN_POINT ( 'NONE',  ( 11.63825819896753977, -4.851203879749700576, -7.660469764776300039 ) ) ;
#55612 = ORIENTED_EDGE ( 'NONE', *, *, #14797, .T. ) ;
#55613 = CARTESIAN_POINT ( 'NONE',  ( 1.834748578981000078, 1.670918626813999941, 2.798091744145999815 ) ) ;
#55614 = CARTESIAN_POINT ( 'NONE',  ( 17.96364285837030650, -0.4729642813570114068, -12.68814481174042363 ) ) ;
#55615 = AXIS2_PLACEMENT_3D ( 'NONE', #30506, #31203, #42027 ) ;
#55616 = CARTESIAN_POINT ( 'NONE',  ( 9.416525748329496182, -4.536323992761255752, 8.432246543101925340 ) ) ;
#55617 = LINE ( 'NONE', #45810, #38004 ) ;
#55618 = CARTESIAN_POINT ( 'NONE',  ( 24.40628504445000146, -12.24027098532000046, 3.187905388436000464 ) ) ;
#55620 = CARTESIAN_POINT ( 'NONE',  ( 4.900006121741999898, -6.122517096885939548E-17, -1.999970730383187734 ) ) ;
#55619 = VECTOR ( 'NONE', #996, 1000.000000000000114 ) ;
#55621 = CARTESIAN_POINT ( 'NONE',  ( 9.360840674114749405, -8.748618759363491648, 6.377268954453214178 ) ) ;
#55622 = CARTESIAN_POINT ( 'NONE',  ( 20.10000000000000142, 11.84999999999999964, 0.000000000000000000 ) ) ;
#55623 = CYLINDRICAL_SURFACE ( 'NONE', #44418, 0.4999999999999998335 ) ;
#55624 = ORIENTED_EDGE ( 'NONE', *, *, #2665, .T. ) ;
#55625 = CARTESIAN_POINT ( 'NONE',  ( 9.163172718159000141, 7.862179196714000007, -5.354466121481999963 ) ) ;
#55626 = CARTESIAN_POINT ( 'NONE',  ( 23.57774091470277611, -2.928866170651173384, 13.64744915248744306 ) ) ;
#55627 = CARTESIAN_POINT ( 'NONE',  ( 7.451720376979478644, -2.261709126496390443, 7.443204203363470661 ) ) ;
#55628 = CARTESIAN_POINT ( 'NONE',  ( 17.77476912165378664, -0.5854932480584860155, 13.88340087527186384 ) ) ;
#55629 = CARTESIAN_POINT ( 'NONE',  ( 1.991204174508000024, 3.176854988377000311, -1.562936765141999862 ) ) ;
#55630 = ORIENTED_EDGE ( 'NONE', *, *, #5903, .T. ) ;
#55631 = CARTESIAN_POINT ( 'NONE',  ( 4.950033214355999966, 0.000000000000000000, -2.049966935984999683 ) ) ;
#55632 = CARTESIAN_POINT ( 'NONE',  ( 10.48389394032039235, -4.970831725323499484, 5.006796266880559010 ) ) ;
#55633 = CARTESIAN_POINT ( 'NONE',  ( 14.00000000000000178, 50.50083396221999976, 44.47484963936999947 ) ) ;
#55634 = CARTESIAN_POINT ( 'NONE',  ( 11.70794988689359961, 4.455786710255300598, 6.606015074393400077 ) ) ;
#55635 = EDGE_CURVE ( 'NONE', #14642, #44229, #68918, .T. ) ;
#55636 = CIRCLE ( 'NONE', #39970, 1.000000000000000666 ) ;
#55637 = CARTESIAN_POINT ( 'NONE',  ( 11.10328610135029948, -4.878060775730400422, -7.825000000000000178 ) ) ;
#55638 = CARTESIAN_POINT ( 'NONE',  ( 11.25809194037999994, -3.275508415657999883, -8.650784343212000849 ) ) ;
#55639 = CARTESIAN_POINT ( 'NONE',  ( 11.72005178113508173, 3.595543782877861805, -11.99782022136548143 ) ) ;
#55640 = CARTESIAN_POINT ( 'NONE',  ( 9.646886009120546390, 5.267629041041144156, -8.036546440280751824 ) ) ;
#55641 = CARTESIAN_POINT ( 'NONE',  ( 12.20883946518622132, -2.687526094403444255, 12.40592204487990990 ) ) ;
#55642 = CARTESIAN_POINT ( 'NONE',  ( 8.558820226389943997, 3.642594333086357050, 5.792987242710919027 ) ) ;
#55643 = ORIENTED_EDGE ( 'NONE', *, *, #29770, .F. ) ;
#55644 = AXIS2_PLACEMENT_3D ( 'NONE', #31949, #16544, #22133 ) ;
#55645 = CARTESIAN_POINT ( 'NONE',  ( 17.95040605897959196, -3.130086699081792379, 13.64560748759991071 ) ) ;
#55646 = CARTESIAN_POINT ( 'NONE',  ( 11.20733594839949809, -3.159733897807000425, -6.537051788466999191 ) ) ;
#55647 = ORIENTED_EDGE ( 'NONE', *, *, #55004, .T. ) ;
#55648 = CARTESIAN_POINT ( 'NONE',  ( 8.973567461188688199, -5.349887746458779070, 7.470579050607700111 ) ) ;
#55649 = CARTESIAN_POINT ( 'NONE',  ( 10.57102344389999971, 3.237334151971200225, 7.962849245488699879 ) ) ;
#55650 = CARTESIAN_POINT ( 'NONE',  ( 9.843930206850000530, 2.750000000000000000, -7.500000000000000000 ) ) ;
#55651 = CARTESIAN_POINT ( 'NONE',  ( 23.61662973629609752, 13.40571813662669776, -3.919378641685453246 ) ) ;
#55652 = CARTESIAN_POINT ( 'NONE',  ( 10.65050915380999896, 5.200037120669999346, 5.937706951697999891 ) ) ;
#55653 = FACE_OUTER_BOUND ( 'NONE', #26758, .T. ) ;
#55654 = CARTESIAN_POINT ( 'NONE',  ( 10.77934687351620546, -4.163624617374463988, 8.750000000000001776 ) ) ;
#55655 = DIRECTION ( 'NONE',  ( -1.000000000000000000, 0.000000000000000000, 0.000000000000000000 ) ) ;
#55656 = DIRECTION ( 'NONE',  ( 1.000000000000000000, 0.000000000000000000, 0.000000000000000000 ) ) ;
#55657 = CARTESIAN_POINT ( 'NONE',  ( 4.000000000000000888, -1.321180510578202849, -1.719428477289353330 ) ) ;
#55658 = EDGE_CURVE ( 'NONE', #55031, #12730, #64827, .T. ) ;
#55660 = EDGE_CURVE ( 'NONE', #46963, #47396, #33777, .T. ) ;
#55659 = CARTESIAN_POINT ( 'NONE',  ( 10.81379776946905125, -2.908665697285443219, -5.100634573475641531 ) ) ;
#55661 = EDGE_LOOP ( 'NONE', ( #6538, #64847, #31029, #66711, #60908, #28129 ) ) ;
#55662 = DIRECTION ( 'NONE',  ( 0.000000000000000000, -0.8648648648648720183, 0.5020047465136825426 ) ) ;
#55663 = EDGE_CURVE ( 'NONE', #49260, #8310, #50022, .T. ) ;
#55664 = LINE ( 'NONE', #29106, #2371 ) ;
#55665 = CARTESIAN_POINT ( 'NONE',  ( 10.75580099727000061, -5.294318740464999173, 4.786926179488999900 ) ) ;
#55666 = CONICAL_SURFACE ( 'NONE', #31113, 12.42515511468000078, 0.7854106315584118425 ) ;
#55667 = CARTESIAN_POINT ( 'NONE',  ( 8.807788144226000426, 4.090932644426789722, 6.546538158064899804 ) ) ;
#55668 = CARTESIAN_POINT ( 'NONE',  ( 10.52022949779799887, 4.709679768527199606, -8.564302809495998758 ) ) ;
#55669 = CARTESIAN_POINT ( 'NONE',  ( 12.70873338277715980, 3.242082958893194089, 13.61943113270052663 ) ) ;
#55670 = CARTESIAN_POINT ( 'NONE',  ( 9.701976361057999654, -3.399137684422000039, 6.026753338319999820 ) ) ;
#55671 = ORIENTED_EDGE ( 'NONE', *, *, #27755, .F. ) ;
#55672 = CIRCLE ( 'NONE', #21119, 2.000000000000000000 ) ;
#55673 = CARTESIAN_POINT ( 'NONE',  ( 23.89320776801300283, -8.313844348291002717, -8.526065358951003148 ) ) ;
#55674 = CARTESIAN_POINT ( 'NONE',  ( 12.80505043854144098, 0.7302158263239096891, 13.98094363220831227 ) ) ;
#55675 = ORIENTED_EDGE ( 'NONE', *, *, #3605, .T. ) ;
#55676 = CARTESIAN_POINT ( 'NONE',  ( 24.32155364739020342, 12.72720341677420741, -3.095246424363175652 ) ) ;
#55677 = CARTESIAN_POINT ( 'NONE',  ( 10.64659662355864711, -2.685854016001090638, 7.981709294338716454 ) ) ;
#55678 = CARTESIAN_POINT ( 'NONE',  ( 23.64071596919400164, -3.067373287554000072, -13.45661305457000090 ) ) ;
#55679 = CIRCLE ( 'NONE', #69032, 2.000000000000000444 ) ;
#55680 = CARTESIAN_POINT ( 'NONE',  ( 4.744253625325000279, 0.4084786803018999879, -1.577726830116000123 ) ) ;
#55681 = EDGE_CURVE ( 'NONE', #5573, #29932, #58154, .T. ) ;
#55682 = CARTESIAN_POINT ( 'NONE',  ( 8.361784236169967244, -5.107027742527944447, 6.686924772338650236 ) ) ;
#55683 = CARTESIAN_POINT ( 'NONE',  ( 11.07110280567999894, 7.379437729801000323, -6.320289087312000120 ) ) ;
#55684 = VECTOR ( 'NONE', #2510, 1000.000000000000000 ) ;
#55685 = CARTESIAN_POINT ( 'NONE',  ( 8.200356874137819219, 3.823158304644485028, -8.849587703040166176 ) ) ;
#55686 = DIRECTION ( 'NONE',  ( 1.000000000000000000, 0.000000000000000000, 0.000000000000000000 ) ) ;
#55687 = CARTESIAN_POINT ( 'NONE',  ( 12.80505043854143388, 3.199698446519374517, 12.18695736643652694 ) ) ;
#55688 = CARTESIAN_POINT ( 'NONE',  ( 9.700159544970999193, -4.268950419651999617, -8.781589108989999559 ) ) ;
#55689 = CARTESIAN_POINT ( 'NONE',  ( 10.29262282008599882, 4.451581486939200083, -8.228386593078399258 ) ) ;
#55690 = DIRECTION ( 'NONE',  ( -1.000000000000000000, 0.000000000000000000, 0.000000000000000000 ) ) ;
#55691 = CARTESIAN_POINT ( 'NONE',  ( 11.44366954483529852, 4.485203148598100320, -6.751356298874699569 ) ) ;
#55692 = CARTESIAN_POINT ( 'NONE',  ( 8.720797255587999786, 5.140789995332999851, -7.451702546394010085 ) ) ;
#55694 = CARTESIAN_POINT ( 'NONE',  ( 10.70985928442000024, -2.874451299444999552, 5.003015709877000283 ) ) ;
#55693 = FACE_OUTER_BOUND ( 'NONE', #12540, .T. ) ;
#55695 = CIRCLE ( 'NONE', #28909, 1.500000000000001110 ) ;
#55696 = CARTESIAN_POINT ( 'NONE',  ( 23.59082918485488278, -13.38373040019899918, 4.039796375151918362 ) ) ;
#55697 = ORIENTED_EDGE ( 'NONE', *, *, #45011, .T. ) ;
#55698 = CARTESIAN_POINT ( 'NONE',  ( 10.44635971519499940, 4.459622816450200311, 8.264615166761799969 ) ) ;
#55699 = CARTESIAN_POINT ( 'NONE',  ( 10.65550933554000146, -4.237674644795000667, 9.105223721671999115 ) ) ;
#55700 = CARTESIAN_POINT ( 'NONE',  ( 9.984292290062997566, 4.868609929059700470, 8.004340253666999416 ) ) ;
#55701 = CARTESIAN_POINT ( 'NONE',  ( 9.936116252963625328, 4.581155023945095550, -6.845942581217610012 ) ) ;
#55702 = CARTESIAN_POINT ( 'NONE',  ( 10.34521071928999980, -2.724119865955000108, 6.497322598008000050 ) ) ;
#55703 = CARTESIAN_POINT ( 'NONE',  ( 12.49122810691469709, 3.040889930145693754, 13.54369178477972468 ) ) ;
#55704 = ORIENTED_EDGE ( 'NONE', *, *, #28897, .F. ) ;
#55705 = B_SPLINE_CURVE_WITH_KNOTS ( 'NONE', 3,
 ( #52137, #39948, #30484, #51457 ),
 .UNSPECIFIED., .F., .F.,
 ( 4, 4 ),
 ( 0.000000000000000000, 1.000000000000000000 ),
 .UNSPECIFIED. ) ;
#55706 = CARTESIAN_POINT ( 'NONE',  ( 9.278038493598998571, -3.173653894988100355, -6.712036445818600150 ) ) ;
#55707 = PLANE ( 'NONE',  #28717 ) ;
#55708 = CARTESIAN_POINT ( 'NONE',  ( 5.873107267216000515, 1.541759477651000187, 0.4799094010597000359 ) ) ;
#55709 = CARTESIAN_POINT ( 'NONE',  ( 17.77301286688677706, 3.166510366255908870, -12.19562279494696178 ) ) ;
#55710 = CARTESIAN_POINT ( 'NONE',  ( 10.50551210286899995, -4.217228369037729685, 6.243812680477911492 ) ) ;
#55711 = DIRECTION ( 'NONE',  ( -5.233425451124840269E-15, 2.123563019594860353E-14, 1.000000000000000000 ) ) ;
#55712 = EDGE_CURVE ( 'NONE', #67791, #53475, #20639, .T. ) ;
#55713 = ADVANCED_FACE ( 'NONE', ( #10543 ), #52508, .T. ) ;
#55714 = CARTESIAN_POINT ( 'NONE',  ( 11.68333460557258796, 4.162011815820000571, -8.490304555719900392 ) ) ;
#55715 = CARTESIAN_POINT ( 'NONE',  ( 5.966666563597951445, 12.43894384121646901, -2.828928431919257580 ) ) ;
#55716 = CARTESIAN_POINT ( 'NONE',  ( 9.441315108303999892, -3.111669560323000017, -8.958991988670002016 ) ) ;
#55717 = CARTESIAN_POINT ( 'NONE',  ( 25.08881572089300249, 11.66016675852999818, 3.018805299122000019 ) ) ;
#55718 = VERTEX_POINT ( 'NONE', #21043 ) ;
#55719 = CARTESIAN_POINT ( 'NONE',  ( 9.911033975247157457, -5.348894881546552682, 7.263563640299063096 ) ) ;
#55720 = CARTESIAN_POINT ( 'NONE',  ( 12.61399518047280210, 0.5951713840684276224, -13.88284414672551392 ) ) ;
#55721 = CARTESIAN_POINT ( 'NONE',  ( 8.348093183609000434, 4.599999999999999645, -6.056236567608999977 ) ) ;
#55722 = CARTESIAN_POINT ( 'NONE',  ( 23.60000000000000142, 9.517611874540000017, 8.103398312166000039 ) ) ;
#55723 = CARTESIAN_POINT ( 'NONE',  ( 4.900006121741999010, 1.599333684796359289, -1.229093439949831224 ) ) ;
#55724 = CARTESIAN_POINT ( 'NONE',  ( 8.623264158775000965, 5.288433695693000480, -8.041290150997999930 ) ) ;
#55725 = CARTESIAN_POINT ( 'NONE',  ( 13.43019412026600179, 12.07125412582999857, 2.305633000807000066 ) ) ;
#55726 = ORIENTED_EDGE ( 'NONE', *, *, #38667, .F. ) ;
#55727 = CARTESIAN_POINT ( 'NONE',  ( 0.1103081484368000076, -1.521127753326000143, -2.712944034833999929 ) ) ;
#55728 = CARTESIAN_POINT ( 'NONE',  ( 17.78669369145615420, 1.919420387948956419, -13.77958849407365527 ) ) ;
#55729 = VERTEX_POINT ( 'NONE', #14431 ) ;
#55730 = CARTESIAN_POINT ( 'NONE',  ( 11.09999965054999826, -2.398081733189999864E-14, 0.000000000000000000 ) ) ;
#55731 = CARTESIAN_POINT ( 'NONE',  ( 25.05002146819219178, 2.896643222720280519, 11.52366225513116937 ) ) ;
#55732 = CARTESIAN_POINT ( 'NONE',  ( 8.316054719590999511, 3.826300099041999747, -9.055335252254000267 ) ) ;
#55733 = CARTESIAN_POINT ( 'NONE',  ( 11.47028665956023197, -4.742415037725370652, 6.450604656432373574 ) ) ;
#55734 = CARTESIAN_POINT ( 'NONE',  ( 11.47500581613029880, -3.011381429075500105, -8.134817373646898275 ) ) ;
#55735 = CARTESIAN_POINT ( 'NONE',  ( 17.69617877290574626, 0.6091736731973926844, -12.68032649603847339 ) ) ;
#55736 = DIRECTION ( 'NONE',  ( 0.000000000000000000, -0.6556630511404241135, 0.7550536162215433222 ) ) ;
#55737 = EDGE_LOOP ( 'NONE', ( #34993, #52549 ) ) ;
#55738 = CARTESIAN_POINT ( 'NONE',  ( 10.09999999999999964, 0.000000000000000000, 11.84999999999999964 ) ) ;
#55739 = CARTESIAN_POINT ( 'NONE',  ( 17.94485468265261119, -2.989306481691796691, -13.55738131292138426 ) ) ;
#55741 = EDGE_CURVE ( 'NONE', #35662, #47463, #60637, .T. ) ;
#55740 = CARTESIAN_POINT ( 'NONE',  ( 9.196339158776000389, 4.112741311853999271, -5.603466076760000192 ) ) ;
#55742 = ORIENTED_EDGE ( 'NONE', *, *, #58396, .T. ) ;
#55743 = CARTESIAN_POINT ( 'NONE',  ( 10.97074841058999972, 2.648521302318000092, -6.788870928221999890 ) ) ;
#55744 = B_SPLINE_CURVE_WITH_KNOTS ( 'NONE', 3,
 ( #44134, #32942, #2170, #49709 ),
 .UNSPECIFIED., .F., .F.,
 ( 4, 4 ),
 ( 0.000000000000000000, 1.000000000000000000 ),
 .UNSPECIFIED. ) ;
#55745 = DIRECTION ( 'NONE',  ( 0.000000000000000000, 1.000000000000000000, 0.000000000000000000 ) ) ;
#55746 = ADVANCED_FACE ( 'NONE', ( #36088 ), #47272, .F. ) ;
#55747 = VERTEX_POINT ( 'NONE', #63678 ) ;
#55748 = CARTESIAN_POINT ( 'NONE',  ( 9.354025935145999782, 3.834207658792500251, 8.629711178834000407 ) ) ;
#55749 = CARTESIAN_POINT ( 'NONE',  ( 18.23116755655862065, -2.220104646260180559, -12.40287289761280398 ) ) ;
#55750 = CARTESIAN_POINT ( 'NONE',  ( 9.623096873515669003, 5.217465845835395299, 7.172815144550900968 ) ) ;
#55751 = CARTESIAN_POINT ( 'NONE',  ( -0.2999999999999999889, 0.5773502691895999739, -1.000000000000000000 ) ) ;
#55752 = CARTESIAN_POINT ( 'NONE',  ( 9.099999931440999390, 5.064317881551000156, 6.844464000216799349 ) ) ;
#55753 = CARTESIAN_POINT ( 'NONE',  ( 9.586013376692998023, 3.227076647348800176, 7.892807122431200639 ) ) ;
#55754 = CARTESIAN_POINT ( 'NONE',  ( 9.428389268916888000, -2.310473079787241257, 7.963614157108587222 ) ) ;
#55755 = ORIENTED_EDGE ( 'NONE', *, *, #53978, .T. ) ;
#55756 = CYLINDRICAL_SURFACE ( 'NONE', #49281, 1.350000000000000533 ) ;
#55757 = CARTESIAN_POINT ( 'NONE',  ( 10.73615471958999912, 3.078044734341000233, -6.088740491863000592 ) ) ;
#55758 = CARTESIAN_POINT ( 'NONE',  ( 7.000000000000000000, 0.6769230769231000533, -2.665384615385000266 ) ) ;
#55759 = CARTESIAN_POINT ( 'NONE',  ( 12.08002994951551123, 2.497059486053646360, -13.77553160571068425 ) ) ;
#55760 = CARTESIAN_POINT ( 'NONE',  ( 5.305026506349999948, 1.500000000000000000, 0.000000000000000000 ) ) ;
#55761 = CARTESIAN_POINT ( 'NONE',  ( 11.06924082387999952, -5.425685649895999774, 8.012912555523998392 ) ) ;
#55762 = ADVANCED_FACE ( 'NONE', ( #9168 ), #60790, .F. ) ;
#55763 = CARTESIAN_POINT ( 'NONE',  ( 17.59617041303008378, 0.6239795106976183670, 13.88114172264461210 ) ) ;
#55764 = CARTESIAN_POINT ( 'NONE',  ( 18.14129716923323699, -2.282346377875212884, 12.49966253006511430 ) ) ;
#55765 = ORIENTED_EDGE ( 'NONE', *, *, #32710, .T. ) ;
#55766 = EDGE_LOOP ( 'NONE', ( #1794, #22169, #62336, #46857 ) ) ;
#55767 = CARTESIAN_POINT ( 'NONE',  ( 8.599639158772999892, 2.261390688294000029, -6.733978371730000134 ) ) ;
#55768 = CARTESIAN_POINT ( 'NONE',  ( 9.158483593794224831, 5.507272619768906807, 6.616252076538792437 ) ) ;
#55769 = CARTESIAN_POINT ( 'NONE',  ( 12.20100803716184679, -2.660536040162761573, 13.63809770095273066 ) ) ;
#55770 = CARTESIAN_POINT ( 'NONE',  ( 9.242435128169496750, -5.510362259932574780, 8.414241021983331237 ) ) ;
#55771 = CARTESIAN_POINT ( 'NONE',  ( 8.128308059623998716, -3.117370956513999758, 8.662188901935000018 ) ) ;
#55772 = FACE_OUTER_BOUND ( 'NONE', #42953, .T. ) ;
#55774 = CARTESIAN_POINT ( 'NONE',  ( 16.39999997735698756, 3.306214596137839745, 11.23948664129755137 ) ) ;
#55773 = CARTESIAN_POINT ( 'NONE',  ( 10.30900081823999948, -5.010295986746999830, 6.967988282883199602 ) ) ;
#55775 = CARTESIAN_POINT ( 'NONE',  ( 9.099999931440999390, 5.064317881551000156, -8.155535999783198875 ) ) ;
#55776 = ORIENTED_EDGE ( 'NONE', *, *, #44597, .T. ) ;
#55777 = DIRECTION ( 'NONE',  ( 0.000000000000000000, 0.7158784314710767704, 0.6982249432342778617 ) ) ;
#55778 = CARTESIAN_POINT ( 'NONE',  ( 7.925588223455998893, 3.381165371184000179, -6.300169931272000312 ) ) ;
#55779 = CARTESIAN_POINT ( 'NONE',  ( 10.90000000296000060, -5.100000000009000445, 5.160242730682999657 ) ) ;
#55780 = CARTESIAN_POINT ( 'NONE',  ( 8.576923877145999242, 3.399999999999999911, 5.924121105096999962 ) ) ;
#55781 = CARTESIAN_POINT ( 'NONE',  ( 17.81530815050373917, -3.068584091768072231, -12.30073186569158850 ) ) ;
#55782 = VERTEX_POINT ( 'NONE', #54580 ) ;
#55784 = CARTESIAN_POINT ( 'NONE',  ( 11.06623059009866061, 3.312237475846871781, 8.035958501307058910 ) ) ;
#55783 = CARTESIAN_POINT ( 'NONE',  ( 11.09999999999999964, -3.512324525112999751, -8.971282648301999174 ) ) ;
#55785 = CARTESIAN_POINT ( 'NONE',  ( 8.216604719590000272, 5.331510020787000315, -8.114341808290998159 ) ) ;
#55786 = CARTESIAN_POINT ( 'NONE',  ( 12.78422835261028112, -1.875000554926937291, 13.78631940402569001 ) ) ;
#55787 = CARTESIAN_POINT ( 'NONE',  ( 10.46887750876899936, 3.307728619566300043, 6.425720373262999274 ) ) ;
#55788 = CARTESIAN_POINT ( 'NONE',  ( 11.57299956498199833, -2.792989229543000107, 7.174999999999999822 ) ) ;
#55789 = B_SPLINE_SURFACE_WITH_KNOTS ( 'NONE', 3, 3, ( 
 ( #45288, #61357, #60325, #59975 ),
 ( #55429, #7520, #55079, #2623 ),
 ( #12781, #17326, #12085, #39345 ),
 ( #44946, #13478, #34797, #23604 ),
 ( #56108, #33416, #6834, #66594 ),
 ( #7185, #12433, #18713, #38652 ),
 ( #66250, #28522, #40046, #8219 ),
 ( #54734, #2966, #29567, #49833 ),
 ( #34461, #50869, #45632, #28875 ) ),
 .UNSPECIFIED., .F., .F., .F.,
 ( 4, 1, 1, 1, 1, 1, 4 ),
 ( 4, 4 ),
 ( -0.01830387170767999727, 0.000000000000000000, 0.2500000000000000000, 0.5000000000000000000, 0.7500000000000000000, 1.000000000000000000, 1.018541916426999983 ),
 ( -0.2206046696922999983, 1.220604669692000099 ),
 .UNSPECIFIED. ) ;
#55790 = CYLINDRICAL_SURFACE ( 'NONE', #33165, 13.17499999999999893 ) ;
#55791 = CARTESIAN_POINT ( 'NONE',  ( 3.458341080379000232, 2.282530897026000094, -2.706516516324000143 ) ) ;
#55792 = ORIENTED_EDGE ( 'NONE', *, *, #43882, .F. ) ;
#55793 = EDGE_CURVE ( 'NONE', #5733, #48489, #43751, .T. ) ;
#55794 = ADVANCED_FACE ( 'NONE', ( #6675 ), #28361, .T. ) ;
#55795 = CARTESIAN_POINT ( 'NONE',  ( 12.41154142318500675, 0.6042324041877048524, -12.58550538354983672 ) ) ;
#55796 = CARTESIAN_POINT ( 'NONE',  ( 7.801415703136094670, -2.973868799469420843, 6.571950203487468833 ) ) ;
#55797 = CARTESIAN_POINT ( 'NONE',  ( 11.07484075165016613, -2.725159248349832364, -6.497852970900667380 ) ) ;
#55798 = CARTESIAN_POINT ( 'NONE',  ( 8.320864158774000430, 3.894644548817000285, 6.044465307984999924 ) ) ;
#55799 = DIRECTION ( 'NONE',  ( 1.000000000000000000, 0.000000000000000000, 0.000000000000000000 ) ) ;
#55800 = ORIENTED_EDGE ( 'NONE', *, *, #6168, .T. ) ;
#55801 = CARTESIAN_POINT ( 'NONE',  ( 5.723333808541000600, 0.8392109641639000639, 1.021861505418000027 ) ) ;
#55802 = EDGE_CURVE ( 'NONE', #21511, #18362, #25593, .T. ) ;
#55803 = EDGE_CURVE ( 'NONE', #18846, #46748, #22235, .T. ) ;
#55804 = CARTESIAN_POINT ( 'NONE',  ( 7.838660841226998244, 2.602490396417999730, -7.495170534277000307 ) ) ;
#55806 = CARTESIAN_POINT ( 'NONE',  ( 9.076707875513999824, -5.109724393580905577, -6.693505495912332570 ) ) ;
#55805 = CARTESIAN_POINT ( 'NONE',  ( 8.610875063856999745, -4.757997781751000410, 5.934102420827000124 ) ) ;
#55807 = CARTESIAN_POINT ( 'NONE',  ( 10.59195391537400077, 5.057233422790000432, 6.781965272201699868 ) ) ;
#55808 = CARTESIAN_POINT ( 'NONE',  ( 10.45222191436347714, -3.562569433230172944, -6.743201413565676816 ) ) ;
#55809 = ORIENTED_EDGE ( 'NONE', *, *, #14752, .F. ) ;
#55810 = FACE_OUTER_BOUND ( 'NONE', #35384, .T. ) ;
#55811 = ORIENTED_EDGE ( 'NONE', *, *, #47373, .F. ) ;
#55812 = CARTESIAN_POINT ( 'NONE',  ( 0.1499942179679999987, 2.750000000000000000, 0.000000000000000000 ) ) ;
#55813 = CARTESIAN_POINT ( 'NONE',  ( 8.341918146793998901, -5.601799093797000140, 7.176147756900999930 ) ) ;
#55814 = CARTESIAN_POINT ( 'NONE',  ( 17.97798355280614402, 0.5935699150349397213, -13.98741755999924941 ) ) ;
#55815 = ORIENTED_EDGE ( 'NONE', *, *, #43986, .F. ) ;
#55816 = CARTESIAN_POINT ( 'NONE',  ( 10.94027433962292228, 9.313027398374178034, -6.234466045321436667 ) ) ;
#55817 = CARTESIAN_POINT ( 'NONE',  ( 8.856463691919834957, -5.100000000000000533, 6.665341197420979746 ) ) ;
#55818 = LINE ( 'NONE', #50225, #44895 ) ;
#55819 = CARTESIAN_POINT ( 'NONE',  ( 25.30000327618300204, 2.078227429405999693, -11.31065739696999906 ) ) ;
#55820 = CARTESIAN_POINT ( 'NONE',  ( 17.80000000005199823, -3.345268251980999974, 11.86064071431999878 ) ) ;
#55821 = ORIENTED_EDGE ( 'NONE', *, *, #38593, .F. ) ;
#55822 = CARTESIAN_POINT ( 'NONE',  ( 8.834364158772999076, 4.141907758973999876, 6.047574021139999978 ) ) ;
#55823 = CARTESIAN_POINT ( 'NONE',  ( 12.72092075291392987, -3.120619064207171611, -13.52200130461745431 ) ) ;
#55824 = CYLINDRICAL_SURFACE ( 'NONE', #50617, 0.5000000000000004441 ) ;
#55825 = SURFACE_SIDE_STYLE ('',( #12481 ) ) ;
#55826 = CARTESIAN_POINT ( 'NONE',  ( 9.702711596877973577, -5.100000000000000533, 6.305985889537642386 ) ) ;
#55827 = EDGE_LOOP ( 'NONE', ( #8107, #32569, #29585, #52790 ) ) ;
#55828 = CARTESIAN_POINT ( 'NONE',  ( 10.71685100253999856, -2.832432432432000269, 6.822293592207000934 ) ) ;
#55829 = DIRECTION ( 'NONE',  ( 1.000000000000000000, 2.664535258987999937E-14, 3.552713678651000428E-14 ) ) ;
#55830 = CARTESIAN_POINT ( 'NONE',  ( 3.499999999999999556, 1.472012334232528197, 3.007095132810396976 ) ) ;
#55831 = CARTESIAN_POINT ( 'NONE',  ( 24.01967453583397472, -3.345244851302060063, -12.71086981538412708 ) ) ;
#55832 = CARTESIAN_POINT ( 'NONE',  ( 5.500000000000000000, 0.000000000000000000, 0.000000000000000000 ) ) ;
#55833 = CARTESIAN_POINT ( 'NONE',  ( 12.54664124763764121, -0.5694488842926265226, -13.88429844810376323 ) ) ;
#55834 = CARTESIAN_POINT ( 'NONE',  ( 18.17157907633054137, -2.603049611614717040, 12.42699283961531265 ) ) ;
#55835 = ORIENTED_EDGE ( 'NONE', *, *, #8362, .F. ) ;
#55836 = CARTESIAN_POINT ( 'NONE',  ( 11.31389666366019853, -4.045876550911099656, -8.532487796751999198 ) ) ;
#55837 = ORIENTED_EDGE ( 'NONE', *, *, #19012, .T. ) ;
#55838 = CARTESIAN_POINT ( 'NONE',  ( 24.30000000000000071, -12.80696435099000041, -50.50083396221000243 ) ) ;
#55839 = CARTESIAN_POINT ( 'NONE',  ( 9.029445280412998542, 5.442817578555000146, -8.106149115450000053 ) ) ;
#55840 = CARTESIAN_POINT ( 'NONE',  ( 2.880411394923000135, 3.016179945678000074, 1.524104863001999988 ) ) ;
#55841 = CARTESIAN_POINT ( 'NONE',  ( 10.32701825126999928, -5.663784181836000187, -6.682035927671000408 ) ) ;
#55842 = EDGE_CURVE ( 'NONE', #13264, #35196, #31415, .T. ) ;
#55843 = CARTESIAN_POINT ( 'NONE',  ( 7.856851002541000106, 2.832432432432000269, -6.822293592207000934 ) ) ;
#55844 = CARTESIAN_POINT ( 'NONE',  ( 6.998282674564999972, -1.401716800305999877, -2.564925509195000141E-10 ) ) ;
#55845 = VERTEX_POINT ( 'NONE', #10890 ) ;
#55846 = EDGE_CURVE ( 'NONE', #69137, #19003, #34769, .T. ) ;
#55847 = CARTESIAN_POINT ( 'NONE',  ( 10.85410941423799791, -3.257202320419700037, 8.174686939644999484 ) ) ;
#55848 = CARTESIAN_POINT ( 'NONE',  ( 10.20577346834789267, 5.100000000000000533, -6.304440313861127798 ) ) ;
#55849 = B_SPLINE_CURVE_WITH_KNOTS ( 'NONE', 3,
 ( #55326, #29116, #38905, #54277 ),
 .UNSPECIFIED., .F., .F.,
 ( 4, 4 ),
 ( 0.000000000000000000, 1.000000000000000000 ),
 .UNSPECIFIED. ) ;
#55850 = B_SPLINE_CURVE_WITH_KNOTS ( 'NONE', 3,
 ( #22363, #16764, #60123, #54875, #28662, #65702, #34251, #17825, #55571, #23052, #12574, #12924, #39140, #44402 ),
 .UNSPECIFIED., .F., .F.,
 ( 4, 2, 2, 2, 2, 2, 4 ),
 ( 0.1255288163819863745, 0.2191764973934874350, 0.3128241784049884955, 0.4064718594164895560, 0.5001195404279905610, 0.6874149024509927930, 0.8747102644739948030 ),
 .UNSPECIFIED. ) ;
#55851 = LINE ( 'NONE', #45705, #51631 ) ;
#55852 = LINE ( 'NONE', #6910, #68926 ) ;
#55854 = CARTESIAN_POINT ( 'NONE',  ( 9.136338985489343756, 3.395526279446049678, 8.727102369890431532 ) ) ;
#55853 = CARTESIAN_POINT ( 'NONE',  ( 9.318724127987000116, 2.755029797911999978, 8.795125756257000660 ) ) ;
#55855 = CARTESIAN_POINT ( 'NONE',  ( 10.40749413291699987, 4.788043169210699723, -7.140435631538599281 ) ) ;
#55856 = CARTESIAN_POINT ( 'NONE',  ( 25.29995758267499895, -11.13046986584000031, -3.427500733308000314 ) ) ;
#55857 = CARTESIAN_POINT ( 'NONE',  ( 9.401721904869997815, 4.875830726371099821, -7.991693846894699860 ) ) ;
#55858 = CARTESIAN_POINT ( 'NONE',  ( 18.00565376249822336, -0.5635217852606937416, 12.58739276154098086 ) ) ;
#55859 = CARTESIAN_POINT ( 'NONE',  ( 7.294792651996000465, -0.9657653571052000618, 0.5483950127678999253 ) ) ;
#55860 = CARTESIAN_POINT ( 'NONE',  ( 8.114220007854932248, 5.048039997173753513, -6.491766777592614446 ) ) ;
#55861 = CARTESIAN_POINT ( 'NONE',  ( 10.06949528041000086, 4.910370880657999315, -8.649591080567999413 ) ) ;
#55862 = ORIENTED_EDGE ( 'NONE', *, *, #6826, .T. ) ;
#55863 = CARTESIAN_POINT ( 'NONE',  ( 8.630418146794999856, -5.808258301303999893, 7.446016267012000256 ) ) ;
#55864 = CARTESIAN_POINT ( 'NONE',  ( 18.14518304970620477, 2.942254210842375262, 13.68733852372544568 ) ) ;
#55865 = CARTESIAN_POINT ( 'NONE',  ( 11.09999058424243046, -2.671414376110614164, 6.690776694877762942 ) ) ;
#55866 = CARTESIAN_POINT ( 'NONE',  ( 10.07503300763299947, -3.118110956362800223, -8.424978748982498544 ) ) ;
#55867 = ORIENTED_EDGE ( 'NONE', *, *, #1617, .F. ) ;
#55868 = CARTESIAN_POINT ( 'NONE',  ( 8.732392219593000604, 2.806082850903000026, 8.615880516515998622 ) ) ;
#55869 = AXIS2_PLACEMENT_3D ( 'NONE', #21419, #10248, #10591 ) ;
#55871 = LINE ( 'NONE', #2382, #27628 ) ;
#55870 = CARTESIAN_POINT ( 'NONE',  ( 10.09259632033899834, -4.802737635155300389, -7.172402329663099430 ) ) ;
#55872 = CARTESIAN_POINT ( 'NONE',  ( 9.888314158772001150, 5.105193280231000053, -8.895607399415000671 ) ) ;
#55873 = VERTEX_POINT ( 'NONE', #16476 ) ;
#55874 = B_SPLINE_CURVE_WITH_KNOTS ( 'NONE', 3,
 ( #17707, #39030, #45310, #13834, #66616, #50890, #34819, #60345, #2985, #49855 ),
 .UNSPECIFIED., .F., .F.,
 ( 4, 2, 2, 2, 4 ),
 ( 0.000000000000000000, 0.2500000000000006661, 0.5000000000000013323, 0.7500000000000006661, 1.000000000000000000 ),
 .UNSPECIFIED. ) ;
#55875 = EDGE_CURVE ( 'NONE', #1268, #18238, #37806, .T. ) ;
#55876 = CARTESIAN_POINT ( 'NONE',  ( 10.30047009227000032, 4.027768540959000276, 9.431354536774000152 ) ) ;
#55877 = CARTESIAN_POINT ( 'NONE',  ( 13.56663763856171734, -9.565814837444753138, -7.877123307579370071 ) ) ;
#55878 = CARTESIAN_POINT ( 'NONE',  ( 11.01456785386839954, 3.053605396817899997, 6.863111178199799767 ) ) ;
#55879 = CARTESIAN_POINT ( 'NONE',  ( 11.03855816545999957, -2.974093234901999949, 8.716125417860000724 ) ) ;
#55880 = CARTESIAN_POINT ( 'NONE',  ( 9.832537864288001472, 2.899999999999999911, 6.571291218949999902 ) ) ;
#55881 = ORIENTED_EDGE ( 'NONE', *, *, #52699, .F. ) ;
#55882 = DIRECTION ( 'NONE',  ( -1.000000000000000000, 0.000000000000000000, 0.000000000000000000 ) ) ;
#55883 = ADVANCED_FACE ( 'NONE', ( #32568 ), #53880, .T. ) ;
#55884 = EDGE_CURVE ( 'NONE', #65259, #64287, #60860, .T. ) ;
#55885 = CARTESIAN_POINT ( 'NONE',  ( 10.65229194037999960, -4.944342461481999962, -8.478476072358999360 ) ) ;
#55886 = AXIS2_PLACEMENT_3D ( 'NONE', #12973, #50368, #67121 ) ;
#55887 = CARTESIAN_POINT ( 'NONE',  ( 7.916668338613877864, -2.408209902419789827, 8.201634448280884726 ) ) ;
#55888 = CARTESIAN_POINT ( 'NONE',  ( 9.013429960698999821, -4.933961117404000341, 8.417889755737999025 ) ) ;
#55889 = CARTESIAN_POINT ( 'NONE',  ( 11.68788784977535933, -4.985985832792199979, -7.443657794094239222 ) ) ;
#55890 = CARTESIAN_POINT ( 'NONE',  ( 9.400113844317999678, -3.746347404385800051, 8.471855267550699509 ) ) ;
#55891 = VERTEX_POINT ( 'NONE', #44453 ) ;
#55892 = CARTESIAN_POINT ( 'NONE',  ( 24.30001697071400457, -8.938702858184001343, 8.938676113071998941 ) ) ;
#55893 = CARTESIAN_POINT ( 'NONE',  ( 11.29303032197930001, -3.336467919271199900, 8.427909097977700270 ) ) ;
#55894 = VERTEX_POINT ( 'NONE', #61209 ) ;
#55895 = FACE_OUTER_BOUND ( 'NONE', #39469, .T. ) ;
#55896 = ORIENTED_EDGE ( 'NONE', *, *, #42187, .F. ) ;
#55897 = CARTESIAN_POINT ( 'NONE',  ( 18.49985170088394426, -7.837663500889314729E-14, -12.52499999999998792 ) ) ;
#55898 = CARTESIAN_POINT ( 'NONE',  ( 9.491735841231999871, 3.920043641733999884, -9.398198753036000497 ) ) ;
#55899 = CARTESIAN_POINT ( 'NONE',  ( 11.13746005378019888, 5.161099018038999731, -6.879992063401499713 ) ) ;
#55900 = DIRECTION ( 'NONE',  ( 0.000000000000000000, -0.7455306007789014311, -0.6664713972124013397 ) ) ;
#55901 = CARTESIAN_POINT ( 'NONE',  ( 12.19329499274038398, 2.371606608387608617, -12.48058234101797126 ) ) ;
#55902 = CARTESIAN_POINT ( 'NONE',  ( 11.24795391537420031, -3.169881940022800215, 6.936213817702099327 ) ) ;
#55903 = CARTESIAN_POINT ( 'NONE',  ( 11.32035090130999855, -3.241273085157000189, 7.030721746772699454 ) ) ;
#55904 = ADVANCED_FACE ( 'NONE', ( #51059 ), #19235, .F. ) ;
#55905 = ORIENTED_EDGE ( 'NONE', *, *, #43168, .T. ) ;
#55906 = CARTESIAN_POINT ( 'NONE',  ( 9.771013540183334456, 3.231816600031359066, 8.499583552997725278 ) ) ;
#55907 = ORIENTED_EDGE ( 'NONE', *, *, #60533, .T. ) ;
#55908 = CARTESIAN_POINT ( 'NONE',  ( 9.475897313459000770, -4.122021308488999836, 9.013573548576999883 ) ) ;
#55909 = CARTESIAN_POINT ( 'NONE',  ( 17.74534446683163225, -0.7110419930699923841, 13.98197980709423760 ) ) ;
#55910 = EDGE_LOOP ( 'NONE', ( #65990, #5142, #20183, #32408 ) ) ;
#55911 = CARTESIAN_POINT ( 'NONE',  ( 12.12640605329509391, -2.733942857944761329, -12.29982446443561628 ) ) ;
#55912 = CARTESIAN_POINT ( 'NONE',  ( 10.37872469555899890, 4.502158848185001006, 8.368784980615899372 ) ) ;
#55913 = CARTESIAN_POINT ( 'NONE',  ( 11.09992055961999924, -2.373397911211000189, -6.776606350776999577 ) ) ;
#55914 = CARTESIAN_POINT ( 'NONE',  ( 6.471693173016667799, -0.7554284705563540925, 1.310679582531384391 ) ) ;
#55915 = CARTESIAN_POINT ( 'NONE',  ( 11.09999607187999970, -1.407106888317999793, -11.46396986501999926 ) ) ;
#55916 = CARTESIAN_POINT ( 'NONE',  ( 9.783303357172172809, 5.333269419498685160, -6.342932607636153186 ) ) ;
#55917 = CARTESIAN_POINT ( 'NONE',  ( 12.52635726938502003, -3.059519608057332807, -13.53867825407381176 ) ) ;
#55918 = CARTESIAN_POINT ( 'NONE',  ( 18.15913468976204825, -0.1616215023347997159, -12.69863621249089825 ) ) ;
#55919 = CARTESIAN_POINT ( 'NONE',  ( 11.81056516821459823, -3.390321848206700128, -8.115298063151199059 ) ) ;
#55920 = DIRECTION ( 'NONE',  ( 0.000000000000000000, 0.000000000000000000, -1.000000000000000000 ) ) ;
#55921 = CARTESIAN_POINT ( 'NONE',  ( 8.058767219590999176, 2.432118421226999949, 6.597517552098000060 ) ) ;
#55922 = ORIENTED_EDGE ( 'NONE', *, *, #63111, .F. ) ;
#55923 = PRESENTATION_STYLE_ASSIGNMENT (( #29024 ) ) ;
#55924 = LINE ( 'NONE', #39845, #61512 ) ;
#55925 = CARTESIAN_POINT ( 'NONE',  ( 18.16706615774980449, 2.626761370952298336, 13.64570327794280757 ) ) ;
#55926 = CARTESIAN_POINT ( 'NONE',  ( 10.91943903453000075, 3.268382602297999817, -6.413946631105000407 ) ) ;
#55927 = AXIS2_PLACEMENT_3D ( 'NONE', #12932, #34258, #55581 ) ;
#55928 = VECTOR ( 'NONE', #3631, 1000.000000000000000 ) ;
#55929 = CARTESIAN_POINT ( 'NONE',  ( 17.85706045311519929, 3.134356930968896116, 12.20392612899626528 ) ) ;
#55930 = CARTESIAN_POINT ( 'NONE',  ( 17.55505043854143565, 3.125000000000000000, -12.28374638332999602 ) ) ;
#55931 = CARTESIAN_POINT ( 'NONE',  ( 9.533434135307000901, 2.564753581125000181, 6.150586364588000343 ) ) ;
#55932 = EDGE_CURVE ( 'NONE', #57184, #61413, #4770, .T. ) ;
#55933 = CARTESIAN_POINT ( 'NONE',  ( 11.50705667793316778, -3.398423525757989339, -8.661791977777625107 ) ) ;
#55934 = VERTEX_POINT ( 'NONE', #29755 ) ;
#55935 = CARTESIAN_POINT ( 'NONE',  ( 12.26151780194103935, -2.191289199348898986, 12.51818198400761339 ) ) ;
#55936 = CARTESIAN_POINT ( 'NONE',  ( 10.31155864497999808, -3.317414799430800088, -8.034587760591801242 ) ) ;
#55937 = CARTESIAN_POINT ( 'NONE',  ( 11.09425120759000016, 2.431871068503000277, 7.769513029648000391 ) ) ;
#55938 = CARTESIAN_POINT ( 'NONE',  ( 12.26077869730539938, -4.595338376575799799, 8.673950353177000139 ) ) ;
#55939 = CARTESIAN_POINT ( 'NONE',  ( 10.44841638348500013, 2.891666689023999925, -7.230023356477299323 ) ) ;
#55940 = CARTESIAN_POINT ( 'NONE',  ( 12.19636936301369978, 0.1422617729927580787, 12.69893308522357245 ) ) ;
#55941 = CARTESIAN_POINT ( 'NONE',  ( 7.416892219589999335, 3.448180532882000104, 9.222462917385000125 ) ) ;
#55942 = CARTESIAN_POINT ( 'NONE',  ( 9.228133567168001150, 2.875367362387999837, 8.669940206484001877 ) ) ;
#55943 = CARTESIAN_POINT ( 'NONE',  ( 12.49819407809062177, 1.955416873541953038, 12.56189665940130773 ) ) ;
#55944 = ORIENTED_EDGE ( 'NONE', *, *, #38432, .F. ) ;
#55945 = CARTESIAN_POINT ( 'NONE',  ( 9.494689158774999527, 2.824732249080000202, -8.992748220058999209 ) ) ;
#55946 = CARTESIAN_POINT ( 'NONE',  ( 10.17349413291699811, 5.162701151235999930, -6.969488574374499201 ) ) ;
#55947 = CARTESIAN_POINT ( 'NONE',  ( 10.81600392782857867, -4.193768045697381375, 9.228900182785400474 ) ) ;
#55949 = FACE_OUTER_BOUND ( 'NONE', #3672, .T. ) ;
#55948 = FACE_OUTER_BOUND ( 'NONE', #1788, .T. ) ;
#55950 = CARTESIAN_POINT ( 'NONE',  ( 9.856038493598999750, -3.273092657276900130, 8.193143574899998782 ) ) ;
#55951 = CARTESIAN_POINT ( 'NONE',  ( 10.30487885159599770, -3.003595720052600448, -7.381132626649399064 ) ) ;
#55952 = VERTEX_POINT ( 'NONE', #55622 ) ;
#55953 = CARTESIAN_POINT ( 'NONE',  ( 2.216204174507999891, 2.754481206214999922, -1.355138954038999977 ) ) ;
#55954 = CARTESIAN_POINT ( 'NONE',  ( 18.13610002190272752, -0.2304169715717201972, -12.69719098617233222 ) ) ;
#55955 = DIRECTION ( 'NONE',  ( 0.000000000000000000, -0.2714570858282905341, -0.9624505444715651947 ) ) ;
#55956 = CARTESIAN_POINT ( 'NONE',  ( 7.000000000000000000, -6.495643345158865323, 2.999999999999999556 ) ) ;
#55957 = CARTESIAN_POINT ( 'NONE',  ( 24.35145719007200071, -12.30648751194999946, 3.205655321895999776 ) ) ;
#55958 = CARTESIAN_POINT ( 'NONE',  ( 16.01451879247772681, 8.585242134253062929, 7.875498515383617892 ) ) ;
#55959 = CYLINDRICAL_SURFACE ( 'NONE', #19694, 1.000000000000000000 ) ;
#55960 = CARTESIAN_POINT ( 'NONE',  ( 7.100000000000000533, 13.04986661130000059, 1.811520473896000016 ) ) ;
#55961 = CARTESIAN_POINT ( 'NONE',  ( 8.785191940379998954, -5.414909314743000301, 8.890670256079998168 ) ) ;
#55962 = ORIENTED_EDGE ( 'NONE', *, *, #50434, .F. ) ;
#55963 = AXIS2_PLACEMENT_3D ( 'NONE', #58187, #21128, #53631 ) ;
#55964 = CARTESIAN_POINT ( 'NONE',  ( 8.470295280410999439, 4.255646040929000229, 9.114085578076998928 ) ) ;
#55965 = ADVANCED_FACE ( 'NONE', ( #35334 ), #8701, .F. ) ;
#55966 = ADVANCED_FACE ( 'NONE', ( #50372 ), #56648, .T. ) ;
#55967 = CARTESIAN_POINT ( 'NONE',  ( 10.97216345563000139, 5.142214104516000361, 4.994019176338999166 ) ) ;
#55968 = DIRECTION ( 'NONE',  ( 2.887756364189944304E-10, 0.4812251768484908099, -0.8765970164032835799 ) ) ;
#55969 = CARTESIAN_POINT ( 'NONE',  ( 17.55505043854144276, -0.6250000000000001110, 13.88107975066923316 ) ) ;
#55970 = CARTESIAN_POINT ( 'NONE',  ( 1.695565801737999978, 3.378571531507999826, -0.5657499728117999505 ) ) ;
#55971 = VERTEX_POINT ( 'NONE', #7721 ) ;
#55972 = CARTESIAN_POINT ( 'NONE',  ( 10.62549262324159471, 5.350086361208822971, -7.676738019119362377 ) ) ;
#55973 = DIRECTION ( 'NONE',  ( 0.000000000000000000, 1.000000000000000000, 0.000000000000000000 ) ) ;
#55974 = CARTESIAN_POINT ( 'NONE',  ( 9.442087588264000075, 4.742492734433000123, 8.809983635807000724 ) ) ;
#55975 = CARTESIAN_POINT ( 'NONE',  ( 10.52641638348499953, 3.025038519517300184, 7.737488872214999702 ) ) ;
#55977 = CARTESIAN_POINT ( 'NONE',  ( 8.624774230494178795, -4.944546604704892268, 6.044843339268166638 ) ) ;
#55976 = AXIS2_PLACEMENT_3D ( 'NONE', #49814, #66229, #55060 ) ;
#55978 = CARTESIAN_POINT ( 'NONE',  ( 4.599999999999999645, -12.59999999999999964, 1.543054966925665076E-15 ) ) ;
#55979 = CARTESIAN_POINT ( 'NONE',  ( 11.53926831409257403, 3.396912098314702977, -11.84566400435341649 ) ) ;
#55980 = DIRECTION ( 'NONE',  ( -0.6684585169941805738, 0.6684585169941805738, 0.3260773253629903334 ) ) ;
#55981 = CARTESIAN_POINT ( 'NONE',  ( 9.629471092178999214, 5.100000000000000533, 6.152188490330000370 ) ) ;
#55982 = EDGE_CURVE ( 'NONE', #58563, #48158, #66791, .T. ) ;
#55983 = CARTESIAN_POINT ( 'NONE',  ( 7.651169844548746823, 5.420674159255254310, 6.473016521238817766 ) ) ;
#55984 = ORIENTED_EDGE ( 'NONE', *, *, #7482, .T. ) ;
#55985 = B_SPLINE_CURVE_WITH_KNOTS ( 'NONE', 3,
 ( #5862, #48522, #632, #17041 ),
 .UNSPECIFIED., .F., .F.,
 ( 4, 4 ),
 ( 0.000000000000000000, 1.000000000000000000 ),
 .UNSPECIFIED. ) ;
#55986 = CARTESIAN_POINT ( 'NONE',  ( 17.92131488010602069, -1.993461139475334321, 13.76793304563129361 ) ) ;
#55987 = CARTESIAN_POINT ( 'NONE',  ( 11.18272066707849888, -2.906477115133000222, -6.838543969064300398 ) ) ;
#55988 = VERTEX_POINT ( 'NONE', #55960 ) ;
#55989 = CARTESIAN_POINT ( 'NONE',  ( 29.60000000000000142, -2.052090822757999903E-07, 7.720759220056000238 ) ) ;
#55990 = ADVANCED_FACE ( 'NONE', ( #2472 ), #13662, .T. ) ;
#55991 = CARTESIAN_POINT ( 'NONE',  ( 10.36325056272499978, 4.892034740700499817, 7.486779603004729111 ) ) ;
#55992 = FACE_OUTER_BOUND ( 'NONE', #13350, .T. ) ;
#55993 = CARTESIAN_POINT ( 'NONE',  ( 9.819055905797000605, 2.899999999999999911, -6.571291218949999902 ) ) ;
#55994 = CARTESIAN_POINT ( 'NONE',  ( 9.256664404737000140, 4.025830366070999311, 9.295863330698999505 ) ) ;
#55995 = CARTESIAN_POINT ( 'NONE',  ( 10.48734600210000067, 4.351287276768000645, -6.182257940481999725 ) ) ;
#55996 = CARTESIAN_POINT ( 'NONE',  ( 10.14601354018232904, -3.000416447002271170, -6.731816600031360842 ) ) ;
#55997 = CARTESIAN_POINT ( 'NONE',  ( 10.64872180584000105, -2.614778238704999591, 6.717279975758000177 ) ) ;
#55998 = CARTESIAN_POINT ( 'NONE',  ( 17.55505043854144276, 0.7192913403693124152, -12.57945229203838267 ) ) ;
#55999 = DIRECTION ( 'NONE',  ( 0.000000000000000000, 0.000000000000000000, -1.000000000000000000 ) ) ;
#56000 = CARTESIAN_POINT ( 'NONE',  ( 10.72749279009019929, -4.225282629687599822, -8.336388861178200216 ) ) ;
#56001 = CARTESIAN_POINT ( 'NONE',  ( 23.58888327362420867, -10.33109198681894902, 9.338987663515077031 ) ) ;
#56002 = EDGE_LOOP ( 'NONE', ( #64467, #19036, #37236, #23191, #10659 ) ) ;
#56003 = CARTESIAN_POINT ( 'NONE',  ( 0.6736883816833351135, 0.9084612428644865956, -3.122795580015885974 ) ) ;
#56004 = CARTESIAN_POINT ( 'NONE',  ( 24.44496488009700030, 8.810487470433001178, 8.810507756548000557 ) ) ;
#56005 = CARTESIAN_POINT ( 'NONE',  ( 8.905196823546312146, 4.608202637908532573, 6.627513167511573045 ) ) ;
#56006 = CARTESIAN_POINT ( 'NONE',  ( 9.185590450029499365, 5.092272840597500405, 8.129537449122580028 ) ) ;
#56007 = CARTESIAN_POINT ( 'NONE',  ( 12.43878596651942026, 1.993461161472736887, 13.76788477248720177 ) ) ;
#56008 = CARTESIAN_POINT ( 'NONE',  ( 10.81579453138999902, -5.374572909254000663, 6.698726302909000729 ) ) ;
#56009 = ORIENTED_EDGE ( 'NONE', *, *, #10783, .F. ) ;
#56010 = CARTESIAN_POINT ( 'NONE',  ( 12.18006440151454939, -0.02055073170813858166, -12.69999918148730700 ) ) ;
#56011 = CARTESIAN_POINT ( 'NONE',  ( 12.39285819377765918, -0.4699225802676950670, 13.88930950616751936 ) ) ;
#56012 = ORIENTED_EDGE ( 'NONE', *, *, #4071, .F. ) ;
#56013 = CARTESIAN_POINT ( 'NONE',  ( 11.12299956498149811, -2.792989229543000107, -7.825000000000000178 ) ) ;
#56014 = CARTESIAN_POINT ( 'NONE',  ( 24.39664321829268800, 12.03536693101104049, -3.224866849775587241 ) ) ;
#56015 = CARTESIAN_POINT ( 'NONE',  ( 23.61264779926599999, -3.132474875089000133, -13.53881878004999884 ) ) ;
#56016 = CARTESIAN_POINT ( 'NONE',  ( -15.86200481174999943, 5.599999999999999645, 6.571291218949999902 ) ) ;
#56017 = CARTESIAN_POINT ( 'NONE',  ( 24.44496350777200178, -12.03536639536000052, -3.224849854974999985 ) ) ;
#56018 = CARTESIAN_POINT ( 'NONE',  ( 11.07144391099999936, 7.549533471103999638, -6.458582346940000107 ) ) ;
#56019 = CARTESIAN_POINT ( 'NONE',  ( -0.02733730371250999922, 2.854424451075999958, -2.356853325602000115 ) ) ;
#56020 = VECTOR ( 'NONE', #21010, 1000.000000000000000 ) ;
#56021 = CARTESIAN_POINT ( 'NONE',  ( 23.59999445750599989, -13.22316420035999940, -4.267800004853000040 ) ) ;
#56022 = DIRECTION ( 'NONE',  ( -1.000000000000000000, 0.000000000000000000, 0.000000000000000000 ) ) ;
#56023 = CARTESIAN_POINT ( 'NONE',  ( 9.485316810687001166, -2.477793449086000077, -8.275032865112999403 ) ) ;
#56024 = CARTESIAN_POINT ( 'NONE',  ( 11.41672066707849886, 4.741156262620799922, -7.051685395375099752 ) ) ;
#56025 = DIRECTION ( 'NONE',  ( 1.000000000000000000, 0.000000000000000000, 0.000000000000000000 ) ) ;
#56026 = CARTESIAN_POINT ( 'NONE',  ( 11.31900581613029821, 4.750686773407899466, -7.982035256002799173 ) ) ;
#56027 = CARTESIAN_POINT ( 'NONE',  ( 10.01258376188599897, 3.037118682679400106, -8.113672563022399586 ) ) ;
#56029 = CARTESIAN_POINT ( 'NONE',  ( 11.49999970531878546, -5.098631745860898512, 7.402706825368051469 ) ) ;
#56028 = CARTESIAN_POINT ( 'NONE',  ( 15.78404792230800346, -8.744893293839998805, -7.778646260181000471 ) ) ;
#56030 = CARTESIAN_POINT ( 'NONE',  ( 10.97534709859367474, -5.193992591243323353, -6.717726803882955622 ) ) ;
#56031 = ORIENTED_EDGE ( 'NONE', *, *, #16561, .T. ) ;
#56032 = DIRECTION ( 'NONE',  ( 0.000000000000000000, 0.000000000000000000, -1.000000000000000000 ) ) ;
#56033 = AXIS2_PLACEMENT_3D ( 'NONE', #56435, #8537, #29887 ) ;
#56034 = CARTESIAN_POINT ( 'NONE',  ( 10.31167756636999933, -2.874479384703000129, 8.900026329558999194 ) ) ;
#56035 = CARTESIAN_POINT ( 'NONE',  ( 9.503038493598998215, 4.726907342723099426, 8.193143574899998782 ) ) ;
#56036 = CARTESIAN_POINT ( 'NONE',  ( 10.84184687351628540, -4.999583552997724389, -6.731816600031354625 ) ) ;
#56037 = CARTESIAN_POINT ( 'NONE',  ( 10.99934110471000004, -5.081022574063999819, 8.239050178861999640 ) ) ;
#56038 = CARTESIAN_POINT ( 'NONE',  ( 0.07500030076246999577, 0.000000000000000000, 0.000000000000000000 ) ) ;
#56039 = VERTEX_POINT ( 'NONE', #3161 ) ;
#56040 = EDGE_CURVE ( 'NONE', #51763, #23757, #36643, .T. ) ;
#56041 = EDGE_CURVE ( 'NONE', #6927, #49400, #1786, .T. ) ;
#56042 = CARTESIAN_POINT ( 'NONE',  ( 9.480671671056999372, -5.126041103316000047, -7.689118697196099639 ) ) ;
#56043 = CARTESIAN_POINT ( 'NONE',  ( 0.07500030076246999577, 0.000000000000000000, 0.000000000000000000 ) ) ;
#56044 = CARTESIAN_POINT ( 'NONE',  ( 18.20778913885554218, 2.166651812353023843, -12.41232206190563225 ) ) ;
#56045 = DIRECTION ( 'NONE',  ( 5.026600068074292105E-17, 0.6482718649732923666, 0.7614089499631913061 ) ) ;
#56046 = LINE ( 'NONE', #35420, #4922 ) ;
#56047 = LINE ( 'NONE', #2903, #62145 ) ;
#56048 = CARTESIAN_POINT ( 'NONE',  ( 9.394730517101999467, -2.624921803719999946, -8.200122328058998988 ) ) ;
#56049 = CARTESIAN_POINT ( 'NONE',  ( 10.20577346834789267, -5.100000000000000533, -6.304440313861129574 ) ) ;
#56050 = ORIENTED_EDGE ( 'NONE', *, *, #8691, .F. ) ;
#56051 = CARTESIAN_POINT ( 'NONE',  ( -2.444943969992999916E-05, -2.899969545325999931, 0.000000000000000000 ) ) ;
#56052 = CARTESIAN_POINT ( 'NONE',  ( 12.48353988083097477, -0.6549277419692678404, -13.98467727287826889 ) ) ;
#56053 = CARTESIAN_POINT ( 'NONE',  ( 13.91144947526900033, -8.829982735797999638, -7.819410275689000045 ) ) ;
#56054 = CARTESIAN_POINT ( 'NONE',  ( 11.09999999999999964, -2.700688486617000006, 5.124965750789000296 ) ) ;
#56055 = CARTESIAN_POINT ( 'NONE',  ( 2.289363843320874725, -3.114462284487641064, -1.632227178342312790 ) ) ;
#56056 = CARTESIAN_POINT ( 'NONE',  ( 8.225464158772000545, 3.844886277615000125, -8.888911790991000927 ) ) ;
#56057 = CARTESIAN_POINT ( 'NONE',  ( 6.612810627809117214, -1.144927662556009196, -1.005512116229802189 ) ) ;
#56058 = VERTEX_POINT ( 'NONE', #45814 ) ;
#56059 = AXIS2_PLACEMENT_3D ( 'NONE', #34151, #61735, #23310 ) ;
#56060 = CARTESIAN_POINT ( 'NONE',  ( 9.115000000004000569, -5.349999999999999645, -7.500000000000000000 ) ) ;
#56061 = CARTESIAN_POINT ( 'NONE',  ( 17.92131488010598517, 1.993461139475334321, -13.76793304563128828 ) ) ;
#56062 = VERTEX_POINT ( 'NONE', #23798 ) ;
#56063 = EDGE_CURVE ( 'NONE', #15587, #16690, #67125, .T. ) ;
#56064 = CARTESIAN_POINT ( 'NONE',  ( 10.43314899746000002, -5.167567567567999731, 6.822293592207000934 ) ) ;
#56065 = CARTESIAN_POINT ( 'NONE',  ( 2.665556799210790917, 0.4581489286485003198, 3.500000000000000444 ) ) ;
#56066 = CARTESIAN_POINT ( 'NONE',  ( 8.704995280412999747, 5.140767546012999567, -6.196177269779999719 ) ) ;
#56067 = CARTESIAN_POINT ( 'NONE',  ( 24.44496264144000364, 8.810483598181999554, -8.810508341310001157 ) ) ;
#56068 = CARTESIAN_POINT ( 'NONE',  ( 11.60477869730532774, -4.467447516829900600, -6.578238193496799724 ) ) ;
#56069 = CARTESIAN_POINT ( 'NONE',  ( -0.2999999999999999889, -0.5773502691895999739, 1.000000000000000000 ) ) ;
#56070 = DIRECTION ( 'NONE',  ( 0.000000000000000000, -0.8648648648648720183, 0.5020047465136825426 ) ) ;
#56071 = EDGE_LOOP ( 'NONE', ( #43240, #26700, #65383, #24814 ) ) ;
#56072 = CARTESIAN_POINT ( 'NONE',  ( 7.712296824873548395, 4.464687595965251887, -8.784369080928565054 ) ) ;
#56073 = CARTESIAN_POINT ( 'NONE',  ( 10.77101354018233259, -4.768183399968641822, 8.499583552997725278 ) ) ;
#56074 = CARTESIAN_POINT ( 'NONE',  ( 18.15919096721063042, -2.338588349689834534, 13.70638546470246233 ) ) ;
#56075 = EDGE_LOOP ( 'NONE', ( #47113, #53031, #11301, #63514 ) ) ;
#56076 = AXIS2_PLACEMENT_3D ( 'NONE', #38557, #3225, #25232 ) ;
#56077 = CARTESIAN_POINT ( 'NONE',  ( 10.29094007826000023, 2.903522982536999919, -8.310916170934000036 ) ) ;
#56078 = CARTESIAN_POINT ( 'NONE',  ( 25.29987667925500361, 10.83443035398000021, 3.855530949778000149 ) ) ;
#56079 = ORIENTED_EDGE ( 'NONE', *, *, #32739, .F. ) ;
#56080 = CARTESIAN_POINT ( 'NONE',  ( 9.278038493598998571, 4.826346105011899645, 8.287963554181398962 ) ) ;
#56081 = CARTESIAN_POINT ( 'NONE',  ( 18.04847759739545410, -3.007479059277872402, -12.23581163759356194 ) ) ;
#56082 = B_SPLINE_CURVE_WITH_KNOTS ( 'NONE', 3,
 ( #26105, #16978, #26451, #32729, #48116, #47430, #48462, #42194, #27483, #48807, #68739, #570, #16294, #43214 ),
 .UNSPECIFIED., .F., .F.,
 ( 4, 2, 2, 2, 2, 2, 4 ),
 ( 0.000000000000000000, 0.1250000000000025813, 0.2500000000000051625, 0.5000000000000103251, 0.6250000000000096589, 0.7500000000000089928, 1.000000000000000000 ),
 .UNSPECIFIED. ) ;
#56083 = CIRCLE ( 'NONE', #59417, 2.999989272562999965 ) ;
#56084 = CARTESIAN_POINT ( 'NONE',  ( 10.99107545325904667, 5.690496933828011805, -4.958831622490459168 ) ) ;
#56085 = DIRECTION ( 'NONE',  ( 0.000000000000000000, -0.000000000000000000, 1.000000000000000000 ) ) ;
#56086 = CARTESIAN_POINT ( 'NONE',  ( 24.56500367226799852, -12.27494567759000077, -3.065703875465999761 ) ) ;
#56087 = CARTESIAN_POINT ( 'NONE',  ( 9.381635378478234699, -2.862680139623721587, 8.816521241667800268 ) ) ;
#56088 = ORIENTED_EDGE ( 'NONE', *, *, #63340, .F. ) ;
#56089 = CARTESIAN_POINT ( 'NONE',  ( 10.34393020684899867, 2.750000000000000000, 7.500000000000000000 ) ) ;
#56090 = CARTESIAN_POINT ( 'NONE',  ( 10.91733584123000078, 3.256275267152000108, -6.361562334135999919 ) ) ;
#56091 = CARTESIAN_POINT ( 'NONE',  ( 10.86133765299000054, -5.065201555913000142, -5.176815510448999902 ) ) ;
#56092 = CARTESIAN_POINT ( 'NONE',  ( 12.39066945341150117, 3.117187738603023561, -13.64855991556033921 ) ) ;
#56093 = CARTESIAN_POINT ( 'NONE',  ( 9.253772138682000659, -4.476015718025199597, -6.312652778810999621 ) ) ;
#56094 = CARTESIAN_POINT ( 'NONE',  ( 10.68403590588000007, -5.436611040123999317, 8.578433628717998971 ) ) ;
#56095 = CARTESIAN_POINT ( 'NONE',  ( 17.55505043854144276, 0.7302158263239096891, 13.98094363220831049 ) ) ;
#56096 = CARTESIAN_POINT ( 'NONE',  ( 7.861476898152417903, 5.109672693010819167, 6.687167769525764527 ) ) ;
#56097 = EDGE_CURVE ( 'NONE', #48769, #65610, #45131, .T. ) ;
#56098 = EDGE_CURVE ( 'NONE', #68689, #59129, #52251, .T. ) ;
#56099 = ORIENTED_EDGE ( 'NONE', *, *, #39223, .T. ) ;
#56100 = VERTEX_POINT ( 'NONE', #29411 ) ;
#56101 = CARTESIAN_POINT ( 'NONE',  ( 8.367589158771000513, 5.461114003844000031, -8.582501063019000398 ) ) ;
#56102 = DIRECTION ( 'NONE',  ( -0.000000000000000000, 1.000000000000000000, 0.000000000000000000 ) ) ;
#56103 = CARTESIAN_POINT ( 'NONE',  ( 12.19167018792508550, -2.619965297397002679, 13.64728369052816248 ) ) ;
#56104 = DIRECTION ( 'NONE',  ( 0.000000000000000000, 0.000000000000000000, 1.000000000000000000 ) ) ;
#56105 = CARTESIAN_POINT ( 'NONE',  ( 23.63066106396900068, 10.04550756903999975, -9.752170026777999823 ) ) ;
#56106 = CARTESIAN_POINT ( 'NONE',  ( 17.75917414208900169, -3.376094807733999836, -11.11072694497999969 ) ) ;
#56108 = CARTESIAN_POINT ( 'NONE',  ( 11.12341523360999851, -6.055729757550999182, 5.272785169106999348 ) ) ;
#56107 = CARTESIAN_POINT ( 'NONE',  ( 9.979721904869998994, -3.004358235431599855, 6.941043897400199114 ) ) ;
#56109 = CARTESIAN_POINT ( 'NONE',  ( 9.048318768181994542, -5.133256012319003858, -6.341058004364997558 ) ) ;
#56110 = ORIENTED_EDGE ( 'NONE', *, *, #52699, .T. ) ;
#56111 = AXIS2_PLACEMENT_3D ( 'NONE', #48298, #38144, #27323 ) ;
#56112 = DIRECTION ( 'NONE',  ( 0.000000000000000000, 0.9510565162985824550, -0.3090169943643944483 ) ) ;
#56113 = DIRECTION ( 'NONE',  ( 0.000000000000000000, -0.2461538461537953471, 0.9692307692307821076 ) ) ;
#56114 = CARTESIAN_POINT ( 'NONE',  ( 17.65762099059919521, 0.6166112555940438389, 12.67984200623734381 ) ) ;
#56115 = CARTESIAN_POINT ( 'NONE',  ( 12.18006440151460801, 0.02055073179308012851, 12.69999918148658935 ) ) ;
#56116 = CARTESIAN_POINT ( 'NONE',  ( 9.898728259668697405, -2.762655044027092721, -6.942780202613654694 ) ) ;
#56117 = VERTEX_POINT ( 'NONE', #39538 ) ;
#56119 = CARTESIAN_POINT ( 'NONE',  ( 3.500000000000000000, 3.200000000000000178, 0.000000000000000000 ) ) ;
#56118 = DIRECTION ( 'NONE',  ( -1.000000000000000000, 0.000000000000000000, 0.000000000000000000 ) ) ;
#56120 = CARTESIAN_POINT ( 'NONE',  ( 9.889535841229999846, 5.798263352390999437, -8.113145944980999502 ) ) ;
#56121 = EDGE_CURVE ( 'NONE', #35290, #11774, #54814, .T. ) ;
#56122 = DIRECTION ( 'NONE',  ( 0.000000000000000000, 0.000000000000000000, -1.000000000000000000 ) ) ;
#56123 = CARTESIAN_POINT ( 'NONE',  ( 7.810726116476000236, -5.086048788582002267, 6.527219528731996512 ) ) ;
#56124 = AXIS2_PLACEMENT_3D ( 'NONE', #7813, #19684, #35424 ) ;
#56125 = EDGE_CURVE ( 'NONE', #68711, #42806, #18562, .T. ) ;
#56126 = DIRECTION ( 'NONE',  ( 0.9999999998973936322, -8.065200975671946287E-06, 1.183914378896991529E-05 ) ) ;
#56127 = DIRECTION ( 'NONE',  ( 0.000000000000000000, 1.000000000000000000, 0.000000000000000000 ) ) ;
#56128 = CARTESIAN_POINT ( 'NONE',  ( 2.881384349028000003, -3.542840650637999911, -0.5934045645267999047 ) ) ;
#56129 = ORIENTED_EDGE ( 'NONE', *, *, #38430, .F. ) ;
#56130 = B_SPLINE_CURVE_WITH_KNOTS ( 'NONE', 3,
 ( #19011, #45248, #50481, #40336, #44571, #55386, #49440, #29528, #7838, #18329, #39653, #12389 ),
 .UNSPECIFIED., .F., .F.,
 ( 4, 2, 2, 2, 2, 4 ),
 ( 0.000000000000000000, 0.2499999999999972800, 0.3749999999999953926, 0.4374999999999937828, 0.4999999999999922284, 1.000000000000000000 ),
 .UNSPECIFIED. ) ;
#56131 = CARTESIAN_POINT ( 'NONE',  ( 12.44955242156041919, -0.5141503178158092213, -12.68598964581897626 ) ) ;
#56132 = CARTESIAN_POINT ( 'NONE',  ( 7.807254669145095249, -3.019363530874672463, 6.522727296858301216 ) ) ;
#56133 = CARTESIAN_POINT ( 'NONE',  ( 23.84129557661856680, -12.96064935002960539, -3.649606885852778593 ) ) ;
#56134 = DIRECTION ( 'NONE',  ( 0.000000000000000000, 1.000000000000000000, 0.000000000000000000 ) ) ;
#56135 = CARTESIAN_POINT ( 'NONE',  ( 10.06577346837133291, -5.100000000000000533, 6.304440313804915874 ) ) ;
#56136 = EDGE_LOOP ( 'NONE', ( #12759, #13168, #67581, #55671 ) ) ;
#56137 = CARTESIAN_POINT ( 'NONE',  ( 5.874576767391999965, -1.238562288345000040, 0.4630760545261999872 ) ) ;
#56138 = CARTESIAN_POINT ( 'NONE',  ( 7.490585841228000419, 4.468431922689999780, -6.183326950307000303 ) ) ;
#56139 = DIRECTION ( 'NONE',  ( 1.000000000000000000, 0.000000000000000000, 0.000000000000000000 ) ) ;
#56140 = FACE_OUTER_BOUND ( 'NONE', #3020, .T. ) ;
#56141 = CARTESIAN_POINT ( 'NONE',  ( 11.51656039236534923, 5.173498198882000132, -7.557111631074219460 ) ) ;
#56142 = ORIENTED_EDGE ( 'NONE', *, *, #35285, .T. ) ;
#56143 = CARTESIAN_POINT ( 'NONE',  ( 9.813358178091998951, -5.349400659402999914, 6.657024270273000255 ) ) ;
#56144 = ORIENTED_EDGE ( 'NONE', *, *, #52394, .T. ) ;
#56145 = EDGE_CURVE ( 'NONE', #40213, #31317, #57665, .T. ) ;
#56146 = CARTESIAN_POINT ( 'NONE',  ( 25.60000000000000142, 0.000000000000000000, 0.000000000000000000 ) ) ;
#56147 = CARTESIAN_POINT ( 'NONE',  ( 9.523691940378000709, -4.852736108563000528, 8.683927195503999386 ) ) ;
#56148 = CARTESIAN_POINT ( 'NONE',  ( 18.22055847946776197, 0.2899337805559810688, -13.99700184298317396 ) ) ;
#56149 = EDGE_LOOP ( 'NONE', ( #56459, #52275, #57975, #5492 ) ) ;
#56150 = CARTESIAN_POINT ( 'NONE',  ( 10.97581046457103326, 8.473166771401304587, -6.548870747866761377 ) ) ;
#56151 = CARTESIAN_POINT ( 'NONE',  ( 10.99999196979000082, -2.861044734458999627E-13, 5.200284647344000995E-13 ) ) ;
#56152 = CARTESIAN_POINT ( 'NONE',  ( 8.187214158772000872, 4.472863460285000592, -8.721137209586000694 ) ) ;
#56153 = CARTESIAN_POINT ( 'NONE',  ( 9.364763540183330903, -5.217465845835395299, -7.827184855449096368 ) ) ;
#56154 = CARTESIAN_POINT ( 'NONE',  ( 17.92628954468417746, -3.345291551440210398, 11.86067033211894284 ) ) ;
#56155 = ORIENTED_EDGE ( 'NONE', *, *, #34423, .T. ) ;
#56156 = CARTESIAN_POINT ( 'NONE',  ( 9.285188841453999586, -5.269672295101000437, 8.747824102203999530 ) ) ;
#56157 = CARTESIAN_POINT ( 'NONE',  ( 12.34838569212906556, -2.927120983245214969, -13.57349088381706181 ) ) ;
#56158 = DIRECTION ( 'NONE',  ( 0.000000000000000000, 1.000000000000000000, 0.000000000000000000 ) ) ;
#56159 = CARTESIAN_POINT ( 'NONE',  ( 16.10004050617000004, 5.773856762095636697, 11.16084031980689417 ) ) ;
#56160 = AXIS2_PLACEMENT_3D ( 'NONE', #15619, #25763, #25070 ) ;
#56161 = B_SPLINE_CURVE_WITH_KNOTS ( 'NONE', 3,
 ( #22945, #34499, #44300, #55812 ),
 .UNSPECIFIED., .F., .F.,
 ( 4, 4 ),
 ( 0.000000000000000000, 1.000000000000000000 ),
 .UNSPECIFIED. ) ;
#56162 = CARTESIAN_POINT ( 'NONE',  ( 9.766851002543001314, -2.832432432432000269, 6.822293592207000934 ) ) ;
#56163 = EDGE_LOOP ( 'NONE', ( #42480, #20881, #28885, #59231 ) ) ;
#56164 = PRODUCT ( 'Positive Post', 'Positive Post', '', ( #42123 ) ) ;
#56165 = LINE ( 'NONE', #29619, #65132 ) ;
#56166 = AXIS2_PLACEMENT_3D ( 'NONE', #38560, #33675, #60583 ) ;
#56167 = CARTESIAN_POINT ( 'NONE',  ( 11.07299956498199833, 5.207010770456999893, -7.825000000000000178 ) ) ;
#56168 = CARTESIAN_POINT ( 'NONE',  ( 10.71654029638703243, 2.829809111552286538, 6.826801520698219328 ) ) ;
#56169 = CARTESIAN_POINT ( 'NONE',  ( 9.893930206848997599, -5.250000000000000000, -7.500000000000000000 ) ) ;
#56170 = CARTESIAN_POINT ( 'NONE',  ( 6.953073139469000630, -9.233001678504999532, 5.200628701625999994 ) ) ;
#56171 = CARTESIAN_POINT ( 'NONE',  ( 12.52788616429851842, -0.5605600754933547369, -13.88478672247768664 ) ) ;
#56172 = CARTESIAN_POINT ( 'NONE',  ( 17.96249544862753922, -2.025954803622692424, 12.54949280001589074 ) ) ;
#56173 = ORIENTED_EDGE ( 'NONE', *, *, #6656, .F. ) ;
#56174 = CARTESIAN_POINT ( 'NONE',  ( 10.85168717260509830, -4.613789146762799831, -8.501809683958001074 ) ) ;
#56175 = VERTEX_POINT ( 'NONE', #51400 ) ;
#56176 = VECTOR ( 'NONE', #30282, 1000.000000000000000 ) ;
#56177 = CARTESIAN_POINT ( 'NONE',  ( 0.1499942179680000265, -2.402872127494069421, 1.384928887584812474 ) ) ;
#56178 = CARTESIAN_POINT ( 'NONE',  ( 9.128895280414001334, 3.880154689736000417, -9.060377011187000562 ) ) ;
#56179 = CARTESIAN_POINT ( 'NONE',  ( 3.089996212309999546, -3.376682894496000120, 0.1350915547969999686 ) ) ;
#56180 = CARTESIAN_POINT ( 'NONE',  ( 10.00074484908000194, -2.373896846742000299, -7.962434077545999855 ) ) ;
#56181 = CARTESIAN_POINT ( 'NONE',  ( 24.53428991195500330, 3.614319144953999530, 12.31267516478999902 ) ) ;
#56182 = AXIS2_PLACEMENT_3D ( 'NONE', #68193, #57709, #40953 ) ;
#56183 = CARTESIAN_POINT ( 'NONE',  ( 9.643637503375364517, -2.635046513920903166, -6.405124639914539841 ) ) ;
#56184 = EDGE_CURVE ( 'NONE', #8310, #47368, #20270, .T. ) ;
#56185 = EDGE_CURVE ( 'NONE', #15766, #34080, #3774, .T. ) ;
#56186 = ORIENTED_EDGE ( 'NONE', *, *, #44778, .F. ) ;
#56187 = ADVANCED_FACE ( 'NONE', ( #68843 ), #51738, .T. ) ;
#56188 = CARTESIAN_POINT ( 'NONE',  ( 11.56379841651039975, -4.401637675674300532, 6.432302808027999141 ) ) ;
#56189 = CARTESIAN_POINT ( 'NONE',  ( 9.634020792350998619, 3.042978295541999945, 8.588098960242001922 ) ) ;
#56190 = FACE_OUTER_BOUND ( 'NONE', #14203, .T. ) ;
#56191 = CARTESIAN_POINT ( 'NONE',  ( 18.29983863915590447, 0.9627071077475295446, -12.32514597913991850 ) ) ;
#56194 = B_SPLINE_CURVE_WITH_KNOTS ( 'NONE', 3,
 ( #38715, #33474, #6889, #7936 ),
 .UNSPECIFIED., .F., .F.,
 ( 4, 4 ),
 ( 0.000000000000000000, 1.000000000000000000 ),
 .UNSPECIFIED. ) ;
#56193 = FACE_OUTER_BOUND ( 'NONE', #5090, .T. ) ;
#56192 = CARTESIAN_POINT ( 'NONE',  ( 10.18756025349000005, 5.387489739490000318, 8.640945789268998922 ) ) ;
#56195 = CARTESIAN_POINT ( 'NONE',  ( 11.23610538575739959, 5.109472165990999848, -7.234742334405199315 ) ) ;
#56196 = CARTESIAN_POINT ( 'NONE',  ( 10.97054688934660049, 2.819834791696201659, -6.661904172904770327 ) ) ;
#56197 = CARTESIAN_POINT ( 'NONE',  ( 9.351063610504999346, 4.411988005505000032, -8.416028484082099581 ) ) ;
#56198 = CARTESIAN_POINT ( 'NONE',  ( 17.84362596415753188, -0.6599616342124031698, 12.58270523616455705 ) ) ;
#56199 = CARTESIAN_POINT ( 'NONE',  ( 24.51327040776200050, 3.324719603035999782, 12.06512239505999950 ) ) ;
#56200 = LINE ( 'NONE', #33850, #15437 ) ;
#56201 = CARTESIAN_POINT ( 'NONE',  ( 10.14522028041000112, 3.576529456695000331, -8.962721799438000403 ) ) ;
#56202 = VERTEX_POINT ( 'NONE', #58358 ) ;
#56203 = CARTESIAN_POINT ( 'NONE',  ( 8.181105646794000208, -5.485781663882000281, 8.532068390166999805 ) ) ;
#56204 = CIRCLE ( 'NONE', #35012, 1.999999999999999556 ) ;
#56205 = CARTESIAN_POINT ( 'NONE',  ( 18.10325613414704193, 2.040025360435026691, 13.85057320474804854 ) ) ;
#56206 = CARTESIAN_POINT ( 'NONE',  ( 23.56666365135700403, -2.009474831861002286, 11.63289034805000277 ) ) ;
#56207 = CARTESIAN_POINT ( 'NONE',  ( 10.12426357027499790, -2.745128867668000350, -7.742104041724699570 ) ) ;
#56208 = ORIENTED_EDGE ( 'NONE', *, *, #54695, .T. ) ;
#56209 = VECTOR ( 'NONE', #34883, 1000.000000000000000 ) ;
#56210 = CARTESIAN_POINT ( 'NONE',  ( 8.834364158772999076, 4.141907758973999876, 6.047574021139999978 ) ) ;
#56212 = DIRECTION ( 'NONE',  ( 0.000000000000000000, -1.000000000000000000, 0.000000000000000000 ) ) ;
#56211 = CARTESIAN_POINT ( 'NONE',  ( 8.546960841229999772, 2.724453559418999582, -8.908010318766001134 ) ) ;
#56213 = CARTESIAN_POINT ( 'NONE',  ( 10.22907665877000127, 4.838498214728000235, -5.852435699035000383 ) ) ;
#56214 = VERTEX_POINT ( 'NONE', #25858 ) ;
#56215 = CARTESIAN_POINT ( 'NONE',  ( 5.138359839683333874, -0.7554284705563483193, -1.310679582531387721 ) ) ;
#56216 = CARTESIAN_POINT ( 'NONE',  ( 17.60315097558334330, -3.246934396132596046, -13.61827533163850923 ) ) ;
#56217 = CARTESIAN_POINT ( 'NONE',  ( 10.30487885159599770, 4.996404279947399552, 7.618867373350600047 ) ) ;
#56218 = CARTESIAN_POINT ( 'NONE',  ( 9.500008250440000523, -2.279684233303000074, 7.877691491255999878 ) ) ;
#56219 = DIRECTION ( 'NONE',  ( -1.000000000000000000, 0.000000000000000000, 0.000000000000000000 ) ) ;
#56220 = VERTEX_POINT ( 'NONE', #41253 ) ;
#56221 = FACE_OUTER_BOUND ( 'NONE', #64049, .T. ) ;
#56222 = CARTESIAN_POINT ( 'NONE',  ( 10.80374194038000013, -2.766944173105999827, -8.073385940268000383 ) ) ;
#56223 = CARTESIAN_POINT ( 'NONE',  ( 7.936743961419510995, -2.283396912964382075, 7.784033659319036680 ) ) ;
#56224 = AXIS2_PLACEMENT_3D ( 'NONE', #49535, #13531, #44996 ) ;
#56225 = CARTESIAN_POINT ( 'NONE',  ( 10.37373728961999930, -2.215269876326000364, 7.703982265807999497 ) ) ;
#56226 = CARTESIAN_POINT ( 'NONE',  ( 10.84657802013509986, -5.315911219205999849, -7.469366283838649423 ) ) ;
#56227 = CARTESIAN_POINT ( 'NONE',  ( 9.628076168957999670, -4.509700402263200125, 6.634524523592600254 ) ) ;
#56228 = ORIENTED_EDGE ( 'NONE', *, *, #29225, .F. ) ;
#56229 = CARTESIAN_POINT ( 'NONE',  ( 10.85561138062999831, -5.068915657236000349, -5.151427698297999846 ) ) ;
#56230 = CARTESIAN_POINT ( 'NONE',  ( 10.94841638348500013, -5.108333310975999630, 7.769976643522699788 ) ) ;
#56231 = VERTEX_POINT ( 'NONE', #40909 ) ;
#56232 = EDGE_CURVE ( 'NONE', #51578, #33943, #53813, .T. ) ;
#56233 = CARTESIAN_POINT ( 'NONE',  ( 16.24412496488131552, -3.380981662633991913, -11.14874627148116559 ) ) ;
#56234 = CIRCLE ( 'NONE', #64042, 12.52500000000000036 ) ;
#56235 = ORIENTED_EDGE ( 'NONE', *, *, #34906, .T. ) ;
#56236 = CARTESIAN_POINT ( 'NONE',  ( 18.49993212792200126, -2.908182645667999999, -12.18276646858999968 ) ) ;
#56237 = CARTESIAN_POINT ( 'NONE',  ( 9.251970280414001380, 5.673443217382001080, -7.051790060464000476 ) ) ;
#56238 = ADVANCED_FACE ( 'NONE', ( #25170 ), #15026, .T. ) ;
#56239 = CARTESIAN_POINT ( 'NONE',  ( 14.46666666157666903, -8.833279249958291501, -7.896561128163722465 ) ) ;
#56240 = CARTESIAN_POINT ( 'NONE',  ( 15.40000000000000036, 43.28911730077999920, 38.02789377380999980 ) ) ;
#56241 = CARTESIAN_POINT ( 'NONE',  ( 12.37479069268420950, 2.046560891103777813, -12.54575476380192711 ) ) ;
#56242 = CARTESIAN_POINT ( 'NONE',  ( 11.74025954179439957, -3.228187097503200320, 6.858707791728399172 ) ) ;
#56243 = CARTESIAN_POINT ( 'NONE',  ( 8.207510841230000409, 5.944584532500000407, 7.106843289410999631 ) ) ;
#56244 = VERTEX_POINT ( 'NONE', #46505 ) ;
#56245 = CARTESIAN_POINT ( 'NONE',  ( 7.766851002543999627, 2.832432432432000269, 6.822293592207000934 ) ) ;
#56246 = CARTESIAN_POINT ( 'NONE',  ( 8.700644353210000403, -5.212258818969000451, 6.157189191035000064 ) ) ;
#56247 = B_SPLINE_CURVE_WITH_KNOTS ( 'NONE', 3,
 ( #67943, #63381, #15156, #52211 ),
 .UNSPECIFIED., .F., .F.,
 ( 4, 4 ),
 ( 0.000000000000000000, 1.000000000000000000 ),
 .UNSPECIFIED. ) ;
#56248 = CARTESIAN_POINT ( 'NONE',  ( 24.09354145009956838, 9.221916985538504363, 9.178197973474382820 ) ) ;
#56249 = ORIENTED_EDGE ( 'NONE', *, *, #30204, .F. ) ;
#56250 = CARTESIAN_POINT ( 'NONE',  ( 12.41832178632831507, -1.871654022356046276, -12.46021467525213566 ) ) ;
#56251 = CARTESIAN_POINT ( 'NONE',  ( 10.42795525820099911, 3.905250696375530239, 8.498986197235801399 ) ) ;
#56252 = CARTESIAN_POINT ( 'NONE',  ( 10.88760685321000032, -5.634843745609000365, -7.088991614236999972 ) ) ;
#56253 = CARTESIAN_POINT ( 'NONE',  ( 9.317462135714000837, 5.100000000000000533, 6.571291218949999902 ) ) ;
#56254 = CARTESIAN_POINT ( 'NONE',  ( 18.23019412026500063, -3.031170125296999807, -11.90979123982999965 ) ) ;
#56255 = CARTESIAN_POINT ( 'NONE',  ( 9.293111399473126255, 2.988705873519680090, -6.748153640515438312 ) ) ;
#56256 = DIRECTION ( 'NONE',  ( 1.000000000000000000, 0.000000000000000000, 0.000000000000000000 ) ) ;
#56257 = CARTESIAN_POINT ( 'NONE',  ( 17.65762099059918810, -0.6166112555940442830, -12.67984200623736513 ) ) ;
#56258 =( LENGTH_UNIT ( ) NAMED_UNIT ( * ) SI_UNIT ( .MILLI., .METRE. ) );
#56259 = CARTESIAN_POINT ( 'NONE',  ( 11.08425954179440076, -3.017023678917100327, -8.316745941391600283 ) ) ;
#56260 = CARTESIAN_POINT ( 'NONE',  ( 17.79016990201544246, -3.160912468841198475, 12.19707490278732642 ) ) ;
#56261 = EDGE_LOOP ( 'NONE', ( #59397, #30437, #18613, #27974, #31339 ) ) ;
#56262 = ORIENTED_EDGE ( 'NONE', *, *, #31509, .T. ) ;
#56263 = VECTOR ( 'NONE', #64927, 1000.000000000000000 ) ;
#56264 = CARTESIAN_POINT ( 'NONE',  ( 9.433148997456999751, -5.167567567567999731, 6.822293592207000934 ) ) ;
#56265 = CARTESIAN_POINT ( 'NONE',  ( 17.88831561175062745, 3.029094439802118011, 13.54684341221733668 ) ) ;
#56266 = CARTESIAN_POINT ( 'NONE',  ( 23.85322410408000238, -3.520566476961000113, 13.16563783490999917 ) ) ;
#56267 = CARTESIAN_POINT ( 'NONE',  ( 13.12913653430047134, 11.69120254989820573, 1.923246422712991066 ) ) ;
#56268 = CARTESIAN_POINT ( 'NONE',  ( 17.57591033989425000, 1.875000590519982246, 12.57541652832150803 ) ) ;
#56269 = CARTESIAN_POINT ( 'NONE',  ( 10.98768472639999949, 0.3876847264043000174, -4.945212061661000469 ) ) ;
#56272 = ADVANCED_FACE ( 'NONE', ( #9771 ), #18785, .F. ) ;
#56271 = CARTESIAN_POINT ( 'NONE',  ( 9.662551629919999385, 4.094830335839000135, 9.119946295870999364 ) ) ;
#56270 = B_SPLINE_CURVE_WITH_KNOTS ( 'NONE', 3,
 ( #8054, #29396, #67796, #50705 ),
 .UNSPECIFIED., .F., .F.,
 ( 4, 4 ),
 ( 0.000000000000000000, 1.000000000000000000 ),
 .UNSPECIFIED. ) ;
#56273 = CARTESIAN_POINT ( 'NONE',  ( 10.29214449041784007, -3.170483834885368779, -8.579383242755033834 ) ) ;
#56274 = EDGE_CURVE ( 'NONE', #606, #64705, #51341, .T. ) ;
#56275 = EDGE_CURVE ( 'NONE', #10401, #60760, #58022, .T. ) ;
#56276 = ORIENTED_EDGE ( 'NONE', *, *, #61590, .T. ) ;
#56277 = CARTESIAN_POINT ( 'NONE',  ( 12.70216005901007783, -1.883184384472673445, 12.57411343304723772 ) ) ;
#56278 = CARTESIAN_POINT ( 'NONE',  ( 9.199088727410998700, -5.000897406023000258, -7.583944523024719331 ) ) ;
#56279 = CARTESIAN_POINT ( 'NONE',  ( 10.03612394578000000, 3.011788727150999989, 8.746962581836999817 ) ) ;
#56280 = CYLINDRICAL_SURFACE ( 'NONE', #24273, 1.500000000000000000 ) ;
#56281 = CIRCLE ( 'NONE', #40644, 11.26964301940000013 ) ;
#56282 = CARTESIAN_POINT ( 'NONE',  ( 11.37964291764649971, 2.731641218595000087, -7.343212302062899433 ) ) ;
#56283 = CARTESIAN_POINT ( 'NONE',  ( 12.64343166449435962, 0.6040886362899380302, 12.68065483099174884 ) ) ;
#56284 = AXIS2_PLACEMENT_3D ( 'NONE', #60968, #13083, #7474 ) ;
#56285 = CARTESIAN_POINT ( 'NONE',  ( 7.283509992105000386, 4.426928431836000044, 9.293321981113999541 ) ) ;
#56286 = CARTESIAN_POINT ( 'NONE',  ( 10.15902941591999920, 4.166415211384999040, 9.114163806478000396 ) ) ;
#56287 = CARTESIAN_POINT ( 'NONE',  ( 12.34565325027254978, 2.076107717502758465, 12.54027567175044844 ) ) ;
#56288 = ORIENTED_EDGE ( 'NONE', *, *, #52440, .T. ) ;
#56289 = AXIS2_PLACEMENT_3D ( 'NONE', #47719, #10644, #21144 ) ;
#56290 = CARTESIAN_POINT ( 'NONE',  ( 9.594139158774000364, 2.212639797530000063, -6.855876382544999537 ) ) ;
#56291 = CARTESIAN_POINT ( 'NONE',  ( 11.57656516821460890, 4.899536366368299589, -8.407828142327998577 ) ) ;
#56292 = ADVANCED_FACE ( 'NONE', ( #26210 ), #50191, .T. ) ;
#56293 = DIRECTION ( 'NONE',  ( 0.000000000000000000, -1.000000000000000000, 0.000000000000000000 ) ) ;
#56295 = FACE_OUTER_BOUND ( 'NONE', #68265, .T. ) ;
#56294 = CARTESIAN_POINT ( 'NONE',  ( 9.459504440379001622, -5.445226602819000838, 7.703375344019999460 ) ) ;
#56296 = CARTESIAN_POINT ( 'NONE',  ( 10.36262143724500007, -3.332852462363599777, 8.250837174995698575 ) ) ;
#56297 = CARTESIAN_POINT ( 'NONE',  ( 10.79718447801629999, -2.996774412198000448, -7.477880487566260115 ) ) ;
#56298 = ORIENTED_EDGE ( 'NONE', *, *, #52640, .F. ) ;
#56299 = CARTESIAN_POINT ( 'NONE',  ( 2.349703346704999696, 1.767505521208999841, -3.127111028022000028 ) ) ;
#56300 = CARTESIAN_POINT ( 'NONE',  ( 12.09997738314739912, 11.69706276465918116, -3.884924152321057367 ) ) ;
#56301 = CARTESIAN_POINT ( 'NONE',  ( 17.79999999998900151, 3.595165934733000057, -11.99793354950999991 ) ) ;
#56302 = FACE_OUTER_BOUND ( 'NONE', #30430, .T. ) ;
#56303 = CARTESIAN_POINT ( 'NONE',  ( 9.959641781044998865, 5.406625910119999823, 7.700299649248999678 ) ) ;
#56304 = DIRECTION ( 'NONE',  ( 1.000000000000000000, 0.000000000000000000, 0.000000000000000000 ) ) ;
#56305 = FACE_BOUND ( 'NONE', #51041, .T. ) ;
#56306 = CARTESIAN_POINT ( 'NONE',  ( 1.700000000000000178, 0.000000000000000000, 0.000000000000000000 ) ) ;
#56307 = CARTESIAN_POINT ( 'NONE',  ( 8.437855646795000553, -2.606998386752999775, 6.345764833140000505 ) ) ;
#56308 = ORIENTED_EDGE ( 'NONE', *, *, #51062, .F. ) ;
#56309 = CARTESIAN_POINT ( 'NONE',  ( 7.571670280409000142, 2.531201476950000195, 8.216704145297999418 ) ) ;
#56310 = DIRECTION ( 'NONE',  ( 1.000000000000000000, 0.000000000000000000, 0.000000000000000000 ) ) ;
#56311 = CARTESIAN_POINT ( 'NONE',  ( 10.98768472633000037, -6.720753151621999599, -5.471698430863999540 ) ) ;
#56312 = CIRCLE ( 'NONE', #58540, 12.59999999999999964 ) ;
#56313 = CARTESIAN_POINT ( 'NONE',  ( 17.91195221636559864, -0.5131987759028846519, 13.88724801698877620 ) ) ;
#56314 = CARTESIAN_POINT ( 'NONE',  ( 2.034112785886000196, 1.767505521208999841, -3.127111028022000028 ) ) ;
#56315 = EDGE_LOOP ( 'NONE', ( #24594, #42985, #54914, #39588 ) ) ;
#56316 = CARTESIAN_POINT ( 'NONE',  ( 11.00000000000000000, 5.079754677601000523, 7.174999999999999822 ) ) ;
#56317 = CARTESIAN_POINT ( 'NONE',  ( 11.91672066707849886, -3.258843737379200078, 7.948314604624900248 ) ) ;
#56318 = CARTESIAN_POINT ( 'NONE',  ( 23.60000000000000142, 11.77655473258999841, -4.190794510628000680 ) ) ;
#56319 = CARTESIAN_POINT ( 'NONE',  ( 9.611387933856001098, 3.334846092635999959, 5.869117602953000556 ) ) ;
#56320 = EDGE_CURVE ( 'NONE', #26090, #29376, #26333, .T. ) ;
#56321 = CARTESIAN_POINT ( 'NONE',  ( 11.16641369783139837, 3.949373449607799902, 6.497808498716000081 ) ) ;
#56322 = CARTESIAN_POINT ( 'NONE',  ( 9.649875981547200610, -2.700874656649667749, 7.923553693498007533 ) ) ;
#56323 = CARTESIAN_POINT ( 'NONE',  ( 10.50084194037999907, -4.616788958496999662, -6.288071994190999270 ) ) ;
#56324 = EDGE_CURVE ( 'NONE', #36624, #3801, #27717, .T. ) ;
#56325 = CARTESIAN_POINT ( 'NONE',  ( 12.80505043854143388, 1.875000000000000000, -12.57545641911172751 ) ) ;
#56326 = CARTESIAN_POINT ( 'NONE',  ( 18.41194552102802007, 3.255591973369043934, -12.09481971601418415 ) ) ;
#56327 = CARTESIAN_POINT ( 'NONE',  ( 12.22109980847048050, -2.722998852016973892, 12.39684006590273668 ) ) ;
#56328 = CARTESIAN_POINT ( 'NONE',  ( 8.567869857589764493, 3.845039034713962245, 5.763696154439774233 ) ) ;
#56329 = ORIENTED_EDGE ( 'NONE', *, *, #45315, .T. ) ;
#56330 = CARTESIAN_POINT ( 'NONE',  ( 17.75752317324811003, -1.908613644657472408, 13.78124409819558771 ) ) ;
#56331 = DIRECTION ( 'NONE',  ( 1.000000000000000000, 0.000000000000000000, 0.000000000000000000 ) ) ;
#56332 = ORIENTED_EDGE ( 'NONE', *, *, #28904, .F. ) ;
#56333 = ORIENTED_EDGE ( 'NONE', *, *, #46654, .F. ) ;
#56334 = CARTESIAN_POINT ( 'NONE',  ( 24.98034594679068121, -2.955830752047062138, -11.57694219477421704 ) ) ;
#56335 = CARTESIAN_POINT ( 'NONE',  ( 5.259732019823497140, -0.7229411925607095446, 0.8718313054307640364 ) ) ;
#56337 = CARTESIAN_POINT ( 'NONE',  ( 8.705449068729999240, -4.363978735910500006, -8.287166017043100297 ) ) ;
#56336 = AXIS2_PLACEMENT_3D ( 'NONE', #55387, #60286, #1551 ) ;
#56338 = CARTESIAN_POINT ( 'NONE',  ( 11.08992526467999973, 5.210543602612999869, 8.327598319864998544 ) ) ;
#56339 = CARTESIAN_POINT ( 'NONE',  ( 10.99693586709999948, 2.980605808171000071, -6.418617723582000778 ) ) ;
#56340 = CARTESIAN_POINT ( 'NONE',  ( 10.11342028323962694, -4.872854478606138073, -7.439524153027672781 ) ) ;
#56341 = CARTESIAN_POINT ( 'NONE',  ( 11.12914445903999905, -3.083861519183999977, 8.586004431109000024 ) ) ;
#56342 = CARTESIAN_POINT ( 'NONE',  ( 18.20009441896382540, -0.3284204639250697944, -12.59572022474404562 ) ) ;
#56343 = B_SPLINE_CURVE_WITH_KNOTS ( 'NONE', 3,
 ( #40375, #13815, #64088, #5711, #68648, #42437, #15176, #4333, #27052, #48025, #15525, #63748, #36852, #41749, #10965, #10614, #31955, #53271 ),
 .UNSPECIFIED., .F., .F.,
 ( 4, 2, 2, 2, 2, 2, 2, 2, 4 ),
 ( 0.000000000000000000, 0.1250000000000000000, 0.2500000000000000000, 0.3750000000000000000, 0.5000000000000000000, 0.6250000000000000000, 0.7500000000000000000, 0.8750000000000000000, 1.000000000000000000 ),
 .UNSPECIFIED. ) ;
#56344 = CARTESIAN_POINT ( 'NONE',  ( 3.400000000000000355, 1.000000000000000000, 0.000000000000000000 ) ) ;
#56345 = CARTESIAN_POINT ( 'NONE',  ( 10.35826357027499789, -3.149486845331399998, -7.664090691848299386 ) ) ;
#56346 = FACE_OUTER_BOUND ( 'NONE', #46303, .T. ) ;
#56347 = VERTEX_POINT ( 'NONE', #3748 ) ;
#56348 = CARTESIAN_POINT ( 'NONE',  ( 11.01815802025999957, -6.613253574126999546, -5.429988750868999681 ) ) ;
#56349 = FILL_AREA_STYLE_COLOUR ( '', #3049 ) ;
#56350 = CARTESIAN_POINT ( 'NONE',  ( 7.000000000000000000, 0.000000000000000000, 0.000000000000000000 ) ) ;
#56351 = DIRECTION ( 'NONE',  ( 1.000000000000000000, 0.000000000000000000, 0.000000000000000000 ) ) ;
#56352 = CARTESIAN_POINT ( 'NONE',  ( 9.811013376692999444, 2.859607053196999704, -6.920441276178300072 ) ) ;
#56353 = CARTESIAN_POINT ( 'NONE',  ( 12.08884934673719869, 2.402320636441721557, 13.79236805980801428 ) ) ;
#56354 = CARTESIAN_POINT ( 'NONE',  ( 10.33537187819000103, -5.153689638257000105, 8.830861236101000600 ) ) ;
#56355 = ORIENTED_EDGE ( 'NONE', *, *, #69128, .F. ) ;
#56356 = CARTESIAN_POINT ( 'NONE',  ( 12.41269347218823604, 0.4865065284325135186, -12.68745508180288262 ) ) ;
#56357 = EDGE_CURVE ( 'NONE', #30294, #60176, #32161, .T. ) ;
#56358 = CARTESIAN_POINT ( 'NONE',  ( 12.13954239761513243, 0.2899337805559719650, 13.99700184298317041 ) ) ;
#56359 = EDGE_CURVE ( 'NONE', #42844, #20915, #57149, .T. ) ;
#56360 = ORIENTED_EDGE ( 'NONE', *, *, #61587, .T. ) ;
#56361 = CARTESIAN_POINT ( 'NONE',  ( 17.80000000001300009, -3.351264566333000072, 11.15757590352999884 ) ) ;
#56362 = CARTESIAN_POINT ( 'NONE',  ( 24.67921570607400383, -3.567514742249000115, 12.13750887372000165 ) ) ;
#56363 = CARTESIAN_POINT ( 'NONE',  ( 23.51521078797799902, -2.987649840005000001, -13.81502094324000041 ) ) ;
#56364 = CARTESIAN_POINT ( 'NONE',  ( 4.798048069770000090, 1.305799815673000186, -0.9751758809245999471 ) ) ;
#56365 = VECTOR ( 'NONE', #53299, 1000.000000000000114 ) ;
#56366 = B_SPLINE_SURFACE_WITH_KNOTS ( 'NONE', 3, 3, ( 
 ( #38418, #16741, #33182, #17444, #32495, #28280, #11160, #16402, #43674, #65674, #6600, #32157, #1361, #5908, #329, #48222, #44023, #38069, #48571, #54151, #6248, #27248, #675, #21643, #42978, #11844, #64285, #27942, #37388, #65326, #22335, #54500, #49600, #44376, #38771 ),
 ( #59395, #49252, #60095, #12201, #33529, #11495, #6947, #64971, #37732, #17086, #54848, #32839, #10815, #23026, #53473, #58711, #21987, #59743, #26908, #5567, #56225, #67049, #60438, #18829, #2738, #12545, #7640, #50296, #17796, #13590, #18137, #66708, #24064, #55542, #39460 ),
 ( #39115, #7295, #18482, #13247, #45398, #45739, #19158, #50638, #33876, #40155, #34222, #29678, #55193, #3078, #2394, #61130, #8334, #60780, #44717, #49947, #66014, #40482, #50980, #23718, #61471, #24411, #12894, #28635, #2060, #34910, #28988, #45054, #66361, #39807, #23378 ),
 ( #55888, #34572, #7992, #29325, #904, #55074, #43900, #48795, #22217, #44258, #43553, #32717, #64506, #44604, #11376, #27468, #64854, #65554, #1941, #23260, #53694, #33062, #27828, #33759, #60319, #18025, #12428, #49477, #28161, #1588, #16963, #65204, #49828, #6829, #11045 ) ),
 .UNSPECIFIED., .F., .F., .F.,
 ( 4, 4 ),
 ( 4, 1, 1, 1, 1, 1, 1, 1, 1, 1, 1, 1, 1, 1, 1, 1, 1, 1, 1, 1, 1, 1, 1, 1, 1, 1, 1, 1, 1, 1, 1, 1, 4 ),
 ( -0.1039086239011999951, 1.103908623900999864 ),
 ( -0.01933701211302999920, 0.01208563257065999909, 0.04350827725433999843, 0.07493092193802000645, 0.1063535666217000075, 0.1377762113054000204, 0.1691988559891000055, 0.2006215006727000150, 0.2320441453564000001, 0.2634667900400999851, 0.2948894347238000258, 0.3263120794074999553, 0.3577347240911999959, 0.3891573687748000054, 0.4205800134584999905, 0.4520026581421999756, 0.4834253028259000162, 0.5148479475096000568, 0.5462705921932000663, 0.5776932368768999959, 0.6091158815606000365, 0.6405385262443000771, 0.6719611709280000067, 0.7033838156117000473, 0.7348064602953000568, 0.7662291049789999864, 0.7976517496627000270, 0.8290743943464000676, 0.8604970390300999972, 0.8919196837138000378, 0.9233423283974000473, 0.9547649730810999769, 0.9861876177648000175 ),
 .UNSPECIFIED. ) ;
#56367 = CARTESIAN_POINT ( 'NONE',  ( 10.07314899745999881, 5.167567567567999731, -6.822293592207000934 ) ) ;
#56368 = AXIS2_PLACEMENT_3D ( 'NONE', #63431, #15552, #51914 ) ;
#56369 = CARTESIAN_POINT ( 'NONE',  ( 0.5157068467740000273, 0.9881876859693999871, -3.396851722846999877 ) ) ;
#56370 = DIRECTION ( 'NONE',  ( 4.886316779972976613E-08, -0.7071067643484966192, -0.7071067980245964169 ) ) ;
#56371 = CARTESIAN_POINT ( 'NONE',  ( 10.53521345716899837, -3.075109701058799772, -8.340879262988799780 ) ) ;
#56372 = CARTESIAN_POINT ( 'NONE',  ( 24.30000000000000071, -10.83443035398000021, 3.855530949778000149 ) ) ;
#56373 = CARTESIAN_POINT ( 'NONE',  ( 10.70287750876920008, 3.530799696887600092, -8.228113772635300194 ) ) ;
#56374 = CARTESIAN_POINT ( 'NONE',  ( 18.19991756629438484, 3.160410836633246845, 11.91446384612377862 ) ) ;
#56375 = CARTESIAN_POINT ( 'NONE',  ( 11.09999999999999964, -0.5000000000000000000, -5.124965750789000296 ) ) ;
#56376 = EDGE_CURVE ( 'NONE', #50139, #61746, #3411, .T. ) ;
#56377 = CARTESIAN_POINT ( 'NONE',  ( 10.08857120343299840, 3.944651031655580287, -8.640469672413999547 ) ) ;
#56379 = CARTESIAN_POINT ( 'NONE',  ( 12.18024789519070872, 2.481080537771255035, 12.45595244966267501 ) ) ;
#56378 = CARTESIAN_POINT ( 'NONE',  ( 9.545101285863999863, -4.558267473659599389, 8.163359157892799089 ) ) ;
#56380 = CARTESIAN_POINT ( 'NONE',  ( 23.59527583324263134, -13.38802479761197972, 4.017745927562742736 ) ) ;
#56381 = EDGE_LOOP ( 'NONE', ( #65741, #32589, #9015, #52612 ) ) ;
#56382 = CARTESIAN_POINT ( 'NONE',  ( 11.19434208742519843, 3.521141233577200325, 6.747282993577999655 ) ) ;
#56383 = CIRCLE ( 'NONE', #578, 1.100000000000000755 ) ;
#56384 = CARTESIAN_POINT ( 'NONE',  ( 9.600494040286998043, -5.206548117663999165, 8.585114612872999373 ) ) ;
#56385 = CARTESIAN_POINT ( 'NONE',  ( 9.908304848515998131, 4.913464051101100516, 7.082356937474298952 ) ) ;
#56386 = DIRECTION ( 'NONE',  ( 1.000000000000000000, 0.000000000000000000, 0.000000000000000000 ) ) ;
#56387 = DIRECTION ( 'NONE',  ( 0.000000000000000000, 1.000000000000000000, 0.000000000000000000 ) ) ;
#56388 = CARTESIAN_POINT ( 'NONE',  ( 13.50018479229300006, 11.60142623882999935, 2.415183939829000259 ) ) ;
#56389 = CARTESIAN_POINT ( 'NONE',  ( 6.949466553314000095, -12.16404195313999992, 3.090625619586999662 ) ) ;
#56390 = ORIENTED_EDGE ( 'NONE', *, *, #32163, .F. ) ;
#56391 = CARTESIAN_POINT ( 'NONE',  ( 10.03791290906799993, -4.722468360609500593, -8.384179803770500428 ) ) ;
#56392 = CARTESIAN_POINT ( 'NONE',  ( 10.99999970531878013, 2.901368254139102376, -7.597293174631950308 ) ) ;
#56393 = CARTESIAN_POINT ( 'NONE',  ( 17.95182328287549822, 1.877974217481243269, -12.45926392518878068 ) ) ;
#56394 = CARTESIAN_POINT ( 'NONE',  ( 3.800000448357999883, -1.625000000000000000, 0.000000000000000000 ) ) ;
#56395 = LINE ( 'NONE', #50458, #67446 ) ;
#56396 = B_SPLINE_CURVE_WITH_KNOTS ( 'NONE', 3,
 ( #66128, #60548, #65434, #54608 ),
 .UNSPECIFIED., .F., .F.,
 ( 4, 4 ),
 ( 0.000000000000000000, 1.000000000000000000 ),
 .UNSPECIFIED. ) ;
#56397 = CARTESIAN_POINT ( 'NONE',  ( 7.761763193589995780, 2.840593260277998411, 6.815714094171000603 ) ) ;
#56398 = CARTESIAN_POINT ( 'NONE',  ( 9.749327024990000368, -5.634417356902000407, -7.003562403358999156 ) ) ;
#56399 = CARTESIAN_POINT ( 'NONE',  ( 25.46373029971899982, -8.354610197568000274, -8.148451206582999262 ) ) ;
#56400 = ADVANCED_FACE ( 'NONE', ( #14939 ), #47106, .F. ) ;
#56401 = ORIENTED_EDGE ( 'NONE', *, *, #66914, .F. ) ;
#56402 = CARTESIAN_POINT ( 'NONE',  ( 18.27946005101762950, 2.709881966519577468, -13.73658560568436293 ) ) ;
#56403 = CARTESIAN_POINT ( 'NONE',  ( 8.970944094206998898, -5.100000000000000533, 6.571291218949999902 ) ) ;
#56404 = CARTESIAN_POINT ( 'NONE',  ( 23.59718018307008336, 13.38963915723865306, 4.008749883956627791 ) ) ;
#56405 = CARTESIAN_POINT ( 'NONE',  ( 11.59999999999999964, 4.000000000000000000, -7.500000000000000000 ) ) ;
#56406 = CARTESIAN_POINT ( 'NONE',  ( 3.050973465878000113, 3.500000000000000000, 0.000000000000000000 ) ) ;
#56407 = CARTESIAN_POINT ( 'NONE',  ( 9.120514158775000269, 5.306366356490000769, -7.996450761531000317 ) ) ;
#56408 = CARTESIAN_POINT ( 'NONE',  ( 16.13886389318898651, 3.397126321181335395, 11.84561170022415766 ) ) ;
#56409 = ORIENTED_EDGE ( 'NONE', *, *, #22558, .F. ) ;
#56410 = CARTESIAN_POINT ( 'NONE',  ( 9.344204180665373727, -2.685408982705638881, -7.853404758885505821 ) ) ;
#56411 = CARTESIAN_POINT ( 'NONE',  ( 18.27871553590497911, 2.567375067704834812, -13.76260043498214003 ) ) ;
#56412 = EDGE_LOOP ( 'NONE', ( #24067, #41668, #39643, #45519, #57749 ) ) ;
#56413 = CARTESIAN_POINT ( 'NONE',  ( 10.83744474310099903, -3.228742141949900279, 7.125715588371799747 ) ) ;
#56414 = CARTESIAN_POINT ( 'NONE',  ( 2.603056799210541783, 2.798833948393625981, 2.150913519912208471 ) ) ;
#56415 = CARTESIAN_POINT ( 'NONE',  ( 9.550320280412000429, 2.370176859044999862, -6.912649125838000508 ) ) ;
#56416 = CARTESIAN_POINT ( 'NONE',  ( 8.789886373836322875, 4.000007821194417446, -8.439846342473931173 ) ) ;
#56417 = CARTESIAN_POINT ( 'NONE',  ( 11.30878751119029957, -5.041025164610000608, -8.044634158732998586 ) ) ;
#56418 = DIRECTION ( 'NONE',  ( 1.000000000000000000, 0.000000000000000000, 0.000000000000000000 ) ) ;
#56419 = CYLINDRICAL_SURFACE ( 'NONE', #57457, 0.5000000000000002220 ) ;
#56420 = VERTEX_POINT ( 'NONE', #57580 ) ;
#56421 = CARTESIAN_POINT ( 'NONE',  ( 8.878359312499435774, 5.126777126183351463, 6.752018918868522235 ) ) ;
#56422 = CARTESIAN_POINT ( 'NONE',  ( 10.63559687351566474, -2.907767014557175678, 8.129523725463618788 ) ) ;
#56423 = CARTESIAN_POINT ( 'NONE',  ( 25.59994555223700274, -9.407310119912859037, 6.227539428020667955 ) ) ;
#56424 = ORIENTED_EDGE ( 'NONE', *, *, #23279, .F. ) ;
#56425 = CARTESIAN_POINT ( 'NONE',  ( 9.819565861057999001, 2.688248842995000221, -7.873038103423000145 ) ) ;
#56426 = CONTEXT_DEPENDENT_SHAPE_REPRESENTATION ( #27990, #46289 ) ;
#56427 = B_SPLINE_CURVE_WITH_KNOTS ( 'NONE', 3,
 ( #53712, #68745, #16645, #20861 ),
 .UNSPECIFIED., .F., .F.,
 ( 4, 4 ),
 ( 0.000000000000000000, 1.000000000000000000 ),
 .UNSPECIFIED. ) ;
#56428 = VERTEX_POINT ( 'NONE', #9336 ) ;
#56429 = CARTESIAN_POINT ( 'NONE',  ( 8.974088727410999056, 2.862182806015999947, 7.404572115919599185 ) ) ;
#56430 = CARTESIAN_POINT ( 'NONE',  ( 18.14814637199133429, -2.302603452852429733, -12.49536313902244089 ) ) ;
#56431 = CIRCLE ( 'NONE', #27377, 11.79499999999999993 ) ;
#56432 = CARTESIAN_POINT ( 'NONE',  ( 11.53937873044000106, -11.52961813267000046, -1.376592384073999975 ) ) ;
#56433 = CARTESIAN_POINT ( 'NONE',  ( 8.477766462057999775, 2.899999999999999911, -6.558719934578999933 ) ) ;
#56434 = EDGE_CURVE ( 'NONE', #6003, #46630, #56903, .T. ) ;
#56435 = CARTESIAN_POINT ( 'NONE',  ( 8.350387243830999395, -4.599999999999999645, 6.632262360512000576 ) ) ;
#56436 = EDGE_CURVE ( 'NONE', #35557, #45838, #19845, .T. ) ;
#56437 = ORIENTED_EDGE ( 'NONE', *, *, #44195, .F. ) ;
#56438 = CARTESIAN_POINT ( 'NONE',  ( 11.59999999999999964, 3.310169951859693427, 6.761031184901315605 ) ) ;
#56439 = CARTESIAN_POINT ( 'NONE',  ( 10.65229834123000074, 4.944334466443999432, -8.478467788338001299 ) ) ;
#56440 = CYLINDRICAL_SURFACE ( 'NONE', #6178, 1.350000000000000089 ) ;
#56441 = CARTESIAN_POINT ( 'NONE',  ( 12.08961158949548675, 2.638129719752015045, -13.74921199938403937 ) ) ;
#56442 = CARTESIAN_POINT ( 'NONE',  ( 9.785684229509998389, -4.901739481456999670, -6.592668585875199661 ) ) ;
#56443 = CARTESIAN_POINT ( 'NONE',  ( 10.34521071928999980, -2.724119865955000108, 6.497322598008000050 ) ) ;
#56444 = CARTESIAN_POINT ( 'NONE',  ( 18.21571869486622930, 0.3016537271415110077, 13.99676704218776990 ) ) ;
#56445 = CARTESIAN_POINT ( 'NONE',  ( 10.91944543538999923, -3.268376408192000149, -6.413937436229999456 ) ) ;
#56446 = ORIENTED_EDGE ( 'NONE', *, *, #61091, .F. ) ;
#56447 = ORIENTED_EDGE ( 'NONE', *, *, #49083, .F. ) ;
#56448 = CARTESIAN_POINT ( 'NONE',  ( 9.567560841232999991, 5.349936549139000519, -7.138437102151999447 ) ) ;
#56449 = CARTESIAN_POINT ( 'NONE',  ( 10.76685100253999927, -2.832432432432000269, 6.822293592207000934 ) ) ;
#56450 = CARTESIAN_POINT ( 'NONE',  ( 12.21068878739219343, -2.693668765267103637, 13.63048043076724625 ) ) ;
#56451 = CARTESIAN_POINT ( 'NONE',  ( 25.20341525953400108, 8.548126993989999534, -7.997462102762000313 ) ) ;
#56452 = CARTESIAN_POINT ( 'NONE',  ( 25.37958977069655475, -3.026682599187875855, -11.38056660099664086 ) ) ;
#56453 = ADVANCED_FACE ( 'NONE', ( #41852 ), #31034, .T. ) ;
#56454 = FACE_OUTER_BOUND ( 'NONE', #47333, .T. ) ;
#56456 = CARTESIAN_POINT ( 'NONE',  ( 2.435247277619000172, 2.372532593102000043, -2.573147701680999599 ) ) ;
#56455 = CARTESIAN_POINT ( 'NONE',  ( 10.25834252387499923, -5.128664655368000425, 7.672773098917999413 ) ) ;
#56458 = AXIS2_PLACEMENT_3D ( 'NONE', #60715, #12832, #34158 ) ;
#56457 = CARTESIAN_POINT ( 'NONE',  ( 8.619872774977997310, -4.492752443836998566, -6.440200355240005337 ) ) ;
#56459 = ORIENTED_EDGE ( 'NONE', *, *, #25281, .F. ) ;
#56460 = EDGE_CURVE ( 'NONE', #43730, #60967, #23856, .T. ) ;
#56461 = CARTESIAN_POINT ( 'NONE',  ( 5.000000000000000000, 0.8000000000000000444, 3.149999999999999911 ) ) ;
#56462 = CIRCLE ( 'NONE', #8498, 13.10000000000000320 ) ;
#56463 = CARTESIAN_POINT ( 'NONE',  ( 23.56666365135700403, -11.07911597678999271, -4.076188921308005142 ) ) ;
#56464 = CARTESIAN_POINT ( 'NONE',  ( 9.932908211424001266, -3.485164486501000081, -6.221839249167999242 ) ) ;
#56465 = FACE_OUTER_BOUND ( 'NONE', #42457, .T. ) ;
#56466 = FACE_OUTER_BOUND ( 'NONE', #48516, .T. ) ;
#56467 = FACE_OUTER_BOUND ( 'NONE', #4983, .T. ) ;
#56468 = CARTESIAN_POINT ( 'NONE',  ( 8.845310841232000953, 5.851083642416999631, -7.072167224702999633 ) ) ;
#56469 = CARTESIAN_POINT ( 'NONE',  ( 10.71503032197929883, 4.743378537856500543, 8.539569492647999027 ) ) ;
#56470 = B_SPLINE_CURVE_WITH_KNOTS ( 'NONE', 3,
 ( #28102, #60261, #34047, #837 ),
 .UNSPECIFIED., .F., .F.,
 ( 4, 4 ),
 ( 0.000000000000000000, 1.000000000000000000 ),
 .UNSPECIFIED. ) ;
#56471 = AXIS2_PLACEMENT_3D ( 'NONE', #48990, #11570, #54227 ) ;
#56472 = CARTESIAN_POINT ( 'NONE',  ( 18.49996808500599954, 0.9036517535198380635, -11.64999999999999858 ) ) ;
#56473 = CARTESIAN_POINT ( 'NONE',  ( 2.347336229053000434, 2.684440549187000258, 1.847963356650000000 ) ) ;
#56474 = VERTEX_POINT ( 'NONE', #47448 ) ;
#56475 = CARTESIAN_POINT ( 'NONE',  ( 12.61664271790066927, 0.6949735217938437515, -12.58082105808780504 ) ) ;
#56476 = CARTESIAN_POINT ( 'NONE',  ( 6.605026506349999771, -1.500000000000000000, 0.000000000000000000 ) ) ;
#56477 = CARTESIAN_POINT ( 'NONE',  ( 8.741144820356497647, 5.068224986544200839, -6.186394335232312081 ) ) ;
#56478 = CARTESIAN_POINT ( 'NONE',  ( 24.26682857475500299, 3.229948578041999863, -12.20213974738999951 ) ) ;
#56479 = DIRECTION ( 'NONE',  ( 0.000000000000000000, -1.000000000000000000, 0.000000000000000000 ) ) ;
#56480 = ORIENTED_EDGE ( 'NONE', *, *, #61779, .T. ) ;
#56481 = CARTESIAN_POINT ( 'NONE',  ( 5.997278627981999399, 0.6694104981402000387, -0.9669902716602000181 ) ) ;
#56482 = DIRECTION ( 'NONE',  ( 1.000000000000000000, 0.000000000000000000, 0.000000000000000000 ) ) ;
#56483 = CARTESIAN_POINT ( 'NONE',  ( 0.6362098952830620435, -0.4390463955410620067, 3.502173745463374122 ) ) ;
#56484 = CARTESIAN_POINT ( 'NONE',  ( 13.43176382712000105, -11.67665677335000041, -2.247227628037000269 ) ) ;
#56485 = CARTESIAN_POINT ( 'NONE',  ( 7.800894426331000275, 3.218815461055000160, 6.398977422524000147 ) ) ;
#56486 = CARTESIAN_POINT ( 'NONE',  ( 11.39700581613019992, 4.869652672166700391, -8.058426314824099990 ) ) ;
#56487 = ORIENTED_EDGE ( 'NONE', *, *, #27709, .F. ) ;
#56488 = CARTESIAN_POINT ( 'NONE',  ( 10.40516264833000015, -5.216401621862000404, 6.765753642936999768 ) ) ;
#56489 = ORIENTED_EDGE ( 'NONE', *, *, #1699, .T. ) ;
#56490 = CARTESIAN_POINT ( 'NONE',  ( 9.454580538893289088, -5.254250442392512710, 7.998733024362086219 ) ) ;
#56491 = CARTESIAN_POINT ( 'NONE',  ( 16.13937158902900393, 3.642730659064999710, 11.02533040164999889 ) ) ;
#56492 = CARTESIAN_POINT ( 'NONE',  ( 18.26112155826667660, -0.1662062226620539818, -13.99901824074930445 ) ) ;
#56493 = EDGE_CURVE ( 'NONE', #39811, #30230, #37223, .T. ) ;
#56494 = ORIENTED_EDGE ( 'NONE', *, *, #11669, .F. ) ;
#56495 = CARTESIAN_POINT ( 'NONE',  ( 10.52717528972000061, -8.216420183534999921, 6.728173953305000232 ) ) ;
#56496 = CARTESIAN_POINT ( 'NONE',  ( 11.06622274902693093, -4.530851388958180515, -8.944471867880441351 ) ) ;
#56497 = CARTESIAN_POINT ( 'NONE',  ( 17.55505043854147118, -3.248109929747637903, 13.61799478206225444 ) ) ;
#56498 = CARTESIAN_POINT ( 'NONE',  ( 5.700000000000000178, -13.04986661130000059, 1.811520473896000016 ) ) ;
#56499 = CARTESIAN_POINT ( 'NONE',  ( 18.11618405628967210, -2.775422336763186504, 12.38314678678514369 ) ) ;
#56500 = ORIENTED_EDGE ( 'NONE', *, *, #10025, .F. ) ;
#56501 = CARTESIAN_POINT ( 'NONE',  ( 10.34020413671000149, -4.202027362542999356, 9.459588031742001135 ) ) ;
#56502 = CARTESIAN_POINT ( 'NONE',  ( 11.59999999999999964, 4.695782097862117865, 8.404145852941008243 ) ) ;
#56504 = DIRECTION ( 'NONE',  ( 0.000000000000000000, 0.000000000000000000, -1.000000000000000000 ) ) ;
#56503 = B_SPLINE_CURVE_WITH_KNOTS ( 'NONE', 3,
 ( #36963, #20876, #37299, #14942, #47109, #26820, #42547, #42213, #36614, #41855 ),
 .UNSPECIFIED., .F., .F.,
 ( 4, 2, 2, 2, 4 ),
 ( 0.000000000000000000, 0.2500000000000000000, 0.5000000000000000000, 0.7500000000000000000, 1.000000000000000000 ),
 .UNSPECIFIED. ) ;
#56505 = CARTESIAN_POINT ( 'NONE',  ( 9.789763540182331525, 3.672815144550904076, 8.717465845835395299 ) ) ;
#56506 = DIRECTION ( 'NONE',  ( 1.000000000000000000, 0.000000000000000000, 0.000000000000000000 ) ) ;
#56507 = ORIENTED_EDGE ( 'NONE', *, *, #46031, .T. ) ;
#56508 = CARTESIAN_POINT ( 'NONE',  ( 17.83817875635889294, 0.5572864142399046594, -13.88496202738553187 ) ) ;
#56509 = VECTOR ( 'NONE', #42726, 1000.000000000000000 ) ;
#56510 = CARTESIAN_POINT ( 'NONE',  ( 10.93448722448066768, -2.832483728680937674, -6.743831965299308173 ) ) ;
#56511 = CARTESIAN_POINT ( 'NONE',  ( 24.14319218954479851, -3.327217583210993812, -12.48607456098757318 ) ) ;
#56512 = CARTESIAN_POINT ( 'NONE',  ( 3.178056799211042005, -2.150913519912214245, 2.798833948393621984 ) ) ;
#56513 = CARTESIAN_POINT ( 'NONE',  ( 12.21985227486504400, -0.2197089332467947187, -13.89766776387045866 ) ) ;
#56514 = CARTESIAN_POINT ( 'NONE',  ( 18.15589597092050056, -2.672372730248489425, 12.40976522372663737 ) ) ;
#56515 = VERTEX_POINT ( 'NONE', #237 ) ;
#56516 = EDGE_CURVE ( 'NONE', #56220, #7173, #63832, .T. ) ;
#56517 = CARTESIAN_POINT ( 'NONE',  ( 10.56080513895999928, -2.973119161490000106, -6.929150654994399083 ) ) ;
#56518 = ADVANCED_FACE ( 'NONE', ( #63853 ), #64882, .T. ) ;
#56519 = VERTEX_POINT ( 'NONE', #27854 ) ;
#56520 = CARTESIAN_POINT ( 'NONE',  ( 10.59303303094000093, 2.436236667456999960, 7.793464546548000804 ) ) ;
#56521 = CARTESIAN_POINT ( 'NONE',  ( 25.46373024410000241, -11.23407150414000100, 3.161076981347000103 ) ) ;
#56522 = CARTESIAN_POINT ( 'NONE',  ( 9.766460841231999979, 3.135494838036999798, -8.598037907310999373 ) ) ;
#56523 = EDGE_CURVE ( 'NONE', #48331, #31044, #2194, .T. ) ;
#56524 = CARTESIAN_POINT ( 'NONE',  ( 3.669618013697999892, -3.382257552941999812, 0.6016812345426000297 ) ) ;
#56525 = CARTESIAN_POINT ( 'NONE',  ( 11.11264194660999927, -2.146089039267000231, -7.517188649391000510 ) ) ;
#56526 = DIRECTION ( 'NONE',  ( -0.7071060865235063719, -0.7071074758489063194, -8.141945933792071646E-10 ) ) ;
#56527 = CARTESIAN_POINT ( 'NONE',  ( 23.73393238974700026, 13.39775320304000061, 3.632760668476999744 ) ) ;
#56528 = B_SPLINE_CURVE_WITH_KNOTS ( 'NONE', 3,
 ( #8375, #34951, #29717, #35636, #68110, #3794, #41216, #51020, #61848, #9047, #55925, #8029, #40867, #30725, #14310, #25130, #30387, #20228, #25473, #13289, #46463, #51697, #13626, #46805, #35963, #29367, #13964, #62190, #56607, #35293, #52033, #8714, #67763, #57278, #3120, #67087, #62527, #56265, #45776, #50682, #4136, #67424, #2777, #24104, #51360, #24792 ),
 .UNSPECIFIED., .F., .F.,
 ( 4, 2, 2, 2, 2, 1, 2, 2, 2, 1, 2, 2, 2, 2, 2, 2, 1, 2, 2, 1, 2, 2, 2, 2, 4 ),
 ( 0.4988098180370147405, 0.5301342044097088202, 0.5457963975960562486, 0.5614585907824035660, 0.5653741390789909227, 0.5692896873755783904, 0.5771207839687497732, 0.5927829771550930937, 0.6006140737482646985, 0.6084451703414361923, 0.6241073635277791798, 0.6397695567141222783, 0.6554317499004652658, 0.6710939430868083644, 0.6867561362731513519, 0.7024183294594943394, 0.7180805226458374380, 0.7494049090185229689, 0.7650671022048658454, 0.7807292953912086109, 0.8120536817638945859, 0.8433780681365805609, 0.8747024545092665360, 0.9373512272546333790, 1.000000000000000000 ),
 .UNSPECIFIED. ) ;
#56529 = ORIENTED_EDGE ( 'NONE', *, *, #12672, .T. ) ;
#56530 = CARTESIAN_POINT ( 'NONE',  ( 10.82949413291699869, -3.087070836781100169, 7.916546720849799712 ) ) ;
#56531 = CARTESIAN_POINT ( 'NONE',  ( 10.00637913184999839, 5.119263020957999899, 8.420380450036001108 ) ) ;
#56532 = CARTESIAN_POINT ( 'NONE',  ( 16.04331666222400088, 9.026410239312001593, 8.606113518243997618 ) ) ;
#56533 = CARTESIAN_POINT ( 'NONE',  ( 9.143927823787139531, 5.249988444743198812, 7.500000155056751439 ) ) ;
#56535 = CARTESIAN_POINT ( 'NONE',  ( 23.56666365135700403, -2.009474831917003268, -11.63289034803000455 ) ) ;
#56534 = CARTESIAN_POINT ( 'NONE',  ( 9.972850246170999355, 5.044468801812000081, 6.258104779495000436 ) ) ;
#56536 = CARTESIAN_POINT ( 'NONE',  ( 11.21149010443640037, 5.137564434800999891, -7.585072163144589652 ) ) ;
#56537 = EDGE_CURVE ( 'NONE', #58094, #5174, #41078, .T. ) ;
#56538 = CYLINDRICAL_SURFACE ( 'NONE', #9056, 3.200000000000000178 ) ;
#56539 = CARTESIAN_POINT ( 'NONE',  ( 9.553696787962998371, 4.172481380750499902, -6.510508982544899403 ) ) ;
#56540 = CARTESIAN_POINT ( 'NONE',  ( 11.02452225494999993, 2.775477745048999800, -6.571291218949999902 ) ) ;
#56541 = CARTESIAN_POINT ( 'NONE',  ( 24.53002386606100060, 3.319300011433999664, 12.04488764000000067 ) ) ;
#56542 = CARTESIAN_POINT ( 'NONE',  ( 8.114506759233030664, 5.047117657413311420, -6.489853823473402450 ) ) ;
#56543 = CARTESIAN_POINT ( 'NONE',  ( 23.64712440262699999, 10.02868315663000054, 9.634752534433001614 ) ) ;
#56544 = ORIENTED_EDGE ( 'NONE', *, *, #11991, .T. ) ;
#56545 = CARTESIAN_POINT ( 'NONE',  ( 7.101308059622001068, -3.554853390786000045, 8.889491623367000273 ) ) ;
#56546 = CARTESIAN_POINT ( 'NONE',  ( 18.20591985607867258, 2.840417715854210101, 13.70884684492145489 ) ) ;
#56547 = CARTESIAN_POINT ( 'NONE',  ( 9.099999931440999390, 5.064317881551000156, 6.844464000216799349 ) ) ;
#56548 = CARTESIAN_POINT ( 'NONE',  ( 10.33744474310099903, 4.771257858050099721, 7.125715588371799747 ) ) ;
#56549 = ORIENTED_EDGE ( 'NONE', *, *, #12563, .T. ) ;
#56550 = VECTOR ( 'NONE', #52362, 1000.000000000000000 ) ;
#56551 = B_SPLINE_CURVE_WITH_KNOTS ( 'NONE', 3,
 ( #61351, #35478, #3301, #14493 ),
 .UNSPECIFIED., .F., .F.,
 ( 4, 4 ),
 ( 0.000000000000000000, 0.1280414556252505165 ),
 .UNSPECIFIED. ) ;
#56552 = CARTESIAN_POINT ( 'NONE',  ( 17.79046541331000242, 3.643254180937999909, 12.02383733079000017 ) ) ;
#56553 = AXIS2_PLACEMENT_3D ( 'NONE', #19686, #46943, #41008 ) ;
#56555 = CARTESIAN_POINT ( 'NONE',  ( 10.55569598648999907, 5.130952141044000214, 6.826612223887499553 ) ) ;
#56554 = CARTESIAN_POINT ( 'NONE',  ( 8.902126402770997871, -3.188752782784400441, -7.194081880505399873 ) ) ;
#56556 = CARTESIAN_POINT ( 'NONE',  ( 10.52384528040999889, 5.441915759804999198, -7.989632847918000103 ) ) ;
#56557 = ORIENTED_EDGE ( 'NONE', *, *, #67967, .F. ) ;
#56558 = CARTESIAN_POINT ( 'NONE',  ( 1.436390132540666942, 0.4581489286485155299, -3.499999999999999556 ) ) ;
#56559 = CARTESIAN_POINT ( 'NONE',  ( 18.14518304970624030, -2.942254210842380147, -13.68733852372544391 ) ) ;
#56560 = CARTESIAN_POINT ( 'NONE',  ( 11.18687482311539938, 5.057677595549000316, 7.072673169413499217 ) ) ;
#56561 = CARTESIAN_POINT ( 'NONE',  ( 17.60000001072100062, -11.41073498373000028, 4.623967591968000335 ) ) ;
#56562 = CARTESIAN_POINT ( 'NONE',  ( 8.832537864289999874, -2.899999999999999911, 6.571291218949999902 ) ) ;
#56563 = ORIENTED_EDGE ( 'NONE', *, *, #42718, .T. ) ;
#56564 = CARTESIAN_POINT ( 'NONE',  ( 11.31944011432000075, -3.562654288336999819, 11.75631193234000094 ) ) ;
#56565 = CARTESIAN_POINT ( 'NONE',  ( 10.95519194037999888, -3.860335380237000180, -6.147338954930000376 ) ) ;
#56566 = APPLICATION_CONTEXT ( 'automotive_design' ) ;
#56567 = B_SPLINE_CURVE_WITH_KNOTS ( 'NONE', 3,
 ( #8472, #24890, #9484, #35728, #61267, #40620 ),
 .UNSPECIFIED., .F., .F.,
 ( 4, 2, 4 ),
 ( 0.000000000000000000, 0.5000000000000000000, 1.000000000000000000 ),
 .UNSPECIFIED. ) ;
#56568 = CARTESIAN_POINT ( 'NONE',  ( 8.252728345141258970, -5.371128151206209900, 8.571272383222918734 ) ) ;
#56570 = CARTESIAN_POINT ( 'NONE',  ( 11.39189666366029918, -4.052152326617509459, -8.673729056199000809 ) ) ;
#56569 = CONICAL_SURFACE ( 'NONE', #8564, 2.050054338200999915, 0.7853981633972997312 ) ;
#56571 = CARTESIAN_POINT ( 'NONE',  ( 9.398101285863999621, -4.735211557675400584, 8.373612278672599274 ) ) ;
#56572 = VERTEX_POINT ( 'NONE', #21552 ) ;
#56573 = CARTESIAN_POINT ( 'NONE',  ( 2.771806799209417083, -3.408904368339104263, -0.9161175952574814874 ) ) ;
#56574 = CARTESIAN_POINT ( 'NONE',  ( 11.11656919669529842, -2.774362666861999838, 7.137881914002699446 ) ) ;
#56575 = ORIENTED_EDGE ( 'NONE', *, *, #22474, .F. ) ;
#56576 = CARTESIAN_POINT ( 'NONE',  ( 16.39999999379500295, -3.351248059343999941, -11.15756683833000018 ) ) ;
#56577 = VERTEX_POINT ( 'NONE', #42544 ) ;
#56578 = EDGE_CURVE ( 'NONE', #22839, #55276, #33893, .T. ) ;
#56579 = EDGE_CURVE ( 'NONE', #12138, #26310, #37633, .T. ) ;
#56580 = CARTESIAN_POINT ( 'NONE',  ( 9.666315108303999537, -3.197530835772000035, -8.817973615970998935 ) ) ;
#56581 = DIRECTION ( 'NONE',  ( 1.000000000000000000, 5.572913924281000893E-12, -1.887560193303999882E-10 ) ) ;
#56582 = DIRECTION ( 'NONE',  ( 1.000000000000000000, 0.000000000000000000, 0.000000000000000000 ) ) ;
#56583 = CARTESIAN_POINT ( 'NONE',  ( 19.39373726536100051, 11.26964301940000013, 9.577061366172998945E-14 ) ) ;
#56584 = CARTESIAN_POINT ( 'NONE',  ( 12.37974467178318072, 2.958002365504007525, -12.33299351980446446 ) ) ;
#56585 = CARTESIAN_POINT ( 'NONE',  ( 11.83456651104149948, -3.887457492043800311, 8.635175889530000148 ) ) ;
#56586 = CARTESIAN_POINT ( 'NONE',  ( 8.014948341228999240, 2.280568568659000483, 6.510284508622999233 ) ) ;
#56587 = B_SPLINE_CURVE_WITH_KNOTS ( 'NONE', 3,
 ( #58083, #15774, #32212, #37104 ),
 .UNSPECIFIED., .F., .F.,
 ( 4, 4 ),
 ( 0.8566590321960471099, 1.000000000000000000 ),
 .UNSPECIFIED. ) ;
#56588 = VERTEX_POINT ( 'NONE', #12110 ) ;
#56589 = CARTESIAN_POINT ( 'NONE',  ( 9.319055905798999007, 2.899999999999999911, -6.571291218949999902 ) ) ;
#56590 = CARTESIAN_POINT ( 'NONE',  ( 8.341918146793998901, -5.601799093797000140, 7.176147756900999930 ) ) ;
#56591 = CARTESIAN_POINT ( 'NONE',  ( 24.22569962767899199, 9.032524208146405442, 9.032526752365093614 ) ) ;
#56592 = ORIENTED_EDGE ( 'NONE', *, *, #29089, .T. ) ;
#56593 = CARTESIAN_POINT ( 'NONE',  ( 12.30575661439783275, -1.958493781132636391, -12.44686177741867006 ) ) ;
#56594 = CARTESIAN_POINT ( 'NONE',  ( 11.42887348028849992, 2.875789035466000065, 6.892162778124999889 ) ) ;
#56595 = CARTESIAN_POINT ( 'NONE',  ( 10.59956814679000026, -4.438148200474000937, -8.958389257466000899 ) ) ;
#56596 = CARTESIAN_POINT ( 'NONE',  ( 14.93333333127366735, 8.815235367372475039, 7.616700428521842703 ) ) ;
#56597 = CARTESIAN_POINT ( 'NONE',  ( 18.40156003475500057, -3.148349829928000165, -12.06792178657999948 ) ) ;
#56598 = CARTESIAN_POINT ( 'NONE',  ( 9.272783876522375124, 3.210141752053232711, -6.518107589053542483 ) ) ;
#56599 = CARTESIAN_POINT ( 'NONE',  ( 12.20320247475637743, -2.331154411892201850, -13.70777421733260049 ) ) ;
#56600 =( NAMED_UNIT ( * ) PLANE_ANGLE_UNIT ( ) SI_UNIT ( $, .RADIAN. ) );
#56601 = CARTESIAN_POINT ( 'NONE',  ( 10.27195525820100031, -4.120672149427799802, -6.227697122196000024 ) ) ;
#56602 = CARTESIAN_POINT ( 'NONE',  ( 4.699999740790659963, -13.17499974068000057, 1.948180898180000060E-09 ) ) ;
#56603 = ORIENTED_EDGE ( 'NONE', *, *, #18620, .T. ) ;
#56604 = ORIENTED_EDGE ( 'NONE', *, *, #43046, .T. ) ;
#56605 = FILL_AREA_STYLE ('',( #9380 ) ) ;
#56606 = DIRECTION ( 'NONE',  ( 1.000000000000000000, 0.000000000000000000, 0.000000000000000000 ) ) ;
#56607 = CARTESIAN_POINT ( 'NONE',  ( 18.06394506374553899, 2.862992422144976068, 13.58968849268369894 ) ) ;
#56608 = ADVANCED_FACE ( 'NONE', ( #49856 ), #39369, .F. ) ;
#56609 = CARTESIAN_POINT ( 'NONE',  ( 9.910156421876999744, 2.531070993918000056, -7.917736616860999277 ) ) ;
#56610 = CARTESIAN_POINT ( 'NONE',  ( 10.58521345716900086, -3.075109701058799772, 6.659120737011199331 ) ) ;
#56611 = AXIS2_PLACEMENT_3D ( 'NONE', #2169, #7399, #28045 ) ;
#56612 = CARTESIAN_POINT ( 'NONE',  ( 18.14695621644401058, 2.700933560328190541, 12.40248159148175766 ) ) ;
#56613 = CARTESIAN_POINT ( 'NONE',  ( 23.55075186166400059, -13.34760076072000068, 4.341130030273000706 ) ) ;
#56614 = CARTESIAN_POINT ( 'NONE',  ( 10.77962664842000073, 2.397507474987000009, 7.755423212350999407 ) ) ;
#56615 = CIRCLE ( 'NONE', #68880, 12.35000000006999876 ) ;
#56616 = CYLINDRICAL_SURFACE ( 'NONE', #44755, 0.4999999999999998335 ) ;
#56617 = VERTEX_POINT ( 'NONE', #17708 ) ;
#56618 = CARTESIAN_POINT ( 'NONE',  ( 12.18117696241649206, -2.542707536216995745, 12.44156325543625208 ) ) ;
#56619 = CARTESIAN_POINT ( 'NONE',  ( 8.869809814040998219, -3.385590752329799891, -8.294571108394100278 ) ) ;
#56620 = CARTESIAN_POINT ( 'NONE',  ( 9.332933391271998502, 5.100349772922000646, 8.693467186193998941 ) ) ;
#56621 = CARTESIAN_POINT ( 'NONE',  ( 11.59590547754519996, -2.684394667508000154, 7.458246194669389872 ) ) ;
#56622 = CARTESIAN_POINT ( 'NONE',  ( 9.675870280412999236, 3.031907308384000022, -8.729608011560001657 ) ) ;
#56623 = AXIS2_PLACEMENT_3D ( 'NONE', #29582, #13151, #50886 ) ;
#56624 = CARTESIAN_POINT ( 'NONE',  ( 11.57656516821460890, 4.899536366368299589, -8.407828142327998577 ) ) ;
#56625 = EDGE_CURVE ( 'NONE', #3801, #65308, #56615, .T. ) ;
#56626 = CARTESIAN_POINT ( 'NONE',  ( 12.18528753443599477, -0.08139242733401307051, 12.69965452654166960 ) ) ;
#56627 = CARTESIAN_POINT ( 'NONE',  ( 7.583051658771000625, 4.763536573491999881, 5.668879554882000349 ) ) ;
#56628 = CARTESIAN_POINT ( 'NONE',  ( 10.49785886974000171, 3.776281431161999880, 5.717632172928999168 ) ) ;
#56629 = VECTOR ( 'NONE', #14466, 1000.000000000000000 ) ;
#56630 = CARTESIAN_POINT ( 'NONE',  ( 12.19523649643094920, 2.361571219431552571, 12.48275271858022961 ) ) ;
#56631 = ORIENTED_EDGE ( 'NONE', *, *, #54800, .T. ) ;
#56632 = CARTESIAN_POINT ( 'NONE',  ( 10.11453584122999949, 5.322769172805999816, -7.951018786192998178 ) ) ;
#56633 = CARTESIAN_POINT ( 'NONE',  ( -0.000000000000000000, 2.533832635911827502, 1.460960874862264225 ) ) ;
#56634 = CARTESIAN_POINT ( 'NONE',  ( 10.88166120451243124, -2.855160512203144485, 8.850519483704566426 ) ) ;
#56636 = CARTESIAN_POINT ( 'NONE',  ( 5.599999999588999522, 0.000000000000000000, 0.000000000000000000 ) ) ;
#56635 = CARTESIAN_POINT ( 'NONE',  ( 25.30000327618300204, 9.659335867304680079, 6.394377797198711910 ) ) ;
#56637 = CARTESIAN_POINT ( 'NONE',  ( 12.09999999999999964, -3.579171096429341503, 8.516100029838437280 ) ) ;
#56638 = CARTESIAN_POINT ( 'NONE',  ( 11.53564291764652872, -4.995889373412399692, -7.376893506359599506 ) ) ;
#56639 = VERTEX_POINT ( 'NONE', #38678 ) ;
#56640 = CARTESIAN_POINT ( 'NONE',  ( 1.105199323181000004, 1.980426728703999828, 3.194707851357999839 ) ) ;
#56641 = CARTESIAN_POINT ( 'NONE',  ( 17.81164675510670037, -0.5699806461405237945, -12.68277882560511749 ) ) ;
#56643 = CARTESIAN_POINT ( 'NONE',  ( 10.59999999999999964, 3.399999999999999911, -4.756097560976000338 ) ) ;
#56642 = CARTESIAN_POINT ( 'NONE',  ( 9.727383000783749623, 5.662315500981915939, 8.092168579200617273 ) ) ;
#56644 = CARTESIAN_POINT ( 'NONE',  ( 11.79999999684100054, -3.345264396959000130, 11.86064773189999855 ) ) ;
#56645 = CARTESIAN_POINT ( 'NONE',  ( 10.40516904918000129, 5.216391323504000255, 6.765759859247999941 ) ) ;
#56646 = CARTESIAN_POINT ( 'NONE',  ( 12.39066945341153492, -3.117187738603024894, 13.64855991556033743 ) ) ;
#56647 = CARTESIAN_POINT ( 'NONE',  ( 24.30001131568331729, -3.256147847238520132, -12.15210920284597407 ) ) ;
#56648 = PLANE ( 'NONE',  #64514 ) ;
#56649 = CARTESIAN_POINT ( 'NONE',  ( 7.988543146792999927, -3.566638198986999964, 5.743608852252999775 ) ) ;
#56650 = ORIENTED_EDGE ( 'NONE', *, *, #18898, .T. ) ;
#56651 = CARTESIAN_POINT ( 'NONE',  ( 7.994579719591000000, 2.263558315407000254, 8.007442119518000112 ) ) ;
#56652 =( BOUNDED_SURFACE ( )  B_SPLINE_SURFACE ( 3, 3, ( 
 ( #3574, #14084, #2549, #9165 ),
 ( #23876, #66518, #35071, #29494 ),
 ( #46240, #51142, #35409, #56736 ),
 ( #14429, #35748, #57066, #21040 ) ),
 .UNSPECIFIED., .F., .F., .T. ) 
 B_SPLINE_SURFACE_WITH_KNOTS ( ( 4, 4 ),
 ( 4, 4 ),
 ( 0.000000000000000000, 1.000000000000000000 ),
 ( 0.000000000000000000, 1.000000000000000000 ),
 .UNSPECIFIED. ) 
 GEOMETRIC_REPRESENTATION_ITEM ( )  RATIONAL_B_SPLINE_SURFACE ( (
 ( 1.512182578520000042, 1.160176301760999840, 1.160176301760999840, 1.512182578520000042),
 ( 1.111288591041000196, 0.8526025270081000196, 0.8526025270081000196, 1.111288591041000196),
 ( 1.111288591041000196, 0.8526025270081000196, 0.8526025270081000196, 1.111288591041000196),
 ( 1.512182578520000042, 1.160176301760999840, 1.160176301760999840, 1.512182578520000042) ) ) 
 REPRESENTATION_ITEM ( '' )  SURFACE ( )  );
#56653 = CARTESIAN_POINT ( 'NONE',  ( 24.44496356267099912, -8.810485190366000197, 8.810508100388000585 ) ) ;
#56654 = CARTESIAN_POINT ( 'NONE',  ( 9.393930206848999376, -5.250000000000000000, -7.500000000000000000 ) ) ;
#56655 = AXIS2_PLACEMENT_3D ( 'NONE', #19674, #40310, #67209 ) ;
#56656 = CARTESIAN_POINT ( 'NONE',  ( 7.793461047962999544, -3.207862402212000141, 6.406748704942000217 ) ) ;
#56657 = CARTESIAN_POINT ( 'NONE',  ( 1.509611342036999870, 0.7365451747729999665, -3.515871166463000019 ) ) ;
#56658 = VERTEX_POINT ( 'NONE', #12454 ) ;
#56659 = CARTESIAN_POINT ( 'NONE',  ( 1.191003052484043367, 1.577065564342242654, -2.901955378219182258 ) ) ;
#56660 = CARTESIAN_POINT ( 'NONE',  ( 11.46949144726329983, -4.580206776679999869, 8.318725197575499664 ) ) ;
#56661 = LINE ( 'NONE', #45142, #28636 ) ;
#56662 = CARTESIAN_POINT ( 'NONE',  ( 9.500006116823001889, 2.279680316922000127, 7.877692351087999256 ) ) ;
#56663 = CARTESIAN_POINT ( 'NONE',  ( 10.74795391537419853, 4.830118059977199785, 6.936213817702099327 ) ) ;
#56664 = EDGE_CURVE ( 'NONE', #46950, #16623, #67182, .T. ) ;
#56665 = EDGE_CURVE ( 'NONE', #3413, #35475, #45311, .T. ) ;
#56666 = B_SPLINE_CURVE_WITH_KNOTS ( 'NONE', 3,
 ( #27218, #26533, #15693, #20942, #20592, #47861 ),
 .UNSPECIFIED., .F., .F.,
 ( 4, 2, 4 ),
 ( 0.3916346334472008972, 0.6958173167236003653, 1.000000000000000000 ),
 .UNSPECIFIED. ) ;
#56667 = CARTESIAN_POINT ( 'NONE',  ( 9.424850063658244181, 5.349972463430670899, 7.500009360578276052 ) ) ;
#56668 = CIRCLE ( 'NONE', #44450, 12.79999953825000425 ) ;
#56669 = CARTESIAN_POINT ( 'NONE',  ( 9.164680296029999340, 2.899999999999999911, -6.162130047625999474 ) ) ;
#56670 = B_SPLINE_CURVE_WITH_KNOTS ( 'NONE', 3,
 ( #19333, #35092, #20368, #41356, #40659, #56754, #51494, #9525, #14103, #56404, #25268, #9182, #8506, #41009, #41692, #62331 ),
 .UNSPECIFIED., .F., .F.,
 ( 4, 2, 2, 2, 2, 2, 2, 4 ),
 ( 0.000000000000000000, 0.1249999999999919509, 0.1874999999999888978, 0.2499999999999858447, 0.3749999999999896749, 0.4374999999999915623, 0.4999999999999935607, 1.000000000000000000 ),
 .UNSPECIFIED. ) ;
#56671 = EDGE_CURVE ( 'NONE', #30666, #34183, #38841, .T. ) ;
#56672 = EDGE_CURVE ( 'NONE', #51112, #55952, #57701, .T. ) ;
#56673 = CARTESIAN_POINT ( 'NONE',  ( 16.10004050617000004, -3.886235259787000018, -11.90683839252000098 ) ) ;
#56674 = CARTESIAN_POINT ( 'NONE',  ( 11.01511860815784871, -5.215118608160429048, 6.608919745756069553 ) ) ;
#56675 = CARTESIAN_POINT ( 'NONE',  ( 8.132398138459945969, 5.154119579187411482, 6.184746403960440730 ) ) ;
#56676 = EDGE_LOOP ( 'NONE', ( #19912, #4095, #19852, #12520, #51705 ) ) ;
#56677 = CARTESIAN_POINT ( 'NONE',  ( 17.57920827037000322, -3.248109283636080757, 13.61799489948998065 ) ) ;
#56678 = DIRECTION ( 'NONE',  ( -1.000000000000000000, 0.000000000000000000, 1.665334536957000056E-14 ) ) ;
#56679 = EDGE_LOOP ( 'NONE', ( #16175, #42285, #38367, #46849 ) ) ;
#56680 = EDGE_LOOP ( 'NONE', ( #33725, #16950, #63166, #23946 ) ) ;
#56681 = CARTESIAN_POINT ( 'NONE',  ( 10.98656920625009903, 4.032067152264009913, 8.391549386185598536 ) ) ;
#56682 = CARTESIAN_POINT ( 'NONE',  ( 9.593930206849998754, 5.250000000000000000, -7.500000000000000000 ) ) ;
#56683 = CARTESIAN_POINT ( 'NONE',  ( 10.94903032197929882, 4.503839166471300004, 8.204588308639600314 ) ) ;
#56684 = CARTESIAN_POINT ( 'NONE',  ( 10.55991859298999991, 5.094266430778000121, 6.075406703384000018 ) ) ;
#56685 = CARTESIAN_POINT ( 'NONE',  ( 10.44806481732999792, 3.684980864017000091, -6.173120265414000052 ) ) ;
#56686 = CARTESIAN_POINT ( 'NONE',  ( 8.973608660036624940, -3.779042157900793786, -6.653412791890684019 ) ) ;
#56687 = CARTESIAN_POINT ( 'NONE',  ( 10.85068991645999859, -4.478102922274999287, 6.162028334171000488 ) ) ;
#56688 = CARTESIAN_POINT ( 'NONE',  ( 18.12277215905345429, 0.4475098806653864392, -12.59205372277267898 ) ) ;
#56689 = CIRCLE ( 'NONE', #26534, 1.449999999999999956 ) ;
#56690 = CARTESIAN_POINT ( 'NONE',  ( 10.87695483801000051, -5.827068285690999438, -7.814745128155998977 ) ) ;
#56691 = CARTESIAN_POINT ( 'NONE',  ( 11.73256516821459883, -3.293702443348299980, -8.212808089543500500 ) ) ;
#56692 = CARTESIAN_POINT ( 'NONE',  ( 4.599999999999999645, -3.125000000000000000, 13.52084414783465682 ) ) ;
#56693 = ORIENTED_EDGE ( 'NONE', *, *, #10391, .F. ) ;
#56694 = CARTESIAN_POINT ( 'NONE',  ( 11.79999999471800010, 3.216299622513999701, -11.40340969442000052 ) ) ;
#56695 = SURFACE_STYLE_USAGE ( .BOTH. , #62275 ) ;
#56696 = CARTESIAN_POINT ( 'NONE',  ( 6.433333126412498437, -12.43895941528792193, -2.828912463766406482 ) ) ;
#56697 = B_SPLINE_CURVE_WITH_KNOTS ( 'NONE', 3,
 ( #14851, #36514, #63062, #15190, #57838, #30935, #8917, #36172, #20435, #26377, #57483, #9245, #10287, #31621, #9946, #26027, #19753, #52942 ),
 .UNSPECIFIED., .F., .F.,
 ( 4, 2, 2, 2, 2, 2, 2, 2, 4 ),
 ( 0.000000000000000000, 0.1250000000000000000, 0.2500000000000000000, 0.3750000000000000000, 0.5000000000000000000, 0.6250000000000000000, 0.7500000000000000000, 0.8750000000000000000, 1.000000000000000000 ),
 .UNSPECIFIED. ) ;
#56698 = CARTESIAN_POINT ( 'NONE',  ( 9.049464847731002237, 7.846607741563002669, 5.258576131806001364 ) ) ;
#56699 = CARTESIAN_POINT ( 'NONE',  ( 9.659038493598998798, 4.925784867300699865, -6.617216466537199970 ) ) ;
#56700 = CARTESIAN_POINT ( 'NONE',  ( 12.23477282158792612, 2.066986176408053044, 13.84657559728969822 ) ) ;
#56701 = CARTESIAN_POINT ( 'NONE',  ( 11.09999999999999964, 4.000000000000000000, -7.500000000000000000 ) ) ;
#56702 = ORIENTED_EDGE ( 'NONE', *, *, #68407, .T. ) ;
#56703 = CARTESIAN_POINT ( 'NONE',  ( 12.46489138717631029, 0.5244033891532404734, -12.68542455842735706 ) ) ;
#56704 = CIRCLE ( 'NONE', #14285, 1.000000000000000666 ) ;
#56705 = CARTESIAN_POINT ( 'NONE',  ( 25.26999686867947759, 8.359966454775140221, 8.486712842816988456 ) ) ;
#56706 = ORIENTED_EDGE ( 'NONE', *, *, #7743, .F. ) ;
#56707 = CARTESIAN_POINT ( 'NONE',  ( 4.400000000000000355, -1.000000000000000000, 0.000000000000000000 ) ) ;
#56708 = CARTESIAN_POINT ( 'NONE',  ( -15.86200481174999943, -5.599999999999999645, -6.571291218949999902 ) ) ;
#56709 = CARTESIAN_POINT ( 'NONE',  ( 10.77101354018289925, -4.768183399968641822, -6.500416447002272058 ) ) ;
#56710 = CARTESIAN_POINT ( 'NONE',  ( 8.433335197172079134, 2.968768240344807463, 6.285779305140361650 ) ) ;
#56711 = VECTOR ( 'NONE', #18234, 1000.000000000000000 ) ;
#56712 = EDGE_CURVE ( 'NONE', #33691, #26552, #29836, .T. ) ;
#56713 = AXIS2_PLACEMENT_3D ( 'NONE', #35591, #52684, #36264 ) ;
#56714 = CARTESIAN_POINT ( 'NONE',  ( 8.636068280300804645, 5.315145854513802171, -7.853667701454011052 ) ) ;
#56715 = CARTESIAN_POINT ( 'NONE',  ( 0.2277818351675000019, 0.6801881511091000254, 3.471639432493999866 ) ) ;
#56716 = CYLINDRICAL_SURFACE ( 'NONE', #31527, 11.84999999999999964 ) ;
#56717 = EDGE_CURVE ( 'NONE', #34080, #53919, #66315, .T. ) ;
#56718 = VECTOR ( 'NONE', #52318, 1000.000000000000000 ) ;
#56719 = CARTESIAN_POINT ( 'NONE',  ( 12.53614341883831251, 3.148504814753053882, 12.20028441070642700 ) ) ;
#56720 = FACE_OUTER_BOUND ( 'NONE', #64890, .T. ) ;
#56721 = CARTESIAN_POINT ( 'NONE',  ( 11.61364291764652812, 3.140345330584100036, -7.393734108507599601 ) ) ;
#56722 = DIRECTION ( 'NONE',  ( 0.000000000000000000, 1.000000000000000000, 0.000000000000000000 ) ) ;
#56723 = CARTESIAN_POINT ( 'NONE',  ( 10.72128915877000033, 4.673511966357999370, -5.778393480304000462 ) ) ;
#56724 = CARTESIAN_POINT ( 'NONE',  ( 8.796784697134999220, 4.619613413415000203, -6.540930833646799947 ) ) ;
#56726 = CARTESIAN_POINT ( 'NONE',  ( 9.248004441081999261, -4.389076025353599420, 6.658556819429599649 ) ) ;
#56725 = CARTESIAN_POINT ( 'NONE',  ( 9.494442991499999707, -4.054579081944059915, 8.365291319916600798 ) ) ;
#56727 = CARTESIAN_POINT ( 'NONE',  ( 17.55505043854143565, 1.875000000000000000, 12.57541666120756041 ) ) ;
#56728 = ORIENTED_EDGE ( 'NONE', *, *, #56516, .T. ) ;
#56729 = VECTOR ( 'NONE', #14862, 1000.000000000000000 ) ;
#56730 = CARTESIAN_POINT ( 'NONE',  ( 11.48522412107029922, 4.047131449166419870, 8.390877922225699947 ) ) ;
#56731 = B_SPLINE_CURVE_WITH_KNOTS ( 'NONE', 3,
 ( #38687, #3259, #29513, #32755 ),
 .UNSPECIFIED., .F., .F.,
 ( 4, 4 ),
 ( 0.000000000000000000, 0.3058164706682733325 ),
 .UNSPECIFIED. ) ;
#56732 = CARTESIAN_POINT ( 'NONE',  ( 10.40727044253999978, -3.797905333157999941, 5.889909992361999969 ) ) ;
#56733 = CARTESIAN_POINT ( 'NONE',  ( 9.378405316141000370, 3.757578743663700038, 6.384219384258999597 ) ) ;
#56734 = CARTESIAN_POINT ( 'NONE',  ( 23.55075821821200321, -2.914207289901999953, 13.72993041849000129 ) ) ;
#56735 = VECTOR ( 'NONE', #17170, 1000.000000000000000 ) ;
#56736 = CARTESIAN_POINT ( 'NONE',  ( 23.60205915885299888, 11.72032963058999400, -3.891881970957998593 ) ) ;
#56737 = CARTESIAN_POINT ( 'NONE',  ( 11.09999999999999964, -4.000000000000000000, 7.500000000000000000 ) ) ;
#56738 = CARTESIAN_POINT ( 'NONE',  ( 23.56666365135700403, 9.069641144872004901, -7.556701426719000025 ) ) ;
#56739 = ORIENTED_EDGE ( 'NONE', *, *, #13632, .F. ) ;
#56740 = CARTESIAN_POINT ( 'NONE',  ( 10.08655864497999843, -2.992894514506000192, -8.288745882156399958 ) ) ;
#56741 = CARTESIAN_POINT ( 'NONE',  ( 10.66823071782296672, -5.044756569124447587, -5.053267171664180601 ) ) ;
#56742 = CARTESIAN_POINT ( 'NONE',  ( 11.98011496860029901, -3.080230834057799960, 7.971338736265699332 ) ) ;
#56743 = PRODUCT ( '510 Connector Pin', '510 Connector Pin', '', ( #62741 ) ) ;
#56744 = CARTESIAN_POINT ( 'NONE',  ( 17.63949335857236633, 1.765638956106261537, -12.47567715783345577 ) ) ;
#56745 = CARTESIAN_POINT ( 'NONE',  ( 8.714021517297007691, -3.496029227938000972, -6.351413116489997179 ) ) ;
#56746 = CARTESIAN_POINT ( 'NONE',  ( 24.70770306079000278, -3.610860736573000107, 12.15153796058999980 ) ) ;
#56747 = CARTESIAN_POINT ( 'NONE',  ( 9.573320215454998561, -2.624754973437999794, -6.486841649805000110 ) ) ;
#56748 = CARTESIAN_POINT ( 'NONE',  ( 0.9051401325418416688, -0.9161175952574773795, -3.408904368339105595 ) ) ;
#56749 = EDGE_LOOP ( 'NONE', ( #40319, #6561, #32684, #35918 ) ) ;
#56750 = CARTESIAN_POINT ( 'NONE',  ( 9.164680296029999340, 2.899999999999999911, -6.162130047625999474 ) ) ;
#56751 = ADVANCED_FACE ( 'NONE', ( #43930 ), #50207, .T. ) ;
#56752 = CARTESIAN_POINT ( 'NONE',  ( 12.27567203567526910, 0.4994936913945444146, -13.99109680828866686 ) ) ;
#56753 = ADVANCED_FACE ( 'NONE', ( #62402 ), #8924, .T. ) ;
#56754 = CARTESIAN_POINT ( 'NONE',  ( 23.62146722581017144, 13.40161425103470805, 3.915220144369890853 ) ) ;
#56755 = CARTESIAN_POINT ( 'NONE',  ( 24.44496356267099912, -8.810485190366000197, 8.810508100388000585 ) ) ;
#56756 = CARTESIAN_POINT ( 'NONE',  ( 18.17992876607663177, 2.487411392565050505, 12.45448399074147972 ) ) ;
#56757 = CARTESIAN_POINT ( 'NONE',  ( 9.700639158771000581, 4.262870449202000422, -8.811513791423999820 ) ) ;
#56758 = CARTESIAN_POINT ( 'NONE',  ( 12.16287348028854964, -4.761955701524100526, 7.088026579158399620 ) ) ;
#56759 = VERTEX_POINT ( 'NONE', #41427 ) ;
#56760 = CARTESIAN_POINT ( 'NONE',  ( 9.312955771054708620, -2.920709800291079627, -8.329395787248037308 ) ) ;
#56761 = CARTESIAN_POINT ( 'NONE',  ( 18.26192063240346286, 2.355523948311720073, -13.80042196861913339 ) ) ;
#56762 = ORIENTED_EDGE ( 'NONE', *, *, #51955, .F. ) ;
#56763 = CARTESIAN_POINT ( 'NONE',  ( 10.56726717315599906, -4.659895246859299789, 8.062357722167599050 ) ) ;
#56764 = CYLINDRICAL_SURFACE ( 'NONE', #16739, 1.000000000000000666 ) ;
#56765 = CARTESIAN_POINT ( 'NONE',  ( 8.564679719593000229, 4.146787477634999775, -5.941926545671999627 ) ) ;
#56766 = CARTESIAN_POINT ( 'NONE',  ( 11.03111947020579819, 3.091200775993899974, 7.825000000000000178 ) ) ;
#56767 = CARTESIAN_POINT ( 'NONE',  ( 11.64122412107036908, -3.937930136014310190, -6.326756392227999015 ) ) ;
#56768 = CARTESIAN_POINT ( 'NONE',  ( 11.09999999999999964, -1.300000000000000044, 9.662944685757000940 ) ) ;
#56769 = PRESENTATION_LAYER_ASSIGNMENT (  '', '', ( #29982 ) ) ;
#56770 = CARTESIAN_POINT ( 'NONE',  ( 9.002599499754321499, -2.949662297526366661, -7.998361244042363261 ) ) ;
#56771 = ORIENTED_EDGE ( 'NONE', *, *, #67625, .F. ) ;
#56772 = FACE_OUTER_BOUND ( 'NONE', #10456, .T. ) ;
#56773 = CARTESIAN_POINT ( 'NONE',  ( 11.14975833414749928, 3.203462856645999945, 7.174999999999999822 ) ) ;
#56774 = CARTESIAN_POINT ( 'NONE',  ( 8.541054719591000932, 3.807713920470999991, -9.221758713517999695 ) ) ;
#56775 = ORIENTED_EDGE ( 'NONE', *, *, #43902, .F. ) ;
#56776 = EDGE_CURVE ( 'NONE', #64065, #51247, #14200, .T. ) ;
#56777 = CONICAL_SURFACE ( 'NONE', #44509, 13.94232984211000037, 1.233427423210649021 ) ;
#56778 = CARTESIAN_POINT ( 'NONE',  ( 10.31499646082999888, 5.458376174241999834, -8.355105941236999456 ) ) ;
#56779 = ORIENTED_EDGE ( 'NONE', *, *, #62610, .F. ) ;
#56780 = CARTESIAN_POINT ( 'NONE',  ( 8.568822372493999140, 3.671800173070400408, 6.426348619097999482 ) ) ;
#56781 = CARTESIAN_POINT ( 'NONE',  ( 17.67527538783546959, -3.190136231796161237, -12.18946489087518970 ) ) ;
#56782 = CARTESIAN_POINT ( 'NONE',  ( 11.26375800691000073, -11.80847110903000186, -1.384521730739000089 ) ) ;
#56783 = PRESENTATION_LAYER_ASSIGNMENT (  '', '', ( #14365 ) ) ;
#56784 = CARTESIAN_POINT ( 'NONE',  ( 4.400020611144109139, -0.9303305181083711961, -0.7135878619021024383 ) ) ;
#56785 = CARTESIAN_POINT ( 'NONE',  ( 13.73895793914714680, -8.868838256396809783, -7.856013393113983945 ) ) ;
#56786 = ORIENTED_EDGE ( 'NONE', *, *, #48715, .F. ) ;
#56787 = CARTESIAN_POINT ( 'NONE',  ( 8.046924339810814786, 4.567502412556758706, -6.230116480647599708 ) ) ;
#56788 = FACE_OUTER_BOUND ( 'NONE', #39547, .T. ) ;
#56789 = CIRCLE ( 'NONE', #5425, 2.000000000000001332 ) ;
#56790 = CARTESIAN_POINT ( 'NONE',  ( 5.500000000000000000, -0.2500000000000000000, 3.149999999999999911 ) ) ;
#56791 = CARTESIAN_POINT ( 'NONE',  ( 12.22680470609049230, 2.076949241994379136, -13.84509419021260435 ) ) ;
#56792 = DIRECTION ( 'NONE',  ( -1.000000000000000000, 0.000000000000000000, 0.000000000000000000 ) ) ;
#56793 = CARTESIAN_POINT ( 'NONE',  ( 18.24051303026600124, 3.055556278716000218, 11.39470302754000031 ) ) ;
#56794 = CARTESIAN_POINT ( 'NONE',  ( 18.14748133481813852, -2.299853946675995520, 12.49599191557683930 ) ) ;
#56795 = ORIENTED_EDGE ( 'NONE', *, *, #12479, .F. ) ;
#56796 = EDGE_LOOP ( 'NONE', ( #43307, #34593, #8963, #59235, #60246 ) ) ;
#56797 = CARTESIAN_POINT ( 'NONE',  ( 9.327795280414001411, 3.161445734422999809, -6.178649910536000434 ) ) ;
#56798 = EDGE_CURVE ( 'NONE', #26237, #60415, #10471, .T. ) ;
#56799 = CARTESIAN_POINT ( 'NONE',  ( 7.202583736560634442, 0.2999999999999999889, 3.098821334907657654 ) ) ;
#56800 = CARTESIAN_POINT ( 'NONE',  ( 12.20625471196118816, -2.679103183993202464, 13.63384013638393100 ) ) ;
#56801 = CARTESIAN_POINT ( 'NONE',  ( 24.14113419639268798, 3.327735694157559099, 12.48984860408194031 ) ) ;
#56802 = CARTESIAN_POINT ( 'NONE',  ( 23.86947024834200093, 9.628432572233000641, -9.781540490154000622 ) ) ;
#56803 = CARTESIAN_POINT ( 'NONE',  ( 18.53959992722300143, -2.682146997965999979, -11.29770844980000000 ) ) ;
#56805 = DIRECTION ( 'NONE',  ( 0.000000000000000000, 1.000000000000000000, 0.000000000000000000 ) ) ;
#56804 = CARTESIAN_POINT ( 'NONE',  ( 9.650442991499998513, -4.071878040089889517, 8.639547276484998761 ) ) ;
#56806 = CARTESIAN_POINT ( 'NONE',  ( 10.47530200610849604, 5.350262918594154371, 7.499984559551275964 ) ) ;
#56807 = ORIENTED_EDGE ( 'NONE', *, *, #44763, .F. ) ;
#56808 = CARTESIAN_POINT ( 'NONE',  ( 7.429572863418363760, 3.823161772629042332, -6.150479629790767788 ) ) ;
#56809 = CIRCLE ( 'NONE', #965, 12.39999890530000037 ) ;
#56810 = CARTESIAN_POINT ( 'NONE',  ( 23.89320776801300283, -11.54071136943000297, -2.936967729234000402 ) ) ;
#56811 = CARTESIAN_POINT ( 'NONE',  ( 9.749152735436000583, -5.239375073306999475, -6.095351682555999240 ) ) ;
#56812 = CARTESIAN_POINT ( 'NONE',  ( 7.954680807037616042, 4.944643250900698561, 6.423735648896208517 ) ) ;
#56813 = CIRCLE ( 'NONE', #48970, 2.400000066501999818 ) ;
#56814 = CARTESIAN_POINT ( 'NONE',  ( 18.18003600477294057, -2.504879791492763630, -12.45042248974575294 ) ) ;
#56815 = CARTESIAN_POINT ( 'NONE',  ( 11.04829169656000154, -5.240875637261000364, 5.064311916315999973 ) ) ;
#56816 = DIRECTION ( 'NONE',  ( 1.000000000000000000, 0.000000000000000000, 0.000000000000000000 ) ) ;
#56817 = CARTESIAN_POINT ( 'NONE',  ( 16.10004050617000004, -3.886235259787000018, -11.90683839252000098 ) ) ;
#56818 = CARTESIAN_POINT ( 'NONE',  ( 6.614116717018000635, 1.103230901197000069, 0.4075104821199000416 ) ) ;
#56819 = CARTESIAN_POINT ( 'NONE',  ( 24.67921570607400383, -3.567514742249000115, 12.13750887372000165 ) ) ;
#56820 = CARTESIAN_POINT ( 'NONE',  ( 3.305748555932999988, 1.181428906966000225, 3.215438517307999788 ) ) ;
#56821 = ORIENTED_EDGE ( 'NONE', *, *, #25478, .T. ) ;
#56822 = CARTESIAN_POINT ( 'NONE',  ( 12.44180168752028770, 0.6226057762474821455, -12.58460959628226128 ) ) ;
#56823 = CARTESIAN_POINT ( 'NONE',  ( 12.24831336539215521, -2.784226791605522777, -12.38079107515907396 ) ) ;
#56824 = CARTESIAN_POINT ( 'NONE',  ( 11.09999999999999964, 7.281355457699000056, 6.286510842043999681 ) ) ;
#56825 = CARTESIAN_POINT ( 'NONE',  ( 8.962739158771999115, 5.445214367171999470, 7.703373622193999459 ) ) ;
#56826 = SURFACE_SIDE_STYLE ('',( #50549 ) ) ;
#56827 = ORIENTED_EDGE ( 'NONE', *, *, #29167, .F. ) ;
#56828 = CARTESIAN_POINT ( 'NONE',  ( 6.652664783001999815, 0.6479012572794000668, 0.9815235057283998588 ) ) ;
#56829 = EDGE_CURVE ( 'NONE', #46546, #61230, #19647, .T. ) ;
#56830 = APPLICATION_PROTOCOL_DEFINITION ( 'draft international standard', 'automotive_design', 1998, #32885 ) ;
#56831 = ADVANCED_FACE ( 'NONE', ( #3330 ), #9600, .T. ) ;
#56832 = CARTESIAN_POINT ( 'NONE',  ( 5.199999999864999722, 0.2499999998655000055, 9.776630292580000159 ) ) ;
#56833 = B_SPLINE_CURVE_WITH_KNOTS ( 'NONE', 3,
 ( #56013, #8807, #3217, #45868 ),
 .UNSPECIFIED., .F., .F.,
 ( 4, 4 ),
 ( 0.000000000000000000, 1.000000000000000000 ),
 .UNSPECIFIED. ) ;
#56834 = CARTESIAN_POINT ( 'NONE',  ( 13.43887202961200167, -11.47449689335000045, -1.782105406474000064 ) ) ;
#56835 = CARTESIAN_POINT ( 'NONE',  ( 7.783732762364405033, 2.886508771623532699, 6.705447760689092540 ) ) ;
#56836 = CARTESIAN_POINT ( 'NONE',  ( 10.68546886766499959, 3.433493735705800187, -6.470713638631999665 ) ) ;
#56837 = VERTEX_POINT ( 'NONE', #20442 ) ;
#56838 = CARTESIAN_POINT ( 'NONE',  ( 10.37026726325999881, -5.571557883540000589, 7.748386351620999868 ) ) ;
#56839 = VERTEX_POINT ( 'NONE', #46335 ) ;
#56840 = CYLINDRICAL_SURFACE ( 'NONE', #68584, 0.4999999999999998335 ) ;
#56841 = CARTESIAN_POINT ( 'NONE',  ( 8.149355646792999508, -2.583664704444999849, 6.684748541034000624 ) ) ;
#56842 = CARTESIAN_POINT ( 'NONE',  ( 18.26152657770008148, 0.1657344298535251004, -13.99903850390423798 ) ) ;
#56843 = ORIENTED_EDGE ( 'NONE', *, *, #42696, .F. ) ;
#56844 = CARTESIAN_POINT ( 'NONE',  ( 8.492977932633323235, 3.398140593268752507, -9.149195927865305222 ) ) ;
#56845 = CARTESIAN_POINT ( 'NONE',  ( 11.01333310117525954, -5.463772421450651784, -7.751599404490038481 ) ) ;
#56846 = CARTESIAN_POINT ( 'NONE',  ( 8.029179719589000896, 3.460181152982999997, -6.031076961652000357 ) ) ;
#56847 = DIRECTION ( 'NONE',  ( -1.000000000000000000, 0.000000000000000000, 0.000000000000000000 ) ) ;
#56848 = CARTESIAN_POINT ( 'NONE',  ( 8.194123395920479780, -2.898248195268428251, 6.620168246131465928 ) ) ;
#56849 = ORIENTED_EDGE ( 'NONE', *, *, #19795, .F. ) ;
#56850 = CARTESIAN_POINT ( 'NONE',  ( 2.105140132540083808, 0.9161175952574701631, 3.408904368339106927 ) ) ;
#56851 = CARTESIAN_POINT ( 'NONE',  ( 9.406851002546000373, 2.832432432432000269, -6.822293592207000934 ) ) ;
#56852 = CARTESIAN_POINT ( 'NONE',  ( 5.396693173017498957, 1.310679582531385279, 0.7554284705563519831 ) ) ;
#56853 = EDGE_CURVE ( 'NONE', #62750, #12534, #60505, .T. ) ;
#56854 = CARTESIAN_POINT ( 'NONE',  ( 10.90635170712999980, -3.089674976714000376, -6.534319251717000121 ) ) ;
#56855 = FACE_OUTER_BOUND ( 'NONE', #39915, .T. ) ;
#56856 = ORIENTED_EDGE ( 'NONE', *, *, #36301, .F. ) ;
#56857 = CARTESIAN_POINT ( 'NONE',  ( 17.96365918282847218, 0.4729502186230333249, -13.88916975806286658 ) ) ;
#56858 = ADVANCED_FACE ( 'NONE', ( #35165 ), #67296, .T. ) ;
#56859 = CARTESIAN_POINT ( 'NONE',  ( 6.949999692120000461, -11.00717859340000082, -1.432487142323000118 ) ) ;
#56860 = CARTESIAN_POINT ( 'NONE',  ( 10.13706886426420084, -2.899999999999999911, 6.444141223280826836 ) ) ;
#56861 = CARTESIAN_POINT ( 'NONE',  ( 12.80505043854144276, 0.6878608935795343937, 12.61273126665598276 ) ) ;
#56862 = CARTESIAN_POINT ( 'NONE',  ( 12.21303990359567848, 0.2014071429975201610, -13.89805485625563186 ) ) ;
#56863 = CARTESIAN_POINT ( 'NONE',  ( 18.17995611468272443, -2.522932803854498918, 12.44624262618111921 ) ) ;
#56864 = VERTEX_POINT ( 'NONE', #35838 ) ;
#56865 = CARTESIAN_POINT ( 'NONE',  ( 11.14767835872009982, -4.874341053673500568, -6.948943352864199952 ) ) ;
#56866 = VERTEX_POINT ( 'NONE', #35503 ) ;
#56867 = CARTESIAN_POINT ( 'NONE',  ( 11.29622358543999994, 3.561657733933999648, 6.266050246368000565 ) ) ;
#56868 = CARTESIAN_POINT ( 'NONE',  ( 0.1499942179680000265, -0.3599680999394040404, 2.749953718116143087 ) ) ;
#56869 = CARTESIAN_POINT ( 'NONE',  ( 9.526695280414001488, 5.462898983065000102, -8.055936939571999744 ) ) ;
#56870 = CARTESIAN_POINT ( 'NONE',  ( 3.564596078290000136, 3.244059008440000280, 1.796025925329000072 ) ) ;
#56871 = CARTESIAN_POINT ( 'NONE',  ( 10.04002603384999937, -2.348908096685999869, -7.136751747961000092 ) ) ;
#56872 = DIRECTION ( 'NONE',  ( 1.000000000000000000, 0.000000000000000000, 0.000000000000000000 ) ) ;
#56873 = CARTESIAN_POINT ( 'NONE',  ( 23.58436998763100334, 13.25821845536999888, 4.304235178824000307 ) ) ;
#56874 = ORIENTED_EDGE ( 'NONE', *, *, #44625, .F. ) ;
#56875 = CARTESIAN_POINT ( 'NONE',  ( 11.71149010443640037, -2.862435565199000109, 7.414927836855409460 ) ) ;
#56876 = CARTESIAN_POINT ( 'NONE',  ( 10.62795461073813996, 2.419700658069591448, -6.689391080427925296 ) ) ;
#56877 = CARTESIAN_POINT ( 'NONE',  ( 15.90830001818700090, 9.238654026387999707, 8.377706362734000933 ) ) ;
#56878 = CARTESIAN_POINT ( 'NONE',  ( 8.335879440378999305, -4.310353212080000773, 9.459493062793997709 ) ) ;
#56879 = CIRCLE ( 'NONE', #53537, 2.574999650349000024 ) ;
#56881 = DIRECTION ( 'NONE',  ( -0.9999999999991096011, 6.425037516353057767E-07, 1.169597258120009531E-06 ) ) ;
#56880 = CARTESIAN_POINT ( 'NONE',  ( 10.55991859298999991, 5.094266430778000121, 6.075406703384000018 ) ) ;
#56882 = CARTESIAN_POINT ( 'NONE',  ( 10.64949279009019989, 3.739015461786900030, -8.468936491037499792 ) ) ;
#56883 = DIRECTION ( 'NONE',  ( 1.000000000000000000, 0.000000000000000000, 0.000000000000000000 ) ) ;
#56884 = CARTESIAN_POINT ( 'NONE',  ( 9.097772138681998300, 3.626242194157900389, -6.567719246739500250 ) ) ;
#56885 = CARTESIAN_POINT ( 'NONE',  ( 17.67403227923241360, 0.7096370184368610001, 12.58000072970462924 ) ) ;
#56886 = PRODUCT_DEFINITION_SHAPE ( 'NONE', 'NONE',  #69198 ) ;
#56887 = CARTESIAN_POINT ( 'NONE',  ( 24.44917776433500123, 3.519943607436000210, 12.30316564740000196 ) ) ;
#56888 = CARTESIAN_POINT ( 'NONE',  ( 10.55569598648999907, 5.130952141044000214, 6.826612223887499553 ) ) ;
#56889 = CARTESIAN_POINT ( 'NONE',  ( 20.10000000000000142, 0.000000000000000000, 0.000000000000000000 ) ) ;
#56890 = VERTEX_POINT ( 'NONE', #57156 ) ;
#56891 = CARTESIAN_POINT ( 'NONE',  ( 7.614808059621999803, -3.326257819185999942, 8.794522506294001118 ) ) ;
#56892 = CARTESIAN_POINT ( 'NONE',  ( 23.60000000000000142, -11.49391741900999975, -4.090215442373000165 ) ) ;
#56893 = FACE_OUTER_BOUND ( 'NONE', #62073, .T. ) ;
#56894 = CARTESIAN_POINT ( 'NONE',  ( 10.35646369190143368, 5.100000000000000533, 6.665341197350102220 ) ) ;
#56895 = ORIENTED_EDGE ( 'NONE', *, *, #39733, .F. ) ;
#56896 = CARTESIAN_POINT ( 'NONE',  ( 18.35309301929700254, 2.844470671424999875, 12.04740840676999802 ) ) ;
#56897 = CARTESIAN_POINT ( 'NONE',  ( 11.76588784977539781, 2.879134238109999799, 7.564049652083489228 ) ) ;
#56898 = CARTESIAN_POINT ( 'NONE',  ( 10.66042971959000063, 2.315663237570999566, -7.431702255173999738 ) ) ;
#56899 = ORIENTED_EDGE ( 'NONE', *, *, #35371, .F. ) ;
#56900 = DIRECTION ( 'NONE',  ( 1.000000000000000000, 0.000000000000000000, 0.000000000000000000 ) ) ;
#56901 = CARTESIAN_POINT ( 'NONE',  ( 11.00000000000000000, -5.200000000000000178, 5.865766984179000332 ) ) ;
#56902 = CARTESIAN_POINT ( 'NONE',  ( 10.15303300763299887, 4.787165141710600480, 6.674373427955200277 ) ) ;
#56903 = LINE ( 'NONE', #35922, #62293 ) ;
#56904 = DIRECTION ( 'NONE',  ( -0.7071068156326932863, 0.000000000000000000, -0.7071067467404001938 ) ) ;
#56905 = ORIENTED_EDGE ( 'NONE', *, *, #39500, .F. ) ;
#56906 = CARTESIAN_POINT ( 'NONE',  ( 11.68591862085600219, -3.663505620393999962, 12.01771987839999944 ) ) ;
#56907 = EDGE_CURVE ( 'NONE', #11716, #22688, #20101, .T. ) ;
#56908 = EDGE_CURVE ( 'NONE', #68613, #53586, #8876, .T. ) ;
#56909 = CARTESIAN_POINT ( 'NONE',  ( 8.263039158770000725, 5.485324155719999872, -6.315380258366999122 ) ) ;
#56910 = CARTESIAN_POINT ( 'NONE',  ( 8.256279407735984677, -5.320103330200151248, 8.633016269157472777 ) ) ;
#56911 = CARTESIAN_POINT ( 'NONE',  ( 11.76588784977539781, -5.120865761890000201, -7.435950347916509884 ) ) ;
#56912 = CARTESIAN_POINT ( 'NONE',  ( 10.20662143724499948, -3.150324864944999970, 8.456261759323901117 ) ) ;
#56913 = ORIENTED_EDGE ( 'NONE', *, *, #48078, .F. ) ;
#56914 = CARTESIAN_POINT ( 'NONE',  ( 10.72098219424000121, -5.042358674275999597, -5.112202241721999663 ) ) ;
#56915 = DIRECTION ( 'NONE',  ( -1.000000000000000000, 0.000000000000000000, 0.000000000000000000 ) ) ;
#56916 = ORIENTED_EDGE ( 'NONE', *, *, #11258, .T. ) ;
#56917 = CARTESIAN_POINT ( 'NONE',  ( 12.80505043854146940, -1.816864895258029522, -13.85234397965874464 ) ) ;
#56918 = ORIENTED_EDGE ( 'NONE', *, *, #12102, .T. ) ;
#56919 = CARTESIAN_POINT ( 'NONE',  ( 9.793154437819998392, -5.792391408692000532, -6.955579396894000510 ) ) ;
#56920 = CARTESIAN_POINT ( 'NONE',  ( 2.478056799210041738, 2.150913519912206695, -2.798833948393626869 ) ) ;
#56921 = CARTESIAN_POINT ( 'NONE',  ( 11.68277869730536977, 3.468607053297499743, -6.452143920160000157 ) ) ;
#56922 = B_SPLINE_CURVE_WITH_KNOTS ( 'NONE', 3,
 ( #35526, #18416, #45674, #50226 ),
 .UNSPECIFIED., .F., .F.,
 ( 4, 4 ),
 ( 0.000000000000000000, 1.000000000000000000 ),
 .UNSPECIFIED. ) ;
#56923 = CARTESIAN_POINT ( 'NONE',  ( 11.72056920625029974, -3.952687217764870198, 8.815417147437999645 ) ) ;
#56924 = CARTESIAN_POINT ( 'NONE',  ( 12.18833199825126101, 2.603395164171333764, -12.42692484756187810 ) ) ;
#56925 = CARTESIAN_POINT ( 'NONE',  ( 10.84995525820099971, -4.107710726525199973, 8.635644537520001052 ) ) ;
#56926 = CARTESIAN_POINT ( 'NONE',  ( 7.565635841228000480, 3.206360348473000332, 5.681727837477000165 ) ) ;
#56927 = ORIENTED_EDGE ( 'NONE', *, *, #43457, .T. ) ;
#56928 = AXIS2_PLACEMENT_3D ( 'NONE', #45920, #52885, #37150 ) ;
#56929 = CARTESIAN_POINT ( 'NONE',  ( 9.521013540183334456, 4.768183399968643599, -8.499583552997725278 ) ) ;
#56930 = CARTESIAN_POINT ( 'NONE',  ( 9.278331853207999913, -5.791549888895000109, 7.752110689268000954 ) ) ;
#56931 = CARTESIAN_POINT ( 'NONE',  ( 25.50736871274565232, -8.309691349922452730, -8.116382010822352555 ) ) ;
#56932 = ORIENTED_EDGE ( 'NONE', *, *, #35158, .T. ) ;
#56933 = B_SPLINE_SURFACE_WITH_KNOTS ( 'NONE', 3, 3, ( 
 ( #24957, #67592, #19367, #25299 ),
 ( #35121, #52210, #40352, #66912 ),
 ( #18690, #20056, #56086, #41384 ),
 ( #29544, #8195, #62694, #3287 ),
 ( #35460, #30217, #29886, #51194 ),
 ( #50846, #14814, #40689, #36135 ) ),
 .UNSPECIFIED., .F., .F., .F.,
 ( 4, 1, 1, 4 ),
 ( 4, 4 ),
 ( 0.1423941366080999915, 0.3333333333333000081, 0.6666666666667000474, 0.8219462302418999444 ),
 ( -0.1256563615234000120, 1.125656361508000192 ),
 .UNSPECIFIED. ) ;
#56934 = CARTESIAN_POINT ( 'NONE',  ( 12.78418764580521660, -3.124999405572221445, -12.28373085793387531 ) ) ;
#56935 = EDGE_CURVE ( 'NONE', #36490, #10153, #37589, .T. ) ;
#56936 = CARTESIAN_POINT ( 'NONE',  ( 10.37457053952199892, 3.551693493661699730, 8.548957288282998945 ) ) ;
#56937 = CARTESIAN_POINT ( 'NONE',  ( 10.86460564679000029, -3.843601288168000174, -5.985268170611000471 ) ) ;
#56938 = CARTESIAN_POINT ( 'NONE',  ( 7.721693597669004205, 9.012061377215999869, -5.588307756570000784 ) ) ;
#56939 = CARTESIAN_POINT ( 'NONE',  ( 17.85446786537200126, -3.297647132553999771, -11.83458225989999946 ) ) ;
#56940 = CARTESIAN_POINT ( 'NONE',  ( 24.36958145734899972, -8.861545501181000262, 8.807436093055001081 ) ) ;
#56941 = CARTESIAN_POINT ( 'NONE',  ( 12.66207816929887819, -1.891226320509243664, -13.78383611977690570 ) ) ;
#56942 = CARTESIAN_POINT ( 'NONE',  ( 11.85159063708299954, -3.174974693948799942, -7.731961446576300467 ) ) ;
#56943 = CARTESIAN_POINT ( 'NONE',  ( 10.22272469555899832, -3.360453478306600239, -6.393520617113999549 ) ) ;
#56944 = CARTESIAN_POINT ( 'NONE',  ( 17.57925688241715179, -3.199751027636643208, 12.18694352263475089 ) ) ;
#56945 = ORIENTED_EDGE ( 'NONE', *, *, #50265, .F. ) ;
#56946 = ORIENTED_EDGE ( 'NONE', *, *, #4804, .T. ) ;
#56947 = CARTESIAN_POINT ( 'NONE',  ( 10.88508678867000157, -5.158304027353000087, 5.065542421513000271 ) ) ;
#56948 = CARTESIAN_POINT ( 'NONE',  ( 12.80000000000000071, -11.23412379136000006, 3.084957477885999833 ) ) ;
#56949 = CARTESIAN_POINT ( 'NONE',  ( 17.55505043854147118, -3.125000000000000000, 13.52084414783465860 ) ) ;
#56950 = CARTESIAN_POINT ( 'NONE',  ( 9.662441121991999893, 4.824173073626999653, -8.517602418144999632 ) ) ;
#56951 = DIRECTION ( 'NONE',  ( 0.000000000000000000, 1.000000000000000000, 0.000000000000000000 ) ) ;
#56952 = CARTESIAN_POINT ( 'NONE',  ( 18.11597065765684533, 2.775858272760586054, 12.38300578299705812 ) ) ;
#56953 = CARTESIAN_POINT ( 'NONE',  ( 18.06944243593800081, 3.222040310929999762, -11.85748006108999952 ) ) ;
#56954 = CARTESIAN_POINT ( 'NONE',  ( 11.05639637898999972, 5.030226177531999632, 6.028288223959999748 ) ) ;
#56955 = CARTESIAN_POINT ( 'NONE',  ( 10.16712151127301667, -5.079456268609191305, -8.329490867415614730 ) ) ;
#56956 = ORIENTED_EDGE ( 'NONE', *, *, #1178, .F. ) ;
#56957 = CARTESIAN_POINT ( 'NONE',  ( 12.43829333464982234, -1.993817424706645802, 12.55522976296197157 ) ) ;
#56958 = CARTESIAN_POINT ( 'NONE',  ( 9.070430433046999141, -4.737822807309499673, -7.044669955395099770 ) ) ;
#56959 = CARTESIAN_POINT ( 'NONE',  ( 9.555697025339000561, 2.440752375194999768, 6.680879724048000234 ) ) ;
#56960 = CARTESIAN_POINT ( 'NONE',  ( 11.22702344389999851, -5.004394439171999664, 8.109550315577399360 ) ) ;
#56961 = CARTESIAN_POINT ( 'NONE',  ( 9.965360841230999966, 4.034680274230000308, -6.102912434217000026 ) ) ;
#56962 = CARTESIAN_POINT ( 'NONE',  ( 10.05862282008599884, 4.666276081381299790, -8.574682153725998290 ) ) ;
#56963 = CARTESIAN_POINT ( 'NONE',  ( 12.51941477301789796, 0.5560043133243441904, 12.68361349193353860 ) ) ;
#56964 = ADVANCED_FACE ( 'NONE', ( #52258 ), #24319, .T. ) ;
#56965 = EDGE_CURVE ( 'NONE', #69137, #13026, #62736, .T. ) ;
#56966 = CARTESIAN_POINT ( 'NONE',  ( 9.149954719592001240, 4.175915362023999933, 5.699506188181000077 ) ) ;
#56967 = CARTESIAN_POINT ( 'NONE',  ( 11.15982925107999968, 5.578232410510000072, 8.067793621926998782 ) ) ;
#56968 = CARTESIAN_POINT ( 'NONE',  ( 11.40156680346000151, -3.471758886279999956, 11.27177987500999912 ) ) ;
#56969 = VERTEX_POINT ( 'NONE', #47019 ) ;
#56970 = CARTESIAN_POINT ( 'NONE',  ( 8.458179719589999479, 5.332332124071999857, -8.487089944253000340 ) ) ;
#56971 = CARTESIAN_POINT ( 'NONE',  ( 7.160780970049000160, 0.2385410637492000052, -1.467737005547999907 ) ) ;
#56972 = CARTESIAN_POINT ( 'NONE',  ( 8.965984360231564310, 5.205022649008997249, 8.206117015345389731 ) ) ;
#56973 = CARTESIAN_POINT ( 'NONE',  ( 9.893930206848997599, 2.750000000000000000, -7.500000000000000000 ) ) ;
#56974 = CARTESIAN_POINT ( 'NONE',  ( 10.27101354018233437, 3.231816600031359066, -6.500416447002272058 ) ) ;
#56975 = VECTOR ( 'NONE', #19527, 1000.000000000000000 ) ;
#56976 = CARTESIAN_POINT ( 'NONE',  ( 10.72333863405319931, -3.380905141010200232, -8.289729326049599223 ) ) ;
#56977 = ORIENTED_EDGE ( 'NONE', *, *, #19128, .T. ) ;
#56978 = CARTESIAN_POINT ( 'NONE',  ( 1.253018509565999805, -2.315742118336999944, -2.746122198278999615 ) ) ;
#56979 = CARTESIAN_POINT ( 'NONE',  ( 11.58810207955109917, 3.203462856645999945, 7.825000000000000178 ) ) ;
#56981 = CARTESIAN_POINT ( 'NONE',  ( 13.60261247405900242, -9.239907047945001395, -8.094831983377998696 ) ) ;
#56980 = CARTESIAN_POINT ( 'NONE',  ( 9.972021765239443170, 2.299830290065005833, 7.025646633466952728 ) ) ;
#56982 = CARTESIAN_POINT ( 'NONE',  ( 18.15114771535201754, -2.688105180961021468, 13.63176637561060645 ) ) ;
#56983 = CARTESIAN_POINT ( 'NONE',  ( 11.83810207955129989, -3.203462856645999945, 7.174999999999999822 ) ) ;
#56984 = CARTESIAN_POINT ( 'NONE',  ( 12.36183802548528377, -3.095880799707801057, 13.65340897264974629 ) ) ;
#56985 = CARTESIAN_POINT ( 'NONE',  ( 17.60000000000000142, 10.78295181803999903, -4.410266442048000002 ) ) ;
#56986 = CARTESIAN_POINT ( 'NONE',  ( 25.29995823066400362, -11.13046982544999963, 3.427501264366999756 ) ) ;
#56987 = CARTESIAN_POINT ( 'NONE',  ( 10.31021345716899873, 4.636538040886300394, 6.921280946186199934 ) ) ;
#56988 = EDGE_LOOP ( 'NONE', ( #38765, #54882, #32655, #52101 ) ) ;
#56989 = CARTESIAN_POINT ( 'NONE',  ( 7.892607780408998686, 5.480308727866000318, 8.192324747680999053 ) ) ;
#56990 = EDGE_CURVE ( 'NONE', #51298, #5657, #3009, .T. ) ;
#56992 = CARTESIAN_POINT ( 'NONE',  ( 11.08729972629000038, -2.258669075224000178, -7.034582301298999418 ) ) ;
#56991 = CARTESIAN_POINT ( 'NONE',  ( 5.621035669130999501, -1.553728905769999891, -0.4396155223175000071 ) ) ;
#56993 = CARTESIAN_POINT ( 'NONE',  ( 7.468789704280648145, -2.309885600679958628, 7.088095784442930203 ) ) ;
#56994 = CARTESIAN_POINT ( 'NONE',  ( 18.09779443563016343, -0.3101119056630274873, 13.89534721487939528 ) ) ;
#56995 = CARTESIAN_POINT ( 'NONE',  ( 2.081794735327000545, 3.036063727655999855, -1.493670828108000004 ) ) ;
#56996 = ORIENTED_EDGE ( 'NONE', *, *, #58923, .T. ) ;
#56997 = CARTESIAN_POINT ( 'NONE',  ( 1.906232294096261715, -0.2008767396709452702, 3.296684669105510945 ) ) ;
#56998 = EDGE_CURVE ( 'NONE', #34006, #4545, #36492, .T. ) ;
#56999 = CARTESIAN_POINT ( 'NONE',  ( 10.93210941423800087, -3.358814833524500276, 8.082391773166900606 ) ) ;
#57000 = CARTESIAN_POINT ( 'NONE',  ( 11.55670819615736455, 3.379350336066780702, 8.119355997108680612 ) ) ;
#57001 = CARTESIAN_POINT ( 'NONE',  ( 10.25888757983999966, 4.512388525173999909, 5.993701490107000929 ) ) ;
#57002 = CARTESIAN_POINT ( 'NONE',  ( 10.96533729122639933, 2.859653469230999612, 7.529998433785960010 ) ) ;
#57003 = B_SPLINE_CURVE_WITH_KNOTS ( 'NONE', 3,
 ( #45234, #54676, #38594, #28465 ),
 .UNSPECIFIED., .F., .F.,
 ( 4, 4 ),
 ( 0.000000000000000000, 1.000000000000000000 ),
 .UNSPECIFIED. ) ;
#57004 = B_SPLINE_CURVE_WITH_KNOTS ( 'NONE', 3,
 ( #40921, #62244, #57000, #9436, #4194, #57334, #63261, #4534, #20283, #25531 ),
 .UNSPECIFIED., .F., .F.,
 ( 4, 2, 2, 2, 4 ),
 ( 0.000000000000000000, 0.2500000000000000000, 0.5000000000000000000, 0.7500000000000000000, 1.000000000000000000 ),
 .UNSPECIFIED. ) ;
#57005 = CARTESIAN_POINT ( 'NONE',  ( 10.91441078832384726, 5.114410788323845658, -6.482042798726318722 ) ) ;
#57006 = CARTESIAN_POINT ( 'NONE',  ( 11.30000000000000071, 0.000000000000000000, 0.000000000000000000 ) ) ;
#57007 = CARTESIAN_POINT ( 'NONE',  ( 10.97601622864088178, -5.224113188238077576, 6.768286317869557145 ) ) ;
#57008 = CARTESIAN_POINT ( 'NONE',  ( 7.613904305967312602, 4.827151911712800114, 5.947730341079782157 ) ) ;
#57009 = EDGE_LOOP ( 'NONE', ( #6823, #7591, #37306, #51421, #28616 ) ) ;
#57010 = CARTESIAN_POINT ( 'NONE',  ( 18.20564091649233163, -2.840274733304995358, 13.70886432971491331 ) ) ;
#57011 = DIRECTION ( 'NONE',  ( 0.4384236320213996119, -0.6355252626312996034, -0.6355252626312996034 ) ) ;
#57012 = ORIENTED_EDGE ( 'NONE', *, *, #15309, .F. ) ;
#57013 = ORIENTED_EDGE ( 'NONE', *, *, #26350, .T. ) ;
#57014 = CARTESIAN_POINT ( 'NONE',  ( 23.58888331804951122, 13.25334641141371073, 4.277494313177894192 ) ) ;
#57015 = CARTESIAN_POINT ( 'NONE',  ( 9.396013540183334456, 3.000416447002273834, 6.731816600031358178 ) ) ;
#57016 = EDGE_CURVE ( 'NONE', #62147, #8401, #64445, .T. ) ;
#57017 = CONICAL_SURFACE ( 'NONE', #14594, 13.22499948080999843, 0.7853981240402999608 ) ;
#57018 = CARTESIAN_POINT ( 'NONE',  ( 11.81056516821459823, 4.609678151793300316, 6.884701936848800052 ) ) ;
#57019 = CARTESIAN_POINT ( 'NONE',  ( 10.06344080699000010, 5.156228702401000952, 6.125219923432000613 ) ) ;
#57020 = CARTESIAN_POINT ( 'NONE',  ( 7.204907196771999978, -0.2999999999999999889, -3.099954730132999714 ) ) ;
#57021 = CARTESIAN_POINT ( 'NONE',  ( 8.922950365671626471, -3.319061674888539315, -6.950586433956124743 ) ) ;
#57022 = CARTESIAN_POINT ( 'NONE',  ( 9.757667269575000191, -4.489271889653999814, 5.986031004145000445 ) ) ;
#57023 = CARTESIAN_POINT ( 'NONE',  ( 18.27543972223746493, -0.08185661189467333121, -12.59973963693671983 ) ) ;
#57024 = CARTESIAN_POINT ( 'NONE',  ( 10.13061232742999884, -2.189322372303999842, -7.101642112140999608 ) ) ;
#57025 = CARTESIAN_POINT ( 'NONE',  ( 10.60441638348510018, -4.841589649988700117, -7.294998899090099798 ) ) ;
#57026 = CARTESIAN_POINT ( 'NONE',  ( 8.239948341229000661, 2.735218126362000124, 6.771983639047999937 ) ) ;
#57027 = ORIENTED_EDGE ( 'NONE', *, *, #57767, .T. ) ;
#57028 = CARTESIAN_POINT ( 'NONE',  ( 9.502376473208929752, -4.922128563344212004, 6.792422036439461408 ) ) ;
#57029 = SURFACE_STYLE_FILL_AREA ( #46202 ) ;
#57030 = CARTESIAN_POINT ( 'NONE',  ( 5.200000000000000178, 0.2500000000000000000, -3.149999999999999911 ) ) ;
#57031 = CARTESIAN_POINT ( 'NONE',  ( 10.28976354018291239, -4.327184855449096368, -6.282534154164603812 ) ) ;
#57032 = CARTESIAN_POINT ( 'NONE',  ( 17.77886761546797345, 1.796012712130039324, 12.47134082573985658 ) ) ;
#57033 = CARTESIAN_POINT ( 'NONE',  ( 12.08002314427566759, 2.496413253464124793, 13.77564875264238253 ) ) ;
#57034 = FACE_OUTER_BOUND ( 'NONE', #41786, .T. ) ;
#57035 = ORIENTED_EDGE ( 'NONE', *, *, #7398, .T. ) ;
#57036 = CARTESIAN_POINT ( 'NONE',  ( 12.33488707444048949, 0.4118223548554933444, -12.69101228721791763 ) ) ;
#57037 = CARTESIAN_POINT ( 'NONE',  ( 12.09634358953520206, -0.1544074001203955548, 13.99915345895492180 ) ) ;
#57038 = ORIENTED_EDGE ( 'NONE', *, *, #62426, .F. ) ;
#57039 = CARTESIAN_POINT ( 'NONE',  ( 12.80505043854143388, 3.199698446519374517, 12.18695736643652694 ) ) ;
#57040 = CARTESIAN_POINT ( 'NONE',  ( 24.52301464528887465, -3.339127113045694095, 12.06936612931750297 ) ) ;
#57041 = CARTESIAN_POINT ( 'NONE',  ( 15.61911349846455899, 9.449623925638377386, 8.220739594287655549 ) ) ;
#57042 = CARTESIAN_POINT ( 'NONE',  ( 10.95672469555900008, -3.566534988568399900, 8.249937779480299938 ) ) ;
#57043 = CARTESIAN_POINT ( 'NONE',  ( 8.755358248830999557, 4.089987329977850194, 6.649720865199900466 ) ) ;
#57044 = EDGE_CURVE ( 'NONE', #23400, #1871, #58035, .T. ) ;
#57045 = EDGE_CURVE ( 'NONE', #24788, #67585, #36362, .T. ) ;
#57046 = CARTESIAN_POINT ( 'NONE',  ( 25.50740514701198336, 11.18379543759817984, -3.138198361856242347 ) ) ;
#57047 = CARTESIAN_POINT ( 'NONE',  ( 9.099999952505998024, -4.749999993641800700, 7.500000000000000000 ) ) ;
#57048 = DIRECTION ( 'NONE',  ( 1.000000000000000000, 0.000000000000000000, 0.000000000000000000 ) ) ;
#57049 = CARTESIAN_POINT ( 'NONE',  ( 9.751909913808001207, -4.316974633926000671, -5.653758079558000027 ) ) ;
#57050 = EDGE_CURVE ( 'NONE', #20897, #44819, #13828, .T. ) ;
#57051 = VECTOR ( 'NONE', #25585, 1000.000000000000000 ) ;
#57052 = CARTESIAN_POINT ( 'NONE',  ( 11.73256516821459883, 4.706297556651700020, -8.212808089543500500 ) ) ;
#57053 = CARTESIAN_POINT ( 'NONE',  ( 11.09999999999999964, 4.000000000000000000, 7.500000000000000000 ) ) ;
#57054 = CARTESIAN_POINT ( 'NONE',  ( 11.27745123989519982, 4.410212499603100689, -8.292221125039500151 ) ) ;
#57055 = CARTESIAN_POINT ( 'NONE',  ( 8.646822372493998543, 3.711294259598199918, -8.444453017408701356 ) ) ;
#57057 = CARTESIAN_POINT ( 'NONE',  ( 9.255786719645998417, -4.065290607273509771, 6.597079156813799194 ) ) ;
#57056 = LINE ( 'NONE', #35738, #54215 ) ;
#57058 = CARTESIAN_POINT ( 'NONE',  ( 23.58414895174732351, -13.37550325405040397, 4.077674481848631238 ) ) ;
#57059 = VERTEX_POINT ( 'NONE', #31629 ) ;
#57060 = VECTOR ( 'NONE', #23759, 1000.000000000000000 ) ;
#57061 = CARTESIAN_POINT ( 'NONE',  ( 10.48791429142999831, 4.016993441347180394, 8.391963954669400039 ) ) ;
#57062 = CARTESIAN_POINT ( 'NONE',  ( 9.269471092183000138, 5.100000000000000533, -6.152188490330000370 ) ) ;
#57063 = CARTESIAN_POINT ( 'NONE',  ( 9.728988259786000015, 3.886559292927400211, 6.640442468193600511 ) ) ;
#57064 = CARTESIAN_POINT ( 'NONE',  ( 11.09999999999999964, 2.646159083949000124, 6.745271721726000536 ) ) ;
#57065 = AXIS2_PLACEMENT_3D ( 'NONE', #3048, #24380, #7959 ) ;
#57066 = CARTESIAN_POINT ( 'NONE',  ( 23.56666365135700403, 12.07812737763999955, -3.551569042617998662 ) ) ;
#57067 = FACE_OUTER_BOUND ( 'NONE', #59046, .T. ) ;
#57068 = DIRECTION ( 'NONE',  ( -1.000000000000000000, 0.000000000000000000, 0.000000000000000000 ) ) ;
#57069 = ORIENTED_EDGE ( 'NONE', *, *, #64655, .T. ) ;
#57070 = CARTESIAN_POINT ( 'NONE',  ( 9.782608878791998919, -4.289688213680199702, -6.254020414961999563 ) ) ;
#57071 = CARTESIAN_POINT ( 'NONE',  ( 10.65520300221153782, -5.038713246137302981, -5.049010194981326194 ) ) ;
#57072 = CARTESIAN_POINT ( 'NONE',  ( 10.94999293566599974, -3.279967330949900450, 6.616719557880299085 ) ) ;
#57073 = CARTESIAN_POINT ( 'NONE',  ( 18.28026264019197811, 2.471821293434738553, -12.35517058147370584 ) ) ;
#57074 = CARTESIAN_POINT ( 'NONE',  ( 8.385191233021004109, -3.508000636384001947, -6.669203184159004039 ) ) ;
#57075 = CARTESIAN_POINT ( 'NONE',  ( 4.700001368028300597, 0.000000000000000000, 0.000000000000000000 ) ) ;
#57076 = CONICAL_SURFACE ( 'NONE', #40363, 2.624999810206000372, 0.7853980665166908626 ) ;
#57077 = CARTESIAN_POINT ( 'NONE',  ( 12.18408897593520201, 2.571470745536066804, -13.65804488217700552 ) ) ;
#57078 = CARTESIAN_POINT ( 'NONE',  ( 11.13107481686000177, -2.674997213776999949, -5.007806838190000498 ) ) ;
#57079 = CARTESIAN_POINT ( 'NONE',  ( 10.79702055961999818, -5.792859009854000263, -7.049265738992000152 ) ) ;
#57080 = CARTESIAN_POINT ( 'NONE',  ( 23.56665676678199972, 13.31363904818000066, -4.296982115204999175 ) ) ;
#57081 = CARTESIAN_POINT ( 'NONE',  ( 12.42222097287479343, 0.6205713442106896016, -13.98624562867392385 ) ) ;
#57082 = CARTESIAN_POINT ( 'NONE',  ( 7.399999923048000028, 0.000000000000000000, 0.000000000000000000 ) ) ;
#57083 = CARTESIAN_POINT ( 'NONE',  ( 11.58810207955109917, 3.203462856645999945, 7.825000000000000178 ) ) ;
#57084 = CARTESIAN_POINT ( 'NONE',  ( 18.18005043835058743, 2.498838836751009040, 12.45183430367551303 ) ) ;
#57085 = CARTESIAN_POINT ( 'NONE',  ( 9.518314158773000244, 4.845406482350000488, -6.387189183984999907 ) ) ;
#57086 = DIRECTION ( 'NONE',  ( 0.000000000000000000, 0.9905022095861402143, -0.1374968101629056305 ) ) ;
#57087 = ORIENTED_EDGE ( 'NONE', *, *, #353, .T. ) ;
#57088 = CARTESIAN_POINT ( 'NONE',  ( 9.229626678759569103, -4.176630817665263784, -8.850101115164489940 ) ) ;
#57089 = CARTESIAN_POINT ( 'NONE',  ( 18.28005242394217689, 2.496404808517244334, -13.77565028140658931 ) ) ;
#57090 = ORIENTED_EDGE ( 'NONE', *, *, #60693, .T. ) ;
#57091 = CARTESIAN_POINT ( 'NONE',  ( 10.38996314287999922, -3.151633609938700342, 7.678836273503299559 ) ) ;
#57092 = CARTESIAN_POINT ( 'NONE',  ( 2.655140132544082654, 0.9161175952574702741, 3.408904368339106927 ) ) ;
#57093 = ADVANCED_FACE ( 'NONE', ( #63769 ), #47681, .T. ) ;
#57094 = CARTESIAN_POINT ( 'NONE',  ( 18.43276988671242123, 2.975106096549898549, -11.26378872114027274 ) ) ;
#57095 = CARTESIAN_POINT ( 'NONE',  ( 13.55370778485685435, 9.344737785247383854, 8.032732227356667920 ) ) ;
#57096 = CARTESIAN_POINT ( 'NONE',  ( 11.39700581613019992, -3.130347327833300053, -8.058426314824099990 ) ) ;
#57097 = CARTESIAN_POINT ( 'NONE',  ( 11.59999999999999964, -3.409519984105200852, -6.540686298265701915 ) ) ;
#57098 = EDGE_CURVE ( 'NONE', #19018, #65197, #1868, .T. ) ;
#57099 = CARTESIAN_POINT ( 'NONE',  ( 5.002943173016664247, -1.199500263597274241, 0.9218200799623669228 ) ) ;
#57100 = ORIENTED_EDGE ( 'NONE', *, *, #21053, .F. ) ;
#57101 = LINE ( 'NONE', #20045, #56629 ) ;
#57102 = CARTESIAN_POINT ( 'NONE',  ( 9.526695280414001488, 5.462898983065000102, -8.055936939571999744 ) ) ;
#57103 = ORIENTED_EDGE ( 'NONE', *, *, #4519, .F. ) ;
#57104 = CARTESIAN_POINT ( 'NONE',  ( 10.56271176071999918, 2.509373760909999973, -8.602415192333999983 ) ) ;
#57105 = FILL_AREA_STYLE ('',( #19711 ) ) ;
#57106 = ORIENTED_EDGE ( 'NONE', *, *, #45145, .F. ) ;
#57107 = CARTESIAN_POINT ( 'NONE',  ( 8.923430433046998900, 3.028322657068899915, 8.099647887697699389 ) ) ;
#57108 = CARTESIAN_POINT ( 'NONE',  ( 17.69826591161636031, -1.891282299241872522, -12.57273691359005596 ) ) ;
#57109 = CARTESIAN_POINT ( 'NONE',  ( 12.10000669845703847, 11.02846243759400124, -3.754394857303852362 ) ) ;
#57110 = AXIS2_PLACEMENT_3D ( 'NONE', #36140, #30553, #7858 ) ;
#57111 = CARTESIAN_POINT ( 'NONE',  ( 5.699999999877000789, -1.433333330872999856, 10.65401593578999950 ) ) ;
#57112 = CARTESIAN_POINT ( 'NONE',  ( 8.579778437876671049, 2.946186682499075005, 6.246120330076514016 ) ) ;
#57113 = EDGE_LOOP ( 'NONE', ( #63405, #5133, #592, #19359, #20867, #28340 ) ) ;
#57114 = CARTESIAN_POINT ( 'NONE',  ( 7.000000000000000000, -7.526486366024999874, -3.526486366024999874 ) ) ;
#57115 = CARTESIAN_POINT ( 'NONE',  ( 10.06949528041000086, 4.910370880657999315, -8.649591080567999413 ) ) ;
#57116 = CARTESIAN_POINT ( 'NONE',  ( 8.101999744244276158, -3.171054102886327719, 8.579047487217421164 ) ) ;
#57117 = CARTESIAN_POINT ( 'NONE',  ( 8.942941355974879158, 3.045333477771414721, 8.051224688103602034 ) ) ;
#57118 = CARTESIAN_POINT ( 'NONE',  ( 18.28005834358922499, -0.01140630886273579121, 14.00000041621361291 ) ) ;
#57119 = CARTESIAN_POINT ( 'NONE',  ( 18.23176382712000176, 2.916721637292999603, 11.52766586543999949 ) ) ;
#57120 = VECTOR ( 'NONE', #9980, 1000.000000000000000 ) ;
#57121 = CARTESIAN_POINT ( 'NONE',  ( 17.72043029666332004, -1.875000000000000444, 12.57545629021522871 ) ) ;
#57123 = EDGE_CURVE ( 'NONE', #1716, #23725, #25314, .T. ) ;
#57122 = B_SPLINE_CURVE_WITH_KNOTS ( 'NONE', 3,
 ( #60678, #12792, #28532, #65570 ),
 .UNSPECIFIED., .F., .F.,
 ( 4, 4 ),
 ( 0.000000000000000000, 0.3058235430633697294 ),
 .UNSPECIFIED. ) ;
#57124 = VERTEX_POINT ( 'NONE', #43144 ) ;
#57125 = VERTEX_POINT ( 'NONE', #840 ) ;
#57126 = CARTESIAN_POINT ( 'NONE',  ( 9.418385841233000377, 3.251172436837000301, -6.320036569851000152 ) ) ;
#57127 = CARTESIAN_POINT ( 'NONE',  ( 9.165599386908368729, 5.579491228604561037, 6.755435461345757453 ) ) ;
#57128 = EDGE_CURVE ( 'NONE', #1282, #5900, #48732, .T. ) ;
#57129 = EDGE_CURVE ( 'NONE', #49363, #61047, #52065, .T. ) ;
#57130 = CARTESIAN_POINT ( 'NONE',  ( 8.191498616105999275, -3.399962740672999750, 6.146646623957999545 ) ) ;
#57131 = CARTESIAN_POINT ( 'NONE',  ( 24.63399677426199830, 8.686855860201999846, -8.588054097598998737 ) ) ;
#57132 = CARTESIAN_POINT ( 'NONE',  ( 24.23232877498800164, 9.064816052010000291, -9.162332550022000532 ) ) ;
#57133 = CARTESIAN_POINT ( 'NONE',  ( 18.26087891924500184, -2.716433685251999908, -11.57325030293000090 ) ) ;
#57135 = DIRECTION ( 'NONE',  ( 1.000000000000000000, 0.000000000000000000, 0.000000000000000000 ) ) ;
#57134 = CARTESIAN_POINT ( 'NONE',  ( 10.63827973160999818, -3.897539901865500145, 8.637205511891998810 ) ) ;
#57136 = CARTESIAN_POINT ( 'NONE',  ( 12.09610237318921655, -4.810409949404850671, 7.825049231485562196 ) ) ;
#57137 = VERTEX_POINT ( 'NONE', #22155 ) ;
#57138 = CARTESIAN_POINT ( 'NONE',  ( 16.00000000448733672, -11.41071763184507759, 4.623975355603788806 ) ) ;
#57139 = CARTESIAN_POINT ( 'NONE',  ( 11.09999999999999964, -6.593648102827000201, 5.598803487171999826 ) ) ;
#57140 = CARTESIAN_POINT ( 'NONE',  ( 9.927742433789001453, -5.651611919872999934, -7.935921913274999184 ) ) ;
#57141 = CARTESIAN_POINT ( 'NONE',  ( 7.954463414819048950, 4.941043969738770691, 6.420455451648299672 ) ) ;
#57142 = DIRECTION ( 'NONE',  ( -1.000000000000000000, 0.000000000000000000, 0.000000000000000000 ) ) ;
#57143 = CARTESIAN_POINT ( 'NONE',  ( 6.949999692120000461, -11.00717859340000082, 1.432487142323000118 ) ) ;
#57144 = CARTESIAN_POINT ( 'NONE',  ( 9.143660841233000269, 2.235961884443999459, -6.794506518623999902 ) ) ;
#57145 = ADVANCED_FACE ( 'NONE', ( #26731 ), #47711, .T. ) ;
#57146 = DIRECTION ( 'NONE',  ( 0.7071067811865474617, -0.7071067811865474617, 5.048524301881336257E-09 ) ) ;
#57147 = CARTESIAN_POINT ( 'NONE',  ( 8.079287380335998137, -4.920039154826996608, 6.237958006931995314 ) ) ;
#57148 = AXIS2_PLACEMENT_3D ( 'NONE', #51164, #8508, #13759 ) ;
#57149 = B_SPLINE_CURVE_WITH_KNOTS ( 'NONE', 3,
 ( #14602, #9684, #36611, #25084, #46417, #62820 ),
 .UNSPECIFIED., .F., .F.,
 ( 4, 2, 4 ),
 ( 0.000000000000000000, 0.5000000000000000000, 1.000000000000000000 ),
 .UNSPECIFIED. ) ;
#57150 = LINE ( 'NONE', #5038, #23325 ) ;
#57151 = CARTESIAN_POINT ( 'NONE',  ( 25.00272134720554007, -3.413729871556085982, 11.76143154378893030 ) ) ;
#57152 = CARTESIAN_POINT ( 'NONE',  ( 2.681109875139000120, 0.2761326424212999786, -3.247312329306000223 ) ) ;
#57153 = VERTEX_POINT ( 'NONE', #59218 ) ;
#57154 = CARTESIAN_POINT ( 'NONE',  ( 12.42881362571445614, -0.4990964484179726823, -12.68679736436867778 ) ) ;
#57155 = CARTESIAN_POINT ( 'NONE',  ( 12.19170508189248991, -2.620143503840312249, -12.42276098599978340 ) ) ;
#57156 = CARTESIAN_POINT ( 'NONE',  ( 11.08380555355736163, 3.999999927305438963, -9.033895164528459532 ) ) ;
#57157 = CARTESIAN_POINT ( 'NONE',  ( 7.250690656965701031, -4.000034976101444428, 9.109408410636810061 ) ) ;
#57158 = VERTEX_POINT ( 'NONE', #21135 ) ;
#57159 = CARTESIAN_POINT ( 'NONE',  ( 9.637068864299580540, -2.899999999999999911, 6.444141223381762096 ) ) ;
#57160 = APPLICATION_PROTOCOL_DEFINITION ( 'draft international standard', 'automotive_design', 1998, #17253 ) ;
#57161 = CARTESIAN_POINT ( 'NONE',  ( 0.7407984155085870492, -3.500070825090493276, 0.4600197968347137789 ) ) ;
#57162 = DIRECTION ( 'NONE',  ( 0.000000000000000000, 0.000000000000000000, -1.000000000000000000 ) ) ;
#57163 = CARTESIAN_POINT ( 'NONE',  ( 1.511390132540624931, 3.499999999999998224, 0.4581489286485194157 ) ) ;
#57165 = VECTOR ( 'NONE', #6648, 1000.000000000000114 ) ;
#57164 = CARTESIAN_POINT ( 'NONE',  ( 11.67403632436368888, 3.023821283238099955, -7.272033745815799755 ) ) ;
#57166 = ORIENTED_EDGE ( 'NONE', *, *, #69042, .F. ) ;
#57167 = CARTESIAN_POINT ( 'NONE',  ( 9.646285452541999206, -2.591464128784999765, 6.760053199270999791 ) ) ;
#57168 = ORIENTED_EDGE ( 'NONE', *, *, #24618, .T. ) ;
#57169 = CARTESIAN_POINT ( 'NONE',  ( 10.90000000000000036, -8.618205959414002137, 7.308661029293999967 ) ) ;
#57170 = CARTESIAN_POINT ( 'NONE',  ( 9.459504440379001622, -5.445226602819000838, 7.703375344019999460 ) ) ;
#57171 = CIRCLE ( 'NONE', #27039, 3.499999999999999556 ) ;
#57172 = CARTESIAN_POINT ( 'NONE',  ( 17.81056431323685985, -0.6834693007276704257, -13.98330741474946137 ) ) ;
#57173 = ORIENTED_EDGE ( 'NONE', *, *, #45626, .F. ) ;
#57174 = CARTESIAN_POINT ( 'NONE',  ( 8.280100731544914439, 3.296994443394544394, -6.103692026910207069 ) ) ;
#57175 = CARTESIAN_POINT ( 'NONE',  ( 7.577233589035318850, 3.528879827026006222, 8.787968233516592065 ) ) ;
#57176 = CARTESIAN_POINT ( 'NONE',  ( 7.333029719588999740, 3.500992739020000410, -8.983283880004998778 ) ) ;
#57177 = EDGE_CURVE ( 'NONE', #26585, #64554, #6253, .T. ) ;
#57178 = CARTESIAN_POINT ( 'NONE',  ( 16.39999997735699822, -3.306214596137841966, -11.23948664129755493 ) ) ;
#57179 = CARTESIAN_POINT ( 'NONE',  ( 18.05168367659330642, -2.879595443346424588, 12.35500515152848955 ) ) ;
#57180 = VERTEX_POINT ( 'NONE', #52598 ) ;
#57181 = CARTESIAN_POINT ( 'NONE',  ( 2.167640132540333386, -1.762666431298160141, 3.058252359239895579 ) ) ;
#57182 = CARTESIAN_POINT ( 'NONE',  ( 12.19240574124822807, -2.623658933770948387, -13.64640170901807714 ) ) ;
#57183 = CARTESIAN_POINT ( 'NONE',  ( 5.365443173017625966, 1.500000000000000000, 0.1963495408493652339 ) ) ;
#57184 = VERTEX_POINT ( 'NONE', #53970 ) ;
#57185 = LINE ( 'NONE', #67664, #44187 ) ;
#57186 = CARTESIAN_POINT ( 'NONE',  ( 4.599999999999999645, -0.6250000000000001110, -13.88107975066922428 ) ) ;
#57187 = ORIENTED_EDGE ( 'NONE', *, *, #54921, .T. ) ;
#57188 = CARTESIAN_POINT ( 'NONE',  ( 23.99446517519106692, 12.72130897981146802, -3.481316059523209105 ) ) ;
#57189 = CARTESIAN_POINT ( 'NONE',  ( 11.79999999713068703, -12.23671679745269181, -1.944304699248228685 ) ) ;
#57190 = CYLINDRICAL_SURFACE ( 'NONE', #18555, 3.500000000000000000 ) ;
#57191 = CARTESIAN_POINT ( 'NONE',  ( 7.871384613761001070, -5.129340912189999990, 6.740051747100999968 ) ) ;
#57192 = CARTESIAN_POINT ( 'NONE',  ( 12.21299871467824971, -0.2005085131878081850, -13.89805835524348865 ) ) ;
#57193 = CARTESIAN_POINT ( 'NONE',  ( 17.81575242098906742, -1.931873426913545355, 12.56596755615858818 ) ) ;
#57194 = ORIENTED_EDGE ( 'NONE', *, *, #36861, .T. ) ;
#57195 = CARTESIAN_POINT ( 'NONE',  ( 3.452384183491000069, 1.140396268832999827, -3.309002319436000317 ) ) ;
#57196 = ORIENTED_EDGE ( 'NONE', *, *, #24272, .T. ) ;
#57197 = CARTESIAN_POINT ( 'NONE',  ( 11.27765994926999937, 3.273804980682999854, 6.368305648407000419 ) ) ;
#57198 = DIRECTION ( 'NONE',  ( 0.000000000000000000, 0.000000000000000000, -1.000000000000000000 ) ) ;
#57199 = CARTESIAN_POINT ( 'NONE',  ( 8.739954719592999410, 3.122811675949999977, -6.006064052396999919 ) ) ;
#57200 = CARTESIAN_POINT ( 'NONE',  ( 2.887168028787000296, 2.953261164984000153, -1.958616092671000120 ) ) ;
#57201 = CARTESIAN_POINT ( 'NONE',  ( 16.39999999231800132, -3.216285993016000155, -11.40340220863999932 ) ) ;
#57202 = CARTESIAN_POINT ( 'NONE',  ( 9.234814475091134511, -3.943962993865710587, 6.616514917701350029 ) ) ;
#57203 = CARTESIAN_POINT ( 'NONE',  ( 9.038695689765509300, -4.943520148687432503, 8.465362812019415983 ) ) ;
#57204 = ORIENTED_EDGE ( 'NONE', *, *, #57207, .F. ) ;
#57205 = CARTESIAN_POINT ( 'NONE',  ( 11.09610807141099897, -3.947296672195129918, 6.360477084256999980 ) ) ;
#57206 = CARTESIAN_POINT ( 'NONE',  ( 3.050973465878000113, 3.500000000000000000, 0.000000000000000000 ) ) ;
#57207 = EDGE_CURVE ( 'NONE', #59568, #16464, #42460, .T. ) ;
#57208 = CARTESIAN_POINT ( 'NONE',  ( 15.39284288850700122, 9.264553731144999915, 8.207894312349999666 ) ) ;
#57209 = DIRECTION ( 'NONE',  ( -1.000000000000000000, 0.000000000000000000, 0.000000000000000000 ) ) ;
#57211 = CARTESIAN_POINT ( 'NONE',  ( 11.09999999999999964, 5.350000000000000533, 7.500000000000000000 ) ) ;
#57210 = CARTESIAN_POINT ( 'NONE',  ( 11.05639637898999972, 5.030226177531999632, 6.028288223959999748 ) ) ;
#57212 = VECTOR ( 'NONE', #10296, 1000.000000000000000 ) ;
#57213 = CARTESIAN_POINT ( 'NONE',  ( 11.62994988689359843, 4.518136976474400157, -8.516279404258998653 ) ) ;
#57214 = DIRECTION ( 'NONE',  ( 1.000000000000000000, 0.000000000000000000, 0.000000000000000000 ) ) ;
#57215 = CARTESIAN_POINT ( 'NONE',  ( 10.11093802597399893, 3.477805217445600228, -6.642005297568199573 ) ) ;
#57216 = CARTESIAN_POINT ( 'NONE',  ( 18.20808481425076408, 0.3124912280145324961, 12.59612551846059958 ) ) ;
#57217 = CARTESIAN_POINT ( 'NONE',  ( 9.136976429976712666, -5.100000000000000533, 6.167827406373843857 ) ) ;
#57218 = DIRECTION ( 'NONE',  ( 1.000000000000000000, 0.000000000000000000, 0.000000000000000000 ) ) ;
#57219 = CARTESIAN_POINT ( 'NONE',  ( 9.261230081853240037, -3.478588282862478120, 6.718925885376237694 ) ) ;
#57220 = ORIENTED_EDGE ( 'NONE', *, *, #22912, .T. ) ;
#57221 = CARTESIAN_POINT ( 'NONE',  ( 8.192495559623999668, -2.550228841911000188, 7.666975032000999946 ) ) ;
#57222 = CARTESIAN_POINT ( 'NONE',  ( 18.30000000000000071, -14.70300865175000027, 5.744762642578000289 ) ) ;
#57223 = ADVANCED_FACE ( 'NONE', ( #53292 ), #5394, .T. ) ;
#57224 = CARTESIAN_POINT ( 'NONE',  ( 17.10000000000000142, -3.283787102340999464, -11.28049554847999936 ) ) ;
#57225 = VERTEX_POINT ( 'NONE', #42803 ) ;
#57226 = B_SPLINE_CURVE_WITH_KNOTS ( 'NONE', 3,
 ( #18424, #61067, #13185, #56162 ),
 .UNSPECIFIED., .F., .F.,
 ( 4, 4 ),
 ( 0.8746679733675616353, 1.000000000000000000 ),
 .UNSPECIFIED. ) ;
#57227 = EDGE_CURVE ( 'NONE', #14358, #22158, #21810, .T. ) ;
#57228 = CARTESIAN_POINT ( 'NONE',  ( 18.16350100824700320, 3.138009765975000143, 11.88148072165000002 ) ) ;
#57229 = CARTESIAN_POINT ( 'NONE',  ( 10.47769598648999967, 5.009476315410999803, 6.898940957443399746 ) ) ;
#57230 = CARTESIAN_POINT ( 'NONE',  ( 10.75102028041000146, 2.478469530773999896, -7.438303846328000013 ) ) ;
#57231 = ORIENTED_EDGE ( 'NONE', *, *, #52985, .F. ) ;
#57232 = CARTESIAN_POINT ( 'NONE',  ( 12.99999999998900080, 12.39025855408000076, 1.832244667012999928 ) ) ;
#57233 = CARTESIAN_POINT ( 'NONE',  ( 9.819055905797000605, 2.899999999999999911, -6.571291218949999902 ) ) ;
#57234 = CARTESIAN_POINT ( 'NONE',  ( 10.49349279008999858, 3.667611644732699627, 6.265968249244999733 ) ) ;
#57235 = CARTESIAN_POINT ( 'NONE',  ( 24.54223752889060961, 8.848832083880790123, -9.279389145428778463 ) ) ;
#57236 = CARTESIAN_POINT ( 'NONE',  ( 15.40000000005200143, 9.187454762873001002, 8.213177997099000649 ) ) ;
#57237 = ORIENTED_EDGE ( 'NONE', *, *, #9080, .F. ) ;
#57238 = CARTESIAN_POINT ( 'NONE',  ( 7.847822007142403855, -5.059730379935329481, 6.600780866611749786 ) ) ;
#57239 = CARTESIAN_POINT ( 'NONE',  ( 7.716064158767000691, 4.574593532473000046, -5.689090339675999530 ) ) ;
#57240 = CARTESIAN_POINT ( 'NONE',  ( 8.286427776887917318, -4.793419134848132757, 9.047669286253999132 ) ) ;
#57241 = CARTESIAN_POINT ( 'NONE',  ( 10.30793802597399988, -4.665064168510499876, 8.592736948783000983 ) ) ;
#57242 = EDGE_LOOP ( 'NONE', ( #59438, #13230, #3687, #17993 ) ) ;
#57244 = CARTESIAN_POINT ( 'NONE',  ( 10.94668920802000045, -5.066629281208999913, -5.177964064427999169 ) ) ;
#57243 = AXIS2_PLACEMENT_3D ( 'NONE', #388, #49662, #1771 ) ;
#57245 = DIRECTION ( 'NONE',  ( 1.000000000000000000, 0.000000000000000000, 0.000000000000000000 ) ) ;
#57246 = ORIENTED_EDGE ( 'NONE', *, *, #14691, .T. ) ;
#57247 = CARTESIAN_POINT ( 'NONE',  ( 12.80505043854144276, 0.6249999999999994449, -25.00000000000000000 ) ) ;
#57248 = VERTEX_POINT ( 'NONE', #12717 ) ;
#57249 = DIRECTION ( 'NONE',  ( 0.000000000000000000, 1.000000000000000000, 0.000000000000000000 ) ) ;
#57250 = CARTESIAN_POINT ( 'NONE',  ( 5.699999999554000496, -0.3000000004460000036, 9.662944681662999358 ) ) ;
#57251 = CARTESIAN_POINT ( 'NONE',  ( 10.73213259636989925, 3.092475607087700418, -7.994504989494399361 ) ) ;
#57252 = EDGE_CURVE ( 'NONE', #23757, #67334, #11937, .T. ) ;
#57253 = CARTESIAN_POINT ( 'NONE',  ( 11.26346886766499900, -4.634677072395899877, 8.653146038559000885 ) ) ;
#57254 = CARTESIAN_POINT ( 'NONE',  ( 12.24870215512120275, 2.784965704346237025, -12.38061966815949866 ) ) ;
#57255 = CARTESIAN_POINT ( 'NONE',  ( 11.34226088462130022, -3.997572771977982775, 8.640738455926999961 ) ) ;
#57256 = CARTESIAN_POINT ( 'NONE',  ( 10.90480513896000048, -3.220259576336399920, 7.933462475324499330 ) ) ;
#57257 = EDGE_LOOP ( 'NONE', ( #54762, #50837, #47032, #52298, #58205 ) ) ;
#57258 = CARTESIAN_POINT ( 'NONE',  ( 9.364763540183330903, 2.782534154164605589, -7.827184855449096368 ) ) ;
#57259 = MECHANICAL_DESIGN_GEOMETRIC_PRESENTATION_REPRESENTATION (  '', ( #62845 ), #23788 ) ;
#57260 = CARTESIAN_POINT ( 'NONE',  ( 11.47657389914466464, -4.648774973711785385, -8.595592487855949315 ) ) ;
#57261 = CARTESIAN_POINT ( 'NONE',  ( 9.854346873516623972, 2.749999999999999112, 7.336375382625534236 ) ) ;
#57262 = ORIENTED_EDGE ( 'NONE', *, *, #48840, .F. ) ;
#57263 = CARTESIAN_POINT ( 'NONE',  ( 12.34719455185581261, -2.925915912524184925, -12.34207449233261755 ) ) ;
#57264 = CARTESIAN_POINT ( 'NONE',  ( 10.13662282008599824, 4.594711216567399781, 6.540749699823199315 ) ) ;
#57265 = CARTESIAN_POINT ( 'NONE',  ( 10.18308064679000147, -2.953580299898999950, -8.606287508253000595 ) ) ;
#57266 = CARTESIAN_POINT ( 'NONE',  ( 10.59031493128999912, 7.471983947861001063, -5.946923603349002718 ) ) ;
#57267 = CARTESIAN_POINT ( 'NONE',  ( 18.30830001818700126, -3.300182612895000478, -12.02694835946000040 ) ) ;
#57268 = CARTESIAN_POINT ( 'NONE',  ( 9.323602683899247623, 2.780955253993290022, -7.180752970636812726 ) ) ;
#57269 = CARTESIAN_POINT ( 'NONE',  ( 12.26189125119393175, -2.190632771808445511, -13.73417700668423436 ) ) ;
#57270 = CARTESIAN_POINT ( 'NONE',  ( 11.51102763632551884, -4.911148285670300595, -7.079572058049399708 ) ) ;
#57271 = FACE_OUTER_BOUND ( 'NONE', #41843, .T. ) ;
#57272 = DIRECTION ( 'NONE',  ( 1.000000000000000000, 0.000000000000000000, 0.000000000000000000 ) ) ;
#57273 = EDGE_LOOP ( 'NONE', ( #769, #64396, #19543, #57632 ) ) ;
#57274 = ORIENTED_EDGE ( 'NONE', *, *, #21522, .T. ) ;
#57275 = CARTESIAN_POINT ( 'NONE',  ( 12.80505043854143388, 3.125000000000000000, 13.52078605991414939 ) ) ;
#57276 =( NAMED_UNIT ( * ) SI_UNIT ( $, .STERADIAN. ) SOLID_ANGLE_UNIT ( ) );
#57277 = FACE_BOUND ( 'NONE', #18551, .T. ) ;
#57278 = CARTESIAN_POINT ( 'NONE',  ( 17.98396147896337638, 2.954720660945521438, 13.56638041066990574 ) ) ;
#57279 = CARTESIAN_POINT ( 'NONE',  ( 10.90421423234000109, 3.863780721621000058, -9.185084890147001246 ) ) ;
#57280 = CARTESIAN_POINT ( 'NONE',  ( 10.62435795695566476, -2.750000000000000000, 7.192559817601734906 ) ) ;
#57281 = CARTESIAN_POINT ( 'NONE',  ( 18.14016391943232520, 2.719929439268204074, 12.39760446975600594 ) ) ;
#57282 = CARTESIAN_POINT ( 'NONE',  ( 23.61813716858800305, -13.16714277698999958, 4.271540868536000346 ) ) ;
#57283 = CARTESIAN_POINT ( 'NONE',  ( 10.31167969999000000, 2.874476822401000220, 8.900029516786000627 ) ) ;
#57284 = CARTESIAN_POINT ( 'NONE',  ( 1.985247277619000217, 2.372532593102000043, -2.573147701680999599 ) ) ;
#57285 = EDGE_CURVE ( 'NONE', #57358, #28975, #14568, .T. ) ;
#57286 = VERTEX_POINT ( 'NONE', #23199 ) ;
#57287 = CARTESIAN_POINT ( 'NONE',  ( 12.37974467178321625, -2.958002365504007969, 12.33299351980446268 ) ) ;
#57288 = EDGE_CURVE ( 'NONE', #40006, #28416, #44882, .T. ) ;
#57289 = CARTESIAN_POINT ( 'NONE',  ( 13.99999999231800096, 8.833253877201999060, 7.896562762484000686 ) ) ;
#57290 = CONICAL_SURFACE ( 'NONE', #9278, 11.19999999998000106, 0.7853981633972997312 ) ;
#57291 = CARTESIAN_POINT ( 'NONE',  ( 9.925639158771000226, 4.357364160690000432, -9.282962013144999247 ) ) ;
#57292 = CARTESIAN_POINT ( 'NONE',  ( 11.26857802013510046, -5.174568897094999897, 7.527343341769989316 ) ) ;
#57293 = CARTESIAN_POINT ( 'NONE',  ( 8.639360841228999277, 5.074768364528000397, -8.296267706722000312 ) ) ;
#57294 = EDGE_CURVE ( 'NONE', #33561, #66341, #68782, .T. ) ;
#57295 = CONICAL_SURFACE ( 'NONE', #5940, 12.42510776559999996, 0.7854022111938739892 ) ;
#57296 = CARTESIAN_POINT ( 'NONE',  ( 0.1499996298882999846, 0.000000000000000000, 0.000000000000000000 ) ) ;
#57297 = CARTESIAN_POINT ( 'NONE',  ( 25.19214487158300031, 8.466223133107002141, 8.226644165488000482 ) ) ;
#57298 = CARTESIAN_POINT ( 'NONE',  ( 12.34869027095183824, 0.4275228316712915144, 12.69032453495386292 ) ) ;
#57299 = CARTESIAN_POINT ( 'NONE',  ( 25.44994642811700203, 1.048050535245999973E-13, -6.616929226765999876E-14 ) ) ;
#57300 = CARTESIAN_POINT ( 'NONE',  ( 10.74609776273999984, 4.263105564403999459, 9.276980853981999786 ) ) ;
#57301 = CARTESIAN_POINT ( 'NONE',  ( 13.99999999485600277, 9.471999751521998689, 8.194948195317001804 ) ) ;
#57302 = VERTEX_POINT ( 'NONE', #60953 ) ;
#57303 = CARTESIAN_POINT ( 'NONE',  ( 9.476970280414001024, 5.511689883260999956, -7.095113581311000672 ) ) ;
#57304 = CARTESIAN_POINT ( 'NONE',  ( 0.000000000000000000, 2.899969545326000375, 0.3804588500739426449 ) ) ;
#57305 = DIRECTION ( 'NONE',  ( -1.000000000000000000, 0.000000000000000000, 0.000000000000000000 ) ) ;
#57306 = CARTESIAN_POINT ( 'NONE',  ( 10.26059687351566652, 3.370476274536378547, 8.592232985442823434 ) ) ;
#57307 = EDGE_CURVE ( 'NONE', #23533, #61768, #39285, .T. ) ;
#57308 = CARTESIAN_POINT ( 'NONE',  ( 10.22934687351566474, 3.836375382625535124, -6.249999999999999112 ) ) ;
#57309 = CARTESIAN_POINT ( 'NONE',  ( 10.40333997687999990, -3.786145554879500441, -6.519583185858300212 ) ) ;
#57310 = ORIENTED_EDGE ( 'NONE', *, *, #63680, .F. ) ;
#57311 = CIRCLE ( 'NONE', #37203, 14.00000000000000000 ) ;
#57312 = CARTESIAN_POINT ( 'NONE',  ( 1.582018817588999982, 2.814509306356999918, 2.491368026013999870 ) ) ;
#57313 = EDGE_CURVE ( 'NONE', #39911, #33013, #32887, .T. ) ;
#57314 = CARTESIAN_POINT ( 'NONE',  ( 10.21194365307746743, -5.865446360225381461, 7.794835729825335235 ) ) ;
#57315 = AXIS2_PLACEMENT_3D ( 'NONE', #33390, #38627, #7156 ) ;
#57317 = CARTESIAN_POINT ( 'NONE',  ( 13.73854985688900143, -9.171197327466000360, -8.173482659384999849 ) ) ;
#57316 = CARTESIAN_POINT ( 'NONE',  ( 9.070789158774999805, 5.349936549139000519, -7.138437102151999447 ) ) ;
#57318 = CARTESIAN_POINT ( 'NONE',  ( 7.716851002542999716, -2.832432432432000269, 6.822293592207000934 ) ) ;
#57319 = CARTESIAN_POINT ( 'NONE',  ( 12.79999998712400178, -11.53033693765999779, 4.891431908114999949 ) ) ;
#57320 = CARTESIAN_POINT ( 'NONE',  ( 17.94528078231818924, -2.988314720655957490, -13.55762497744564499 ) ) ;
#57321 = CARTESIAN_POINT ( 'NONE',  ( 11.56441235500451015, 3.361299021099800388, 8.085115074060599483 ) ) ;
#57322 = DIRECTION ( 'NONE',  ( -1.000000000000000000, 0.000000000000000000, -1.233561263588000078E-14 ) ) ;
#57323 = CARTESIAN_POINT ( 'NONE',  ( 7.758191940376999440, -5.797088532631000213, 8.340479314546998424 ) ) ;
#57324 = ORIENTED_EDGE ( 'NONE', *, *, #54353, .T. ) ;
#57325 = CARTESIAN_POINT ( 'NONE',  ( 8.160739158772001289, 5.944584532500000407, 7.106843289410999631 ) ) ;
#57327 = CARTESIAN_POINT ( 'NONE',  ( 10.57314899745999881, -5.167567567567999731, -6.822293592207000934 ) ) ;
#57326 = CARTESIAN_POINT ( 'NONE',  ( 5.671449988747999882, -0.9919734638370999447, -1.274097314648999779 ) ) ;
#57328 = CARTESIAN_POINT ( 'NONE',  ( 7.623314959413727721, -5.001887204095511130, 6.074294720979810158 ) ) ;
#57329 = DIRECTION ( 'NONE',  ( 0.000000000000000000, -0.1218274111675001214, 0.9925512993736016476 ) ) ;
#57330 = CARTESIAN_POINT ( 'NONE',  ( 1.366565493715000024, -3.591455136169999562, 0.07279325410826999188 ) ) ;
#57331 = ORIENTED_EDGE ( 'NONE', *, *, #2992, .T. ) ;
#57332 = CARTESIAN_POINT ( 'NONE',  ( 0.7431103717477000048, 2.848815883361000001, -1.248255999701999963 ) ) ;
#57333 = CARTESIAN_POINT ( 'NONE',  ( 11.76487482311540056, -3.069598554678400149, 7.124095752359899336 ) ) ;
#57334 = CARTESIAN_POINT ( 'NONE',  ( 11.47822875044625945, 4.169680329100683203, 8.360317195474184615 ) ) ;
#57335 = CARTESIAN_POINT ( 'NONE',  ( 10.31457848836000046, 5.362142879234999882, 6.677781064327999339 ) ) ;
#57336 = CARTESIAN_POINT ( 'NONE',  ( 10.86687616594229944, 3.655053560864600204, 8.587337146608000182 ) ) ;
#57337 = CARTESIAN_POINT ( 'NONE',  ( 24.22565377178775137, -3.306156338801836458, 12.33873653827660455 ) ) ;
#57338 = CARTESIAN_POINT ( 'NONE',  ( 17.79999999998900151, 3.595165934733000057, -11.99793354950999991 ) ) ;
#57339 = CARTESIAN_POINT ( 'NONE',  ( 12.33003632436370012, -5.243255406354000669, 7.790336465152099876 ) ) ;
#57340 = CARTESIAN_POINT ( 'NONE',  ( 8.361173146690900282, 2.869241151408781221, -6.758878718175449052 ) ) ;
#57341 = FACE_OUTER_BOUND ( 'NONE', #47314, .T. ) ;
#57342 = CARTESIAN_POINT ( 'NONE',  ( 11.09999999999999964, 2.899999999999999911, -4.467422426380999845 ) ) ;
#57343 = VERTEX_POINT ( 'NONE', #33003 ) ;
#57344 = CARTESIAN_POINT ( 'NONE',  ( 15.49019623963660308, -9.469115506160978413, -8.198265202209942260 ) ) ;
#57345 = CARTESIAN_POINT ( 'NONE',  ( 13.25828219467850388, -12.15323025559006531, -2.051492516881108230 ) ) ;
#57346 = ORIENTED_EDGE ( 'NONE', *, *, #37310, .T. ) ;
#57347 = CARTESIAN_POINT ( 'NONE',  ( 8.427696207745832169, 3.798469702271707771, 6.010277740195467899 ) ) ;
#57348 = CARTESIAN_POINT ( 'NONE',  ( 10.80133863405319872, 4.534404523786000674, 6.818303296693398963 ) ) ;
#57349 = EDGE_CURVE ( 'NONE', #68545, #67326, #46542, .T. ) ;
#57350 = CARTESIAN_POINT ( 'NONE',  ( 10.31167969999000000, 2.874476822401000220, 8.900029516786000627 ) ) ;
#57351 = CARTESIAN_POINT ( 'NONE',  ( 9.792312867577999569, 4.284154069364999984, -9.000485152170000447 ) ) ;
#57352 = CARTESIAN_POINT ( 'NONE',  ( 9.606837339593626623, -4.864872534707646246, -7.367607524272325570 ) ) ;
#57353 = CARTESIAN_POINT ( 'NONE',  ( 10.07101719722999889, -4.042170815906999337, 8.920201479886998186 ) ) ;
#57354 = CARTESIAN_POINT ( 'NONE',  ( 18.27048529734874549, -0.1170514037749927627, -12.59946170170351465 ) ) ;
#57355 = CARTESIAN_POINT ( 'NONE',  ( 12.39978108233925269, 2.975905172412623756, -12.32787332408411984 ) ) ;
#57356 = CARTESIAN_POINT ( 'NONE',  ( 10.99826088462129903, -3.998156935320088756, -6.633804182961699603 ) ) ;
#57357 = CARTESIAN_POINT ( 'NONE',  ( 8.404999999999999361, 5.190914425723000214, -8.768195054477999406 ) ) ;
#57358 = VERTEX_POINT ( 'NONE', #18650 ) ;
#57359 = AXIS2_PLACEMENT_3D ( 'NONE', #66697, #61460, #57577 ) ;
#57360 = PLANE ( 'NONE',  #26989 ) ;
#57361 = SHAPE_REPRESENTATION_RELATIONSHIP ( 'NONE' , 'NONE' ,  #60729, #18558 ) ;
#57362 = CARTESIAN_POINT ( 'NONE',  ( 10.99249554220161684, 5.864913444040075419, -4.994565819417503327 ) ) ;
#57363 = CARTESIAN_POINT ( 'NONE',  ( 24.66807826201277010, -3.571100427736410676, -12.15100773339871232 ) ) ;
#57364 = CARTESIAN_POINT ( 'NONE',  ( 10.15434687351570631, -2.749999999999998668, -7.336375382625537789 ) ) ;
#57365 = AXIS2_PLACEMENT_3D ( 'NONE', #13630, #67768, #34955 ) ;
#57366 = CARTESIAN_POINT ( 'NONE',  ( 17.84632148815558139, 1.821395309707476429, 12.46765979085770937 ) ) ;
#57367 = CARTESIAN_POINT ( 'NONE',  ( 12.43989325004533164, 3.148871498663009305, 13.64128470488402378 ) ) ;
#57368 = CARTESIAN_POINT ( 'NONE',  ( 9.520803773887999810, -3.270557529354000348, 5.711489293131999823 ) ) ;
#57369 = ORIENTED_EDGE ( 'NONE', *, *, #12560, .T. ) ;
#57370 = CARTESIAN_POINT ( 'NONE',  ( 12.64261153907313506, -0.6049396497490575619, -12.68060203380715834 ) ) ;
#57371 = CARTESIAN_POINT ( 'NONE',  ( 12.35439258730998446, -0.5721320424853859610, 13.98830666644471954 ) ) ;
#57372 = EDGE_CURVE ( 'NONE', #4626, #40201, #15433, .T. ) ;
#57373 = VERTEX_POINT ( 'NONE', #23543 ) ;
#57374 = CARTESIAN_POINT ( 'NONE',  ( 12.21279934347913176, -2.064970636307561502, 12.42964156345203541 ) ) ;
#57375 = EDGE_CURVE ( 'NONE', #26545, #53432, #43185, .T. ) ;
#57376 = CARTESIAN_POINT ( 'NONE',  ( 7.906851002540999929, 2.832432432432000269, -6.822293592207000934 ) ) ;
#57377 = CARTESIAN_POINT ( 'NONE',  ( 10.64601354018249779, -3.000416447002271170, -6.731816600031360842 ) ) ;
#57378 = CARTESIAN_POINT ( 'NONE',  ( 12.01518179236249040, -4.180996681294200101, 8.347076615013298451 ) ) ;
#57379 = ADVANCED_FACE ( 'NONE', ( #17620 ), #39984, .F. ) ;
#57380 = DIRECTION ( 'NONE',  ( 0.000000000000000000, -1.000000000000000000, 0.000000000000000000 ) ) ;
#57381 = DIRECTION ( 'NONE',  ( -0.8987684456439055669, 0.000000000000000000, -0.4384236320214022764 ) ) ;
#57382 = CARTESIAN_POINT ( 'NONE',  ( 8.101999744244302804, 3.171054102886417869, 8.579047487216984180 ) ) ;
#57383 = CARTESIAN_POINT ( 'NONE',  ( 12.15399652902987171, 2.797872959086249445, 12.28545279959702796 ) ) ;
#57384 = B_SPLINE_CURVE_WITH_KNOTS ( 'NONE', 3,
 ( #54595, #55292, #2155, #7387 ),
 .UNSPECIFIED., .F., .F.,
 ( 4, 4 ),
 ( 0.000000000000000000, 1.000000000000000000 ),
 .UNSPECIFIED. ) ;
#57385 = CARTESIAN_POINT ( 'NONE',  ( 11.09999999999999964, 2.700688487044999864, -5.124965750789000296 ) ) ;
#57386 = CARTESIAN_POINT ( 'NONE',  ( 10.74795391537419853, 4.830118059977199785, -8.063786182297898009 ) ) ;
#57387 = CARTESIAN_POINT ( 'NONE',  ( 10.03976415876999972, 2.255572964181999929, -8.111983882175000105 ) ) ;
#57388 = CARTESIAN_POINT ( 'NONE',  ( 9.124051052051999733, 5.255397705012999410, -7.745684736446600382 ) ) ;
#57390 = CARTESIAN_POINT ( 'NONE',  ( 9.227215710425999973, -4.373963964882100264, 6.691239224408199071 ) ) ;
#57389 = CARTESIAN_POINT ( 'NONE',  ( 15.36427412810700055, -8.819457004710999470, -7.692809699200999773 ) ) ;
#57391 = CARTESIAN_POINT ( 'NONE',  ( 17.10000000000000142, 3.470217030164000072, 11.92928724693999953 ) ) ;
#57392 = ORIENTED_EDGE ( 'NONE', *, *, #64083, .F. ) ;
#57393 = AXIS2_PLACEMENT_3D ( 'NONE', #68914, #10878, #58092 ) ;
#57394 = DIRECTION ( 'NONE',  ( 0.000000000000000000, 0.9916377111174248249, -0.1290528957048031888 ) ) ;
#57395 = EDGE_CURVE ( 'NONE', #52670, #19784, #64565, .T. ) ;
#57396 = CARTESIAN_POINT ( 'NONE',  ( 3.500000000000000000, -1.789730407083999886, 2.652709005895000249 ) ) ;
#57397 = CARTESIAN_POINT ( 'NONE',  ( 9.530220962691416275, 2.706107893675387288, -8.716938213633312671 ) ) ;
#57398 = CARTESIAN_POINT ( 'NONE',  ( 9.351063610504999346, 4.411988005505000032, 6.583971515917899531 ) ) ;
#57399 = CARTESIAN_POINT ( 'NONE',  ( 9.176241837494625742, 3.342362352854908458, -8.077100505959180055 ) ) ;
#57400 = DIRECTION ( 'NONE',  ( 1.000000000000000000, 0.000000000000000000, 0.000000000000000000 ) ) ;
#57401 = CARTESIAN_POINT ( 'NONE',  ( 12.58320380180961884, -3.084393765090618356, 13.53199207997351117 ) ) ;
#57402 = CARTESIAN_POINT ( 'NONE',  ( 12.21849864558328136, 2.283168037611178036, 13.71702792529043258 ) ) ;
#57403 = CARTESIAN_POINT ( 'NONE',  ( 23.62942910622400206, 3.420921953095000134, -13.57770915236000064 ) ) ;
#57404 = ORIENTED_EDGE ( 'NONE', *, *, #17210, .T. ) ;
#57405 = CARTESIAN_POINT ( 'NONE',  ( 4.387482791987999953, -0.7931398200715998881, -0.8110703280130999726 ) ) ;
#57406 = CIRCLE ( 'NONE', #44058, 9.250000000000000000 ) ;
#57407 = CARTESIAN_POINT ( 'NONE',  ( 9.048063610504998522, -3.475294527116599586, -8.666648427848999248 ) ) ;
#57408 = CARTESIAN_POINT ( 'NONE',  ( 8.826226023015690814, 5.100000000000000533, -6.272440530347759946 ) ) ;
#57409 = CARTESIAN_POINT ( 'NONE',  ( 11.93856039236529831, -2.967715280237000375, 7.449760924956519759 ) ) ;
#57410 = B_SPLINE_CURVE_WITH_KNOTS ( 'NONE', 3,
 ( #41437, #62744, #14864, #53642, #26740, #27420, #42810, #58536, #21143, #38245, #37904, #69030, #42469, #5403, #22165, #63777, #59572, #16579 ),
 .UNSPECIFIED., .F., .F.,
 ( 4, 2, 2, 2, 2, 2, 2, 2, 4 ),
 ( 0.000000000000000000, 0.1250000000000000000, 0.2500000000000000000, 0.3750000000000000000, 0.5000000000000000000, 0.6250000000000000000, 0.7500000000000000000, 0.8750000000000000000, 1.000000000000000000 ),
 .UNSPECIFIED. ) ;
#57411 = CARTESIAN_POINT ( 'NONE',  ( 17.67525416028801644, 1.770698066894638156, -12.47496018400917173 ) ) ;
#57412 = CARTESIAN_POINT ( 'NONE',  ( 8.914818027809994661, -3.440065392353999663, -6.172246220506001357 ) ) ;
#57413 = VECTOR ( 'NONE', #27089, 1000.000000000000114 ) ;
#57414 = CARTESIAN_POINT ( 'NONE',  ( 18.06413707770591515, 2.862722769414956847, 12.35962335206644802 ) ) ;
#57415 = FACE_OUTER_BOUND ( 'NONE', #33104, .T. ) ;
#57416 = DIRECTION ( 'NONE',  ( -1.000000000000000000, 0.000000000000000000, 0.000000000000000000 ) ) ;
#57417 = CARTESIAN_POINT ( 'NONE',  ( 10.53198305961999992, -2.323723769066000422, -8.279488812962998878 ) ) ;
#57418 = CARTESIAN_POINT ( 'NONE',  ( 23.73953442324672025, 3.508702049063129547, -13.37373019756607739 ) ) ;
#57419 = FACE_OUTER_BOUND ( 'NONE', #28866, .T. ) ;
#57420 = CARTESIAN_POINT ( 'NONE',  ( 6.899999691988000450, 13.87069231928999891, -4.225386915259999654 ) ) ;
#57421 = DIRECTION ( 'NONE',  ( 0.000000000000000000, 0.7071067811865475727, 0.7071067811865475727 ) ) ;
#57422 = CARTESIAN_POINT ( 'NONE',  ( 18.10184514648642207, 2.186078922847817019, 12.51950284167777383 ) ) ;
#57423 = CARTESIAN_POINT ( 'NONE',  ( 9.061929719594999710, 4.092867382745001059, -5.937785237406000505 ) ) ;
#57424 = CARTESIAN_POINT ( 'NONE',  ( 12.18748876160954886, -4.600381688599499697, 6.875627981711399883 ) ) ;
#57425 = VERTEX_POINT ( 'NONE', #14780 ) ;
#57426 = CARTESIAN_POINT ( 'NONE',  ( 17.97988082628305762, 1.926206752467414463, -13.86685907515736638 ) ) ;
#57427 = ORIENTED_EDGE ( 'NONE', *, *, #14802, .T. ) ;
#57428 = CARTESIAN_POINT ( 'NONE',  ( 10.11134252387499899, -4.857027829858100887, 7.631191628371899682 ) ) ;
#57429 = CARTESIAN_POINT ( 'NONE',  ( 11.51145123989532948, 4.605239108938600445, 6.331134574721999364 ) ) ;
#57430 = CARTESIAN_POINT ( 'NONE',  ( 4.149992563292000725, -1.747525841223982912, -1.007210908820215023 ) ) ;
#57431 = EDGE_CURVE ( 'NONE', #25079, #24359, #56047, .T. ) ;
#57432 = CARTESIAN_POINT ( 'NONE',  ( 8.496516550600020423, -5.350579948490476134, 7.852800305270212000 ) ) ;
#57433 = EDGE_CURVE ( 'NONE', #59370, #56214, #19731, .T. ) ;
#57434 = CARTESIAN_POINT ( 'NONE',  ( 10.86190547754509872, -3.108323067758099967, -7.528299448264639260 ) ) ;
#57435 = CARTESIAN_POINT ( 'NONE',  ( 11.09999999999999964, 0.5000000000000000000, -5.124965750789000296 ) ) ;
#57436 = CARTESIAN_POINT ( 'NONE',  ( 11.53926573483131968, -12.16827677290229737, -1.947218182817292975 ) ) ;
#57437 = ORIENTED_EDGE ( 'NONE', *, *, #22270, .T. ) ;
#57438 = CARTESIAN_POINT ( 'NONE',  ( 13.67057712374000289, 9.352787036275000077, 8.106596622149000453 ) ) ;
#57439 = CARTESIAN_POINT ( 'NONE',  ( 9.974220280410998285, 5.496789211521000418, -7.043125396300999874 ) ) ;
#57440 = ORIENTED_EDGE ( 'NONE', *, *, #60927, .T. ) ;
#57441 = VECTOR ( 'NONE', #24495, 1000.000000000000000 ) ;
#57442 = CARTESIAN_POINT ( 'NONE',  ( 11.08752642792000032, 2.871528932589999972, -6.302908019754999813 ) ) ;
#57443 = ORIENTED_EDGE ( 'NONE', *, *, #48697, .F. ) ;
#57444 = CARTESIAN_POINT ( 'NONE',  ( 8.972076168957999087, 3.350848599899200142, 6.397735581984999698 ) ) ;
#57445 = CARTESIAN_POINT ( 'NONE',  ( 18.06549347002472317, -2.139198186095363940, -12.52833527917196754 ) ) ;
#57446 = CARTESIAN_POINT ( 'NONE',  ( 17.80000000005199823, -3.345268251980999974, 11.86064071431999878 ) ) ;
#57447 = CARTESIAN_POINT ( 'NONE',  ( 4.400031710115373862, -1.251998559788349619, 0.3836858220209141135 ) ) ;
#57448 = CARTESIAN_POINT ( 'NONE',  ( 11.83810207955129989, -3.203462856645999945, 7.174999999999999822 ) ) ;
#57449 = EDGE_LOOP ( 'NONE', ( #61290, #45600, #22201, #61855 ) ) ;
#57450 = CARTESIAN_POINT ( 'NONE',  ( 12.10154284453400209, 11.81398323980999976, -3.695357857504999899 ) ) ;
#57451 = DIRECTION ( 'NONE',  ( 0.000000000000000000, 0.000000000000000000, -1.000000000000000000 ) ) ;
#57452 = CIRCLE ( 'NONE', #63032, 0.5000000000000002220 ) ;
#57453 = LINE ( 'NONE', #46642, #3929 ) ;
#57454 = LINE ( 'NONE', #57806, #48383 ) ;
#57455 = ADVANCED_FACE ( 'NONE', ( #57415 ), #23156, .F. ) ;
#57456 = CARTESIAN_POINT ( 'NONE',  ( 18.27776594916668174, -0.05915529127692874256, 13.99988012777929214 ) ) ;
#57457 = AXIS2_PLACEMENT_3D ( 'NONE', #29870, #51179, #56070 ) ;
#57458 = LINE ( 'NONE', #30227, #55928 ) ;
#57459 = CARTESIAN_POINT ( 'NONE',  ( 10.17310292480999934, -4.709171320598000143, -8.664883863910000983 ) ) ;
#57460 = VERTEX_POINT ( 'NONE', #6256 ) ;
#57461 = ORIENTED_EDGE ( 'NONE', *, *, #4469, .T. ) ;
#57462 = CARTESIAN_POINT ( 'NONE',  ( 8.731095280410999138, 2.469361196073999842, -7.826019481986000059 ) ) ;
#57463 = CARTESIAN_POINT ( 'NONE',  ( 4.999999999844999543, 0.04999999984535999364, 9.776630291645998838 ) ) ;
#57464 = CARTESIAN_POINT ( 'NONE',  ( 1.134306799208000260, 1.762666431298139713, 3.058252359239908458 ) ) ;
#57465 = CARTESIAN_POINT ( 'NONE',  ( 23.60000333944509521, 2.996291596448416694, 13.57008848946830248 ) ) ;
#57466 = CARTESIAN_POINT ( 'NONE',  ( 24.63626978684600033, 8.802569683972000902, -9.348439433646998253 ) ) ;
#57468 = CIRCLE ( 'NONE', #39624, 12.52500000000000036 ) ;
#57467 = CARTESIAN_POINT ( 'NONE',  ( 9.915292290062998504, 4.749786674456300872, -7.064651992867799990 ) ) ;
#57470 = CARTESIAN_POINT ( 'NONE',  ( 7.744301850232000461, 3.130385018321999890, 6.467396599055999395 ) ) ;
#57469 = CARTESIAN_POINT ( 'NONE',  ( 9.574455549952999078, -3.111370763671500228, 8.216988513669100769 ) ) ;
#57471 = CARTESIAN_POINT ( 'NONE',  ( 7.909525359152002721, -3.174976509417001491, 6.234240719816002141 ) ) ;
#57472 = ORIENTED_EDGE ( 'NONE', *, *, #21523, .T. ) ;
#57473 = CARTESIAN_POINT ( 'NONE',  ( 9.841846873515665450, 3.000416447002276943, -6.731816600031354625 ) ) ;
#57474 = EDGE_CURVE ( 'NONE', #3060, #2983, #30911, .T. ) ;
#57475 = CARTESIAN_POINT ( 'NONE',  ( 11.09999999999999964, -5.555182244517999912, 5.124965749841000395 ) ) ;
#57476 = CARTESIAN_POINT ( 'NONE',  ( 10.01364655415099847, 4.619310611972400338, 6.380697202105999999 ) ) ;
#57477 = DIRECTION ( 'NONE',  ( 0.9999999999889699343, 2.769066798711915030E-06, 3.793722030377884974E-06 ) ) ;
#57478 = LINE ( 'NONE', #24303, #38848 ) ;
#57479 = CARTESIAN_POINT ( 'NONE',  ( 10.95304521165000011, -5.154933323944999479, 5.180455670148000458 ) ) ;
#57480 = CARTESIAN_POINT ( 'NONE',  ( 10.12125395348339296, 3.646954034496816099, 8.849054885470943432 ) ) ;
#57481 = CARTESIAN_POINT ( 'NONE',  ( 13.87289819560299975, 8.829573912736998764, 7.542332231507000273 ) ) ;
#57482 = CARTESIAN_POINT ( 'NONE',  ( 16.24418116637980347, -3.625803901490415981, -11.98884806668273306 ) ) ;
#57483 = CARTESIAN_POINT ( 'NONE',  ( 10.99809687351654119, -4.327184855449103473, 6.282534154164607365 ) ) ;
#57484 = B_SPLINE_SURFACE_WITH_KNOTS ( 'NONE', 3, 3, ( 
 ( #51338, #19865, #4456, #30701, #34926, #56926, #35269, #41196, #41875, #51673, #3770, #40842, #56586, #62501, #8689, #56243, #68086, #3095, #8349, #3432, #40498, #61825, #62165, #30036, #29695, #67741, #9357, #14961, #9025, #47127, #50996, #19175, #30365, #35943, #68428 ),
 ( #24768, #36285, #14624, #9708, #25107, #46094, #67401, #52010, #19522, #4113, #46782, #24430, #20202, #45754, #57602, #31054, #14287, #52364, #43607, #42567, #59328, #31739, #48502, #52708, #10743, #42912, #64218, #20896, #5841, #16332, #11429, #32769, #21574, #48849, #37661 ),
 ( #27521, #58992, #21236, #607, #11094, #21918, #15311, #53058, #32428, #36635, #43255, #954, #63875, #26147, #22267, #53405, #53744, #57959, #5503, #10057, #31393, #15989, #36984, #4802, #38002, #64561, #16676, #27179, #10400, #54083, #6180, #26492, #32089, #47472, #68778 ),
 ( #26840, #42233, #63539, #15650, #58295, #5157, #48156, #47822, #259, #69131, #37320, #58640, #43954, #27876, #39744, #44311, #18074, #38702, #22611, #54432, #44656, #17018, #65260, #49186, #1992, #12830, #17374, #38349, #60024, #55822, #12477, #59677, #12134, #60371, #7574 ) ),
 .UNSPECIFIED., .F., .F., .F.,
 ( 4, 4 ),
 ( 4, 1, 1, 1, 1, 1, 1, 1, 1, 1, 1, 1, 1, 1, 1, 1, 1, 1, 1, 1, 1, 1, 1, 1, 1, 1, 1, 1, 1, 1, 1, 1, 4 ),
 ( -0.1039370721279000015, 1.103937072127999963 ),
 ( -0.02000000000000000042, 0.01250000000000000069, 0.04499999999999999833, 0.07749999999999999944, 0.1100000000000000006, 0.1424999999999999878, 0.1749999999999999889, 0.2074999999999999900, 0.2399999999999999911, 0.2725000000000000200, 0.3049999999999999933, 0.3375000000000000222, 0.3699999999999999956, 0.4025000000000000244, 0.4349999999999999978, 0.4675000000000000266, 0.5000000000000000000, 0.5324999999999999734, 0.5649999999999999467, 0.5975000000000000311, 0.6300000000000000044, 0.6624999999999999778, 0.6949999999999999512, 0.7275000000000000355, 0.7600000000000000089, 0.7924999999999999822, 0.8249999999999999556, 0.8575000000000000400, 0.8900000000000000133, 0.9224999999999999867, 0.9549999999999999600, 0.9875000000000000444, 1.020000000000000018 ),
 .UNSPECIFIED. ) ;
#57485 = CARTESIAN_POINT ( 'NONE',  ( 9.174642513462172744, 2.649442673323004538, 7.499981897072118819 ) ) ;
#57486 =( GEOMETRIC_REPRESENTATION_CONTEXT ( 3 ) GLOBAL_UNCERTAINTY_ASSIGNED_CONTEXT ( ( #46497 ) ) GLOBAL_UNIT_ASSIGNED_CONTEXT ( ( #17480, #28314, #50332 ) ) REPRESENTATION_CONTEXT ( 'NONE', 'WORKASPACE' ) );
#57487 = DIRECTION ( 'NONE',  ( -1.000000000000000000, 0.000000000000000000, 0.000000000000000000 ) ) ;
#57488 = CARTESIAN_POINT ( 'NONE',  ( 3.062565470666999801, -3.214256637597999955, -0.5383687126906999687 ) ) ;
#57489 = VERTEX_POINT ( 'NONE', #42036 ) ;
#57490 = CARTESIAN_POINT ( 'NONE',  ( 12.20981273398931499, 0.1908418880314473598, -12.69807545005480875 ) ) ;
#57491 = CARTESIAN_POINT ( 'NONE',  ( 12.72293129229483988, -3.125000000000000444, -12.28373127578713842 ) ) ;
#57492 = CARTESIAN_POINT ( 'NONE',  ( 8.649445371194000032, 5.100000000000000533, -6.459601070175000181 ) ) ;
#57493 = DIRECTION ( 'NONE',  ( 0.7071067811865470176, -0.7011937492001459882, 0.09125418391856598976 ) ) ;
#57494 = CARTESIAN_POINT ( 'NONE',  ( 8.866178911608058044, -2.879880053984696264, -6.717471171832306354 ) ) ;
#57495 = VERTEX_POINT ( 'NONE', #52868 ) ;
#57496 = CYLINDRICAL_SURFACE ( 'NONE', #19888, 0.5000000000000002220 ) ;
#57497 = APPLICATION_PROTOCOL_DEFINITION ( 'draft international standard', 'automotive_design', 1998, #8793 ) ;
#57498 = CARTESIAN_POINT ( 'NONE',  ( 17.94287612696653156, 0.4902485962002651187, 12.68726381691200800 ) ) ;
#57499 = CARTESIAN_POINT ( 'NONE',  ( 13.55192027319500170, -11.56672964510999968, -2.320600286854999972 ) ) ;
#57500 = CARTESIAN_POINT ( 'NONE',  ( 7.798681789217144278, 2.959779466931951486, 6.592102449522434071 ) ) ;
#57501 = CARTESIAN_POINT ( 'NONE',  ( 10.81013259637009938, 2.968328969579000276, -8.062151801142800167 ) ) ;
#57502 = EDGE_LOOP ( 'NONE', ( #65932, #64866, #24677, #61405 ) ) ;
#57503 = CARTESIAN_POINT ( 'NONE',  ( 11.14993998249000029, -2.627133311863999676, 6.696092388640000337 ) ) ;
#57504 = ORIENTED_EDGE ( 'NONE', *, *, #44248, .F. ) ;
#57505 = CARTESIAN_POINT ( 'NONE',  ( 7.559808771084921553, -3.823091902406630549, 8.850087896820790334 ) ) ;
#57506 = CARTESIAN_POINT ( 'NONE',  ( 9.021581853209999835, -2.193670085072000120, 7.400591740205000768 ) ) ;
#57507 = AXIS2_PLACEMENT_3D ( 'NONE', #64149, #17303, #52027 ) ;
#57508 = CARTESIAN_POINT ( 'NONE',  ( 17.74252317112528132, -0.7057854747025560371, -13.98219993205038847 ) ) ;
#57509 = EDGE_CURVE ( 'NONE', #38751, #26914, #58758, .T. ) ;
#57510 = ORIENTED_EDGE ( 'NONE', *, *, #50048, .F. ) ;
#57511 = CARTESIAN_POINT ( 'NONE',  ( 8.449122411348595207, 4.354617778861483934, -9.219396266972353260 ) ) ;
#57512 = EDGE_CURVE ( 'NONE', #40403, #55462, #54554, .T. ) ;
#57513 = CARTESIAN_POINT ( 'NONE',  ( 7.660810569926313818, 2.650836722355680575, 7.733623655995972790 ) ) ;
#57514 = CARTESIAN_POINT ( 'NONE',  ( 8.169495280408000326, 4.466585441010000324, -5.831585202652000532 ) ) ;
#57515 = B_SPLINE_CURVE_WITH_KNOTS ( 'NONE', 3,
 ( #21721, #59132, #21047, #47279, #32573, #21384, #53885, #5987, #15799, #27325, #31892, #52512, #26646, #22065, #57753, #61, #4612, #25946 ),
 .UNSPECIFIED., .F., .F.,
 ( 4, 2, 2, 2, 2, 2, 2, 2, 4 ),
 ( 0.1254138569076999055, 0.2190601518424659111, 0.3127064467772319167, 0.4063527417119979224, 0.4999990366467639280, 0.5936453315815299892, 0.6872916265162959393, 0.7809379214510618894, 0.8745842163858279505 ),
 .UNSPECIFIED. ) ;
#57516 = LINE ( 'NONE', #51930, #6325 ) ;
#57517 = ADVANCED_FACE ( 'NONE', ( #54506 ), #39122, .F. ) ;
#57518 = CARTESIAN_POINT ( 'NONE',  ( 8.156860996257041307, -3.022118299483437021, 6.361385428469135128 ) ) ;
#57519 = VERTEX_POINT ( 'NONE', #44725 ) ;
#57520 = CARTESIAN_POINT ( 'NONE',  ( 9.657547180956999711, -5.333447643521000536, 6.049925825719999928 ) ) ;
#57521 = EDGE_CURVE ( 'NONE', #46365, #6210, #21241, .T. ) ;
#57522 = CARTESIAN_POINT ( 'NONE',  ( 12.18008396645310398, -2.512642877105788930, -13.67072295643538560 ) ) ;
#57523 = CARTESIAN_POINT ( 'NONE',  ( 5.500859839683752028, -0.3926218265389255779, 1.460959015002472494 ) ) ;
#57524 = VERTEX_POINT ( 'NONE', #49954 ) ;
#57525 = CARTESIAN_POINT ( 'NONE',  ( 10.85290698989999925, -3.170384785323999921, -8.782188229854000383 ) ) ;
#57526 = CARTESIAN_POINT ( 'NONE',  ( 8.218755356758000730, 2.895318267055999595, 6.639774629398000449 ) ) ;
#57527 = ORIENTED_EDGE ( 'NONE', *, *, #30618, .T. ) ;
#57528 = CARTESIAN_POINT ( 'NONE',  ( 23.61209254828138171, -10.11819938911013494, 9.629780466774583658 ) ) ;
#57529 = CARTESIAN_POINT ( 'NONE',  ( 23.96071418768165628, 12.77533843076500020, -3.513734256132603928 ) ) ;
#57530 = CARTESIAN_POINT ( 'NONE',  ( 17.57568447735986794, -0.6247443594537128719, -12.67930618256806419 ) ) ;
#57531 = CARTESIAN_POINT ( 'NONE',  ( 5.344609839684291153, 1.500000000000000888, -0.1963495408493590444 ) ) ;
#57532 = CARTESIAN_POINT ( 'NONE',  ( 21.72233714749290101, 0.000000000000000000, 0.000000000000000000 ) ) ;
#57533 = CARTESIAN_POINT ( 'NONE',  ( 3.000973465876999757, 3.500000000000000000, 0.000000000000000000 ) ) ;
#57534 = CARTESIAN_POINT ( 'NONE',  ( 12.58300520725473426, 3.084588251740255860, 13.53188417542246746 ) ) ;
#57535 = CIRCLE ( 'NONE', #67561, 0.9500000000000007327 ) ;
#57536 = CARTESIAN_POINT ( 'NONE',  ( 17.80000000005199823, 3.345268251980999974, -11.86064071431999878 ) ) ;
#57537 = ORIENTED_EDGE ( 'NONE', *, *, #50603, .T. ) ;
#57538 = CARTESIAN_POINT ( 'NONE',  ( 10.69568717260499824, -4.466067913030199676, -8.260703168378098482 ) ) ;
#57539 = EDGE_LOOP ( 'NONE', ( #32490, #41620, #64211, #68255 ) ) ;
#57540 = CARTESIAN_POINT ( 'NONE',  ( 10.46085995768999943, 5.403395036974999677, 7.721808039505000387 ) ) ;
#57541 = EDGE_CURVE ( 'NONE', #23725, #49775, #21961, .T. ) ;
#57542 = CARTESIAN_POINT ( 'NONE',  ( 5.700000000000000178, 0.000000000000000000, 0.000000000000000000 ) ) ;
#57543 = CARTESIAN_POINT ( 'NONE',  ( 12.26168426244253240, 2.190490593926006646, -13.73426451135290449 ) ) ;
#57544 = CARTESIAN_POINT ( 'NONE',  ( 3.012918919220000102, 1.930662435474000072, 2.971610853962999954 ) ) ;
#57545 = B_SPLINE_CURVE_WITH_KNOTS ( 'NONE', 3,
 ( #11471, #59033, #11136, #42278 ),
 .UNSPECIFIED., .F., .F.,
 ( 4, 4 ),
 ( 0.000000000000000000, 1.000000000000000000 ),
 .UNSPECIFIED. ) ;
#57546 = B_SPLINE_CURVE_WITH_KNOTS ( 'NONE', 3,
 ( #39966, #61283, #13399, #50795 ),
 .UNSPECIFIED., .F., .F.,
 ( 4, 4 ),
 ( 0.000000000000000000, 1.000000000000000000 ),
 .UNSPECIFIED. ) ;
#57547 = CARTESIAN_POINT ( 'NONE',  ( 5.700000000000000178, 0.000000000000000000, 0.000000000000000000 ) ) ;
#57548 = CARTESIAN_POINT ( 'NONE',  ( 8.073148997456000231, 5.167567567567999731, -6.822293592207000934 ) ) ;
#57549 = CARTESIAN_POINT ( 'NONE',  ( 18.04535492090956694, 0.3877560770473448826, 13.89272419024897154 ) ) ;
#57550 = VERTEX_POINT ( 'NONE', #61137 ) ;
#57551 = CARTESIAN_POINT ( 'NONE',  ( 11.60887482311539998, -2.815046254222000055, 7.021250586468399391 ) ) ;
#57552 = CARTESIAN_POINT ( 'NONE',  ( 10.26947109217999810, 5.100000000000000533, -6.152188490330000370 ) ) ;
#57553 = CARTESIAN_POINT ( 'NONE',  ( 4.599999999999999645, 0.000000000000000000, 0.000000000000000000 ) ) ;
#57554 = DIRECTION ( 'NONE',  ( 0.000000000000000000, 0.000000000000000000, -1.000000000000000000 ) ) ;
#57556 = CARTESIAN_POINT ( 'NONE',  ( 4.500000125099000492, 3.641531520771000148E-13, 3.197442310919999608E-14 ) ) ;
#57555 = CARTESIAN_POINT ( 'NONE',  ( 10.93727498060999892, 5.425427353909999972, 7.240585962396000497 ) ) ;
#57557 = CARTESIAN_POINT ( 'NONE',  ( 11.30995122972050027, 4.452766304612699955, -6.452959986593999275 ) ) ;
#57558 = VECTOR ( 'NONE', #47350, 1000.000000000000114 ) ;
#57559 = CARTESIAN_POINT ( 'NONE',  ( 25.52466960993000100, -11.20857090970999970, 3.138534493961999683 ) ) ;
#57560 = CIRCLE ( 'NONE', #27430, 0.9999999999999996669 ) ;
#57561 = EDGE_CURVE ( 'NONE', #40252, #27371, #18641, .T. ) ;
#57562 = CARTESIAN_POINT ( 'NONE',  ( 9.349051052051999378, 4.850870049477099322, -7.666517576877299511 ) ) ;
#57563 = CARTESIAN_POINT ( 'NONE',  ( 17.55505043854144631, 0.7192913403693016461, 12.57945229203838444 ) ) ;
#57564 = CARTESIAN_POINT ( 'NONE',  ( 7.060865949841000244, 0.9925148835426000904, 0.7974449476027000161 ) ) ;
#57565 = CARTESIAN_POINT ( 'NONE',  ( 24.37816252494532421, -8.911180844771308784, 9.054574243701839720 ) ) ;
#57566 = ADVANCED_FACE ( 'NONE', ( #55895 ), #38460, .F. ) ;
#57567 = CARTESIAN_POINT ( 'NONE',  ( 24.96659818554506316, -2.078227411456102125, -11.31065740026955702 ) ) ;
#57568 = ORIENTED_EDGE ( 'NONE', *, *, #13690, .F. ) ;
#57569 = CARTESIAN_POINT ( 'NONE',  ( 7.058516392956000196, -4.314043295739000250, 8.819145559946001356 ) ) ;
#57570 = CARTESIAN_POINT ( 'NONE',  ( 17.87779404330688138, 3.171907921506167849, 13.63594617280360310 ) ) ;
#57571 = DIRECTION ( 'NONE',  ( 0.000000000000000000, 1.000000000000000000, 0.000000000000000000 ) ) ;
#57572 = ORIENTED_EDGE ( 'NONE', *, *, #32710, .F. ) ;
#57573 = CARTESIAN_POINT ( 'NONE',  ( 9.310863317747999801, -3.039136629551499880, 7.499999999926881600 ) ) ;
#57574 = CARTESIAN_POINT ( 'NONE',  ( 10.88813259637009878, 2.844182332072999753, 6.870201387206400057 ) ) ;
#57575 = CARTESIAN_POINT ( 'NONE',  ( 10.22094528040999961, 2.563078870232999851, -8.004103956955001209 ) ) ;
#57576 = ORIENTED_EDGE ( 'NONE', *, *, #46541, .T. ) ;
#57577 = DIRECTION ( 'NONE',  ( 0.000000000000000000, 1.000000000000000000, 0.000000000000000000 ) ) ;
#57578 = CARTESIAN_POINT ( 'NONE',  ( 8.599999952505998024, 4.749999993641800700, -7.500000000000000000 ) ) ;
#57579 = CARTESIAN_POINT ( 'NONE',  ( 10.96118313518939935, 3.207251432249800249, 6.497569908212999401 ) ) ;
#57580 = CARTESIAN_POINT ( 'NONE',  ( 24.60000000000000142, 0.000000000000000000, 5.000000000000000000 ) ) ;
#57581 = CARTESIAN_POINT ( 'NONE',  ( 8.913573341230998537, 2.550580605805000012, 8.854682662413999594 ) ) ;
#57582 = ORIENTED_EDGE ( 'NONE', *, *, #23124, .T. ) ;
#57583 = FACE_OUTER_BOUND ( 'NONE', #19515, .T. ) ;
#57584 = FACE_OUTER_BOUND ( 'NONE', #31072, .T. ) ;
#57585 = CARTESIAN_POINT ( 'NONE',  ( 8.128369806614207604, -5.084382722290230916, 6.139741310093872251 ) ) ;
#57586 = CARTESIAN_POINT ( 'NONE',  ( 9.550076168958000267, -4.579425901182000658, 6.516130052788599691 ) ) ;
#57587 = ORIENTED_EDGE ( 'NONE', *, *, #22606, .F. ) ;
#57588 = CARTESIAN_POINT ( 'NONE',  ( 10.33538764829999934, -4.566957278416999166, -4.713742776521000266 ) ) ;
#57589 = DIRECTION ( 'NONE',  ( 0.000000000000000000, 1.000000000000000000, 0.000000000000000000 ) ) ;
#57590 = VERTEX_POINT ( 'NONE', #34230 ) ;
#57591 = CARTESIAN_POINT ( 'NONE',  ( 8.786046699800500903, 4.845411057630703233, 7.038404655459764570 ) ) ;
#57592 = LINE ( 'NONE', #60876, #10008 ) ;
#57593 = VECTOR ( 'NONE', #45633, 1000.000000000000114 ) ;
#57594 = ORIENTED_EDGE ( 'NONE', *, *, #35059, .F. ) ;
#57595 = CARTESIAN_POINT ( 'NONE',  ( 9.416972128128000108, -4.783349162191000481, -6.231236652334000148 ) ) ;
#57596 = CARTESIAN_POINT ( 'NONE',  ( 2.384306799209666927, -1.762666431298145930, -3.058252359239904905 ) ) ;
#57597 = CARTESIAN_POINT ( 'NONE',  ( 11.60477869730532774, 3.532552483170099844, -6.578238193496799724 ) ) ;
#57598 = CARTESIAN_POINT ( 'NONE',  ( 11.96989666366029859, -4.058428102321880004, 6.185029684353999357 ) ) ;
#57599 = CARTESIAN_POINT ( 'NONE',  ( 8.624846738991013950, -5.035341376712734629, 6.089196183450023447 ) ) ;
#57600 = EDGE_CURVE ( 'NONE', #46623, #34343, #57897, .T. ) ;
#57601 = CARTESIAN_POINT ( 'NONE',  ( 10.70226357027499908, -2.879914860223000250, 7.283900408233900059 ) ) ;
#57602 = CARTESIAN_POINT ( 'NONE',  ( 8.052732780410000402, 4.968147183437999992, 5.971792472497999604 ) ) ;
#57603 = EDGE_CURVE ( 'NONE', #4640, #68416, #3085, .T. ) ;
#57604 = EDGE_LOOP ( 'NONE', ( #43775, #15550, #42121, #56355, #45217, #18602, #45596, #2644, #3863, #29850, #4114, #13763 ) ) ;
#57605 = CARTESIAN_POINT ( 'NONE',  ( 3.500000000000000000, -3.129623072336949807, -0.6860468956751279990 ) ) ;
#57606 = VECTOR ( 'NONE', #51817, 999.9999999999998863 ) ;
#57607 = CARTESIAN_POINT ( 'NONE',  ( 9.059370559623998176, -4.192917962110999319, 5.525484568403999930 ) ) ;
#57608 = CARTESIAN_POINT ( 'NONE',  ( 25.55279089809471671, -8.264493593867687338, -8.081392981407944376 ) ) ;
#57609 = ORIENTED_EDGE ( 'NONE', *, *, #57826, .F. ) ;
#57610 = CARTESIAN_POINT ( 'NONE',  ( 12.58288255545466683, -3.084271795211693590, -12.29604036100132625 ) ) ;
#57611 = VECTOR ( 'NONE', #25378, 1000.000000000000000 ) ;
#57612 = CARTESIAN_POINT ( 'NONE',  ( 10.75101814679000078, -2.478465696309000155, -7.438303690845000204 ) ) ;
#57613 = CARTESIAN_POINT ( 'NONE',  ( 18.50005573548403248, 2.729642361726667854, 11.32578974454715137 ) ) ;
#57614 = CARTESIAN_POINT ( 'NONE',  ( 18.38069952315600020, -3.381269036354999979, -12.09968217836000015 ) ) ;
#57615 = DIRECTION ( 'NONE',  ( 0.7071064022000087546, 0.6140603781994079524, 0.3506143007542043555 ) ) ;
#57616 = CARTESIAN_POINT ( 'NONE',  ( 12.29504137777690609, -2.138585174375769782, -13.74345269122309254 ) ) ;
#57617 = CARTESIAN_POINT ( 'NONE',  ( 11.77359063708300013, -3.044227915785300276, -7.768721787835699999 ) ) ;
#57618 = CARTESIAN_POINT ( 'NONE',  ( 13.69997185827400088, -10.10519270881757059, -5.872265061164112510 ) ) ;
#57619 = CYLINDRICAL_SURFACE ( 'NONE', #16590, 1.350000000000000533 ) ;
#57620 = ORIENTED_EDGE ( 'NONE', *, *, #25669, .T. ) ;
#57621 = ORIENTED_EDGE ( 'NONE', *, *, #21874, .F. ) ;
#57622 = DIRECTION ( 'NONE',  ( 1.000000000000000000, 0.000000000000000000, 0.000000000000000000 ) ) ;
#57623 = EDGE_CURVE ( 'NONE', #56039, #27357, #45405, .T. ) ;
#57624 = SURFACE_SIDE_STYLE ('',( #40519 ) ) ;
#57625 = DIRECTION ( 'NONE',  ( 0.000000000000000000, -0.9510199984508466153, 0.3091293621553143911 ) ) ;
#57626 = CARTESIAN_POINT ( 'NONE',  ( 7.717918988116000634, 2.852331522235000083, 6.784355039830999523 ) ) ;
#57627 = CARTESIAN_POINT ( 'NONE',  ( 10.49937419337999955, 2.985313722448000195, -6.358656051156999389 ) ) ;
#57628 = CARTESIAN_POINT ( 'NONE',  ( 24.67921430886200085, -8.727631620858000261, -9.158313288899000426 ) ) ;
#57629 = CARTESIAN_POINT ( 'NONE',  ( 17.87019584817731754, 3.039826384816739502, 12.30925258946623835 ) ) ;
#57630 = CARTESIAN_POINT ( 'NONE',  ( 17.98628609634500108, 3.388648274289000284, -11.90503202562999974 ) ) ;
#57631 = CARTESIAN_POINT ( 'NONE',  ( 9.447841622600000377, 5.447457912891000120, 7.431328695644999982 ) ) ;
#57632 = ORIENTED_EDGE ( 'NONE', *, *, #9650, .F. ) ;
#57633 = CARTESIAN_POINT ( 'NONE',  ( 10.61341493184000129, -5.180137390751999860, -4.762641710075000034 ) ) ;
#57634 = ORIENTED_EDGE ( 'NONE', *, *, #1261, .T. ) ;
#57635 = CARTESIAN_POINT ( 'NONE',  ( 12.21993702172676954, -2.719929609653446434, 12.39763114037444680 ) ) ;
#57636 = CARTESIAN_POINT ( 'NONE',  ( 8.564919648097475857, 5.350116636189168773, -7.500005043868485544 ) ) ;
#57637 = CARTESIAN_POINT ( 'NONE',  ( 10.74599736040000053, 5.242718773683000322, 8.978699897073999736 ) ) ;
#57638 = CARTESIAN_POINT ( 'NONE',  ( 11.31013259637009938, -5.031671030421000168, 6.937848198857199833 ) ) ;
#57639 = CARTESIAN_POINT ( 'NONE',  ( 9.468110841233000841, 4.082930418187999955, -6.104944817728999773 ) ) ;
#57640 = LINE ( 'NONE', #23510, #660 ) ;
#57641 = CARTESIAN_POINT ( 'NONE',  ( 10.54272335273199879, 4.444874504667400750, -8.698083075453000745 ) ) ;
#57642 = CARTESIAN_POINT ( 'NONE',  ( 12.49190496432325226, -0.5409888710114151289, 12.68448745112149467 ) ) ;
#57643 = CARTESIAN_POINT ( 'NONE',  ( 5.557969180995212533, -12.17302321295568213, -3.765215263422377223 ) ) ;
#57644 = CARTESIAN_POINT ( 'NONE',  ( 7.100000000000000533, 0.000000000000000000, 0.000000000000000000 ) ) ;
#57645 = CARTESIAN_POINT ( 'NONE',  ( 17.55505043854144276, -0.6250000000000001110, -25.00000000000000000 ) ) ;
#57646 = EDGE_CURVE ( 'NONE', #50417, #35693, #55201, .T. ) ;
#57647 = VERTEX_POINT ( 'NONE', #40163 ) ;
#57648 = CARTESIAN_POINT ( 'NONE',  ( 9.327795280414001411, 3.161445734422999809, -6.178649910536000434 ) ) ;
#57649 = CARTESIAN_POINT ( 'NONE',  ( 7.459654161154999130, -1.040770095916999871, 1.062041426571000091 ) ) ;
#57650 = CARTESIAN_POINT ( 'NONE',  ( 10.97051713369074655, -2.309060732479470079, 7.058091048960522862 ) ) ;
#57651 = CARTESIAN_POINT ( 'NONE',  ( 9.188137270893804498, 4.829658083092700060, -8.579838158914373736 ) ) ;
#57652 = CARTESIAN_POINT ( 'NONE',  ( 10.14601354018233259, 4.999583552997728830, -6.731816600031361730 ) ) ;
#57653 = CARTESIAN_POINT ( 'NONE',  ( 11.18687482311539938, -2.942322404451000128, -7.927326830586499007 ) ) ;
#57654 = VERTEX_POINT ( 'NONE', #55549 ) ;
#57655 = CONICAL_SURFACE ( 'NONE', #66597, 1.150087858351999781, 0.7854644967339313721 ) ;
#57656 = CARTESIAN_POINT ( 'NONE',  ( 2.472081873819000020, 2.864690124100000013, -2.197449004149000462 ) ) ;
#57657 = CARTESIAN_POINT ( 'NONE',  ( 13.92027728199409431, 8.815475954240564960, 7.616421984250506760 ) ) ;
#57660 = CARTESIAN_POINT ( 'NONE',  ( 13.46053068095500116, -9.490401724732999256, -7.804222448269000800 ) ) ;
#57659 = CARTESIAN_POINT ( 'NONE',  ( 9.939403263311918479, 2.266755596462933564, 7.738633765297627143 ) ) ;
#57658 = UNCERTAINTY_MEASURE_WITH_UNIT (LENGTH_MEASURE( 1.000000000000000082E-05 ), #62354, 'distance_accuracy_value', 'NONE');
#57661 = CARTESIAN_POINT ( 'NONE',  ( 15.89979320884932967, 4.771864030974168003, 11.40757335769640513 ) ) ;
#57662 = VERTEX_POINT ( 'NONE', #61478 ) ;
#57663 = CARTESIAN_POINT ( 'NONE',  ( 17.92197813837935527, -1.993632751867237207, -13.76786175838294923 ) ) ;
#57664 = CARTESIAN_POINT ( 'NONE',  ( 10.89979975933730039, 4.819074589197400726, 7.781807394638899922 ) ) ;
#57665 = LINE ( 'NONE', #63248, #22107 ) ;
#57666 = CARTESIAN_POINT ( 'NONE',  ( 7.577019353207000485, -5.480312458445999901, 8.192326492433998908 ) ) ;
#57667 = ORIENTED_EDGE ( 'NONE', *, *, #57623, .T. ) ;
#57668 = CARTESIAN_POINT ( 'NONE',  ( 9.385308886257000438, 4.135077451221000011, 9.175524215473998879 ) ) ;
#57670 = CARTESIAN_POINT ( 'NONE',  ( 10.40685100253999984, 2.832432432432000269, -6.822293592207000934 ) ) ;
#57669 = DIRECTION ( 'NONE',  ( -1.000000000000000000, 0.000000000000000000, 0.000000000000000000 ) ) ;
#57671 = CARTESIAN_POINT ( 'NONE',  ( 7.642454705974068396, -5.316671649445813053, 6.363707368334387660 ) ) ;
#57672 = CARTESIAN_POINT ( 'NONE',  ( 17.91802112668279179, -0.5089014838709605693, 13.88746088750631635 ) ) ;
#57673 = CARTESIAN_POINT ( 'NONE',  ( 24.23232976021700225, 3.402404391673000017, 12.43152572969999881 ) ) ;
#57674 = VERTEX_POINT ( 'NONE', #13934 ) ;
#57675 = CARTESIAN_POINT ( 'NONE',  ( 4.600000207916445483, -13.27499874714999883, 0.000000000000000000 ) ) ;
#57676 = CARTESIAN_POINT ( 'NONE',  ( 11.64179841651039915, -4.353306409735099969, 6.560784671286499226 ) ) ;
#57677 = FACE_OUTER_BOUND ( 'NONE', #60798, .T. ) ;
#57678 = CARTESIAN_POINT ( 'NONE',  ( 9.799251915619999309, 4.057329420971000467, 9.430703183047999261 ) ) ;
#57679 = CARTESIAN_POINT ( 'NONE',  ( 10.69456919669529960, 5.093991349577000172, 7.176777099639999768 ) ) ;
#57680 = CARTESIAN_POINT ( 'NONE',  ( 23.74396322974578766, -3.264338234022875707, 13.24371991867584519 ) ) ;
#57681 = CARTESIAN_POINT ( 'NONE',  ( 10.31905590579000176, 2.899999999999999911, -6.571291218949999902 ) ) ;
#57682 = EDGE_CURVE ( 'NONE', #47578, #25073, #39566, .T. ) ;
#57683 = DIRECTION ( 'NONE',  ( 0.000000000000000000, 1.000000000000000000, 0.000000000000000000 ) ) ;
#57684 = EDGE_CURVE ( 'NONE', #35474, #2919, #33884, .T. ) ;
#57685 = CARTESIAN_POINT ( 'NONE',  ( 8.352297532185232853, 2.893034095650034665, -6.685148257416485329 ) ) ;
#57686 = AXIS2_PLACEMENT_3D ( 'NONE', #54080, #12131, #59674 ) ;
#57687 = CARTESIAN_POINT ( 'NONE',  ( 18.21736474454390375, -2.220153890850323553, 13.82285830752080713 ) ) ;
#57688 = CARTESIAN_POINT ( 'NONE',  ( 18.09696660044057026, 2.811537062192479119, -13.60243477576679538 ) ) ;
#57689 = ORIENTED_EDGE ( 'NONE', *, *, #35220, .T. ) ;
#57690 = CARTESIAN_POINT ( 'NONE',  ( 10.86301932002748138, 2.749999999999999112, 7.200148911387369566 ) ) ;
#57691 = CARTESIAN_POINT ( 'NONE',  ( 9.211801307670125283, -3.888124047000113048, -6.244821713992729784 ) ) ;
#57692 = VERTEX_POINT ( 'NONE', #35260 ) ;
#57693 = CARTESIAN_POINT ( 'NONE',  ( 7.890669427268998781, -4.660296165433000404, 6.322498843348999920 ) ) ;
#57694 = CARTESIAN_POINT ( 'NONE',  ( 10.87518447801629939, 4.865987311498500389, 7.519093628927509876 ) ) ;
#57695 = VECTOR ( 'NONE', #66126, 1000.000000000000114 ) ;
#57696 = CARTESIAN_POINT ( 'NONE',  ( 11.11845610223999969, 5.767025078915000158, 7.178418469370999588 ) ) ;
#57697 = CARTESIAN_POINT ( 'NONE',  ( 10.04002816746000093, 2.348904337896000172, -7.136750921008999882 ) ) ;
#57698 = CARTESIAN_POINT ( 'NONE',  ( 10.30371347217102773, -3.410708369063949696, -8.130653431319531776 ) ) ;
#57699 = CARTESIAN_POINT ( 'NONE',  ( 9.966331042021000286, -2.304002513595999613, 6.575636708208000059 ) ) ;
#57700 = CARTESIAN_POINT ( 'NONE',  ( 18.24552617758597606, -0.2196334679052314443, -12.59809060309703277 ) ) ;
#57701 = CIRCLE ( 'NONE', #45443, 11.84999999999999964 ) ;
#57702 = CARTESIAN_POINT ( 'NONE',  ( 9.002567663965152178, 5.272335535898198700, 7.950868213405990481 ) ) ;
#57703 = CARTESIAN_POINT ( 'NONE',  ( 10.67410807141119911, -3.953638752893899877, -8.502397868920999358 ) ) ;
#57704 = CARTESIAN_POINT ( 'NONE',  ( 25.46373154986600085, 8.354608910739999672, 8.148450287869000164 ) ) ;
#57705 = VERTEX_POINT ( 'NONE', #23726 ) ;
#57706 = EDGE_CURVE ( 'NONE', #6268, #17363, #24595, .T. ) ;
#57707 = CIRCLE ( 'NONE', #32030, 12.35000000006999876 ) ;
#57708 = CYLINDRICAL_SURFACE ( 'NONE', #3456, 1.350000000000000089 ) ;
#57709 = DIRECTION ( 'NONE',  ( 1.000000000000000000, 0.000000000000000000, 0.000000000000000000 ) ) ;
#57710 = CARTESIAN_POINT ( 'NONE',  ( 25.22252232637437785, 8.509544449812528555, 8.058439155819339561 ) ) ;
#57711 = EDGE_CURVE ( 'NONE', #43682, #4376, #65443, .T. ) ;
#57712 = CARTESIAN_POINT ( 'NONE',  ( 17.65082925870466113, 1.766819657443030600, 12.47551016841904215 ) ) ;
#57713 = CARTESIAN_POINT ( 'NONE',  ( 12.16922513814159679, 2.166987123599053433, 13.83127908232058267 ) ) ;
#57714 = CARTESIAN_POINT ( 'NONE',  ( 9.242349231304000767, -5.206700957550999931, 8.808818370147001531 ) ) ;
#57715 = AXIS2_PLACEMENT_3D ( 'NONE', #28924, #28567, #6878 ) ;
#57716 = CARTESIAN_POINT ( 'NONE',  ( 12.53103059986594481, -0.5618114787718360148, -12.68327018738675172 ) ) ;
#57717 = CARTESIAN_POINT ( 'NONE',  ( 12.33591485593543347, -0.5568603909045801714, 13.98892293345219962 ) ) ;
#57718 = ORIENTED_EDGE ( 'NONE', *, *, #42524, .T. ) ;
#57719 = CARTESIAN_POINT ( 'NONE',  ( 24.55996189763800075, 8.848787117368999589, 9.333438204885000644 ) ) ;
#57720 = CARTESIAN_POINT ( 'NONE',  ( 9.000480666858997836, -3.573487373903700082, -8.706015266875999359 ) ) ;
#57721 = CARTESIAN_POINT ( 'NONE',  ( 0.000000000000000000, 0.000000000000000000, 0.000000000000000000 ) ) ;
#57722 = CARTESIAN_POINT ( 'NONE',  ( 9.786673210037999837, -2.381198102024000285, 7.612749732462000374 ) ) ;
#57723 = CARTESIAN_POINT ( 'NONE',  ( 16.03045494250125813, 9.206206171697990825, 8.492540761685223316 ) ) ;
#57724 = CARTESIAN_POINT ( 'NONE',  ( 11.67056785386840012, -4.718624889240500053, 7.016391833292499491 ) ) ;
#57725 = FACE_OUTER_BOUND ( 'NONE', #16433, .T. ) ;
#57726 = CARTESIAN_POINT ( 'NONE',  ( 0.7654415426042999737, 2.838478058858999731, -1.283102133118000143 ) ) ;
#57727 = DIRECTION ( 'NONE',  ( 0.000000000000000000, -1.000000000000000000, 0.000000000000000000 ) ) ;
#57728 = CARTESIAN_POINT ( 'NONE',  ( 12.53569427112573820, 1.812281311417180740, 12.46898785302652257 ) ) ;
#57729 = CARTESIAN_POINT ( 'NONE',  ( 4.574515983791000080E-07, 0.000000000000000000, 0.000000000000000000 ) ) ;
#57730 = CARTESIAN_POINT ( 'NONE',  ( 11.63410404293056999, 3.557672215630899970, -8.400720262063998689 ) ) ;
#57731 = CARTESIAN_POINT ( 'NONE',  ( 12.01556330254185845, 11.99897551495936909, -3.593484177663820667 ) ) ;
#57732 = CARTESIAN_POINT ( 'NONE',  ( 10.84974221959000218, 5.265003089217000998, -6.385808769407000263 ) ) ;
#57733 = CARTESIAN_POINT ( 'NONE',  ( 9.352013376692999813, 2.859607053196999704, -6.920441276178300072 ) ) ;
#57735 = CARTESIAN_POINT ( 'NONE',  ( 12.25843860535923469, 2.803243370102336929, 12.37572767901811588 ) ) ;
#57734 = FACE_OUTER_BOUND ( 'NONE', #40890, .T. ) ;
#57736 = CARTESIAN_POINT ( 'NONE',  ( 5.500000000000000000, -12.65263727151999795, -3.063503113339999917 ) ) ;
#57737 = ORIENTED_EDGE ( 'NONE', *, *, #60574, .F. ) ;
#57738 = VECTOR ( 'NONE', #30485, 1000.000000000000227 ) ;
#57739 = CARTESIAN_POINT ( 'NONE',  ( 12.24748280284102542, -0.2825744477460949144, 12.69577188568745285 ) ) ;
#57740 = CARTESIAN_POINT ( 'NONE',  ( 10.35226354018316108, 2.907767014557178342, 8.129523725463624118 ) ) ;
#57741 = FACE_OUTER_BOUND ( 'NONE', #60739, .T. ) ;
#57742 = PRODUCT_DEFINITION ( 'UNKNOWN', '', #37394, #47874 ) ;
#57743 = EDGE_CURVE ( 'NONE', #17363, #59240, #62106, .T. ) ;
#57744 = CARTESIAN_POINT ( 'NONE',  ( 9.097772138681998300, 3.626242194157900389, 8.432280753260499750 ) ) ;
#57745 = CARTESIAN_POINT ( 'NONE',  ( 4.149992563292000725, -2.000000000000000000, 0.000000000000000000 ) ) ;
#57746 = CARTESIAN_POINT ( 'NONE',  ( 12.20418674196361764, -2.672312675674152427, 13.63540648336421945 ) ) ;
#57747 = CARTESIAN_POINT ( 'NONE',  ( 12.18008396645303826, 2.512642877094447780, 13.67072295643779078 ) ) ;
#57748 = CARTESIAN_POINT ( 'NONE',  ( 8.154367619217863350, 3.070658246196826369, 6.308684818284896245 ) ) ;
#57749 = ORIENTED_EDGE ( 'NONE', *, *, #27402, .T. ) ;
#57750 = CARTESIAN_POINT ( 'NONE',  ( 5.287471543204999236, -0.1506867338748000273, 1.266511664267000015 ) ) ;
#57751 = CARTESIAN_POINT ( 'NONE',  ( 9.478659112603999404, -4.555852086785099786, -8.652134039551000910 ) ) ;
#57752 = VECTOR ( 'NONE', #48557, 1000.000000000000000 ) ;
#57753 = CARTESIAN_POINT ( 'NONE',  ( 9.773267324721318872, -2.820167152981252645, -8.180006241673510203 ) ) ;
#57754 = CARTESIAN_POINT ( 'NONE',  ( 11.06591429142999949, -3.980313504646230349, 8.533318907609000803 ) ) ;
#57755 = CARTESIAN_POINT ( 'NONE',  ( 18.16360624365136189, 2.642789843301108998, -12.41718366361782699 ) ) ;
#57756 = CARTESIAN_POINT ( 'NONE',  ( 13.99999999393278927, -9.282302710986076733, -8.207095416277889299 ) ) ;
#57757 = CARTESIAN_POINT ( 'NONE',  ( 17.63951772021993492, 3.120582521217798444, 12.28507980727042614 ) ) ;
#57759 = AXIS2_PLACEMENT_3D ( 'NONE', #17385, #66307, #50584 ) ;
#57758 = CARTESIAN_POINT ( 'NONE',  ( 8.212416242268998801, 3.104180772687998857, 6.104177153569003700 ) ) ;
#57760 = CARTESIAN_POINT ( 'NONE',  ( 11.13506629761000077, -2.665575611901000119, -5.176677555269999509 ) ) ;
#57761 = CARTESIAN_POINT ( 'NONE',  ( 11.15264435320999858, -2.317067032475999877, -7.596564138533999255 ) ) ;
#57762 = CARTESIAN_POINT ( 'NONE',  ( 9.153455117183082024, -2.649843614532905178, 7.852866721134374117 ) ) ;
#57763 = CARTESIAN_POINT ( 'NONE',  ( 12.61757770595761308, 0.7057854747025396058, -13.98219993205039025 ) ) ;
#57764 = CARTESIAN_POINT ( 'NONE',  ( 13.55436146409600262, -9.071829816454000550, -7.538704307477999578 ) ) ;
#57765 = EDGE_CURVE ( 'NONE', #50821, #40899, #6057, .T. ) ;
#57766 = CARTESIAN_POINT ( 'NONE',  ( 18.18005044575085449, -2.500000006795658702, -13.67340643792831401 ) ) ;
#57767 = EDGE_CURVE ( 'NONE', #62603, #2862, #1181, .T. ) ;
#57768 = CARTESIAN_POINT ( 'NONE',  ( 2.873890132544666631, -2.150913519912200922, -2.798833948393631754 ) ) ;
#57769 = ORIENTED_EDGE ( 'NONE', *, *, #31966, .F. ) ;
#57770 = CARTESIAN_POINT ( 'NONE',  ( 9.550320280412000429, 2.370176859044999862, -6.912649125838000508 ) ) ;
#57771 = CARTESIAN_POINT ( 'NONE',  ( 11.00595525820100029, -4.081787880721680750, 8.362327856951900173 ) ) ;
#57772 = ORIENTED_EDGE ( 'NONE', *, *, #34631, .F. ) ;
#57773 = EDGE_CURVE ( 'NONE', #68416, #53136, #17914, .T. ) ;
#57774 = DIRECTION ( 'NONE',  ( 1.000000000000000000, 0.000000000000000000, -0.000000000000000000 ) ) ;
#57775 = CARTESIAN_POINT ( 'NONE',  ( 17.92019487611647932, 3.148838011673610993, -13.64129243465967711 ) ) ;
#57776 = ORIENTED_EDGE ( 'NONE', *, *, #28409, .F. ) ;
#57777 = CARTESIAN_POINT ( 'NONE',  ( 11.39189666366029918, 3.947847673382490541, 6.326270943800999191 ) ) ;
#57778 = CARTESIAN_POINT ( 'NONE',  ( 8.596685841231000325, 2.141799395716999843, -7.895788736628000848 ) ) ;
#57779 = CARTESIAN_POINT ( 'NONE',  ( 18.29999744883402002, 2.794302572679392416, -11.51706234618142233 ) ) ;
#57780 = CARTESIAN_POINT ( 'NONE',  ( 10.40480513895999870, -3.220259576336399920, -7.066537524675499782 ) ) ;
#57781 = CARTESIAN_POINT ( 'NONE',  ( 12.18394749351824480, -0.08111026479008709433, -13.89976203980642566 ) ) ;
#57782 = CARTESIAN_POINT ( 'NONE',  ( 24.32155143133507380, 9.044166503376443345, -9.474459912027812791 ) ) ;
#57783 = B_SPLINE_CURVE_WITH_KNOTS ( 'NONE', 3,
 ( #38261, #864, #38612, #39922 ),
 .UNSPECIFIED., .F., .F.,
 ( 4, 4 ),
 ( 0.000000000000000000, 1.000000000000000000 ),
 .UNSPECIFIED. ) ;
#57784 = CARTESIAN_POINT ( 'NONE',  ( 11.09999999999999964, 6.518040529534999905, 5.523195900108999190 ) ) ;
#57785 = ORIENTED_EDGE ( 'NONE', *, *, #9730, .T. ) ;
#57786 = CARTESIAN_POINT ( 'NONE',  ( 13.55279538703999975, 9.560508190731999534, 7.863756665013000635 ) ) ;
#57787 = CARTESIAN_POINT ( 'NONE',  ( 10.12339528040999959, 3.988943694240999704, -8.966360307350999648 ) ) ;
#57788 = EDGE_LOOP ( 'NONE', ( #39313, #64777, #21882 ) ) ;
#57789 = VECTOR ( 'NONE', #40996, 1000.000000000000000 ) ;
#57790 = CARTESIAN_POINT ( 'NONE',  ( 10.99480479316000014, 3.850613903518000036, -9.347963496621000345 ) ) ;
#57791 = ORIENTED_EDGE ( 'NONE', *, *, #22785, .F. ) ;
#57792 = CARTESIAN_POINT ( 'NONE',  ( 8.718784697134999817, 4.694174896253500151, 8.574479223074998657 ) ) ;
#57793 = CARTESIAN_POINT ( 'NONE',  ( 18.08809746899279602, -2.173637705205955672, -12.52162896472547260 ) ) ;
#57794 = EDGE_CURVE ( 'NONE', #27849, #29214, #38707, .T. ) ;
#57795 =( GEOMETRIC_REPRESENTATION_CONTEXT ( 3 ) GLOBAL_UNCERTAINTY_ASSIGNED_CONTEXT ( ( #68835 ) ) GLOBAL_UNIT_ASSIGNED_CONTEXT ( ( #360, #42668, #32191 ) ) REPRESENTATION_CONTEXT ( 'NONE', 'WORKASPACE' ) );
#57796 = DIRECTION ( 'NONE',  ( 0.000000000000000000, -0.9553735099700838562, 0.2954005017724949944 ) ) ;
#57797 = B_SPLINE_CURVE_WITH_KNOTS ( 'NONE', 3,
 ( #52808, #47570, #68874, #20992 ),
 .UNSPECIFIED., .F., .F.,
 ( 4, 4 ),
 ( 0.000000000000000000, 1.000000000000000000 ),
 .UNSPECIFIED. ) ;
#57798 = CIRCLE ( 'NONE', #20980, 13.89999852641999922 ) ;
#57799 = CARTESIAN_POINT ( 'NONE',  ( 4.099967492754000631, 2.049969825927307809, 8.734272638079285836E-09 ) ) ;
#57800 = CARTESIAN_POINT ( 'NONE',  ( 10.90000000000000036, 0.2999999999999999889, -4.902439024389999567 ) ) ;
#57801 = ORIENTED_EDGE ( 'NONE', *, *, #41103, .T. ) ;
#57802 = CARTESIAN_POINT ( 'NONE',  ( 12.46445792838400024, 11.52135921566999954, -4.763665720747999544 ) ) ;
#57803 = CARTESIAN_POINT ( 'NONE',  ( 9.783240866989459050, -5.333689009038027784, -6.342574321089660572 ) ) ;
#57804 = CARTESIAN_POINT ( 'NONE',  ( 10.35685100253999913, 2.832432432432000269, -6.822293592207000934 ) ) ;
#57805 = CIRCLE ( 'NONE', #58911, 0.3000000000000000444 ) ;
#57806 = CARTESIAN_POINT ( 'NONE',  ( 4.599999999999999645, 1.787797342887044394, 13.88538010501570952 ) ) ;
#57807 = CARTESIAN_POINT ( 'NONE',  ( 8.400739158770999637, 4.933589693325000525, -9.154576215408999573 ) ) ;
#57808 = DIRECTION ( 'NONE',  ( 0.000000000000000000, 0.8445101382956362590, 0.5355395655933231636 ) ) ;
#57809 = CARTESIAN_POINT ( 'NONE',  ( 9.949439740260999088, -2.508493821066999807, -7.171861383782999866 ) ) ;
#57810 = VERTEX_POINT ( 'NONE', #62493 ) ;
#57811 = ORIENTED_EDGE ( 'NONE', *, *, #59986, .T. ) ;
#57812 = VECTOR ( 'NONE', #53045, 999.9999999999998863 ) ;
#57813 = CARTESIAN_POINT ( 'NONE',  ( 9.020585841232000135, 4.920236664407999783, -6.448229650796999834 ) ) ;
#57814 = PLANE ( 'NONE',  #63379 ) ;
#57815 = CARTESIAN_POINT ( 'NONE',  ( 12.42225203013928514, -3.001455243171148535, 13.55441486463508660 ) ) ;
#57816 = CARTESIAN_POINT ( 'NONE',  ( 23.91316326678529336, 3.340384790131674109, 12.91004685077541048 ) ) ;
#57817 = CARTESIAN_POINT ( 'NONE',  ( 10.76947109217999810, -5.100000000000000533, -6.152188490330000370 ) ) ;
#57818 = CARTESIAN_POINT ( 'NONE',  ( 10.16858376188599955, 3.268856270222099791, -7.965979387614599894 ) ) ;
#57820 = CARTESIAN_POINT ( 'NONE',  ( 8.684778640374556602, 5.715811837031070652, 7.158423063840858802 ) ) ;
#57819 = CARTESIAN_POINT ( 'NONE',  ( 9.447809814040999399, -3.301541394817099739, 6.596733927440100231 ) ) ;
#57821 = CARTESIAN_POINT ( 'NONE',  ( 7.782404085375001834, -2.843788791114000958, 6.809963588862000705 ) ) ;
#57822 = ORIENTED_EDGE ( 'NONE', *, *, #56537, .T. ) ;
#57823 = CARTESIAN_POINT ( 'NONE',  ( 14.39999999825366750, -11.41071763166321240, 4.623975355197338821 ) ) ;
#57824 = CARTESIAN_POINT ( 'NONE',  ( 7.782975328289005290, -3.196931270636999667, 6.293200827887002191 ) ) ;
#57825 = EDGE_CURVE ( 'NONE', #54335, #1602, #14616, .T. ) ;
#57826 = EDGE_CURVE ( 'NONE', #53716, #24573, #46773, .T. ) ;
#57827 = CARTESIAN_POINT ( 'NONE',  ( 9.532392757686999119, 4.863450031739999346, 6.556157624301499176 ) ) ;
#57828 = CARTESIAN_POINT ( 'NONE',  ( 29.60000000000000142, 0.000000000000000000, 0.000000000000000000 ) ) ;
#57829 = CARTESIAN_POINT ( 'NONE',  ( 10.12549839661999940, -5.788806995403000144, 7.335561828691000485 ) ) ;
#57830 = CARTESIAN_POINT ( 'NONE',  ( 18.13624123201584837, 2.730018939185353322, -12.39502206882475299 ) ) ;
#57831 = CARTESIAN_POINT ( 'NONE',  ( 16.13862479881500178, -3.581551568669000041, -11.04584923442999944 ) ) ;
#57832 = B_SPLINE_CURVE_WITH_KNOTS ( 'NONE', 3,
 ( #49875, #44651, #28919, #23647 ),
 .UNSPECIFIED., .F., .F.,
 ( 4, 4 ),
 ( 0.000000000000000000, 1.000000000000000000 ),
 .UNSPECIFIED. ) ;
#57833 = B_SPLINE_CURVE_WITH_KNOTS ( 'NONE', 3,
 ( #11412, #6163, #27504, #59662, #38332, #15635 ),
 .UNSPECIFIED., .F., .F.,
 ( 4, 2, 4 ),
 ( 0.000000000000000000, 0.5000000000000000000, 1.000000000000000000 ),
 .UNSPECIFIED. ) ;
#57834 = CARTESIAN_POINT ( 'NONE',  ( 13.46018463513500052, 9.195629459350000090, 7.535158378801000367 ) ) ;
#57835 = CARTESIAN_POINT ( 'NONE',  ( 8.185765847591000011, -4.942196905450001232, 6.196983455206997782 ) ) ;
#57836 = CARTESIAN_POINT ( 'NONE',  ( 10.04193802597399987, -4.450760089576400347, -6.759376420744099612 ) ) ;
#57837 = B_SPLINE_CURVE_WITH_KNOTS ( 'NONE', 3,
 ( #6132, #16964, #26791, #15938, #42858, #21186, #10351, #42517, #16283, #53008, #37608, #53695, #27829, #53353, #27469, #11046, #63826, #26442, #59627, #48796, #207, #59274, #54030, #31687, #37954, #32380, #21527, #22218, #64507, #5788, #5455, #11377, #905, #16628, #32718, #49134, #58591, #1246, #43554, #5105, #63483, #27131 ),
 .UNSPECIFIED., .F., .F.,
 ( 4, 2, 2, 2, 2, 2, 2, 2, 2, 2, 2, 2, 2, 1, 2, 2, 2, 2, 2, 1, 2, 4 ),
 ( 0.4997863768984587285, 0.5623130797861424224, 0.6248397826738261163, 0.6404714583957457075, 0.6561031341176652987, 0.6873664855615019276, 0.7029981612834201865, 0.7186298370053385565, 0.7264456748662961871, 0.7342615127272538178, 0.7498931884491690791, 0.7811565398929997128, 0.7889723777539620064, 0.7967882156149244111, 0.8124198913368532171, 0.8280515670587820232, 0.8436832427807109402, 0.8749465942245686634, 0.8905782699464975805, 0.9062099456684264975, 0.9374732971122843317, 1.000000000000000000 ),
 .UNSPECIFIED. ) ;
#57838 = CARTESIAN_POINT ( 'NONE',  ( 11.09184687351642751, -3.000416447002275167, 6.731816600031356401 ) ) ;
#57839 = AXIS2_PLACEMENT_3D ( 'NONE', #22060, #64704, #16815 ) ;
#57840 = CARTESIAN_POINT ( 'NONE',  ( 0.1359928592618749876, 2.324556273228959184E-06, -3.136013406113613122 ) ) ;
#57841 = CARTESIAN_POINT ( 'NONE',  ( 0.1499942179680000265, -0.7197945678028380145, -2.678379783547566451 ) ) ;
#57842 = CARTESIAN_POINT ( 'NONE',  ( 2.967201571784999992, -1.671031821269000295, 2.798024169910999781 ) ) ;
#57843 = EDGE_LOOP ( 'NONE', ( #4143, #63717, #32090, #1156, #21411 ) ) ;
#57844 = CARTESIAN_POINT ( 'NONE',  ( 12.29653175235436002, 0.3639343692979905565, -12.69299665021505419 ) ) ;
#57845 = CARTESIAN_POINT ( 'NONE',  ( 12.20125275665228060, -2.661451430028674459, -12.41248063380501421 ) ) ;
#57846 = DIRECTION ( 'NONE',  ( 0.000000000000000000, -1.000000000000000000, 0.000000000000000000 ) ) ;
#57848 = DIRECTION ( 'NONE',  ( 0.000000000000000000, 1.000000000000000000, 0.000000000000000000 ) ) ;
#57847 = CIRCLE ( 'NONE', #4242, 1.500000000000000000 ) ;
#57849 = DIRECTION ( 'NONE',  ( 1.000000000000000000, 0.000000000000000000, 0.000000000000000000 ) ) ;
#57850 = EDGE_LOOP ( 'NONE', ( #44502, #27380, #44295, #34412 ) ) ;
#57851 = FACE_OUTER_BOUND ( 'NONE', #55766, .T. ) ;
#57852 = APPLICATION_PROTOCOL_DEFINITION ( 'draft international standard', 'automotive_design', 1998, #42282 ) ;
#57853 = ADVANCED_FACE ( 'NONE', ( #63170 ), #14276, .T. ) ;
#57854 = CARTESIAN_POINT ( 'NONE',  ( 16.39999999485600313, -3.595156957901000094, -11.99794989424000136 ) ) ;
#57855 = CARTESIAN_POINT ( 'NONE',  ( 13.58722619340700177, -11.45202530529999940, -1.920069653109999885 ) ) ;
#57856 = CARTESIAN_POINT ( 'NONE',  ( 10.64200660896710637, 3.294104879791080798, 8.705431914969542717 ) ) ;
#57857 = CIRCLE ( 'NONE', #47791, 1.000000000000000888 ) ;
#57858 = CARTESIAN_POINT ( 'NONE',  ( 13.24816728597000193, 12.42904273309000018, 1.833878933190999927 ) ) ;
#57859 = ORIENTED_EDGE ( 'NONE', *, *, #38884, .F. ) ;
#57860 = EDGE_CURVE ( 'NONE', #20353, #67057, #7169, .T. ) ;
#57861 = CARTESIAN_POINT ( 'NONE',  ( 9.966331042021000286, -2.304002513595999613, 6.575636708208000059 ) ) ;
#57862 = EDGE_LOOP ( 'NONE', ( #9611, #11752, #65277, #4395, #14189 ) ) ;
#57863 = CARTESIAN_POINT ( 'NONE',  ( 9.453819884702960863, -5.259191288891824634, 7.986286180968190429 ) ) ;
#57864 = CARTESIAN_POINT ( 'NONE',  ( 8.636456853209999451, -3.869396851328000153, 5.695656592546999519 ) ) ;
#57865 = CARTESIAN_POINT ( 'NONE',  ( 15.91802873821099951, 8.603382153815999800, 8.072764124688998066 ) ) ;
#57866 = ORIENTED_EDGE ( 'NONE', *, *, #24702, .T. ) ;
#57867 = CARTESIAN_POINT ( 'NONE',  ( 8.580688975202768631, 2.255905088303147288, -7.709247227175728412 ) ) ;
#57868 = B_SPLINE_CURVE_WITH_KNOTS ( 'NONE', 3,
 ( #15204, #67642, #8587, #62408, #35844, #9259, #31296, #20107, #35170, #41436, #36186, #52606, #30600, #40743, #67303, #24670, #57498, #42126, #9607, #30949, #26045, #52264, #4360, #26738, #58535, #11326, #5402, #53979, #10300, #36882, #48055, #10642, #1196, #16913, #53641, #64802, #16577, #6082, #32330, #64455, #42809, #501, #52957, #32667, #63776, #37902 ),
 .UNSPECIFIED., .F., .F.,
 ( 4, 2, 2, 2, 2, 2, 2, 2, 2, 2, 2, 2, 2, 2, 1, 2, 2, 2, 2, 2, 1, 2, 2, 4 ),
 ( 0.000000000000000000, 0.06247329711059514817, 0.09370994566589528618, 0.1249465942211954311, 0.1405649184988454758, 0.1561832427764955067, 0.1874198913317954851, 0.2030382156094475421, 0.2186565398870995436, 0.2264657020259255582, 0.2342748641647515728, 0.2498931884424035743, 0.2811298369977103806, 0.2889389991365332588, 0.2967481612753561371, 0.3123664855530020046, 0.3279848098306478166, 0.3436031341082936841, 0.3748397826635854746, 0.3904581069412313421, 0.4060764312188773206, 0.4373130797741676679, 0.4685497283294579596, 0.4997863768847483068 ),
 .UNSPECIFIED. ) ;
#57869 = CARTESIAN_POINT ( 'NONE',  ( 10.97843137008999825, -5.235400103863000254, 6.782920672145000829 ) ) ;
#57870 = AXIS2_PLACEMENT_3D ( 'NONE', #59313, #15637, #21902 ) ;
#57871 = CARTESIAN_POINT ( 'NONE',  ( 8.368395280410000581, 4.586183217919999500, -9.013777652867000612 ) ) ;
#57872 = CARTESIAN_POINT ( 'NONE',  ( 5.500000000000000000, 0.000000000000000000, 0.000000000000000000 ) ) ;
#57873 = CARTESIAN_POINT ( 'NONE',  ( 7.100000000000000533, 4.000000000000000000, 7.500000000000000000 ) ) ;
#57874 = EDGE_LOOP ( 'NONE', ( #57035, #26888, #39400, #39096, #50244 ) ) ;
#57875 = CARTESIAN_POINT ( 'NONE',  ( 9.124702828701000357, -4.778665285493000070, 8.799745834808000211 ) ) ;
#57876 = CARTESIAN_POINT ( 'NONE',  ( 12.21849864557798249, -2.283168037624248470, -13.71702792528834358 ) ) ;
#57877 = CARTESIAN_POINT ( 'NONE',  ( 12.71479700542636060, 11.41062399033359753, -4.624005385416205982 ) ) ;
#57878 = ORIENTED_EDGE ( 'NONE', *, *, #33147, .F. ) ;
#57879 = LINE ( 'NONE', #14889, #42605 ) ;
#57880 = VERTEX_POINT ( 'NONE', #68765 ) ;
#57881 = CARTESIAN_POINT ( 'NONE',  ( 8.424688440789140031, 5.350083765069828523, 7.500019236172019710 ) ) ;
#57882 = CARTESIAN_POINT ( 'NONE',  ( 10.83776233157765390, 3.727019380500508738, 9.251996054089767441 ) ) ;
#57883 = CARTESIAN_POINT ( 'NONE',  ( 5.000655990069000190, -1.131303444065999919, 1.070517240248999968 ) ) ;
#57884 = EDGE_CURVE ( 'NONE', #37829, #48911, #4509, .T. ) ;
#57885 = PLANE ( 'NONE',  #5334 ) ;
#57886 = CARTESIAN_POINT ( 'NONE',  ( 0.000000000000000000, 0.000000000000000000, 0.000000000000000000 ) ) ;
#57887 = CARTESIAN_POINT ( 'NONE',  ( 15.40000000009400161, -8.833277835210999740, -7.896561221812000930 ) ) ;
#57888 = CARTESIAN_POINT ( 'NONE',  ( 12.47278092208622802, 3.029458323191938529, 13.54674174801983710 ) ) ;
#57889 = CARTESIAN_POINT ( 'NONE',  ( 10.73930809942999964, -2.762991917822000154, 6.801028165221000066 ) ) ;
#57890 = EDGE_LOOP ( 'NONE', ( #22948, #203, #17815, #22327 ) ) ;
#57891 = CARTESIAN_POINT ( 'NONE',  ( 11.64975833414749928, -4.796537143354000499, 7.174999999999999822 ) ) ;
#57892 = VERTEX_POINT ( 'NONE', #62833 ) ;
#57893 = CARTESIAN_POINT ( 'NONE',  ( 9.555697025339000561, 2.440752375194999768, 6.680879724048000234 ) ) ;
#57894 =( REPRESENTATION_RELATIONSHIP ('NONE','NONE', #10823, #15732 ) REPRESENTATION_RELATIONSHIP_WITH_TRANSFORMATION ( #48053 )SHAPE_REPRESENTATION_RELATIONSHIP( ) );
#57895 = FACE_OUTER_BOUND ( 'NONE', #45837, .T. ) ;
#57896 = CARTESIAN_POINT ( 'NONE',  ( 9.617285841233000454, 5.306366356490000769, -7.996450761531000317 ) ) ;
#57897 = B_SPLINE_CURVE_WITH_KNOTS ( 'NONE', 3,
 ( #24071, #61816, #60445, #51330, #18145, #23385, #45408, #39816, #24420, #39467 ),
 .UNSPECIFIED., .F., .F.,
 ( 4, 2, 2, 2, 4 ),
 ( 0.3934091950370091628, 0.5450568962777568860, 0.6967045975185046647, 0.8483522987592523323, 1.000000000000000000 ),
 .UNSPECIFIED. ) ;
#57898 = CARTESIAN_POINT ( 'NONE',  ( 2.852007699173999988, -2.078510391984000449, -3.070736864395000154 ) ) ;
#57899 = CARTESIAN_POINT ( 'NONE',  ( 25.31012846324300014, 2.730838012578999940, 11.36012275232000057 ) ) ;
#57900 = CARTESIAN_POINT ( 'NONE',  ( 8.070148464763398977, 5.142014101325858455, -6.778269516176797183 ) ) ;
#57901 = AXIS2_PLACEMENT_3D ( 'NONE', #33143, #49906, #60738 ) ;
#57902 = DIRECTION ( 'NONE',  ( 0.7808688094474018904, 0.3122742207642010270, -0.5410440956875032237 ) ) ;
#57903 = EDGE_LOOP ( 'NONE', ( #22393, #43959, #13577, #39702 ) ) ;
#57904 = VECTOR ( 'NONE', #27315, 1000.000000000000000 ) ;
#57905 = CARTESIAN_POINT ( 'NONE',  ( 11.39975833414730033, -3.203462856645999945, -7.174999999999999822 ) ) ;
#57906 = CARTESIAN_POINT ( 'NONE',  ( 11.83041235500449950, -4.942357465271699724, 8.363295307663500822 ) ) ;
#57907 = CARTESIAN_POINT ( 'NONE',  ( 3.280140132543750475, -3.408904368339108260, 0.9161175952574674985 ) ) ;
#57908 = CARTESIAN_POINT ( 'NONE',  ( 15.36900185986900169, 9.263677555280001030, 8.208910455558001473 ) ) ;
#57909 = CARTESIAN_POINT ( 'NONE',  ( 8.977754440379998258, -2.019079883662000086, 7.390983468784999566 ) ) ;
#57911 = CARTESIAN_POINT ( 'NONE',  ( 12.15832103308141399, 2.898357473917167138, -13.69738840704374816 ) ) ;
#57910 = CARTESIAN_POINT ( 'NONE',  ( 10.96580581817999978, 4.930645553951000792, 6.170542400361000546 ) ) ;
#57912 = CARTESIAN_POINT ( 'NONE',  ( 11.20733594839949809, 4.840266102192999575, -6.537051788466999191 ) ) ;
#57913 = CARTESIAN_POINT ( 'NONE',  ( 25.09299657149600193, -11.65481462448000016, 3.020019921150999931 ) ) ;
#57914 = CARTESIAN_POINT ( 'NONE',  ( 9.273063610504998167, 4.355629271815800507, -8.290718512198798962 ) ) ;
#57915 = EDGE_CURVE ( 'NONE', #46967, #52961, #63703, .T. ) ;
#57916 = ADVANCED_FACE ( 'NONE', ( #4792 ), #21564, .F. ) ;
#57917 = CARTESIAN_POINT ( 'NONE',  ( 18.27776587948807219, 0.05827135643915087176, 12.59987075990256677 ) ) ;
#57918 = B_SPLINE_SURFACE_WITH_KNOTS ( 'NONE', 3, 3, ( 
 ( #51543, #62379, #14496, #57466 ),
 ( #61354, #35814, #24640, #29209 ),
 ( #40043, #57132, #46656, #20076 ),
 ( #45285, #9229, #13474, #8216 ),
 ( #40710, #29563, #50520, #51210 ),
 ( #66933, #13810, #3639, #56802 ),
 ( #14834, #19386, #66590, #30568 ),
 ( #34794, #30238, #18710, #56105 ),
 ( #45629, #41405, #3978, #45961 ),
 ( #3306, #2963, #24976, #35141 ),
 ( #14153, #24292, #62711, #2619 ),
 ( #23951, #62038, #67271, #40371 ) ),
 .UNSPECIFIED., .F., .F., .F.,
 ( 4, 1, 1, 1, 1, 1, 1, 1, 1, 4 ),
 ( 4, 4 ),
 ( 0.01098129032804999981, 0.05000000000000000278, 0.1000000000000000056, 0.1499999999999999944, 0.2000000000000000111, 0.2500000000000000000, 0.2999999999999999889, 0.3499999999999999778, 0.4000000000000000222, 0.4470328610943000158 ),
 ( -0.2706696436996000044, 1.270788880587000014 ),
 .UNSPECIFIED. ) ;
#57919 = CARTESIAN_POINT ( 'NONE',  ( 6.928033420461000347, 0.6960533226924000560, -1.066074183599000191 ) ) ;
#57920 = DIRECTION ( 'NONE',  ( 0.000000000000000000, -1.000000000000000000, 0.000000000000000000 ) ) ;
#57921 = CARTESIAN_POINT ( 'NONE',  ( 10.20000099824999928, -1.190159082397999942E-13, -12.49999978039866733 ) ) ;
#57922 = ORIENTED_EDGE ( 'NONE', *, *, #36173, .F. ) ;
#57923 = CARTESIAN_POINT ( 'NONE',  ( 7.283516392955999841, -4.426925773067000414, 9.293310812901001583 ) ) ;
#57924 = CARTESIAN_POINT ( 'NONE',  ( 8.860769353209001054, -2.935738482289000029, 6.259841087764999479 ) ) ;
#57925 = EDGE_CURVE ( 'NONE', #18184, #64966, #34642, .T. ) ;
#57926 = CYLINDRICAL_SURFACE ( 'NONE', #42733, 3.200000000000000178 ) ;
#57927 = CARTESIAN_POINT ( 'NONE',  ( 9.129428851719998406, -5.099284414202999827, 6.151604790022999758 ) ) ;
#57928 = ORIENTED_EDGE ( 'NONE', *, *, #3488, .T. ) ;
#57929 = CARTESIAN_POINT ( 'NONE',  ( 18.23590051321700400, 3.219096189435000088, 11.95421454054999977 ) ) ;
#57930 = CARTESIAN_POINT ( 'NONE',  ( 10.89324174884020024, 3.967693531726030010, 6.325557131097000685 ) ) ;
#57931 = CARTESIAN_POINT ( 'NONE',  ( 10.33453278041000090, 3.295703187163999459, -6.149878749787999865 ) ) ;
#57932 = VERTEX_POINT ( 'NONE', #48491 ) ;
#57933 = FACE_OUTER_BOUND ( 'NONE', #45602, .T. ) ;
#57935 = CARTESIAN_POINT ( 'NONE',  ( 10.14393020684899938, 5.250000000000000000, -7.500000000000000000 ) ) ;
#57934 = B_SPLINE_CURVE_WITH_KNOTS ( 'NONE', 3,
 ( #49873, #7565, #19085, #40088, #13518, #34839, #50223, #60706, #40411, #8599, #28918, #56150, #1986, #23308, #29949, #24338, #39738, #29607, #34503, #18068, #35182, #66976, #2325, #3348, #12471, #44648, #46004, #13854, #23646, #33804, #44985, #7224, #55816, #61733, #39385, #29256, #12824, #34149, #55468, #50565, #50908, #2667, #23993, #51252, #45670 ),
 .UNSPECIFIED., .F., .F.,
 ( 4, 2, 2, 2, 2, 2, 2, 2, 2, 1, 2, 2, 2, 2, 1, 1, 1, 2, 2, 2, 2, 1, 2, 2, 4 ),
 ( 0.000000000000000000, 0.1249999999999692468, 0.1874999999999541478, 0.2499999999999399369, 0.3749999999999112377, 0.4374999999998979150, 0.4687499999998902545, 0.4999999999998826494, 0.5624999999998692157, 0.5937499999998616662, 0.6093749999998585576, 0.6249999999998553379, 0.6874999999998469002, 0.7187499999998420153, 0.7343749999998387956, 0.7421874999998367972, 0.7460937499998359090, 0.7480468749998355760, 0.7499999999998353539, 0.8124999999998712141, 0.8437499999998891997, 0.8593749999998983036, 0.8671874999999030775, 0.8749999999999079625, 1.000000000000000000 ),
 .UNSPECIFIED. ) ;
#57936 = CARTESIAN_POINT ( 'NONE',  ( 10.37041638348499895, 2.758294858530000226, 7.802464414828100381 ) ) ;
#57937 = CARTESIAN_POINT ( 'NONE',  ( 10.85738557828999973, -2.754556666341999804, 8.976367391363998749 ) ) ;
#57938 = CARTESIAN_POINT ( 'NONE',  ( 9.041948341230998665, 2.707986230053999854, 5.994446745591000436 ) ) ;
#57939 = ORIENTED_EDGE ( 'NONE', *, *, #50585, .T. ) ;
#57940 = DIRECTION ( 'NONE',  ( -0.5298945028670929425, -2.005738535499974775E-09, -0.8480635682725891078 ) ) ;
#57941 = CARTESIAN_POINT ( 'NONE',  ( 7.616614158767000653, 2.462963193532999640, -6.383277393009000100 ) ) ;
#57942 = CARTESIAN_POINT ( 'NONE',  ( 8.224446432042114452, -5.652657913853214033, 8.042967277513600521 ) ) ;
#57943 = CARTESIAN_POINT ( 'NONE',  ( 9.626063610504999701, -3.531653260805799999, 6.458661544034999480 ) ) ;
#57944 = ORIENTED_EDGE ( 'NONE', *, *, #37638, .F. ) ;
#57945 = CARTESIAN_POINT ( 'NONE',  ( 15.86268444654400156, -3.728894906265999509, -11.70612128528000007 ) ) ;
#57946 = CARTESIAN_POINT ( 'NONE',  ( 6.313359839683334584, 1.310679582531387943, -0.7554284705563468760 ) ) ;
#57947 = VERTEX_POINT ( 'NONE', #22600 ) ;
#57948 = CARTESIAN_POINT ( 'NONE',  ( 8.810863317747999801, 4.960863370448500120, 7.499999999926881600 ) ) ;
#57949 = CARTESIAN_POINT ( 'NONE',  ( 6.899999691988000450, 12.20988339176000004, 3.111064831550000243 ) ) ;
#57950 = ORIENTED_EDGE ( 'NONE', *, *, #31967, .T. ) ;
#57951 = CARTESIAN_POINT ( 'NONE',  ( 18.14710216240463581, 0.2005085131878108773, -13.89805835524348865 ) ) ;
#57952 = CARTESIAN_POINT ( 'NONE',  ( 9.844904806657000407, -2.626678530444999993, -7.387134320497999340 ) ) ;
#57953 = CARTESIAN_POINT ( 'NONE',  ( 2.415556799209791716, -0.4581489286485083134, -3.500000000000000888 ) ) ;
#57954 = CIRCLE ( 'NONE', #40104, 1.300156908083999863 ) ;
#57955 = CARTESIAN_POINT ( 'NONE',  ( 11.35034208742529849, 3.369365911179700301, -8.491292290686200062 ) ) ;
#57956 = CARTESIAN_POINT ( 'NONE',  ( 12.33003632436370012, -5.243255406354000669, 7.790336465152099876 ) ) ;
#57957 = CARTESIAN_POINT ( 'NONE',  ( 24.34833239334600208, -12.15210528830085757, -3.256146798339317527 ) ) ;
#57958 = CARTESIAN_POINT ( 'NONE',  ( 11.09610807141099897, -3.947296672195129918, 6.360477084256999980 ) ) ;
#57959 = CARTESIAN_POINT ( 'NONE',  ( 8.154704719592000828, 4.255646040929000229, 9.114085578076998928 ) ) ;
#57960 = ORIENTED_EDGE ( 'NONE', *, *, #49648, .F. ) ;
#57961 = LINE ( 'NONE', #3773, #31787 ) ;
#57962 = CARTESIAN_POINT ( 'NONE',  ( 8.353308059623998361, -2.800111029801999774, 9.079936276749000612 ) ) ;
#57963 = CARTESIAN_POINT ( 'NONE',  ( 11.04782425406999913, -5.235403588978999601, 5.041461677707999911 ) ) ;
#57964 = VERTEX_POINT ( 'NONE', #21905 ) ;
#57965 = CARTESIAN_POINT ( 'NONE',  ( 12.20420485406511979, -2.672372548754605504, -12.40973746665996380 ) ) ;
#57966 = EDGE_CURVE ( 'NONE', #62671, #12641, #32418, .T. ) ;
#57967 = CARTESIAN_POINT ( 'NONE',  ( 8.082952751019996995, 10.21641539395999843, -5.351219519932003621 ) ) ;
#57968 = DIRECTION ( 'NONE',  ( 0.000000000000000000, -0.2714570858282905341, 0.9624505444715651947 ) ) ;
#57969 = CARTESIAN_POINT ( 'NONE',  ( 23.59378684139632298, -13.38703058558571080, -4.024018919119528803 ) ) ;
#57970 = CARTESIAN_POINT ( 'NONE',  ( 12.55438499206309011, -1.927376109800346571, -13.77831414012769429 ) ) ;
#57971 = EDGE_CURVE ( 'NONE', #23400, #10787, #52819, .T. ) ;
#57972 = CARTESIAN_POINT ( 'NONE',  ( 11.56025819896753859, -4.986099335708799707, -7.685900384398899554 ) ) ;
#57973 = CARTESIAN_POINT ( 'NONE',  ( 9.766851002543001314, -2.832432432432000269, 6.822293592207000934 ) ) ;
#57974 = CARTESIAN_POINT ( 'NONE',  ( 18.17205452211572947, -2.859046691836187648, 12.27135926524918297 ) ) ;
#57975 = ORIENTED_EDGE ( 'NONE', *, *, #51859, .F. ) ;
#57976 = B_SPLINE_CURVE_WITH_KNOTS ( 'NONE', 3,
 ( #40089, #28562, #1637, #6873 ),
 .UNSPECIFIED., .F., .F.,
 ( 4, 4 ),
 ( 0.000000000000000000, 1.000000000000000000 ),
 .UNSPECIFIED. ) ;
#57977 = ORIENTED_EDGE ( 'NONE', *, *, #26798, .T. ) ;
#57978 = CARTESIAN_POINT ( 'NONE',  ( 0.000000000000000000, 0.000000000000000000, 0.000000000000000000 ) ) ;
#57979 = CARTESIAN_POINT ( 'NONE',  ( 11.87299956498129916, -5.207010770456999893, 7.825000000000000178 ) ) ;
#57980 = CARTESIAN_POINT ( 'NONE',  ( 4.900006121742000786, -0.2617993877991476315, 2.000000000000000444 ) ) ;
#57981 = CARTESIAN_POINT ( 'NONE',  ( 10.10656234570999956, 4.887646627408000377, -6.257286147482000516 ) ) ;
#57982 = CARTESIAN_POINT ( 'NONE',  ( 10.60519595724999853, -5.343977295764999802, -7.731524081231999190 ) ) ;
#57983 = CARTESIAN_POINT ( 'NONE',  ( 17.98035626696890432, 2.958002308262752234, 12.33297292539930723 ) ) ;
#57984 = CARTESIAN_POINT ( 'NONE',  ( 24.45367377732199898, -12.43820265659000057, 3.092926956713999864 ) ) ;
#57985 = B_SPLINE_CURVE_WITH_KNOTS ( 'NONE', 3,
 ( #52526, #25961, #62666, #25269 ),
 .UNSPECIFIED., .F., .F.,
 ( 4, 4 ),
 ( 0.000000000000000000, 0.1254223444949154886 ),
 .UNSPECIFIED. ) ;
#57986 = CARTESIAN_POINT ( 'NONE',  ( 17.74710428552098662, -3.180431966555338441, -12.19205794678746990 ) ) ;
#57987 = VERTEX_POINT ( 'NONE', #42900 ) ;
#57988 = CARTESIAN_POINT ( 'NONE',  ( 9.144189324567731703, 2.621867583237485810, -6.380228173633875066 ) ) ;
#57989 = EDGE_LOOP ( 'NONE', ( #65065, #43448, #37543, #64291, #29304, #39843, #55675, #35116 ) ) ;
#57990 = CARTESIAN_POINT ( 'NONE',  ( 9.347254965556000883, 4.028327103212000715, 9.469449669541999626 ) ) ;
#57991 = CARTESIAN_POINT ( 'NONE',  ( 23.57810697541089340, -10.23415488232117099, -9.534542369472955414 ) ) ;
#57992 = CARTESIAN_POINT ( 'NONE',  ( 11.09647882763000126, 3.099775370665000196, 6.097099813297999660 ) ) ;
#57993 = CARTESIAN_POINT ( 'NONE',  ( 12.10988784977536525, -4.851105903694400645, 7.548634759728509280 ) ) ;
#57994 = CARTESIAN_POINT ( 'NONE',  ( 6.875000000000000000, 5.574137966889000317, -8.240733100917999820 ) ) ;
#57995 = CARTESIAN_POINT ( 'NONE',  ( 10.97885795247000118, 9.422687720258000610, -6.230811109673999759 ) ) ;
#57996 = CARTESIAN_POINT ( 'NONE',  ( 24.48566042065300152, 8.805064172929998989, 8.922039496844000439 ) ) ;
#57997 = CARTESIAN_POINT ( 'NONE',  ( 12.27392562293324829, -0.3300695133819704918, 12.69424233780835287 ) ) ;
#57998 = CARTESIAN_POINT ( 'NONE',  ( 8.893204545404998385, -3.399999999998999822, -6.188268997420999007 ) ) ;
#58000 = ADVANCED_FACE ( 'NONE', ( #37650 ), #27169, .F. ) ;
#57999 = B_SPLINE_CURVE_WITH_KNOTS ( 'NONE', 3,
 ( #28059, #7069, #1482, #22799, #6025, #65448, #43098, #16179, #32614, #12321, #33652, #54269, #22451, #64747, #27026 ),
 .UNSPECIFIED., .F., .F.,
 ( 4, 2, 2, 2, 1, 2, 2, 4 ),
 ( 0.000000000000000000, 0.5000000000000474065, 0.6250000000000575096, 0.6875000000000628386, 0.7187500000000658362, 0.7343750000000649480, 0.7500000000000640599, 1.000000000000000000 ),
 .UNSPECIFIED. ) ;
#58001 = CARTESIAN_POINT ( 'NONE',  ( 10.68903608760000168, 2.568976842941999905, 7.728092503410000091 ) ) ;
#58002 = CARTESIAN_POINT ( 'NONE',  ( 9.192135076938702909, -2.763579744383045433, 8.048932413616332937 ) ) ;
#58003 = ORIENTED_EDGE ( 'NONE', *, *, #64394, .F. ) ;
#58004 = CARTESIAN_POINT ( 'NONE',  ( 9.178620280414001797, 2.990001567622999623, -8.695425648791999862 ) ) ;
#58005 = CARTESIAN_POINT ( 'NONE',  ( -0.000000000000000000, 0.7586348975815447870, 2.824745580908568421 ) ) ;
#58006 = EDGE_CURVE ( 'NONE', #58925, #15028, #21114, .T. ) ;
#58007 = EDGE_CURVE ( 'NONE', #38892, #40442, #46132, .T. ) ;
#58008 = FACE_OUTER_BOUND ( 'NONE', #21575, .T. ) ;
#58009 = CARTESIAN_POINT ( 'NONE',  ( 9.219380188869688908, 4.353236832146805568, -8.814507018246107606 ) ) ;
#58010 = CARTESIAN_POINT ( 'NONE',  ( 10.17726354018233437, 4.629523725463628558, -6.407767014557180119 ) ) ;
#58011 = CARTESIAN_POINT ( 'NONE',  ( 11.33456651104149948, -3.887457492043800311, -6.364824110469998963 ) ) ;
#58012 = VERTEX_POINT ( 'NONE', #49175 ) ;
#58013 = CARTESIAN_POINT ( 'NONE',  ( 10.14393020684899938, -2.750000000000000000, -7.500000000000000000 ) ) ;
#58014 = CARTESIAN_POINT ( 'NONE',  ( 10.43470728713959161, -2.143801129421504470, 7.848344630244035613 ) ) ;
#58016 = CARTESIAN_POINT ( 'NONE',  ( 13.99932787941000178, -9.131694343880999654, -8.218494815692999111 ) ) ;
#58015 = CARTESIAN_POINT ( 'NONE',  ( 9.711073749820098300, 5.731818165367177365, 7.738391472525679049 ) ) ;
#58017 = CARTESIAN_POINT ( 'NONE',  ( 18.13950502211732640, -2.721680756027779147, 13.62394404485162624 ) ) ;
#58018 = VERTEX_POINT ( 'NONE', #13514 ) ;
#58019 = CARTESIAN_POINT ( 'NONE',  ( 10.68362359175999998, 2.603561947343000060, 7.762063351517999976 ) ) ;
#58020 = CARTESIAN_POINT ( 'NONE',  ( 18.03429950922811287, -2.098690172523155262, -13.75037901049766376 ) ) ;
#58021 = CARTESIAN_POINT ( 'NONE',  ( 11.68748876160954886, 3.399618311400500303, 6.875627981711399883 ) ) ;
#58022 = LINE ( 'NONE', #68492, #40000 ) ;
#58023 = CARTESIAN_POINT ( 'NONE',  ( 9.250897313459001126, -4.135077143711000325, 9.175520401071999288 ) ) ;
#58024 = VERTEX_POINT ( 'NONE', #66633 ) ;
#58025 = CARTESIAN_POINT ( 'NONE',  ( 7.647239158771000689, 5.850290547079999293, 6.784176679236000318 ) ) ;
#58026 = EDGE_CURVE ( 'NONE', #58018, #11014, #15002, .T. ) ;
#58028 = CARTESIAN_POINT ( 'NONE',  ( 10.75915805961999894, -5.387268372866000021, -6.278119777966000292 ) ) ;
#58027 = CARTESIAN_POINT ( 'NONE',  ( 10.22514748322304534, -2.649941783575446408, 7.500008211948054004 ) ) ;
#58029 = VECTOR ( 'NONE', #53293, 1000.000000000000000 ) ;
#58030 = CARTESIAN_POINT ( 'NONE',  ( 7.566932968645870616, -3.846483248383185227, 5.765333662263238956 ) ) ;
#58031 = CARTESIAN_POINT ( 'NONE',  ( 17.97864539831671493, -0.4596704778279275261, 13.88977177192326096 ) ) ;
#58032 = CARTESIAN_POINT ( 'NONE',  ( 23.74313554628299983, 3.207763596684000351, 13.21072658733999994 ) ) ;
#58033 = EDGE_LOOP ( 'NONE', ( #7748, #44995, #29390, #55100 ) ) ;
#58034 = DIRECTION ( 'NONE',  ( 0.000000000000000000, 0.000000000000000000, -1.000000000000000000 ) ) ;
#58035 = B_SPLINE_CURVE_WITH_KNOTS ( 'NONE', 3,
 ( #149, #11319, #37546, #63424 ),
 .UNSPECIFIED., .F., .F.,
 ( 4, 4 ),
 ( 0.000000000000000000, 1.000000000000000000 ),
 .UNSPECIFIED. ) ;
#58036 = CARTESIAN_POINT ( 'NONE',  ( 11.03057053952199951, -4.340412141385700195, 8.296503712697200328 ) ) ;
#58037 = CARTESIAN_POINT ( 'NONE',  ( 9.285195242305000818, 5.269680202247999823, 8.747831873285999649 ) ) ;
#58038 = CARTESIAN_POINT ( 'NONE',  ( 10.30047009227000032, 4.027768540959000276, 9.431354536774000152 ) ) ;
#58039 = CARTESIAN_POINT ( 'NONE',  ( 11.16225954179439839, 4.877394611789299894, 6.770980925167799036 ) ) ;
#58040 = ORIENTED_EDGE ( 'NONE', *, *, #25983, .F. ) ;
#58041 = CARTESIAN_POINT ( 'NONE',  ( 8.893204545404998385, -3.399999999998999822, -6.188268997420999007 ) ) ;
#58042 = CARTESIAN_POINT ( 'NONE',  ( 12.32338852522665107, 1.942342658536874378, -12.44939237451325909 ) ) ;
#58043 = CARTESIAN_POINT ( 'NONE',  ( 12.26077869730539938, -4.595338376575799799, 8.673950353177000139 ) ) ;
#58044 = DIRECTION ( 'NONE',  ( -0.000000000000000000, -0.000000000000000000, 1.000000000000000000 ) ) ;
#58045 = CARTESIAN_POINT ( 'NONE',  ( 18.27898184041761453, -2.472823623527009129, 13.77990254017906935 ) ) ;
#58046 = CARTESIAN_POINT ( 'NONE',  ( 10.36503728015203230, -2.650011783303574564, -7.500002219258004921 ) ) ;
#58047 = EDGE_LOOP ( 'NONE', ( #10044, #30329, #18127, #4723 ) ) ;
#58048 = CARTESIAN_POINT ( 'NONE',  ( 15.95676543642413847, -9.288185316739916431, -8.402783510542167988 ) ) ;
#58049 = FACE_OUTER_BOUND ( 'NONE', #37298, .T. ) ;
#58050 = ORIENTED_EDGE ( 'NONE', *, *, #18421, .F. ) ;
#58051 = CARTESIAN_POINT ( 'NONE',  ( 24.30001682246400208, -8.938702682732001747, -8.938676171235998780 ) ) ;
#58052 = CARTESIAN_POINT ( 'NONE',  ( 11.71210404293059959, 3.618181340822599790, 6.722495590581700320 ) ) ;
#58053 = CARTESIAN_POINT ( 'NONE',  ( 10.47253786429000044, -2.899999999999999911, -6.571291218949999902 ) ) ;
#58054 = CARTESIAN_POINT ( 'NONE',  ( 9.843622243630001378, 5.021682716044000294, -8.761466596873999535 ) ) ;
#58055 = CARTESIAN_POINT ( 'NONE',  ( 8.872292071306626227, -3.125836066416603387, -7.462990653670714458 ) ) ;
#58057 = B_SPLINE_CURVE_WITH_KNOTS ( 'NONE', 3,
 ( #15049, #57690, #2, #47565, #4896, #68867, #9800, #10488, #20988, #42652 ),
 .UNSPECIFIED., .F., .F.,
 ( 4, 2, 2, 2, 4 ),
 ( 0.000000000000000000, 0.2500000000000000000, 0.5000000000000000000, 0.7500000000000000000, 1.000000000000000000 ),
 .UNSPECIFIED. ) ;
#58056 = CARTESIAN_POINT ( 'NONE',  ( 10.33537187819000103, -5.153689638257000105, 8.830861236101000600 ) ) ;
#58058 = CARTESIAN_POINT ( 'NONE',  ( 17.97798751929653704, -0.5846869236304562678, -12.58643362292763612 ) ) ;
#58059 = EDGE_CURVE ( 'NONE', #17363, #52029, #65309, .T. ) ;
#58060 = CARTESIAN_POINT ( 'NONE',  ( 9.039569060871647466, 4.932468115888118732, 8.476030941254864004 ) ) ;
#58061 = CARTESIAN_POINT ( 'NONE',  ( 11.24025954179439957, -3.228187097503200320, -8.141292208271599051 ) ) ;
#58062 = CARTESIAN_POINT ( 'NONE',  ( 7.545267219589999463, 2.302289264429000504, 6.875166305059000393 ) ) ;
#58063 = ORIENTED_EDGE ( 'NONE', *, *, #45024, .T. ) ;
#58064 = B_SPLINE_CURVE_WITH_KNOTS ( 'NONE', 3,
 ( #39132, #51002, #34932, #60803 ),
 .UNSPECIFIED., .F., .F.,
 ( 4, 4 ),
 ( 0.000000000000000000, 1.000000000000000000 ),
 .UNSPECIFIED. ) ;
#58065 = DIRECTION ( 'NONE',  ( 0.000000000000000000, 0.000000000000000000, -1.000000000000000000 ) ) ;
#58066 = FACE_OUTER_BOUND ( 'NONE', #60619, .T. ) ;
#58067 = CARTESIAN_POINT ( 'NONE',  ( 8.702564146836889947, 2.714984396920538945, 7.027277620402957226 ) ) ;
#58068 = CARTESIAN_POINT ( 'NONE',  ( 10.78515324564000011, 10.04038604719000816, 5.237765435261001912 ) ) ;
#58069 = CARTESIAN_POINT ( 'NONE',  ( 12.75695018768100830, 1.789009927756595175, 13.88522413357867080 ) ) ;
#58070 = CARTESIAN_POINT ( 'NONE',  ( 13.69997185827399910, 9.599065136398388987, 6.667560658748404201 ) ) ;
#58071 = B_SPLINE_CURVE_WITH_KNOTS ( 'NONE', 3,
 ( #59961, #897, #39335, #54023 ),
 .UNSPECIFIED., .F., .F.,
 ( 4, 4 ),
 ( 0.000000000000000000, 1.000000000000000000 ),
 .UNSPECIFIED. ) ;
#58072 = CARTESIAN_POINT ( 'NONE',  ( 9.242197237618364980, -2.679953703640003404, 7.218470457551299901 ) ) ;
#58073 = CARTESIAN_POINT ( 'NONE',  ( 12.11831821888145555, -0.2353130933619223264, 13.99804086085458721 ) ) ;
#58074 = ORIENTED_EDGE ( 'NONE', *, *, #1228, .T. ) ;
#58075 = CARTESIAN_POINT ( 'NONE',  ( 12.80505043854146940, -1.760845406083394016, 12.47635457398814829 ) ) ;
#58076 = CARTESIAN_POINT ( 'NONE',  ( 9.532392757686999119, -3.136549968260000210, -8.443842375698499936 ) ) ;
#58077 = CARTESIAN_POINT ( 'NONE',  ( 5.500000000000000000, 0.000000000000000000, 0.000000000000000000 ) ) ;
#58078 = AXIS2_PLACEMENT_3D ( 'NONE', #32856, #33202, #42993 ) ;
#58079 = CARTESIAN_POINT ( 'NONE',  ( 10.99433452212999818, -3.697619272994999928, 5.729306330972000261 ) ) ;
#58080 = CARTESIAN_POINT ( 'NONE',  ( 11.59672200990539892, -4.817867935977999672, 7.785290430335599865 ) ) ;
#58081 = CARTESIAN_POINT ( 'NONE',  ( 8.712681907068999365, 3.774194491866800227, 6.635485632555699453 ) ) ;
#58082 = CARTESIAN_POINT ( 'NONE',  ( 0.1347486600378000055, -1.491878233134000142, -2.734521550864000172 ) ) ;
#58083 = CARTESIAN_POINT ( 'NONE',  ( 7.725062132959652494, -2.650631715052233162, 7.500008390440855877 ) ) ;
#58084 = CARTESIAN_POINT ( 'NONE',  ( 12.18809860077013596, 2.859021363400007232, 12.27136516364851460 ) ) ;
#58085 = CARTESIAN_POINT ( 'NONE',  ( 9.399896294736999280, -5.679455740088000582, -8.329752476417999318 ) ) ;
#58086 = CARTESIAN_POINT ( 'NONE',  ( 10.82179975933729921, 4.948878321068100661, -7.173532873542499466 ) ) ;
#58087 = CARTESIAN_POINT ( 'NONE',  ( 12.08335418496251101, 11.66230666314208264, -4.568774126650350986 ) ) ;
#58088 = ADVANCED_FACE ( 'NONE', ( #2661 ), #23989, .T. ) ;
#58089 = CARTESIAN_POINT ( 'NONE',  ( 10.09249221959000131, 2.841614569232000065, -8.724659027040001291 ) ) ;
#58090 = CARTESIAN_POINT ( 'NONE',  ( 10.08655864497999843, 5.007105485494000696, -8.288745882156399958 ) ) ;
#58092 = DIRECTION ( 'NONE',  ( 0.000000000000000000, 1.000000000000000000, 0.000000000000000000 ) ) ;
#58091 = CARTESIAN_POINT ( 'NONE',  ( 15.45728973496400194, -8.836548693809998412, -7.950469186927999310 ) ) ;
#58093 = DIRECTION ( 'NONE',  ( 0.000000000000000000, -0.4815106998112011483, 0.8764402124317022258 ) ) ;
#58094 = VERTEX_POINT ( 'NONE', #18752 ) ;
#58095 = CARTESIAN_POINT ( 'NONE',  ( 12.34378620388170233, 0.4226185367035117935, 12.69055435919257313 ) ) ;
#58096 = DIRECTION ( 'NONE',  ( 0.8660254037844541397, 0.000000000000000000, -0.4999999999999731326 ) ) ;
#58097 = CARTESIAN_POINT ( 'NONE',  ( 10.87522165821000009, -4.831071966430999787, 6.312786525516999703 ) ) ;
#58098 = CARTESIAN_POINT ( 'NONE',  ( 10.08359632033899800, 3.197262364844699611, 7.827597670336898794 ) ) ;
#58099 = CARTESIAN_POINT ( 'NONE',  ( 14.70000000000000107, -9.329726667597000755, -8.204053922562998480 ) ) ;
#58100 = CARTESIAN_POINT ( 'NONE',  ( 12.20145977811407434, -2.662504703663703509, 13.63765425733092052 ) ) ;
#58101 = CARTESIAN_POINT ( 'NONE',  ( 10.90000000164000049, 5.100000000007000267, 5.160242739040000082 ) ) ;
#58102 = CARTESIAN_POINT ( 'NONE',  ( 23.61990251228100135, 2.978955071604999727, -13.51777065273999945 ) ) ;
#58103 = ORIENTED_EDGE ( 'NONE', *, *, #33756, .T. ) ;
#58104 = EDGE_CURVE ( 'NONE', #58625, #5748, #31729, .T. ) ;
#58105 = CARTESIAN_POINT ( 'NONE',  ( 4.842745154312999567, -0.9264254985263000730, 0.8766476166769999745 ) ) ;
#58106 = CARTESIAN_POINT ( 'NONE',  ( 8.794772138681999252, -4.476015718025199597, -6.312652778810999621 ) ) ;
#58107 = CARTESIAN_POINT ( 'NONE',  ( 18.29999744883402002, -2.794302572679392416, 11.51706234618142055 ) ) ;
#58108 = CARTESIAN_POINT ( 'NONE',  ( 12.14633327354034797, -4.864904118400500188, 8.065722083251399610 ) ) ;
#58109 = EDGE_CURVE ( 'NONE', #1971, #36315, #44541, .T. ) ;
#58110 = AXIS2_PLACEMENT_3D ( 'NONE', #16181, #64061, #58831 ) ;
#58111 = CARTESIAN_POINT ( 'NONE',  ( 18.16983287387825996, 2.613005487247105130, -12.42455217891717467 ) ) ;
#58112 = CARTESIAN_POINT ( 'NONE',  ( 8.578316401368688560, 5.031557300139490430, 6.208917336984066893 ) ) ;
#58113 = CARTESIAN_POINT ( 'NONE',  ( 18.15011306039755823, 2.691200174448529658, 12.40496142756183673 ) ) ;
#58114 = CARTESIAN_POINT ( 'NONE',  ( 18.27929200418771671, 2.710634889609412124, 13.73643850023514013 ) ) ;
#58115 = FACE_OUTER_BOUND ( 'NONE', #62384, .T. ) ;
#58116 = DIRECTION ( 'NONE',  ( -1.000000000000000000, 0.000000000000000000, -2.893429392030000019E-14 ) ) ;
#58117 = CARTESIAN_POINT ( 'NONE',  ( 8.933536308090499034, 2.899999999999999911, -6.665341197412910645 ) ) ;
#58118 = PLANE ( 'NONE',  #40886 ) ;
#58119 = DIRECTION ( 'NONE',  ( 1.000000000000000000, 0.000000000000000000, 0.000000000000000000 ) ) ;
#58120 = DIRECTION ( 'NONE',  ( 0.000000000000000000, -0.9659258262890757507, 0.2588190451024927063 ) ) ;
#58121 = CARTESIAN_POINT ( 'NONE',  ( 23.58568869556000180, 13.39453640560000025, -4.037491894581999752 ) ) ;
#58122 = AXIS2_PLACEMENT_3D ( 'NONE', #46325, #35830, #37201 ) ;
#58123 = ORIENTED_EDGE ( 'NONE', *, *, #49441, .F. ) ;
#58124 = CARTESIAN_POINT ( 'NONE',  ( 8.456370280410999030, 2.836879604150999601, -8.783908972046001296 ) ) ;
#58125 = CARTESIAN_POINT ( 'NONE',  ( 11.93718179236249988, -4.209680326224799707, 8.481317998227099864 ) ) ;
#58126 = VERTEX_POINT ( 'NONE', #23641 ) ;
#58127 = CARTESIAN_POINT ( 'NONE',  ( 25.60000000000000142, 13.52296156804999860, -3.623466631435000362 ) ) ;
#58128 = CARTESIAN_POINT ( 'NONE',  ( 10.84226088462129844, -3.997572771977982775, -6.359261544073000039 ) ) ;
#58129 = EDGE_LOOP ( 'NONE', ( #29363, #22682, #22082, #1363 ) ) ;
#58130 = CARTESIAN_POINT ( 'NONE',  ( 11.14256920625030034, 4.042230905578960254, 8.674127893687000324 ) ) ;
#58131 = CARTESIAN_POINT ( 'NONE',  ( 18.23289209646694431, 3.217460216929902028, -11.19708622233978090 ) ) ;
#58132 = CARTESIAN_POINT ( 'NONE',  ( 10.20000099824999928, -12.50000000000000000, 0.000000000000000000 ) ) ;
#58133 = CARTESIAN_POINT ( 'NONE',  ( 11.36056039236529891, -3.108928759355700233, -7.543366519014379712 ) ) ;
#58134 = CARTESIAN_POINT ( 'NONE',  ( 12.29062815658215513, 0.3550741888481653286, -13.89389891668081134 ) ) ;
#58135 = B_SPLINE_CURVE_WITH_KNOTS ( 'NONE', 3,
 ( #63203, #31077, #11116, #69152, #68798, #10419, #281, #42589, #47492, #57980, #21259, #63897, #53765, #64239, #15673, #26863, #10077, #15331 ),
 .UNSPECIFIED., .F., .F.,
 ( 4, 2, 2, 2, 2, 2, 2, 2, 4 ),
 ( 0.000000000000000000, 0.1249999999999999722, 0.2500000000000000000, 0.3750000000000000000, 0.5000000000000001110, 0.6250000000000001110, 0.7500000000000000000, 0.8750000000000000000, 1.000000000000000000 ),
 .UNSPECIFIED. ) ;
#58136 = CARTESIAN_POINT ( 'NONE',  ( 9.565735834902588053, -3.588654020114534049, 6.337235623390005124 ) ) ;
#58137 = CARTESIAN_POINT ( 'NONE',  ( 13.60429364930200080, 11.50682694388999927, 2.143319390578000139 ) ) ;
#58138 = ORIENTED_EDGE ( 'NONE', *, *, #49874, .T. ) ;
#58139 = LINE ( 'NONE', #52544, #65550 ) ;
#58140 = CARTESIAN_POINT ( 'NONE',  ( 9.237204719595000668, 3.071719032003000116, -6.037263251225000182 ) ) ;
#58141 = ORIENTED_EDGE ( 'NONE', *, *, #56359, .T. ) ;
#58142 = CARTESIAN_POINT ( 'NONE',  ( 8.668369459057998938, 3.037916315484999963, -6.050520490110999461 ) ) ;
#58143 = EDGE_LOOP ( 'NONE', ( #10638, #42376, #62012, #51510 ) ) ;
#58144 = CARTESIAN_POINT ( 'NONE',  ( 11.72006721069024593, -11.52583591982215161, -1.696350940455132239 ) ) ;
#58145 = PRESENTATION_STYLE_ASSIGNMENT (( #20740 ) ) ;
#58146 = DIRECTION ( 'NONE',  ( -1.000000000000000000, 0.000000000000000000, 0.000000000000000000 ) ) ;
#58147 = FACE_OUTER_BOUND ( 'NONE', #53983, .T. ) ;
#58148 = CARTESIAN_POINT ( 'NONE',  ( 15.40000000009400161, 8.833277835210999740, 7.896561221812000930 ) ) ;
#58149 = ORIENTED_EDGE ( 'NONE', *, *, #53574, .T. ) ;
#58150 = CARTESIAN_POINT ( 'NONE',  ( 12.29459504890800048, 12.00990144118000025, -3.349639255392000248 ) ) ;
#58151 = DIRECTION ( 'NONE',  ( -1.000000000000000000, 0.000000000000000000, 0.000000000000000000 ) ) ;
#58152 = CARTESIAN_POINT ( 'NONE',  ( 11.59999999999999964, 4.000000000000000000, -7.500000000000000000 ) ) ;
#58153 = DIRECTION ( 'NONE',  ( 1.000000000000000000, 0.000000000000000000, 0.000000000000000000 ) ) ;
#58154 = B_SPLINE_CURVE_WITH_KNOTS ( 'NONE', 3,
 ( #62982, #47959, #26292, #41338, #47618, #68929, #30850, #53199, #15458, #5300, #57748, #20698, #68232, #15109, #40991, #26642, #42375 ),
 .UNSPECIFIED., .F., .F.,
 ( 4, 2, 2, 2, 1, 2, 2, 2, 4 ),
 ( 0.000000000000000000, 0.2500000000000131006, 0.3750000000000214273, 0.4375000000000257572, 0.4687500000000269784, 0.4843750000000265898, 0.5000000000000262013, 0.7500000000000131006, 1.000000000000000000 ),
 .UNSPECIFIED. ) ;
#58155 = AXIS2_PLACEMENT_3D ( 'NONE', #7851, #23926, #29541 ) ;
#58156 = CARTESIAN_POINT ( 'NONE',  ( 9.883629719592001095, 5.656948148960999845, -6.994239053114000626 ) ) ;
#58157 = CARTESIAN_POINT ( 'NONE',  ( 17.86534991953400109, -3.412585803847000054, 11.89775424487000066 ) ) ;
#58158 = CARTESIAN_POINT ( 'NONE',  ( 10.29094647910999782, -2.903513699412000104, -8.310923036409999298 ) ) ;
#58159 = ORIENTED_EDGE ( 'NONE', *, *, #61485, .F. ) ;
#58160 = ORIENTED_EDGE ( 'NONE', *, *, #13606, .T. ) ;
#58161 = AXIS2_PLACEMENT_3D ( 'NONE', #67019, #40452, #23690 ) ;
#58162 = CARTESIAN_POINT ( 'NONE',  ( 10.21685100254000034, -2.832432432432000269, 6.822293592207000934 ) ) ;
#58163 = CARTESIAN_POINT ( 'NONE',  ( 7.896812975352940356, 5.287194663100549974, 7.026484571482192187 ) ) ;
#58164 = CARTESIAN_POINT ( 'NONE',  ( 4.000000000000000000, -2.750000000000000000, 0.000000000000000000 ) ) ;
#58165 = CARTESIAN_POINT ( 'NONE',  ( 24.69847697201900161, 8.734418378053000254, -9.243512260004999703 ) ) ;
#58166 = EDGE_CURVE ( 'NONE', #11014, #58018, #3809, .T. ) ;
#58167 = EDGE_CURVE ( 'NONE', #66560, #22085, #45666, .T. ) ;
#58168 = CARTESIAN_POINT ( 'NONE',  ( 11.59966954483535773, 4.638989336656000440, -6.514072057539499916 ) ) ;
#58169 = CARTESIAN_POINT ( 'NONE',  ( 9.459367640780998343, 4.408706755790200660, -6.735364967924099666 ) ) ;
#58171 = CARTESIAN_POINT ( 'NONE',  ( 10.27733372368999909, -3.426503291345000424, 5.004059351583000748 ) ) ;
#58170 = CARTESIAN_POINT ( 'NONE',  ( 9.724417874593999755, -4.924352284713100047, 7.107043063332000088 ) ) ;
#58172 = CARTESIAN_POINT ( 'NONE',  ( 8.228217774218997249, -3.441349337319001389, 6.127431371819001882 ) ) ;
#58173 = VERTEX_POINT ( 'NONE', #49518 ) ;
#58174 = CARTESIAN_POINT ( 'NONE',  ( 10.31021345716899873, 4.636538040886300394, -8.078719053813800954 ) ) ;
#58175 = AXIS2_PLACEMENT_3D ( 'NONE', #47906, #20641, #10150 ) ;
#58176 = CARTESIAN_POINT ( 'NONE',  ( 9.608380199233998553, 5.269225938816000543, 7.659530259549099718 ) ) ;
#58177 = CARTESIAN_POINT ( 'NONE',  ( 5.599999999976000176, -7.849276784099999367E-14, -1.865174681369999824E-14 ) ) ;
#58178 = CARTESIAN_POINT ( 'NONE',  ( 10.62197618263000010, -5.779779175739000685, 7.256573549370999743 ) ) ;
#58179 = CARTESIAN_POINT ( 'NONE',  ( 17.81528574998282721, 3.068593513703687936, -12.30074760041392068 ) ) ;
#58180 = CARTESIAN_POINT ( 'NONE',  ( 16.44004776902900034, -3.254301421112999915, -11.33671678219000079 ) ) ;
#58181 = CARTESIAN_POINT ( 'NONE',  ( 13.50542051561400214, 9.036698429651000453, 7.720610530813999617 ) ) ;
#58182 = FACE_OUTER_BOUND ( 'NONE', #8776, .T. ) ;
#58183 = CARTESIAN_POINT ( 'NONE',  ( 10.11591290906799934, -4.635529777446699917, -8.277781595084700683 ) ) ;
#58184 = CARTESIAN_POINT ( 'NONE',  ( 17.60000003393297163, 11.45048720807753284, -4.713173851737514575 ) ) ;
#58185 = ADVANCED_FACE ( 'NONE', ( #13171 ), #1580, .T. ) ;
#58186 = FACE_OUTER_BOUND ( 'NONE', #43154, .T. ) ;
#58187 = CARTESIAN_POINT ( 'NONE',  ( 5.699999545467999695, 0.000000000000000000, 0.000000000000000000 ) ) ;
#58188 = CARTESIAN_POINT ( 'NONE',  ( 10.61094409420999973, 5.100000000000000533, -6.571291218949999902 ) ) ;
#58189 = ORIENTED_EDGE ( 'NONE', *, *, #49441, .T. ) ;
#58190 = CARTESIAN_POINT ( 'NONE',  ( 12.20096618732086213, 0.1616215023347943314, -12.69863621249090002 ) ) ;
#58191 = CARTESIAN_POINT ( 'NONE',  ( 8.232750256041883929, -4.666560802762334426, 6.122829837889073978 ) ) ;
#58192 = CARTESIAN_POINT ( 'NONE',  ( 9.433148997456999751, -5.167567567567999731, 6.822293592207000934 ) ) ;
#58193 = PLANE ( 'NONE',  #33483 ) ;
#58194 = CARTESIAN_POINT ( 'NONE',  ( 1.561390132540708908, 3.499999999999999112, 0.4581489286485193602 ) ) ;
#58195 = ORIENTED_EDGE ( 'NONE', *, *, #31322, .F. ) ;
#58196 = DIRECTION ( 'NONE',  ( 0.000000000000000000, 0.5000000000000169864, 0.8660254037844288266 ) ) ;
#58197 = CARTESIAN_POINT ( 'NONE',  ( 10.52435971519499880, -3.467537960339900138, -6.614211617270199461 ) ) ;
#58198 = DIRECTION ( 'NONE',  ( 1.000000000000000000, 0.000000000000000000, 0.000000000000000000 ) ) ;
#58199 = CARTESIAN_POINT ( 'NONE',  ( 0.000000000000000000, 0.000000000000000000, 0.000000000000000000 ) ) ;
#58200 = CARTESIAN_POINT ( 'NONE',  ( 8.191498566858999908, 3.399962487441000381, 6.146646668338000552 ) ) ;
#58201 = CARTESIAN_POINT ( 'NONE',  ( 10.64902344389989963, 3.116469856398800253, -6.963800219468099684 ) ) ;
#58202 = ORIENTED_EDGE ( 'NONE', *, *, #37700, .T. ) ;
#58203 = CARTESIAN_POINT ( 'NONE',  ( 9.520803773887999810, -3.270557529354000348, 5.711489293131999823 ) ) ;
#58204 = CARTESIAN_POINT ( 'NONE',  ( 8.811649685568998080, -3.898643963693099845, -8.457700632733599733 ) ) ;
#58205 = ORIENTED_EDGE ( 'NONE', *, *, #24805, .F. ) ;
#58206 = CARTESIAN_POINT ( 'NONE',  ( 13.46547102623810943, 11.49951335169978606, 1.866756745161230580 ) ) ;
#58207 = CARTESIAN_POINT ( 'NONE',  ( 9.047980646795000581, -2.806079842068999852, 8.615883328687999665 ) ) ;
#58208 = CARTESIAN_POINT ( 'NONE',  ( 17.87597250029675777, -0.6552116771452581867, -13.98466387211990281 ) ) ;
#58209 = VERTEX_POINT ( 'NONE', #54766 ) ;
#58210 = CARTESIAN_POINT ( 'NONE',  ( 8.646472257129413919, 2.666605646700320076, -6.358381277404491883 ) ) ;
#58211 = CIRCLE ( 'NONE', #37010, 13.27499874714999883 ) ;
#58212 = CARTESIAN_POINT ( 'NONE',  ( 7.034679719589999713, 3.562914451704999763, -5.997303864335000512 ) ) ;
#58213 = CARTESIAN_POINT ( 'NONE',  ( 12.80505043854146940, -3.125000000000000000, -12.28373071562070074 ) ) ;
#58214 = CARTESIAN_POINT ( 'NONE',  ( 8.170084059452333847, -3.293748801396804371, 6.167716128177580970 ) ) ;
#58215 = ORIENTED_EDGE ( 'NONE', *, *, #66656, .F. ) ;
#58216 = CARTESIAN_POINT ( 'NONE',  ( 11.18051369187999988, -5.340070732632000272, 8.416150632189001612 ) ) ;
#58217 = LINE ( 'NONE', #39657, #18353 ) ;
#58218 = CARTESIAN_POINT ( 'NONE',  ( 9.307788144226000426, -3.909067355573210278, 6.546538158064899804 ) ) ;
#58219 = VERTEX_POINT ( 'NONE', #2320 ) ;
#58220 = DIRECTION ( 'NONE',  ( 0.000000000000000000, 0.6884191022827191864, -0.7253131321107147977 ) ) ;
#58221 = EDGE_LOOP ( 'NONE', ( #64530, #16639, #23767, #61728 ) ) ;
#58222 = FACE_OUTER_BOUND ( 'NONE', #38336, .T. ) ;
#58223 = CARTESIAN_POINT ( 'NONE',  ( 5.099999999649000415, -1.199999999999999956, -9.776630298829998011 ) ) ;
#58224 = CARTESIAN_POINT ( 'NONE',  ( 11.56493925477931306, 5.173530340702487962, -7.948835763880663485 ) ) ;
#58225 = AXIS2_PLACEMENT_3D ( 'NONE', #57186, #58220, #40766 ) ;
#58226 = DIRECTION ( 'NONE',  ( -0.000000000000000000, -0.000000000000000000, 1.000000000000000000 ) ) ;
#58227 = EDGE_CURVE ( 'NONE', #9042, #38413, #56161, .T. ) ;
#58228 = DIRECTION ( 'NONE',  ( 0.000000000000000000, 1.000000000000000000, 0.000000000000000000 ) ) ;
#58229 = DIRECTION ( 'NONE',  ( 0.000000000000000000, -1.000000000000000000, 0.000000000000000000 ) ) ;
#58230 = EDGE_CURVE ( 'NONE', #26679, #57184, #33632, .T. ) ;
#58231 = CARTESIAN_POINT ( 'NONE',  ( 9.539763540182331525, -3.672815144550900524, -8.717465845835397076 ) ) ;
#58232 = ORIENTED_EDGE ( 'NONE', *, *, #10751, .T. ) ;
#58233 = CARTESIAN_POINT ( 'NONE',  ( 10.57102344389999971, -4.762665848028800220, -7.037150754511299233 ) ) ;
#58234 = ORIENTED_EDGE ( 'NONE', *, *, #8547, .T. ) ;
#58235 = CARTESIAN_POINT ( 'NONE',  ( 11.05935155529000014, 2.480238120735000162, 6.610075178640000715 ) ) ;
#58236 = CARTESIAN_POINT ( 'NONE',  ( 10.68342665876999931, 3.810131921595000026, -5.661115150006999386 ) ) ;
#58237 = DIRECTION ( 'NONE',  ( 0.000000000000000000, 1.000000000000000000, 0.000000000000000000 ) ) ;
#58238 = CARTESIAN_POINT ( 'NONE',  ( 12.24735473125024576, 2.217676833728435160, -13.72929951782216484 ) ) ;
#58239 = DIRECTION ( 'NONE',  ( -1.000000000000000000, 0.000000000000000000, 0.000000000000000000 ) ) ;
#58240 = CARTESIAN_POINT ( 'NONE',  ( 17.75641289383300148, -0.5920240553917509585, 13.88302649426328372 ) ) ;
#58241 = CARTESIAN_POINT ( 'NONE',  ( 23.50387503050299998, 6.898380679426999507, -11.95208534113000098 ) ) ;
#58242 = ORIENTED_EDGE ( 'NONE', *, *, #42695, .T. ) ;
#58243 = CARTESIAN_POINT ( 'NONE',  ( 12.29580333567063377, 0.3624858757096150463, 13.89364165471758739 ) ) ;
#58244 = CARTESIAN_POINT ( 'NONE',  ( 10.67764828895399987, -2.998858038575999974, 6.953185708700699408 ) ) ;
#58245 = DIRECTION ( 'NONE',  ( 1.000000000000000000, 0.000000000000000000, 0.000000000000000000 ) ) ;
#58246 = DIRECTION ( 'NONE',  ( 1.000000000000000000, 0.000000000000000000, 0.000000000000000000 ) ) ;
#58247 = EDGE_CURVE ( 'NONE', #51926, #29332, #49465, .T. ) ;
#58248 = CARTESIAN_POINT ( 'NONE',  ( 7.410855646792000151, -2.302293129340000188, 6.875167727519000849 ) ) ;
#58250 = DIRECTION ( 'NONE',  ( 0.000000000000000000, 1.000000000000000000, 0.000000000000000000 ) ) ;
#58249 = CARTESIAN_POINT ( 'NONE',  ( 9.509901345851000443, 5.077442745148000647, 8.469003100811999474 ) ) ;
#58251 = CARTESIAN_POINT ( 'NONE',  ( 10.74379975933729980, 5.078682052940000524, -7.128873141726999485 ) ) ;
#58252 = AXIS2_PLACEMENT_3D ( 'NONE', #56069, #8179, #55040 ) ;
#58253 = EDGE_CURVE ( 'NONE', #49595, #32140, #58627, .T. ) ;
#58254 = CARTESIAN_POINT ( 'NONE',  ( 25.31133132558300147, -11.20189781360999959, 3.316394190663999986 ) ) ;
#58255 = CARTESIAN_POINT ( 'NONE',  ( 8.819151519676999840, 4.021721698617580110, -8.504175633905001419 ) ) ;
#58256 = CARTESIAN_POINT ( 'NONE',  ( 17.84384701673185702, 0.6598665579121832936, 12.58271022457860688 ) ) ;
#58257 = CARTESIAN_POINT ( 'NONE',  ( 7.081534928999000833, -0.4954122222813999721, 1.324342293603000043 ) ) ;
#58258 = CARTESIAN_POINT ( 'NONE',  ( 11.09999999999999964, 4.000000000000000000, -7.500000000000000000 ) ) ;
#58259 = EDGE_LOOP ( 'NONE', ( #67490, #43274, #41550, #24758 ) ) ;
#58260 = CARTESIAN_POINT ( 'NONE',  ( 8.251331853209000755, -5.773185758034999893, 7.141496747382000798 ) ) ;
#58261 = CARTESIAN_POINT ( 'NONE',  ( 8.822164158776001130, 2.644017913812000131, -7.838184857420000817 ) ) ;
#58262 = CARTESIAN_POINT ( 'NONE',  ( 17.99827832423966711, 3.095912246742684282, 13.65340184222058184 ) ) ;
#58263 = DIRECTION ( 'NONE',  ( 0.000000000000000000, -0.2588190451024927063, 0.9659258262890757507 ) ) ;
#58264 = ORIENTED_EDGE ( 'NONE', *, *, #49874, .F. ) ;
#58265 = VECTOR ( 'NONE', #1410, 999.9999999999998863 ) ;
#58266 = CARTESIAN_POINT ( 'NONE',  ( 18.44495723965300016, 2.860707309908000262, 12.13834028902000028 ) ) ;
#58267 = ADVANCED_FACE ( 'NONE', ( #3343, #35177 ), #35518, .F. ) ;
#58268 = CARTESIAN_POINT ( 'NONE',  ( 11.27745123989519982, 4.410212499603100689, 6.707778874960499849 ) ) ;
#58269 = CARTESIAN_POINT ( 'NONE',  ( 10.34939834122999969, 2.653159779809000085, -7.312415497503999440 ) ) ;
#58270 = ORIENTED_EDGE ( 'NONE', *, *, #36018, .F. ) ;
#58271 = CARTESIAN_POINT ( 'NONE',  ( 9.185590450029501142, 5.092272840597503070, -6.870462550877411090 ) ) ;
#58272 = CARTESIAN_POINT ( 'NONE',  ( 18.00435067849408810, -1.907656978620086763, 12.45493970930050764 ) ) ;
#58273 = CARTESIAN_POINT ( 'NONE',  ( 11.33041235500449950, 3.057642534728299832, 8.363295307663500822 ) ) ;
#58274 = CARTESIAN_POINT ( 'NONE',  ( 7.954963149567436886, -4.950001034494477814, 6.428732759487574278 ) ) ;
#58275 = CARTESIAN_POINT ( 'NONE',  ( 7.694010841228000608, 5.850290547079999293, 6.784176679236000318 ) ) ;
#58276 = VERTEX_POINT ( 'NONE', #36538 ) ;
#58277 = DIRECTION ( 'NONE',  ( 0.000000000000000000, 0.000000000000000000, -1.000000000000000000 ) ) ;
#58278 = CARTESIAN_POINT ( 'NONE',  ( 5.699994923231000321, 12.50864296698000011, 2.924709704137000266 ) ) ;
#58279 = CARTESIAN_POINT ( 'NONE',  ( 8.541367865291375594, -3.305226939453190127, 5.905633504331038175 ) ) ;
#58280 = CARTESIAN_POINT ( 'NONE',  ( 10.79683585285767577, -3.460706475588385178, -8.187933206668011721 ) ) ;
#58281 = ORIENTED_EDGE ( 'NONE', *, *, #18232, .F. ) ;
#58282 = CARTESIAN_POINT ( 'NONE',  ( 16.04731601457200085, -3.899361801049999965, -11.84592592973999992 ) ) ;
#58283 = FACE_OUTER_BOUND ( 'NONE', #58033, .T. ) ;
#58284 = EDGE_LOOP ( 'NONE', ( #56144, #44577, #40755, #54796 ) ) ;
#58285 = CARTESIAN_POINT ( 'NONE',  ( 10.10226354018233330, -2.907767014557176566, 6.870476274536374106 ) ) ;
#58286 = CARTESIAN_POINT ( 'NONE',  ( 24.56713313357033002, -8.731543158497419910, -8.723146645339960870 ) ) ;
#58287 = PLANE ( 'NONE',  #7661 ) ;
#58288 = CARTESIAN_POINT ( 'NONE',  ( 9.536892889968999754, -5.099406281193999746, -6.669356233738001016 ) ) ;
#58289 = LINE ( 'NONE', #5150, #1477 ) ;
#58290 = CARTESIAN_POINT ( 'NONE',  ( 10.97635090131019986, 4.999207052587699707, -8.118017011233499503 ) ) ;
#58291 = CARTESIAN_POINT ( 'NONE',  ( 11.59590547754519996, -2.684394667508000154, 7.458246194669389872 ) ) ;
#58292 = CARTESIAN_POINT ( 'NONE',  ( 12.78418516728948973, 3.124999463064650040, -12.28374650604039964 ) ) ;
#58293 = CARTESIAN_POINT ( 'NONE',  ( 10.96887750876899936, -4.692271380433699512, 6.425720373262999274 ) ) ;
#58294 = ORIENTED_EDGE ( 'NONE', *, *, #66043, .F. ) ;
#58295 = CARTESIAN_POINT ( 'NONE',  ( 7.229676658770999964, 2.630487280353000390, 6.995957894972000268 ) ) ;
#58296 = EDGE_LOOP ( 'NONE', ( #18778, #64538, #7277, #8676, #37518 ) ) ;
#58297 = B_SPLINE_CURVE_WITH_KNOTS ( 'NONE', 3,
 ( #23154, #54273, #65797, #48694 ),
 .UNSPECIFIED., .F., .F.,
 ( 4, 4 ),
 ( 0.000000000000000000, 1.000000000000000000 ),
 .UNSPECIFIED. ) ;
#58298 = CARTESIAN_POINT ( 'NONE',  ( 15.40000000001299973, -8.815237407733999220, -7.616696375847999967 ) ) ;
#58299 = CARTESIAN_POINT ( 'NONE',  ( 8.802620559624999785, -3.975070057433999438, 9.483761758588999058 ) ) ;
#58300 = CARTESIAN_POINT ( 'NONE',  ( 9.099999986286999132, -4.750000013710600655, 7.500000000038047787 ) ) ;
#58301 = ORIENTED_EDGE ( 'NONE', *, *, #54779, .T. ) ;
#58302 = CARTESIAN_POINT ( 'NONE',  ( 12.76350962112090137, -3.123958135104670575, -12.28404825260450473 ) ) ;
#58303 = CARTESIAN_POINT ( 'NONE',  ( 24.67921311619700120, 3.567517360056999820, 12.13750603036999998 ) ) ;
#58304 = CARTESIAN_POINT ( 'NONE',  ( 23.59999443371599881, 2.915558930973999985, 13.58549620949000136 ) ) ;
#58305 = EDGE_CURVE ( 'NONE', #38378, #3659, #41443, .T. ) ;
#58306 = CARTESIAN_POINT ( 'NONE',  ( 10.65434687351636178, 5.250000000000002665, 7.663624617374463988 ) ) ;
#58307 = CARTESIAN_POINT ( 'NONE',  ( 12.12605828839494038, -2.774939115234953846, -13.72225238672861281 ) ) ;
#58308 = ADVANCED_FACE ( 'NONE', ( #25357 ), #56840, .T. ) ;
#58309 = CARTESIAN_POINT ( 'NONE',  ( 10.53057053952199951, -4.340412141385700195, -6.703496287302799672 ) ) ;
#58310 = EDGE_CURVE ( 'NONE', #68324, #50475, #47001, .T. ) ;
#58311 = CARTESIAN_POINT ( 'NONE',  ( 7.103945121988524569, 0.6535162433261614279, -1.132143873356089570 ) ) ;
#58312 = CARTESIAN_POINT ( 'NONE',  ( 17.82398025068296832, -3.148553868299628800, 12.20027175159510513 ) ) ;
#58313 = ORIENTED_EDGE ( 'NONE', *, *, #21131, .T. ) ;
#58314 = ORIENTED_EDGE ( 'NONE', *, *, #15474, .T. ) ;
#58315 = CIRCLE ( 'NONE', #50539, 1.049999999999999822 ) ;
#58316 = DIRECTION ( 'NONE',  ( 0.000000000000000000, 0.000000000000000000, 1.000000000000000000 ) ) ;
#58317 = CARTESIAN_POINT ( 'NONE',  ( 5.000000000000000000, 0.8000000000000000444, -3.149999999999999911 ) ) ;
#58318 = CARTESIAN_POINT ( 'NONE',  ( 11.09999999999999964, -2.649999999999999911, 7.500000000000000000 ) ) ;
#58319 = CARTESIAN_POINT ( 'NONE',  ( 10.11859053700000111, 3.393394511985999618, -5.921995869926000466 ) ) ;
#58320 = CARTESIAN_POINT ( 'NONE',  ( 18.29983863916000075, 2.861762957209999847, -11.98830831200999825 ) ) ;
#58321 = CARTESIAN_POINT ( 'NONE',  ( 18.05707515698803078, 2.118723117023476821, -12.53248177915881278 ) ) ;
#58322 = CIRCLE ( 'NONE', #4709, 1.600000000000000089 ) ;
#58323 = CARTESIAN_POINT ( 'NONE',  ( 8.076862866721999268, 2.879478799711000292, -6.727223656603999125 ) ) ;
#58324 = CARTESIAN_POINT ( 'NONE',  ( 17.92325670915549907, -1.853371315644311901, -12.46300045701685910 ) ) ;
#58325 = VERTEX_POINT ( 'NONE', #25701 ) ;
#58326 = CARTESIAN_POINT ( 'NONE',  ( 8.831347292302233143, 5.765877224304255755, -7.300045774259967146 ) ) ;
#58327 = CARTESIAN_POINT ( 'NONE',  ( 12.35410221487145499, -2.932869452542228306, 12.34012701440640214 ) ) ;
#58328 = CARTESIAN_POINT ( 'NONE',  ( 8.608142887202433258, 5.166153502812370846, -8.205198856529275275 ) ) ;
#58329 = CARTESIAN_POINT ( 'NONE',  ( 9.687870098586998324, 5.912263966150999472, 7.772301113561999486 ) ) ;
#58330 = CARTESIAN_POINT ( 'NONE',  ( 11.89700581613019992, -3.130347327833300053, 6.941573685175900010 ) ) ;
#58331 = CARTESIAN_POINT ( 'NONE',  ( 8.921135841230999119, 3.292387953886000140, -6.294868737226000377 ) ) ;
#58332 = CARTESIAN_POINT ( 'NONE',  ( 11.51518179236248862, 3.819003318705799899, -6.652923384986699773 ) ) ;
#58333 = CARTESIAN_POINT ( 'NONE',  ( 12.37008254743958524, -0.4489258298041881590, 12.68932177688764362 ) ) ;
#58334 = DIRECTION ( 'NONE',  ( 0.000000000000000000, 0.000000000000000000, -1.000000000000000000 ) ) ;
#58335 = DIRECTION ( 'NONE',  ( 0.000000000000000000, 0.9553735099700838562, 0.2954005017724949944 ) ) ;
#58336 = FACE_OUTER_BOUND ( 'NONE', #30597, .T. ) ;
#58337 = B_SPLINE_SURFACE_WITH_KNOTS ( 'NONE', 3, 3, ( 
 ( #58814, #58470, #32941, #54252 ),
 ( #38525, #52887, #21072, #31568 ),
 ( #42740, #4986, #47986, #68959 ),
 ( #6353, #15822, #27008, #53229 ),
 ( #42402, #10575, #22092, #64385 ),
 ( #53573, #49017, #1124, #37152 ),
 ( #27701, #32596, #16164, #26672 ),
 ( #53911, #22438, #63710, #5328 ),
 ( #16506, #6011, #64044, #27350 ),
 ( #32263, #48326, #431, #48673 ) ),
 .UNSPECIFIED., .F., .F., .F.,
 ( 4, 1, 1, 1, 1, 1, 1, 4 ),
 ( 4, 4 ),
 ( 0.07063076901675999220, 0.1428571428570999946, 0.2857142857143000203, 0.4285714285713999594, 0.5714285714286000406, 0.7142857142856999797, 0.8571428571429000609, 0.9582423226859000387 ),
 ( -0.1917799910644999994, 1.191756862851000021 ),
 .UNSPECIFIED. ) ;
#58338 = ORIENTED_EDGE ( 'NONE', *, *, #52874, .F. ) ;
#58339 = CARTESIAN_POINT ( 'NONE',  ( 9.567560841232999991, 5.349936549139000519, -7.138437102151999447 ) ) ;
#58340 = CARTESIAN_POINT ( 'NONE',  ( 7.282926398363001042, -0.9657653571052000618, 0.5483950127678999253 ) ) ;
#58341 = CARTESIAN_POINT ( 'NONE',  ( 11.00448450226549113, -2.648588503021471308, 6.387884280188352193 ) ) ;
#58342 = CARTESIAN_POINT ( 'NONE',  ( 3.500000000000000000, 3.499738125128000199, -0.04281419768536000314 ) ) ;
#58343 = DIRECTION ( 'NONE',  ( 1.000000000000000000, 0.000000000000000000, 0.000000000000000000 ) ) ;
#58344 = CARTESIAN_POINT ( 'NONE',  ( 10.21462282008599942, -3.476853648246800432, -8.343818446627699004 ) ) ;
#58345 = ORIENTED_EDGE ( 'NONE', *, *, #4218, .T. ) ;
#58346 = AXIS2_PLACEMENT_3D ( 'NONE', #54958, #55306, #23487 ) ;
#58347 = DIRECTION ( 'NONE',  ( 0.000000000000000000, 0.000000000000000000, -1.000000000000000000 ) ) ;
#58348 = CARTESIAN_POINT ( 'NONE',  ( 7.694010841228000608, 5.850290547079999293, 6.784176679236000318 ) ) ;
#58349 = EDGE_CURVE ( 'NONE', #25195, #41892, #11080, .T. ) ;
#58352 = CARTESIAN_POINT ( 'NONE',  ( 13.55458079702099994, -9.509022223680998920, -7.924557572090001223 ) ) ;
#58351 = CARTESIAN_POINT ( 'NONE',  ( 9.509454719593000149, 3.116293075258000478, -6.208411413796000033 ) ) ;
#58350 = PRODUCT_DEFINITION_CONTEXT ( 'detailed design', #39623, 'design' ) ;
#58353 = CARTESIAN_POINT ( 'NONE',  ( 18.18005043852540581, -2.520325007585945354, 13.66916896904711898 ) ) ;
#58354 = ORIENTED_EDGE ( 'NONE', *, *, #21431, .T. ) ;
#58355 = CARTESIAN_POINT ( 'NONE',  ( 10.96207813434000045, 5.399835028078000754, 7.743264559064000352 ) ) ;
#58356 = CARTESIAN_POINT ( 'NONE',  ( 18.02623320712471511, -2.911124530445448055, -13.57757619639374624 ) ) ;
#58357 = CARTESIAN_POINT ( 'NONE',  ( 11.78594988689359901, 4.393436444036099786, 6.728309553046099012 ) ) ;
#58358 = CARTESIAN_POINT ( 'NONE',  ( 7.100000000000000533, 12.03770622561999915, 3.722046322334000124 ) ) ;
#58359 = CARTESIAN_POINT ( 'NONE',  ( 8.218894353209000414, -3.011617647609999615, 8.801438026873999121 ) ) ;
#58360 = ORIENTED_EDGE ( 'NONE', *, *, #60057, .F. ) ;
#58361 = CARTESIAN_POINT ( 'NONE',  ( 8.096551658772000337, 5.061727314042999915, 5.824077473724000420 ) ) ;
#58363 = CARTESIAN_POINT ( 'NONE',  ( 10.72129555961999792, -4.673507771948999689, -5.778404201896999659 ) ) ;
#58362 = CARTESIAN_POINT ( 'NONE',  ( 10.47683719568447636, 4.186288604638629174, -6.645958924689391090 ) ) ;
#58364 = CARTESIAN_POINT ( 'NONE',  ( 7.593455520019030125, -4.408259056465409387, 5.809061053540682806 ) ) ;
#58365 = VECTOR ( 'NONE', #58116, 1000.000000000000000 ) ;
#58366 = CARTESIAN_POINT ( 'NONE',  ( 18.02961597941495953, -0.4069473555476081916, 13.89198745891521192 ) ) ;
#58367 = CARTESIAN_POINT ( 'NONE',  ( 2.167611958084000090, -0.2760264376601999636, -3.247374627496999899 ) ) ;
#58368 = VERTEX_POINT ( 'NONE', #67998 ) ;
#58369 = CARTESIAN_POINT ( 'NONE',  ( 9.393930206848999376, 2.750000000000000000, -7.500000000000000000 ) ) ;
#58370 = CARTESIAN_POINT ( 'NONE',  ( 11.95764291764649911, -5.132124077409000229, 7.639947095788999221 ) ) ;
#58371 = CARTESIAN_POINT ( 'NONE',  ( 9.910633732652998518, 2.107262079134000210, 7.885285091859000062 ) ) ;
#58372 = CARTESIAN_POINT ( 'NONE',  ( 10.91610672858429965, 3.088399709291500095, 8.185766014210599906 ) ) ;
#58373 = EDGE_LOOP ( 'NONE', ( #28566, #21790, #64647, #51932 ) ) ;
#58374 = CARTESIAN_POINT ( 'NONE',  ( 24.13789385032118773, -3.328480681758700488, 12.49557795887629119 ) ) ;
#58375 = FACE_OUTER_BOUND ( 'NONE', #59188, .T. ) ;
#58376 = CARTESIAN_POINT ( 'NONE',  ( 12.01145123989533126, -3.394760891061399999, 6.331134574721999364 ) ) ;
#58377 = CARTESIAN_POINT ( 'NONE',  ( 24.95409859149600251, -3.532259266401000186, -11.87003396491999929 ) ) ;
#58378 = CARTESIAN_POINT ( 'NONE',  ( 17.82373361328025041, -1.839709763185445546, 13.87859827090101383 ) ) ;
#58379 = CARTESIAN_POINT ( 'NONE',  ( 18.05125194750646855, 2.880159330030322096, -13.58544989776502554 ) ) ;
#58380 = ORIENTED_EDGE ( 'NONE', *, *, #20066, .F. ) ;
#58381 = CARTESIAN_POINT ( 'NONE',  ( 16.00806624337635142, -9.235483320791386674, -8.460674029563278964 ) ) ;
#58382 = CARTESIAN_POINT ( 'NONE',  ( 24.30000000000000071, 2.548720605937000006, -12.21654710926000220 ) ) ;
#58383 = ORIENTED_EDGE ( 'NONE', *, *, #1699, .F. ) ;
#58384 = CARTESIAN_POINT ( 'NONE',  ( 10.32992855215000105, -4.904916250652000542, 4.624355442463000010 ) ) ;
#58385 = CARTESIAN_POINT ( 'NONE',  ( 10.87103032197929942, 4.583685623598699799, 8.316248703309600643 ) ) ;
#58386 = CARTESIAN_POINT ( 'NONE',  ( 9.758140238852000437, 2.901378080241999946, 6.555076849497999625 ) ) ;
#58387 = CARTESIAN_POINT ( 'NONE',  ( 10.90421423234000109, 3.863780721621000058, -9.185084890147001246 ) ) ;
#58388 = CARTESIAN_POINT ( 'NONE',  ( 8.751496707488000126, -3.918323994020610268, -8.356402621895700378 ) ) ;
#58389 = EDGE_CURVE ( 'NONE', #57460, #10927, #26941, .T. ) ;
#58390 = CARTESIAN_POINT ( 'NONE',  ( 9.799258316471000541, -4.057329063942999525, 9.430691159271001212 ) ) ;
#58391 = EDGE_CURVE ( 'NONE', #47477, #44536, #47033, .T. ) ;
#58392 = CARTESIAN_POINT ( 'NONE',  ( 17.63678281077947219, 0.6199686954221031998, -12.67962180225518942 ) ) ;
#58393 = CARTESIAN_POINT ( 'NONE',  ( 12.23606560776517860, 2.758669204905062067, -12.38755309841745422 ) ) ;
#58394 = CARTESIAN_POINT ( 'NONE',  ( 10.47718582084299932, -4.656536239972400182, -6.741111985563299491 ) ) ;
#58395 = EDGE_CURVE ( 'NONE', #33299, #63876, #53649, .T. ) ;
#58396 = EDGE_CURVE ( 'NONE', #35557, #29557, #14434, .T. ) ;
#58397 = CARTESIAN_POINT ( 'NONE',  ( 8.855420280411999912, 5.633477595780999714, 7.451234169193000412 ) ) ;
#58398 = VERTEX_POINT ( 'NONE', #64125 ) ;
#58399 = AXIS2_PLACEMENT_3D ( 'NONE', #63231, #52758, #4165 ) ;
#58400 = CARTESIAN_POINT ( 'NONE',  ( 11.12299956498149811, 5.207010770456999893, 7.174999999999999822 ) ) ;
#58401 = CARTESIAN_POINT ( 'NONE',  ( 0.000000000000000000, 0.000000000000000000, 0.000000000000000000 ) ) ;
#58402 = CARTESIAN_POINT ( 'NONE',  ( 25.10987708584536904, 8.510208471453900358, 8.211061621397103494 ) ) ;
#58403 = CARTESIAN_POINT ( 'NONE',  ( 17.55505043854143565, 1.760910691117812066, 12.47634535983623039 ) ) ;
#58404 = CARTESIAN_POINT ( 'NONE',  ( 11.07128326594000001, 6.555132067871999979, 5.493445694320000072 ) ) ;
#58405 = CARTESIAN_POINT ( 'NONE',  ( 11.13602668609999924, 9.532506022458999695, 6.386669746941000092 ) ) ;
#58406 = DIRECTION ( 'NONE',  ( 1.000000000000000000, 0.000000000000000000, 0.000000000000000000 ) ) ;
#58407 = DIRECTION ( 'NONE',  ( 1.000000000000000000, 0.000000000000000000, 0.000000000000000000 ) ) ;
#58408 = ORIENTED_EDGE ( 'NONE', *, *, #60102, .F. ) ;
#58409 = CARTESIAN_POINT ( 'NONE',  ( 12.30583355256791300, -1.958333444515658606, 12.44688698484233669 ) ) ;
#58410 = CARTESIAN_POINT ( 'NONE',  ( 10.16360887879199915, -4.258572737033900601, -6.387851364408000165 ) ) ;
#58411 = DIRECTION ( 'NONE',  ( 0.000000000000000000, -1.000000000000000000, 0.000000000000000000 ) ) ;
#58412 = EDGE_CURVE ( 'NONE', #40911, #6003, #67784, .T. ) ;
#58413 = CARTESIAN_POINT ( 'NONE',  ( 9.261668853699999815, -2.944250413017999612, 6.507387951280999339 ) ) ;
#58414 = CARTESIAN_POINT ( 'NONE',  ( 11.22749279009020107, -4.225282629687599822, 6.663611138821799784 ) ) ;
#58415 = CARTESIAN_POINT ( 'NONE',  ( 12.68688152457048268, 0.7100593550699842993, 12.57997761080729759 ) ) ;
#58416 = AXIS2_PLACEMENT_3D ( 'NONE', #48952, #28316, #44412 ) ;
#58417 = CARTESIAN_POINT ( 'NONE',  ( 0.5734915348667000146, -3.063090672237000156, -0.9584583608479999572 ) ) ;
#58418 = CARTESIAN_POINT ( 'NONE',  ( 4.974988406525884699, 0.3003884035085989668, -1.160233976767930386 ) ) ;
#58419 = CARTESIAN_POINT ( 'NONE',  ( 12.08482599452294437, 2.564444806221811479, 12.33627826672299044 ) ) ;
#58421 = CARTESIAN_POINT ( 'NONE',  ( 9.110944094209999733, 5.100000000000000533, -6.571291218949999902 ) ) ;
#58420 = CARTESIAN_POINT ( 'NONE',  ( 10.11295058442699890, 4.453199839589800035, -6.451980747609000311 ) ) ;
#58422 = CARTESIAN_POINT ( 'NONE',  ( 10.99410672858429905, 3.198097575668700010, -6.896755974168000236 ) ) ;
#58423 = CARTESIAN_POINT ( 'NONE',  ( 25.55279130549196509, 8.264493201100965081, 8.081392654661549102 ) ) ;
#58424 = CARTESIAN_POINT ( 'NONE',  ( 10.54684221959000112, 3.691673619534999951, -9.157283848447001162 ) ) ;
#58425 = CARTESIAN_POINT ( 'NONE',  ( 8.997405316140000053, 3.728406863338599830, -8.750048621292000561 ) ) ;
#58427 = CARTESIAN_POINT ( 'NONE',  ( 18.12841930325617668, -0.2489729014350941239, 12.69672092237004257 ) ) ;
#58426 = CARTESIAN_POINT ( 'NONE',  ( 18.02668091122101401, -11.82887279600184272, 3.432551977438183410 ) ) ;
#58428 = B_SPLINE_CURVE_WITH_KNOTS ( 'NONE', 3,
 ( #57130, #42431, #51880, #25316 ),
 .UNSPECIFIED., .F., .F.,
 ( 4, 4 ),
 ( 0.000000000000000000, 1.000000000000000000 ),
 .UNSPECIFIED. ) ;
#58429 = CARTESIAN_POINT ( 'NONE',  ( 10.98768472638000127, 7.408460511344000743, 6.159405790617999976 ) ) ;
#58430 = ORIENTED_EDGE ( 'NONE', *, *, #51828, .T. ) ;
#58431 = CARTESIAN_POINT ( 'NONE',  ( 0.9287915396056000139, -1.955279592509000075, 2.607329530612999768 ) ) ;
#58432 = DIRECTION ( 'NONE',  ( 1.000000000000000000, 0.000000000000000000, 0.000000000000000000 ) ) ;
#58433 = EDGE_CURVE ( 'NONE', #855, #52478, #11945, .T. ) ;
#58434 = CARTESIAN_POINT ( 'NONE',  ( 9.399846034910298798, 5.293376409283213846, -8.716279758284748880 ) ) ;
#58435 = CARTESIAN_POINT ( 'NONE',  ( 9.275076168957998135, 3.490299597736799875, 6.634524523592600254 ) ) ;
#58436 = CARTESIAN_POINT ( 'NONE',  ( 1.593676743165000117E-07, 2.574999840614999425, 3.034233182443000263E-10 ) ) ;
#58437 = EDGE_CURVE ( 'NONE', #46332, #53670, #39441, .T. ) ;
#58438 = CARTESIAN_POINT ( 'NONE',  ( 12.17997927555901505, -2.482106649064418136, 13.67725710540907613 ) ) ;
#58439 = CARTESIAN_POINT ( 'NONE',  ( 12.19551626499556463, 2.360211740085632393, 13.70208339271400355 ) ) ;
#58440 = CARTESIAN_POINT ( 'NONE',  ( 23.58444653190300144, 2.899227940640999979, -13.63439735100000050 ) ) ;
#58441 = ORIENTED_EDGE ( 'NONE', *, *, #40286, .T. ) ;
#58442 = B_SPLINE_CURVE_WITH_KNOTS ( 'NONE', 3,
 ( #29873, #19016, #24946, #30208 ),
 .UNSPECIFIED., .F., .F.,
 ( 4, 4 ),
 ( 0.000000000000000000, 0.1836163425310814723 ),
 .UNSPECIFIED. ) ;
#58443 = AXIS2_PLACEMENT_3D ( 'NONE', #46184, #25543, #45502 ) ;
#58444 = CARTESIAN_POINT ( 'NONE',  ( 5.048003487648000664, 0.3164883147558000265, -1.235560760781999834 ) ) ;
#58445 = CARTESIAN_POINT ( 'NONE',  ( 9.453329965421998438, -4.888489908445900589, -8.420309768537698858 ) ) ;
#58446 = AXIS2_PLACEMENT_3D ( 'NONE', #36330, #31779, #64259 ) ;
#58447 = DIRECTION ( 'NONE',  ( 0.000000000000000000, 0.007439385635787961089, 0.9999723273877941798 ) ) ;
#58448 = DIRECTION ( 'NONE',  ( 0.000000000000000000, -0.9916377111174248249, -0.1290528957048032721 ) ) ;
#58449 = CARTESIAN_POINT ( 'NONE',  ( 18.15862102414876489, 2.662578152609974769, -12.41223253473083332 ) ) ;
#58450 = CARTESIAN_POINT ( 'NONE',  ( 13.99999999485600277, -9.471999751521998689, -8.194948195317001804 ) ) ;
#58451 = CARTESIAN_POINT ( 'NONE',  ( 17.71871529296970493, 3.104542143063796722, 12.28994062198843906 ) ) ;
#58452 = CYLINDRICAL_SURFACE ( 'NONE', #68042, 1.350000000000000089 ) ;
#58453 = CARTESIAN_POINT ( 'NONE',  ( 24.34833292637366853, 3.256146932298328522, -12.15210578825087140 ) ) ;
#58454 = CARTESIAN_POINT ( 'NONE',  ( 11.18114303127866727, 3.379301870158037069, -8.119425260350670470 ) ) ;
#58455 = CARTESIAN_POINT ( 'NONE',  ( 11.50001544675000176, -12.52500000000000213, 1.310230436065862980 ) ) ;
#58456 = CARTESIAN_POINT ( 'NONE',  ( 24.26257012332692398, 8.985986007774535267, -8.985987282385920594 ) ) ;
#58457 = DIRECTION ( 'NONE',  ( -1.000000000000000000, 0.000000000000000000, -5.088522196198629516E-14 ) ) ;
#58458 = CARTESIAN_POINT ( 'NONE',  ( 24.22094041469999937, 12.17087951192999995, -3.345634150892999870 ) ) ;
#58459 = ORIENTED_EDGE ( 'NONE', *, *, #17346, .T. ) ;
#58460 = CARTESIAN_POINT ( 'NONE',  ( 8.233179719589999834, 5.203550244299999683, -8.391678825488000371 ) ) ;
#58462 = VECTOR ( 'NONE', #35840, 1000.000000000000000 ) ;
#58461 = CARTESIAN_POINT ( 'NONE',  ( 12.03564291764652872, -4.995889373412399692, 7.623106493640399606 ) ) ;
#58463 = ORIENTED_EDGE ( 'NONE', *, *, #28754, .F. ) ;
#58464 = CARTESIAN_POINT ( 'NONE',  ( 9.099999999999999645, -12.35000000006999876, 0.000000000000000000 ) ) ;
#58465 = CARTESIAN_POINT ( 'NONE',  ( 11.61759063708296047, -2.782734359457999851, -7.842242470354300110 ) ) ;
#58466 = ORIENTED_EDGE ( 'NONE', *, *, #29936, .F. ) ;
#58467 = CARTESIAN_POINT ( 'NONE',  ( 11.34523293495530005, 2.684794526488000432, 7.552870914315270134 ) ) ;
#58469 = CARTESIAN_POINT ( 'NONE',  ( 9.292835841232999883, 5.200883864107000321, -6.027780766890000308 ) ) ;
#58468 = CONICAL_SURFACE ( 'NONE', #2681, 12.69999976913000062, 0.7853981453603698926 ) ;
#58470 = CARTESIAN_POINT ( 'NONE',  ( 17.76418844530500252, -3.313976920866999798, 11.22406790378000174 ) ) ;
#58471 = B_SPLINE_CURVE_WITH_KNOTS ( 'NONE', 3,
 ( #61693, #19387, #23952, #61013, #13131, #18711 ),
 .UNSPECIFIED., .F., .F.,
 ( 4, 2, 4 ),
 ( 0.000000000000000000, 0.5000000000000000000, 1.000000000000000000 ),
 .UNSPECIFIED. ) ;
#58472 = CARTESIAN_POINT ( 'NONE',  ( 11.59603632436369125, -4.842640371965599932, -7.303218851299499548 ) ) ;
#58473 = CARTESIAN_POINT ( 'NONE',  ( 12.25734203442973502, 0.3012395218291776811, -13.89560941714155540 ) ) ;
#58474 = CARTESIAN_POINT ( 'NONE',  ( 11.60000000000000142, -4.094072174251358831, -6.471240206706526443 ) ) ;
#58475 = CARTESIAN_POINT ( 'NONE',  ( 13.05728973496400336, 11.72286803092000085, 1.966956593348999860 ) ) ;
#58476 = ORIENTED_EDGE ( 'NONE', *, *, #19676, .T. ) ;
#58477 = EDGE_CURVE ( 'NONE', #26858, #58783, #59492, .T. ) ;
#58478 = ADVANCED_FACE ( 'NONE', ( #37227 ), #22513, .T. ) ;
#58479 =( BOUNDED_SURFACE ( )  B_SPLINE_SURFACE ( 3, 3, ( 
 ( #63465, #67675, #37254, #41471, #35880, #30638, #51948, #41129, #69066 ),
 ( #25043, #26078, #62778, #62441, #47756, #20830, #21172, #14562, #15922 ),
 ( #25384, #46722, #15242, #58573, #30302, #51609, #3704, #36916, #46375 ),
 ( #10335, #31671, #9642, #68366, #41811, #28146, #43883, #59952, #17305 ) ),
 .UNSPECIFIED., .F., .F., .T. ) 
 B_SPLINE_SURFACE_WITH_KNOTS ( ( 4, 4 ),
 ( 4, 1, 1, 1, 1, 1, 4 ),
 ( 0.000000000000000000, 1.000000000000000000 ),
 ( 0.8657679006235999841, 0.8794646334505999974, 0.9056938526918999477, 0.9344431701380999655, 0.9658387281735000274, 1.000000000000000000, 1.004641266558000012 ),
 .UNSPECIFIED. ) 
 GEOMETRIC_REPRESENTATION_ITEM ( )  RATIONAL_B_SPLINE_SURFACE ( (
 ( 1.157353709788000007, 1.157353709788000007, 1.157353709788000007, 1.157353709788000007, 1.157353709788000007, 1.157353709788000007, 1.157353709788000007, 1.157353709788000007, 1.157353709788000007),
 ( 0.9475487634039000406, 0.9475487634039000406, 0.9475487634039000406, 0.9475487634039000406, 0.9475487634039000406, 0.9475487634039000406, 0.9475487634039000406, 0.9475487634039000406, 0.9475487634039000406),
 ( 0.9475487634039000406, 0.9475487634039000406, 0.9475487634039000406, 0.9475487634039000406, 0.9475487634039000406, 0.9475487634039000406, 0.9475487634039000406, 0.9475487634039000406, 0.9475487634039000406),
 ( 1.157353709788000007, 1.157353709788000007, 1.157353709788000007, 1.157353709788000007, 1.157353709788000007, 1.157353709788000007, 1.157353709788000007, 1.157353709788000007, 1.157353709788000007) ) ) 
 REPRESENTATION_ITEM ( '' )  SURFACE ( )  );
#58480 = CARTESIAN_POINT ( 'NONE',  ( 8.704862649514709005, 2.649860810595531468, 7.852951878456049251 ) ) ;
#58481 = ORIENTED_EDGE ( 'NONE', *, *, #39850, .T. ) ;
#58482 = CARTESIAN_POINT ( 'NONE',  ( 10.77934687351631382, 3.836375382625536012, -6.249999999999999112 ) ) ;
#58483 = ORIENTED_EDGE ( 'NONE', *, *, #49648, .T. ) ;
#58484 = CARTESIAN_POINT ( 'NONE',  ( 8.693455549952998851, 4.995562869655000071, 8.303267676773000261 ) ) ;
#58485 = CARTESIAN_POINT ( 'NONE',  ( 17.68557836066964839, 11.86191914806434333, -3.298674357360816156 ) ) ;
#58486 = B_SPLINE_SURFACE_WITH_KNOTS ( 'NONE', 3, 3, ( 
 ( #15866, #21120, #69007, #27060, #37198, #42445, #52585, #32646, #31963, #53620, #63754, #52935, #10620, #5717, #37534, #27398, #11309, #42787, #53958, #59205, #26369, #47696, #43130, #41756, #6061, #5380, #53279, #5030, #48373, #48031, #58516, #63410, #21797, #48727, #26719 ),
 ( #63057, #137, #31613, #21451, #64096, #829, #482, #15534, #64435, #16557, #16210, #15184, #58865, #10971, #36508, #9937, #57829, #36858, #20773, #32310, #37885, #31274, #47349, #4678, #58178, #26020, #68655, #42105, #10280, #60594, #65129, #54657, #17250, #6407, #44182 ),
 ( #55005, #2216, #39271, #7800, #12701, #29140, #28443, #34038, #60941, #55350, #7447, #49066, #50447, #12354, #28799, #33687, #60252, #23187, #1517, #65481, #43486, #55702, #44872, #23531, #50110, #11653, #59897, #43830, #66176, #38225, #59553, #7106, #1174, #32988, #18296 ),
 ( #13057, #17954, #54304, #39618, #27754, #22487, #17605, #49757, #1867, #38573, #64783, #38930, #34385, #12005, #6752, #44533, #65827, #22146, #16896, #33342, #28092, #49405, #22836, #34727, #8831, #18640, #61288, #8489, #18979, #20010, #46585, #67203, #30172, #24570, #56037 ) ),
 .UNSPECIFIED., .F., .F., .F.,
 ( 4, 4 ),
 ( 4, 1, 1, 1, 1, 1, 1, 1, 1, 1, 1, 1, 1, 1, 1, 1, 1, 1, 1, 1, 1, 1, 1, 1, 1, 1, 1, 1, 1, 1, 1, 1, 4 ),
 ( -0.1039086239011999951, 1.103908623900999864 ),
 ( -0.01933701211302999920, 0.01208563257065999909, 0.04350827725433999843, 0.07493092193802000645, 0.1063535666217000075, 0.1377762113054000204, 0.1691988559891000055, 0.2006215006727000150, 0.2320441453564000001, 0.2634667900400999851, 0.2948894347238000258, 0.3263120794074999553, 0.3577347240911999959, 0.3891573687748000054, 0.4205800134584999905, 0.4520026581421999756, 0.4834253028259000162, 0.5148479475096000568, 0.5462705921932000663, 0.5776932368768999959, 0.6091158815606000365, 0.6405385262443000771, 0.6719611709280000067, 0.7033838156117000473, 0.7348064602953000568, 0.7662291049789999864, 0.7976517496627000270, 0.8290743943464000676, 0.8604970390300999972, 0.8919196837138000378, 0.9233423283974000473, 0.9547649730810999769, 0.9861876177648000175 ),
 .UNSPECIFIED. ) ;
#58487 = CARTESIAN_POINT ( 'NONE',  ( 18.18005043835062295, -2.498838836691497534, -12.45183430368941835 ) ) ;
#58488 = CARTESIAN_POINT ( 'NONE',  ( 12.20096535489426870, 0.1616183441363953921, 13.89875400931294536 ) ) ;
#58489 = ORIENTED_EDGE ( 'NONE', *, *, #51913, .T. ) ;
#58490 = CARTESIAN_POINT ( 'NONE',  ( 11.95406170795600076, 11.84685177148000079, -3.896686237526999719 ) ) ;
#58491 = CARTESIAN_POINT ( 'NONE',  ( 18.26656969954900234, 11.60886806805999960, -4.031065632098000506 ) ) ;
#58492 = EDGE_CURVE ( 'NONE', #51766, #54068, #18359, .T. ) ;
#58493 = CARTESIAN_POINT ( 'NONE',  ( 10.31021345716899873, 4.636538040886300394, 6.921280946186199934 ) ) ;
#58494 = CARTESIAN_POINT ( 'NONE',  ( 11.09999999999999964, 4.000000000000000000, 7.500000000000000000 ) ) ;
#58495 = CIRCLE ( 'NONE', #59594, 12.35000000006999876 ) ;
#58496 = CARTESIAN_POINT ( 'NONE',  ( 9.494689158774999527, 2.824732249080000202, -8.992748220058999209 ) ) ;
#58497 = CARTESIAN_POINT ( 'NONE',  ( 18.19046715839422035, 12.06204093805255084, -3.374120125975932805 ) ) ;
#58498 = CARTESIAN_POINT ( 'NONE',  ( 10.26368921839999970, -4.794141574281000295, -8.804455889106000299 ) ) ;
#58499 = ORIENTED_EDGE ( 'NONE', *, *, #8797, .T. ) ;
#58500 = ORIENTED_EDGE ( 'NONE', *, *, #36389, .T. ) ;
#58501 = CARTESIAN_POINT ( 'NONE',  ( 10.98148521858999871, 5.115205842040000839, -4.906648178026999929 ) ) ;
#58502 = CARTESIAN_POINT ( 'NONE',  ( 8.616995677562000466, -4.876077402042000131, 5.996974966533000106 ) ) ;
#58503 = CARTESIAN_POINT ( 'NONE',  ( 11.09999999999999964, 5.449702572737000317, -5.124965750789000296 ) ) ;
#58504 = CARTESIAN_POINT ( 'NONE',  ( 7.000000000000000000, -7.526486366024999874, -3.526486366024999874 ) ) ;
#58505 = CARTESIAN_POINT ( 'NONE',  ( 11.55300581613033906, 5.107584469683000172, -8.211208432468300344 ) ) ;
#58506 = CARTESIAN_POINT ( 'NONE',  ( 9.788646554150998824, 4.419749732651400365, -8.258629096756299859 ) ) ;
#58508 = CARTESIAN_POINT ( 'NONE',  ( 10.27506785289999947, -3.374327226904999755, 5.003467443561000039 ) ) ;
#58507 = CARTESIAN_POINT ( 'NONE',  ( 10.61093802597399893, -4.522194782554399772, 8.357994702431799539 ) ) ;
#58509 = LINE ( 'NONE', #25667, #62045 ) ;
#58510 = ORIENTED_EDGE ( 'NONE', *, *, #68687, .T. ) ;
#58511 = CARTESIAN_POINT ( 'NONE',  ( 4.000000000000000000, 2.750000000000000000, 0.000000000000000000 ) ) ;
#58512 = CONICAL_SURFACE ( 'NONE', #67441, 3.249989426617000188, 0.7853950157668545540 ) ;
#58513 = CARTESIAN_POINT ( 'NONE',  ( 7.684934563448005740, -2.928065616737000720, 6.508603912219004251 ) ) ;
#58514 = CARTESIAN_POINT ( 'NONE',  ( 9.712899699504999873, -4.008306780893000187, -8.877926425468999128 ) ) ;
#58515 = CARTESIAN_POINT ( 'NONE',  ( 5.679181292414646087, -13.00268187323304225, -2.124261077943678355 ) ) ;
#58516 = CARTESIAN_POINT ( 'NONE',  ( 11.08492081570999943, -3.668392767032000013, 5.558160538745999801 ) ) ;
#58517 = EDGE_CURVE ( 'NONE', #5374, #24349, #16587, .T. ) ;
#58518 = CARTESIAN_POINT ( 'NONE',  ( 18.01273579184442752, 2.926031893962671049, -12.34206213438296551 ) ) ;
#58519 = CARTESIAN_POINT ( 'NONE',  ( 6.999998782146999332, 0.000000000000000000, 0.000000000000000000 ) ) ;
#58520 = LINE ( 'NONE', #14848, #10110 ) ;
#58521 = CARTESIAN_POINT ( 'NONE',  ( 7.531666666664000864, 4.679885623500713798, -6.320388375721750940 ) ) ;
#58522 = CARTESIAN_POINT ( 'NONE',  ( 9.687329965421998423, -4.602191201513400109, -8.123757726465999696 ) ) ;
#58523 = CARTESIAN_POINT ( 'NONE',  ( 6.204134283177999976, -1.390318139369000061, -0.4728033673814999727 ) ) ;
#58524 = CARTESIAN_POINT ( 'NONE',  ( 6.999999999999999112, 9.413677030445844807, -4.695585979740934057 ) ) ;
#58525 = CARTESIAN_POINT ( 'NONE',  ( 0.1499942179680000542, -0.3599680999393992664, -2.749953718116143087 ) ) ;
#58526 = ORIENTED_EDGE ( 'NONE', *, *, #17947, .F. ) ;
#58527 = CARTESIAN_POINT ( 'NONE',  ( 12.21327642329898389, -0.2013262877421473085, -12.69785743964336078 ) ) ;
#58528 = CARTESIAN_POINT ( 'NONE',  ( 10.08728840308773300, -2.899999999999999911, -6.305985889617788942 ) ) ;
#58529 = CARTESIAN_POINT ( 'NONE',  ( 11.00000000000000000, -4.968589424331200100, -7.174999999999999822 ) ) ;
#58530 = CARTESIAN_POINT ( 'NONE',  ( 3.499684904184919176, -2.717109755674974814, -1.809093184580113700 ) ) ;
#58531 = CARTESIAN_POINT ( 'NONE',  ( 10.21921441925191054, 4.353287638978129870, -8.814644987549721478 ) ) ;
#58532 = VERTEX_POINT ( 'NONE', #26399 ) ;
#58533 = CARTESIAN_POINT ( 'NONE',  ( 7.652389431507828910, -3.170862826441127158, 8.579327016467345857 ) ) ;
#58534 = CARTESIAN_POINT ( 'NONE',  ( 10.60746886766490071, -4.498335456194499926, -6.594573315824700188 ) ) ;
#58535 = CARTESIAN_POINT ( 'NONE',  ( 18.02962380328376213, 0.4069377568334723860, 12.69123026945923627 ) ) ;
#58536 = CARTESIAN_POINT ( 'NONE',  ( 10.44809687351624916, -4.327184855449103473, 6.282534154164604701 ) ) ;
#58537 = CARTESIAN_POINT ( 'NONE',  ( 10.98937577273788868, 3.538822733277925181, -8.699885912910444219 ) ) ;
#58538 = CARTESIAN_POINT ( 'NONE',  ( 11.60988784977536348, 3.148894096305599799, -7.451365240271489832 ) ) ;
#58539 = ORIENTED_EDGE ( 'NONE', *, *, #50073, .F. ) ;
#58540 = AXIS2_PLACEMENT_3D ( 'NONE', #8902, #30242, #46313 ) ;
#58541 = CARTESIAN_POINT ( 'NONE',  ( 10.22399006116000031, -5.507891002176999784, 6.589804341508000540 ) ) ;
#58542 = CARTESIAN_POINT ( 'NONE',  ( 8.770072224255999416, -3.906223101245800411, -8.386086300777899183 ) ) ;
#58544 = ORIENTED_EDGE ( 'NONE', *, *, #22830, .T. ) ;
#58543 = B_SPLINE_CURVE_WITH_KNOTS ( 'NONE', 3,
 ( #3992, #56116, #3651, #45973, #50877 ),
 .UNSPECIFIED., .F., .F.,
 ( 4, 1, 4 ),
 ( 0.000000000000000000, 0.1250503395655981342, 0.2125974459517032678 ),
 .UNSPECIFIED. ) ;
#58545 = CARTESIAN_POINT ( 'NONE',  ( 7.202583736560634442, 0.2999999999999999889, -3.098821334907657654 ) ) ;
#58546 = CARTESIAN_POINT ( 'NONE',  ( 8.957394353210000659, -2.678334737187000325, 8.735278777293000729 ) ) ;
#58547 = CARTESIAN_POINT ( 'NONE',  ( 17.71954595323150627, -0.7115697451012072960, -13.98190580764195801 ) ) ;
#58548 = EDGE_LOOP ( 'NONE', ( #26234, #23727, #63199, #33879 ) ) ;
#58549 = CARTESIAN_POINT ( 'NONE',  ( 23.56664322114200161, -2.935586410151000081, -13.67842711829000102 ) ) ;
#58550 = CARTESIAN_POINT ( 'NONE',  ( 6.884360841229000272, 5.757004663580000070, -7.968612095259000050 ) ) ;
#58551 = CARTESIAN_POINT ( 'NONE',  ( 12.80505043854146940, -3.174798964346249530, -12.21921514949791820 ) ) ;
#58552 = CARTESIAN_POINT ( 'NONE',  ( 23.58333993490100156, 3.064215547964999882E-13, 1.261213355973999610E-13 ) ) ;
#58553 = ORIENTED_EDGE ( 'NONE', *, *, #786, .T. ) ;
#58554 = CARTESIAN_POINT ( 'NONE',  ( 10.40727044253999978, -3.797905333157999941, 5.889909992361999969 ) ) ;
#58555 = EDGE_CURVE ( 'NONE', #5914, #43538, #36969, .T. ) ;
#58556 = EDGE_CURVE ( 'NONE', #50502, #47384, #11334, .T. ) ;
#58557 = CARTESIAN_POINT ( 'NONE',  ( 4.599999999999999645, 0.7192913403693119712, -12.57945229203838267 ) ) ;
#58558 = CARTESIAN_POINT ( 'NONE',  ( 11.20158531382784162, 4.272452942476327564, -6.250000000000000000 ) ) ;
#58559 = ORIENTED_EDGE ( 'NONE', *, *, #44330, .T. ) ;
#58560 = B_SPLINE_CURVE_WITH_KNOTS ( 'NONE', 3,
 ( #35821, #9236, #15862, #26016, #57473, #52930, #69002, #21115, #30575, #14840, #31270, #51890, #37194, #3985, #9580, #52235, #4674, #36503 ),
 .UNSPECIFIED., .F., .F.,
 ( 4, 2, 2, 2, 2, 2, 2, 2, 4 ),
 ( 0.000000000000000000, 0.1250000000000000000, 0.2500000000000000000, 0.3750000000000000000, 0.5000000000000000000, 0.6250000000000000000, 0.7500000000000000000, 0.8750000000000000000, 1.000000000000000000 ),
 .UNSPECIFIED. ) ;
#58561 = AXIS2_PLACEMENT_3D ( 'NONE', #42049, #36808, #10228 ) ;
#58562 = CARTESIAN_POINT ( 'NONE',  ( 6.159193173016667799, -0.3926218265389189721, -1.460959015002473604 ) ) ;
#58563 = VERTEX_POINT ( 'NONE', #59579 ) ;
#58564 = FACE_OUTER_BOUND ( 'NONE', #47977, .T. ) ;
#58565 = CARTESIAN_POINT ( 'NONE',  ( 18.09779443567301271, 0.3101119055885873110, -13.89534721488124447 ) ) ;
#58566 = CARTESIAN_POINT ( 'NONE',  ( 4.863817101178999458, 1.226378114769999916, 0.9601309097413999183 ) ) ;
#58567 = AXIS2_PLACEMENT_3D ( 'NONE', #34748, #14789, #57086 ) ;
#58568 = CARTESIAN_POINT ( 'NONE',  ( 7.910745297646997187, 4.529763905033002303, -6.316445270365000475 ) ) ;
#58569 = CARTESIAN_POINT ( 'NONE',  ( 8.023148997453999343, 5.167567567567999731, -6.822293592207000934 ) ) ;
#58570 = PLANE ( 'NONE',  #9452 ) ;
#58571 = CARTESIAN_POINT ( 'NONE',  ( 10.10000011340999926, -1.190159082397999942E-13, -1.214010018759999782E-13 ) ) ;
#58572 = VERTEX_POINT ( 'NONE', #48404 ) ;
#58573 = CARTESIAN_POINT ( 'NONE',  ( 7.802608290491005683, -4.876635182444005068, 6.352765399118998069 ) ) ;
#58574 = B_SPLINE_CURVE_WITH_KNOTS ( 'NONE', 3,
 ( #43099, #48002, #21088, #10246, #64400, #16523 ),
 .UNSPECIFIED., .F., .F.,
 ( 4, 2, 4 ),
 ( 0.000000000000000000, 0.5000000000000000000, 1.000000000000000000 ),
 .UNSPECIFIED. ) ;
#58575 = ORIENTED_EDGE ( 'NONE', *, *, #1093, .F. ) ;
#58576 = CARTESIAN_POINT ( 'NONE',  ( 9.667078842372998082, 4.541623431405000133, 5.824038024834000460 ) ) ;
#58577 = CARTESIAN_POINT ( 'NONE',  ( 11.02418915877000138, 2.407889430138999920, -8.439554272735000140 ) ) ;
#58578 = EDGE_CURVE ( 'NONE', #28207, #129, #7744, .T. ) ;
#58579 = VECTOR ( 'NONE', #17376, 1000.000000000000000 ) ;
#58580 = DIRECTION ( 'NONE',  ( 1.000000000000000000, 0.000000000000000000, 0.000000000000000000 ) ) ;
#58581 = CARTESIAN_POINT ( 'NONE',  ( 12.21197387330458461, 2.302545343651722920, -13.71336076199744802 ) ) ;
#58582 = DIRECTION ( 'NONE',  ( 0.000000000000000000, 1.000000000000000000, 0.000000000000000000 ) ) ;
#58583 = EDGE_CURVE ( 'NONE', #35262, #26212, #49093, .T. ) ;
#58584 = CARTESIAN_POINT ( 'NONE',  ( 8.881777890044364909, -4.415113854800245541, -6.197856508860001057 ) ) ;
#58585 = CARTESIAN_POINT ( 'NONE',  ( 7.100000000000000533, 0.000000000000000000, 0.000000000000000000 ) ) ;
#58586 = CARTESIAN_POINT ( 'NONE',  ( 18.16002775360864518, 0.1622926919634330167, 13.89880504291887320 ) ) ;
#58587 = B_SPLINE_CURVE_WITH_KNOTS ( 'NONE', 3,
 ( #22629, #64584, #59348, #28587 ),
 .UNSPECIFIED., .F., .F.,
 ( 4, 4 ),
 ( 0.000000000000000000, 1.000000000000000000 ),
 .UNSPECIFIED. ) ;
#58588 = ORIENTED_EDGE ( 'NONE', *, *, #38918, .F. ) ;
#58589 = CARTESIAN_POINT ( 'NONE',  ( 12.83903456837200174, -11.55258133652000119, 4.939873833509000889 ) ) ;
#58590 = CARTESIAN_POINT ( 'NONE',  ( 11.78118179236250107, -4.267047616085000605, 8.749800764654999341 ) ) ;
#58591 = CARTESIAN_POINT ( 'NONE',  ( 17.75497764268494549, -0.5922531181022384628, -13.88301284246451139 ) ) ;
#58592 = CARTESIAN_POINT ( 'NONE',  ( 8.373668146795001377, -2.202816532622999812, 7.706987678916999762 ) ) ;
#58594 = CARTESIAN_POINT ( 'NONE',  ( 10.33253786428999987, -2.899999999999999911, 6.571291218949999902 ) ) ;
#58593 = CARTESIAN_POINT ( 'NONE',  ( 13.99999999439439335, 9.377150629848445718, 8.201012428486359696 ) ) ;
#58595 = CARTESIAN_POINT ( 'NONE',  ( 11.08425954179440076, 4.982976321082899673, -8.316745941391600283 ) ) ;
#58596 = FACE_OUTER_BOUND ( 'NONE', #49667, .T. ) ;
#58597 = CARTESIAN_POINT ( 'NONE',  ( 9.653000818238998804, 3.232852935619000334, -7.903971937289999694 ) ) ;
#58598 = B_SPLINE_CURVE_WITH_KNOTS ( 'NONE', 3,
 ( #24453, #40196, #9384, #13628, #30728, #34953, #56267, #8377 ),
 .UNSPECIFIED., .F., .F.,
 ( 4, 2, 2, 4 ),
 ( 0.000000000000000000, 0.2500000000000014433, 0.5000000000000028866, 1.000000000000000000 ),
 .UNSPECIFIED. ) ;
#58599 = CARTESIAN_POINT ( 'NONE',  ( 18.11105811251409037, -0.2856309244984046591, 12.69568149856437067 ) ) ;
#58600 = CARTESIAN_POINT ( 'NONE',  ( 6.915494267272999984, 1.396408403708000012, -0.2221503625482000033 ) ) ;
#58601 = CARTESIAN_POINT ( 'NONE',  ( 5.000000000000000000, 0.000000000000000000, 0.000000000000000000 ) ) ;
#58602 = VERTEX_POINT ( 'NONE', #44215 ) ;
#58603 = CARTESIAN_POINT ( 'NONE',  ( 8.187144353207999714, -4.968144979409999884, 5.971795951526999602 ) ) ;
#58604 = CARTESIAN_POINT ( 'NONE',  ( 8.175739158770999992, 4.686731264770999772, -8.717075579553000608 ) ) ;
#58605 = CARTESIAN_POINT ( 'NONE',  ( 25.29987261392200182, 8.756202924575998026, -7.455126447192999883 ) ) ;
#58606 = CARTESIAN_POINT ( 'NONE',  ( 17.80000000000000071, -13.72414332887999855, 50.50083396221000243 ) ) ;
#58607 = ORIENTED_EDGE ( 'NONE', *, *, #18706, .T. ) ;
#58608 = CARTESIAN_POINT ( 'NONE',  ( 0.9218879684122999185, 1.034012873651999787, -3.554373790709000058 ) ) ;
#58609 = AXIS2_PLACEMENT_3D ( 'NONE', #43047, #53, #28010 ) ;
#58610 = CARTESIAN_POINT ( 'NONE',  ( 10.28014141025500017, 4.417352327511700594, 6.756653759087999589 ) ) ;
#58611 = CARTESIAN_POINT ( 'NONE',  ( 2.409338192682000113, 0.3184749856117999878, -3.745257128239000366 ) ) ;
#58612 = ADVANCED_FACE ( 'NONE', ( #22863 ), #18324, .T. ) ;
#58613 = ORIENTED_EDGE ( 'NONE', *, *, #67342, .F. ) ;
#58614 = ADVANCED_FACE ( 'NONE', ( #60279 ), #61312, .F. ) ;
#58615 = CARTESIAN_POINT ( 'NONE',  ( 12.50564389185356973, -0.6551943188411786245, -12.58295456804122914 ) ) ;
#58616 = CARTESIAN_POINT ( 'NONE',  ( 24.44496264144000364, 8.810483598181999554, -8.810508341310001157 ) ) ;
#58617 = CARTESIAN_POINT ( 'NONE',  ( 17.79016990201540693, 3.160912468841193590, -12.19707490278732820 ) ) ;
#58618 = CARTESIAN_POINT ( 'NONE',  ( 5.606877745311565242, 12.12699005521752049, 3.748526802953684012 ) ) ;
#58619 = CARTESIAN_POINT ( 'NONE',  ( 5.500000000000000000, 11.95749337870000062, 3.642574926947999892 ) ) ;
#58620 = ORIENTED_EDGE ( 'NONE', *, *, #7257, .T. ) ;
#58621 = CARTESIAN_POINT ( 'NONE',  ( 8.999999001754000361, 12.50000000000000000, 0.000000000000000000 ) ) ;
#58622 = CARTESIAN_POINT ( 'NONE',  ( 8.046420280407000192, 5.281793838578000333, -8.397855149904000172 ) ) ;
#58623 = CARTESIAN_POINT ( 'NONE',  ( 8.412003453006938969, -2.446741332449001494, 8.282553572544875564 ) ) ;
#58624 = CARTESIAN_POINT ( 'NONE',  ( 11.06623059009866061, -4.687762524153129995, -6.964041498692941090 ) ) ;
#58625 = VERTEX_POINT ( 'NONE', #59926 ) ;
#58626 = CARTESIAN_POINT ( 'NONE',  ( 15.90567905817900218, -3.588626488247999902, -11.74852861413999960 ) ) ;
#58627 = B_SPLINE_CURVE_WITH_KNOTS ( 'NONE', 3,
 ( #45998, #20455, #9266, #13850, #9614, #24679, #41782, #67310, #63087, #29945, #42135, #8595 ),
 .UNSPECIFIED., .F., .F.,
 ( 4, 2, 2, 2, 2, 4 ),
 ( 0.000000000000000000, 0.2499999999999976130, 0.3749999999999962252, 0.4374999999999957256, 0.4999999999999952260, 1.000000000000000000 ),
 .UNSPECIFIED. ) ;
#58628 = DIRECTION ( 'NONE',  ( 1.000000000000000000, 0.000000000000000000, 0.000000000000000000 ) ) ;
#58629 = EDGE_LOOP ( 'NONE', ( #9137, #61830, #59853, #52982 ) ) ;
#58630 = CARTESIAN_POINT ( 'NONE',  ( 11.10000000000000142, 3.333792990081902552, -8.929221575986867165 ) ) ;
#58631 = CARTESIAN_POINT ( 'NONE',  ( 4.000000000000000000, 0.000000000000000000, 0.000000000000000000 ) ) ;
#58632 = CARTESIAN_POINT ( 'NONE',  ( 8.810863317747999801, 4.960863370448500120, 7.499999999926881600 ) ) ;
#58633 = ORIENTED_EDGE ( 'NONE', *, *, #34512, .F. ) ;
#58634 = CARTESIAN_POINT ( 'NONE',  ( 15.49269116706140537, -8.815195450845674685, -7.616746626196380987 ) ) ;
#58635 = CARTESIAN_POINT ( 'NONE',  ( 11.15278751119019773, 3.209519379020799867, -7.913556523549700294 ) ) ;
#58636 = CARTESIAN_POINT ( 'NONE',  ( 12.39876276414167933, 2.975035832937170888, -12.32812070139215166 ) ) ;
#58638 = CIRCLE ( 'NONE', #21800, 13.10000000000000142 ) ;
#58637 = CARTESIAN_POINT ( 'NONE',  ( 10.99349279008999858, -4.332388355267299929, 6.265968249244999733 ) ) ;
#58639 = ORIENTED_EDGE ( 'NONE', *, *, #55009, .F. ) ;
#58640 = CARTESIAN_POINT ( 'NONE',  ( 7.678989158771000412, 2.599243720295000060, 7.909344432242998657 ) ) ;
#58641 = EDGE_CURVE ( 'NONE', #32947, #28894, #60375, .T. ) ;
#58642 = EDGE_CURVE ( 'NONE', #56420, #54978, #17192, .T. ) ;
#58643 = ORIENTED_EDGE ( 'NONE', *, *, #1740, .F. ) ;
#58644 = CARTESIAN_POINT ( 'NONE',  ( 11.33570505509991655, 4.908984911270270146, 7.824998694764690121 ) ) ;
#58645 = ADVANCED_FACE ( 'NONE', ( #12036 ), #40650, .T. ) ;
#58646 = CARTESIAN_POINT ( 'NONE',  ( 16.04718133169100014, -8.956716759973000208, -8.677900031540000114 ) ) ;
#58647 = DIRECTION ( 'NONE',  ( 1.000000000000000000, 0.000000000000000000, 0.000000000000000000 ) ) ;
#58648 = ORIENTED_EDGE ( 'NONE', *, *, #25273, .T. ) ;
#58649 = B_SPLINE_SURFACE_WITH_KNOTS ( 'NONE', 3, 3, ( 
 ( #51757, #57339, #63267, #58043, #10144, #46179, #67486, #64646, #58722, #58376, #68860, #48232, #22349, #42318, #21999, #6262, #20982, #27600, #47901, #32850, #37742, #48930, #338, #10482, #31820, #27259, #37064, #42988, #26918, #17098, #43342, #4889, #16752, #16411, #53139 ),
 ( #26579, #38080, #48583, #37401, #20726, #11856, #1036, #10826, #33195, #54162, #43687, #64297, #5917, #53483, #21655, #21318, #26230, #15736, #38431, #687, #32170, #59406, #11506, #64983, #47559, #42647, #53820, #63619, #59754, #5239, #5576, #63958, #16068, #59069, #11170 ),
 ( #32505, #38783, #54860, #60110, #60797, #2411, #12214, #6615, #6962, #45416, #2075, #49264, #28293, #49961, #66376, #8007, #17812, #49613, #66030, #29343, #65339, #23734, #33544, #13263, #44733, #18500, #1720, #34588, #18154, #39825, #23393, #23040, #44389, #17458, #65689 ),
 ( #27953, #55208, #45072, #61145, #39128, #39475, #24079, #50312, #54514, #7308, #60454, #12910, #40171, #34238, #55557, #12559, #33891, #7657, #28650, #61487, #55903, #22692, #13605, #29003, #50655, #2755, #66725, #18845, #1374, #44036, #57256, #41529, #35613, #25797, #20551 ) ),
 .UNSPECIFIED., .F., .F., .F.,
 ( 4, 4 ),
 ( 4, 1, 1, 1, 1, 1, 1, 1, 1, 1, 1, 1, 1, 1, 1, 1, 1, 1, 1, 1, 1, 1, 1, 1, 1, 1, 1, 1, 1, 1, 1, 1, 4 ),
 ( -0.02000000000000000042, 1.020000000000000018 ),
 ( 0.1633025096610999927, 0.1899619885200000136, 0.2166214673788000034, 0.2432809462376999965, 0.2699404250964999585, 0.2965999039553000038, 0.3232593828141999692, 0.3499188616730000145, 0.3765783405318000043, 0.4032378193906999697, 0.4298972982494999595, 0.4565567771083000048, 0.4832162559671999702, 0.5098757348260000155, 0.5365352136848999809, 0.5631946925437000262, 0.5898541714025000715, 0.6165136502614000369, 0.6431731291201999712, 0.6698326079790000165, 0.6964920868378999819, 0.7231515656967000272, 0.7498110445554999615, 0.7764705234143999268, 0.8031300022731999722, 0.8297894811320000175, 0.8564489599908999828, 0.8831084388497000282, 0.9097679177085999935, 0.9364273965674000388, 0.9630868754261999731, 0.9897463542851000495, 1.016405833144000015 ),
 .UNSPECIFIED. ) ;
#58650 = CARTESIAN_POINT ( 'NONE',  ( 12.38986377076840206, -2.032719501308457577, -12.54823268863294849 ) ) ;
#58651 = CARTESIAN_POINT ( 'NONE',  ( 0.3870378418490574290, -3.299192355781437325, -0.8857457579047530727 ) ) ;
#58652 = CARTESIAN_POINT ( 'NONE',  ( 0.000000000000000000, 2.899999999999999911, -7.500000000000000000 ) ) ;
#58653 = CARTESIAN_POINT ( 'NONE',  ( 10.64393020684969926, 5.250000000000000000, 7.500000000000000000 ) ) ;
#58654 = CARTESIAN_POINT ( 'NONE',  ( 12.48191940168460157, -1.864230036291391057, -13.87532606992096618 ) ) ;
#58655 = CARTESIAN_POINT ( 'NONE',  ( 11.33872066707849768, -3.141388196630700236, -6.980638253271099103 ) ) ;
#58656 = CARTESIAN_POINT ( 'NONE',  ( 7.110549024909053273, 0.7930388321308440291, -1.030519542554439560 ) ) ;
#58657 = CARTESIAN_POINT ( 'NONE',  ( 17.92000013766230637, -3.102113379644124702, 12.21216327800867774 ) ) ;
#58658 = ORIENTED_EDGE ( 'NONE', *, *, #18365, .T. ) ;
#58659 = CARTESIAN_POINT ( 'NONE',  ( -2.147830119999999621, -1.300000000000000044, 9.662944685757000940 ) ) ;
#58660 = ORIENTED_EDGE ( 'NONE', *, *, #57860, .F. ) ;
#58661 = DIRECTION ( 'NONE',  ( 1.000000000000000000, 0.000000000000000000, 0.000000000000000000 ) ) ;
#58662 = CARTESIAN_POINT ( 'NONE',  ( 25.60000000000000142, 0.000000000000000000, -10.75000000000000000 ) ) ;
#58663 = DIRECTION ( 'NONE',  ( 0.000000000000000000, 0.000000000000000000, -1.000000000000000000 ) ) ;
#58664 = CARTESIAN_POINT ( 'NONE',  ( 10.04002816746000093, 2.348904337896000172, -7.136750921008999882 ) ) ;
#58665 = EDGE_CURVE ( 'NONE', #55474, #41793, #60764, .T. ) ;
#58666 = CARTESIAN_POINT ( 'NONE',  ( 10.88016425062000003, -2.793121555136000023, -6.864957546339999439 ) ) ;
#58667 = CIRCLE ( 'NONE', #56471, 2.749999999999999556 ) ;
#58668 = CARTESIAN_POINT ( 'NONE',  ( 9.080795537700433684, 5.100000000000000533, -6.662590550605527184 ) ) ;
#58669 = CARTESIAN_POINT ( 'NONE',  ( 15.90007192502618238, 3.569777767583313111, 11.29792192708077181 ) ) ;
#58670 = CARTESIAN_POINT ( 'NONE',  ( 8.762289945692000259, 3.761977284103799946, -8.411288920148800585 ) ) ;
#58671 = B_SPLINE_CURVE_WITH_KNOTS ( 'NONE', 3,
 ( #19701, #4295, #56766, #8863, #20727, #9891 ),
 .UNSPECIFIED., .F., .F.,
 ( 4, 1, 1, 4 ),
 ( 0.000000000000000000, 0.3333333333333000081, 0.6666666666667000474, 1.000000000000000000 ),
 .UNSPECIFIED. ) ;
#58672 = ORIENTED_EDGE ( 'NONE', *, *, #67550, .F. ) ;
#58673 = CARTESIAN_POINT ( 'NONE',  ( 10.84393020684979980, 2.750000000000000000, 7.500000000000000000 ) ) ;
#58674 = CARTESIAN_POINT ( 'NONE',  ( 10.65050915380999896, 5.200037120669999346, 5.937706951697999891 ) ) ;
#58675 = DIRECTION ( 'NONE',  ( 0.000000000000000000, -1.000000000000000000, 0.000000000000000000 ) ) ;
#58676 = CARTESIAN_POINT ( 'NONE',  ( 11.52301463001509951, -3.452642973349600464, 8.376661845795100092 ) ) ;
#58677 = CARTESIAN_POINT ( 'NONE',  ( 18.31386961183700279, 3.086648833569000328, -11.29009770192999973 ) ) ;
#58678 = CARTESIAN_POINT ( 'NONE',  ( 11.14434831560999939, 10.07920604617999949, -5.729928524014000324 ) ) ;
#58679 = CARTESIAN_POINT ( 'NONE',  ( 11.03120992439402315, 2.698003081065078135, -8.692097047312476121 ) ) ;
#58680 = CARTESIAN_POINT ( 'NONE',  ( 5.569720047903312654, -12.16229356903719250, -3.760137167885687415 ) ) ;
#58681 = CARTESIAN_POINT ( 'NONE',  ( 1.700000000000000178, -1.500000000000000000, 0.000000000000000000 ) ) ;
#58682 =( NAMED_UNIT ( * ) PLANE_ANGLE_UNIT ( ) SI_UNIT ( $, .RADIAN. ) );
#58683 = ORIENTED_EDGE ( 'NONE', *, *, #34201, .T. ) ;
#58684 = CARTESIAN_POINT ( 'NONE',  ( 9.318935841232999451, 2.644017913812000131, -7.838184857420000817 ) ) ;
#58685 = FACE_OUTER_BOUND ( 'NONE', #46232, .T. ) ;
#58686 = CARTESIAN_POINT ( 'NONE',  ( 17.80546914520760993, 3.072731260628056127, 13.53510445278182672 ) ) ;
#58687 = DIRECTION ( 'NONE',  ( 0.000000000000000000, -1.000000000000000000, 0.000000000000000000 ) ) ;
#58688 = CARTESIAN_POINT ( 'NONE',  ( 10.69798710318595170, 4.886986039840945040, 4.803896147895557966 ) ) ;
#58689 = CARTESIAN_POINT ( 'NONE',  ( 10.98995257254739855, -5.095356924909000718, -7.818564472783199548 ) ) ;
#58690 = VERTEX_POINT ( 'NONE', #66548 ) ;
#58691 = CARTESIAN_POINT ( 'NONE',  ( 11.09999999999999964, 2.700000000000000178, -5.160242730539000178 ) ) ;
#58692 = CARTESIAN_POINT ( 'NONE',  ( 10.16571249083272654, -5.659096789895665225, 6.739882715535322255 ) ) ;
#58693 = CIRCLE ( 'NONE', #21862, 0.7499999936418002555 ) ;
#58695 = CARTESIAN_POINT ( 'NONE',  ( 4.966698988835610784, -2.066632171653634664, 9.814764551474491144E-10 ) ) ;
#58694 = CARTESIAN_POINT ( 'NONE',  ( 9.401145280412999128, 3.927090956378999742, -9.230892435423001530 ) ) ;
#58696 = CARTESIAN_POINT ( 'NONE',  ( 2.268533155335109353, 3.242759788008271915, -0.3142191302543209663 ) ) ;
#58697 = EDGE_CURVE ( 'NONE', #63565, #37562, #26136, .T. ) ;
#58698 = ORIENTED_EDGE ( 'NONE', *, *, #41435, .F. ) ;
#58699 = ADVANCED_FACE ( 'NONE', ( #55035 ), #44566, .F. ) ;
#58700 = CARTESIAN_POINT ( 'NONE',  ( 11.18706938844999854, 3.186790175674999670, 6.232702730851999995 ) ) ;
#58701 = CARTESIAN_POINT ( 'NONE',  ( 17.88684482918182184, -3.030051203688146622, -13.54658895838268151 ) ) ;
#58702 = CARTESIAN_POINT ( 'NONE',  ( 11.24025954179439957, 4.771812902496799680, 6.858707791728399172 ) ) ;
#58703 = CARTESIAN_POINT ( 'NONE',  ( 9.625489929093001606, -3.134630999349000025, 8.626959345509000343 ) ) ;
#58704 = CARTESIAN_POINT ( 'NONE',  ( 8.604019353210000887, -5.165500668528999917, 8.645534272955000432 ) ) ;
#58705 = ORIENTED_EDGE ( 'NONE', *, *, #24808, .F. ) ;
#58706 = CARTESIAN_POINT ( 'NONE',  ( 8.417489158772999858, 2.029098103856999735, 7.726995416028000108 ) ) ;
#58707 = B_SPLINE_CURVE_WITH_KNOTS ( 'NONE', 3,
 ( #6269, #12223, #33550, #48938, #48240, #38441, #23047, #27963, #27610, #58730, #1046, #11864, #49272, #59077 ),
 .UNSPECIFIED., .F., .F.,
 ( 4, 2, 2, 2, 2, 2, 4 ),
 ( 0.000000000000000000, 0.1249999999999999722, 0.2499999999999999445, 0.4999999999999993339, 0.6249999999999994449, 0.7499999999999996669, 1.000000000000000000 ),
 .UNSPECIFIED. ) ;
#58709 = CARTESIAN_POINT ( 'NONE',  ( 10.50898185320999900, -4.485028460808000439, -9.114431591966999591 ) ) ;
#58708 = CARTESIAN_POINT ( 'NONE',  ( 10.96914282210478042, 4.267867395145749754, -6.667932297870764913 ) ) ;
#58710 = CARTESIAN_POINT ( 'NONE',  ( 7.772509392072763035, -5.050159846104850914, 8.886365745317096554 ) ) ;
#58711 = CARTESIAN_POINT ( 'NONE',  ( 10.06343867337000120, -5.156226070197000411, 6.125223053176999777 ) ) ;
#58712 = CARTESIAN_POINT ( 'NONE',  ( 24.45284689113699983, 3.540778225556000081, 12.31935692833000040 ) ) ;
#58713 = EDGE_LOOP ( 'NONE', ( #2989, #57090, #62816, #66032 ) ) ;
#58714 = FACE_OUTER_BOUND ( 'NONE', #5699, .T. ) ;
#58715 = B_SPLINE_CURVE_WITH_KNOTS ( 'NONE', 3,
 ( #30136, #47839, #19630, #35711, #16008, #57028, #9128, #51781, #28584, #27540 ),
 .UNSPECIFIED., .F., .F.,
 ( 4, 2, 2, 2, 4 ),
 ( 0.3934091950370091628, 0.5450568962777568860, 0.6967045975185046647, 0.8483522987592523323, 1.000000000000000000 ),
 .UNSPECIFIED. ) ;
#58716 = CARTESIAN_POINT ( 'NONE',  ( 12.10533460557258323, -3.815825449682300086, 6.374224726731999802 ) ) ;
#58717 = CIRCLE ( 'NONE', #34179, 2.000000000000000444 ) ;
#58718 = CARTESIAN_POINT ( 'NONE',  ( 10.91195257254739914, 2.772832764353999835, 7.143100915737699452 ) ) ;
#58719 = ORIENTED_EDGE ( 'NONE', *, *, #55200, .F. ) ;
#58720 = CARTESIAN_POINT ( 'NONE',  ( 8.664129719593997692, 5.524776413195999325, -7.147585171405999915 ) ) ;
#58721 = CARTESIAN_POINT ( 'NONE',  ( 12.08853825830067841, 2.367028970089855910, -12.37569070051500830 ) ) ;
#58722 = CARTESIAN_POINT ( 'NONE',  ( 12.05300581613033906, -2.892415530317000272, 6.788791567531699656 ) ) ;
#58723 = CARTESIAN_POINT ( 'NONE',  ( 24.67332979692900352, -3.458637065210999673, -12.04350545405000084 ) ) ;
#58725 = EDGE_CURVE ( 'NONE', #38787, #65648, #28121, .T. ) ;
#58724 = CARTESIAN_POINT ( 'NONE',  ( 18.11145169124867138, 2.784830482480015412, -13.60891328693460522 ) ) ;
#58726 = EDGE_LOOP ( 'NONE', ( #53339, #66614, #498, #53376 ) ) ;
#58727 = CARTESIAN_POINT ( 'NONE',  ( 8.992847592598998574, -5.108134449482000683, -6.664326587025001025 ) ) ;
#58728 = CARTESIAN_POINT ( 'NONE',  ( 23.99449529258459179, 9.375514267760260978, 9.276290998956193690 ) ) ;
#58729 = ORIENTED_EDGE ( 'NONE', *, *, #33500, .F. ) ;
#58730 = CARTESIAN_POINT ( 'NONE',  ( 10.01008022827853772, -3.057295994144781037, -8.976432196558560506 ) ) ;
#58731 = CARTESIAN_POINT ( 'NONE',  ( 10.57564694612699974, 3.068007311611700150, 7.128058497017000228 ) ) ;
#58732 = CARTESIAN_POINT ( 'NONE',  ( 10.31498017945866685, 2.650031506806222570, -7.499998780888569527 ) ) ;
#58733 = CARTESIAN_POINT ( 'NONE',  ( 10.35427764559999986, 4.879113829302000660, -8.944031201701999834 ) ) ;
#58734 = CARTESIAN_POINT ( 'NONE',  ( 8.229964631809997044, 4.681828315382999151, 6.132208354562998842 ) ) ;
#58735 = CARTESIAN_POINT ( 'NONE',  ( 10.94797187187000098, -2.864324950622999744, 8.846246404612999825 ) ) ;
#58736 = CARTESIAN_POINT ( 'NONE',  ( 17.65692019170432303, 0.6169782284476039713, -12.67981870385671428 ) ) ;
#58737 = CARTESIAN_POINT ( 'NONE',  ( 9.051837186271754376, 4.773597817256774789, 8.611999504439044273 ) ) ;
#58738 = CARTESIAN_POINT ( 'NONE',  ( 10.82179975933729921, -3.051121678931899783, -7.173532873542499466 ) ) ;
#58739 = CARTESIAN_POINT ( 'NONE',  ( 8.689260841231000398, 2.550241116032999855, 7.666973618349000041 ) ) ;
#58740 = EDGE_LOOP ( 'NONE', ( #45886, #25172, #1420, #43053, #773, #16749 ) ) ;
#58741 = DIRECTION ( 'NONE',  ( 0.000000000000000000, 1.000000000000000000, 0.000000000000000000 ) ) ;
#58742 = CARTESIAN_POINT ( 'NONE',  ( 12.08810207955109917, -4.796537143354000499, 7.825000000000000178 ) ) ;
#58743 = CARTESIAN_POINT ( 'NONE',  ( 11.40162633574000139, 12.25609765133000018, 1.727435033673999865 ) ) ;
#58744 = EDGE_CURVE ( 'NONE', #30625, #11095, #16158, .T. ) ;
#58745 = VECTOR ( 'NONE', #43162, 1000.000000000000000 ) ;
#58746 = CARTESIAN_POINT ( 'NONE',  ( 17.99911394258097630, 3.049496102151219912, 12.22541657636149282 ) ) ;
#58747 = CARTESIAN_POINT ( 'NONE',  ( 7.100000000000000533, 13.94845324556000143, -4.312847325879000770 ) ) ;
#58748 = CARTESIAN_POINT ( 'NONE',  ( 11.05758752493000152, 9.474230211708000837, 6.311392455611000152 ) ) ;
#58749 = CARTESIAN_POINT ( 'NONE',  ( 9.225036374688860619, -2.649952446100997339, 7.500002253091946791 ) ) ;
#58750 = CARTESIAN_POINT ( 'NONE',  ( 10.01059687351599692, -3.370476274536376771, -8.592232985442825210 ) ) ;
#58751 = ORIENTED_EDGE ( 'NONE', *, *, #5034, .T. ) ;
#58752 = CARTESIAN_POINT ( 'NONE',  ( 12.23408645687635143, -2.036599147259928078, 12.43432143783615551 ) ) ;
#58753 = CARTESIAN_POINT ( 'NONE',  ( 9.302417874593999159, -5.050800927762999493, -7.946712276748498560 ) ) ;
#58754 = CARTESIAN_POINT ( 'NONE',  ( 13.73140886085690582, -8.907522817021714445, -7.508769385438534449 ) ) ;
#58755 = CARTESIAN_POINT ( 'NONE',  ( 8.295159150710981422, 2.930861795617814014, -6.461078406439177080 ) ) ;
#58756 = CARTESIAN_POINT ( 'NONE',  ( 11.49410672858429905, -4.801902424331299990, 8.103244025831999764 ) ) ;
#58757 = VECTOR ( 'NONE', #19587, 1000.000000000000000 ) ;
#58758 = B_SPLINE_CURVE_WITH_KNOTS ( 'NONE', 3,
 ( #9870, #27595, #15467, #36442, #64640, #1715, #36794, #60103, #58114, #48921, #41687, #31548, #1029, #26302, #49258, #22341, #47630, #33188 ),
 .UNSPECIFIED., .F., .F.,
 ( 4, 2, 2, 2, 2, 2, 2, 2, 4 ),
 ( 0.000000000000000000, 0.06250000000000024980, 0.1250000000000004996, 0.2500000000000009992, 0.4999999999999992228, 0.7499999999999974465, 0.8749999999999965583, 0.9374999999999983347, 1.000000000000000000 ),
 .UNSPECIFIED. ) ;
#58759 = CARTESIAN_POINT ( 'NONE',  ( 11.62994988689359843, 4.518136976474400157, -8.516279404258998653 ) ) ;
#58760 = CARTESIAN_POINT ( 'NONE',  ( 8.712501735000000025, 3.641148095589300304, 6.723921629386799381 ) ) ;
#58761 = CARTESIAN_POINT ( 'NONE',  ( 5.000000000000000000, 0.2999999999999999889, -3.149999999999999911 ) ) ;
#58762 = CARTESIAN_POINT ( 'NONE',  ( 9.585607375975767397, 5.315314066450707919, -7.853683613172021794 ) ) ;
#58763 = CARTESIAN_POINT ( 'NONE',  ( 12.10796728133592026, 2.678710578830982847, 12.31197141455839272 ) ) ;
#58765 = CARTESIAN_POINT ( 'NONE',  ( 8.496698341230001006, 5.198556077301000222, 8.332552905512999430 ) ) ;
#58764 = CARTESIAN_POINT ( 'NONE',  ( 9.049126402770998112, 5.068373778467000434, -7.097120470443400109 ) ) ;
#58766 = CARTESIAN_POINT ( 'NONE',  ( 11.38379707368349969, 3.433355370490100533, -6.509947486183500054 ) ) ;
#58767 = CARTESIAN_POINT ( 'NONE',  ( 7.859795284898003942, 2.854589328742001886, -6.788356039251000063 ) ) ;
#58768 = CARTESIAN_POINT ( 'NONE',  ( 10.77401721959000014, 3.826866801954999620, -5.823193568970000733 ) ) ;
#58769 = CARTESIAN_POINT ( 'NONE',  ( 8.870759580228998686, 2.755835090116000696, -7.202614619576299226 ) ) ;
#58771 = CARTESIAN_POINT ( 'NONE',  ( 12.34829947334116262, 2.926730327392950137, 12.34183739587882300 ) ) ;
#58770 = CARTESIAN_POINT ( 'NONE',  ( 12.10000669845703847, 11.02846243759400124, -3.754394857303852362 ) ) ;
#58772 = CARTESIAN_POINT ( 'NONE',  ( 8.069038185141000241, 5.112620281584000281, -6.682995288704000281 ) ) ;
#58773 = ORIENTED_EDGE ( 'NONE', *, *, #33418, .F. ) ;
#58774 = CARTESIAN_POINT ( 'NONE',  ( 12.23478131640822753, 0.2564338549407608747, 12.69653134296957120 ) ) ;
#58775 = CARTESIAN_POINT ( 'NONE',  ( 9.051550650638001017, 2.899999999999999911, 6.227445478845999638 ) ) ;
#58776 = CARTESIAN_POINT ( 'NONE',  ( 12.60217350508042067, -12.11433231916790376, 3.180975838886041185 ) ) ;
#58777 = CARTESIAN_POINT ( 'NONE',  ( 9.222405316139999698, 3.815922504313999930, 6.652755395362000002 ) ) ;
#58778 = ADVANCED_FACE ( 'NONE', ( #1545 ), #58512, .T. ) ;
#58779 = EDGE_CURVE ( 'NONE', #31672, #65921, #28688, .T. ) ;
#58780 = CARTESIAN_POINT ( 'NONE',  ( 12.52680909801651765, -3.059742249080376286, 13.53867541207075220 ) ) ;
#58781 = CARTESIAN_POINT ( 'NONE',  ( 12.18999301580459793, 2.611634498301437013, 13.64910281353442656 ) ) ;
#58782 = CARTESIAN_POINT ( 'NONE',  ( 8.969356963619999235, -5.119357025014000584, -7.499999999914821025 ) ) ;
#58783 = VERTEX_POINT ( 'NONE', #55379 ) ;
#58784 = EDGE_CURVE ( 'NONE', #25251, #34596, #68650, .T. ) ;
#58785 = EDGE_CURVE ( 'NONE', #47667, #59469, #49584, .T. ) ;
#58786 = CARTESIAN_POINT ( 'NONE',  ( 4.261179876531000055, 0.2683639413831000464, 1.246891768540999923 ) ) ;
#58787 = B_SPLINE_CURVE_WITH_KNOTS ( 'NONE', 3,
 ( #48208, #42624, #65313, #11482 ),
 .UNSPECIFIED., .F., .F.,
 ( 4, 4 ),
 ( 0.000000000000000000, 1.000000000000000000 ),
 .UNSPECIFIED. ) ;
#58788 = CARTESIAN_POINT ( 'NONE',  ( 11.48513281071060277, -5.084573083995119980, -7.824999134348144203 ) ) ;
#58789 = CIRCLE ( 'NONE', #33102, 2.000000000000000444 ) ;
#58790 = CYLINDRICAL_SURFACE ( 'NONE', #8641, 1.350000000000000533 ) ;
#58791 = CARTESIAN_POINT ( 'NONE',  ( 11.02946886766499901, -4.430164648092599577, 8.281567006984099422 ) ) ;
#58792 = CARTESIAN_POINT ( 'NONE',  ( 17.69815883927265787, 3.108482560213371215, -12.28876257455221221 ) ) ;
#58793 = CARTESIAN_POINT ( 'NONE',  ( 10.44728840309080020, -2.899999999999999911, 6.305985889617041984 ) ) ;
#58794 =( GEOMETRIC_REPRESENTATION_CONTEXT ( 3 ) GLOBAL_UNCERTAINTY_ASSIGNED_CONTEXT ( ( #4513 ) ) GLOBAL_UNIT_ASSIGNED_CONTEXT ( ( #12748, #3282, #45935 ) ) REPRESENTATION_CONTEXT ( 'NONE', 'WORKASPACE' ) );
#58795 = CARTESIAN_POINT ( 'NONE',  ( 18.02583793286699176, 2.911580782565375891, 12.34610277261516309 ) ) ;
#58797 = CARTESIAN_POINT ( 'NONE',  ( 15.88771848669683351, 8.938332686942986882, 8.488529254939262358 ) ) ;
#58796 = B_SPLINE_CURVE_WITH_KNOTS ( 'NONE', 3,
 ( #25241, #36077, #31873, #9497 ),
 .UNSPECIFIED., .F., .F.,
 ( 4, 4 ),
 ( 0.000000000000000000, 0.1254150264828375605 ),
 .UNSPECIFIED. ) ;
#58798 = CARTESIAN_POINT ( 'NONE',  ( 10.56170564679000101, -5.057490041178001050, -8.595713413570999606 ) ) ;
#58799 = AXIS2_PLACEMENT_3D ( 'NONE', #35421, #18988, #36099 ) ;
#58800 = CARTESIAN_POINT ( 'NONE',  ( 4.750859839682917141, 0.3926218265389220807, -1.460959015002473382 ) ) ;
#58801 = CARTESIAN_POINT ( 'NONE',  ( 11.03776785110999903, -5.237767851104999650, 6.571291218949999902 ) ) ;
#58802 = CARTESIAN_POINT ( 'NONE',  ( 11.47755399909358154, -3.866653594937912608, 6.221473734489901375 ) ) ;
#58803 = DIRECTION ( 'NONE',  ( 1.000000000000000000, 0.000000000000000000, 0.000000000000000000 ) ) ;
#58804 = ORIENTED_EDGE ( 'NONE', *, *, #25394, .F. ) ;
#58805 = CARTESIAN_POINT ( 'NONE',  ( 9.889535841229999846, 5.798263352390999437, -8.113145944980999502 ) ) ;
#58806 = CARTESIAN_POINT ( 'NONE',  ( 11.62133729122639991, -4.865898216891100247, 7.522778681411049995 ) ) ;
#58807 = ORIENTED_EDGE ( 'NONE', *, *, #62223, .T. ) ;
#58808 = AXIS2_PLACEMENT_3D ( 'NONE', #56901, #4434, #26118 ) ;
#58809 = DIRECTION ( 'NONE',  ( -1.000000000000000000, 0.000000000000000000, 0.000000000000000000 ) ) ;
#58810 = CARTESIAN_POINT ( 'NONE',  ( 10.89149144726329865, -4.659577337894599935, -6.569275630703699242 ) ) ;
#58811 = ORIENTED_EDGE ( 'NONE', *, *, #44683, .T. ) ;
#58812 = CARTESIAN_POINT ( 'NONE',  ( 10.52799293566599914, 4.806678152079100208, 6.510429574318199464 ) ) ;
#58813 = CARTESIAN_POINT ( 'NONE',  ( 25.30000327618300204, 2.078227429405999693, -11.31065739696999906 ) ) ;
#58814 = CARTESIAN_POINT ( 'NONE',  ( 17.75907622778400352, -3.376089723145999866, 11.11072845602000037 ) ) ;
#58815 = DIRECTION ( 'NONE',  ( 1.000000000000000000, 0.000000000000000000, 0.000000000000000000 ) ) ;
#58816 = CARTESIAN_POINT ( 'NONE',  ( 12.28049946582619434, 0.3399327003773965905, -13.89440849576309667 ) ) ;
#58817 = CARTESIAN_POINT ( 'NONE',  ( 11.59999999999999609, -4.755880058522732767, -6.982116912833851607 ) ) ;
#58818 = CARTESIAN_POINT ( 'NONE',  ( 10.36950884864999978, -2.719121019997000399, -7.031782724641000293 ) ) ;
#58819 = CARTESIAN_POINT ( 'NONE',  ( 13.55192027319500170, 11.56672964510999968, 2.320600286854999972 ) ) ;
#58820 = VERTEX_POINT ( 'NONE', #45919 ) ;
#58821 = CARTESIAN_POINT ( 'NONE',  ( 8.921135841230999119, 3.292387953886000140, -6.294868737226000377 ) ) ;
#58822 = EDGE_LOOP ( 'NONE', ( #39039, #50533, #16238, #56913, #35358, #7100 ) ) ;
#58823 = CARTESIAN_POINT ( 'NONE',  ( 0.2623669365312372159, 3.203502798912969851, -0.5608766408606025156 ) ) ;
#58824 = ORIENTED_EDGE ( 'NONE', *, *, #67102, .F. ) ;
#58825 = CARTESIAN_POINT ( 'NONE',  ( 9.605304848515999083, 5.163382381259999931, 6.968092280137199168 ) ) ;
#58826 = CARTESIAN_POINT ( 'NONE',  ( 17.98409414022582453, -2.954502725563342480, -12.33397020297173796 ) ) ;
#58827 = ADVANCED_FACE ( 'NONE', ( #25627 ), #2183, .F. ) ;
#58828 = CARTESIAN_POINT ( 'NONE',  ( 24.81043909399123848, -8.607472784691234224, 8.518286398806663939 ) ) ;
#58829 = CARTESIAN_POINT ( 'NONE',  ( 10.35226354018316108, 2.907767014557178342, -6.870476274536370553 ) ) ;
#58830 = EDGE_CURVE ( 'NONE', #42044, #59692, #20245, .T. ) ;
#58831 = DIRECTION ( 'NONE',  ( 0.000000000000000000, 0.9916377111174248249, -0.1290528957048032721 ) ) ;
#58832 = CARTESIAN_POINT ( 'NONE',  ( 12.19409625758322413, -0.1321590433901052575, 13.89915950722681970 ) ) ;
#58833 = EDGE_LOOP ( 'NONE', ( #14100, #34919 ) ) ;
#58834 = CARTESIAN_POINT ( 'NONE',  ( 11.60000000000000320, 4.109635333090444043, 6.362414725044395425 ) ) ;
#58835 = CARTESIAN_POINT ( 'NONE',  ( 18.46722213196600393, 12.01216300861999997, -3.678628708156000293 ) ) ;
#58836 = CARTESIAN_POINT ( 'NONE',  ( 9.454862456499625978, 4.412447805680870694, 8.271634030165902374 ) ) ;
#58837 = CARTESIAN_POINT ( 'NONE',  ( 4.443175434508999544, -0.2631654914794999689, -1.157398794349000060 ) ) ;
#58838 = CIRCLE ( 'NONE', #68863, 0.3000000000000000999 ) ;
#58839 = CARTESIAN_POINT ( 'NONE',  ( 9.444964158775000840, 3.920043641733999884, -9.398198753036000497 ) ) ;
#58840 = CARTESIAN_POINT ( 'NONE',  ( 18.26123302403700066, -2.828310120379999848, 11.95646042099000006 ) ) ;
#58841 = CARTESIAN_POINT ( 'NONE',  ( 10.02800210979000184, -3.452027005875999865, -6.074520565702999697 ) ) ;
#58842 = B_SPLINE_CURVE_WITH_KNOTS ( 'NONE', 3,
 ( #17990, #49445, #1553, #22876 ),
 .UNSPECIFIED., .F., .F.,
 ( 4, 4 ),
 ( 0.000000000000000000, 1.000000000000000000 ),
 .UNSPECIFIED. ) ;
#58843 = ORIENTED_EDGE ( 'NONE', *, *, #62690, .T. ) ;
#58844 = ORIENTED_EDGE ( 'NONE', *, *, #51525, .F. ) ;
#58845 = CARTESIAN_POINT ( 'NONE',  ( 11.13709883339000051, 5.336586328279000035, -5.177930967251000105 ) ) ;
#58846 = MECHANICAL_DESIGN_GEOMETRIC_PRESENTATION_REPRESENTATION (  '', ( #19781 ), #14245 ) ;
#58847 = DIRECTION ( 'NONE',  ( 0.000000000000000000, 1.000000000000000000, 0.000000000000000000 ) ) ;
#58848 = FACE_BOUND ( 'NONE', #15978, .T. ) ;
#58849 = DIRECTION ( 'NONE',  ( 0.000000000000000000, 0.9979288589194752479, -0.06432723012592840572 ) ) ;
#58850 = CARTESIAN_POINT ( 'NONE',  ( 9.343930206849998754, -5.250000000000000000, -7.500000000000000000 ) ) ;
#58851 = CARTESIAN_POINT ( 'NONE',  ( 11.51145123989532948, 4.605239108938600445, -8.668865425277999748 ) ) ;
#58852 = CARTESIAN_POINT ( 'NONE',  ( 9.687329965421998423, 3.397808798486600335, -8.123757726465999696 ) ) ;
#58854 = CARTESIAN_POINT ( 'NONE',  ( 4.399736634486760778, 0.3091794154604233236, -1.210059008288320470 ) ) ;
#58853 = CARTESIAN_POINT ( 'NONE',  ( 10.45896314288000006, -3.017187828228399926, 7.707177545471399327 ) ) ;
#58855 = CARTESIAN_POINT ( 'NONE',  ( 8.268606633798000871, -2.876811830795998670, 6.331441650266997456 ) ) ;
#58856 = ORIENTED_EDGE ( 'NONE', *, *, #63984, .F. ) ;
#58857 = VECTOR ( 'NONE', #4174, 1000.000000000000000 ) ;
#58858 = CARTESIAN_POINT ( 'NONE',  ( 9.905786073958001481, -2.698967003257000119, 8.979227319929000473 ) ) ;
#58859 = CARTESIAN_POINT ( 'NONE',  ( 30.60000000000000142, 0.000000000000000000, 0.000000000000000000 ) ) ;
#58860 = DIRECTION ( 'NONE',  ( 0.000000000000000000, 0.000000000000000000, -1.000000000000000000 ) ) ;
#58862 = EDGE_CURVE ( 'NONE', #26055, #4160, #57833, .T. ) ;
#58861 = B_SPLINE_CURVE_WITH_KNOTS ( 'NONE', 3,
 ( #24722, #29989, #14579, #51627, #15606, #10010, #46738, #57911, #31006, #68382, #25402, #52320, #35896, #30654, #25752, #26098, #46046, #67353 ),
 .UNSPECIFIED., .F., .F.,
 ( 4, 2, 2, 2, 2, 2, 2, 2, 4 ),
 ( 0.000000000000000000, 0.06249999999999873712, 0.1249999999999974742, 0.2499999999999972800, 0.4999999999999987788, 0.7500000000000002220, 0.8750000000000001110, 0.9375000000000000000, 1.000000000000000000 ),
 .UNSPECIFIED. ) ;
#58863 = B_SPLINE_CURVE_WITH_KNOTS ( 'NONE', 3,
 ( #36117, #25284, #9536, #57430, #46618, #25629, #20039, #52194, #4293, #59845 ),
 .UNSPECIFIED., .F., .F.,
 ( 4, 2, 2, 2, 4 ),
 ( 0.000000000000000000, 0.1249999999999998890, 0.2499999999999997780, 0.3749999999999996669, 0.4999999999999994449 ),
 .UNSPECIFIED. ) ;
#58864 = CIRCLE ( 'NONE', #48792, 1.500000000000001332 ) ;
#58865 = CARTESIAN_POINT ( 'NONE',  ( 9.877259503622999759, -2.207992199716000137, 7.624813542847999059 ) ) ;
#58866 = CARTESIAN_POINT ( 'NONE',  ( 18.17608830303050027, 2.571081552045474616, -12.43475473545199073 ) ) ;
#58867 = CARTESIAN_POINT ( 'NONE',  ( 25.39940118446284956, 11.19882020338194195, -3.252373299299911036 ) ) ;
#58868 = EDGE_CURVE ( 'NONE', #11696, #518, #45272, .T. ) ;
#58869 = EDGE_CURVE ( 'NONE', #59745, #46774, #54496, .T. ) ;
#58870 = CARTESIAN_POINT ( 'NONE',  ( 6.702501388090612799, 4.665922358581495288, -8.797387867328911426 ) ) ;
#58871 = CARTESIAN_POINT ( 'NONE',  ( 9.206076168957999073, -4.439974903344300117, -8.247081005603298820 ) ) ;
#58872 = CARTESIAN_POINT ( 'NONE',  ( 5.857901922764000346, -1.131660731475000015, -0.3201946116248999830 ) ) ;
#58873 = DIRECTION ( 'NONE',  ( 1.000000000000000000, 0.000000000000000000, 0.000000000000000000 ) ) ;
#58874 = CARTESIAN_POINT ( 'NONE',  ( 25.29987333571600061, -10.83443035398000021, -3.855530949778000149 ) ) ;
#58875 = VERTEX_POINT ( 'NONE', #29247 ) ;
#58876 = CARTESIAN_POINT ( 'NONE',  ( 12.23161381921988600, -0.2487950381773050834, -12.69672507751632828 ) ) ;
#58877 = CARTESIAN_POINT ( 'NONE',  ( 9.972537864286000087, -2.899999999999999911, -6.571291218949999902 ) ) ;
#58878 = CARTESIAN_POINT ( 'NONE',  ( 5.477523075960000654, -12.82224764859999766, 2.276049205302000278 ) ) ;
#58879 = CARTESIAN_POINT ( 'NONE',  ( 2.134821978926408459, 2.196258588983220683, -2.381953655762986788 ) ) ;
#58880 = CARTESIAN_POINT ( 'NONE',  ( 3.500000000000000888, -1.551591189650207037, 2.828749889131733752 ) ) ;
#58881 = ORIENTED_EDGE ( 'NONE', *, *, #39533, .F. ) ;
#58882 = CARTESIAN_POINT ( 'NONE',  ( 25.31013104180999918, -11.20357036551999919, -3.315088882916999768 ) ) ;
#58883 = ITEM_DEFINED_TRANSFORMATION ( 'NONE', 'NONE', #29638,  #9676 ) ;
#58885 = CARTESIAN_POINT ( 'NONE',  ( 11.27745123989519982, -3.589787500396900199, -8.292221125039500151 ) ) ;
#58884 =( BOUNDED_SURFACE ( )  B_SPLINE_SURFACE ( 3, 3, ( 
 ( #21598, #68802, #5183, #10081, #42937, #58323, #64245, #11120, #37688 ),
 ( #20923, #53769, #27205, #26172, #48526, #42259, #63563, #15677, #37006 ),
 ( #10424, #31766, #53083, #60737, #49211, #60050, #7253, #54110, #6206 ),
 ( #50252, #33835, #44677, #49905, #18443, #45015, #982, #1318, #33141 ) ),
 .UNSPECIFIED., .F., .F., .T. ) 
 B_SPLINE_SURFACE_WITH_KNOTS ( ( 4, 4 ),
 ( 4, 1, 1, 1, 1, 1, 4 ),
 ( 0.000000000000000000, 1.000000000000000000 ),
 ( -0.004646279661397999423, 0.000000000000000000, 0.03269534097185999855, 0.06255479614191999937, 0.08986301827557000022, 0.1148786485006999952, 0.1376622693536999897 ),
 .UNSPECIFIED. ) 
 GEOMETRIC_REPRESENTATION_ITEM ( )  RATIONAL_B_SPLINE_SURFACE ( (
 ( 1.187699524740999824, 1.187699524740999824, 1.187699524740999824, 1.187699524740999824, 1.187699524740999824, 1.187699524740999824, 1.187699524740999824, 1.187699524740999824, 1.187699524740999824),
 ( 0.9374334917530999789, 0.9374334917530999789, 0.9374334917530999789, 0.9374334917530999789, 0.9374334917530999789, 0.9374334917530999789, 0.9374334917530999789, 0.9374334917530999789, 0.9374334917530999789),
 ( 0.9374334917530999789, 0.9374334917530999789, 0.9374334917530999789, 0.9374334917530999789, 0.9374334917530999789, 0.9374334917530999789, 0.9374334917530999789, 0.9374334917530999789, 0.9374334917530999789),
 ( 1.187699524740999824, 1.187699524740999824, 1.187699524740999824, 1.187699524740999824, 1.187699524740999824, 1.187699524740999824, 1.187699524740999824, 1.187699524740999824, 1.187699524740999824) ) ) 
 REPRESENTATION_ITEM ( '' )  SURFACE ( )  );
#58886 = DIRECTION ( 'NONE',  ( 0.000000000000000000, 0.000000000000000000, -1.000000000000000000 ) ) ;
#58887 = EDGE_CURVE ( 'NONE', #41143, #59809, #1059, .T. ) ;
#58888 = CARTESIAN_POINT ( 'NONE',  ( 13.70006033574439286, -11.41449502534927163, -2.331043471727575422 ) ) ;
#58889 = LINE ( 'NONE', #53301, #6016 ) ;
#58890 = CARTESIAN_POINT ( 'NONE',  ( 10.35814141025499957, 4.483492689244800822, -8.361148840840000318 ) ) ;
#58891 = ORIENTED_EDGE ( 'NONE', *, *, #46237, .T. ) ;
#58892 = VECTOR ( 'NONE', #24588, 1000.000000000000000 ) ;
#58893 = CARTESIAN_POINT ( 'NONE',  ( 10.24478558459999888, -5.265199116477000452, 8.959495174640998982 ) ) ;
#58894 = CARTESIAN_POINT ( 'NONE',  ( 8.720712484379999907, -4.219532685969900498, -8.340498368324299250 ) ) ;
#58895 = EDGE_LOOP ( 'NONE', ( #14689, #41704, #39325, #18241, #60787 ) ) ;
#58896 = CARTESIAN_POINT ( 'NONE',  ( 13.66714157633269444, 11.44713007569950669, 2.165075719398914966 ) ) ;
#58897 = CARTESIAN_POINT ( 'NONE',  ( 8.032370559622998840, -3.524751762020000179, 5.573845465339999805 ) ) ;
#58898 =( GEOMETRIC_REPRESENTATION_CONTEXT ( 3 ) GLOBAL_UNCERTAINTY_ASSIGNED_CONTEXT ( ( #5211 ) ) GLOBAL_UNIT_ASSIGNED_CONTEXT ( ( #29365, #66055, #50680 ) ) REPRESENTATION_CONTEXT ( 'NONE', 'WORKASPACE' ) );
#58899 = CARTESIAN_POINT ( 'NONE',  ( 9.667489158770999680, 4.808846957865000604, -8.639578604182998944 ) ) ;
#58900 = EDGE_LOOP ( 'NONE', ( #47362, #48321, #34060, #47130 ) ) ;
#58901 = CARTESIAN_POINT ( 'NONE',  ( 6.421289894894001371, 1.034288144986173608, 1.130377649294558973 ) ) ;
#58902 = CARTESIAN_POINT ( 'NONE',  ( 7.572795280404999829, 2.598436872309000112, -6.481704782070000448 ) ) ;
#58903 = CIRCLE ( 'NONE', #24320, 2.250000000000000000 ) ;
#58904 = CARTESIAN_POINT ( 'NONE',  ( -0.2999999999999999889, 1.154700538379000108, 0.000000000000000000 ) ) ;
#58905 = CARTESIAN_POINT ( 'NONE',  ( 9.488130154828182228, 4.942993110859213779, 8.465850029259959442 ) ) ;
#58906 = VERTEX_POINT ( 'NONE', #50557 ) ;
#58907 = CARTESIAN_POINT ( 'NONE',  ( 9.753140057121997941, -4.104977100659999323, 9.293279163877999238 ) ) ;
#58908 = FACE_OUTER_BOUND ( 'NONE', #39172, .T. ) ;
#58909 = DIRECTION ( 'NONE',  ( -1.000000000000000000, 0.000000000000000000, 0.000000000000000000 ) ) ;
#58910 = EDGE_LOOP ( 'NONE', ( #40863, #48135, #64898, #50175 ) ) ;
#58911 = AXIS2_PLACEMENT_3D ( 'NONE', #37556, #31988, #48745 ) ;
#58912 = CARTESIAN_POINT ( 'NONE',  ( 6.107109839683332986, -1.199500263597270244, -0.9218200799623728070 ) ) ;
#58913 = CARTESIAN_POINT ( 'NONE',  ( 10.31152944037999930, -2.716820959546999870, -7.950167805575999225 ) ) ;
#58914 = EDGE_LOOP ( 'NONE', ( #17946, #60444, #66115, #60956 ) ) ;
#58915 = CARTESIAN_POINT ( 'NONE',  ( 4.879623228227333520, 1.445318020077273502, 0.4634605740919915950 ) ) ;
#58916 = CARTESIAN_POINT ( 'NONE',  ( 17.77886761546800187, -1.796012712130053313, -12.47134082573985658 ) ) ;
#58917 = CARTESIAN_POINT ( 'NONE',  ( 4.784861683301000923, 1.115330177132999978, 0.8731915261176000920 ) ) ;
#58918 = CARTESIAN_POINT ( 'NONE',  ( 7.737176379004002236, 4.819032099609000142, -6.334771630424004485 ) ) ;
#58919 = CARTESIAN_POINT ( 'NONE',  ( 16.20650642310300071, 3.719849042574000286, 12.00042637259999978 ) ) ;
#58920 = CARTESIAN_POINT ( 'NONE',  ( 10.42914631115497315, 5.349770684922701136, 7.570573233677396097 ) ) ;
#58921 = CARTESIAN_POINT ( 'NONE',  ( 24.30001696810800027, 12.21047201856000086, 3.271805692349999628 ) ) ;
#58922 = AXIS2_PLACEMENT_3D ( 'NONE', #3026, #29967, #3700 ) ;
#58923 = EDGE_CURVE ( 'NONE', #7995, #64186, #33982, .T. ) ;
#58924 = B_SPLINE_SURFACE_WITH_KNOTS ( 'NONE', 3, 3, ( 
 ( #14280, #30030, #49002, #35606, #56919, #24073, #19516, #40836, #17180, #55551, #43767, #24761, #40165, #3087, #13936, #38509, #62159, #51332, #8682 ),
 ( #60791, #66370, #50306, #61480, #45410, #12904, #45748, #2404, #27688, #46087, #34232, #29336, #67058, #66719, #50648, #35263, #7649, #67395, #28997 ),
 ( #18838, #19168, #23728, #39818, #45066, #13256, #34581, #13599, #40492, #34920, #61819, #56580, #25101, #26139, #63869, #35937, #36279, #57595, #68422 ),
 ( #42224, #31048, #9019, #30359, #41189, #14618, #41523, #53051, #51667, #57952, #41868, #46433, #36629, #9702, #31387, #52357, #58288, #10051, #52701 ) ),
 .UNSPECIFIED., .F., .F., .F.,
 ( 4, 4 ),
 ( 4, 1, 1, 1, 1, 1, 1, 1, 1, 1, 1, 1, 1, 1, 1, 1, 4 ),
 ( -0.1039086239011999951, 1.103908623900999864 ),
 ( -0.008849010032007000384, 0.01991027257200999809, 0.04866955517603999831, 0.07742883778006000306, 0.1061881203840999988, 0.1349474029881000126, 0.1637066855920999986, 0.1924659681960999846, 0.2212252508002000018, 0.2499845334042000156, 0.2787438160081999738, 0.3075030986121999876, 0.3362623812162000014, 0.3650216638202999908, 0.3937809464243000046, 0.4225402290282999629, 0.4512995116322999767 ),
 .UNSPECIFIED. ) ;
#58925 = VERTEX_POINT ( 'NONE', #23985 ) ;
#58926 = CARTESIAN_POINT ( 'NONE',  ( 17.55505043854147118, -1.875000000000000000, -12.57541666120755863 ) ) ;
#58927 = VERTEX_POINT ( 'NONE', #6862 ) ;
#58928 = CARTESIAN_POINT ( 'NONE',  ( 10.55813337864000090, 2.466561068647000532, 6.633529813744000414 ) ) ;
#58929 = FACE_OUTER_BOUND ( 'NONE', #55459, .T. ) ;
#58930 = CARTESIAN_POINT ( 'NONE',  ( 17.82606829449534658, -12.11439310048800877, 3.181038237424487214 ) ) ;
#58931 = CARTESIAN_POINT ( 'NONE',  ( 9.020585841232000135, 4.920236664407999783, -6.448229650796999834 ) ) ;
#58932 = CARTESIAN_POINT ( 'NONE',  ( 5.500000000000000000, 0.000000000000000000, 0.000000000000000000 ) ) ;
#58933 = CARTESIAN_POINT ( 'NONE',  ( 18.06357043707759402, -0.3639325664385105186, 13.89360161040563035 ) ) ;
#58934 = CARTESIAN_POINT ( 'NONE',  ( 18.06407613809071577, 0.3627976897793646627, 13.89363072199764204 ) ) ;
#58935 = ORIENTED_EDGE ( 'NONE', *, *, #47292, .F. ) ;
#58936 = CARTESIAN_POINT ( 'NONE',  ( 12.38194801265183109, 0.4608083867824496749, 13.88973595540270978 ) ) ;
#58937 = CIRCLE ( 'NONE', #62284, 11.29999999999999538 ) ;
#58938 = CARTESIAN_POINT ( 'NONE',  ( 11.70733594839949809, -3.159733897807000425, 8.462948211532999920 ) ) ;
#58939 = CARTESIAN_POINT ( 'NONE',  ( 7.100000000000000533, -13.04986661130000059, -1.811520473896000016 ) ) ;
#58940 = CARTESIAN_POINT ( 'NONE',  ( 7.641206853206999661, -4.524489047957000132, 9.047757046927999980 ) ) ;
#58942 = CARTESIAN_POINT ( 'NONE',  ( 12.62563329236320619, -11.41733447966565862, 4.609296053777788060 ) ) ;
#58941 = CARTESIAN_POINT ( 'NONE',  ( 11.08992526467999973, 5.210543602612999869, 8.327598319864998544 ) ) ;
#58943 = CARTESIAN_POINT ( 'NONE',  ( 10.30072469555899950, 4.570852684939899824, -6.512367818249299667 ) ) ;
#58944 = CARTESIAN_POINT ( 'NONE',  ( 24.66122485234200212, -8.759220508654999904, -9.243943008462998989 ) ) ;
#58945 = AXIS2_PLACEMENT_3D ( 'NONE', #35750, #57068, #68575 ) ;
#58946 = CARTESIAN_POINT ( 'NONE',  ( 9.450367640780999778, 4.408706755790200660, -6.735364967924099666 ) ) ;
#58947 = CARTESIAN_POINT ( 'NONE',  ( 18.13994946422174337, -0.2205037192104046251, 12.69742880170239019 ) ) ;
#58948 = CARTESIAN_POINT ( 'NONE',  ( 6.604081922979999852, -1.551699729542000084, -0.09740341920656001018 ) ) ;
#58949 = VECTOR ( 'NONE', #44855, 1000.000000000000000 ) ;
#58950 = CARTESIAN_POINT ( 'NONE',  ( 7.100000000000000533, 0.000000000000000000, 0.000000000000000000 ) ) ;
#58951 = VERTEX_POINT ( 'NONE', #12814 ) ;
#58952 = CARTESIAN_POINT ( 'NONE',  ( 8.315519353208999931, -5.485781663882000281, 8.532068390166999805 ) ) ;
#58953 = CARTESIAN_POINT ( 'NONE',  ( 8.150000662387999029, 3.037570195374000164E-13, -3.945735770681999509E-14 ) ) ;
#58954 = ADVANCED_FACE ( 'NONE', ( #22940 ), #48309, .F. ) ;
#58955 = ADVANCED_FACE ( 'NONE', ( #59227 ), #63437, .T. ) ;
#58956 = CARTESIAN_POINT ( 'NONE',  ( 24.30000000000000071, 8.756202924575998026, -7.455126447192999883 ) ) ;
#58957 = CARTESIAN_POINT ( 'NONE',  ( 10.98768472567999943, 6.720753181080999283, 5.471698459870999898 ) ) ;
#58958 = ORIENTED_EDGE ( 'NONE', *, *, #894, .F. ) ;
#58959 = VECTOR ( 'NONE', #30598, 1000.000000000000000 ) ;
#58960 = CARTESIAN_POINT ( 'NONE',  ( 0.7818389912891999805, 2.420060471650000267, -2.350339292168000416 ) ) ;
#58961 = DIRECTION ( 'NONE',  ( -1.000000000000000000, 0.000000000000000000, 0.000000000000000000 ) ) ;
#58962 = CARTESIAN_POINT ( 'NONE',  ( 10.91733584123000078, 3.256275267152000108, -6.361562334135999919 ) ) ;
#58963 = ORIENTED_EDGE ( 'NONE', *, *, #45927, .T. ) ;
#58964 = CARTESIAN_POINT ( 'NONE',  ( 9.393930206848999376, 2.750000000000000000, -7.500000000000000000 ) ) ;
#58965 = CARTESIAN_POINT ( 'NONE',  ( 10.36409408021999923, -3.399999909169000301, -4.954046131279000065 ) ) ;
#58966 = CARTESIAN_POINT ( 'NONE',  ( 18.24165222613598303, 2.712088604378295909, -12.30466175173926935 ) ) ;
#58967 = CARTESIAN_POINT ( 'NONE',  ( 8.599999986286999132, 3.249999986289399789, -7.499999999961952213 ) ) ;
#58968 = CARTESIAN_POINT ( 'NONE',  ( 7.501448341228000416, 2.138190256467000339, 6.814770510101999967 ) ) ;
#58969 = ORIENTED_EDGE ( 'NONE', *, *, #22389, .T. ) ;
#58970 = CARTESIAN_POINT ( 'NONE',  ( 5.730001685446000081, 0.8487381973356000753, -1.373673328256999948 ) ) ;
#58971 = B_SPLINE_CURVE_WITH_KNOTS ( 'NONE', 3,
 ( #25522, #46850, #42632, #68154, #37384, #20273 ),
 .UNSPECIFIED., .F., .F.,
 ( 4, 2, 4 ),
 ( 0.000000000000000000, 0.3470917641979919255, 0.6941835283959838510 ),
 .UNSPECIFIED. ) ;
#58972 = CARTESIAN_POINT ( 'NONE',  ( 6.911604719590999757, 5.620828677136000096, -7.589710348707000342 ) ) ;
#58973 = ADVANCED_FACE ( 'NONE', ( #26394 ), #53336, .F. ) ;
#58974 = CARTESIAN_POINT ( 'NONE',  ( 8.319350023656893356, -4.124618607633898648, 9.242618487877578559 ) ) ;
#58975 = CARTESIAN_POINT ( 'NONE',  ( 9.624051052051999733, -2.744602294987000146, 7.254315263553399618 ) ) ;
#58977 = ORIENTED_EDGE ( 'NONE', *, *, #44161, .T. ) ;
#58976 = VECTOR ( 'NONE', #54289, 1000.000000000000114 ) ;
#58978 = DIRECTION ( 'NONE',  ( 0.000000000000000000, 1.000000000000000000, 0.000000000000000000 ) ) ;
#58979 = CARTESIAN_POINT ( 'NONE',  ( 11.68610928851700237, 11.49703662065999943, 1.632765284408000062 ) ) ;
#58980 = ORIENTED_EDGE ( 'NONE', *, *, #50775, .T. ) ;
#58981 = EDGE_CURVE ( 'NONE', #48042, #47885, #28116, .T. ) ;
#58982 = DIRECTION ( 'NONE',  ( 1.000000000000000000, 0.000000000000000000, 0.000000000000000000 ) ) ;
#58983 = DIRECTION ( 'NONE',  ( 1.000000000000000000, 0.000000000000000000, 0.000000000000000000 ) ) ;
#58984 = CARTESIAN_POINT ( 'NONE',  ( 17.55505043854143921, 0.6250000000000002220, -13.88107975066922428 ) ) ;
#58985 = EDGE_LOOP ( 'NONE', ( #30851, #31539, #335, #5741, #16183, #36906, #48286, #12660, #9897, #35357, #55792 ) ) ;
#58986 = CARTESIAN_POINT ( 'NONE',  ( 11.07508065833999922, -8.038176207971000409, 6.929846776222000848 ) ) ;
#58987 = CARTESIAN_POINT ( 'NONE',  ( 9.803754904607863807, -2.991223623039768853, -8.479528301168882010 ) ) ;
#58988 = CARTESIAN_POINT ( 'NONE',  ( 24.14474118650271706, -12.92575622504552690, 3.214623506209951742 ) ) ;
#58989 = CARTESIAN_POINT ( 'NONE',  ( 12.48990506108388665, 3.039826403548175460, -12.30927084193774235 ) ) ;
#58990 = CARTESIAN_POINT ( 'NONE',  ( 11.73195122972050086, -3.492749840905900349, 8.673036084990000560 ) ) ;
#58991 = ORIENTED_EDGE ( 'NONE', *, *, #43001, .T. ) ;
#58992 = CARTESIAN_POINT ( 'NONE',  ( 7.149100552923999707, 4.351669901925999895, 8.977196921526999773 ) ) ;
#58993 = EDGE_LOOP ( 'NONE', ( #23847, #48474, #61676, #60656, #5827 ) ) ;
#58994 = CARTESIAN_POINT ( 'NONE',  ( 9.393930206848999376, 2.750000000000000000, -7.500000000000000000 ) ) ;
#58995 = CARTESIAN_POINT ( 'NONE',  ( 16.04331666222400088, -9.026410239312999906, -8.606113518243997618 ) ) ;
#58996 = CARTESIAN_POINT ( 'NONE',  ( 11.07071178722999960, 5.425106496613000040, -5.078392693150000525 ) ) ;
#58997 = ORIENTED_EDGE ( 'NONE', *, *, #58391, .T. ) ;
#58998 = DIRECTION ( 'NONE',  ( 0.000000000000000000, 1.000000000000000000, 0.000000000000000000 ) ) ;
#58999 = CARTESIAN_POINT ( 'NONE',  ( 16.10004050617000360, -8.286228349446556507, -9.446703038322569412 ) ) ;
#59000 = DIRECTION ( 'NONE',  ( 0.000000000000000000, 0.000000000000000000, -1.000000000000000000 ) ) ;
#59001 = CARTESIAN_POINT ( 'NONE',  ( 5.000030787343000327, -2.099962892531005210, 0.2748844998327746869 ) ) ;
#59002 = CARTESIAN_POINT ( 'NONE',  ( 12.63921101284457293, -1.806754227364050669, -13.88292698645336465 ) ) ;
#59003 = B_SPLINE_CURVE_WITH_KNOTS ( 'NONE', 3,
 ( #7330, #2101, #23418, #66057, #18175, #18866, #40521, #40194, #61510, #34613, #61168, #9382, #19199, #24451 ),
 .UNSPECIFIED., .F., .F.,
 ( 4, 2, 2, 2, 2, 2, 4 ),
 ( 0.1252897355259763035, 0.3125850975489872230, 0.4998804595719981148, 0.5935281405835034496, 0.6871758215950088955, 0.7808235026065142304, 0.8744711836180196762 ),
 .UNSPECIFIED. ) ;
#59004 = CIRCLE ( 'NONE', #16571, 12.50000000000000000 ) ;
#59005 = CARTESIAN_POINT ( 'NONE',  ( 10.82179975933729921, -3.051121678931899783, -7.173532873542499466 ) ) ;
#59006 = DIRECTION ( 'NONE',  ( 1.000000000000000000, 0.000000000000000000, 0.000000000000000000 ) ) ;
#59007 = CARTESIAN_POINT ( 'NONE',  ( 17.79586754331425524, -3.158948767300545413, 12.19758365745370021 ) ) ;
#59008 = VERTEX_POINT ( 'NONE', #33012 ) ;
#59009 = CARTESIAN_POINT ( 'NONE',  ( 10.76346886766499900, -4.634677072395899877, -6.346853961441000003 ) ) ;
#59010 = ORIENTED_EDGE ( 'NONE', *, *, #52244, .F. ) ;
#59011 = CIRCLE ( 'NONE', #61264, 11.50000000000000178 ) ;
#59012 = CARTESIAN_POINT ( 'NONE',  ( 25.30000327618300204, -0.6965695964343677771, -11.50000000000000000 ) ) ;
#59013 = CARTESIAN_POINT ( 'NONE',  ( 5.000000000000000000, -1.352284263959000032, -11.01731942304999912 ) ) ;
#59014 = CARTESIAN_POINT ( 'NONE',  ( 9.961660622462840564, 5.351629337096509786, 7.263483964539687143 ) ) ;
#59015 = CARTESIAN_POINT ( 'NONE',  ( 10.21685100254000034, -2.832432432432000269, 6.822293592207000934 ) ) ;
#59016 = CARTESIAN_POINT ( 'NONE',  ( 8.767881343006999728, -4.605543323398999966, -6.293427432547999523 ) ) ;
#59017 = PRODUCT_DEFINITION ( 'UNKNOWN', '', #32954, #68144 ) ;
#59018 = CARTESIAN_POINT ( 'NONE',  ( 23.62948033907000323, -13.46907223791000163, 3.826138227952000204 ) ) ;
#59019 = CARTESIAN_POINT ( 'NONE',  ( 10.62697636434999993, 3.142921793056999924, 8.668445734229999644 ) ) ;
#59020 = ORIENTED_EDGE ( 'NONE', *, *, #48840, .T. ) ;
#59021 = CARTESIAN_POINT ( 'NONE',  ( 8.789886373836322875, 4.000007821194420110, 6.560153657526067938 ) ) ;
#59022 = CARTESIAN_POINT ( 'NONE',  ( 10.31167969999000000, 2.874476822401000220, 8.900029516786000627 ) ) ;
#59023 = CARTESIAN_POINT ( 'NONE',  ( 2.103056799209332528, 2.798833948393625981, 2.150913519912208471 ) ) ;
#59024 = CARTESIAN_POINT ( 'NONE',  ( 11.93856039236529831, -2.967715280237000375, 7.449760924956519759 ) ) ;
#59025 = CARTESIAN_POINT ( 'NONE',  ( 18.23887202961200060, 3.252214874110999965, -11.14733497513999971 ) ) ;
#59026 = AXIS2_PLACEMENT_3D ( 'NONE', #57542, #4739, #26083 ) ;
#59027 = CARTESIAN_POINT ( 'NONE',  ( 11.00075737667999931, 8.791598996395000754, -6.553657304443999188 ) ) ;
#59028 = B_SPLINE_CURVE_WITH_KNOTS ( 'NONE', 3,
 ( #28968, #7275, #2039, #49230 ),
 .UNSPECIFIED., .F., .F.,
 ( 4, 4 ),
 ( 0.000000000000000000, 1.000000000000000000 ),
 .UNSPECIFIED. ) ;
#59029 = CARTESIAN_POINT ( 'NONE',  ( 12.44044950778751080, -0.5080407711865464471, 12.68632595416892883 ) ) ;
#59030 = CARTESIAN_POINT ( 'NONE',  ( 23.91258968280600072, -9.487094596478000241, -9.248012932198999891 ) ) ;
#59031 = CARTESIAN_POINT ( 'NONE',  ( 18.50003594167399967, -2.686563651857999613, -11.33603604486000016 ) ) ;
#59032 = EDGE_LOOP ( 'NONE', ( #16418, #17103, #10833 ) ) ;
#59033 = CARTESIAN_POINT ( 'NONE',  ( 6.633333333537346554, 12.50865282024215297, -2.924692170536358660 ) ) ;
#59034 = CARTESIAN_POINT ( 'NONE',  ( 7.194243953316000528, 0.9749085416657999881, 0.7832989749747000241 ) ) ;
#59035 = EDGE_CURVE ( 'NONE', #32586, #37575, #51163, .T. ) ;
#59036 = EDGE_CURVE ( 'NONE', #28970, #12254, #28823, .T. ) ;
#59037 = CARTESIAN_POINT ( 'NONE',  ( 18.17246482408070918, 2.400822122662769509, 13.69396077230720721 ) ) ;
#59038 = CARTESIAN_POINT ( 'NONE',  ( 24.60320129348500018, 8.810542265399000428, -9.295223627480998729 ) ) ;
#59039 = CARTESIAN_POINT ( 'NONE',  ( 11.08841369783139896, -4.057552111898620417, -8.639288317626999003 ) ) ;
#59040 = VERTEX_POINT ( 'NONE', #60963 ) ;
#59041 = CARTESIAN_POINT ( 'NONE',  ( 5.699999545467999695, -12.03770622561999915, 3.722046322334000124 ) ) ;
#59042 = CARTESIAN_POINT ( 'NONE',  ( 7.731795280408999993, 4.580608786027000612, 9.213365309690999538 ) ) ;
#59044 = CARTESIAN_POINT ( 'NONE',  ( 27.09999999999999787, 0.000000000000000000, 0.000000000000000000 ) ) ;
#59043 = CARTESIAN_POINT ( 'NONE',  ( 8.854170280414001226, 4.902869380824999901, -8.978557145469999057 ) ) ;
#59045 = CARTESIAN_POINT ( 'NONE',  ( 10.65445404538374241, 3.176394930960259266, 4.782660509943262639 ) ) ;
#59046 = EDGE_LOOP ( 'NONE', ( #36377, #47332, #8856, #28019 ) ) ;
#59047 = CARTESIAN_POINT ( 'NONE',  ( 9.500006116823001889, 2.279680316922000127, 7.877692351087999256 ) ) ;
#59049 = CARTESIAN_POINT ( 'NONE',  ( 17.65774109649150958, -3.116847231231422377, -13.52303903038508004 ) ) ;
#59048 = CIRCLE ( 'NONE', #30077, 1.350000000000000533 ) ;
#59050 = CARTESIAN_POINT ( 'NONE',  ( 10.55103166480599874, 2.999015536536000504, 7.429424106427209296 ) ) ;
#59051 = CARTESIAN_POINT ( 'NONE',  ( 10.68361719090999884, -2.603550124652000086, 7.762065570229999878 ) ) ;
#59052 = CARTESIAN_POINT ( 'NONE',  ( 8.411456853209999807, -3.882020254083999866, 5.870054788755000530 ) ) ;
#59053 = EDGE_LOOP ( 'NONE', ( #41876, #27779, #50483, #17296 ) ) ;
#59054 = LINE ( 'NONE', #53804, #67833 ) ;
#59056 = CARTESIAN_POINT ( 'NONE',  ( 9.991527686541001430, -4.805948463426999773, -8.932428271061001013 ) ) ;
#59055 = CARTESIAN_POINT ( 'NONE',  ( 12.32697677577000128, -11.50538345640999971, 4.553133914476999777 ) ) ;
#59057 = CARTESIAN_POINT ( 'NONE',  ( 7.739691844317393432, -5.527372948754030624, 8.333565270828541927 ) ) ;
#59058 = FACE_OUTER_BOUND ( 'NONE', #7440, .T. ) ;
#59059 = CARTESIAN_POINT ( 'NONE',  ( 0.1499996298882999846, 0.000000000000000000, 0.000000000000000000 ) ) ;
#59060 = ORIENTED_EDGE ( 'NONE', *, *, #706, .F. ) ;
#59061 = CARTESIAN_POINT ( 'NONE',  ( 9.529346873515667227, 4.163624617374466652, -8.749999999999998224 ) ) ;
#59062 = CARTESIAN_POINT ( 'NONE',  ( 11.05103166480599874, -5.000984463463999496, 7.429424106427209296 ) ) ;
#59063 = EDGE_CURVE ( 'NONE', #509, #28630, #65853, .T. ) ;
#59064 = CARTESIAN_POINT ( 'NONE',  ( 10.27610941423800028, 4.844410192686099847, 8.266982106121901097 ) ) ;
#59065 = ORIENTED_EDGE ( 'NONE', *, *, #10436, .F. ) ;
#59066 = B_SPLINE_SURFACE_WITH_KNOTS ( 'NONE', 3, 3, ( 
 ( #20476, #45430, #63459, #8021, #36214, #2771, #9634, #25722, #47055, #29359, #41804, #50672, #13619, #34942, #63107, #57883, #9984, #52632, #11699, #58566, #32357, #880, #16260, #48082, #16941, #185, #5431, #12056, #33039, #5766, #64145, #38274, #43874, #10671, #26771 ),
 ( #64484, #1222, #27108, #531, #64831, #22196, #32017, #53331, #43532, #22535, #21503, #49111, #65180, #59601, #37584, #11020, #32694, #16606, #42836, #58917, #54351, #17299, #6455, #37931, #38624, #53673, #27805, #59945, #59250, #48424, #21845, #48772, #11356, #43179, #54007 ),
 ( #6109, #27448, #57750, #16139, #10207, #68577, #9862, #4268, #31540, #58444, #30852, #26644, #52860, #68931, #46931, #58105, #59, #47620, #21045, #42377, #15460, #37462, #47961, #15113, #25944, #47277, #41340, #63682, #20700, #15797, #10546, #25604, #58786, #67898, #52510 ),
 ( #4960, #21382, #68234, #26294, #42029, #20016, #36785, #51820, #37126, #31890, #42714, #20356, #53201, #36433, #64018, #4610, #41679, #5302, #62653, #63331, #3918, #46592, #10892, #25254, #14773, #36091, #57405, #9510, #52166, #62984, #31206, #48648, #11925, #11233, #21718 ) ),
 .UNSPECIFIED., .F., .F., .F.,
 ( 4, 4 ),
 ( 4, 1, 1, 1, 1, 1, 1, 1, 1, 1, 1, 1, 1, 1, 1, 1, 1, 1, 1, 1, 1, 1, 1, 1, 1, 1, 1, 1, 1, 1, 1, 1, 4 ),
 ( -0.02636945251836000231, 1.026369452518000047 ),
 ( -0.01357143068969000020, 0.008482144181056000543, 0.03053571905179999768, 0.05258929392254999696, 0.07464286879330001012, 0.09669644366403999658, 0.1187500185347999948, 0.1408035934054999994, 0.1628571682763000072, 0.1849107431469999840, 0.2069643180178000197, 0.2290178928884999965, 0.2510714677593000044, 0.2731250426299999812, 0.2951786175007999891, 0.3172321923715000214, 0.3392857672423000293, 0.3613393421130000061, 0.3833929169837999584, 0.4054464918545000462, 0.4275000667252000230, 0.4495536415960000309, 0.4716072164667000077, 0.4936607913374999601, 0.5157143662081999924, 0.5377679410790000558, 0.5598215159496999771, 0.5818750908205000405, 0.6039286656911999618, 0.6259822405620000252, 0.6480358154326999465, 0.6700893903035000099, 0.6921429651742000422 ),
 .UNSPECIFIED. ) ;
#59067 = CARTESIAN_POINT ( 'NONE',  ( 8.813304719595000947, 3.880154689736000417, -9.060377011187000562 ) ) ;
#59068 = CARTESIAN_POINT ( 'NONE',  ( 12.20599951553714924, 2.074681531931801715, -12.42802467457380899 ) ) ;
#59069 = CARTESIAN_POINT ( 'NONE',  ( 10.94999293566599974, -3.279967330949900450, 6.616719557880299085 ) ) ;
#59070 = ORIENTED_EDGE ( 'NONE', *, *, #29769, .F. ) ;
#59071 = CARTESIAN_POINT ( 'NONE',  ( 7.948851576340711489, 4.916978202369310935, -6.401965507567116020 ) ) ;
#59072 = CARTESIAN_POINT ( 'NONE',  ( 18.17219575274162935, 2.599291946997700276, -13.65190342897701470 ) ) ;
#59073 = ORIENTED_EDGE ( 'NONE', *, *, #45108, .F. ) ;
#59074 = CARTESIAN_POINT ( 'NONE',  ( 8.432504440379000599, -5.430412429559000387, 7.210798766422999329 ) ) ;
#59075 = CARTESIAN_POINT ( 'NONE',  ( 9.099999986286999132, -3.249999986289399789, 7.499999999961952213 ) ) ;
#59076 = VERTEX_POINT ( 'NONE', #60618 ) ;
#59077 = CARTESIAN_POINT ( 'NONE',  ( 9.934999999999998721, -4.640430492595999823, -9.117542781427999898 ) ) ;
#59078 = CARTESIAN_POINT ( 'NONE',  ( 10.77256919669529900, 4.962345366016100101, 7.215672285280100517 ) ) ;
#59079 = CARTESIAN_POINT ( 'NONE',  ( 10.50285691784999997, 5.158890929072000198, 8.369954994793999958 ) ) ;
#59080 = CARTESIAN_POINT ( 'NONE',  ( 10.87696123885999810, 5.827079664135999870, -7.814747088295999511 ) ) ;
#59081 = CARTESIAN_POINT ( 'NONE',  ( 25.60000000000000142, 0.000000000000000000, 0.000000000000000000 ) ) ;
#59082 = CARTESIAN_POINT ( 'NONE',  ( 10.05691733561000056, -2.453480799114999833, 6.657106310117000270 ) ) ;
#59083 = CARTESIAN_POINT ( 'NONE',  ( 17.57569811463524445, 0.6249994333735308105, -12.67928921956171173 ) ) ;
#59084 = CARTESIAN_POINT ( 'NONE',  ( 12.63924565014722923, 1.874999999999999556, -12.57545536278438902 ) ) ;
#59085 = CARTESIAN_POINT ( 'NONE',  ( 11.04333729122639873, -5.003122373830000136, -7.473611442402849470 ) ) ;
#59086 = CARTESIAN_POINT ( 'NONE',  ( 7.507482780409000078, 3.501518846194999757, 9.055971388486000251 ) ) ;
#59087 = EDGE_LOOP ( 'NONE', ( #66104, #6186, #39366, #45017, #26843 ) ) ;
#59088 =( LENGTH_UNIT ( ) NAMED_UNIT ( * ) SI_UNIT ( .MILLI., .METRE. ) );
#59089 = CARTESIAN_POINT ( 'NONE',  ( 23.56666365135700403, -11.07911597677999360, 4.076188921367005058 ) ) ;
#59090 = CARTESIAN_POINT ( 'NONE',  ( 9.246656068972805897, 2.697145242899015471, 7.146653512472456171 ) ) ;
#59091 = CARTESIAN_POINT ( 'NONE',  ( 11.42397234076999979, 12.13750352647000064, 1.893412522203000048 ) ) ;
#59092 = CARTESIAN_POINT ( 'NONE',  ( 18.23533704695767810, 2.231030541001932210, 12.40091240268597872 ) ) ;
#59093 = EDGE_CURVE ( 'NONE', #12815, #55845, #61113, .T. ) ;
#59094 = CARTESIAN_POINT ( 'NONE',  ( 11.02144803208000035, 6.116354541702999192, 5.112466721998999652 ) ) ;
#59095 = ADVANCED_FACE ( 'NONE', ( #55374 ), #30526, .T. ) ;
#59096 = CARTESIAN_POINT ( 'NONE',  ( 11.12483613036000030, 7.237663138348001013, 6.298788344941000261 ) ) ;
#59097 = CARTESIAN_POINT ( 'NONE',  ( 9.070985106021000277, -8.666611253863997888, -6.095301607234000052 ) ) ;
#59098 = DIRECTION ( 'NONE',  ( 1.000000000000000000, 0.000000000000000000, 0.000000000000000000 ) ) ;
#59099 = EDGE_LOOP ( 'NONE', ( #17080, #45867, #61453, #60142 ) ) ;
#59100 = CARTESIAN_POINT ( 'NONE',  ( 12.28182936075429943, -2.978585426876346087, 12.24287970063667252 ) ) ;
#59101 = CARTESIAN_POINT ( 'NONE',  ( 10.03495058442699950, -3.601336184534900120, -6.578094656394299911 ) ) ;
#59102 = CARTESIAN_POINT ( 'NONE',  ( 8.174990947233128580, -2.650692654197974729, 7.500004443805800669 ) ) ;
#59103 = CARTESIAN_POINT ( 'NONE',  ( 9.882266086202999844, -4.932716797830999589, 6.390980246320999925 ) ) ;
#59104 = CARTESIAN_POINT ( 'NONE',  ( 10.92026088462129962, 4.002135146349410810, -6.496532863517000322 ) ) ;
#59105 = CARTESIAN_POINT ( 'NONE',  ( 12.47371306568759408, 0.6398865404514789690, 12.58374251866278826 ) ) ;
#59106 = DIRECTION ( 'NONE',  ( 1.000000000000000000, 0.000000000000000000, 0.000000000000000000 ) ) ;
#59107 = CARTESIAN_POINT ( 'NONE',  ( 5.082577295415885210, 1.197764792580507054, 0.04139071277677507793 ) ) ;
#59108 = CARTESIAN_POINT ( 'NONE',  ( 12.26287255281685695, 2.811570894161414813, 12.37351047967075424 ) ) ;
#59109 = CARTESIAN_POINT ( 'NONE',  ( 18.32727125556385417, -3.363648366948407631, -12.06493410109945152 ) ) ;
#59110 = CARTESIAN_POINT ( 'NONE',  ( 10.59610807141099897, 4.052703327804870526, -8.639522915742999132 ) ) ;
#59111 = CARTESIAN_POINT ( 'NONE',  ( 8.076862866721999268, 2.879478799711000292, -6.727223656603999125 ) ) ;
#59112 = EDGE_CURVE ( 'NONE', #6243, #27153, #37775, .T. ) ;
#59113 = CARTESIAN_POINT ( 'NONE',  ( 11.06878584122999953, 5.318802051720999735, -7.168446171767000052 ) ) ;
#59114 = CARTESIAN_POINT ( 'NONE',  ( 8.617468108405999416, 5.230803879475000251, -7.848577323721800170 ) ) ;
#59116 = CARTESIAN_POINT ( 'NONE',  ( 12.80505043854146940, -1.875000000000000444, -13.78627172894481667 ) ) ;
#59115 = CARTESIAN_POINT ( 'NONE',  ( 8.196365526475007712, 5.108366921470007149, 6.411205986879997099 ) ) ;
#59117 = CIRCLE ( 'NONE', #7776, 1.600000000000000089 ) ;
#59118 = DIRECTION ( 'NONE',  ( 0.000000000000000000, -1.000000000000000000, 0.000000000000000000 ) ) ;
#59119 = ORIENTED_EDGE ( 'NONE', *, *, #24388, .T. ) ;
#59120 = ADVANCED_FACE ( 'NONE', ( #67567 ), #24244, .F. ) ;
#59121 = CARTESIAN_POINT ( 'NONE',  ( 12.31508698957360615, 0.3880315155551694595, 12.69202109204528739 ) ) ;
#59122 = CARTESIAN_POINT ( 'NONE',  ( 9.674373738639999942, -2.899999999999999911, -6.185493860157000867 ) ) ;
#59123 = CARTESIAN_POINT ( 'NONE',  ( 11.89965592520902682, -11.89526654130121841, 3.923396420608940893 ) ) ;
#59124 = CARTESIAN_POINT ( 'NONE',  ( 24.45625629573268256, -3.500080033065961160, -12.27866820334083187 ) ) ;
#59125 = CARTESIAN_POINT ( 'NONE',  ( 12.61514273204572589, -1.812907417374193031, 13.88212581052982486 ) ) ;
#59126 = CARTESIAN_POINT ( 'NONE',  ( 11.05213295841000054, 2.768281150710999672, 4.976717609956999411 ) ) ;
#59127 = CARTESIAN_POINT ( 'NONE',  ( 7.364999999998000035, 2.649999999999999911, -7.500000000000000000 ) ) ;
#59128 = B_SPLINE_CURVE_WITH_KNOTS ( 'NONE', 3,
 ( #31219, #5996, #59485, #6340, #48660, #58802, #10562, #21059, #26307, #4974 ),
 .UNSPECIFIED., .F., .F.,
 ( 4, 2, 2, 2, 4 ),
 ( 0.000000000000000000, 0.2500000000000000000, 0.5000000000000000000, 0.7500000000000000000, 1.000000000000000000 ),
 .UNSPECIFIED. ) ;
#59129 = VERTEX_POINT ( 'NONE', #35096 ) ;
#59130 = LINE ( 'NONE', #1790, #17022 ) ;
#59131 = CARTESIAN_POINT ( 'NONE',  ( 18.29058466016384443, -10.98038933998877553, 3.892884224343166721 ) ) ;
#59132 = CARTESIAN_POINT ( 'NONE',  ( 9.575345697731034278, -5.349773134808791575, -7.676679544872200722 ) ) ;
#59133 = CARTESIAN_POINT ( 'NONE',  ( 10.79399293566600093, -3.453258297007899991, 6.829299525004299376 ) ) ;
#59134 = EDGE_CURVE ( 'NONE', #68518, #34052, #50291, .T. ) ;
#59135 = CARTESIAN_POINT ( 'NONE',  ( 18.17458387927298702, 2.583096938294931810, -12.43185036011799482 ) ) ;
#59136 = CARTESIAN_POINT ( 'NONE',  ( 8.474485200571999499, 5.100000000000000533, 6.560614371780999043 ) ) ;
#59137 = CARTESIAN_POINT ( 'NONE',  ( 11.49056651104150006, 4.085456792591960706, 8.361971998931499783 ) ) ;
#59138 = DIRECTION ( 'NONE',  ( 0.000000000000000000, 0.000000000000000000, -1.000000000000000000 ) ) ;
#59139 = CARTESIAN_POINT ( 'NONE',  ( 10.94033064679000233, -5.142732045902000948, -6.493502833853999512 ) ) ;
#59140 = CARTESIAN_POINT ( 'NONE',  ( 11.22823073745748168, 3.830325957789608715, -8.360328963510957223 ) ) ;
#59141 = DIRECTION ( 'NONE',  ( -0.7071067811865974218, 0.7071067811864975017, 9.304588036591961259E-09 ) ) ;
#59142 = PLANE ( 'NONE',  #68970 ) ;
#59143 = LINE ( 'NONE', #10908, #39868 ) ;
#59144 = ORIENTED_EDGE ( 'NONE', *, *, #54536, .F. ) ;
#59145 = CARTESIAN_POINT ( 'NONE',  ( 7.382526753210433945, 2.847550462391403858, 8.801350187526136182 ) ) ;
#59146 = CARTESIAN_POINT ( 'NONE',  ( 11.79364426047339975, -3.533902447304699823, 6.769896129503799820 ) ) ;
#59147 = ORIENTED_EDGE ( 'NONE', *, *, #33312, .F. ) ;
#59148 = CARTESIAN_POINT ( 'NONE',  ( 18.05225003025152120, -2.879247418710622508, 13.58568546892325912 ) ) ;
#59150 = CARTESIAN_POINT ( 'NONE',  ( 11.08841369783139896, -4.057552111898620417, -8.639288317626999003 ) ) ;
#59149 = B_SPLINE_CURVE_WITH_KNOTS ( 'NONE', 3,
 ( #57485, #19755, #9592, #67289 ),
 .UNSPECIFIED., .F., .F.,
 ( 4, 4 ),
 ( 0.8745776555051315571, 1.000000000000000000 ),
 .UNSPECIFIED. ) ;
#59152 = ORIENTED_EDGE ( 'NONE', *, *, #2442, .F. ) ;
#59151 = B_SPLINE_CURVE_WITH_KNOTS ( 'NONE', 3,
 ( #53027, #15622, #14593, #25421 ),
 .UNSPECIFIED., .F., .F.,
 ( 4, 4 ),
 ( 0.000000000000000000, 1.000000000000000000 ),
 .UNSPECIFIED. ) ;
#59153 = CARTESIAN_POINT ( 'NONE',  ( 10.69057802013490033, 2.966773425016000054, 7.524052967375959966 ) ) ;
#59154 = CARTESIAN_POINT ( 'NONE',  ( 5.696014035686344457, 0.1224074471714921564, 1.126874554618065849 ) ) ;
#59155 = DIRECTION ( 'NONE',  ( 0.000000000000000000, -0.1218274111675001353, 0.9925512993736016476 ) ) ;
#59156 = CARTESIAN_POINT ( 'NONE',  ( 8.725348536223782148, -2.649439212887072959, 7.500023728975150128 ) ) ;
#59157 = FACE_BOUND ( 'NONE', #62972, .T. ) ;
#59158 = CARTESIAN_POINT ( 'NONE',  ( 12.20957190034697248, 0.1900921649601574615, -13.89825464817679901 ) ) ;
#59159 = CARTESIAN_POINT ( 'NONE',  ( 11.59999999999999964, -4.569820763625128457, -6.730205196242793342 ) ) ;
#59160 = CARTESIAN_POINT ( 'NONE',  ( 9.898134631442999876, -2.965923230546999800, -6.610863544715000373 ) ) ;
#59161 = CARTESIAN_POINT ( 'NONE',  ( 13.22410434383600197, 11.56587205782000005, 1.788415454164999918 ) ) ;
#59162 = ORIENTED_EDGE ( 'NONE', *, *, #31344, .F. ) ;
#59163 = LINE ( 'NONE', #13362, #55684 ) ;
#59164 = EDGE_LOOP ( 'NONE', ( #5058, #8244, #19206, #57427, #35187 ) ) ;
#59166 = VECTOR ( 'NONE', #38605, 1000.000000000000227 ) ;
#59165 = B_SPLINE_CURVE_WITH_KNOTS ( 'NONE', 3,
 ( #68118, #37012, #67773, #68455, #20578, #62534, #31086, #10427, #36668, #4486, #41903, #47502 ),
 .UNSPECIFIED., .F., .F.,
 ( 4, 2, 2, 2, 2, 4 ),
 ( 0.000000000000000000, 0.2500000000000179301, 0.3750000000000234812, 0.4375000000000240363, 0.5000000000000245359, 1.000000000000000000 ),
 .UNSPECIFIED. ) ;
#59167 = CARTESIAN_POINT ( 'NONE',  ( 10.20918109782000016, 3.334760637131999772, -5.769467581755999497 ) ) ;
#59168 =( NAMED_UNIT ( * ) SI_UNIT ( $, .STERADIAN. ) SOLID_ANGLE_UNIT ( ) );
#59169 = ORIENTED_EDGE ( 'NONE', *, *, #35794, .T. ) ;
#59170 = DIRECTION ( 'NONE',  ( 0.000000000000000000, 0.9999808993455937545, 0.006180691221632959691 ) ) ;
#59171 = CARTESIAN_POINT ( 'NONE',  ( 17.80592519432568821, -3.072462716380374381, -12.29957259991316931 ) ) ;
#59172 = CARTESIAN_POINT ( 'NONE',  ( 10.90000000000000036, -8.618205959414002137, 7.308661029293999967 ) ) ;
#59173 = FACE_OUTER_BOUND ( 'NONE', #8941, .T. ) ;
#59174 = EDGE_CURVE ( 'NONE', #30733, #31977, #24930, .T. ) ;
#59175 = EDGE_CURVE ( 'NONE', #34148, #7076, #31968, .T. ) ;
#59176 = CARTESIAN_POINT ( 'NONE',  ( 10.79499900793999956, -3.503951165873000040, 6.168577387731000172 ) ) ;
#59177 = DIRECTION ( 'NONE',  ( -1.000000000000000000, 0.000000000000000000, 0.000000000000000000 ) ) ;
#59178 = ADVANCED_FACE ( 'NONE', ( #46264 ), #5880, .F. ) ;
#59179 = CARTESIAN_POINT ( 'NONE',  ( 12.19004662364084091, 0.1118032413084496662, 13.89939982891986148 ) ) ;
#59180 = ORIENTED_EDGE ( 'NONE', *, *, #58784, .T. ) ;
#59181 = CARTESIAN_POINT ( 'NONE',  ( 6.956590560819000402, 5.278582711742999756, -7.933273873238999130 ) ) ;
#59182 = CARTESIAN_POINT ( 'NONE',  ( 18.18731764114100358, 11.62758720635999765, -4.758865308234000224 ) ) ;
#59183 = CARTESIAN_POINT ( 'NONE',  ( 9.632166486775625813, 3.137137839323436594, 7.355082228165340297 ) ) ;
#59184 = CARTESIAN_POINT ( 'NONE',  ( 4.418014461077000021, 0.5835563493861999351, -1.200305805718000274 ) ) ;
#59185 = CARTESIAN_POINT ( 'NONE',  ( 9.793039158772000263, 5.817107086401000160, -6.945352709928000579 ) ) ;
#59186 = CARTESIAN_POINT ( 'NONE',  ( 18.53935907712300235, -2.923447147946000246, 12.21821814482000157 ) ) ;
#59187 = CARTESIAN_POINT ( 'NONE',  ( 10.58996262057999971, -2.876743158681999812, -6.236533224899999617 ) ) ;
#59188 = EDGE_LOOP ( 'NONE', ( #34658, #4749, #55811, #2414 ) ) ;
#59189 = CARTESIAN_POINT ( 'NONE',  ( 8.771960841230001193, 3.061731693614000438, -8.535706278603999664 ) ) ;
#59190 = CARTESIAN_POINT ( 'NONE',  ( 5.700000001242999659, -1.249999998757000075, 1.883720477311000285E-09 ) ) ;
#59191 = CARTESIAN_POINT ( 'NONE',  ( 17.92262925323456102, -1.881361389426406960, 13.87306285016402363 ) ) ;
#59192 = CARTESIAN_POINT ( 'NONE',  ( 1.700000000000000178, 0.000000000000000000, 0.000000000000000000 ) ) ;
#59193 = CARTESIAN_POINT ( 'NONE',  ( 24.77993120524800119, 8.657413043978001710, -9.170265824677001021 ) ) ;
#59194 = CARTESIAN_POINT ( 'NONE',  ( 10.73213259636989925, 3.092475607087700418, -7.994504989494399361 ) ) ;
#59195 = CARTESIAN_POINT ( 'NONE',  ( 9.330709346416998784, 4.907312911337299965, -7.069157126958599768 ) ) ;
#59197 = CARTESIAN_POINT ( 'NONE',  ( 2.050973465875999935, 3.500000000000000000, 0.000000000000000000 ) ) ;
#59196 = CARTESIAN_POINT ( 'NONE',  ( 10.58359632033899977, -4.802737635155300389, 7.827597670336898794 ) ) ;
#59198 = DIRECTION ( 'NONE',  ( -0.8987684456439056779, 0.000000000000000000, 0.4384236320214023319 ) ) ;
#59199 = EDGE_LOOP ( 'NONE', ( #36552, #10487, #49699, #27715, #44495, #56329 ) ) ;
#59200 = VECTOR ( 'NONE', #41056, 1000.000000000000000 ) ;
#59201 = CARTESIAN_POINT ( 'NONE',  ( 24.30001697071400457, -8.938702858184001343, 8.938676113071998941 ) ) ;
#59202 = CARTESIAN_POINT ( 'NONE',  ( 10.52638330645999964, -2.451090818816000105, 6.282756943804999494 ) ) ;
#59203 = CARTESIAN_POINT ( 'NONE',  ( 10.48444474310099928, 5.015709705366000470, 7.007085334055199510 ) ) ;
#59204 = CARTESIAN_POINT ( 'NONE',  ( 11.09999999999999964, 6.080160889643000388, -5.239944403408999918 ) ) ;
#59205 = CARTESIAN_POINT ( 'NONE',  ( 10.40226385995999969, -2.765692573780999641, 9.035345396600000356 ) ) ;
#59206 = CARTESIAN_POINT ( 'NONE',  ( 23.59999193302000364, -13.22318594659000013, 4.267778254689999606 ) ) ;
#59207 = DIRECTION ( 'NONE',  ( -1.000000000000000000, 0.000000000000000000, 0.000000000000000000 ) ) ;
#59208 = AXIS2_PLACEMENT_3D ( 'NONE', #53749, #9942, #63759 ) ;
#59209 = CARTESIAN_POINT ( 'NONE',  ( 9.052088727410998459, -5.000897406023000258, -7.583944523024719331 ) ) ;
#59210 = CARTESIAN_POINT ( 'NONE',  ( 5.140365123072000664, -0.1287196877685000129, 1.257471894813999791 ) ) ;
#59211 = EDGE_CURVE ( 'NONE', #54978, #56420, #1633, .T. ) ;
#59212 = DIRECTION ( 'NONE',  ( -1.000000000000000000, 0.000000000000000000, 0.000000000000000000 ) ) ;
#59213 = DIRECTION ( 'NONE',  ( -0.000000000000000000, 1.000000000000000000, 0.000000000000000000 ) ) ;
#59214 = ORIENTED_EDGE ( 'NONE', *, *, #534, .F. ) ;
#59215 = CARTESIAN_POINT ( 'NONE',  ( 12.23671932425159881, -4.127012898954600217, 6.643164954553199664 ) ) ;
#59216 = CARTESIAN_POINT ( 'NONE',  ( 10.72749279009019929, 3.774717370312400178, -8.336388861178200216 ) ) ;
#59217 = EDGE_CURVE ( 'NONE', #1282, #49213, #4382, .T. ) ;
#59218 = CARTESIAN_POINT ( 'NONE',  ( 1.500973465873999935, 3.500000000000000000, 0.000000000000000000 ) ) ;
#59219 = CARTESIAN_POINT ( 'NONE',  ( 25.36444524348200247, -8.489942824528000642, 7.945382091837999816 ) ) ;
#59220 = CARTESIAN_POINT ( 'NONE',  ( 12.43656315537375612, 1.853531805833888324, 12.46297683056294048 ) ) ;
#59221 = ORIENTED_EDGE ( 'NONE', *, *, #68640, .T. ) ;
#59222 = CARTESIAN_POINT ( 'NONE',  ( 25.08243281028700267, -11.33758179239000086, -3.319403910104000044 ) ) ;
#59223 = CARTESIAN_POINT ( 'NONE',  ( 11.36056039236529891, -3.108928759355700233, -7.543366519014379712 ) ) ;
#59224 = CARTESIAN_POINT ( 'NONE',  ( 23.60000000000000142, -2.204728229456999866, -11.99913219504999873 ) ) ;
#59225 = LINE ( 'NONE', #6424, #16482 ) ;
#59226 = CARTESIAN_POINT ( 'NONE',  ( 11.79999999471800010, -11.69117318561000118, -1.923227876431999883 ) ) ;
#59227 = FACE_OUTER_BOUND ( 'NONE', #17896, .T. ) ;
#59228 = ORIENTED_EDGE ( 'NONE', *, *, #64851, .T. ) ;
#59229 = CARTESIAN_POINT ( 'NONE',  ( 10.57893103570000015, -4.649956431060000561, 5.681096060554999383 ) ) ;
#59230 = FACE_OUTER_BOUND ( 'NONE', #7160, .T. ) ;
#59231 = ORIENTED_EDGE ( 'NONE', *, *, #37520, .F. ) ;
#59232 = CARTESIAN_POINT ( 'NONE',  ( 9.947288403111267385, -2.899999999999999911, 6.305985889562331970 ) ) ;
#59233 = CARTESIAN_POINT ( 'NONE',  ( 9.216851002545999094, -2.832432432432000269, 6.822293592207000934 ) ) ;
#59234 = CARTESIAN_POINT ( 'NONE',  ( 8.225464158772000545, 3.844886277615000125, -8.888911790991000927 ) ) ;
#59235 = ORIENTED_EDGE ( 'NONE', *, *, #51445, .T. ) ;
#59236 = CARTESIAN_POINT ( 'NONE',  ( 6.355026506350000659, 1.500000000000000000, 0.000000000000000000 ) ) ;
#59237 = CARTESIAN_POINT ( 'NONE',  ( 7.025820280407000240, 2.268824274702999855, -7.434159913875999948 ) ) ;
#59238 = CARTESIAN_POINT ( 'NONE',  ( 10.09393020684899867, -2.750000000000000000, -7.500000000000000000 ) ) ;
#59239 = CARTESIAN_POINT ( 'NONE',  ( 9.502125899204576953, 4.762576840438827119, 8.617734806663701619 ) ) ;
#59240 = VERTEX_POINT ( 'NONE', #27519 ) ;
#59241 = CARTESIAN_POINT ( 'NONE',  ( 10.53138988903999973, -5.607755226963999640, 7.280101849877000042 ) ) ;
#59242 = CARTESIAN_POINT ( 'NONE',  ( 25.29883596902100251, 11.38086143259999972, -3.116303541651999964 ) ) ;
#59243 = SURFACE_STYLE_USAGE ( .BOTH. , #15907 ) ;
#59244 = ORIENTED_EDGE ( 'NONE', *, *, #7177, .F. ) ;
#59245 = CARTESIAN_POINT ( 'NONE',  ( 10.52314899745999988, -5.167567567567999731, -6.822293592207000934 ) ) ;
#59246 = CARTESIAN_POINT ( 'NONE',  ( 10.17270027370999941, -4.650151116117000605, -8.655526539784000661 ) ) ;
#59247 = ORIENTED_EDGE ( 'NONE', *, *, #35140, .F. ) ;
#59248 = CARTESIAN_POINT ( 'NONE',  ( 9.533342523874999586, 3.007153757386999526, 7.651982363644999730 ) ) ;
#59249 = FACE_OUTER_BOUND ( 'NONE', #65438, .T. ) ;
#59250 = CARTESIAN_POINT ( 'NONE',  ( 4.476974183299000210, -1.413654420883999840, 0.08947517539409000076 ) ) ;
#59251 = CARTESIAN_POINT ( 'NONE',  ( 11.60000000000000142, 3.599560744838743886, -6.596661741119738132 ) ) ;
#59252 = CARTESIAN_POINT ( 'NONE',  ( 24.56710111988151013, 11.92027008148530776, -3.200169502113732189 ) ) ;
#59253 = CARTESIAN_POINT ( 'NONE',  ( 11.33830977893730108, 3.023401864784708515, 8.326430086672806041 ) ) ;
#59254 = CARTESIAN_POINT ( 'NONE',  ( 3.230140132544583764, -3.408904368339107815, 0.9161175952574674985 ) ) ;
#59255 = EDGE_CURVE ( 'NONE', #40685, #7462, #29514, .T. ) ;
#59256 = CIRCLE ( 'NONE', #18004, 1.349999999999999201 ) ;
#59257 = EDGE_CURVE ( 'NONE', #9710, #37068, #66921, .T. ) ;
#59258 = EDGE_CURVE ( 'NONE', #8285, #24513, #24343, .T. ) ;
#59259 = CARTESIAN_POINT ( 'NONE',  ( 9.326027934855707358, -3.975910976255049967, 9.239577797941210591 ) ) ;
#59260 = ORIENTED_EDGE ( 'NONE', *, *, #24786, .F. ) ;
#59261 = CARTESIAN_POINT ( 'NONE',  ( 9.966324641169999055, 2.303991951421000106, 6.575630951545000435 ) ) ;
#59262 = CARTESIAN_POINT ( 'NONE',  ( 10.03976415876999972, 2.255572964181999929, -8.111983882175000105 ) ) ;
#59263 = CARTESIAN_POINT ( 'NONE',  ( 10.90000000000000036, -1.199999999999999956, 9.776630298829998011 ) ) ;
#59264 = CARTESIAN_POINT ( 'NONE',  ( 12.78089888617682846, 1.787816964400945619, -13.88537754411822434 ) ) ;
#59265 = CARTESIAN_POINT ( 'NONE',  ( 24.66807826193371511, -12.30863159266774609, -2.982840176837593837 ) ) ;
#59266 = FACE_OUTER_BOUND ( 'NONE', #36113, .T. ) ;
#59267 = CARTESIAN_POINT ( 'NONE',  ( 17.88582179699705677, -0.5306878043354128494, 13.88636785578044730 ) ) ;
#59268 = CARTESIAN_POINT ( 'NONE',  ( 25.47132987582600450, -2.701711062754999837, 11.27933522402000044 ) ) ;
#59269 = ORIENTED_EDGE ( 'NONE', *, *, #8449, .T. ) ;
#59270 = EDGE_LOOP ( 'NONE', ( #37948, #39103, #29746, #50740, #42967 ) ) ;
#59271 = CARTESIAN_POINT ( 'NONE',  ( 12.78475456301477386, 0.6249999999999994449, 13.88107975066923494 ) ) ;
#59272 = CARTESIAN_POINT ( 'NONE',  ( 10.82118582084300051, -4.836160649475099937, 8.466515260542900378 ) ) ;
#59273 = CARTESIAN_POINT ( 'NONE',  ( 7.246486640886755204, -2.683814467610606158, 7.146108783255461283 ) ) ;
#59274 = CARTESIAN_POINT ( 'NONE',  ( 17.97806348698183854, -0.4608880372975631690, -13.88973238275042021 ) ) ;
#59275 = ADVANCED_FACE ( 'NONE', ( #66292 ), #29260, .F. ) ;
#59276 = CARTESIAN_POINT ( 'NONE',  ( 8.887168146795000112, -2.193670085072000120, 7.400591740205000768 ) ) ;
#59277 = DIRECTION ( 'NONE',  ( -1.000000000000000000, 0.000000000000000000, 0.000000000000000000 ) ) ;
#59279 = CYLINDRICAL_SURFACE ( 'NONE', #64121, 1.350000000000000533 ) ;
#59278 = CARTESIAN_POINT ( 'NONE',  ( 9.956405316140999773, -4.271593136661399726, 6.249951378708000327 ) ) ;
#59280 = CARTESIAN_POINT ( 'NONE',  ( 11.52733460557258915, 4.206337284815599986, -8.761245990815998752 ) ) ;
#59281 = CARTESIAN_POINT ( 'NONE',  ( 24.41456973790700147, -8.821771448540999927, -8.767658430047001517 ) ) ;
#59282 = DIRECTION ( 'NONE',  ( 0.000000000000000000, -0.9906588508047033947, 0.1363636363636003546 ) ) ;
#59283 = CARTESIAN_POINT ( 'NONE',  ( 18.17005379958825273, 0.1118057330073154582, 12.69934308675516377 ) ) ;
#59284 = DIRECTION ( 'NONE',  ( -0.7071068496915847712, 0.000000000000000000, -0.7071067126815037129 ) ) ;
#59285 = CARTESIAN_POINT ( 'NONE',  ( 23.95123756517200064, 9.462321155404998407, 9.411281308674000812 ) ) ;
#59286 = ORIENTED_EDGE ( 'NONE', *, *, #47235, .T. ) ;
#59287 = CARTESIAN_POINT ( 'NONE',  ( 8.919605646795000453, -5.165500668528999917, 8.645534272955000432 ) ) ;
#59288 = CARTESIAN_POINT ( 'NONE',  ( 8.474089158773999486, 4.131080973160000447, -6.108642999115999395 ) ) ;
#59289 = CONICAL_SURFACE ( 'NONE', #41432, 12.42511170355999894, 0.7854024644601717009 ) ;
#59290 = DIRECTION ( 'NONE',  ( 0.000000000000000000, 0.000000000000000000, -1.000000000000000000 ) ) ;
#59291 = DIRECTION ( 'NONE',  ( -0.7071064907087092344, 0.08614501498594114015, -0.7018400438780093564 ) ) ;
#59292 = B_SPLINE_CURVE_WITH_KNOTS ( 'NONE', 3,
 ( #23493, #3538, #24875, #39577 ),
 .UNSPECIFIED., .F., .F.,
 ( 4, 4 ),
 ( 0.000000000000000000, 1.000000000000000000 ),
 .UNSPECIFIED. ) ;
#59293 = CARTESIAN_POINT ( 'NONE',  ( 0.8312974075931000018, 0.9881876859693999871, -3.396851722846999877 ) ) ;
#59294 = EDGE_CURVE ( 'NONE', #25042, #60421, #32756, .T. ) ;
#59295 = CARTESIAN_POINT ( 'NONE',  ( 11.31900581613029821, 4.750686773407899466, 7.017964743997199939 ) ) ;
#59296 = FACE_OUTER_BOUND ( 'NONE', #42393, .T. ) ;
#59297 = VERTEX_POINT ( 'NONE', #54775 ) ;
#59298 = CARTESIAN_POINT ( 'NONE',  ( 12.39267273778989242, -0.5917181940048676925, -12.58609996267492903 ) ) ;
#59300 = AXIS2_PLACEMENT_3D ( 'NONE', #1137, #22449, #43791 ) ;
#59299 = CARTESIAN_POINT ( 'NONE',  ( 5.000000000000000000, 0.000000000000000000, 0.000000000000000000 ) ) ;
#59301 = CARTESIAN_POINT ( 'NONE',  ( 17.77874050697764829, 3.164693776342188070, -12.19609433843463009 ) ) ;
#59302 = EDGE_CURVE ( 'NONE', #34904, #65107, #6876, .T. ) ;
#59303 = CARTESIAN_POINT ( 'NONE',  ( 15.40000000009400161, -8.833277835210999740, -7.896561221812000930 ) ) ;
#59304 = CARTESIAN_POINT ( 'NONE',  ( 8.475642219593000348, 5.095085596809999728, 6.286981168432999922 ) ) ;
#59305 = ORIENTED_EDGE ( 'NONE', *, *, #41274, .T. ) ;
#59306 = CARTESIAN_POINT ( 'NONE',  ( 6.659332659907000185, 0.8975578082598999474, -1.162289642979999815 ) ) ;
#59307 = B_SPLINE_CURVE_WITH_KNOTS ( 'NONE', 3,
 ( #19096, #8949, #30290, #9977, #3014, #30623, #61741, #13861, #35191, #56502, #8609, #3690, #29956, #51260, #47738, #27099, #32349, #37239, #69053, #53999, #32008, #36902, #68698, #52625, #38266, #27440, #5074, #5757, #21494, #15906 ),
 .UNSPECIFIED., .F., .F.,
 ( 4, 2, 1, 1, 2, 2, 2, 2, 2, 2, 2, 2, 2, 2, 2, 4 ),
 ( 0.000000000000000000, 0.1250000000000020817, 0.1875000000000028033, 0.2187500000000024702, 0.2343750000000020262, 0.2500000000000015543, 0.3750000000000015543, 0.4375000000000014433, 0.5000000000000013323, 0.5625000000000011102, 0.6250000000000009992, 0.6875000000000007772, 0.7500000000000005551, 0.8125000000000004441, 0.8750000000000002220, 1.000000000000000000 ),
 .UNSPECIFIED. ) ;
#59308 = B_SPLINE_CURVE_WITH_KNOTS ( 'NONE', 3,
 ( #57139, #20770, #30578, #46664, #63407, #57475, #21116 ),
 .UNSPECIFIED., .F., .F.,
 ( 4, 1, 1, 1, 4 ),
 ( 0.000000000000000000, 0.2500000143192999680, 0.5000000056314000130, 0.7499999969435999780, 1.000000000000000000 ),
 .UNSPECIFIED. ) ;
#59309 = CARTESIAN_POINT ( 'NONE',  ( 7.449720280409000139, 5.287968704092000927, -6.611025344044000107 ) ) ;
#59310 = CARTESIAN_POINT ( 'NONE',  ( 8.540376343031317319, -3.285755531537955410, 5.914236678129165092 ) ) ;
#59311 = CARTESIAN_POINT ( 'NONE',  ( 9.066809814040999171, -3.217492037304399588, 6.488038963273999649 ) ) ;
#59312 = ORIENTED_EDGE ( 'NONE', *, *, #7827, .T. ) ;
#59313 = CARTESIAN_POINT ( 'NONE',  ( 7.100000000000000533, 0.000000000000000000, 0.000000000000000000 ) ) ;
#59314 = B_SPLINE_CURVE_WITH_KNOTS ( 'NONE', 3,
 ( #42786, #44181, #34725, #13056, #56036, #49756, #18295, #59896, #7104, #39270, #1516, #23185, #7799, #66516, #60940, #24216, #12003, #17952 ),
 .UNSPECIFIED., .F., .F.,
 ( 4, 2, 2, 2, 2, 2, 2, 2, 4 ),
 ( 0.000000000000000000, 0.1250000000000000000, 0.2500000000000000000, 0.3750000000000000000, 0.5000000000000000000, 0.6250000000000000000, 0.7500000000000000000, 0.8750000000000000000, 1.000000000000000000 ),
 .UNSPECIFIED. ) ;
#59315 = CARTESIAN_POINT ( 'NONE',  ( 11.74267124137200113, 11.57041781403000158, 1.757356211607000063 ) ) ;
#59316 = EDGE_LOOP ( 'NONE', ( #18832, #51759, #27042, #21839 ) ) ;
#59317 = CARTESIAN_POINT ( 'NONE',  ( 12.43699713721653310, 3.107380776471872608, -12.21088077982606102 ) ) ;
#59318 = CYLINDRICAL_SURFACE ( 'NONE', #27940, 0.5000000000000000000 ) ;
#59319 = CLOSED_SHELL ( 'NONE', ( #8829, #41041, #68523, #34504, #3549, #59443, #42963, #24537, #10105, #34803, #36180, #32657, #41355, #39447, #1800, #41925, #48380, #24309, #39449, #35746, #27899, #10974, #7199, #55345, #3382, #25645, #27878, #61568, #50069, #34017, #30395, #44728, #61780, #25533, #58699, #56831, #59842, #68693, #18566, #15699, #47149, #64364, #17228, #13497, #21460, #32227, #68724, #31825, #51904, #18033, #21648, #8526, #53821, #66774, #63561, #33846, #2908, #49670, #14831, #38740, #58973, #30285, #23660, #19009, #31741, #26714, #65563, #40148, #25739, #20746, #21084, #61059, #25196, #40478, #11385, #25090, #57517, #54096, #22556, #39139, #26673, #63306, #62036, #39060, #45174, #46318, #26154, #55450, #20531, #32362, #6146, #10670, #32878, #28257, #20046, #21454, #47665, #65447, #27618, #52444, #32748, #22339, #41625, #13129, #6771, #41992, #16304, #13742, #52388, #62651, #34802, #43196, #55108, #40528, #60327, #52647, #11676, #27057, #4578, #22276, #16947, #4959, #65782, #1403, #34936, #12081, #50435, #30153, #20063, #34881, #25922, #31987, #47434, #272, #33455, #48376, #59562, #51521, #34889, #21098, #24409, #42865, #12625, #17355, #57145, #46718, #66753, #28905, #55746, #21403, #26441, #65612, #52041, #3681, #55594, #23836, #33981, #12960, #39415, #34888, #32243, #45593, #32459, #7340, #49525, #27954, #25054, #30535, #3303, #4776, #36079, #54928, #51193, #68960, #68241, #37014, #11340, #8148, #55762, #10918, #55284, #16082, #35585, #63707, #43169, #57853, #35225, #16642, #5902, #62096, #1337, #33813, #12331, #40643, #32135, #62832, #5608, #63762, #57223, #25331, #5120, #7592, #38659, #10958, #51484, #12707, #44281, #41971, #43490, #41904, #62946, #19816, #4127, #15915, #28752, #27958, #41006, #18934, #41353, #63507, #58185, #55965, #45230, #61671, #41573, #66152, #53263, #10865, #28091, #23534, #54385, #56608, #11062, #52795, #52249, #45846, #34528, #43716, #9680, #46983, #56858, #59649, #12586, #21599, #67041, #51383, #37736, #33704, #28322, #5517, #53842, #65278, #47099, #28096, #56453, #13463, #22473, #401, #52165, #43485, #2958, #15610, #39183, #11285, #51526, #60393, #53741, #45004, #31013, #26239, #18621, #48043, #28414, #43317, #55237, #40893, #19095, #36811, #61261, #40207, #20912, #43410, #3939, #61361, #26695, #17760, #45673, #10177, #62289, #37094, #67164, #2933, #33018, #14279, #24139, #62134, #3813, #45337, #19657, #11344, #54573, #58267 ) ) ;
#59320 = CARTESIAN_POINT ( 'NONE',  ( 18.15598102061104768, -0.1720826668005526749, -13.89857125525884207 ) ) ;
#59321 = ORIENTED_EDGE ( 'NONE', *, *, #28582, .F. ) ;
#59322 = DIRECTION ( 'NONE',  ( -1.000000000000000000, 0.000000000000000000, 0.000000000000000000 ) ) ;
#59323 =( LENGTH_UNIT ( ) NAMED_UNIT ( * ) SI_UNIT ( .MILLI., .METRE. ) );
#59324 = CARTESIAN_POINT ( 'NONE',  ( 11.44366954483529852, 4.485203148598100320, -6.751356298874699569 ) ) ;
#59325 = CARTESIAN_POINT ( 'NONE',  ( 11.53192018828833731, 3.091029700564639437, -7.175001928748123703 ) ) ;
#59326 = CARTESIAN_POINT ( 'NONE',  ( 10.62426357027499968, -2.745128867668000350, 7.257895958275299542 ) ) ;
#59327 = EDGE_LOOP ( 'NONE', ( #27725, #670, #48236, #67082 ) ) ;
#59328 = CARTESIAN_POINT ( 'NONE',  ( 8.437857780412000963, 2.606995215518000286, 6.345762205468999717 ) ) ;
#59329 = VERTEX_POINT ( 'NONE', #28212 ) ;
#59330 = DIRECTION ( 'NONE',  ( 0.9999999999998953060, -4.575887298088981526E-07, 2.007391389072990910E-09 ) ) ;
#59331 = CARTESIAN_POINT ( 'NONE',  ( 15.86122879894100102, -8.802595411723000751, -8.571496522999998646 ) ) ;
#59332 = B_SPLINE_CURVE_WITH_KNOTS ( 'NONE', 3,
 ( #18926, #67148, #25193, #13687, #46527, #67835, #9446, #19956, #15047, #19261, #41280, #62927, #36373, #8092, #42650, #32173, #10148, #11172, #58379, #37403, #689, #37745, #21657, #57688, #4893, #58724, #5578, #31148, #26581, #9798, #10829, #31478, #63960, #36727, #52449, #31824, #26921, #4544, #10486, #52800, #16754, #42990, #64299, #53486, #26233, #59072, #340, #53141, #47563, #27263, #25884 ),
 .UNSPECIFIED., .F., .F.,
 ( 4, 2, 2, 2, 2, 2, 2, 2, 2, 2, 2, 2, 2, 1, 2, 2, 2, 2, 2, 2, 2, 2, 2, 2, 2, 4 ),
 ( 0.000000000000000000, 0.06261444088627614313, 0.1252288817725522863, 0.1565361022156903370, 0.1878433226588283878, 0.2191505431019664663, 0.2348041533235355194, 0.2504577635451045725, 0.2817649839882465646, 0.2974185942098189206, 0.3130722044313913321, 0.3287258146529636327, 0.3443794248745360442, 0.3600330350961084003, 0.3678598402068946061, 0.3756866453176807563, 0.3913402555392500592, 0.3991670606500349328, 0.4069938657608198618, 0.4226474759823886096, 0.4304742810931723174, 0.4343876836485654480, 0.4383010862039585231, 0.4539546964255286032, 0.4696083066470986278, 0.5009155270902381218 ),
 .UNSPECIFIED. ) ;
#59333 = CARTESIAN_POINT ( 'NONE',  ( 10.09393020684899867, 5.250000000000000000, 7.500000000000000000 ) ) ;
#59334 = ORIENTED_EDGE ( 'NONE', *, *, #8071, .T. ) ;
#59335 = CARTESIAN_POINT ( 'NONE',  ( 12.18490839767386014, -2.421563015655832984, -12.46949130182972354 ) ) ;
#59336 = CARTESIAN_POINT ( 'NONE',  ( 16.10004050617000004, -7.492404338401445152, -10.08789649943574851 ) ) ;
#59337 = CARTESIAN_POINT ( 'NONE',  ( 7.913901703519866437, 2.864539049585775654, -6.759697255404577554 ) ) ;
#59338 = CARTESIAN_POINT ( 'NONE',  ( 24.16219716209097967, -3.322358446342811966, -12.45205009512240224 ) ) ;
#59339 = CARTESIAN_POINT ( 'NONE',  ( 12.35155033006833136, -1.948172666216914983, -13.86379038907994854 ) ) ;
#59340 = CARTESIAN_POINT ( 'NONE',  ( 10.20641772631199906, -3.568446272909699957, -8.388315195900499788 ) ) ;
#59341 = CARTESIAN_POINT ( 'NONE',  ( 12.35552214746119049, -1.907986453762815060, 12.45488571128362665 ) ) ;
#59342 = EDGE_CURVE ( 'NONE', #10933, #8271, #23669, .T. ) ;
#59344 = EDGE_CURVE ( 'NONE', #12470, #67865, #1132, .T. ) ;
#59343 = CARTESIAN_POINT ( 'NONE',  ( 17.81282484970914126, -3.152868460668823758, 12.19915726504404851 ) ) ;
#59345 = EDGE_LOOP ( 'NONE', ( #21421, #58463, #59942, #53967 ) ) ;
#59346 = CARTESIAN_POINT ( 'NONE',  ( 11.22567835872029995, -4.993948309075300074, -6.873560442659099046 ) ) ;
#59347 = EDGE_LOOP ( 'NONE', ( #19217, #25367, #49799, #40530, #10953, #28261, #59010, #37925 ) ) ;
#59348 = CARTESIAN_POINT ( 'NONE',  ( 14.30001311048500057, -12.52500000000000036, 4.931155131476459494E-11 ) ) ;
#59349 = CARTESIAN_POINT ( 'NONE',  ( 8.753601108637971251, -2.714205948350681297, 7.027810827039939312 ) ) ;
#59350 = CARTESIAN_POINT ( 'NONE',  ( 9.934212804449000345, 5.120437537252000126, -8.883398686237999442 ) ) ;
#59351 = FACE_OUTER_BOUND ( 'NONE', #5595, .T. ) ;
#59352 = CARTESIAN_POINT ( 'NONE',  ( 24.30000000000000071, 12.03537377768999939, 3.224868684338999980 ) ) ;
#59353 = CARTESIAN_POINT ( 'NONE',  ( 24.23234572864199876, -12.46720875768999903, 3.269128814187999943 ) ) ;
#59354 = CARTESIAN_POINT ( 'NONE',  ( 10.06843885510000014, 4.148608506723999945, 8.941445591976998841 ) ) ;
#59355 = VECTOR ( 'NONE', #19242, 1000.000000000000000 ) ;
#59356 = ORIENTED_EDGE ( 'NONE', *, *, #20847, .F. ) ;
#59357 = CARTESIAN_POINT ( 'NONE',  ( 18.49055856039300139, 2.949841519493000330, 11.23086453091999992 ) ) ;
#59358 = CARTESIAN_POINT ( 'NONE',  ( 9.476372460169001144, 5.098395626600999542, 6.305536056092000408 ) ) ;
#59359 = CARTESIAN_POINT ( 'NONE',  ( 9.709999999999999076, -4.496968146123999865, -8.755198255949000696 ) ) ;
#59360 = EDGE_CURVE ( 'NONE', #41424, #54112, #41913, .T. ) ;
#59361 = CARTESIAN_POINT ( 'NONE',  ( 11.15413259636999932, -4.783377755405500587, 7.073141822156699732 ) ) ;
#59362 = DIRECTION ( 'NONE',  ( 1.000000000000000000, 0.000000000000000000, 0.000000000000000000 ) ) ;
#59363 = CARTESIAN_POINT ( 'NONE',  ( 11.66287348028854964, 3.238044298475899918, -7.911973420841600380 ) ) ;
#59364 = EDGE_CURVE ( 'NONE', #26163, #683, #1640, .T. ) ;
#59365 = CARTESIAN_POINT ( 'NONE',  ( 10.24369552910394532, 5.492882802562766287, 8.410537742903038350 ) ) ;
#59366 = VECTOR ( 'NONE', #13865, 1000.000000000000114 ) ;
#59367 = CARTESIAN_POINT ( 'NONE',  ( 23.51706659920400355, -10.50862010217999831, -9.449478156932999084 ) ) ;
#59368 = FACE_OUTER_BOUND ( 'NONE', #52105, .T. ) ;
#59369 = DIRECTION ( 'NONE',  ( 1.000000000000000000, 0.000000000000000000, -4.146618578177000290E-14 ) ) ;
#59370 = VERTEX_POINT ( 'NONE', #61404 ) ;
#59371 = DIRECTION ( 'NONE',  ( 0.000000000000000000, 0.000000000000000000, -1.000000000000000000 ) ) ;
#59372 = DIRECTION ( 'NONE',  ( -1.000000000000000000, 0.000000000000000000, 0.000000000000000000 ) ) ;
#59373 = CARTESIAN_POINT ( 'NONE',  ( 18.08802622730387100, 2.172927601657333341, 13.73737356033239188 ) ) ;
#59374 = CARTESIAN_POINT ( 'NONE',  ( 24.41555930013399944, 8.820896577363999569, -8.766783479041999172 ) ) ;
#59375 = CARTESIAN_POINT ( 'NONE',  ( 10.64118447801629941, -2.722297859592000435, -7.471828720557429193 ) ) ;
#59376 = EDGE_LOOP ( 'NONE', ( #20193, #33366, #62158, #4176 ) ) ;
#59377 = CARTESIAN_POINT ( 'NONE',  ( 5.604756202875922355, -12.12903653623212108, 3.749090042451754812 ) ) ;
#59378 = CARTESIAN_POINT ( 'NONE',  ( 8.694607780412001219, 5.290207928847999064, 8.768105151414001597 ) ) ;
#59380 = CARTESIAN_POINT ( 'NONE',  ( 11.59999999999999964, 5.179498027601999510, 7.825000000000000178 ) ) ;
#59379 = CARTESIAN_POINT ( 'NONE',  ( 8.754720280412998434, 5.687930027805999877, -7.109876198051000351 ) ) ;
#59381 = CARTESIAN_POINT ( 'NONE',  ( 3.190706351837349075, 1.551038532097675393, -2.865019036274451203 ) ) ;
#59382 = ORIENTED_EDGE ( 'NONE', *, *, #31882, .T. ) ;
#59383 = CARTESIAN_POINT ( 'NONE',  ( 9.813360311708999362, 5.349397258738000538, 6.657026394682000081 ) ) ;
#59384 = CARTESIAN_POINT ( 'NONE',  ( 17.98066499537654650, -1.926393605117494578, -13.86683778668631106 ) ) ;
#59385 = CARTESIAN_POINT ( 'NONE',  ( 10.69872335273220010, 4.349306362047499874, 6.559289673553299060 ) ) ;
#59386 = EDGE_CURVE ( 'NONE', #4266, #38087, #25271, .T. ) ;
#59387 = CARTESIAN_POINT ( 'NONE',  ( 11.07345355053000091, -3.998673159585000025, 8.920828114954002075 ) ) ;
#59388 = CARTESIAN_POINT ( 'NONE',  ( 8.146781841545999825, 3.121749852590999907, 6.130949854565998614 ) ) ;
#59389 = ORIENTED_EDGE ( 'NONE', *, *, #17525, .T. ) ;
#59390 = FACE_OUTER_BOUND ( 'NONE', #49718, .T. ) ;
#59392 = CARTESIAN_POINT ( 'NONE',  ( 10.69829435321000055, -2.534030585780999711, -6.667788699001999220 ) ) ;
#59391 = CARTESIAN_POINT ( 'NONE',  ( 12.83944380997200163, -12.16696032571000075, 3.135189167188999537 ) ) ;
#59393 = B_SPLINE_CURVE_WITH_KNOTS ( 'NONE', 3,
 ( #66110, #39552, #12636, #33966, #2829, #55289 ),
 .UNSPECIFIED., .F., .F.,
 ( 4, 2, 4 ),
 ( 0.000000000000000000, 0.5000000000000000000, 1.000000000000000000 ),
 .UNSPECIFIED. ) ;
#59394 = CARTESIAN_POINT ( 'NONE',  ( 7.806446110424286822, -4.398161847081256681, 9.193498077367777910 ) ) ;
#59395 = CARTESIAN_POINT ( 'NONE',  ( 9.194602547868999665, -5.157768569202000108, 8.637845986715998237 ) ) ;
#59396 = CYLINDRICAL_SURFACE ( 'NONE', #27661, 0.5000000000000002220 ) ;
#59397 = ORIENTED_EDGE ( 'NONE', *, *, #25174, .T. ) ;
#59399 = CARTESIAN_POINT ( 'NONE',  ( 24.89161184346078670, -11.59760657164508046, -3.206054533605021462 ) ) ;
#59398 = CIRCLE ( 'NONE', #56059, 11.35000000000000675 ) ;
#59400 = CARTESIAN_POINT ( 'NONE',  ( 11.71149010443640037, -2.862435565199000109, 7.414927836855409460 ) ) ;
#59401 = CARTESIAN_POINT ( 'NONE',  ( 8.228219317832992985, 3.441361860949001539, 6.127431671619995690 ) ) ;
#59402 = CARTESIAN_POINT ( 'NONE',  ( 10.15303300763299887, 4.787165141710600480, 6.674373427955200277 ) ) ;
#59403 = EDGE_LOOP ( 'NONE', ( #26831, #46772, #55173, #64280 ) ) ;
#59404 = CARTESIAN_POINT ( 'NONE',  ( 8.374639158773000247, 2.721111233225000259, -6.936528696292000085 ) ) ;
#59405 = CARTESIAN_POINT ( 'NONE',  ( 12.12616169587827741, 2.733465040722955486, -12.29993066094647958 ) ) ;
#59406 = CARTESIAN_POINT ( 'NONE',  ( 11.43479632507519916, -3.442212747724900268, 6.465962698293999722 ) ) ;
#59407 = CARTESIAN_POINT ( 'NONE',  ( 7.966901574931999797, 4.609574279519000228, -6.276317554486000816 ) ) ;
#59408 = AXIS2_PLACEMENT_3D ( 'NONE', #60923, #38913, #18623 ) ;
#59409 = CARTESIAN_POINT ( 'NONE',  ( 5.227606837614000135, -0.3108367803229999948, 1.065889863396000115 ) ) ;
#59410 = EDGE_LOOP ( 'NONE', ( #61799, #26860, #41201, #34766 ) ) ;
#59411 = CARTESIAN_POINT ( 'NONE',  ( 9.138566940380000503, -2.933824946949000090, 8.496487880080000110 ) ) ;
#59412 = B_SPLINE_CURVE_WITH_KNOTS ( 'NONE', 3,
 ( #10422, #37685, #32111, #26514 ),
 .UNSPECIFIED., .F., .F.,
 ( 4, 4 ),
 ( 0.000000000000000000, 1.000000000000000000 ),
 .UNSPECIFIED. ) ;
#59413 = CARTESIAN_POINT ( 'NONE',  ( 5.690443173017207812, 0.1963495408493637351, -1.499999999999999778 ) ) ;
#59414 = EDGE_LOOP ( 'NONE', ( #287, #54247, #41373, #50147, #66988 ) ) ;
#59415 = CARTESIAN_POINT ( 'NONE',  ( 9.541846873516668381, 4.999583552997725278, 6.731816600031356401 ) ) ;
#59416 = CARTESIAN_POINT ( 'NONE',  ( 11.21564426047340035, 4.539962866738299851, 6.654192128557399499 ) ) ;
#59417 = AXIS2_PLACEMENT_3D ( 'NONE', #63985, #38466, #32880 ) ;
#59418 = CARTESIAN_POINT ( 'NONE',  ( 24.96658174203286151, -8.756202942073826989, 7.455126426642118886 ) ) ;
#59419 = CARTESIAN_POINT ( 'NONE',  ( 10.09133754351999990, 2.216715295763999727, -8.007133643737999407 ) ) ;
#59420 = CARTESIAN_POINT ( 'NONE',  ( 25.59994555223599733, 2.024003533649000097, -11.01554633311000053 ) ) ;
#59421 = CARTESIAN_POINT ( 'NONE',  ( 9.211801307670125283, 4.111875952999886508, -6.244821713992729784 ) ) ;
#59422 = CARTESIAN_POINT ( 'NONE',  ( 0.000000000000000000, -2.899999999999999911, 7.500000000000000000 ) ) ;
#59423 = CARTESIAN_POINT ( 'NONE',  ( 17.75589797987078100, 0.5919389804100245733, -12.68142457171642690 ) ) ;
#59424 = CARTESIAN_POINT ( 'NONE',  ( 12.18798377887743278, 2.400256349710756076, -12.47427327511915962 ) ) ;
#59425 = CARTESIAN_POINT ( 'NONE',  ( 11.11302897915239818, -3.708003626182200030, -8.602736702002999891 ) ) ;
#59426 = EDGE_CURVE ( 'NONE', #20309, #9109, #53624, .T. ) ;
#59428 = EDGE_CURVE ( 'NONE', #38686, #59040, #15222, .T. ) ;
#59427 = CARTESIAN_POINT ( 'NONE',  ( 9.566490007895001924, 4.108964550738000376, 8.851615252874999840 ) ) ;
#59429 = ORIENTED_EDGE ( 'NONE', *, *, #12009, .F. ) ;
#59430 = FACE_OUTER_BOUND ( 'NONE', #39130, .T. ) ;
#59431 = CARTESIAN_POINT ( 'NONE',  ( 24.39664890229900251, 8.853228234369833416, 8.853228234369833416 ) ) ;
#59432 = CARTESIAN_POINT ( 'NONE',  ( 23.60000000000000142, 11.49391741900999975, 4.090215442373000165 ) ) ;
#59433 = CARTESIAN_POINT ( 'NONE',  ( 18.28006803703874183, 2.506146490485266387, 12.34827083869106978 ) ) ;
#59434 = CARTESIAN_POINT ( 'NONE',  ( 11.02038863743000086, 6.425337680708999244, 5.276379190389000051 ) ) ;
#59435 = CARTESIAN_POINT ( 'NONE',  ( 10.67905590578999941, 2.899999999999999911, 6.571291218949999902 ) ) ;
#59436 = CARTESIAN_POINT ( 'NONE',  ( 10.61342028323962872, -4.872854478606138073, 7.560475846972328995 ) ) ;
#59437 = CARTESIAN_POINT ( 'NONE',  ( 9.979346873516126593, -3.836375382625532904, -8.749999999999998224 ) ) ;
#59438 = ORIENTED_EDGE ( 'NONE', *, *, #46654, .T. ) ;
#59439 = CARTESIAN_POINT ( 'NONE',  ( 12.70853553880221298, -3.193755089013870840, 12.18851650745940418 ) ) ;
#59440 = B_SPLINE_CURVE_WITH_KNOTS ( 'NONE', 3,
 ( #14645, #9044, #67760, #9378, #30384, #52380, #51694, #46461, #41214, #35961, #19887, #52031, #62524, #62861, #4133, #31074 ),
 .UNSPECIFIED., .F., .F.,
 ( 4, 2, 2, 2, 2, 2, 2, 4 ),
 ( 0.000000000000000000, 0.06250000000000113798, 0.1250000000000022760, 0.2500000000000024980, 0.5000000000000011102, 0.7499999999999997780, 0.8749999999999998890, 1.000000000000000000 ),
 .UNSPECIFIED. ) ;
#59441 = CARTESIAN_POINT ( 'NONE',  ( 9.882975701332998852, -3.263119632394200220, -8.182531775206799196 ) ) ;
#59442 = CARTESIAN_POINT ( 'NONE',  ( 10.29378723213999969, 3.483632952461999999, 6.176337842045999338 ) ) ;
#59443 = ADVANCED_FACE ( 'NONE', ( #4375 ), #20463, .F. ) ;
#59444 = CARTESIAN_POINT ( 'NONE',  ( 9.634027193201999850, -3.042970193091000031, 8.588108172435999776 ) ) ;
#59445 = AXIS2_PLACEMENT_3D ( 'NONE', #12779, #33762, #49480 ) ;
#59446 = EDGE_CURVE ( 'NONE', #57225, #115, #50796, .T. ) ;
#59447 = CARTESIAN_POINT ( 'NONE',  ( 11.11302897915239818, 4.291996373817799970, -8.602736702002999891 ) ) ;
#59448 = CARTESIAN_POINT ( 'NONE',  ( 12.33572460179970953, -0.5483668826291607790, 12.58806376549905082 ) ) ;
#59449 = CARTESIAN_POINT ( 'NONE',  ( 9.587885841227999251, 3.762712042852999872, 8.787816121229999666 ) ) ;
#59450 = CARTESIAN_POINT ( 'NONE',  ( 9.905792474809000936, 2.698958900805999761, 8.979236532123000103 ) ) ;
#59451 = CARTESIAN_POINT ( 'NONE',  ( 12.75673482301074735, 1.762409409947518046, 12.47613375359912169 ) ) ;
#59452 = CARTESIAN_POINT ( 'NONE',  ( 13.70005190196300227, 9.005348107749998832, 7.391036106496999381 ) ) ;
#59453 = CARTESIAN_POINT ( 'NONE',  ( 11.28533594839949750, 4.750012929834699804, -6.640482273977399430 ) ) ;
#59454 = DIRECTION ( 'NONE',  ( 0.000000000000000000, 0.000000000000000000, -1.000000000000000000 ) ) ;
#59455 = CARTESIAN_POINT ( 'NONE',  ( 10.57657334123000048, 5.344886503256999433, -7.298885378918000377 ) ) ;
#59456 = FACE_OUTER_BOUND ( 'NONE', #46419, .T. ) ;
#59458 = CARTESIAN_POINT ( 'NONE',  ( 17.89454609201841251, -0.5248351044085231010, 12.68540052859852452 ) ) ;
#59457 = CARTESIAN_POINT ( 'NONE',  ( 7.712330476186004979, 4.866816057961001363, 6.392636141994996635 ) ) ;
#59459 = DIRECTION ( 'NONE',  ( 0.000000000000000000, 0.9624505444715647506, -0.2714570858282915333 ) ) ;
#59460 = EDGE_LOOP ( 'NONE', ( #39730, #64763, #927, #14044 ) ) ;
#59461 = AXIS2_PLACEMENT_3D ( 'NONE', #60381, #49538, #38713 ) ;
#59462 = CARTESIAN_POINT ( 'NONE',  ( 12.40638932693400420, 0.4813547430073586986, 12.68771948605883892 ) ) ;
#59463 = CARTESIAN_POINT ( 'NONE',  ( 23.65870916658217382, -10.04306394571245953, -9.454468549935667099 ) ) ;
#59464 = CARTESIAN_POINT ( 'NONE',  ( 3.452384183491000069, 1.140396268832999827, -3.309002319436000317 ) ) ;
#59465 = CARTESIAN_POINT ( 'NONE',  ( 9.349051052051999378, 4.850870049477099322, 7.333482423122699601 ) ) ;
#59466 = CARTESIAN_POINT ( 'NONE',  ( 12.70875935989989713, -1.793877008111231186, 13.88459618876652790 ) ) ;
#59467 = FACE_OUTER_BOUND ( 'NONE', #233, .T. ) ;
#59468 = CARTESIAN_POINT ( 'NONE',  ( 24.03012267896300003, 3.726860619367999838, -13.01722844268999957 ) ) ;
#59469 = VERTEX_POINT ( 'NONE', #62423 ) ;
#59470 = CARTESIAN_POINT ( 'NONE',  ( 16.39999999347100257, -3.345256695718999751, -11.86066175541999890 ) ) ;
#59471 = CARTESIAN_POINT ( 'NONE',  ( 17.66658675203450102, -10.78295181804075398, 4.410266442045759128 ) ) ;
#59472 = CARTESIAN_POINT ( 'NONE',  ( 18.15262501847808707, -3.263149105984915810, -11.18369374219367174 ) ) ;
#59473 = FACE_OUTER_BOUND ( 'NONE', #10941, .T. ) ;
#59474 = CARTESIAN_POINT ( 'NONE',  ( 11.11257802013489915, -4.891884252872400474, 7.520762592984879369 ) ) ;
#59475 = CARTESIAN_POINT ( 'NONE',  ( 17.77761373051709981, 1.915879702936831519, -12.56867159344775153 ) ) ;
#59476 = CARTESIAN_POINT ( 'NONE',  ( 10.46085995768999943, 5.403395036974999677, 7.721808039505000387 ) ) ;
#59477 = CARTESIAN_POINT ( 'NONE',  ( 11.83518044953559922, 4.768048975940600620, 7.099502491684900107 ) ) ;
#59478 = EDGE_CURVE ( 'NONE', #31587, #9710, #41996, .T. ) ;
#59479 = EDGE_CURVE ( 'NONE', #50218, #24787, #13647, .T. ) ;
#59480 = CARTESIAN_POINT ( 'NONE',  ( 10.17905590578999941, -2.899999999999999911, 6.571291218949999902 ) ) ;
#59481 = CARTESIAN_POINT ( 'NONE',  ( 10.13035685320999946, -2.409329538444999752, -8.058042649154000259 ) ) ;
#59482 = CARTESIAN_POINT ( 'NONE',  ( 11.21253483539785556, 3.661009989788314822, -8.308639362931231176 ) ) ;
#59483 = B_SPLINE_SURFACE_WITH_KNOTS ( 'NONE', 3, 3, ( 
 ( #34559, #2044, #60765, #23364, #44704, #12880, #66345, #18467, #39793, #61116, #13233, #55870, #67370, #57836, #64102, #52941, #52590, #63415, #53285, #26375, #31280, #40812, #47701, #9944, #16216, #47357, #68661, #58522, #62136, #19495, #14255, #69012, #32314, #37204, #5037, #21458, #42794, #31620, #67034, #19144, #21125, #37538, #42451, #10627, #63761, #53627, #58871, #24396, #31971, #10976, #45726, #5385, #4684, #40465, #35240, #26724, #61796, #13913, #56554, #48037, #142, #8658, #36866, #3404, #30005, #20778, #51307 ),
 ( #24738, #46065, #15871, #15539, #42110, #36513, #26026, #58183, #10285, #6758, #34043, #64438, #38229, #17612, #6410, #16899, #43833, #5721, #37889, #11312, #59556, #49763, #48379, #54662, #38578, #21801, #33346, #32995, #28098, #27063, #44540, #49410, #27403, #12010, #11656, #48730, #55011, #65833, #54310, #1521, #16562, #22841, #27758, #32650, #44188, #33692, #833, #39276, #17254, #59209, #59902, #49069, #7112, #65485, #53962, #38935, #1180, #22149, #43134, #22491, #60257, #28450, #12361, #60598, #1873, #12709, #23192 ),
 ( #65133, #17959, #486, #6067, #43491, #64788, #24226, #56391, #34730, #29498, #7453, #19673, #8837, #35414, #19319, #44876, #23883, #7804, #66870, #50805, #23536, #29841, #29145, #40994, #30176, #62319, #13407, #8494, #2897, #56042, #24911, #45565, #24574, #51481, #66524, #61291, #51148, #55706, #45219, #28804, #3578, #66180, #46245, #3246, #18983, #40309, #67551, #14433, #50115, #61629, #45898, #55356, #18301, #18644, #67208, #8149, #39975, #13744, #2222, #39625, #60946, #35077, #13060, #34389, #40645, #61978, #50452 ),
 ( #2552, #14088, #56740, #36092, #9170, #35754, #53202, #62985, #68235, #3919, #68932, #25945, #52167, #10548, #57070, #63332, #25605, #25255, #15114, #14774, #63683, #15798, #46933, #60, #21383, #37127, #57751, #58445, #30509, #46593, #62654, #51821, #4611, #36786, #36434, #9863, #67899, #42715, #31891, #5303, #21046, #20017, #4269, #57407, #47278, #31207, #41341, #10208, #9511, #64019, #26645, #30853, #52511, #58106, #68579, #20701, #47962, #42030, #4962, #20357, #41680, #15461, #31541, #52861, #26295, #47621, #42378 ) ),
 .UNSPECIFIED., .F., .F., .F.,
 ( 4, 4 ),
 ( 4, 1, 1, 1, 1, 1, 1, 1, 1, 1, 1, 1, 1, 1, 1, 1, 1, 1, 1, 1, 1, 1, 1, 1, 1, 1, 1, 1, 1, 1, 1, 1, 1, 1, 1, 1, 1, 1, 1, 1, 1, 1, 1, 1, 1, 1, 1, 1, 1, 1, 1, 1, 1, 1, 1, 1, 1, 1, 1, 1, 1, 1, 1, 1, 4 ),
 ( -0.02000000000000000042, 1.020000000000000018 ),
 ( -0.02000000000000000042, -0.003749999999999999861, 0.01250000000000000069, 0.02875000000000000125, 0.04499999999999999833, 0.06124999999999999889, 0.07749999999999999944, 0.09375000000000000000, 0.1100000000000000006, 0.1262500000000000011, 0.1424999999999999878, 0.1587500000000000022, 0.1749999999999999889, 0.1912500000000000033, 0.2074999999999999900, 0.2237500000000000044, 0.2399999999999999911, 0.2562499999999999778, 0.2725000000000000200, 0.2887500000000000067, 0.3049999999999999933, 0.3212499999999999800, 0.3375000000000000222, 0.3537500000000000089, 0.3699999999999999956, 0.3862499999999999822, 0.4025000000000000244, 0.4187500000000000111, 0.4349999999999999978, 0.4512499999999999845, 0.4675000000000000266, 0.4837500000000000133, 0.5000000000000000000, 0.5162499999999999867, 0.5324999999999999734, 0.5487499999999999600, 0.5649999999999999467, 0.5812500000000000444, 0.5975000000000000311, 0.6137500000000000178, 0.6300000000000000044, 0.6462499999999999911, 0.6624999999999999778, 0.6787499999999999645, 0.6949999999999999512, 0.7112500000000000488, 0.7275000000000000355, 0.7437500000000000222, 0.7600000000000000089, 0.7762499999999999956, 0.7924999999999999822, 0.8087499999999999689, 0.8249999999999999556, 0.8412500000000000533, 0.8575000000000000400, 0.8737500000000000266, 0.8900000000000000133, 0.9062500000000000000, 0.9224999999999999867, 0.9387499999999999734, 0.9549999999999999600, 0.9712499999999999467, 0.9875000000000000444, 1.003749999999999920, 1.020000000000000018 ),
 .UNSPECIFIED. ) ;
#59484 = CARTESIAN_POINT ( 'NONE',  ( 5.500000000000000000, -12.78667792605000031, 2.345384795463000049 ) ) ;
#59485 = CARTESIAN_POINT ( 'NONE',  ( 11.38210843320517007, -5.137688304401064165, 6.901605483505062644 ) ) ;
#59486 = CARTESIAN_POINT ( 'NONE',  ( 9.390724454320221071, 5.236106858288462007, 6.940950143625023827 ) ) ;
#59487 = ORIENTED_EDGE ( 'NONE', *, *, #31453, .F. ) ;
#59488 = CARTESIAN_POINT ( 'NONE',  ( 9.193385841233000733, 2.981992329588000423, -5.895876591910999664 ) ) ;
#59489 = CARTESIAN_POINT ( 'NONE',  ( 10.78026357027499849, -3.014700852776899698, 7.309904858193100097 ) ) ;
#59490 = ORIENTED_EDGE ( 'NONE', *, *, #10523, .T. ) ;
#59491 = CONICAL_SURFACE ( 'NONE', #57243, 1.449999999967999553, 0.7853981633972997312 ) ;
#59492 = B_SPLINE_CURVE_WITH_KNOTS ( 'NONE', 3,
 ( #47726, #856, #5411, #32340 ),
 .UNSPECIFIED., .F., .F.,
 ( 4, 4 ),
 ( 0.000000000000000000, 0.3916346334472008972 ),
 .UNSPECIFIED. ) ;
#59493 = CARTESIAN_POINT ( 'NONE',  ( 17.96968152693882104, -2.032227188856706945, 13.76161273592455281 ) ) ;
#59494 = CARTESIAN_POINT ( 'NONE',  ( 11.55194988689359903, -3.419512757306400363, -8.638573882912000457 ) ) ;
#59495 = VERTEX_POINT ( 'NONE', #14202 ) ;
#59496 = CARTESIAN_POINT ( 'NONE',  ( 10.60235971519489873, 4.605301262871499546, 8.506961598696999971 ) ) ;
#59497 = CARTESIAN_POINT ( 'NONE',  ( 5.889917153847927800, -0.8233002406113282268, -0.7791036658657048974 ) ) ;
#59498 = CARTESIAN_POINT ( 'NONE',  ( 23.59999196693599899, 2.915561532799999966, -13.58550759281999909 ) ) ;
#59499 = VECTOR ( 'NONE', #22823, 1000.000000000000000 ) ;
#59500 = FACE_OUTER_BOUND ( 'NONE', #8877, .T. ) ;
#59501 = DIRECTION ( 'NONE',  ( 0.000000000000000000, -1.000000000000000000, 0.000000000000000000 ) ) ;
#59502 = CARTESIAN_POINT ( 'NONE',  ( 11.10000001610000098, 9.513034266426000585, -6.346422930067999957 ) ) ;
#59503 = DIRECTION ( 'NONE',  ( 0.000000000000000000, -0.01629188381079070894, 0.9998672784534433644 ) ) ;
#59504 = CARTESIAN_POINT ( 'NONE',  ( 9.792315001194999979, -4.284154785471999460, -9.000488933596999530 ) ) ;
#59505 = CARTESIAN_POINT ( 'NONE',  ( 4.000000000000000000, -2.040156275101109973, -0.6926574996740213486 ) ) ;
#59506 = ORIENTED_EDGE ( 'NONE', *, *, #35989, .T. ) ;
#59507 = EDGE_CURVE ( 'NONE', #61047, #52223, #9408, .T. ) ;
#59509 = EDGE_CURVE ( 'NONE', #60354, #36822, #16105, .T. ) ;
#59508 = CARTESIAN_POINT ( 'NONE',  ( 9.617285841233000454, 5.306366356490000769, -7.996450761531000317 ) ) ;
#59510 = ORIENTED_EDGE ( 'NONE', *, *, #5594, .F. ) ;
#59511 = VECTOR ( 'NONE', #10917, 1000.000000000000114 ) ;
#59512 = CARTESIAN_POINT ( 'NONE',  ( 0.5502919481377350763, -3.103829730453177671, -0.9712058421138561881 ) ) ;
#59513 = PRESENTATION_STYLE_ASSIGNMENT (( #54264 ) ) ;
#59514 = EDGE_CURVE ( 'NONE', #29064, #57460, #21919, .T. ) ;
#59515 = ORIENTED_EDGE ( 'NONE', *, *, #33620, .F. ) ;
#59516 = CARTESIAN_POINT ( 'NONE',  ( 9.457462135716001583, -5.100000000000000533, -6.571291218949999902 ) ) ;
#59517 = FILL_AREA_STYLE ('',( #38185 ) ) ;
#59518 = AXIS2_PLACEMENT_3D ( 'NONE', #4225, #46551, #30808 ) ;
#59519 = CARTESIAN_POINT ( 'NONE',  ( 10.67375944625267614, 3.325302618462734561, 6.944236520041479288 ) ) ;
#59520 = CARTESIAN_POINT ( 'NONE',  ( 8.999999001754000361, 0.000000000000000000, 0.000000000000000000 ) ) ;
#59521 = CARTESIAN_POINT ( 'NONE',  ( 12.52635726938498628, 3.059519608057332363, 13.53867825407380998 ) ) ;
#59522 = DIRECTION ( 'NONE',  ( -0.9999999999991096011, -6.425037516353057767E-07, -1.169597258120009531E-06 ) ) ;
#59523 = CARTESIAN_POINT ( 'NONE',  ( 7.854336256796271343, 2.876636076216872340, -6.723928215619836557 ) ) ;
#59524 = CARTESIAN_POINT ( 'NONE',  ( 12.21299871467824971, 0.2005085131878075189, 13.89805835524349931 ) ) ;
#59525 = ORIENTED_EDGE ( 'NONE', *, *, #20144, .T. ) ;
#59526 = CARTESIAN_POINT ( 'NONE',  ( 7.371771682458000186, 2.534482666265000184, -7.314862106114000007 ) ) ;
#59527 = LINE ( 'NONE', #66151, #36254 ) ;
#59528 = CARTESIAN_POINT ( 'NONE',  ( 9.885457958598628636, 4.856131813426149968, 7.680473230592850697 ) ) ;
#59529 = CARTESIAN_POINT ( 'NONE',  ( 4.231470154306000708, -1.075475585643000054, -0.8543500892798999713 ) ) ;
#59530 = EDGE_CURVE ( 'NONE', #59750, #25932, #32005, .T. ) ;
#59531 = CARTESIAN_POINT ( 'NONE',  ( 9.377520280414000098, 4.092867382745001059, -5.937785237406000505 ) ) ;
#59532 = DIRECTION ( 'NONE',  ( 0.000000000000000000, 1.000000000000000000, 0.000000000000000000 ) ) ;
#59533 = CARTESIAN_POINT ( 'NONE',  ( 10.31499432720999998, -5.458372854186999135, -8.355103994551999591 ) ) ;
#59534 = ORIENTED_EDGE ( 'NONE', *, *, #61446, .F. ) ;
#59535 = CARTESIAN_POINT ( 'NONE',  ( 8.179520121434947555, 4.176734390553195730, -8.849463778351122301 ) ) ;
#59536 = CARTESIAN_POINT ( 'NONE',  ( 11.04796807810000026, 5.246614701511999712, -5.093099051827000068 ) ) ;
#59537 = CARTESIAN_POINT ( 'NONE',  ( 11.79999999684100054, -3.345264396959000130, 11.86064773189999855 ) ) ;
#59538 = CARTESIAN_POINT ( 'NONE',  ( 11.09999999999999964, -2.649999999999999911, 7.500000000000000000 ) ) ;
#59539 = CARTESIAN_POINT ( 'NONE',  ( 8.567745513186627804, -3.352117027730234344, 5.929420235999764088 ) ) ;
#59540 = CARTESIAN_POINT ( 'NONE',  ( 0.1499942179679999987, 5.893556041935713383E-16, -2.749976859058071543 ) ) ;
#59541 = CIRCLE ( 'NONE', #5939, 1.625000000000000000 ) ;
#59542 = CARTESIAN_POINT ( 'NONE',  ( 11.47500581613029880, 4.988618570924500339, -8.134817373646898275 ) ) ;
#59543 = CARTESIAN_POINT ( 'NONE',  ( 10.14124205625000030, 3.639798001706899822, -8.437601616732200327 ) ) ;
#59545 = CARTESIAN_POINT ( 'NONE',  ( 8.335860198546281907, 4.831625175398913896, -6.127235342693542641 ) ) ;
#59544 = CARTESIAN_POINT ( 'NONE',  ( 9.496455549952999675, -3.218304396998100003, 8.130709350565298976 ) ) ;
#59546 = CARTESIAN_POINT ( 'NONE',  ( 10.90540321535448420, 2.790089835004012198, -6.887843015912778810 ) ) ;
#59547 = ORIENTED_EDGE ( 'NONE', *, *, #4563, .T. ) ;
#59548 = VECTOR ( 'NONE', #10785, 1000.000000000000000 ) ;
#59549 = CARTESIAN_POINT ( 'NONE',  ( 11.05946005378019947, 5.036385109519999403, 8.053412743695298914 ) ) ;
#59550 = CARTESIAN_POINT ( 'NONE',  ( 9.380781717619999682, -2.204246399534000034, 7.545378188773000261 ) ) ;
#59551 = CARTESIAN_POINT ( 'NONE',  ( 9.935646554150999066, 4.552790318865400643, 6.500921769151600138 ) ) ;
#59552 = CARTESIAN_POINT ( 'NONE',  ( 5.660639679273599789, -12.98305834912500956, -2.241106595026677528 ) ) ;
#59553 = CARTESIAN_POINT ( 'NONE',  ( 10.90374822854000136, -3.726845778959999578, 5.900452123196999743 ) ) ;
#59554 = CARTESIAN_POINT ( 'NONE',  ( 11.66486084871730000, -2.792989229543000107, 7.825000000000000178 ) ) ;
#59555 = CARTESIAN_POINT ( 'NONE',  ( 10.64393020684969926, 5.250000000000000000, 7.500000000000000000 ) ) ;
#59556 = CARTESIAN_POINT ( 'NONE',  ( 9.786633995697998856, -3.001718438313799808, -7.610798122400000310 ) ) ;
#59557 = CARTESIAN_POINT ( 'NONE',  ( 5.426046267568000125, 0.6950325411885999172, -1.124902434106000104 ) ) ;
#59558 = CARTESIAN_POINT ( 'NONE',  ( 11.56623059009865528, -4.687762524153129995, 8.035958501307058910 ) ) ;
#59559 = CIRCLE ( 'NONE', #7068, 13.98989069978000188 ) ;
#59560 = CARTESIAN_POINT ( 'NONE',  ( 8.061933748689000367, 4.603465626214999773, -6.221450782568999749 ) ) ;
#59561 = EDGE_CURVE ( 'NONE', #12318, #1268, #36169, .T. ) ;
#59562 = ADVANCED_FACE ( 'NONE', ( #37235 ), #61919, .T. ) ;
#59563 = CARTESIAN_POINT ( 'NONE',  ( 11.99056651104150006, -3.914543207408039738, 8.361971998931499783 ) ) ;
#59564 = CARTESIAN_POINT ( 'NONE',  ( 11.34287482311539996, 4.803125295093300551, -7.824481664695199790 ) ) ;
#59565 = CARTESIAN_POINT ( 'NONE',  ( 6.953052440528999512, -9.233022020364000326, -5.200634764108000851 ) ) ;
#59566 = CARTESIAN_POINT ( 'NONE',  ( 8.630000000000000782, 4.924138593003999809, -8.484107647018999998 ) ) ;
#59567 = CARTESIAN_POINT ( 'NONE',  ( 1.040556799208345984, 3.500000000000000888, -0.4581489286485045387 ) ) ;
#59568 = VERTEX_POINT ( 'NONE', #10658 ) ;
#59569 = CARTESIAN_POINT ( 'NONE',  ( 7.621217240535393067, -3.646027591375869292, 8.814378988131492676 ) ) ;
#59570 = CARTESIAN_POINT ( 'NONE',  ( 10.65413259636999932, -4.783377755405500587, -7.926858177843299380 ) ) ;
#59571 = CARTESIAN_POINT ( 'NONE',  ( 0.7000000000000000666, 0.000000000000000000, -0.5999999999999999778 ) ) ;
#59572 = CARTESIAN_POINT ( 'NONE',  ( 10.58351354018237345, -2.750000000000000000, 7.336375382625531572 ) ) ;
#59573 = DIRECTION ( 'NONE',  ( -1.000000000000000000, 0.000000000000000000, 0.000000000000000000 ) ) ;
#59574 = CARTESIAN_POINT ( 'NONE',  ( 13.64495723965300122, 12.20594327342000085, 2.556931772870000064 ) ) ;
#59575 = EDGE_LOOP ( 'NONE', ( #46182, #36620, #64416, #51538, #54999 ) ) ;
#59576 = PLANE ( 'NONE',  #45155 ) ;
#59577 = CARTESIAN_POINT ( 'NONE',  ( 8.768793171737998549, -4.404188085824999987, -8.374125585548998885 ) ) ;
#59578 = ORIENTED_EDGE ( 'NONE', *, *, #39146, .T. ) ;
#59579 = CARTESIAN_POINT ( 'NONE',  ( 12.80505043854146940, -1.875000000000000444, 12.57545641911172396 ) ) ;
#59580 = CARTESIAN_POINT ( 'NONE',  ( 24.74121292487855683, 8.638778361025718056, -8.580587272887251871 ) ) ;
#59581 = CARTESIAN_POINT ( 'NONE',  ( 9.617764158771999305, 5.322769172805999816, -7.951018786192998178 ) ) ;
#59582 = VERTEX_POINT ( 'NONE', #53319 ) ;
#59583 = CARTESIAN_POINT ( 'NONE',  ( 23.75091537440847134, -13.09198522470825132, 3.783037687685711692 ) ) ;
#59584 = CARTESIAN_POINT ( 'NONE',  ( 11.83003632436370012, -5.243255406354000669, -7.209663534847899236 ) ) ;
#59585 = CARTESIAN_POINT ( 'NONE',  ( 7.075545280406999815, 2.634456420141999988, -6.433888043919999689 ) ) ;
#59586 = DIRECTION ( 'NONE',  ( 0.000000000000000000, 1.000000000000000000, 0.000000000000000000 ) ) ;
#59587 = CARTESIAN_POINT ( 'NONE',  ( 7.903233148129999996, 5.126111344052000085, 6.730859635691999188 ) ) ;
#59588 = VERTEX_POINT ( 'NONE', #53661 ) ;
#59589 = CARTESIAN_POINT ( 'NONE',  ( 9.696086916451999826, -2.554404004330999900, 7.600685922079000179 ) ) ;
#59590 = VECTOR ( 'NONE', #65896, 1000.000000000000000 ) ;
#59591 = CARTESIAN_POINT ( 'NONE',  ( 24.69899733841000256, 12.37167067653999908, -2.942311114818999762 ) ) ;
#59592 = DIRECTION ( 'NONE',  ( -1.000000000000000000, 0.000000000000000000, 0.000000000000000000 ) ) ;
#59593 = ORIENTED_EDGE ( 'NONE', *, *, #61959, .F. ) ;
#59594 = AXIS2_PLACEMENT_3D ( 'NONE', #58585, #31681, #36926 ) ;
#59595 = CARTESIAN_POINT ( 'NONE',  ( 16.10005255078199937, 3.632778330393000132, 11.06917548872000090 ) ) ;
#59596 = CARTESIAN_POINT ( 'NONE',  ( 10.50084194037999907, -4.616788958496999662, -6.288071994190999270 ) ) ;
#59597 = ADVANCED_FACE ( 'NONE', ( #5754 ), #17644, .F. ) ;
#59598 = ORIENTED_EDGE ( 'NONE', *, *, #54312, .T. ) ;
#59599 = CARTESIAN_POINT ( 'NONE',  ( 9.026759580228999269, 3.023107159668900312, 7.733500918284399894 ) ) ;
#59600 = CARTESIAN_POINT ( 'NONE',  ( 17.74439936569998366, -1.785463535057947970, -12.47285731025142930 ) ) ;
#59601 = CARTESIAN_POINT ( 'NONE',  ( 4.990120016635999356, -1.409123102148000184, -0.1442114013433999919 ) ) ;
#59602 = CARTESIAN_POINT ( 'NONE',  ( 8.298828076409998644, 5.104449167533000598, -6.663856854024003518 ) ) ;
#59603 = CARTESIAN_POINT ( 'NONE',  ( 24.63609380610749966, 11.85365310353625823, -3.193521306612203237 ) ) ;
#59604 = CARTESIAN_POINT ( 'NONE',  ( 7.135647982796729849, 4.855545130758272876, -8.555041308852223025 ) ) ;
#59605 = B_SPLINE_CURVE_WITH_KNOTS ( 'NONE', 3,
 ( #67129, #12627, #29068, #61551 ),
 .UNSPECIFIED., .F., .F.,
 ( 4, 4 ),
 ( 0.000000000000000000, 1.000000000000000000 ),
 .UNSPECIFIED. ) ;
#59606 = CARTESIAN_POINT ( 'NONE',  ( 9.434038493598999153, 4.627468580434300094, 8.098323595618600379 ) ) ;
#59607 = CARTESIAN_POINT ( 'NONE',  ( 9.346662412757066107, -3.521875972694050283, 9.173020653676831060 ) ) ;
#59608 = ORIENTED_EDGE ( 'NONE', *, *, #55660, .T. ) ;
#59609 = CARTESIAN_POINT ( 'NONE',  ( 8.228368194306998618, -4.806758213702000404, 6.177034600996000435 ) ) ;
#59610 = CARTESIAN_POINT ( 'NONE',  ( 11.17788388625999829, 2.412139249855000056, -7.075601348558000048 ) ) ;
#59611 = CIRCLE ( 'NONE', #60716, 1.300162295583999539 ) ;
#59612 = CARTESIAN_POINT ( 'NONE',  ( 1.700000811628999964, 0.000000000000000000, -1.775000326286801045 ) ) ;
#59613 = CARTESIAN_POINT ( 'NONE',  ( 12.18472282150162478, 2.421014800242781373, -13.68991273180144574 ) ) ;
#59614 = CARTESIAN_POINT ( 'NONE',  ( 3.606513041767000161, 1.901420734585999917, 3.183432923345000276 ) ) ;
#59615 = CARTESIAN_POINT ( 'NONE',  ( 9.215289122285998502, -4.861979632688999686, 8.938813901364000003 ) ) ;
#59616 = EDGE_CURVE ( 'NONE', #35697, #43682, #32835, .T. ) ;
#59617 = CARTESIAN_POINT ( 'NONE',  ( 18.11117642456259347, -0.2854033456632683041, 13.89606078824648172 ) ) ;
#59618 = AXIS2_PLACEMENT_3D ( 'NONE', #7778, #55328, #7425 ) ;
#59619 = CARTESIAN_POINT ( 'NONE',  ( 17.90980351667704085, 0.5146449799214740661, 13.88717540043435861 ) ) ;
#59620 = VERTEX_POINT ( 'NONE', #44222 ) ;
#59621 = EDGE_LOOP ( 'NONE', ( #38969, #25558, #54951, #63393 ) ) ;
#59622 = CARTESIAN_POINT ( 'NONE',  ( 10.46754281781999829, 2.318340407652000223, 6.549777679168999001 ) ) ;
#59623 = CARTESIAN_POINT ( 'NONE',  ( 12.31853810497323920, -0.3923498216886506240, 13.89254714538524027 ) ) ;
#59624 = CIRCLE ( 'NONE', #62951, 14.00000000000000000 ) ;
#59625 = CARTESIAN_POINT ( 'NONE',  ( 10.59964828895399869, -2.878385131502000149, 6.887384543790600056 ) ) ;
#59626 = CARTESIAN_POINT ( 'NONE',  ( 9.660601868375998436, -2.901236202253999696, -6.151180522693000086 ) ) ;
#59627 = CARTESIAN_POINT ( 'NONE',  ( 18.02496672418951107, -0.4121037243925090299, -13.89177745834417088 ) ) ;
#59628 = CARTESIAN_POINT ( 'NONE',  ( 9.069724726289001282, -4.108965473266000146, 8.851626696081998702 ) ) ;
#59629 = CARTESIAN_POINT ( 'NONE',  ( 0.7000000000000000666, -0.5773502691895999739, 1.000000000000000000 ) ) ;
#59631 = CARTESIAN_POINT ( 'NONE',  ( 13.99999999347100044, -9.187456302440001110, -8.213201953411001455 ) ) ;
#59630 = CARTESIAN_POINT ( 'NONE',  ( 9.779101285863999848, -4.823683599683300294, 8.478738839062499366 ) ) ;
#59632 = CARTESIAN_POINT ( 'NONE',  ( 10.27195525820100031, 3.879327850572200198, -6.227697122196000024 ) ) ;
#59633 = CARTESIAN_POINT ( 'NONE',  ( 7.523326529072416946, 5.204747376180668184, -6.795163621442438462 ) ) ;
#59634 = DIRECTION ( 'NONE',  ( 1.000000000000000000, 0.000000000000000000, 0.000000000000000000 ) ) ;
#59635 = CARTESIAN_POINT ( 'NONE',  ( 17.74611058647004214, -0.5951698179256270649, 12.68122092285040559 ) ) ;
#59636 = B_SPLINE_SURFACE_WITH_KNOTS ( 'NONE', 3, 3, ( 
 ( #3428, #19170, #40494, #8684, #61482, #14282, #30032, #18496, #29339, #13601, #44729, #51334, #34922, #24764, #67397, #66372, #19518, #23389, #55899, #8345, #66026, #8003, #55205, #18150, #39821, #34583, #39471, #29691, #12906, #34234, #55553, #30696, #52703, #46778, #62497 ),
 ( #62838, #25445, #63177, #56921, #63534, #20546, #41870, #15645, #36979, #68082, #69126, #57955, #52006, #14956, #35609, #42563, #4798, #42227, #20198, #31050, #58290, #41192, #52360, #9353, #4452, #15306, #53053, #36631, #5151, #4109, #10053, #25793, #51669, #31389, #9021 ),
 ( #41525, #36281, #26141, #57597, #47467, #3765, #30361, #9704, #47123, #63871, #10395, #68424, #31733, #68772, #20891, #26486, #47818, #21232, #25103, #46435, #67737, #19860, #14620, #35939, #57251, #53739, #37657, #49182, #15985, #32424, #64900, #11089, #65255, #6874, #27517 ),
 ( #11770, #32085, #27872, #48152, #64213, #59324, #48845, #17014, #1293, #21914, #22605, #54079, #58635, #5499, #38698, #5837, #950, #255, #43950, #49524, #33113, #17370, #11424, #37997, #60020, #6175, #27175, #33460, #12130, #32765, #43603, #22263, #21570, #54428, #54773 ) ),
 .UNSPECIFIED., .F., .F., .F.,
 ( 4, 4 ),
 ( 4, 1, 1, 1, 1, 1, 1, 1, 1, 1, 1, 1, 1, 1, 1, 1, 1, 1, 1, 1, 1, 1, 1, 1, 1, 1, 1, 1, 1, 1, 1, 1, 4 ),
 ( -0.02000000000000000042, 1.020000000000000018 ),
 ( 0.1633025096610999927, 0.1899619885200000136, 0.2166214673788000034, 0.2432809462376999965, 0.2699404250964999585, 0.2965999039553000038, 0.3232593828141999692, 0.3499188616730000145, 0.3765783405318000043, 0.4032378193906999697, 0.4298972982494999595, 0.4565567771083000048, 0.4832162559671999702, 0.5098757348260000155, 0.5365352136848999809, 0.5631946925437000262, 0.5898541714025000715, 0.6165136502614000369, 0.6431731291201999712, 0.6698326079790000165, 0.6964920868378999819, 0.7231515656967000272, 0.7498110445554999615, 0.7764705234143999268, 0.8031300022731999722, 0.8297894811320000175, 0.8564489599908999828, 0.8831084388497000282, 0.9097679177085999935, 0.9364273965674000388, 0.9630868754261999731, 0.9897463542851000495, 1.016405833144000015 ),
 .UNSPECIFIED. ) ;
#59637 = CARTESIAN_POINT ( 'NONE',  ( 11.10000000000000142, -5.360253205841783775, 6.560009693585453938 ) ) ;
#59638 = DIRECTION ( 'NONE',  ( 1.000000000000000000, 0.000000000000000000, 0.000000000000000000 ) ) ;
#59639 = EDGE_LOOP ( 'NONE', ( #16305, #23480, #7867, #45656, #19697 ) ) ;
#59640 = CARTESIAN_POINT ( 'NONE',  ( 8.096558059622999792, -5.061720701958000390, 5.824087910811999613 ) ) ;
#59641 = CARTESIAN_POINT ( 'NONE',  ( 8.415504719592000527, 2.469361196073999842, -7.826019481986000059 ) ) ;
#59642 = LINE ( 'NONE', #16644, #6999 ) ;
#59643 = CARTESIAN_POINT ( 'NONE',  ( 7.024698286478646025, -1.201388655186206300, -0.6934264365339433134 ) ) ;
#59644 = CARTESIAN_POINT ( 'NONE',  ( 0.5845045405018999274, -1.124254478562000115, 3.354249223527999924 ) ) ;
#59645 = CARTESIAN_POINT ( 'NONE',  ( 11.40211496860029783, 4.793947479907100018, 7.906860999147899527 ) ) ;
#59646 = CARTESIAN_POINT ( 'NONE',  ( 10.53871084122999946, 5.103389446345000025, -6.705205355781999721 ) ) ;
#59647 = VERTEX_POINT ( 'NONE', #33724 ) ;
#59648 = EDGE_CURVE ( 'NONE', #15625, #54866, #13526, .T. ) ;
#59649 = ADVANCED_FACE ( 'NONE', ( #39306 ), #49443, .F. ) ;
#59650 = CARTESIAN_POINT ( 'NONE',  ( 12.09898038912532847, -0.1637242582067878482, -12.59894148523290980 ) ) ;
#59651 = DIRECTION ( 'NONE',  ( 0.000000000000000000, 1.000000000000000000, 0.000000000000000000 ) ) ;
#59652 = CARTESIAN_POINT ( 'NONE',  ( 18.26373780016885107, 2.633255345072546216, -12.32177353326231461 ) ) ;
#59653 = CARTESIAN_POINT ( 'NONE',  ( 5.600889858812243105, 12.13276343987783257, 3.750125071915198838 ) ) ;
#59654 = CARTESIAN_POINT ( 'NONE',  ( 8.090517219592001652, 5.342170561818999630, 8.432311822615000452 ) ) ;
#59655 = ORIENTED_EDGE ( 'NONE', *, *, #18539, .F. ) ;
#59656 = CARTESIAN_POINT ( 'NONE',  ( 6.508089701055999932, -1.390318139369000061, -0.4728033673814999727 ) ) ;
#59657 = ADVANCED_FACE ( 'NONE', ( #40005 ), #44064, .T. ) ;
#59658 = ADVANCED_FACE ( 'NONE', ( #33377 ), #2251, .F. ) ;
#59659 = CARTESIAN_POINT ( 'NONE',  ( 7.797795280408000629, 2.733910551100999786, -6.580132171107999639 ) ) ;
#59661 = CARTESIAN_POINT ( 'NONE',  ( 8.795853127542962113, -3.970210778477947233, -8.445853177989366856 ) ) ;
#59660 = CARTESIAN_POINT ( 'NONE',  ( 8.399899185017186909, -2.585175040501215715, 8.516097464460264277 ) ) ;
#59662 = CARTESIAN_POINT ( 'NONE',  ( 13.84418086767167466, 9.492976300297533143, 8.170822042178436106 ) ) ;
#59663 = ORIENTED_EDGE ( 'NONE', *, *, #3732, .F. ) ;
#59664 = CARTESIAN_POINT ( 'NONE',  ( 11.09999999999999964, -2.700000000746000328, 5.148510364898998937 ) ) ;
#59665 = ORIENTED_EDGE ( 'NONE', *, *, #44078, .T. ) ;
#59666 = CARTESIAN_POINT ( 'NONE',  ( 11.10000000000000142, 2.264782496563556791, -7.479749973481406577 ) ) ;
#59667 = CARTESIAN_POINT ( 'NONE',  ( 16.22809631267600139, 3.350750460640000039, 11.21314580301999797 ) ) ;
#59668 = VECTOR ( 'NONE', #66202, 1000.000000000000114 ) ;
#59669 = CARTESIAN_POINT ( 'NONE',  ( 17.67410956179875470, 0.7206971133477627633, -13.98143832535762776 ) ) ;
#59670 = ORIENTED_EDGE ( 'NONE', *, *, #23183, .T. ) ;
#59671 = CARTESIAN_POINT ( 'NONE',  ( 13.50000000000339639, 9.396284335645857411, 7.729197028970922645 ) ) ;
#59672 = SURFACE_SIDE_STYLE ('',( #21913 ) ) ;
#59673 = CARTESIAN_POINT ( 'NONE',  ( 10.09393020685000053, -2.750000000000000000, 7.500000000000000000 ) ) ;
#59674 = DIRECTION ( 'NONE',  ( 0.000000000000000000, 0.000000000000000000, 1.000000000000000000 ) ) ;
#59675 = CARTESIAN_POINT ( 'NONE',  ( 11.41195257254739914, -5.227167235646000165, 7.143100915737699452 ) ) ;
#59676 = ORIENTED_EDGE ( 'NONE', *, *, #57123, .F. ) ;
#59677 = CARTESIAN_POINT ( 'NONE',  ( 8.962739158771999115, 5.445214367171999470, 7.703373622193999459 ) ) ;
#59678 = CARTESIAN_POINT ( 'NONE',  ( 8.564919648097475857, 5.350116636189168773, -7.500005043868485544 ) ) ;
#59679 = EDGE_CURVE ( 'NONE', #6927, #54265, #15244, .T. ) ;
#59680 = CARTESIAN_POINT ( 'NONE',  ( 9.393930206848999376, -5.250000000000000000, -7.500000000000000000 ) ) ;
#59681 = CARTESIAN_POINT ( 'NONE',  ( 15.55534550153200080, -9.119897322331999234, -8.232476562723000768 ) ) ;
#59682 = CARTESIAN_POINT ( 'NONE',  ( 11.12487850024999858, 6.581971541694000116, -5.643519261885000304 ) ) ;
#59683 = ORIENTED_EDGE ( 'NONE', *, *, #64901, .T. ) ;
#59684 = CARTESIAN_POINT ( 'NONE',  ( 12.18947222198080205, -2.391413182808839633, -12.47619792628429813 ) ) ;
#59685 = CARTESIAN_POINT ( 'NONE',  ( 10.77101354018289925, 3.231816600031359066, -6.500416447002272058 ) ) ;
#59686 = CARTESIAN_POINT ( 'NONE',  ( 11.33810207955129812, 4.796537143354000499, -7.825000000000000178 ) ) ;
#59687 = CARTESIAN_POINT ( 'NONE',  ( 11.89975833414730033, -3.203462856645999945, 7.825000000000000178 ) ) ;
#59688 = CARTESIAN_POINT ( 'NONE',  ( 12.29903578917718932, -3.040996334883329766, -13.66573881806045421 ) ) ;
#59689 = CARTESIAN_POINT ( 'NONE',  ( 11.38379707368349969, -4.566644629509899467, -6.509947486183500054 ) ) ;
#59690 = CARTESIAN_POINT ( 'NONE',  ( 12.80505043854146940, -1.760845406083394016, 12.47635457398814829 ) ) ;
#59691 = CARTESIAN_POINT ( 'NONE',  ( 18.05438665931233189, -1.958444820271050046, 12.44686948166836160 ) ) ;
#59692 = VERTEX_POINT ( 'NONE', #51851 ) ;
#59693 = CARTESIAN_POINT ( 'NONE',  ( 11.30367835872029936, -5.113555564477999305, -6.798177532456199934 ) ) ;
#59694 = VERTEX_POINT ( 'NONE', #3949 ) ;
#59695 = CARTESIAN_POINT ( 'NONE',  ( 11.55259020248000112, -12.34178403982000205, -1.785089783152000065 ) ) ;
#59696 = CARTESIAN_POINT ( 'NONE',  ( 9.833904719592002408, 5.048004622677000341, -6.120508709481000231 ) ) ;
#59697 = CARTESIAN_POINT ( 'NONE',  ( 10.83768005408999890, 5.758100475276000552, -6.911469147650000977 ) ) ;
#59698 = CARTESIAN_POINT ( 'NONE',  ( 10.46009514222999925, -2.565650894080999667, -6.975682682930000489 ) ) ;
#59699 = EDGE_CURVE ( 'NONE', #50821, #33837, #54360, .T. ) ;
#59700 = CARTESIAN_POINT ( 'NONE',  ( 9.110944094209999733, 5.100000000000000533, -6.571291218949999902 ) ) ;
#59701 = CARTESIAN_POINT ( 'NONE',  ( 24.56892806240000127, 12.57303442533000037, 2.966957253552999774 ) ) ;
#59702 = CARTESIAN_POINT ( 'NONE',  ( 5.699999999877000789, -1.433333330872999856, 10.65401593578999950 ) ) ;
#59703 = EDGE_LOOP ( 'NONE', ( #21592, #40468, #27185, #48066 ) ) ;
#59704 = EDGE_CURVE ( 'NONE', #44736, #55747, #61064, .T. ) ;
#59705 = CARTESIAN_POINT ( 'NONE',  ( 23.60000000000000142, 2.548720605937000006, 12.21654710926000220 ) ) ;
#59706 = CARTESIAN_POINT ( 'NONE',  ( 9.318724127987000116, 2.755029797911999978, 8.795125756257000660 ) ) ;
#59707 = CARTESIAN_POINT ( 'NONE',  ( 10.44079553768663615, 5.100000000000000533, 6.662590550639045262 ) ) ;
#59708 = B_SPLINE_CURVE_WITH_KNOTS ( 'NONE', 3,
 ( #54942, #44810, #44472, #60189, #12294, #24159, #65765, #18579, #23120, #12638, #33624, #7043, #17891, #28378, #8086, #50390 ),
 .UNSPECIFIED., .F., .F.,
 ( 4, 2, 2, 2, 2, 2, 2, 4 ),
 ( 0.000000000000000000, 0.06250000000000123512, 0.1250000000000024702, 0.2500000000000007216, 0.5000000000000004441, 0.7500000000000002220, 0.8750000000000002220, 1.000000000000000000 ),
 .UNSPECIFIED. ) ;
#59709 = CARTESIAN_POINT ( 'NONE',  ( 11.34393020684979980, -5.250000000000000000, 7.500000000000000000 ) ) ;
#59710 = CARTESIAN_POINT ( 'NONE',  ( 11.09999999999999964, -2.700000000000000178, -5.157071250680000496 ) ) ;
#59711 = CARTESIAN_POINT ( 'NONE',  ( 11.78179573085659904, 4.973133828855400118, -7.668383662421899061 ) ) ;
#59712 = CARTESIAN_POINT ( 'NONE',  ( 24.53428991268900106, -12.47024905405999995, -3.026245386525999947 ) ) ;
#59713 = VECTOR ( 'NONE', #66642, 1000.000000000000000 ) ;
#59714 = CARTESIAN_POINT ( 'NONE',  ( 23.73577082021700235, -9.841767396222000031, -9.786596206530999709 ) ) ;
#59715 = FACE_OUTER_BOUND ( 'NONE', #46352, .T. ) ;
#59716 = CARTESIAN_POINT ( 'NONE',  ( 10.81021345716900051, -3.363461959113699606, 6.921280946186199934 ) ) ;
#59717 = ORIENTED_EDGE ( 'NONE', *, *, #43371, .F. ) ;
#59718 = DIRECTION ( 'NONE',  ( -1.000000000000000000, 0.000000000000000000, 0.000000000000000000 ) ) ;
#59719 = CARTESIAN_POINT ( 'NONE',  ( 6.840023874967999795, -0.9883789325241000290, 0.7262708681523000198 ) ) ;
#59720 = CARTESIAN_POINT ( 'NONE',  ( 18.09690629521215044, 2.811641957965460570, 13.60235445620235595 ) ) ;
#59721 = CARTESIAN_POINT ( 'NONE',  ( 11.09999999999999964, 5.299771130038000599, -5.136740763824000133 ) ) ;
#59722 = CARTESIAN_POINT ( 'NONE',  ( 10.15303300763299887, -3.212834858289399964, -8.325626572044798834 ) ) ;
#59723 = ORIENTED_EDGE ( 'NONE', *, *, #47753, .T. ) ;
#59724 = CARTESIAN_POINT ( 'NONE',  ( 10.66914689902483104, -4.353380376947088237, -8.814970433265349570 ) ) ;
#59725 = CARTESIAN_POINT ( 'NONE',  ( 8.630420280412000267, 5.808262417891000062, 7.446016144116000213 ) ) ;
#59727 = CARTESIAN_POINT ( 'NONE',  ( 5.200000000000000178, -1.199999999999999956, -9.776630298829998011 ) ) ;
#59726 = CARTESIAN_POINT ( 'NONE',  ( 9.708354719591000048, 5.481267232667000222, -8.005061172455999241 ) ) ;
#59728 = CARTESIAN_POINT ( 'NONE',  ( 10.82894633243970084, -2.649868422364446197, -7.263390030261637875 ) ) ;
#59729 = EDGE_LOOP ( 'NONE', ( #47725, #4007, #39299, #46684 ) ) ;
#59730 = B_SPLINE_CURVE_WITH_KNOTS ( 'NONE', 3,
 ( #22992, #39427, #2026, #24032, #18107, #66674, #39083, #60406, #60745, #44688, #13895, #29646, #18449, #8301, #50606, #18797, #39775, #2707 ),
 .UNSPECIFIED., .F., .F.,
 ( 4, 2, 2, 2, 2, 2, 2, 2, 4 ),
 ( 0.000000000000000000, 0.1249999999999994726, 0.2499999999999989453, 0.3749999999999991673, 0.4999999999999994449, 0.6249999999999994449, 0.7499999999999994449, 0.8749999999999995559, 1.000000000000000000 ),
 .UNSPECIFIED. ) ;
#59731 = CARTESIAN_POINT ( 'NONE',  ( 10.83658792121999959, 5.133186143592999962, 8.848368005200001107 ) ) ;
#59732 = CARTESIAN_POINT ( 'NONE',  ( 18.02709866344915923, -1.963667282347026921, -13.86160417883469975 ) ) ;
#59733 = CARTESIAN_POINT ( 'NONE',  ( 10.77256919669529900, 4.962345366016100101, 7.215672285280100517 ) ) ;
#59734 = CARTESIAN_POINT ( 'NONE',  ( 9.736871746126999128, -2.742172332680000046, 6.839224809731999422 ) ) ;
#59735 = CARTESIAN_POINT ( 'NONE',  ( 7.764631182151003230, 2.924915923740001311, 6.482382710726004582 ) ) ;
#59736 = EDGE_LOOP ( 'NONE', ( #31458, #61197, #55467, #48501 ) ) ;
#59737 = CARTESIAN_POINT ( 'NONE',  ( 24.30857393632600250, 12.13191889359999998, -3.290345171646999578 ) ) ;
#59738 = EDGE_CURVE ( 'NONE', #518, #30733, #14390, .T. ) ;
#59739 = ADVANCED_FACE ( 'NONE', ( #45595 ), #67928, .T. ) ;
#59741 = CARTESIAN_POINT ( 'NONE',  ( 11.07691935321000010, -3.101896674955000321, -8.926549689995999515 ) ) ;
#59740 = CARTESIAN_POINT ( 'NONE',  ( 12.10154284453400209, -11.81398323980999976, 3.695357857504999899 ) ) ;
#59742 = CARTESIAN_POINT ( 'NONE',  ( 7.654159297465730205, -5.473926550294729410, 6.558698546940537888 ) ) ;
#59743 = CARTESIAN_POINT ( 'NONE',  ( 10.18755811987000115, -5.387486580809999204, 8.640943191857999750 ) ) ;
#59744 = CARTESIAN_POINT ( 'NONE',  ( 11.71922412107039868, -3.930460928605089777, -6.185573549454999487 ) ) ;
#59745 = VERTEX_POINT ( 'NONE', #41024 ) ;
#59746 = DIRECTION ( 'NONE',  ( 0.7071065367651552247, 0.7071070256078553218, -1.045644868292934240E-09 ) ) ;
#59747 = CARTESIAN_POINT ( 'NONE',  ( 11.80995122972050027, -3.547233695387300045, 8.547040013405998948 ) ) ;
#59748 = CARTESIAN_POINT ( 'NONE',  ( 7.545207810761997536, 3.529659010889000026, 6.570477302111996210 ) ) ;
#59749 = CARTESIAN_POINT ( 'NONE',  ( 10.64118447801629941, 5.277702140407999565, 7.528171279442569919 ) ) ;
#59750 = VERTEX_POINT ( 'NONE', #20043 ) ;
#59751 = CARTESIAN_POINT ( 'NONE',  ( 8.573539158775000502, 5.361622798585000460, -7.185294144754000634 ) ) ;
#59752 = CARTESIAN_POINT ( 'NONE',  ( 23.82002767510200414, 12.91624849431999955, -3.707179493336999698 ) ) ;
#59753 = CARTESIAN_POINT ( 'NONE',  ( 12.28182936075425857, 2.978585426876357189, -12.24287970063667075 ) ) ;
#59754 = CARTESIAN_POINT ( 'NONE',  ( 11.14391429142989942, -3.977620450637519678, 8.674673860548999471 ) ) ;
#59755 = EDGE_CURVE ( 'NONE', #47838, #54862, #60823, .T. ) ;
#59756 = ORIENTED_EDGE ( 'NONE', *, *, #23791, .F. ) ;
#59757 = CARTESIAN_POINT ( 'NONE',  ( 23.59999443371599881, 2.915558930973999985, 13.58549620949000136 ) ) ;
#59758 = CARTESIAN_POINT ( 'NONE',  ( 10.56059687351646481, 4.629523725463624118, -8.592232985442823434 ) ) ;
#59759 = ORIENTED_EDGE ( 'NONE', *, *, #23411, .F. ) ;
#59760 = CARTESIAN_POINT ( 'NONE',  ( 8.817629440380001071, -3.894643656844000379, 6.044452984962999764 ) ) ;
#59761 = CARTESIAN_POINT ( 'NONE',  ( 5.794609839684291330, 1.500000000000001110, -0.1963495408493590721 ) ) ;
#59762 = ORIENTED_EDGE ( 'NONE', *, *, #6289, .T. ) ;
#59763 = FACE_OUTER_BOUND ( 'NONE', #65440, .T. ) ;
#59765 = CARTESIAN_POINT ( 'NONE',  ( 10.94487616594229884, 3.696562859151900415, 8.456491899811199531 ) ) ;
#59764 = CIRCLE ( 'NONE', #36311, 11.84999999999999964 ) ;
#59766 = CARTESIAN_POINT ( 'NONE',  ( 10.60770805961999841, -2.392337812398999564, -6.587351599745000286 ) ) ;
#59767 = CARTESIAN_POINT ( 'NONE',  ( 10.63559687351579974, 5.092232985442826099, 8.129523725463617012 ) ) ;
#59768 = CARTESIAN_POINT ( 'NONE',  ( 18.53600088859200312, -11.84356608895999941, 4.189033083324999573 ) ) ;
#59769 = CARTESIAN_POINT ( 'NONE',  ( 10.57893103570000015, -4.649956431060000561, 5.681096060554999383 ) ) ;
#59770 = DIRECTION ( 'NONE',  ( -1.000000000000000000, -1.308972661142999917E-10, -2.029855754503000182E-09 ) ) ;
#59771 = CARTESIAN_POINT ( 'NONE',  ( 17.93599305328152482, -0.4959072410923969776, -12.68697406334525546 ) ) ;
#59772 = CARTESIAN_POINT ( 'NONE',  ( 12.19311196912284778, 2.627115699720651065, -12.42106741852103191 ) ) ;
#59773 = CARTESIAN_POINT ( 'NONE',  ( 10.98995257254739855, -5.095356924909000718, -7.818564472783199548 ) ) ;
#59774 = CARTESIAN_POINT ( 'NONE',  ( 8.738426658774001154, 5.414918126383000185, 8.890678916765999418 ) ) ;
#59775 = ORIENTED_EDGE ( 'NONE', *, *, #59963, .F. ) ;
#59776 = SURFACE_STYLE_FILL_AREA ( #22370 ) ;
#59777 = DIRECTION ( 'NONE',  ( 0.9999999999777403614, -3.933702046811161244E-06, -5.389360668004222102E-06 ) ) ;
#59778 = DIRECTION ( 'NONE',  ( -0.4999999999999719669, 0.6407827956774649891, -0.5825782426110679424 ) ) ;
#59779 = CARTESIAN_POINT ( 'NONE',  ( 11.35642168284000242, 12.27417251877000126, 1.600391102631000040 ) ) ;
#59780 = CARTESIAN_POINT ( 'NONE',  ( 18.10215020711899214, 2.952580169587743164, 12.24917755118608831 ) ) ;
#59781 = CARTESIAN_POINT ( 'NONE',  ( 25.46372797112000086, -8.354608193938998895, 8.148457429720000533 ) ) ;
#59782 = CARTESIAN_POINT ( 'NONE',  ( 11.05294428647999894, 9.762867297161999858, 6.037733508755000145 ) ) ;
#59783 = EDGE_CURVE ( 'NONE', #42751, #25355, #15053, .T. ) ;
#59784 = CARTESIAN_POINT ( 'NONE',  ( 10.03084989804662719, -4.391573077584247642, 8.282433891029866047 ) ) ;
#59785 = CARTESIAN_POINT ( 'NONE',  ( 9.989763540182750035, -3.672815144550900524, -8.717465845835395299 ) ) ;
#59786 = AXIS2_PLACEMENT_3D ( 'NONE', #30149, #9143, #52135 ) ;
#59787 = ORIENTED_EDGE ( 'NONE', *, *, #10561, .T. ) ;
#59788 = CARTESIAN_POINT ( 'NONE',  ( 12.30724456330684546, -3.003488097433224535, 12.23679193692684741 ) ) ;
#59789 = CARTESIAN_POINT ( 'NONE',  ( 9.175772138681999479, -4.424886761933599644, -6.440186012775000357 ) ) ;
#59790 = CARTESIAN_POINT ( 'NONE',  ( 24.35146665670700017, -3.377061749054000028, -12.26054704401999906 ) ) ;
#59791 = CARTESIAN_POINT ( 'NONE',  ( 8.268281802725203633, 3.021318042435896079, -6.294810243494267432 ) ) ;
#59792 = B_SPLINE_SURFACE_WITH_KNOTS ( 'NONE', 3, 3, ( 
 ( #12410, #60645, #12758, #34087 ),
 ( #28854, #2265, #44923, #20057 ),
 ( #35461, #8884, #47666, #68626 ),
 ( #25300, #14480, #52906, #41724 ),
 ( #63028, #46638, #41385, #9213 ) ),
 .UNSPECIFIED., .F., .F., .F.,
 ( 4, 1, 4 ),
 ( 4, 4 ),
 ( 0.5689291519175999623, 0.5833333333333000637, 0.5933409168203001016 ),
 ( -0.1884349902748000127, 1.188531000832999895 ),
 .UNSPECIFIED. ) ;
#59793 = CARTESIAN_POINT ( 'NONE',  ( 10.96949144726329806, 3.419793223320000131, -6.681274802424499448 ) ) ;
#59794 = CARTESIAN_POINT ( 'NONE',  ( 12.48372201234963086, -0.6448943924266594685, 12.58348668657566094 ) ) ;
#59795 = CARTESIAN_POINT ( 'NONE',  ( 11.51456785386839954, -4.946394603182100447, 6.863111178199799767 ) ) ;
#59796 = CARTESIAN_POINT ( 'NONE',  ( 8.662857780412000608, 2.741641653469999884, 6.457329666915000210 ) ) ;
#59797 = CARTESIAN_POINT ( 'NONE',  ( 9.595493858556999101, 3.928424745541000185, 5.531312048131000303 ) ) ;
#59798 = B_SPLINE_CURVE_WITH_KNOTS ( 'NONE', 3,
 ( #66583, #18701, #56096, #67601, #40034, #51203, #35132, #61346, #29896, #29556, #24633, #13466, #41050, #45953, #8207 ),
 .UNSPECIFIED., .F., .F.,
 ( 4, 2, 2, 2, 1, 2, 2, 4 ),
 ( 0.000000000000000000, 0.2500000000000130451, 0.3750000000000203726, 0.4375000000000243139, 0.4687500000000262568, 0.4843750000000273670, 0.5000000000000285327, 1.000000000000000000 ),
 .UNSPECIFIED. ) ;
#59799 = CARTESIAN_POINT ( 'NONE',  ( 12.74469048821893402, 1.763307075768890453, 12.47600695802491266 ) ) ;
#59800 = VERTEX_POINT ( 'NONE', #25633 ) ;
#59801 = CARTESIAN_POINT ( 'NONE',  ( 10.00975366370549757, 4.592545519478158589, -8.996633650733423693 ) ) ;
#59802 = CARTESIAN_POINT ( 'NONE',  ( 10.81764560330029923, 4.349570499512200428, -6.414140625063999401 ) ) ;
#59803 = CARTESIAN_POINT ( 'NONE',  ( 17.88638781139528788, -0.6398865404514794131, 12.58374251866278826 ) ) ;
#59804 = CARTESIAN_POINT ( 'NONE',  ( 11.16544712921906957, 3.267598948716616825, 7.017906594554381705 ) ) ;
#59806 = PLANE ( 'NONE',  #61948 ) ;
#59805 = CARTESIAN_POINT ( 'NONE',  ( 8.222961399606997901, 4.680050665548002087, 6.135920769709001021 ) ) ;
#59807 = CARTESIAN_POINT ( 'NONE',  ( 10.94903032197929882, -3.496160833528699996, -6.795411691360399686 ) ) ;
#59808 = CARTESIAN_POINT ( 'NONE',  ( 17.55505043854144276, 0.6250000000000001110, -25.00000000000000000 ) ) ;
#59809 = VERTEX_POINT ( 'NONE', #62681 ) ;
#59810 = CARTESIAN_POINT ( 'NONE',  ( 1.596338831776999978, -1.247131703260000002, -3.010971457459999723 ) ) ;
#59811 = CARTESIAN_POINT ( 'NONE',  ( 5.500000000000000000, 0.4800000000000000377, -1.889999999999999902 ) ) ;
#59812 = AXIS2_PLACEMENT_3D ( 'NONE', #32975, #43816, #49053 ) ;
#59813 = CARTESIAN_POINT ( 'NONE',  ( 12.08097595788930789, -12.02669421650221437, 3.498808775436077934 ) ) ;
#59814 = CARTESIAN_POINT ( 'NONE',  ( 11.09999999999999964, -3.512324525112999751, -8.971282648301999174 ) ) ;
#59815 = CARTESIAN_POINT ( 'NONE',  ( 12.21285350005642911, -2.096151405059779815, 13.84220188050174016 ) ) ;
#59816 = CARTESIAN_POINT ( 'NONE',  ( 10.95289953070000166, 2.845666449107000062, 5.174586383325000760 ) ) ;
#59817 = DIRECTION ( 'NONE',  ( 0.000000000000000000, 1.000000000000000000, 0.000000000000000000 ) ) ;
#59818 = CARTESIAN_POINT ( 'NONE',  ( 13.43019412026500170, -12.07125412582999857, -2.305633000807000066 ) ) ;
#59819 = VERTEX_POINT ( 'NONE', #46962 ) ;
#59820 = ADVANCED_FACE ( 'NONE', ( #19354 ), #14464, .F. ) ;
#59821 = ADVANCED_FACE ( 'NONE', ( #9197 ), #56419, .T. ) ;
#59822 = FACE_OUTER_BOUND ( 'NONE', #47393, .T. ) ;
#59823 = CARTESIAN_POINT ( 'NONE',  ( 11.09999999999999964, -2.899999999999999911, 4.467422426380999845 ) ) ;
#59824 = CARTESIAN_POINT ( 'NONE',  ( 7.100000000000000533, 0.000000000000000000, 0.000000000000000000 ) ) ;
#59825 = CARTESIAN_POINT ( 'NONE',  ( 0.9898832362503998672, 3.344697682836000219, -1.715043639744999959 ) ) ;
#59826 = CARTESIAN_POINT ( 'NONE',  ( 11.07102344389999971, -4.762665848028800220, 7.962849245488699879 ) ) ;
#59827 = CARTESIAN_POINT ( 'NONE',  ( 18.01444767332560204, 2.076107767824256989, -12.54031350746514129 ) ) ;
#59828 = FACE_OUTER_BOUND ( 'NONE', #52268, .T. ) ;
#59829 = CARTESIAN_POINT ( 'NONE',  ( 11.68748876160954886, 3.399618311400500303, 6.875627981711399883 ) ) ;
#59830 = CARTESIAN_POINT ( 'NONE',  ( 11.50002544571312058, -3.809924653178162313, 11.93174516965595622 ) ) ;
#59831 = CARTESIAN_POINT ( 'NONE',  ( 11.24323064679000161, -2.479730344050999680, -7.587230764681999418 ) ) ;
#59832 = FACE_OUTER_BOUND ( 'NONE', #16596, .T. ) ;
#59833 = CARTESIAN_POINT ( 'NONE',  ( 10.42499241036494162, 5.349775919985349404, 7.500001834605750872 ) ) ;
#59834 = CARTESIAN_POINT ( 'NONE',  ( 9.424850063658244181, 5.349972463430670899, 7.500009360578276052 ) ) ;
#59835 = ADVANCED_FACE ( 'NONE', ( #20385 ), #32920, .F. ) ;
#59836 = ORIENTED_EDGE ( 'NONE', *, *, #39245, .T. ) ;
#59837 = CARTESIAN_POINT ( 'NONE',  ( 7.436329166470820873, 2.279372969473476118, 7.816946968581012456 ) ) ;
#59838 = ORIENTED_EDGE ( 'NONE', *, *, #40642, .T. ) ;
#59839 = CARTESIAN_POINT ( 'NONE',  ( 17.71863970650579745, -3.103558472751648090, 13.52675378075879209 ) ) ;
#59840 = CARTESIAN_POINT ( 'NONE',  ( 10.29657053952199952, -4.502253688815499366, -6.324815923923999605 ) ) ;
#59841 = ORIENTED_EDGE ( 'NONE', *, *, #61424, .F. ) ;
#59842 = ADVANCED_FACE ( 'NONE', ( #40677 ), #37705, .F. ) ;
#59843 = CARTESIAN_POINT ( 'NONE',  ( 11.52166954483529793, 4.562096242626500597, 8.367285821793199574 ) ) ;
#59844 = CARTESIAN_POINT ( 'NONE',  ( 5.437476544805053713, -0.2480724261212651216, -1.105189088554211274 ) ) ;
#59845 = CARTESIAN_POINT ( 'NONE',  ( 4.149992563291999836, 4.286198015044692593E-16, -1.999973142472143861 ) ) ;
#59846 = CIRCLE ( 'NONE', #25214, 1.300133550998999743 ) ;
#59847 = CARTESIAN_POINT ( 'NONE',  ( 10.58844943056000076, 3.754657019866000311, 5.545350295858999523 ) ) ;
#59848 = CARTESIAN_POINT ( 'NONE',  ( 12.15646017001375512, -2.140061664339810932, -13.83614491991404272 ) ) ;
#59849 = CARTESIAN_POINT ( 'NONE',  ( 10.64393020684899938, -2.750000000000000000, 7.500000000000000000 ) ) ;
#59850 = CARTESIAN_POINT ( 'NONE',  ( 17.85445698522930869, 0.6551943188411784025, -12.58295456804123091 ) ) ;
#59851 = CARTESIAN_POINT ( 'NONE',  ( 10.31499432720999998, -5.458372854186999135, -8.355103994551999591 ) ) ;
#59852 = CARTESIAN_POINT ( 'NONE',  ( 11.02214804248266766, 5.404890988670800311, -8.010352125880700669 ) ) ;
#59853 = ORIENTED_EDGE ( 'NONE', *, *, #45924, .F. ) ;
#59854 = CARTESIAN_POINT ( 'NONE',  ( 5.555026506349999948, -1.500000000000000000, 0.000000000000000000 ) ) ;
#59855 = VERTEX_POINT ( 'NONE', #32602 ) ;
#59856 = CIRCLE ( 'NONE', #37539, 12.84999890301999947 ) ;
#59857 = CARTESIAN_POINT ( 'NONE',  ( 11.58810207955109917, 3.203462856645999945, 7.825000000000000178 ) ) ;
#59858 = SURFACE_STYLE_USAGE ( .BOTH. , #27020 ) ;
#59859 = ORIENTED_EDGE ( 'NONE', *, *, #55489, .F. ) ;
#59860 = CARTESIAN_POINT ( 'NONE',  ( 10.87208388895120770, 2.964986218627933212, -4.888821409244461513 ) ) ;
#59861 = CARTESIAN_POINT ( 'NONE',  ( 10.28117360717000039, -4.719545580892999581, 4.850090003780999304 ) ) ;
#59862 = CARTESIAN_POINT ( 'NONE',  ( 10.42760663304247615, 4.647051049978554005, 8.087719785218890678 ) ) ;
#59863 = CARTESIAN_POINT ( 'NONE',  ( 23.57774079265084310, 13.28347076428885565, -4.287252149520854871 ) ) ;
#59864 = CARTESIAN_POINT ( 'NONE',  ( 12.25689739436619341, 2.199570998105316200, 13.73255685804838500 ) ) ;
#59865 = CARTESIAN_POINT ( 'NONE',  ( 10.23808992278000041, -2.752437370156000540, 6.820045513931999537 ) ) ;
#59866 = B_SPLINE_CURVE_WITH_KNOTS ( 'NONE', 3,
 ( #39498, #60820, #22715, #45094, #18523, #55582, #6986, #7684, #44061, #6283, #49287, #32872, #49637, #29026, #17124, #1743, #54541, #27631, #1060, #11881 ),
 .UNSPECIFIED., .F., .F.,
 ( 4, 2, 2, 2, 2, 2, 2, 2, 2, 4 ),
 ( 0.000000000000000000, 0.1250000000000000555, 0.2500000000000001110, 0.3750000000000001665, 0.5000000000000002220, 0.6250000000000002220, 0.7500000000000003331, 0.8750000000000004441, 0.9375000000000002220, 1.000000000000000000 ),
 .UNSPECIFIED. ) ;
#59867 = DIRECTION ( 'NONE',  ( 0.000000000000000000, -0.2714570858282905341, 0.9624505444715651947 ) ) ;
#59868 = FACE_OUTER_BOUND ( 'NONE', #32455, .T. ) ;
#59869 = ORIENTED_EDGE ( 'NONE', *, *, #39665, .F. ) ;
#59870 = CARTESIAN_POINT ( 'NONE',  ( 7.586271682458000321, 5.321245676936000812, -7.068438969505000280 ) ) ;
#59871 = DIRECTION ( 'NONE',  ( -0.5000000000000150990, 0.08222066253632250021, -0.8621135439442261239 ) ) ;
#59872 = CARTESIAN_POINT ( 'NONE',  ( 9.353545867770625577, 4.858658389798049981, 7.331958223794097229 ) ) ;
#59873 = CARTESIAN_POINT ( 'NONE',  ( 4.328357053668000276, -0.7950496099306999520, -0.9874988013310997959 ) ) ;
#59874 = CARTESIAN_POINT ( 'NONE',  ( 9.178620280414001797, 2.990001567622999623, -8.695425648791999862 ) ) ;
#59875 = CARTESIAN_POINT ( 'NONE',  ( 5.599999772733800008, -6.661338147750999827E-14, 12.69999976912998108 ) ) ;
#59876 = CARTESIAN_POINT ( 'NONE',  ( 10.79839246847000034, -5.269358106415999110, -6.148714306659999629 ) ) ;
#59877 = PRODUCT_RELATED_PRODUCT_CATEGORY ( 'part', '', ( #56164 ) ) ;
#59878 = CARTESIAN_POINT ( 'NONE',  ( 9.099999999999999645, 0.000000000000000000, 0.000000000000000000 ) ) ;
#59879 = CARTESIAN_POINT ( 'NONE',  ( 10.52314899745999988, -5.167567567567999731, -6.822293592207000934 ) ) ;
#59880 = CARTESIAN_POINT ( 'NONE',  ( 4.451675502116665406, -0.4062801362093708679, 1.464321016255251795 ) ) ;
#59881 = CARTESIAN_POINT ( 'NONE',  ( 8.625788328778114078, -2.987667598876605712, -6.606157699978479236 ) ) ;
#59882 = DIRECTION ( 'NONE',  ( 0.9999999999999762412, 2.179566365501950425E-07, -9.624109672044771190E-10 ) ) ;
#59883 = CARTESIAN_POINT ( 'NONE',  ( 10.99999999997000089, -4.000000000000000000, -8.949999999965999820 ) ) ;
#59884 = CARTESIAN_POINT ( 'NONE',  ( 10.89835090130999973, 4.878966983716200190, -8.043647632228999811 ) ) ;
#59885 = CARTESIAN_POINT ( 'NONE',  ( 9.609329965421999020, 3.302375896175799852, -8.222608407156599242 ) ) ;
#59887 = FACE_BOUND ( 'NONE', #44396, .T. ) ;
#59886 = CARTESIAN_POINT ( 'NONE',  ( 10.48227973160899928, -3.922199073804859992, 8.363513150096299142 ) ) ;
#59888 = CARTESIAN_POINT ( 'NONE',  ( 11.34184687351628540, -4.999583552997724389, 8.268183399968647151 ) ) ;
#59889 = VERTEX_POINT ( 'NONE', #53916 ) ;
#59890 = CIRCLE ( 'NONE', #43173, 11.10000000000000675 ) ;
#59891 = B_SPLINE_CURVE_WITH_KNOTS ( 'NONE', 3,
 ( #51916, #46688, #62068, #67992 ),
 .UNSPECIFIED., .F., .F.,
 ( 4, 4 ),
 ( 0.000000000000000000, 1.000000000000000000 ),
 .UNSPECIFIED. ) ;
#59892 = CARTESIAN_POINT ( 'NONE',  ( 10.60746886766490071, 3.501664543805500074, 8.405426684175299812 ) ) ;
#59893 = AXIS2_PLACEMENT_3D ( 'NONE', #48169, #21588, #31408 ) ;
#59894 = CARTESIAN_POINT ( 'NONE',  ( 11.14698053895999941, -5.129799765052999838, 5.886044098803999702 ) ) ;
#59895 = CARTESIAN_POINT ( 'NONE',  ( 9.355088727410999283, 2.725263018055000153, 7.393088754863899936 ) ) ;
#59896 = CARTESIAN_POINT ( 'NONE',  ( 10.78976354018297634, -4.327184855449096368, -6.282534154164603812 ) ) ;
#59897 = CARTESIAN_POINT ( 'NONE',  ( 10.65550933554000146, -4.237674644795000667, 9.105223721671999115 ) ) ;
#59898 = CARTESIAN_POINT ( 'NONE',  ( 9.645238140867222754, -5.359248881483462235, 6.398502314407720881 ) ) ;
#59899 = CARTESIAN_POINT ( 'NONE',  ( 11.80561165699200110, 3.526771526455999783, -11.96112153682000034 ) ) ;
#59900 = ADVANCED_FACE ( 'NONE', ( #6017 ), #783, .F. ) ;
#59901 = EDGE_CURVE ( 'NONE', #33691, #51514, #26678, .T. ) ;
#59902 = CARTESIAN_POINT ( 'NONE',  ( 9.026759580228999269, -4.976892840331100132, -7.266499081715599218 ) ) ;
#59903 = VECTOR ( 'NONE', #37707, 1000.000000000000114 ) ;
#59904 = CARTESIAN_POINT ( 'NONE',  ( 11.09999999999999964, 2.649999999999999911, -7.500000000000000000 ) ) ;
#59905 = CARTESIAN_POINT ( 'NONE',  ( 5.577289226418999490, 0.8392109641639000639, 1.021861505418000027 ) ) ;
#59906 = CARTESIAN_POINT ( 'NONE',  ( 10.95046608577698066, -2.858708611104648245, -5.102140212562284560 ) ) ;
#59907 = CARTESIAN_POINT ( 'NONE',  ( 24.41456973790700147, -3.182129207855000086, 12.02370739584000070 ) ) ;
#59908 = CARTESIAN_POINT ( 'NONE',  ( 13.50018479229797030, -11.10053973472247790, -4.255642710877533652 ) ) ;
#59909 = CARTESIAN_POINT ( 'NONE',  ( 11.46595122972049907, 4.343798595649099425, -6.704952129760900270 ) ) ;
#59910 = CARTESIAN_POINT ( 'NONE',  ( 12.48799821678961308, 1.955167389914997722, -13.77408040568415615 ) ) ;
#59911 = CARTESIAN_POINT ( 'NONE',  ( 5.500000000000000000, 0.000000000000000000, 0.000000000000000000 ) ) ;
#59912 = CARTESIAN_POINT ( 'NONE',  ( 12.61551017423881405, 3.176304576345524211, 12.19307927065969999 ) ) ;
#59913 = ORIENTED_EDGE ( 'NONE', *, *, #53656, .F. ) ;
#59914 = CARTESIAN_POINT ( 'NONE',  ( 7.704343083128708969, -2.684466035400899120, 7.853284348082095079 ) ) ;
#59915 = CARTESIAN_POINT ( 'NONE',  ( 12.17676779642099660, -0.3651687365794661910, -13.99525266148724256 ) ) ;
#59916 = LINE ( 'NONE', #23549, #29877 ) ;
#59917 = CARTESIAN_POINT ( 'NONE',  ( 25.48313369564800368, -8.422746779740000633, -7.953667242360999978 ) ) ;
#59918 = CARTESIAN_POINT ( 'NONE',  ( 3.500000000000000000, -2.069127319938742993, 2.446168983457449819 ) ) ;
#59919 = CARTESIAN_POINT ( 'NONE',  ( 6.999999999999999112, 8.786168856256553639, 4.620315609150635439 ) ) ;
#59920 = CARTESIAN_POINT ( 'NONE',  ( 13.43043922992600159, 12.41458792447999926, 1.928118222792999825 ) ) ;
#59921 = ORIENTED_EDGE ( 'NONE', *, *, #25663, .T. ) ;
#59922 = DIRECTION ( 'NONE',  ( 1.000000000000000000, 0.000000000000000000, 0.000000000000000000 ) ) ;
#59923 = CARTESIAN_POINT ( 'NONE',  ( 17.67504841906447055, 3.238437383711908701, -13.62029908313572157 ) ) ;
#59924 = ORIENTED_EDGE ( 'NONE', *, *, #67293, .T. ) ;
#59925 = EDGE_CURVE ( 'NONE', #22688, #5733, #39395, .T. ) ;
#59926 = CARTESIAN_POINT ( 'NONE',  ( 21.10000000000000142, 11.84999999999999964, 0.000000000000000000 ) ) ;
#59927 = CARTESIAN_POINT ( 'NONE',  ( 25.26126739128486065, 8.521553289640936057, -7.991940988076141394 ) ) ;
#59928 = CARTESIAN_POINT ( 'NONE',  ( 8.871889158775999817, 2.702406276695999754, -6.981052078638000147 ) ) ;
#59929 = CARTESIAN_POINT ( 'NONE',  ( 5.500000000000000000, 11.00717859340000082, 1.432487142323000118 ) ) ;
#59930 = CARTESIAN_POINT ( 'NONE',  ( 11.38678751119029897, -5.166297436425000278, -8.110172976325500827 ) ) ;
#59931 = CARTESIAN_POINT ( 'NONE',  ( 7.365035841224999658, 5.899473592675000155, -7.539390303202999633 ) ) ;
#59932 = CARTESIAN_POINT ( 'NONE',  ( 8.660633043440231660, 4.489919511865821278, -8.784469522291857402 ) ) ;
#59933 = CARTESIAN_POINT ( 'NONE',  ( 10.19601354018233330, -3.000416447002272058, 8.268183399968641822 ) ) ;
#59934 = VERTEX_POINT ( 'NONE', #4990 ) ;
#59935 = CARTESIAN_POINT ( 'NONE',  ( 10.56492304196000021, -4.212244324161999565, 8.933470634735002136 ) ) ;
#59936 = CARTESIAN_POINT ( 'NONE',  ( 10.90000000000000036, 5.100000000000000533, -6.436740704805999691 ) ) ;
#59937 = CARTESIAN_POINT ( 'NONE',  ( 25.50731759324898107, 8.309739206314244342, -8.116424455511989322 ) ) ;
#59938 = VERTEX_POINT ( 'NONE', #63364 ) ;
#59939 = TOROIDAL_SURFACE ( 'NONE', #29829, 13.79999999999999893, 0.2000000000000000111 ) ;
#59940 = CARTESIAN_POINT ( 'NONE',  ( 11.35399482404720040, -3.445326802703576163, 11.33548354870907282 ) ) ;
#59941 = CARTESIAN_POINT ( 'NONE',  ( 11.10664194037999941, -5.324199331986000594, -7.809344861333999965 ) ) ;
#59942 = ORIENTED_EDGE ( 'NONE', *, *, #6691, .T. ) ;
#59943 = CARTESIAN_POINT ( 'NONE',  ( 9.609329965421999020, 3.302375896175799852, 6.777391592843399870 ) ) ;
#59944 = CARTESIAN_POINT ( 'NONE',  ( 18.24314268136838990, -2.253095180823014854, -12.39692251310592574 ) ) ;
#59945 = CARTESIAN_POINT ( 'NONE',  ( 4.511183905521000348, -1.322317977380999876, -0.5078386052281999019 ) ) ;
#59946 = CIRCLE ( 'NONE', #65476, 2.524999655449999825 ) ;
#59947 = CARTESIAN_POINT ( 'NONE',  ( 7.740705559937997471, 4.511742753184996957, -6.425237059776996773 ) ) ;
#59948 = CARTESIAN_POINT ( 'NONE',  ( 16.04506009312500225, 3.874776422117000241, 11.85383417895000058 ) ) ;
#59949 = CARTESIAN_POINT ( 'NONE',  ( 23.60205915885299888, 2.171992490544001786, 12.06370038613001228 ) ) ;
#59950 = VECTOR ( 'NONE', #50460, 1000.000000000000000 ) ;
#59951 = CARTESIAN_POINT ( 'NONE',  ( 10.06525461470299909, 3.026595211686900377, 7.252360304610999897 ) ) ;
#59952 = CARTESIAN_POINT ( 'NONE',  ( 8.222954734881996686, -4.680061443183004322, 6.135926641887999189 ) ) ;
#59953 = VERTEX_POINT ( 'NONE', #15492 ) ;
#59954 = CARTESIAN_POINT ( 'NONE',  ( 10.46754281781999829, 2.318340407652000223, 6.549777679168999001 ) ) ;
#59955 = CARTESIAN_POINT ( 'NONE',  ( 10.29667028040999988, 2.755514216060999999, -6.622437150225000124 ) ) ;
#59956 = CARTESIAN_POINT ( 'NONE',  ( 13.43777338887524486, 12.12041883920677243, 2.246947635350981631 ) ) ;
#59957 = CARTESIAN_POINT ( 'NONE',  ( 12.18763606713061520, 2.400822034753086864, -13.69401148367744092 ) ) ;
#59958 = CARTESIAN_POINT ( 'NONE',  ( 9.988317406969001055, -3.762080884004200154, -8.756892549790999070 ) ) ;
#59959 = CARTESIAN_POINT ( 'NONE',  ( 25.18909985880100066, 2.894851937781000029, 11.44762852350000060 ) ) ;
#59960 = CARTESIAN_POINT ( 'NONE',  ( 18.24552752486709650, -0.2229649748661350905, 13.99822903660538564 ) ) ;
#59961 = CARTESIAN_POINT ( 'NONE',  ( 7.716851002542999716, -2.832432432432000269, 6.822293592207000934 ) ) ;
#59962 = EDGE_CURVE ( 'NONE', #53841, #62127, #40700, .T. ) ;
#59963 = EDGE_CURVE ( 'NONE', #38087, #64166, #42406, .T. ) ;
#59964 = VERTEX_POINT ( 'NONE', #44491 ) ;
#59965 = ORIENTED_EDGE ( 'NONE', *, *, #27709, .T. ) ;
#59966 = VECTOR ( 'NONE', #14121, 1000.000000000000000 ) ;
#59967 = CARTESIAN_POINT ( 'NONE',  ( 9.793039158772000263, 5.817107086401000160, -6.945352709928000579 ) ) ;
#59968 = CARTESIAN_POINT ( 'NONE',  ( 12.29893553472659029, -0.3669576693511948928, 13.89348614079305655 ) ) ;
#59969 = CARTESIAN_POINT ( 'NONE',  ( 12.76431812847650704, -0.6240106079411803508, -13.88114051191588594 ) ) ;
#59970 = CARTESIAN_POINT ( 'NONE',  ( 7.298591271593769747, -3.170842933427397536, 6.420501794657867300 ) ) ;
#59971 = CARTESIAN_POINT ( 'NONE',  ( 10.96985955311839867, 2.886498072322427166, -4.936516855179674756 ) ) ;
#59972 = CARTESIAN_POINT ( 'NONE',  ( 8.989144353209001181, -5.284133759825000887, 6.489273023403000273 ) ) ;
#59973 = CARTESIAN_POINT ( 'NONE',  ( 11.57907162307749971, -4.814611760850799449, 7.825000000000000178 ) ) ;
#59975 = CARTESIAN_POINT ( 'NONE',  ( 10.96239488738000034, -6.767643977940999811, 5.462428178478999641 ) ) ;
#59974 = CARTESIAN_POINT ( 'NONE',  ( 10.38700081824000065, -5.131870447930000800, 6.903968392969799694 ) ) ;
#59976 = CARTESIAN_POINT ( 'NONE',  ( 9.203545614489009097, -5.098876553266001643, -6.624379381313996618 ) ) ;
#59977 = FACE_OUTER_BOUND ( 'NONE', #67264, .T. ) ;
#59978 = CARTESIAN_POINT ( 'NONE',  ( 23.58017449365151208, 10.23400074257411063, -9.531361764565000172 ) ) ;
#59979 = CARTESIAN_POINT ( 'NONE',  ( 17.69686089611048985, -0.6090396975623083575, 12.68033511803395363 ) ) ;
#59980 = CARTESIAN_POINT ( 'NONE',  ( 6.736914452361000727, 0.2494103027241000026, -1.534615152291000095 ) ) ;
#59981 = CARTESIAN_POINT ( 'NONE',  ( 17.99291067209890826, -2.946084426705714687, -12.33636513593941508 ) ) ;
#59982 = ORIENTED_EDGE ( 'NONE', *, *, #53763, .T. ) ;
#59984 = DIRECTION ( 'NONE',  ( -0.7071067811864923947, -0.6115518252005933686, -0.3549709355621961659 ) ) ;
#59983 = CARTESIAN_POINT ( 'NONE',  ( 8.417495559623999313, -2.029110377978999846, 7.726994002375999315 ) ) ;
#59985 = CARTESIAN_POINT ( 'NONE',  ( 9.988985841228000595, 3.986577607995999806, -9.280166295424001177 ) ) ;
#59986 = EDGE_CURVE ( 'NONE', #11316, #3245, #40268, .T. ) ;
#59987 = DIRECTION ( 'NONE',  ( 1.000000000000000000, 0.000000000000000000, 0.000000000000000000 ) ) ;
#59988 = CARTESIAN_POINT ( 'NONE',  ( 23.60205915885299888, 9.361474752760003071, -7.912850866705011477 ) ) ;
#59989 = VECTOR ( 'NONE', #17255, 1000.000000000000000 ) ;
#59990 = EDGE_CURVE ( 'NONE', #21830, #56890, #10166, .T. ) ;
#59991 = CARTESIAN_POINT ( 'NONE',  ( 13.49980696792483137, -10.14812545701395585, -7.065329385613733137 ) ) ;
#59992 = COLOUR_RGB ( '', 0.31764706, 0.68627451, 0.89019608) ;
#59993 = CARTESIAN_POINT ( 'NONE',  ( 8.193905507992999659, 3.399974105831999882, 6.145257027059000343 ) ) ;
#59994 = CARTESIAN_POINT ( 'NONE',  ( 2.452246804060000507, -1.767275544862999981, -3.127392849687999909 ) ) ;
#59995 = VERTEX_POINT ( 'NONE', #7405 ) ;
#59996 = CARTESIAN_POINT ( 'NONE',  ( 12.27567264278500048, -0.4920215530101137436, -12.59040071882420264 ) ) ;
#59997 = CARTESIAN_POINT ( 'NONE',  ( 6.999999691988000095, 12.11716380430000051, -3.069905306952000146 ) ) ;
#59998 = CARTESIAN_POINT ( 'NONE',  ( 18.01279894578400942, 3.038334268486855283, -12.22818629355008468 ) ) ;
#59999 = CARTESIAN_POINT ( 'NONE',  ( 11.09999999999999964, -2.700000000000000178, -6.461133846875999787 ) ) ;
#60000 = CARTESIAN_POINT ( 'NONE',  ( 8.694607780412001219, 5.290207928847999064, 8.768105151414001597 ) ) ;
#60001 = ORIENTED_EDGE ( 'NONE', *, *, #6486, .F. ) ;
#60002 = CARTESIAN_POINT ( 'NONE',  ( 6.637459438551000623, -0.9243234316805000184, -1.323994513613999890 ) ) ;
#60003 = CARTESIAN_POINT ( 'NONE',  ( 7.558029719586000006, 3.447598131391000020, -9.141997724497999300 ) ) ;
#60005 = CARTESIAN_POINT ( 'NONE',  ( 10.83658792121999959, 5.133186143592999962, 8.848368005200001107 ) ) ;
#60004 = CARTESIAN_POINT ( 'NONE',  ( 8.590676109800844173, -4.354029080878516034, 5.795624387936125110 ) ) ;
#60006 = VECTOR ( 'NONE', #55457, 1000.000000000000000 ) ;
#60007 = CARTESIAN_POINT ( 'NONE',  ( 11.63611496860034933, 5.171412538012999605, -6.899705789500199415 ) ) ;
#60008 = ORIENTED_EDGE ( 'NONE', *, *, #33084, .F. ) ;
#60009 = DIRECTION ( 'NONE',  ( -1.000000000000000000, 0.000000000000000000, 0.000000000000000000 ) ) ;
#60010 = CARTESIAN_POINT ( 'NONE',  ( 14.80000000000000071, -3.283787102340999464, 11.28049554847999936 ) ) ;
#60011 = ORIENTED_EDGE ( 'NONE', *, *, #12818, .T. ) ;
#60012 = EDGE_CURVE ( 'NONE', #20309, #64166, #44829, .T. ) ;
#60013 = CARTESIAN_POINT ( 'NONE',  ( 12.61298032294660310, 3.180483649502660271, -12.19204447434304051 ) ) ;
#60014 = CARTESIAN_POINT ( 'NONE',  ( 16.15961700471899931, 3.514971253533999640, 11.06754630474000045 ) ) ;
#60015 = CARTESIAN_POINT ( 'NONE',  ( 17.96724268330523344, -0.4699225802676937902, -13.88930950616751225 ) ) ;
#60016 = ORIENTED_EDGE ( 'NONE', *, *, #46287, .T. ) ;
#60017 = CARTESIAN_POINT ( 'NONE',  ( 24.30001694968100168, 3.271769180623000040, -12.21048179117000032 ) ) ;
#60018 = CARTESIAN_POINT ( 'NONE',  ( 8.099999999999999645, 0.000000000000000000, -11.84999999999999964 ) ) ;
#60019 = AXIS2_PLACEMENT_3D ( 'NONE', #46418, #51653, #56219 ) ;
#60020 = CARTESIAN_POINT ( 'NONE',  ( 10.65413259636999932, 3.216622244594500302, -7.926858177843299380 ) ) ;
#60021 = CARTESIAN_POINT ( 'NONE',  ( 8.745593092018999926, -5.100000000000000533, 6.404090157675000228 ) ) ;
#60022 = CARTESIAN_POINT ( 'NONE',  ( 5.302805487806614870, -0.3471608085200784677, 1.190492330534066445 ) ) ;
#60023 = ORIENTED_EDGE ( 'NONE', *, *, #19425, .F. ) ;
#60024 = CARTESIAN_POINT ( 'NONE',  ( 8.770176658772999900, 3.049618631524000367, 6.392542946894000266 ) ) ;
#60025 = CARTESIAN_POINT ( 'NONE',  ( 23.55757948181399897, -13.49847953779999976, -4.022400660198999667 ) ) ;
#60026 = CARTESIAN_POINT ( 'NONE',  ( 9.948096873516666605, -4.327184855449103473, 6.282534154164604701 ) ) ;
#60027 = DIRECTION ( 'NONE',  ( -1.000000000000000000, 0.000000000000000000, 0.000000000000000000 ) ) ;
#60028 = B_SPLINE_CURVE_WITH_KNOTS ( 'NONE', 3,
 ( #41077, #46327, #68314, #62729 ),
 .UNSPECIFIED., .F., .F.,
 ( 4, 4 ),
 ( 0.000000000000000000, 0.1070776897655759813 ),
 .UNSPECIFIED. ) ;
#60029 = VERTEX_POINT ( 'NONE', #12311 ) ;
#60030 = CARTESIAN_POINT ( 'NONE',  ( 12.21847001913372388, -2.284010606415768585, -12.49926433191011732 ) ) ;
#60031 = CARTESIAN_POINT ( 'NONE',  ( 0.4464730966431282311, -0.4520039235917613363, -3.446451393816258868 ) ) ;
#60032 = CARTESIAN_POINT ( 'NONE',  ( 8.375950119029546670, 5.618014493828255240, -8.286326870345469331 ) ) ;
#60033 = CARTESIAN_POINT ( 'NONE',  ( 9.123929153134385572, 5.099761357576720222, 6.165062780802453624 ) ) ;
#60034 = CARTESIAN_POINT ( 'NONE',  ( 6.825988380485000562, -9.284830207118000445, 5.366267983674999797 ) ) ;
#60035 = CARTESIAN_POINT ( 'NONE',  ( 10.57564694612699974, -4.931992688388300294, -7.871941502982999772 ) ) ;
#60036 = CARTESIAN_POINT ( 'NONE',  ( 11.12299956498149811, 5.207010770456999893, -7.825000000000000178 ) ) ;
#60037 = VECTOR ( 'NONE', #32096, 1000.000000000000000 ) ;
#60038 = CARTESIAN_POINT ( 'NONE',  ( 17.55505043854147118, -1.760845406083394682, 12.47635457398815184 ) ) ;
#60039 = EDGE_LOOP ( 'NONE', ( #33482, #30023 ) ) ;
#60040 = CARTESIAN_POINT ( 'NONE',  ( 11.05435090131019926, -2.880552878538999995, -8.192386390235398608 ) ) ;
#60041 = VERTEX_POINT ( 'NONE', #28398 ) ;
#60042 = B_SPLINE_CURVE_WITH_KNOTS ( 'NONE', 3,
 ( #9924, #20760, #37183, #10608, #47336, #26705, #42090, #14832, #47683, #62377, #68994, #57464, #15170, #10266, #46652, #9227, #14494, #30566 ),
 .UNSPECIFIED., .F., .F.,
 ( 4, 2, 2, 2, 2, 2, 2, 2, 4 ),
 ( 0.000000000000000000, 0.1250000000000000278, 0.2500000000000000000, 0.3749999999999999445, 0.4999999999999999445, 0.6249999999999998890, 0.7499999999999998890, 0.8750000000000000000, 1.000000000000000000 ),
 .UNSPECIFIED. ) ;
#60043 = VECTOR ( 'NONE', #31901, 1000.000000000000000 ) ;
#60044 = CARTESIAN_POINT ( 'NONE',  ( 25.30000327618300204, -6.604245036507551141E-15, -11.49994408209238017 ) ) ;
#60045 = CARTESIAN_POINT ( 'NONE',  ( 9.237204719595000668, 3.071719032003000116, -6.037263251225000182 ) ) ;
#60046 = CARTESIAN_POINT ( 'NONE',  ( 2.461241760148999980, 0.2941929363790999896, 3.366553971799000067 ) ) ;
#60047 = CARTESIAN_POINT ( 'NONE',  ( 10.09454055528000005, -5.362855569781999954, -7.550030734599999960 ) ) ;
#60048 = AXIS2_PLACEMENT_3D ( 'NONE', #58606, #69098, #26808 ) ;
#60049 = CARTESIAN_POINT ( 'NONE',  ( 24.30001683570900184, 3.271769286791000209, 12.21048169671000139 ) ) ;
#60050 = CARTESIAN_POINT ( 'NONE',  ( 7.802644552000999489, 3.157760251094000825, -6.317964942532003469 ) ) ;
#60051 = EDGE_CURVE ( 'NONE', #438, #50410, #49023, .T. ) ;
#60053 = EDGE_CURVE ( 'NONE', #57674, #58925, #4967, .T. ) ;
#60052 = CARTESIAN_POINT ( 'NONE',  ( 11.46550210169813511, 3.941925478257526372, 6.192987292895718809 ) ) ;
#60054 = ORIENTED_EDGE ( 'NONE', *, *, #38115, .T. ) ;
#60055 = AXIS2_PLACEMENT_3D ( 'NONE', #24376, #57209, #57554 ) ;
#60056 = FACE_OUTER_BOUND ( 'NONE', #45327, .T. ) ;
#60057 = EDGE_CURVE ( 'NONE', #44042, #61329, #8557, .T. ) ;
#60058 = CARTESIAN_POINT ( 'NONE',  ( 11.12487750876920067, -4.543557328885200697, 6.656497609330299881 ) ) ;
#60059 = CARTESIAN_POINT ( 'NONE',  ( 10.80815748598999981, 2.937526572573000205, 8.948458885032000154 ) ) ;
#60060 = CARTESIAN_POINT ( 'NONE',  ( 5.500000000000000000, 0.8000000000000000444, -3.149999999999999911 ) ) ;
#60061 = CARTESIAN_POINT ( 'NONE',  ( 12.80505043854144276, -0.6878608935795413881, -12.61273126665598454 ) ) ;
#60062 = CARTESIAN_POINT ( 'NONE',  ( 17.79319863334400154, 3.315493116453000155, -11.22361396466000016 ) ) ;
#60063 = CIRCLE ( 'NONE', #62307, 0.7499999936418002555 ) ;
#60064 = CARTESIAN_POINT ( 'NONE',  ( 11.46179707368349909, 3.501542828836900156, -6.629085939160999530 ) ) ;
#60065 = CARTESIAN_POINT ( 'NONE',  ( 10.97843137008999825, 5.235400103863000254, 6.782920672145000829 ) ) ;
#60066 = B_SPLINE_CURVE_WITH_KNOTS ( 'NONE', 3,
 ( #57083, #42042, #46945, #26308 ),
 .UNSPECIFIED., .F., .F.,
 ( 4, 4 ),
 ( 0.000000000000000000, 1.000000000000000000 ),
 .UNSPECIFIED. ) ;
#60067 = CARTESIAN_POINT ( 'NONE',  ( 10.03696314287999947, 5.117257953482000410, -7.264481182560499128 ) ) ;
#60068 = CARTESIAN_POINT ( 'NONE',  ( 23.58444971190600015, -10.35811008870000016, -9.328007211334000459 ) ) ;
#60069 = CARTESIAN_POINT ( 'NONE',  ( 8.179999999999999716, 4.924138593003999809, -8.484107647018999998 ) ) ;
#60070 = VECTOR ( 'NONE', #18572, 1000.000000000000114 ) ;
#60071 = CARTESIAN_POINT ( 'NONE',  ( 24.66708179685902991, 3.571422468837009756, -12.15221134863278962 ) ) ;
#60072 = EDGE_LOOP ( 'NONE', ( #59723, #40518, #44642, #32152 ) ) ;
#60073 = CARTESIAN_POINT ( 'NONE',  ( 8.566230646795000681, -5.212258818969000451, 6.157189191035000064 ) ) ;
#60074 = CARTESIAN_POINT ( 'NONE',  ( 9.705151033051999221, -4.316974633926000671, -5.653758079558000027 ) ) ;
#60075 = CARTESIAN_POINT ( 'NONE',  ( 18.12600850643434569, 2.245563876552335358, 13.72409254399188150 ) ) ;
#60076 = LINE ( 'NONE', #18119, #17786 ) ;
#60077 = CARTESIAN_POINT ( 'NONE',  ( 11.50271932425157040, -4.187398418774900044, -8.764198628556998827 ) ) ;
#60078 = ORIENTED_EDGE ( 'NONE', *, *, #14410, .T. ) ;
#60079 = CARTESIAN_POINT ( 'NONE',  ( 10.56498513754060653, -5.349957030113857925, -7.500000808964294663 ) ) ;
#60080 = CARTESIAN_POINT ( 'NONE',  ( 8.822982780412001347, 2.678331728353000152, 8.735281589464001684 ) ) ;
#60082 = DIRECTION ( 'NONE',  ( 0.000000000000000000, -0.007439385635786961021, -0.9999723273877941798 ) ) ;
#60081 = CARTESIAN_POINT ( 'NONE',  ( 9.640910841231999484, 2.212639797530000063, -6.855876382544999537 ) ) ;
#60083 = CARTESIAN_POINT ( 'NONE',  ( 2.478117972721348927, -2.680622207154140568, 1.851572140801842625 ) ) ;
#60084 = ORIENTED_EDGE ( 'NONE', *, *, #35139, .T. ) ;
#60085 = CARTESIAN_POINT ( 'NONE',  ( 9.465106464520001595, 2.290037071913000322, 6.601704384062999864 ) ) ;
#60086 = CARTESIAN_POINT ( 'NONE',  ( 18.21732822554151809, -2.220719680094997095, -13.82275391900495798 ) ) ;
#60087 = CARTESIAN_POINT ( 'NONE',  ( 11.33872066707849768, 4.858611803369300652, 8.019361746728900897 ) ) ;
#60088 = CARTESIAN_POINT ( 'NONE',  ( 9.687876499438001332, -5.912252057206999645, 7.772299417761000306 ) ) ;
#60089 = CARTESIAN_POINT ( 'NONE',  ( 7.640464943433003420, 3.216280862983999622, 6.362631827276998386 ) ) ;
#60090 = ORIENTED_EDGE ( 'NONE', *, *, #61873, .F. ) ;
#60091 = CARTESIAN_POINT ( 'NONE',  ( 8.350412160844999931, 2.899104497346000286, -6.601769487399000269 ) ) ;
#60093 = CARTESIAN_POINT ( 'NONE',  ( 11.15264435320999858, -2.317067032475999877, -7.596564138533999255 ) ) ;
#60092 = FACE_OUTER_BOUND ( 'NONE', #48486, .T. ) ;
#60094 = CARTESIAN_POINT ( 'NONE',  ( 7.685231687083611263, -5.714952426232358107, 7.177445099263493056 ) ) ;
#60095 = CARTESIAN_POINT ( 'NONE',  ( 9.256662271119999730, -4.025830307267999508, 9.295859242339000517 ) ) ;
#60096 = CARTESIAN_POINT ( 'NONE',  ( 11.80233327354039830, -5.101536739857000846, -6.779499720266399798 ) ) ;
#60097 = CARTESIAN_POINT ( 'NONE',  ( 10.18330484851600026, -2.961576783819000358, 7.025224608805800131 ) ) ;
#60098 = ORIENTED_EDGE ( 'NONE', *, *, #4156, .T. ) ;
#60099 = CARTESIAN_POINT ( 'NONE',  ( 23.95415685822884200, -9.440317297343241876, 9.313970111589597423 ) ) ;
#60100 = CARTESIAN_POINT ( 'NONE',  ( 11.51041369783139956, -4.064477673403060543, 6.223614866029000048 ) ) ;
#60101 = VERTEX_POINT ( 'NONE', #27706 ) ;
#60102 = EDGE_CURVE ( 'NONE', #37807, #14642, #63518, .T. ) ;
#60103 = CARTESIAN_POINT ( 'NONE',  ( 18.20180239426969138, 2.898381337229589683, 13.69738341128404002 ) ) ;
#60104 = ORIENTED_EDGE ( 'NONE', *, *, #37727, .F. ) ;
#60105 = CARTESIAN_POINT ( 'NONE',  ( 8.142589158771000868, 5.074768364528000397, -8.296267706722000312 ) ) ;
#60106 = ADVANCED_FACE ( 'NONE', ( #23490 ), #37137, .F. ) ;
#60107 = VECTOR ( 'NONE', #15694, 1000.000000000000114 ) ;
#60108 = CARTESIAN_POINT ( 'NONE',  ( 23.61357239562000032, 13.29063276735999999, -4.053366244155999887 ) ) ;
#60109 = CARTESIAN_POINT ( 'NONE',  ( 12.56948062052969206, 3.161141996800560516, -12.19701735778311935 ) ) ;
#60110 = CARTESIAN_POINT ( 'NONE',  ( 12.10477869730532774, -4.467447516829900600, 8.421761806503198500 ) ) ;
#60111 = CARTESIAN_POINT ( 'NONE',  ( 7.988487219432808040, 5.103181190368189846, -6.649650124670951179 ) ) ;
#60112 = LINE ( 'NONE', #29264, #11526 ) ;
#60113 = ORIENTED_EDGE ( 'NONE', *, *, #73, .F. ) ;
#60114 = CARTESIAN_POINT ( 'NONE',  ( 23.56666365135700403, 11.16210620494999439, 3.571147222960000533 ) ) ;
#60115 = CARTESIAN_POINT ( 'NONE',  ( 23.59999192078999997, 10.30759737717999869, 9.317725909430999209 ) ) ;
#60116 = EDGE_LOOP ( 'NONE', ( #22829, #20238, #37680, #32506 ) ) ;
#60117 = PLANE ( 'NONE',  #14903 ) ;
#60118 = CARTESIAN_POINT ( 'NONE',  ( 10.81764560330029923, 4.349570499512200428, 8.585859374935999710 ) ) ;
#60119 = CARTESIAN_POINT ( 'NONE',  ( 23.56666365135700403, 2.963314674619003330, -12.23574966049000423 ) ) ;
#60120 = CARTESIAN_POINT ( 'NONE',  ( 10.85939066780000140, 2.936977800747000433, -5.180095930491999567 ) ) ;
#60121 = VECTOR ( 'NONE', #54344, 1000.000000000000000 ) ;
#60122 = CARTESIAN_POINT ( 'NONE',  ( 7.690241772926001751, 4.592291064388997590, 6.438923047733998928 ) ) ;
#60123 = CARTESIAN_POINT ( 'NONE',  ( 7.996487690580287300, -5.313957503663140791, 7.853744048643361175 ) ) ;
#60124 = CARTESIAN_POINT ( 'NONE',  ( 12.18524896721729966, -2.583003884521777760, -13.65547336762760544 ) ) ;
#60125 = CARTESIAN_POINT ( 'NONE',  ( 18.14682445378390341, 0.2013262877421451713, -12.69785743964336078 ) ) ;
#60126 = CARTESIAN_POINT ( 'NONE',  ( 12.19004578040465070, 2.611920287575038024, -12.42482035883542046 ) ) ;
#60127 = CARTESIAN_POINT ( 'NONE',  ( 11.62579573085663043, -2.760622544769000264, -7.714452430741599365 ) ) ;
#60128 = CARTESIAN_POINT ( 'NONE',  ( 9.316114158771000575, 3.677414437776999723, 9.250745771096999803 ) ) ;
#60129 = EDGE_LOOP ( 'NONE', ( #31841, #21164, #65682, #24834 ) ) ;
#60130 = CARTESIAN_POINT ( 'NONE',  ( 11.59999999999999964, -2.935681553670999921, -8.155535082817699788 ) ) ;
#60131 = CARTESIAN_POINT ( 'NONE',  ( 11.09999999999999964, -2.649999999999999911, 7.500000000000000000 ) ) ;
#60132 = CARTESIAN_POINT ( 'NONE',  ( 11.83966971788800215, 12.22235437154000159, 1.953272420501999784 ) ) ;
#60133 = CARTESIAN_POINT ( 'NONE',  ( 10.52662718686000076, 4.933722097448000277, -6.506013113666999637 ) ) ;
#60134 = CARTESIAN_POINT ( 'NONE',  ( 18.13206058706447621, 2.916601882134809642, 12.25780480496326241 ) ) ;
#60135 = CARTESIAN_POINT ( 'NONE',  ( 18.53682820967700451, 2.877067450793000081, -12.22924281482000097 ) ) ;
#60137 = ADVANCED_FACE ( 'NONE', ( #13281 ), #29021, .T. ) ;
#60136 = CARTESIAN_POINT ( 'NONE',  ( 9.471374412057000924, 2.030666183831999927, 7.549764512038000142 ) ) ;
#60138 = CARTESIAN_POINT ( 'NONE',  ( 10.36012881141662767, -3.130392736003965393, 7.403483289911290122 ) ) ;
#60139 = ADVANCED_FACE ( 'NONE', ( #24100 ), #52987, .F. ) ;
#60140 = CARTESIAN_POINT ( 'NONE',  ( 10.90000000000000036, -1.433333333332999837, -10.65401593558000037 ) ) ;
#60141 = EDGE_CURVE ( 'NONE', #51331, #21554, #20219, .T. ) ;
#60142 = ORIENTED_EDGE ( 'NONE', *, *, #37057, .F. ) ;
#60143 = CARTESIAN_POINT ( 'NONE',  ( 12.09872039853184589, -2.644866564252636554, 12.31930286224045368 ) ) ;
#60144 = CARTESIAN_POINT ( 'NONE',  ( 10.40644474310099810, -3.106516218291800246, -7.933599538786499039 ) ) ;
#60145 = CARTESIAN_POINT ( 'NONE',  ( 11.09999999999999964, 2.700228869961999845, 5.136740763824000133 ) ) ;
#60146 = CARTESIAN_POINT ( 'NONE',  ( 24.30000000000000071, -3.224868684338999980, -12.03537377768999939 ) ) ;
#60147 = CARTESIAN_POINT ( 'NONE',  ( 11.30995122972050027, 4.452766304612699955, -6.452959986593999275 ) ) ;
#60148 = ORIENTED_EDGE ( 'NONE', *, *, #68407, .F. ) ;
#60149 = CARTESIAN_POINT ( 'NONE',  ( 12.54926746055851616, -0.6731412448965049533, 12.58200685883812930 ) ) ;
#60150 = VECTOR ( 'NONE', #12503, 1000.000000000000000 ) ;
#60151 = CARTESIAN_POINT ( 'NONE',  ( 9.010198341230998054, 5.040787533781999841, 8.522957620707000359 ) ) ;
#60152 = CARTESIAN_POINT ( 'NONE',  ( 10.15403136780999915, 5.267988602993999514, 5.992335067371000079 ) ) ;
#60153 = COLOUR_RGB ( '', 0.31764706, 0.68627451, 0.89019608) ;
#60154 = CARTESIAN_POINT ( 'NONE',  ( 12.72250989631410789, 3.119868145445779284, 12.28529260172211757 ) ) ;
#60155 = VERTEX_POINT ( 'NONE', #37250 ) ;
#60156 = FACE_OUTER_BOUND ( 'NONE', #18543, .T. ) ;
#60157 = CARTESIAN_POINT ( 'NONE',  ( 10.54687750876899877, 3.382085645339300228, -8.458891008702400072 ) ) ;
#60158 = ADVANCED_FACE ( 'NONE', ( #9372 ), #37357, .F. ) ;
#60159 = CARTESIAN_POINT ( 'NONE',  ( 9.649875981546212955, 2.700874656648012184, 7.923553693498652351 ) ) ;
#60161 = CARTESIAN_POINT ( 'NONE',  ( 24.45625570098342294, 8.883597759657003934, -9.170492528765944229 ) ) ;
#60160 = CARTESIAN_POINT ( 'NONE',  ( 9.819055905797000605, 2.899999999999999911, -6.571291218949999902 ) ) ;
#60162 = CARTESIAN_POINT ( 'NONE',  ( 9.250151519676999001, -3.981249765141819719, 6.633192605878799775 ) ) ;
#60163 = CARTESIAN_POINT ( 'NONE',  ( 11.31825954179440075, -3.333768806796900019, -8.053565341712399572 ) ) ;
#60164 = CARTESIAN_POINT ( 'NONE',  ( 23.59999467231800097, -10.30760443253999981, -9.317695455237998914 ) ) ;
#60165 = ORIENTED_EDGE ( 'NONE', *, *, #43505, .F. ) ;
#60166 = B_SPLINE_CURVE_WITH_KNOTS ( 'NONE', 3,
 ( #52240, #30250, #67622, #19400 ),
 .UNSPECIFIED., .F., .F.,
 ( 4, 4 ),
 ( 0.000000000000000000, 1.000000000000000000 ),
 .UNSPECIFIED. ) ;
#60167 = CARTESIAN_POINT ( 'NONE',  ( 1.448519645393000044, 0.8376700968564000371, 3.321615185007000370 ) ) ;
#60168 = CARTESIAN_POINT ( 'NONE',  ( 12.79999999975700042, 11.86189249994999884, -3.298671769835999967 ) ) ;
#60169 = DIRECTION ( 'NONE',  ( -0.7071069400699796503, -0.7071066223030796349, -2.150925218129939376E-09 ) ) ;
#60170 = CARTESIAN_POINT ( 'NONE',  ( 8.943784697134999462, 4.470490447737899942, 8.228249052908999772 ) ) ;
#60171 = CARTESIAN_POINT ( 'NONE',  ( 10.62947109217999930, 5.100000000000000533, 6.152188490330000370 ) ) ;
#60172 = CARTESIAN_POINT ( 'NONE',  ( 12.08142877465145659, -2.567860614650635753, 13.76250926564159016 ) ) ;
#60173 = CARTESIAN_POINT ( 'NONE',  ( 10.87371169044000041, 2.935964136801999746, 5.107130734584000464 ) ) ;
#60174 = CARTESIAN_POINT ( 'NONE',  ( 24.08693222998299888, 3.426481660494999915, -12.66967535867999928 ) ) ;
#60175 = CARTESIAN_POINT ( 'NONE',  ( 13.64718133169100156, -12.21462133634999958, -2.516296819814999974 ) ) ;
#60176 = VERTEX_POINT ( 'NONE', #27808 ) ;
#60177 = CARTESIAN_POINT ( 'NONE',  ( 7.448333333331000006, 3.320114376499284425, -6.320388375721752716 ) ) ;
#60178 = CARTESIAN_POINT ( 'NONE',  ( 12.65360965087631939, 11.23193385079074957, -3.094113056604177014 ) ) ;
#60179 = CARTESIAN_POINT ( 'NONE',  ( 11.19955063476129631, -3.023401864784706294, -6.673569913327194847 ) ) ;
#60180 = DIRECTION ( 'NONE',  ( 1.000000000000000000, 0.000000000000000000, 0.000000000000000000 ) ) ;
#60181 = CARTESIAN_POINT ( 'NONE',  ( 1.514384680100000047, 3.707157770482000014, -0.6207725330884000803 ) ) ;
#60182 = DIRECTION ( 'NONE',  ( -1.000000000000000000, 0.000000000000000000, 0.000000000000000000 ) ) ;
#60183 = CARTESIAN_POINT ( 'NONE',  ( 17.86190681601106078, 1.955416883085901558, -12.56193573862143786 ) ) ;
#60184 = CARTESIAN_POINT ( 'NONE',  ( 10.34947814066000049, 4.457562099971999814, 6.154877938302999674 ) ) ;
#60185 = CARTESIAN_POINT ( 'NONE',  ( 11.78594988689359901, 4.393436444036099786, 6.728309553046099012 ) ) ;
#60186 = CARTESIAN_POINT ( 'NONE',  ( 5.500000000000000000, 0.8000000000000000444, 3.149999999999999911 ) ) ;
#60187 = CARTESIAN_POINT ( 'NONE',  ( 10.77401935321000082, -3.826867196099999813, -5.823197386290999589 ) ) ;
#60188 = EDGE_CURVE ( 'NONE', #42732, #32376, #20185, .T. ) ;
#60189 = CARTESIAN_POINT ( 'NONE',  ( 17.74278521991431390, -0.7069209314805200428, -13.98214394338238087 ) ) ;
#60190 = FACE_OUTER_BOUND ( 'NONE', #65083, .T. ) ;
#60191 = CARTESIAN_POINT ( 'NONE',  ( 12.19252377756937911, -2.624242476340350461, 12.42177825689173432 ) ) ;
#60192 = B_SPLINE_CURVE_WITH_KNOTS ( 'NONE', 3,
 ( #29239, #61039, #66962, #13503, #29931, #3332, #51235, #24665 ),
 .UNSPECIFIED., .F., .F.,
 ( 4, 2, 2, 4 ),
 ( 0.000000000000000000, 0.2500000000000022760, 0.5000000000000045519, 1.000000000000000000 ),
 .UNSPECIFIED. ) ;
#60193 = EDGE_LOOP ( 'NONE', ( #28842, #22963, #54652, #27841, #19287 ) ) ;
#60194 = CARTESIAN_POINT ( 'NONE',  ( 7.325000000000000178, 4.000000000000000000, 9.239711431703000244 ) ) ;
#60195 = ORIENTED_EDGE ( 'NONE', *, *, #57285, .T. ) ;
#60196 = CARTESIAN_POINT ( 'NONE',  ( 18.12879638218882761, -2.748081584522202636, 13.61770999214558309 ) ) ;
#60197 = CARTESIAN_POINT ( 'NONE',  ( 21.60000052036201268, -13.89999947951999992, -2.298221717064000337E-09 ) ) ;
#60198 = ORIENTED_EDGE ( 'NONE', *, *, #64933, .F. ) ;
#60199 = CARTESIAN_POINT ( 'NONE',  ( 11.40211496860029783, 4.793947479907100018, 7.906860999147899527 ) ) ;
#60200 = CARTESIAN_POINT ( 'NONE',  ( 5.970710119748616762, 0.2212404501104190957, -1.111240891371765516 ) ) ;
#60201 = CARTESIAN_POINT ( 'NONE',  ( 23.61436141550033341, 3.070533063945404262, -13.52808024449816848 ) ) ;
#60202 = CARTESIAN_POINT ( 'NONE',  ( 9.471374412057000924, 2.030666183831999927, 7.549764512038000142 ) ) ;
#60203 = CARTESIAN_POINT ( 'NONE',  ( 21.59999953993000332, 12.84999890301999947, 0.000000000000000000 ) ) ;
#60204 = CARTESIAN_POINT ( 'NONE',  ( 11.09999999997999964, 7.815194234324999378, -6.645247174075000096 ) ) ;
#60205 = CARTESIAN_POINT ( 'NONE',  ( 11.80912799980900019, 3.189026639965999443, -11.45098040807999951 ) ) ;
#60206 = CIRCLE ( 'NONE', #24313, 13.98989063586999571 ) ;
#60207 = CARTESIAN_POINT ( 'NONE',  ( 9.882901294779998125, -4.314558311729999929, -9.161035779983999205 ) ) ;
#60208 = CARTESIAN_POINT ( 'NONE',  ( 25.59994555223599733, -8.527741194213000142, -7.260611644044000279 ) ) ;
#60209 = CARTESIAN_POINT ( 'NONE',  ( 10.53324933263040819, -3.041617253709827384, -5.009215415433663665 ) ) ;
#60210 = ORIENTED_EDGE ( 'NONE', *, *, #38119, .T. ) ;
#60211 = CARTESIAN_POINT ( 'NONE',  ( 8.942941355974880935, 3.045333477771414721, -6.948775311896397078 ) ) ;
#60212 =( NAMED_UNIT ( * ) PLANE_ANGLE_UNIT ( ) SI_UNIT ( $, .RADIAN. ) );
#60213 = EDGE_LOOP ( 'NONE', ( #28548, #8935, #42463, #38777, #28929, #30953 ) ) ;
#60214 = CARTESIAN_POINT ( 'NONE',  ( 10.91079984335361353, 2.946977204686775931, -4.907707240660267090 ) ) ;
#60215 = CARTESIAN_POINT ( 'NONE',  ( 11.14212519252000000, -5.326817661814000182, 4.985844344934000638 ) ) ;
#60216 = CARTESIAN_POINT ( 'NONE',  ( 10.35376078907947495, 4.858294075600578132, 7.334408124199476298 ) ) ;
#60217 = CARTESIAN_POINT ( 'NONE',  ( 9.310585478579783469, 3.370455731697034718, 8.592274333092914773 ) ) ;
#60218 = CARTESIAN_POINT ( 'NONE',  ( 12.23404092485628247, 2.245077680571258671, 13.72419654341781126 ) ) ;
#60219 = CARTESIAN_POINT ( 'NONE',  ( 10.31457635473999979, -5.362146312020000138, 6.677778992223999843 ) ) ;
#60220 = VERTEX_POINT ( 'NONE', #21848 ) ;
#60221 = CARTESIAN_POINT ( 'NONE',  ( 7.856038276909000473, 2.869044596334999753, -6.744487387516000076 ) ) ;
#60222 = EDGE_CURVE ( 'NONE', #15952, #61459, #32700, .T. ) ;
#60223 = CARTESIAN_POINT ( 'NONE',  ( 12.18894359730774113, 0.3856318793704044401, 13.99470184309725873 ) ) ;
#60224 = EDGE_CURVE ( 'NONE', #26452, #57662, #35190, .T. ) ;
#60225 = ORIENTED_EDGE ( 'NONE', *, *, #36667, .F. ) ;
#60226 = CARTESIAN_POINT ( 'NONE',  ( 7.366090560818999933, 5.017953588770000195, -6.429833855306000601 ) ) ;
#60227 = CARTESIAN_POINT ( 'NONE',  ( 17.69319447854400096, 11.81408139396000045, -3.326117390868000179 ) ) ;
#60228 = CARTESIAN_POINT ( 'NONE',  ( 23.58312315446800156, -2.940929503173999926, -13.62839437077999882 ) ) ;
#60229 = CARTESIAN_POINT ( 'NONE',  ( 4.715620154312000878, -1.320023218807999887, -0.6740770609419000081 ) ) ;
#60230 = B_SPLINE_SURFACE_WITH_KNOTS ( 'NONE', 3, 3, ( 
 ( #54122, #60068, #43645, #59367 ),
 ( #48542, #42950, #12173, #33155 ),
 ( #43296, #38040, #54471, #64604 ),
 ( #38388, #22305, #16372, #6219 ),
 ( #27560, #16710, #64942, #22647 ),
 ( #33503, #6573, #37702, #59714 ),
 ( #17414, #54818, #21958, #11813 ),
 ( #59030, #11465, #32807, #43992 ),
 ( #49222, #48887, #11132, #994 ),
 ( #65298, #32466, #17055, #21615 ),
 ( #1330, #38739, #6918, #28250 ),
 ( #49570, #1680, #64258, #22996 ) ),
 .UNSPECIFIED., .F., .F., .F.,
 ( 4, 1, 1, 1, 1, 1, 1, 1, 1, 4 ),
 ( 4, 4 ),
 ( 0.5516038081316999575, 0.5999999999999999778, 0.6500000000000000222, 0.6999999999999999556, 0.7500000000000000000, 0.8000000000000000444, 0.8499999999999999778, 0.9000000000000000222, 0.9499999999999999556, 0.9893631058703999948 ),
 ( -0.2706695798834999889, 1.270788350771999919 ),
 .UNSPECIFIED. ) ;
#60231 = CARTESIAN_POINT ( 'NONE',  ( 10.10682028041000002, 4.294368353031000396, -8.968663198664000191 ) ) ;
#60232 = CARTESIAN_POINT ( 'NONE',  ( 4.049969279409727285, -2.099966510537780273, -9.844681520548669431E-09 ) ) ;
#60233 = CARTESIAN_POINT ( 'NONE',  ( 10.74708735964999917, -5.603138702306000418, -6.963343193308999979 ) ) ;
#60234 = CARTESIAN_POINT ( 'NONE',  ( 11.59999999999999964, 5.064318446328999634, -8.155535082817699788 ) ) ;
#60235 = DIRECTION ( 'NONE',  ( 0.000000000000000000, -0.1218274111675000937, -0.9925512993736016476 ) ) ;
#60236 = CARTESIAN_POINT ( 'NONE',  ( 25.60000000000000142, -13.52296156804999860, 3.623466631435000362 ) ) ;
#60237 = CARTESIAN_POINT ( 'NONE',  ( 9.172139116365000788, -4.730747404809998891, -8.668230005597001409 ) ) ;
#60238 = LINE ( 'NONE', #53607, #17958 ) ;
#60239 = CARTESIAN_POINT ( 'NONE',  ( 1.699999999999999956, 0.000000000000000000, 0.000000000000000000 ) ) ;
#60240 = CARTESIAN_POINT ( 'NONE',  ( 11.05946005378019947, 5.036385109519999403, -6.946587256304699309 ) ) ;
#60241 = ADVANCED_FACE ( 'NONE', ( #11023 ), #58570, .F. ) ;
#60242 = CARTESIAN_POINT ( 'NONE',  ( 9.052088727410998459, 2.999102593977000186, -7.583944523024719331 ) ) ;
#60244 = CARTESIAN_POINT ( 'NONE',  ( 9.581163468719386955, -9.035708932181607977, -6.816351070799541390 ) ) ;
#60243 = CARTESIAN_POINT ( 'NONE',  ( 10.07701337669299946, -4.772923352651200268, 7.892807122431200639 ) ) ;
#60245 = CARTESIAN_POINT ( 'NONE',  ( 11.19601354018301365, -3.000416447002272058, 8.268183399968641822 ) ) ;
#60246 = ORIENTED_EDGE ( 'NONE', *, *, #36263, .T. ) ;
#60247 = EDGE_CURVE ( 'NONE', #18238, #65620, #67723, .T. ) ;
#60248 = CARTESIAN_POINT ( 'NONE',  ( 11.01790547754519878, 5.174295865741999734, 7.462730980357120458 ) ) ;
#60249 = CARTESIAN_POINT ( 'NONE',  ( 11.25041341105000114, -5.730771985297000271, 8.122672103119001008 ) ) ;
#60250 = CARTESIAN_POINT ( 'NONE',  ( 9.910317406968998100, 4.212364169857599983, 6.378110563671000044 ) ) ;
#60251 = CARTESIAN_POINT ( 'NONE',  ( 10.30371347217102596, 4.589291630936051192, -8.130653431319531776 ) ) ;
#60252 = CARTESIAN_POINT ( 'NONE',  ( 10.03491210303999992, -5.615910465798999773, 7.351455544018000943 ) ) ;
#60253 = CARTESIAN_POINT ( 'NONE',  ( 10.90076026837999912, -2.899999999941999640, -5.152573395210000129 ) ) ;
#60255 = CARTESIAN_POINT ( 'NONE',  ( 10.62309687351639020, 5.217465845835395299, 7.172815144550900968 ) ) ;
#60254 = UNCERTAINTY_MEASURE_WITH_UNIT (LENGTH_MEASURE( 1.000000000000000082E-05 ), #45434, 'distance_accuracy_value', 'NONE');
#60256 = VERTEX_POINT ( 'NONE', #11360 ) ;
#60257 = CARTESIAN_POINT ( 'NONE',  ( 8.773468108405998223, -3.033597967472499768, -7.773695785133000413 ) ) ;
#60258 = CARTESIAN_POINT ( 'NONE',  ( 17.60000000085000238, 12.11987927271999865, -3.159802730921999814 ) ) ;
#60259 = DIRECTION ( 'NONE',  ( -1.000000000000000000, 0.000000000000000000, 0.000000000000000000 ) ) ;
#60260 = CARTESIAN_POINT ( 'NONE',  ( 8.789886373836322875, 4.000007821194417446, -8.439846342473931173 ) ) ;
#60261 = CARTESIAN_POINT ( 'NONE',  ( 24.34833281187866660, -3.256146913723438896, 12.15210571892843916 ) ) ;
#60262 = CARTESIAN_POINT ( 'NONE',  ( 13.50018479229797208, -10.27880801399731858, -5.973155204427725629 ) ) ;
#60263 = CARTESIAN_POINT ( 'NONE',  ( 10.40749413291699987, 4.788043169210699723, -7.140435631538599281 ) ) ;
#60264 = CARTESIAN_POINT ( 'NONE',  ( 12.19576242957160872, 2.360357254155278639, -13.70208745183198928 ) ) ;
#60265 = CARTESIAN_POINT ( 'NONE',  ( 10.99999999883999990, 0.3999999988385999905, -7.388315149414999894 ) ) ;
#60266 = CARTESIAN_POINT ( 'NONE',  ( 5.694051799045005247, 13.02176618969100552, 2.006311319538786719 ) ) ;
#60267 = ORIENTED_EDGE ( 'NONE', *, *, #45454, .T. ) ;
#60268 = CARTESIAN_POINT ( 'NONE',  ( 24.67332274059700126, -12.15930828887999837, -3.026486267162999511 ) ) ;
#60269 = CARTESIAN_POINT ( 'NONE',  ( 12.54917863858677762, -0.6836428945794239542, -13.98330131869062321 ) ) ;
#60270 = CARTESIAN_POINT ( 'NONE',  ( 14.04004776902899998, -8.829547661313998930, -7.819892149868999276 ) ) ;
#60271 = CARTESIAN_POINT ( 'NONE',  ( 25.29878307837499918, -8.389243454266001265, -8.298034019942999606 ) ) ;
#60272 = CARTESIAN_POINT ( 'NONE',  ( 10.57101354018312023, -3.231816600031356845, -8.499583552997725278 ) ) ;
#60273 = CARTESIAN_POINT ( 'NONE',  ( 8.099999999999999645, 0.000000000000000000, 11.84999999999999964 ) ) ;
#60274 = CARTESIAN_POINT ( 'NONE',  ( 13.46281931570200108, 12.03411875281000043, 2.480748420245000307 ) ) ;
#60275 = ORIENTED_EDGE ( 'NONE', *, *, #41907, .F. ) ;
#60276 = CARTESIAN_POINT ( 'NONE',  ( 6.949999692292999853, -1.332267629549999942E-14, 1.576516694967999966E-14 ) ) ;
#60277 = CARTESIAN_POINT ( 'NONE',  ( 18.17485192111303860, 2.583003800953513007, -13.65552556266986528 ) ) ;
#60278 = ORIENTED_EDGE ( 'NONE', *, *, #34750, .T. ) ;
#60279 = FACE_OUTER_BOUND ( 'NONE', #7470, .T. ) ;
#60280 = CARTESIAN_POINT ( 'NONE',  ( 8.160745559622998968, -5.944572422272999646, 7.106845737860000511 ) ) ;
#60281 = CARTESIAN_POINT ( 'NONE',  ( 9.021064158776001207, 4.883347899767999323, -6.417062834774999835 ) ) ;
#60282 = CARTESIAN_POINT ( 'NONE',  ( 23.94498309455302731, -12.80023880358030475, 3.529808243006147706 ) ) ;
#60283 = CARTESIAN_POINT ( 'NONE',  ( 11.75203632436369894, -5.109717061557999429, -7.240848640331599917 ) ) ;
#60284 = B_SPLINE_CURVE_WITH_KNOTS ( 'NONE', 3,
 ( #37834, #88, #47648, #37489 ),
 .UNSPECIFIED., .F., .F.,
 ( 4, 4 ),
 ( 0.000000000000000000, 1.000000000000000000 ),
 .UNSPECIFIED. ) ;
#60285 = CARTESIAN_POINT ( 'NONE',  ( 7.936333720142999759, -5.123034382927999175, 6.721303993095999907 ) ) ;
#60286 = DIRECTION ( 'NONE',  ( 0.000000000000000000, -0.6664713972124013397, 0.7455306007789014311 ) ) ;
#60287 = ORIENTED_EDGE ( 'NONE', *, *, #6524, .F. ) ;
#60288 = CARTESIAN_POINT ( 'NONE',  ( 10.13050497920000126, -3.092053006542000215, 8.629388195475000245 ) ) ;
#60289 = CARTESIAN_POINT ( 'NONE',  ( 18.12469242183976093, -2.757364536338188898, -13.61544764698360943 ) ) ;
#60290 = CARTESIAN_POINT ( 'NONE',  ( 9.096889158776001238, 2.235961884443999459, -6.794506518623999902 ) ) ;
#60291 = ORIENTED_EDGE ( 'NONE', *, *, #26125, .F. ) ;
#60292 = CARTESIAN_POINT ( 'NONE',  ( 10.38153063908000107, 2.772139908660999907, -8.408082511401000048 ) ) ;
#60293 = CARTESIAN_POINT ( 'NONE',  ( 10.87946694038000039, -2.817416132545000007, -6.828662897514999663 ) ) ;
#60294 = ORIENTED_EDGE ( 'NONE', *, *, #8365, .F. ) ;
#60295 = CARTESIAN_POINT ( 'NONE',  ( 9.913279731609000223, 4.090130512164860122, 8.500359330993999762 ) ) ;
#60296 = CARTESIAN_POINT ( 'NONE',  ( 18.24677884388065863, -2.264233918701653803, -12.39489312188808512 ) ) ;
#60297 = CARTESIAN_POINT ( 'NONE',  ( 9.674373738639999942, -2.899999999999999911, -6.185493860157000867 ) ) ;
#60298 = CARTESIAN_POINT ( 'NONE',  ( 16.31137892731300099, 3.415016125706999972, 11.89702177947000017 ) ) ;
#60299 = CARTESIAN_POINT ( 'NONE',  ( 24.35365242081700288, 3.193712117558000774, 11.49150331547998860 ) ) ;
#60300 = CARTESIAN_POINT ( 'NONE',  ( 10.11591290906799934, 3.364470222553300083, 6.722218404915299317 ) ) ;
#60301 = ADVANCED_FACE ( 'NONE', ( #22539 ), #35179, .T. ) ;
#60302 = PLANE ( 'NONE',  #48193 ) ;
#60303 = EDGE_CURVE ( 'NONE', #31596, #59588, #41898, .T. ) ;
#60304 = EDGE_LOOP ( 'NONE', ( #63438, #28791 ) ) ;
#60305 = LINE ( 'NONE', #38632, #52619 ) ;
#60306 = CARTESIAN_POINT ( 'NONE',  ( 11.00119221959000093, 4.640446572790000168, -9.059321223816999336 ) ) ;
#60307 = B_SPLINE_CURVE_WITH_KNOTS ( 'NONE', 3,
 ( #4068, #47779, #69086, #15947 ),
 .UNSPECIFIED., .F., .F.,
 ( 4, 4 ),
 ( 0.000000000000000000, 1.000000000000000000 ),
 .UNSPECIFIED. ) ;
#60308 = CARTESIAN_POINT ( 'NONE',  ( 11.50000000000000000, -4.968589424331200100, 7.825000000000000178 ) ) ;
#60309 = CARTESIAN_POINT ( 'NONE',  ( 12.17997927555898308, 2.482106649064417692, -13.67725710540907436 ) ) ;
#60310 = CARTESIAN_POINT ( 'NONE',  ( 11.16684687351590277, -3.231816600031351516, 8.499583552997723501 ) ) ;
#60311 = CARTESIAN_POINT ( 'NONE',  ( 10.83668192271000130, -4.288535286065000562, 9.448729895547000268 ) ) ;
#60312 = CARTESIAN_POINT ( 'NONE',  ( 17.86760510161943571, 0.5416168188285641616, 13.88579828294358798 ) ) ;
#60313 = CARTESIAN_POINT ( 'NONE',  ( 17.75497764282780366, 0.5922531180535276496, 13.88301284246674783 ) ) ;
#60314 = ORIENTED_EDGE ( 'NONE', *, *, #21303, .T. ) ;
#60315 = VERTEX_POINT ( 'NONE', #64836 ) ;
#60316 = CARTESIAN_POINT ( 'NONE',  ( 8.351014158771000950, 5.616457598545999907, -8.245813000738998255 ) ) ;
#60317 = CARTESIAN_POINT ( 'NONE',  ( 12.42592716720131030, -0.4969868314062168002, 13.88804154507259447 ) ) ;
#60318 = CARTESIAN_POINT ( 'NONE',  ( 12.23477845766454308, -0.2559490220536964067, -13.89683205629668628 ) ) ;
#60319 = CARTESIAN_POINT ( 'NONE',  ( 10.44080359545000114, -5.435731278187999393, 7.303630150377999009 ) ) ;
#60320 = CARTESIAN_POINT ( 'NONE',  ( 9.157210916635261100, -5.507291520428013953, 6.616308516811844953 ) ) ;
#60321 = CARTESIAN_POINT ( 'NONE',  ( 7.486433059621999675, -5.321924421352999701, 8.118250081378000971 ) ) ;
#60323 = AXIS2_PLACEMENT_3D ( 'NONE', #29700, #1725, #18160 ) ;
#60322 = FACE_OUTER_BOUND ( 'NONE', #60862, .T. ) ;
#60325 = CARTESIAN_POINT ( 'NONE',  ( 11.01655322883999943, -6.705649024436000083, 5.522682893586000397 ) ) ;
#60324 = CARTESIAN_POINT ( 'NONE',  ( 10.28568422951000016, -4.901739481456999670, 8.407331414124799451 ) ) ;
#60326 = CARTESIAN_POINT ( 'NONE',  ( 10.14887885159599890, 5.269014563305000287, -7.348611220446799486 ) ) ;
#60327 = ADVANCED_FACE ( 'NONE', ( #57271 ), #44621, .F. ) ;
#60328 = CARTESIAN_POINT ( 'NONE',  ( 24.54687940532799928, -8.860358431052000938, -9.345000394951000544 ) ) ;
#60329 = B_SPLINE_CURVE_WITH_KNOTS ( 'NONE', 3,
 ( #24791, #40193, #50333, #61509, #29716, #8374 ),
 .UNSPECIFIED., .F., .F.,
 ( 4, 2, 4 ),
 ( 0.000000000000000000, 0.4999999999999994449, 1.000000000000000000 ),
 .UNSPECIFIED. ) ;
#60330 = CARTESIAN_POINT ( 'NONE',  ( 17.60000000798000386, 11.41069016990000051, -4.623987642516999230 ) ) ;
#60331 = CARTESIAN_POINT ( 'NONE',  ( 17.88568294903051381, 0.5304820368560144717, 12.68508456201358747 ) ) ;
#60332 = CARTESIAN_POINT ( 'NONE',  ( 11.59999999999999964, 4.000000000000000000, -7.500000000000000000 ) ) ;
#60333 = CARTESIAN_POINT ( 'NONE',  ( 17.63951772023416709, -3.120582521214973148, -12.28507980727128057 ) ) ;
#60334 = VERTEX_POINT ( 'NONE', #34775 ) ;
#60336 = CARTESIAN_POINT ( 'NONE',  ( 8.927279675098239053, 5.100000000000000533, -6.498507975215145116 ) ) ;
#60335 = CARTESIAN_POINT ( 'NONE',  ( 24.14469781561994211, -3.678927484064260511, 12.80140212425259705 ) ) ;
#60337 = CARTESIAN_POINT ( 'NONE',  ( 8.555820280412000045, 2.414630869937000046, -6.801495146585999407 ) ) ;
#60338 = FACE_OUTER_BOUND ( 'NONE', #10387, .T. ) ;
#60339 = CARTESIAN_POINT ( 'NONE',  ( 10.31498017945871126, -2.650031506806249659, -7.499998780888571304 ) ) ;
#60340 = CARTESIAN_POINT ( 'NONE',  ( 7.895317210312003731, -5.140737874544996977, 6.778394131643998399 ) ) ;
#60341 = CARTESIAN_POINT ( 'NONE',  ( 18.05828223140173705, -3.296090368282506233, -11.87625427050431703 ) ) ;
#60342 = CARTESIAN_POINT ( 'NONE',  ( 2.638201263761000170, 2.164689359125999690, -2.654983729890999733 ) ) ;
#60343 = VERTEX_POINT ( 'NONE', #18003 ) ;
#60344 = CARTESIAN_POINT ( 'NONE',  ( 12.09634453438820501, -0.1521017209118943059, -12.59908727444664045 ) ) ;
#60345 = CARTESIAN_POINT ( 'NONE',  ( 11.93114108301962162, -3.379311755690166841, 8.119401481368297979 ) ) ;
#60346 = DIRECTION ( 'NONE',  ( 1.000000000000000000, 0.000000000000000000, 0.000000000000000000 ) ) ;
#60347 = CARTESIAN_POINT ( 'NONE',  ( 9.143920280410000601, 5.791553967443999973, 7.752111263209999770 ) ) ;
#60348 = VERTEX_POINT ( 'NONE', #33391 ) ;
#60349 = CARTESIAN_POINT ( 'NONE',  ( 6.356846742204999678, 0.002905985354530999862, 1.468509142934999900 ) ) ;
#60350 = CARTESIAN_POINT ( 'NONE',  ( 10.93613845918347138, 9.381696929438323451, 6.182830334041338638 ) ) ;
#60352 = CARTESIAN_POINT ( 'NONE',  ( 0.000000000000000000, 5.100000000000000533, 7.500000000000000000 ) ) ;
#60351 = DIRECTION ( 'NONE',  ( -1.000000000000000000, 0.000000000000000000, 0.000000000000000000 ) ) ;
#60353 = CARTESIAN_POINT ( 'NONE',  ( 12.80505043854143388, 1.875000000000000000, 12.57541666120756041 ) ) ;
#60354 = VERTEX_POINT ( 'NONE', #13453 ) ;
#60355 = DIRECTION ( 'NONE',  ( 0.9999999999999326095, -3.671478400246118675E-07, 1.807828440105059414E-09 ) ) ;
#60356 = CARTESIAN_POINT ( 'NONE',  ( 9.625489929093001606, -3.134630999349000025, 8.626959345509000343 ) ) ;
#60357 = ORIENTED_EDGE ( 'NONE', *, *, #50916, .F. ) ;
#60358 = CARTESIAN_POINT ( 'NONE',  ( 9.525000000000000355, -4.417172942406000224, 8.783926296998000538 ) ) ;
#60360 = CARTESIAN_POINT ( 'NONE',  ( 25.10988277031431437, -8.510211365751388257, -8.211054588496716988 ) ) ;
#60359 = AXIS2_PLACEMENT_3D ( 'NONE', #60740, #25307, #55501 ) ;
#60361 = CARTESIAN_POINT ( 'NONE',  ( 17.78490373093669774, -0.5812901181791690908, -13.88363587338389493 ) ) ;
#60362 = ADVANCED_FACE ( 'NONE', ( #2597 ), #54707, .F. ) ;
#60363 = ADVANCED_FACE ( 'NONE', ( #34085, #12059 ), #38981, .F. ) ;
#60364 = VERTEX_POINT ( 'NONE', #50844 ) ;
#60365 = CARTESIAN_POINT ( 'NONE',  ( 10.56742170454999830, -8.204434595504999095, 6.610786703431000610 ) ) ;
#60366 = DIRECTION ( 'NONE',  ( 0.000000000000000000, -1.000000000000000000, 0.000000000000000000 ) ) ;
#60367 = CARTESIAN_POINT ( 'NONE',  ( 7.391614158769000298, 2.869384229876999814, -6.678559560168999987 ) ) ;
#60368 = LINE ( 'NONE', #28211, #21954 ) ;
#60369 = CARTESIAN_POINT ( 'NONE',  ( 11.54752711762115958, -2.837609288610280167, 7.175009463222314032 ) ) ;
#60370 = ORIENTED_EDGE ( 'NONE', *, *, #42187, .T. ) ;
#60371 = CARTESIAN_POINT ( 'NONE',  ( 9.069718325438000051, 4.108964550738000376, 8.851615252874999840 ) ) ;
#60372 = CARTESIAN_POINT ( 'NONE',  ( 24.15420937678199920, -12.81569892223000018, -3.249518417564999595 ) ) ;
#60373 = AXIS2_PLACEMENT_3D ( 'NONE', #58859, #36164, #31272 ) ;
#60374 = CARTESIAN_POINT ( 'NONE',  ( 11.03776785110999903, 5.237767851104999650, 6.571291218949999902 ) ) ;
#60375 = B_SPLINE_CURVE_WITH_KNOTS ( 'NONE', 3,
 ( #1898, #39647, #43856, #13433, #44899, #38962 ),
 .UNSPECIFIED., .F., .F.,
 ( 4, 2, 4 ),
 ( 0.000000000000000000, 0.5000000000000000000, 1.000000000000000000 ),
 .UNSPECIFIED. ) ;
#60376 = CARTESIAN_POINT ( 'NONE',  ( 12.70851731081069502, -1.792711832340346145, 13.88474979353782501 ) ) ;
#60377 = EDGE_LOOP ( 'NONE', ( #54101, #47036, #2384, #32365 ) ) ;
#60378 = B_SPLINE_SURFACE_WITH_KNOTS ( 'NONE', 3, 3, ( 
 ( #68311, #42448, #62394, #36863 ),
 ( #41074, #26373, #31617, #25677 ),
 ( #67627, #9243, #47010, #26023 ),
 ( #57481, #19751, #30585, #52588 ),
 ( #14510, #51897, #47355, #3995 ),
 ( #69010, #46670, #20090, #58181 ),
 ( #9588, #30933, #41760, #63060 ),
 ( #15187, #10283, #68659, #57834 ),
 ( #21123, #21438, #16199, #43473 ) ),
 .UNSPECIFIED., .F., .F., .F.,
 ( 4, 1, 1, 1, 1, 1, 4 ),
 ( 4, 4 ),
 ( 0.02209653170518000032, 0.1666666666667000196, 0.3333333333333000081, 0.5000000000000000000, 0.6666666666667000474, 0.8333333333333000637, 0.9492823795161999811 ),
 ( -0.1916656884162999952, 1.191851428473000185 ),
 .UNSPECIFIED. ) ;
#60379 = CARTESIAN_POINT ( 'NONE',  ( 23.74396220697517634, 13.10156841507209613, -3.794861878603663197 ) ) ;
#60380 = CARTESIAN_POINT ( 'NONE',  ( 10.84393020684979980, 2.750000000000000000, -7.500000000000000000 ) ) ;
#60381 = CARTESIAN_POINT ( 'NONE',  ( 16.00017105474300294, 1.714184350020999865E-13, 1.962874307536999842E-13 ) ) ;
#60382 = CARTESIAN_POINT ( 'NONE',  ( 5.000030787343000327, -0.5496608443529829024, 2.045306479342562156 ) ) ;
#60383 = CARTESIAN_POINT ( 'NONE',  ( 9.041074696474980854, -2.899999999999999911, 6.201633003103719233 ) ) ;
#60384 = CARTESIAN_POINT ( 'NONE',  ( 5.500000000000000000, -1.406666666667000021, 10.45580168561000001 ) ) ;
#60385 = CARTESIAN_POINT ( 'NONE',  ( 17.84275129854003694, -3.054939169952809230, 12.30480372676524681 ) ) ;
#60386 = ORIENTED_EDGE ( 'NONE', *, *, #38919, .F. ) ;
#60387 = EDGE_CURVE ( 'NONE', #58572, #15150, #16836, .T. ) ;
#60388 = CARTESIAN_POINT ( 'NONE',  ( 11.51145123989532948, -3.394760891061399999, -8.668865425277999748 ) ) ;
#60389 = EDGE_CURVE ( 'NONE', #48412, #65865, #11891, .T. ) ;
#60390 = VERTEX_POINT ( 'NONE', #55752 ) ;
#60391 = CARTESIAN_POINT ( 'NONE',  ( 0.1499942179680000542, 2.749953718116142642, 0.3599680999394014314 ) ) ;
#60392 = CARTESIAN_POINT ( 'NONE',  ( 8.351014158771000950, 5.616457598545999907, -8.245813000738998255 ) ) ;
#60393 = ADVANCED_FACE ( 'NONE', ( #7853 ), #68944, .F. ) ;
#60394 = CARTESIAN_POINT ( 'NONE',  ( 3.425331920129000007, 1.732887122961999982, 2.901267362544000417 ) ) ;
#60395 = CARTESIAN_POINT ( 'NONE',  ( 11.10061802256000085, -3.093055606601000207, -6.153681532251999542 ) ) ;
#60396 = LINE ( 'NONE', #38726, #66281 ) ;
#60397 = CARTESIAN_POINT ( 'NONE',  ( 23.74225507199300367, 13.04612777714000060, 3.828889919760000371 ) ) ;
#60398 = LINE ( 'NONE', #23337, #60150 ) ;
#60399 = ORIENTED_EDGE ( 'NONE', *, *, #45150, .T. ) ;
#60400 = CARTESIAN_POINT ( 'NONE',  ( 23.60000000000000142, 0.000000000000000000, 0.000000000000000000 ) ) ;
#60401 = AXIS2_PLACEMENT_3D ( 'NONE', #10619, #47694, #58860 ) ;
#60402 = CARTESIAN_POINT ( 'NONE',  ( 11.42026088462129962, -3.997864853650589634, 8.503467136482999678 ) ) ;
#60403 = CARTESIAN_POINT ( 'NONE',  ( 10.59344747867000081, 5.297752619853000944, 8.474195539311001113 ) ) ;
#60404 = CARTESIAN_POINT ( 'NONE',  ( 25.39940835236649264, -2.782819894115065029, 11.32465380471084693 ) ) ;
#60405 = CARTESIAN_POINT ( 'NONE',  ( 8.924662153698962541, -5.350575487761723537, 7.500021879703682615 ) ) ;
#60406 = CARTESIAN_POINT ( 'NONE',  ( 11.01666666666767469, 3.382745367833757122, 8.852578401491365767 ) ) ;
#60407 = CARTESIAN_POINT ( 'NONE',  ( 11.19102897915239936, 4.256858847510399890, -8.470038342183499935 ) ) ;
#60408 = VECTOR ( 'NONE', #59777, 1000.000000000000114 ) ;
#60409 = EDGE_CURVE ( 'NONE', #36918, #11759, #25133, .T. ) ;
#60410 = CARTESIAN_POINT ( 'NONE',  ( 7.100000000000521894, 4.275133281870672874, -6.140122557344056098 ) ) ;
#60411 = CARTESIAN_POINT ( 'NONE',  ( 10.34091290906799898, 3.277531639390499851, -8.384179803770500428 ) ) ;
#60412 = CARTESIAN_POINT ( 'NONE',  ( 23.58679018630100188, -10.27406905139999971, 9.417699698887998849 ) ) ;
#60413 = AXIS2_PLACEMENT_3D ( 'NONE', #26797, #63139, #15264 ) ;
#60414 = CARTESIAN_POINT ( 'NONE',  ( 8.113858213201577740, 5.049150732340172532, -6.494099727906681885 ) ) ;
#60415 = VERTEX_POINT ( 'NONE', #62358 ) ;
#60416 = CARTESIAN_POINT ( 'NONE',  ( 9.298691940377999288, -5.159251056493999954, 9.109488373271000583 ) ) ;
#60417 = CARTESIAN_POINT ( 'NONE',  ( 9.617147628285000138, -2.491831134779999957, -6.388915175267000812 ) ) ;
#60418 = CARTESIAN_POINT ( 'NONE',  ( 18.05368493555551268, 1.987806113122528640, 13.85816345346370504 ) ) ;
#60419 = CARTESIAN_POINT ( 'NONE',  ( 23.56664676942400050, 2.935522432666999748, 13.67843419499999946 ) ) ;
#60420 = CARTESIAN_POINT ( 'NONE',  ( 11.20733594839949809, -3.159733897807000425, -6.537051788466999191 ) ) ;
#60421 = VERTEX_POINT ( 'NONE', #57446 ) ;
#60422 = CARTESIAN_POINT ( 'NONE',  ( 25.19966451436399879, 3.337967404952000283, -11.59330719735999971 ) ) ;
#60423 = CARTESIAN_POINT ( 'NONE',  ( 8.373670280412000011, 2.202812441249000219, 7.706988150133999405 ) ) ;
#60425 = DIRECTION ( 'NONE',  ( 1.000000000000000000, 0.000000000000000000, 0.000000000000000000 ) ) ;
#60424 = CARTESIAN_POINT ( 'NONE',  ( 8.397785841227999981, 5.616457598545999907, -8.245813000738998255 ) ) ;
#60426 = CARTESIAN_POINT ( 'NONE',  ( 10.64556415877000006, 2.988929467935999895, -5.952329570726999641 ) ) ;
#60427 = EDGE_LOOP ( 'NONE', ( #3885, #14209, #63795, #48972 ) ) ;
#60428 = CARTESIAN_POINT ( 'NONE',  ( 9.910633732652998518, 2.107262079134000210, 7.885285091859000062 ) ) ;
#60429 = CARTESIAN_POINT ( 'NONE',  ( 17.71791196170131144, -3.103760126671077035, -13.52664063941736217 ) ) ;
#60430 = CARTESIAN_POINT ( 'NONE',  ( 10.89149144726329865, 3.340422662105400065, 8.430724369296298093 ) ) ;
#60431 = CARTESIAN_POINT ( 'NONE',  ( 9.722771884505998941, -5.493781611190000191, 6.566828939965000167 ) ) ;
#60432 = CARTESIAN_POINT ( 'NONE',  ( 1.700000811628999964, 0.000000000000000000, 0.000000000000000000 ) ) ;
#60433 = ORIENTED_EDGE ( 'NONE', *, *, #66436, .F. ) ;
#60434 = CARTESIAN_POINT ( 'NONE',  ( 11.09999999999999964, 5.299311513382999550, 5.124965750789000296 ) ) ;
#60436 = CARTESIAN_POINT ( 'NONE',  ( 11.18236694037999968, -4.516641106826999597, -8.757887038823000125 ) ) ;
#60435 = CARTESIAN_POINT ( 'NONE',  ( 11.85864217039400259, -11.85700164854999983, 4.150661879143999755 ) ) ;
#60437 = CARTESIAN_POINT ( 'NONE',  ( 8.093329789650123729, -4.416228695728097620, 5.811362191399359389 ) ) ;
#60438 = CARTESIAN_POINT ( 'NONE',  ( 10.49785673611999925, -3.776281940467000275, 5.717636230565000588 ) ) ;
#60439 = CARTESIAN_POINT ( 'NONE',  ( 23.64132674793100364, 3.068957318205999929, 13.45500447039000136 ) ) ;
#60440 = CARTESIAN_POINT ( 'NONE',  ( 10.05665911260400058, -4.496147888241900148, 6.471616938597000157 ) ) ;
#60441 = VERTEX_POINT ( 'NONE', #3961 ) ;
#60442 = CARTESIAN_POINT ( 'NONE',  ( 23.81728156613312564, -9.687086922993964677, 9.414217616044480152 ) ) ;
#60443 = CARTESIAN_POINT ( 'NONE',  ( 10.89918582084299992, -4.746348444722899629, 8.362701637490498996 ) ) ;
#60444 = ORIENTED_EDGE ( 'NONE', *, *, #56275, .F. ) ;
#60445 = CARTESIAN_POINT ( 'NONE',  ( 9.035395982797805203, 3.688926447190844726, 6.345787448237017792 ) ) ;
#60446 = ORIENTED_EDGE ( 'NONE', *, *, #47519, .F. ) ;
#60447 = EDGE_CURVE ( 'NONE', #55474, #61815, #4649, .T. ) ;
#60448 = ADVANCED_FACE ( 'NONE', ( #46634 ), #51924, .T. ) ;
#60449 = CARTESIAN_POINT ( 'NONE',  ( 9.301695280414000067, 5.619431609641999614, -8.115423117607999615 ) ) ;
#60450 = CARTESIAN_POINT ( 'NONE',  ( 24.23279599547700158, 12.46651541951000119, -3.268895217084000215 ) ) ;
#60451 = EDGE_CURVE ( 'NONE', #58276, #55894, #26009, .T. ) ;
#60452 = CARTESIAN_POINT ( 'NONE',  ( 25.30000327618300204, 8.756202924575998026, 7.455126447192999883 ) ) ;
#60453 = CARTESIAN_POINT ( 'NONE',  ( 12.32471554566191685, 3.019419751198737956, -12.23287256106958054 ) ) ;
#60454 = CARTESIAN_POINT ( 'NONE',  ( 11.73589666366019912, -4.039600775206940497, 6.608753462694600067 ) ) ;
#60455 = B_SPLINE_CURVE_WITH_KNOTS ( 'NONE', 3,
 ( #40244, #29772, #28729, #12637 ),
 .UNSPECIFIED., .F., .F.,
 ( 4, 4 ),
 ( 0.000000000000000000, 1.000000000000000000 ),
 .UNSPECIFIED. ) ;
#60456 = CARTESIAN_POINT ( 'NONE',  ( 12.79999998712400178, 11.53033693765999779, -4.891431908114999949 ) ) ;
#60457 = ORIENTED_EDGE ( 'NONE', *, *, #6486, .T. ) ;
#60458 = CARTESIAN_POINT ( 'NONE',  ( 24.35365242081700288, 10.90899669677000006, 3.315896191878997978 ) ) ;
#60459 = LINE ( 'NONE', #66036, #32 ) ;
#60460 = VERTEX_POINT ( 'NONE', #19366 ) ;
#60461 = CARTESIAN_POINT ( 'NONE',  ( 12.09642313398532742, -2.633248533341327580, -12.32177498806537130 ) ) ;
#60462 = CARTESIAN_POINT ( 'NONE',  ( 10.64533863405319991, 4.703785194191100416, 6.602238051205399749 ) ) ;
#60463 = CARTESIAN_POINT ( 'NONE',  ( 10.98633305961999973, -3.015090804604000141, -9.064432363387998848 ) ) ;
#60464 = CARTESIAN_POINT ( 'NONE',  ( 10.75911768454999873, 4.477564074640000058, -5.708570851020999370 ) ) ;
#60465 = CARTESIAN_POINT ( 'NONE',  ( 17.60631394974399910, -11.38841897587999874, 4.575468659046999953 ) ) ;
#60466 = CARTESIAN_POINT ( 'NONE',  ( 10.46754921866999943, -2.318350880468999620, 6.549783596838000044 ) ) ;
#60467 = FACE_OUTER_BOUND ( 'NONE', #66906, .T. ) ;
#60468 = CARTESIAN_POINT ( 'NONE',  ( 18.12848705786299419, 0.2487950381773061104, -12.69672507751632828 ) ) ;
#60469 = AXIS2_PLACEMENT_3D ( 'NONE', #44589, #65187, #7161 ) ;
#60470 = CARTESIAN_POINT ( 'NONE',  ( 12.19400419508993139, 2.631361540197885152, -12.42001554614283165 ) ) ;
#60471 = CARTESIAN_POINT ( 'NONE',  ( 11.21149010443640037, -2.862435565199000109, -7.585072163144589652 ) ) ;
#60472 = CARTESIAN_POINT ( 'NONE',  ( 9.059364158773000497, 4.192919163547999872, 5.525472271700999194 ) ) ;
#60473 = ORIENTED_EDGE ( 'NONE', *, *, #38938, .F. ) ;
#60474 = CARTESIAN_POINT ( 'NONE',  ( 9.129282595918652987, 5.249943393780839074, -7.730023426265350217 ) ) ;
#60475 = CARTESIAN_POINT ( 'NONE',  ( 5.500000000000000000, -0.2500000000000000000, 9.776630298829998011 ) ) ;
#60476 = CARTESIAN_POINT ( 'NONE',  ( 10.62793268324000096, 3.100586971929999880, 8.599896650316999569 ) ) ;
#60477 = EDGE_CURVE ( 'NONE', #24606, #28975, #68686, .T. ) ;
#60478 = CARTESIAN_POINT ( 'NONE',  ( 24.63807759523900032, -3.694099725974000048, 12.29546658197999953 ) ) ;
#60479 = CARTESIAN_POINT ( 'NONE',  ( 18.08264632488620194, 2.164896798301381153, 12.52334278189866623 ) ) ;
#60480 = DIRECTION ( 'NONE',  ( 0.000000000000000000, 0.8514547570628037132, -0.5244280662542021298 ) ) ;
#60481 = CARTESIAN_POINT ( 'NONE',  ( 9.380783851237000093, 2.204242311415999911, 7.545378292079000460 ) ) ;
#60482 = CARTESIAN_POINT ( 'NONE',  ( 10.05617904522862638, -4.616765641734932757, 8.120590373834733811 ) ) ;
#60483 = CARTESIAN_POINT ( 'NONE',  ( 2.244900308897999963, 3.200088964812000114, -0.3100843839799999890 ) ) ;
#60484 = ORIENTED_EDGE ( 'NONE', *, *, #62668, .F. ) ;
#60485 = CARTESIAN_POINT ( 'NONE',  ( 12.29441019255336975, -2.991168332544440034, 12.23980925793768293 ) ) ;
#60486 = CARTESIAN_POINT ( 'NONE',  ( 9.173759580228997734, -4.976892840331100132, -7.266499081715599218 ) ) ;
#60487 = DIRECTION ( 'NONE',  ( 0.000000000000000000, 0.000000000000000000, -1.000000000000000000 ) ) ;
#60488 = CARTESIAN_POINT ( 'NONE',  ( 9.201637546194751494, 4.272535203994794806, 8.730330573913894554 ) ) ;
#60489 = CARTESIAN_POINT ( 'NONE',  ( 11.03502897915239878, 4.327133900127000388, -8.735435061820998826 ) ) ;
#60490 = EDGE_CURVE ( 'NONE', #8323, #57590, #19318, .T. ) ;
#60491 = CARTESIAN_POINT ( 'NONE',  ( 12.28357442006480937, -0.4998493492226937507, 12.59008424712975227 ) ) ;
#60492 = CARTESIAN_POINT ( 'NONE',  ( 8.946010841230998878, 5.458692773671000253, 7.456452194274000078 ) ) ;
#60493 = CARTESIAN_POINT ( 'NONE',  ( 10.02991192131000098, 2.506457833269999824, 6.215406506815000398 ) ) ;
#60494 = CARTESIAN_POINT ( 'NONE',  ( 12.68485691281874672, 1.770762539963691484, 12.47495103249912596 ) ) ;
#60495 = EDGE_LOOP ( 'NONE', ( #20469, #57504, #28384, #57568, #54475, #56262, #14951 ) ) ;
#60496 = CARTESIAN_POINT ( 'NONE',  ( 9.734454719592999794, 3.021734963141999852, -6.070209284876999511 ) ) ;
#60497 = CARTESIAN_POINT ( 'NONE',  ( 10.32118582084299874, 3.163839350524900063, -6.533484739457099622 ) ) ;
#60498 = DIRECTION ( 'NONE',  ( 0.000000000000000000, 0.000000000000000000, -1.000000000000000000 ) ) ;
#60500 = CARTESIAN_POINT ( 'NONE',  ( 17.97807132104770744, -0.4608801940066536984, 12.68876176373188258 ) ) ;
#60499 = CARTESIAN_POINT ( 'NONE',  ( 9.331129440379999807, -4.141908960411000429, 6.047561724438000219 ) ) ;
#60501 = CARTESIAN_POINT ( 'NONE',  ( 10.31196314287999982, -3.017187828228399926, 7.707177545471399327 ) ) ;
#60502 = CARTESIAN_POINT ( 'NONE',  ( 11.14595257254739913, -4.831736303435800295, -7.741895249827200232 ) ) ;
#60503 = ORIENTED_EDGE ( 'NONE', *, *, #2910, .F. ) ;
#60504 = AXIS2_PLACEMENT_3D ( 'NONE', #50308, #28647, #61821 ) ;
#60505 = B_SPLINE_CURVE_WITH_KNOTS ( 'NONE', 3,
 ( #19413, #45984, #25687, #13835 ),
 .UNSPECIFIED., .F., .F.,
 ( 4, 4 ),
 ( 0.000000000000000000, 1.000000000000000000 ),
 .UNSPECIFIED. ) ;
#60506 = CARTESIAN_POINT ( 'NONE',  ( 1.019382100425000104, -2.055220836715000221, 2.740599349591000156 ) ) ;
#60507 = CARTESIAN_POINT ( 'NONE',  ( 9.665180073187563892, -2.900412407185302577, -6.162603501924860616 ) ) ;
#60508 = DIRECTION ( 'NONE',  ( 1.000000000000000000, -4.332706595949694629E-15, 1.401268137124204108E-14 ) ) ;
#60509 = CARTESIAN_POINT ( 'NONE',  ( 18.04486049889702670, -2.888348857472848863, 13.58339007193440828 ) ) ;
#60510 = CARTESIAN_POINT ( 'NONE',  ( 7.717918988116000634, 2.852331522235000083, 6.784355039830999523 ) ) ;
#60511 = CARTESIAN_POINT ( 'NONE',  ( 12.80505043854146940, -1.787816316115923732, 13.88537766212463431 ) ) ;
#60512 = CARTESIAN_POINT ( 'NONE',  ( 10.95551210286900101, -4.217228369037729685, 6.243812680477911492 ) ) ;
#60513 = CARTESIAN_POINT ( 'NONE',  ( 5.000000004731000480, 0.05000000473133000417, 3.150000012852999909 ) ) ;
#60514 = CARTESIAN_POINT ( 'NONE',  ( 12.97415039705200179, -12.11604096695999999, -2.033011318525000277 ) ) ;
#60515 = ORIENTED_EDGE ( 'NONE', *, *, #21940, .F. ) ;
#60516 = CARTESIAN_POINT ( 'NONE',  ( 7.375416666664626142, 2.649999999999999467, -7.323285413235579355 ) ) ;
#60517 = CARTESIAN_POINT ( 'NONE',  ( 8.849999778957998942, 4.000000000000000000, 6.500000166194499940 ) ) ;
#60518 = CARTESIAN_POINT ( 'NONE',  ( 7.424327003564875405, -2.348384993112772712, 8.046123069814775874 ) ) ;
#60519 = VECTOR ( 'NONE', #35386, 1000.000000000000000 ) ;
#60520 = CARTESIAN_POINT ( 'NONE',  ( 10.70577346828306453, 5.100000000000000533, -6.304440314035878679 ) ) ;
#60521 = CARTESIAN_POINT ( 'NONE',  ( 1.132929084573000011, 0.9191385115525000371, 3.644662079466999938 ) ) ;
#60522 = ORIENTED_EDGE ( 'NONE', *, *, #55092, .F. ) ;
#60523 = CARTESIAN_POINT ( 'NONE',  ( 10.79212049822984554, 3.170455386494787309, -8.579526322294437790 ) ) ;
#60524 = CARTESIAN_POINT ( 'NONE',  ( 17.89701680218574609, 1.976751596789643850, -12.55823001632907143 ) ) ;
#60525 = CARTESIAN_POINT ( 'NONE',  ( 9.959641781044998865, 5.406625910119999823, 7.700299649248999678 ) ) ;
#60526 = CARTESIAN_POINT ( 'NONE',  ( 11.28949010443639978, 5.000675062740000065, 7.425165037173959703 ) ) ;
#60527 = VECTOR ( 'NONE', #15594, 1000.000000000000114 ) ;
#60528 = EDGE_CURVE ( 'NONE', #50859, #32857, #52757, .T. ) ;
#60529 = EDGE_CURVE ( 'NONE', #12119, #60421, #47318, .T. ) ;
#60530 = CARTESIAN_POINT ( 'NONE',  ( 11.03111947020579819, 3.091200775993899974, -7.174999999999999822 ) ) ;
#60531 = LINE ( 'NONE', #55978, #47198 ) ;
#60532 = CARTESIAN_POINT ( 'NONE',  ( 15.89979320884932612, -5.681736459261024663, -10.98277228430214691 ) ) ;
#60533 = EDGE_CURVE ( 'NONE', #47471, #2054, #13787, .T. ) ;
#60534 = EDGE_CURVE ( 'NONE', #44670, #22409, #56431, .T. ) ;
#60535 = LINE ( 'NONE', #17540, #38840 ) ;
#60536 = DIRECTION ( 'NONE',  ( 0.000000000000000000, 0.000000000000000000, 1.000000000000000000 ) ) ;
#60537 = VERTEX_POINT ( 'NONE', #57109 ) ;
#60538 = CARTESIAN_POINT ( 'NONE',  ( 8.696135841231001251, 3.038023536984999939, -5.861661709981000001 ) ) ;
#60539 = ORIENTED_EDGE ( 'NONE', *, *, #3707, .T. ) ;
#60540 = CARTESIAN_POINT ( 'NONE',  ( 18.09702113181633365, -2.811936484508641865, 13.60234957393456590 ) ) ;
#60541 = CARTESIAN_POINT ( 'NONE',  ( 11.25656651104150008, -3.873914634362100262, -6.228222165170999247 ) ) ;
#60542 = EDGE_LOOP ( 'NONE', ( #62352, #14401, #56507, #52546 ) ) ;
#60543 = CYLINDRICAL_SURFACE ( 'NONE', #3371, 0.6250000000000005551 ) ;
#60544 = CARTESIAN_POINT ( 'NONE',  ( 5.792965594767167659, -1.015451808980873949, 0.5038350337957896441 ) ) ;
#60545 = CARTESIAN_POINT ( 'NONE',  ( 23.66004879239100234, 13.39256445865000167, -3.813547382634999483 ) ) ;
#60546 = CARTESIAN_POINT ( 'NONE',  ( 9.629022744239000176, 5.794335169544999609, 7.414871903737999759 ) ) ;
#60547 = CARTESIAN_POINT ( 'NONE',  ( 24.39664275023335804, -8.810499738035991513, -8.810499738035991513 ) ) ;
#60548 = CARTESIAN_POINT ( 'NONE',  ( 16.86666666233133327, -3.345268057356067359, -11.86064107292373571 ) ) ;
#60549 = CARTESIAN_POINT ( 'NONE',  ( 11.25913761803000135, 3.706864829039000053, -11.29572955805999968 ) ) ;
#60550 = CARTESIAN_POINT ( 'NONE',  ( 11.08752429429999964, -2.871531501602999636, -6.302910744985999791 ) ) ;
#60551 = CARTESIAN_POINT ( 'NONE',  ( 11.04859286640838256, 4.978068212549554339, -8.665561624473726354 ) ) ;
#60552 = DIRECTION ( 'NONE',  ( 1.000000000000000000, 0.000000000000000000, 0.000000000000000000 ) ) ;
#60553 = ORIENTED_EDGE ( 'NONE', *, *, #43451, .F. ) ;
#60554 = EDGE_CURVE ( 'NONE', #57425, #29163, #64188, .T. ) ;
#60555 = CARTESIAN_POINT ( 'NONE',  ( 9.909870477708999204, 2.749999999999999556, 7.249610810850631637 ) ) ;
#60556 = B_SPLINE_CURVE_WITH_KNOTS ( 'NONE', 3,
 ( #59407, #22000, #11857, #53823, #5577, #38784, #37744, #26920, #43346, #59071, #64648, #339, #65690, #38081, #6263, #49266, #60111, #27603 ),
 .UNSPECIFIED., .F., .F.,
 ( 4, 2, 2, 2, 2, 2, 2, 2, 4 ),
 ( 0.000000000000000000, 0.2500000000000080491, 0.3750000000000123235, 0.4375000000000129896, 0.4687500000000133227, 0.5000000000000136557, 0.6250000000000094369, 0.7500000000000052180, 1.000000000000000000 ),
 .UNSPECIFIED. ) ;
#60557 = CONICAL_SURFACE ( 'NONE', #33766, 1.349999998858999906, 0.7853981633972997312 ) ;
#60558 = DIRECTION ( 'NONE',  ( 1.000000000000000000, 0.000000000000000000, 0.000000000000000000 ) ) ;
#60559 = CARTESIAN_POINT ( 'NONE',  ( 10.32936131915000111, -4.919631126329000459, 4.567352568837999449 ) ) ;
#60560 = CARTESIAN_POINT ( 'NONE',  ( 5.000030787343000327, 1.679270695423614956, -1.290525307673968003 ) ) ;
#60561 = CARTESIAN_POINT ( 'NONE',  ( 9.383499245234510511, 2.750003956825025853, 7.663630899194567192 ) ) ;
#60562 = CARTESIAN_POINT ( 'NONE',  ( 12.39818000720378599, 2.025460462753591706, 13.76267819017275507 ) ) ;
#60563 = CARTESIAN_POINT ( 'NONE',  ( 9.351499161061999743, -4.821938821912000073, 8.950150764319998231 ) ) ;
#60564 = ORIENTED_EDGE ( 'NONE', *, *, #10722, .T. ) ;
#60565 = CARTESIAN_POINT ( 'NONE',  ( 24.35365242081700288, -8.326148686889998984, -7.789520173161003314 ) ) ;
#60566 = CARTESIAN_POINT ( 'NONE',  ( 12.41655229043184860, -0.4896942981276220519, 13.88839019180477052 ) ) ;
#60567 = VERTEX_POINT ( 'NONE', #24616 ) ;
#60568 = CARTESIAN_POINT ( 'NONE',  ( 7.605771682457999283, 5.346164515353000191, -7.398308812559000636 ) ) ;
#60569 = DIRECTION ( 'NONE',  ( 0.000000000000000000, 0.9586234969520801563, 0.2846769943134941361 ) ) ;
#60570 = CARTESIAN_POINT ( 'NONE',  ( 24.02990352322499845, -3.726800819761000305, -13.01750903018000116 ) ) ;
#60571 = CARTESIAN_POINT ( 'NONE',  ( 11.04677151279999947, -2.764386413791999786, -5.039776830043000366 ) ) ;
#60572 = VECTOR ( 'NONE', #8018, 1000.000000000000114 ) ;
#60573 = CARTESIAN_POINT ( 'NONE',  ( 8.590779719591999708, 2.836879604150999601, -8.783908972046001296 ) ) ;
#60574 = EDGE_CURVE ( 'NONE', #28137, #34321, #5011, .T. ) ;
#60575 = FACE_OUTER_BOUND ( 'NONE', #64267, .T. ) ;
#60576 = CARTESIAN_POINT ( 'NONE',  ( 10.99479839230999900, -3.850614833844999918, -9.347951988117998212 ) ) ;
#60577 = DIRECTION ( 'NONE',  ( -1.000000000000000000, 0.000000000000000000, 0.000000000000000000 ) ) ;
#60578 = CARTESIAN_POINT ( 'NONE',  ( 24.53428991195500330, 3.614319144953999530, 12.31267516478999902 ) ) ;
#60579 = EDGE_CURVE ( 'NONE', #47477, #43973, #26286, .T. ) ;
#60580 =( LENGTH_UNIT ( ) NAMED_UNIT ( * ) SI_UNIT ( .MILLI., .METRE. ) );
#60581 = CARTESIAN_POINT ( 'NONE',  ( 9.260142521132999960, -3.283392111224999965, -8.676955243274001361 ) ) ;
#60582 = CARTESIAN_POINT ( 'NONE',  ( 11.29364426047339975, 4.466097552695299733, -8.230103870496201068 ) ) ;
#60583 = DIRECTION ( 'NONE',  ( 0.000000000000000000, 0.000000000000000000, 1.000000000000000000 ) ) ;
#60584 = CARTESIAN_POINT ( 'NONE',  ( 10.56080513895999928, 5.026880838510000338, -6.929150654994399083 ) ) ;
#60585 = CARTESIAN_POINT ( 'NONE',  ( 8.773468108405998223, 4.966402032527499344, -7.773695785133000413 ) ) ;
#60587 = CARTESIAN_POINT ( 'NONE',  ( 10.26948634882999833, -3.369491526607000242, 4.845903792981999914 ) ) ;
#60586 = CARTESIAN_POINT ( 'NONE',  ( 9.302265421554999136, -4.188500707411799695, 6.524915741324599949 ) ) ;
#60588 = CARTESIAN_POINT ( 'NONE',  ( 9.268025422169147376, -5.100000000000000533, 6.452077467066149374 ) ) ;
#60589 = ORIENTED_EDGE ( 'NONE', *, *, #5349, .T. ) ;
#60590 = CARTESIAN_POINT ( 'NONE',  ( 10.43614141025499897, 4.549633050978300730, 6.521048559232099251 ) ) ;
#60591 = CARTESIAN_POINT ( 'NONE',  ( 9.075489683949001574, -4.020837068201999820, 8.948702918089999514 ) ) ;
#60592 = CARTESIAN_POINT ( 'NONE',  ( 10.31558376188599802, 3.037118682679400106, 6.886327436977599525 ) ) ;
#60593 = CARTESIAN_POINT ( 'NONE',  ( 9.606837339593626623, 3.135127465292355087, -7.367607524272325570 ) ) ;
#60594 = CARTESIAN_POINT ( 'NONE',  ( 10.93227479887999998, -2.539880901735999785, 6.453614191797999666 ) ) ;
#60595 = CARTESIAN_POINT ( 'NONE',  ( 9.979272590049129477, -2.371809606018679517, 6.860647176154606619 ) ) ;
#60596 = CARTESIAN_POINT ( 'NONE',  ( 11.72754826524499983, 3.413272067235999963, -11.89753034518999897 ) ) ;
#60597 = ORIENTED_EDGE ( 'NONE', *, *, #15998, .F. ) ;
#60598 = CARTESIAN_POINT ( 'NONE',  ( 8.697480666858998788, -3.665111009453500213, -8.446938520915798776 ) ) ;
#60599 = AXIS2_PLACEMENT_3D ( 'NONE', #1262, #22576, #27488 ) ;
#60600 = CARTESIAN_POINT ( 'NONE',  ( 10.98768472569999943, 5.449702578894000560, 4.945212061318999375 ) ) ;
#60601 = CARTESIAN_POINT ( 'NONE',  ( 6.125178865300000552, -1.528745275297999973, -0.5198780721924000092 ) ) ;
#60602 = CARTESIAN_POINT ( 'NONE',  ( 23.60000000000000142, 0.000000000000000000, 0.000000000000000000 ) ) ;
#60603 = CARTESIAN_POINT ( 'NONE',  ( 11.49999672495000524, 11.45771900890041728, -2.434039779711009821 ) ) ;
#60604 = CARTESIAN_POINT ( 'NONE',  ( 11.69518313518939934, -4.537300658085600347, 6.820583637845799352 ) ) ;
#60605 = CARTESIAN_POINT ( 'NONE',  ( 11.31410538575739899, 4.975963290822400076, -7.266662245194900116 ) ) ;
#60606 = CARTESIAN_POINT ( 'NONE',  ( 12.18501279888951316, 2.418803504819920125, -13.69036126157237732 ) ) ;
#60607 = CARTESIAN_POINT ( 'NONE',  ( 9.658740731405000446, -5.476443305113000370, -7.051545409824000465 ) ) ;
#60608 = CARTESIAN_POINT ( 'NONE',  ( 11.36486084871759950, 2.792989229543000107, -7.825000000000000178 ) ) ;
#60609 = ORIENTED_EDGE ( 'NONE', *, *, #26995, .T. ) ;
#60610 = CARTESIAN_POINT ( 'NONE',  ( 18.20361801367284826, 2.140066979998675123, -13.83614404522070096 ) ) ;
#60611 = EDGE_CURVE ( 'NONE', #59647, #23464, #36917, .T. ) ;
#60612 = CARTESIAN_POINT ( 'NONE',  ( 12.61664971283087233, -0.7055305429986125088, -13.98221279804358019 ) ) ;
#60613 = EDGE_CURVE ( 'NONE', #55988, #54460, #29650, .T. ) ;
#60614 = CARTESIAN_POINT ( 'NONE',  ( 8.379056333468048123, 2.650684137603387835, -7.263287199838283748 ) ) ;
#60615 = CARTESIAN_POINT ( 'NONE',  ( 24.95773344659900062, -8.510917023874998932, -8.990083141738999473 ) ) ;
#60616 = CARTESIAN_POINT ( 'NONE',  ( 10.46684687351657672, -4.768183399968645375, -8.499583552997723501 ) ) ;
#60617 = FACE_OUTER_BOUND ( 'NONE', #53106, .T. ) ;
#60618 = CARTESIAN_POINT ( 'NONE',  ( 5.000030787343000327, 2.099962892530999881, 0.000000000000000000 ) ) ;
#60619 = EDGE_LOOP ( 'NONE', ( #7678, #27312, #44156, #24245, #30258 ) ) ;
#60620 = CARTESIAN_POINT ( 'NONE',  ( 0.1189017606508744468, -1.063211791521875504, -2.979546336419315544 ) ) ;
#60621 = CARTESIAN_POINT ( 'NONE',  ( 17.85663772380316061, 3.182036958951508954, -13.63358608099387403 ) ) ;
#60622 = VERTEX_POINT ( 'NONE', #48690 ) ;
#60623 = CARTESIAN_POINT ( 'NONE',  ( 8.445233760363150211, 5.313925467271168657, 7.853812692271652907 ) ) ;
#60624 = CARTESIAN_POINT ( 'NONE',  ( 8.610058059625000482, -5.329429281359999493, 6.027400270608000099 ) ) ;
#60625 = CARTESIAN_POINT ( 'NONE',  ( 8.406645280410000254, 3.807713920470999991, -9.221758713517999695 ) ) ;
#60626 = CARTESIAN_POINT ( 'NONE',  ( 11.62299956498149989, -2.792989229543000107, 7.174999999999999822 ) ) ;
#60627 = CARTESIAN_POINT ( 'NONE',  ( 11.80233327354039830, -5.101536739857000846, -6.779499720266399798 ) ) ;
#60628 = CARTESIAN_POINT ( 'NONE',  ( 17.94896820972214613, 0.4852478460479964784, -12.68752000237319066 ) ) ;
#60629 = DIRECTION ( 'NONE',  ( -1.000000000000000000, 0.000000000000000000, 0.000000000000000000 ) ) ;
#60630 = ORIENTED_EDGE ( 'NONE', *, *, #44290, .T. ) ;
#60631 = CARTESIAN_POINT ( 'NONE',  ( 9.199609130449999839, -2.551382302226000487, 7.536606162076999738 ) ) ;
#60632 = CARTESIAN_POINT ( 'NONE',  ( 18.17228756843369197, -2.598712620565390097, -13.65197972922593017 ) ) ;
#60633 = CARTESIAN_POINT ( 'NONE',  ( 9.594139158774000364, 2.212639797530000063, -6.855876382544999537 ) ) ;
#60634 = ORIENTED_EDGE ( 'NONE', *, *, #41319, .T. ) ;
#60635 = ADVANCED_FACE ( 'NONE', ( #32956 ), #48340, .F. ) ;
#60636 = CARTESIAN_POINT ( 'NONE',  ( 10.93146722582000052, 2.472885155055999817, -7.514158739122999364 ) ) ;
#60637 = B_SPLINE_CURVE_WITH_KNOTS ( 'NONE', 3,
 ( #4608, #51818, #25942, #36431 ),
 .UNSPECIFIED., .F., .F.,
 ( 4, 4 ),
 ( 0.000000000000000000, 1.000000000000000000 ),
 .UNSPECIFIED. ) ;
#60638 = ORIENTED_EDGE ( 'NONE', *, *, #37135, .F. ) ;
#60639 = CARTESIAN_POINT ( 'NONE',  ( 9.811963142879999822, 4.982812171771600518, 7.707177545471399327 ) ) ;
#60640 = CARTESIAN_POINT ( 'NONE',  ( 18.18564075751668341, -2.124969003714949345, -12.41952547471440660 ) ) ;
#60641 = CARTESIAN_POINT ( 'NONE',  ( 10.90437356726000040, -2.900476673752999890, 5.132566153004000320 ) ) ;
#60642 = FACE_OUTER_BOUND ( 'NONE', #51841, .T. ) ;
#60643 = CARTESIAN_POINT ( 'NONE',  ( 23.89320776801300283, 3.288740538451999651, 12.20874841473999872 ) ) ;
#60644 = CARTESIAN_POINT ( 'NONE',  ( 8.750151519676999001, 4.018750234858180725, 6.633192605878799775 ) ) ;
#60645 = CARTESIAN_POINT ( 'NONE',  ( 6.829431761257999334, -9.270817568204998693, -5.218560984457999652 ) ) ;
#60646 = VERTEX_POINT ( 'NONE', #5343 ) ;
#60647 = DIRECTION ( 'NONE',  ( 0.000000000000000000, -0.7071067811865475727, 0.7071067811865475727 ) ) ;
#60648 = CARTESIAN_POINT ( 'NONE',  ( 10.75102028041000146, 2.478469530773999896, -7.438303846328000013 ) ) ;
#60649 = PLANE ( 'NONE',  #60898 ) ;
#60650 = CARTESIAN_POINT ( 'NONE',  ( 12.43942356506265590, 3.006998533878516788, -13.55276137517231838 ) ) ;
#60651 = AXIS2_PLACEMENT_3D ( 'NONE', #11056, #27482, #38661 ) ;
#60652 = CARTESIAN_POINT ( 'NONE',  ( 10.29226717315700057, -4.973628086880700572, -6.670281532133299329 ) ) ;
#60653 = CARTESIAN_POINT ( 'NONE',  ( 9.843726350706999639, -4.115123626494000320, 9.466607949400000166 ) ) ;
#60654 = CARTESIAN_POINT ( 'NONE',  ( 17.85480509960783380, -0.6653129401483779404, 13.98418548573915743 ) ) ;
#60655 = CARTESIAN_POINT ( 'NONE',  ( 17.81146176625148314, 0.5702785222608648397, 13.88425216382746541 ) ) ;
#60656 = ORIENTED_EDGE ( 'NONE', *, *, #27615, .F. ) ;
#60657 = ORIENTED_EDGE ( 'NONE', *, *, #54256, .F. ) ;
#60658 = CARTESIAN_POINT ( 'NONE',  ( 8.690229719593000723, 2.414630869937000046, -6.801495146585999407 ) ) ;
#60659 = EDGE_CURVE ( 'NONE', #45966, #52078, #7266, .T. ) ;
#60660 = CARTESIAN_POINT ( 'NONE',  ( 12.21236231058155042, 0.1994024997942437372, 13.89809293279921754 ) ) ;
#60661 = CARTESIAN_POINT ( 'NONE',  ( 12.18001976712855772, -2.492954602552174048, 13.67495394281278642 ) ) ;
#60662 = CARTESIAN_POINT ( 'NONE',  ( 23.56697384540236939, 3.042303125952126486, -13.65541767842539933 ) ) ;
#60663 = CARTESIAN_POINT ( 'NONE',  ( 8.705995559625000269, -2.542850487891999745, 7.419808283050000064 ) ) ;
#60664 = DIRECTION ( 'NONE',  ( -1.000000000000000000, -5.940303223299999030E-14, -1.603881870291000016E-12 ) ) ;
#60666 = CARTESIAN_POINT ( 'NONE',  ( 16.39999999231800132, 3.216285993016000155, 11.40340220863999932 ) ) ;
#60665 = CARTESIAN_POINT ( 'NONE',  ( 10.08305105205200114, -2.744602294987000146, 7.254315263553399618 ) ) ;
#60667 = VECTOR ( 'NONE', #8926, 1000.000000000000114 ) ;
#60668 = CARTESIAN_POINT ( 'NONE',  ( 10.61656919669529842, 5.225637333137999718, -7.862118085997298778 ) ) ;
#60669 = EDGE_LOOP ( 'NONE', ( #14305, #10587 ) ) ;
#60670 = CARTESIAN_POINT ( 'NONE',  ( 12.35913878034446611, -0.5835546240207333257, 13.98799446466930263 ) ) ;
#60671 = CIRCLE ( 'NONE', #57315, 3.200000000000000178 ) ;
#60672 = CARTESIAN_POINT ( 'NONE',  ( 10.45746213570999927, 5.100000000000000533, -6.571291218949999902 ) ) ;
#60673 = CARTESIAN_POINT ( 'NONE',  ( 7.877465161153600626, 5.139684818804880706, 6.768899810017460439 ) ) ;
#60674 = CARTESIAN_POINT ( 'NONE',  ( 12.76431688229904537, -0.6240105543035401325, 12.67935574133242582 ) ) ;
#60675 = CARTESIAN_POINT ( 'NONE',  ( 18.07102077504177728, -2.852831731489053446, -12.36232801722093555 ) ) ;
#60676 = ORIENTED_EDGE ( 'NONE', *, *, #67430, .T. ) ;
#60678 = CARTESIAN_POINT ( 'NONE',  ( 9.573148997458000409, 5.167567567567999731, -6.822293592207000934 ) ) ;
#60677 = CARTESIAN_POINT ( 'NONE',  ( 23.66004879239100234, -3.393653467490999720, 13.50507469661999949 ) ) ;
#60679 = CARTESIAN_POINT ( 'NONE',  ( 9.410004719593999312, 2.495531372253999791, -7.930944806125000746 ) ) ;
#60680 = CARTESIAN_POINT ( 'NONE',  ( 12.47202999840593129, -1.970716439074158943, 13.77157652140723876 ) ) ;
#60681 = CARTESIAN_POINT ( 'NONE',  ( 8.295839940244002619, -5.118638632597003912, 6.383292232312004266 ) ) ;
#60682 = CARTESIAN_POINT ( 'NONE',  ( 8.200000998245998929, 3.037570195374000164E-13, -12.49999978039658544 ) ) ;
#60683 = CARTESIAN_POINT ( 'NONE',  ( 11.59999999999999964, -4.817420948848700313, -7.174999999999999822 ) ) ;
#60684 = CARTESIAN_POINT ( 'NONE',  ( 3.072112146792000065, 3.006932304320000249, -1.965249848430999924 ) ) ;
#60685 = ORIENTED_EDGE ( 'NONE', *, *, #60613, .F. ) ;
#60686 = CARTESIAN_POINT ( 'NONE',  ( 12.10431270533525350, 0.1860047152749561838, -12.59864695008082869 ) ) ;
#60687 = CARTESIAN_POINT ( 'NONE',  ( 24.60109543021109602, -12.20853568610929329, 3.061026903515568165 ) ) ;
#60688 = CARTESIAN_POINT ( 'NONE',  ( 24.05250961456292913, -12.62704480724583078, -3.430091672397665103 ) ) ;
#60689 = CARTESIAN_POINT ( 'NONE',  ( 7.641204719590000138, 4.524487726177000013, 9.047753146378999745 ) ) ;
#60690 = ORIENTED_EDGE ( 'NONE', *, *, #13282, .T. ) ;
#60691 = CARTESIAN_POINT ( 'NONE',  ( 6.832448840113999999, -0.8351886993729999986, 1.025064727650000007 ) ) ;
#60692 = ADVANCED_FACE ( 'NONE', ( #27719 ), #21762, .T. ) ;
#60693 = EDGE_CURVE ( 'NONE', #12534, #24760, #58574, .T. ) ;
#60694 = CARTESIAN_POINT ( 'NONE',  ( 10.95262535236630086, 9.076036533295676278, 6.378678306765203310 ) ) ;
#60696 = CARTESIAN_POINT ( 'NONE',  ( 7.844724277266999835, 4.719412473309000156, 6.357657803787000184 ) ) ;
#60695 = DIRECTION ( 'NONE',  ( 0.000000000000000000, -0.7614089499631907509, -0.6482718649732928107 ) ) ;
#60697 = CARTESIAN_POINT ( 'NONE',  ( 10.72191429142990060, 4.025072603369280522, -6.183971186511000084 ) ) ;
#60698 = ORIENTED_EDGE ( 'NONE', *, *, #35747, .F. ) ;
#60699 = AXIS2_PLACEMENT_3D ( 'NONE', #54457, #6558, #49210 ) ;
#60700 = CARTESIAN_POINT ( 'NONE',  ( -0.2999999999999999889, 0.5773502691895999739, -1.000000000000000000 ) ) ;
#60701 = VERTEX_POINT ( 'NONE', #68623 ) ;
#60702 = CARTESIAN_POINT ( 'NONE',  ( 9.492234138830133006, -4.893440334305921624, 8.512184316248376348 ) ) ;
#60703 = CARTESIAN_POINT ( 'NONE',  ( 25.34044016535778354, -2.679925846854998905, -11.33984901862687167 ) ) ;
#60704 = CARTESIAN_POINT ( 'NONE',  ( 18.22962728801297416, 0.2678304234474076506, -13.99744223245316199 ) ) ;
#60705 = ORIENTED_EDGE ( 'NONE', *, *, #11448, .F. ) ;
#60706 = CARTESIAN_POINT ( 'NONE',  ( 10.98606062297321806, 8.050563008166918166, -6.521190260545529860 ) ) ;
#60707 = CARTESIAN_POINT ( 'NONE',  ( 18.30017264560542145, -0.9191760148722679657, 11.85014035458664772 ) ) ;
#60708 = CARTESIAN_POINT ( 'NONE',  ( 8.038039158770001080, 5.092576903264999899, -6.628615687103999399 ) ) ;
#60709 = CARTESIAN_POINT ( 'NONE',  ( 9.614639751325485761, -2.815014287255568348, 7.040280035170891182 ) ) ;
#60710 = CARTESIAN_POINT ( 'NONE',  ( 5.452606837613999780, -0.4199405305951999789, 1.440017343911000003 ) ) ;
#60711 = VERTEX_POINT ( 'NONE', #11274 ) ;
#60712 = CARTESIAN_POINT ( 'NONE',  ( 24.53429010490700080, 8.855930189872001534, 9.286429716155000236 ) ) ;
#60713 = CARTESIAN_POINT ( 'NONE',  ( 12.76382664775976750, -3.125000000000000444, -13.52078629068866533 ) ) ;
#60714 = EDGE_CURVE ( 'NONE', #23464, #46101, #63378, .T. ) ;
#60715 = CARTESIAN_POINT ( 'NONE',  ( 0.000000000000000000, 0.000000000000000000, 0.000000000000000000 ) ) ;
#60716 = AXIS2_PLACEMENT_3D ( 'NONE', #35932, #57245, #14950 ) ;
#60717 = DIRECTION ( 'NONE',  ( -0.000000000000000000, 0.6884191022827191864, 0.7253131321107147977 ) ) ;
#60718 = ORIENTED_EDGE ( 'NONE', *, *, #4039, .T. ) ;
#60719 = CARTESIAN_POINT ( 'NONE',  ( 10.71654240785884582, -2.829812247203900899, 6.826803421738888211 ) ) ;
#60720 = EDGE_CURVE ( 'NONE', #24854, #40590, #15502, .T. ) ;
#60721 = CIRCLE ( 'NONE', #48442, 1.999999999999999778 ) ;
#60722 = CARTESIAN_POINT ( 'NONE',  ( 8.942941355974880935, -4.954666522228586167, -6.948775311896397966 ) ) ;
#60723 = CARTESIAN_POINT ( 'NONE',  ( 24.30000000000000071, -10.83443035398000021, -3.855530949778000149 ) ) ;
#60724 = CARTESIAN_POINT ( 'NONE',  ( 9.973631561148998514, -4.684311564990208510, -8.575598637068459595 ) ) ;
#60725 = CARTESIAN_POINT ( 'NONE',  ( 11.09999999999999964, -1.300000000000000044, -10.46294468575422876 ) ) ;
#60726 = CARTESIAN_POINT ( 'NONE',  ( 6.013359839683499075, -1.310679582531389276, 0.7554284705563443225 ) ) ;
#60727 = CARTESIAN_POINT ( 'NONE',  ( 17.76260332629192717, -3.089553855563651918, 12.29447117690774149 ) ) ;
#60728 = ORIENTED_EDGE ( 'NONE', *, *, #14218, .T. ) ;
#60729 = SHAPE_REPRESENTATION ( 'Terminal Screw', ( #9676 ), #9731 ) ;
#60730 = CARTESIAN_POINT ( 'NONE',  ( 11.15278751119019773, -4.790480620979200133, -7.913556523549700294 ) ) ;
#60731 = ORIENTED_EDGE ( 'NONE', *, *, #28896, .F. ) ;
#60732 = CARTESIAN_POINT ( 'NONE',  ( 18.14737500098294376, 2.299536442365951228, 13.71390152310211974 ) ) ;
#60733 = CARTESIAN_POINT ( 'NONE',  ( 9.295789158775001226, 5.835196551504000517, -7.008466539623000813 ) ) ;
#60734 = CARTESIAN_POINT ( 'NONE',  ( 2.293573906239000149, 2.743716934200000068, -1.972779657783999996 ) ) ;
#60735 = CARTESIAN_POINT ( 'NONE',  ( 9.819572261909000233, -2.688237737290000151, -7.873041261681999359 ) ) ;
#60736 = CARTESIAN_POINT ( 'NONE',  ( 25.29987667925500361, 10.83443035398000021, 3.855530949778000149 ) ) ;
#60737 = CARTESIAN_POINT ( 'NONE',  ( 8.066302634316002695, 3.111242948840002409, -6.203702194951995708 ) ) ;
#60738 = DIRECTION ( 'NONE',  ( 0.000000000000000000, -1.000000000000000000, 0.000000000000000000 ) ) ;
#60739 = EDGE_LOOP ( 'NONE', ( #25964, #54192, #48637, #18682, #14350 ) ) ;
#60740 = CARTESIAN_POINT ( 'NONE',  ( 27.64127793187000037, 5.599999999999999645, -6.571291218949999902 ) ) ;
#60741 = CARTESIAN_POINT ( 'NONE',  ( 11.88795122972049967, -3.601717549869600354, 8.421043941822800249 ) ) ;
#60742 = CARTESIAN_POINT ( 'NONE',  ( 10.03490996941999924, 5.615906393494999982, 7.351455918368999143 ) ) ;
#60743 = CARTESIAN_POINT ( 'NONE',  ( 10.85460595134973794, -2.649926015912494215, -7.676664732030310745 ) ) ;
#60744 = CARTESIAN_POINT ( 'NONE',  ( 0.7000000000000000666, 1.154700538379000108, 0.000000000000000000 ) ) ;
#60745 = CARTESIAN_POINT ( 'NONE',  ( 11.00833333333434183, 3.620091288824011766, 8.928205453214854259 ) ) ;
#60746 = VECTOR ( 'NONE', #44781, 1000.000000000000000 ) ;
#60747 = CARTESIAN_POINT ( 'NONE',  ( 10.87518447801629939, 4.865987311498500389, -7.480906371072489236 ) ) ;
#60748 = CARTESIAN_POINT ( 'NONE',  ( 4.500000000000000000, 0.000000000000000000, 0.000000000000000000 ) ) ;
#60749 = ADVANCED_FACE ( 'NONE', ( #59173 ), #61969, .T. ) ;
#60750 = EDGE_CURVE ( 'NONE', #67010, #15838, #62652, .T. ) ;
#60751 = CARTESIAN_POINT ( 'NONE',  ( 10.39157120343299923, 3.944651031655580287, -8.640469672413999547 ) ) ;
#60752 = CARTESIAN_POINT ( 'NONE',  ( 23.51521052042600246, -10.47031424384000076, 9.494913483761999728 ) ) ;
#60753 = CARTESIAN_POINT ( 'NONE',  ( 0.8414471766558753174, -1.482381544592732414, -3.195448105648677650 ) ) ;
#60754 = CARTESIAN_POINT ( 'NONE',  ( 10.10735778041000010, 4.293584699549000128, -8.994197232567001876 ) ) ;
#60755 = EDGE_LOOP ( 'NONE', ( #47679, #39378, #12807, #14378, #16622 ) ) ;
#60756 = CARTESIAN_POINT ( 'NONE',  ( 7.501441940376999185, -2.138201851198999748, 6.814774777484000623 ) ) ;
#60757 = CARTESIAN_POINT ( 'NONE',  ( 17.57587588171168136, 3.124999410540973521, 13.52078618842886115 ) ) ;
#60758 = CARTESIAN_POINT ( 'NONE',  ( 24.35365242081699932, -1.906711579001001189, 11.36048031431998595 ) ) ;
#60759 = CARTESIAN_POINT ( 'NONE',  ( 10.41964694612699915, -5.186980343482999523, -7.973702485506099613 ) ) ;
#60760 = VERTEX_POINT ( 'NONE', #1483 ) ;
#60761 = AXIS2_PLACEMENT_3D ( 'NONE', #34647, #44789, #12619 ) ;
#60762 = B_SPLINE_CURVE_WITH_KNOTS ( 'NONE', 3,
 ( #2225, #39981, #45222, #17257, #55015, #54313 ),
 .UNSPECIFIED., .F., .F.,
 ( 4, 2, 4 ),
 ( 0.000000000000000000, 0.5000000000000000000, 1.000000000000000000 ),
 .UNSPECIFIED. ) ;
#60763 = CARTESIAN_POINT ( 'NONE',  ( 8.898551658772998252, 5.146726419831999522, 6.597424767138000412 ) ) ;
#60764 = CIRCLE ( 'NONE', #25035, 12.24999851416000141 ) ;
#60766 = CARTESIAN_POINT ( 'NONE',  ( 11.84388784977539899, 2.744254309011999737, 7.571757098260779806 ) ) ;
#60765 = CARTESIAN_POINT ( 'NONE',  ( 10.32055864497999842, -3.317414799430800088, -8.034587760591801242 ) ) ;
#60767 = CARTESIAN_POINT ( 'NONE',  ( 10.26693915877000052, 5.500023470133998948, -6.419501519420999891 ) ) ;
#60768 = ORIENTED_EDGE ( 'NONE', *, *, #65506, .T. ) ;
#60769 = CARTESIAN_POINT ( 'NONE',  ( 10.55813337864000090, 2.466561068647000532, 6.633529813744000414 ) ) ;
#60770 = CARTESIAN_POINT ( 'NONE',  ( 25.46375345652300126, 2.879422156700999658, -11.30951020355999859 ) ) ;
#60771 = CARTESIAN_POINT ( 'NONE',  ( 10.52226222744799955, 3.119510978356100139, 6.774721295617600170 ) ) ;
#60772 = CARTESIAN_POINT ( 'NONE',  ( 10.22399006116000031, -5.507891002176999784, 6.589804341508000540 ) ) ;
#60773 = CARTESIAN_POINT ( 'NONE',  ( 8.577620559625000141, -3.981661727120999750, 8.959239802162999311 ) ) ;
#60774 = ORIENTED_EDGE ( 'NONE', *, *, #22329, .F. ) ;
#60775 = CARTESIAN_POINT ( 'NONE',  ( 11.61689913334100055, -3.709679022145000005, 12.00356807880999988 ) ) ;
#60776 = EDGE_CURVE ( 'NONE', #35849, #21130, #64251, .T. ) ;
#60777 = EDGE_CURVE ( 'NONE', #51100, #64627, #7551, .T. ) ;
#60778 = CARTESIAN_POINT ( 'NONE',  ( 10.31152944037999930, -2.716820959546999870, -7.950167805575999225 ) ) ;
#60779 = CARTESIAN_POINT ( 'NONE',  ( 7.898990479458490199, -2.593905526383240012, 8.523572096125727526 ) ) ;
#60780 = CARTESIAN_POINT ( 'NONE',  ( 10.09697182628999990, -5.253379538902000156, 8.530665717066000298 ) ) ;
#60781 = FACE_OUTER_BOUND ( 'NONE', #13935, .T. ) ;
#60782 = CARTESIAN_POINT ( 'NONE',  ( 9.803367640780999537, -3.461752753411900141, 8.506987760366000018 ) ) ;
#60783 = ORIENTED_EDGE ( 'NONE', *, *, #10269, .T. ) ;
#60784 = LINE ( 'NONE', #55546, #61173 ) ;
#60785 = EDGE_CURVE ( 'NONE', #40269, #17831, #59764, .T. ) ;
#60786 = CARTESIAN_POINT ( 'NONE',  ( 11.68272066707849888, -2.906477115133000222, 8.161456030935699602 ) ) ;
#60787 = ORIENTED_EDGE ( 'NONE', *, *, #62564, .T. ) ;
#60788 = CARTESIAN_POINT ( 'NONE',  ( 18.49993212792200126, -2.908182645667999999, -12.18276646858999968 ) ) ;
#60789 = ORIENTED_EDGE ( 'NONE', *, *, #44680, .T. ) ;
#60790 = B_SPLINE_SURFACE_WITH_KNOTS ( 'NONE', 3, 3, ( 
 ( #3916, #58440, #63328, #62648 ),
 ( #36780, #25602, #15793, #25250 ),
 ( #58102, #10205, #52162, #31538 ),
 ( #4265, #14771, #37124, #46589 ),
 ( #52857, #20014, #67896, #57403 ),
 ( #4956, #9508, #46929, #20352 ),
 ( #41676, #65046, #38494, #32909 ),
 ( #38142, #22408, #7026, #59468 ),
 ( #38851, #60174, #17161, #28017 ),
 ( #33606, #11566, #32234, #54223 ),
 ( #1439, #6321, #53547, #27672 ),
 ( #12280, #48646, #49324, #1097 ) ),
 .UNSPECIFIED., .F., .F., .F.,
 ( 4, 1, 1, 1, 1, 1, 1, 1, 1, 4 ),
 ( 4, 4 ),
 ( 0.5527776740318000037, 0.5999999999999999778, 0.6500000000000000222, 0.6999999999999999556, 0.7500000000000000000, 0.8000000000000000444, 0.8499999999999999778, 0.9000000000000000222, 0.9499999999999999556, 0.9893859725818999751 ),
 ( -0.2706685848836000163, 1.270789706183999890 ),
 .UNSPECIFIED. ) ;
#60791 = CARTESIAN_POINT ( 'NONE',  ( 10.01574583856000089, -4.333399685216000385, -9.088699530815999239 ) ) ;
#60792 = CARTESIAN_POINT ( 'NONE',  ( 9.790085841230000696, 5.149303692842000402, -5.987168472229000393 ) ) ;
#60793 = DIRECTION ( 'NONE',  ( 0.000000000000000000, 0.000000000000000000, 1.000000000000000000 ) ) ;
#60794 = CARTESIAN_POINT ( 'NONE',  ( 8.244294876368201130, 4.976357605550050245, 6.306308086258407997 ) ) ;
#60795 = CARTESIAN_POINT ( 'NONE',  ( 12.41914228198395698, 3.089530644545721128, -12.21535262842080805 ) ) ;
#60796 = CARTESIAN_POINT ( 'NONE',  ( 11.93302763632549990, -5.035790660926999784, 7.977941233841399971 ) ) ;
#60797 = CARTESIAN_POINT ( 'NONE',  ( 12.06322412107030928, -3.945399343424460525, 8.532060764998998792 ) ) ;
#60798 = EDGE_LOOP ( 'NONE', ( #22776, #51452, #45622, #64502 ) ) ;
#60799 = CARTESIAN_POINT ( 'NONE',  ( 9.635596873516668381, 5.092232985442826099, 8.129523725463617012 ) ) ;
#60800 = CIRCLE ( 'NONE', #30655, 0.8000000000000002665 ) ;
#60801 = ORIENTED_EDGE ( 'NONE', *, *, #42317, .T. ) ;
#60802 = CARTESIAN_POINT ( 'NONE',  ( 8.919605646795000453, -5.165500668528999917, 8.645534272955000432 ) ) ;
#60803 = CARTESIAN_POINT ( 'NONE',  ( 24.30000000000000071, -2.078227429405999693, 11.31065739696999906 ) ) ;
#60804 = ORIENTED_EDGE ( 'NONE', *, *, #58305, .F. ) ;
#60805 = B_SPLINE_SURFACE_WITH_KNOTS ( 'NONE', 3, 3, ( 
 ( #5605, #36402, #4234, #25574 ),
 ( #47243, #10179, #30819, #57719 ),
 ( #15077, #19988, #9477, #10858 ),
 ( #36755, #47930, #25912, #31854 ),
 ( #9827, #47591, #10514, #37430 ),
 ( #63649, #68546, #68897, #52828 ) ),
 .UNSPECIFIED., .F., .F., .F.,
 ( 4, 1, 1, 4 ),
 ( 4, 4 ),
 ( 0.1811037619699999990, 0.3333333333333000081, 0.6666666666667000474, 0.8725156331704999602 ),
 ( -0.1256563615239000009, 1.125656361510000147 ),
 .UNSPECIFIED. ) ;
#60806 = CARTESIAN_POINT ( 'NONE',  ( 12.53569427112577372, -1.812281311417189178, -12.46898785302652080 ) ) ;
#60807 = ADVANCED_FACE ( 'NONE', ( #44837 ), #54623, .F. ) ;
#60808 = CARTESIAN_POINT ( 'NONE',  ( 11.45764291764649911, 2.867875922590999771, 7.639947095788999221 ) ) ;
#60809 = CARTESIAN_POINT ( 'NONE',  ( 10.38053305961999939, -5.283785200568999585, -8.830188095997000275 ) ) ;
#60810 = CARTESIAN_POINT ( 'NONE',  ( 18.15645116484899901, -11.61859527604000064, 4.781095881906999523 ) ) ;
#60811 = DIRECTION ( 'NONE',  ( 0.000000000000000000, -0.1218274111675001214, -0.9925512993736016476 ) ) ;
#60812 = CARTESIAN_POINT ( 'NONE',  ( 12.70159504149946805, -3.116720374454505116, -13.52307403002092556 ) ) ;
#60813 = CARTESIAN_POINT ( 'NONE',  ( 18.17001854112162462, 0.1120021961262575583, -12.69934078656688925 ) ) ;
#60814 = CARTESIAN_POINT ( 'NONE',  ( 11.14595257254739913, -4.831736303435800295, -7.741895249827200232 ) ) ;
#60815 = CARTESIAN_POINT ( 'NONE',  ( 10.20226357027499908, -2.879914860223000250, -7.716099591766099053 ) ) ;
#60816 = CARTESIAN_POINT ( 'NONE',  ( 7.283509992105000386, 4.426928431836000044, 9.293321981113999541 ) ) ;
#60817 = ORIENTED_EDGE ( 'NONE', *, *, #14526, .T. ) ;
#60818 = CIRCLE ( 'NONE', #64139, 2.000000000000000444 ) ;
#60819 = FACE_OUTER_BOUND ( 'NONE', #1906, .T. ) ;
#60820 = CARTESIAN_POINT ( 'NONE',  ( 7.460114837477927807, 5.349842312901899710, 7.234364343742836212 ) ) ;
#60821 = B_SPLINE_CURVE_WITH_KNOTS ( 'NONE', 3,
 ( #28949, #43980, #66321, #17045 ),
 .UNSPECIFIED., .F., .F.,
 ( 4, 4 ),
 ( 0.000000000000000000, 1.000000000000000000 ),
 .UNSPECIFIED. ) ;
#60822 = CARTESIAN_POINT ( 'NONE',  ( 24.33740572418300019, -3.364255348473000229, 12.26555798179999890 ) ) ;
#60823 = CIRCLE ( 'NONE', #18410, 14.00000000000000000 ) ;
#60824 = CARTESIAN_POINT ( 'NONE',  ( 18.12635565526706216, 2.245741716918843167, 12.50718761097852472 ) ) ;
#60825 = CARTESIAN_POINT ( 'NONE',  ( 18.30830001818700126, 3.300182612895000478, -12.02694835946000040 ) ) ;
#60826 = B_SPLINE_CURVE_WITH_KNOTS ( 'NONE', 3,
 ( #15186, #37887, #58867, #42789 ),
 .UNSPECIFIED., .F., .F.,
 ( 4, 4 ),
 ( 0.000000000000000000, 1.000000000000000000 ),
 .UNSPECIFIED. ) ;
#60827 = CARTESIAN_POINT ( 'NONE',  ( 10.06344080699000010, 5.156228702401000952, 6.125219923432000613 ) ) ;
#60828 = FACE_OUTER_BOUND ( 'NONE', #68445, .T. ) ;
#60829 = CARTESIAN_POINT ( 'NONE',  ( 8.100000113405998903, 3.037570195374000164E-13, -3.946654265865999873E-14 ) ) ;
#60830 = ORIENTED_EDGE ( 'NONE', *, *, #55425, .F. ) ;
#60831 = CARTESIAN_POINT ( 'NONE',  ( 12.48995884033426762, -1.960141145868676382, 12.56111957647684463 ) ) ;
#60832 = CARTESIAN_POINT ( 'NONE',  ( 9.123101285863999266, -4.646739515667500875, -6.731514281717299930 ) ) ;
#60833 = CARTESIAN_POINT ( 'NONE',  ( 9.792569055495000896, 3.463432304708999876, 6.184396499233999478 ) ) ;
#60834 = CIRCLE ( 'NONE', #37368, 9.250000000000000000 ) ;
#60835 = CARTESIAN_POINT ( 'NONE',  ( 9.120327454391752298, 5.191173620088457064, 7.911210609455967102 ) ) ;
#60836 = CARTESIAN_POINT ( 'NONE',  ( 10.20226357027499908, 5.120085139777000194, -7.716099591766099053 ) ) ;
#60837 = CARTESIAN_POINT ( 'NONE',  ( 12.78111495345091875, -0.7189971323193962149, 12.57946912511938109 ) ) ;
#60838 = EDGE_CURVE ( 'NONE', #47384, #46507, #15970, .T. ) ;
#60839 = ADVANCED_FACE ( 'NONE', ( #65449 ), #64490, .F. ) ;
#60840 = CARTESIAN_POINT ( 'NONE',  ( 7.326301658771000369, 3.394842219570000097, 9.388954446285000088 ) ) ;
#60841 = CARTESIAN_POINT ( 'NONE',  ( 9.194604681486000075, 5.157771204918000230, 8.637848577075999401 ) ) ;
#60842 = CARTESIAN_POINT ( 'NONE',  ( 8.766851002546001581, -2.832432432432000269, 6.822293592207000934 ) ) ;
#60843 = ORIENTED_EDGE ( 'NONE', *, *, #8050, .T. ) ;
#60844 = CARTESIAN_POINT ( 'NONE',  ( 9.892489158770999325, 5.099602161831000124, -9.049221499261999924 ) ) ;
#60845 = CARTESIAN_POINT ( 'NONE',  ( 11.61759063708296047, 5.217265640542000149, -7.842242470354300110 ) ) ;
#60846 = CARTESIAN_POINT ( 'NONE',  ( 10.78447049185723650, -4.843240479914882712, 9.027236721787854634 ) ) ;
#60848 = DIRECTION ( 'NONE',  ( 0.000000000000000000, -0.7071067811865475727, 0.7071067811865475727 ) ) ;
#60847 = CARTESIAN_POINT ( 'NONE',  ( 8.304129440378000382, -3.650411072918999800, 6.083135626079000602 ) ) ;
#60849 = CARTESIAN_POINT ( 'NONE',  ( 10.75944474310099963, -3.106516218291800246, 7.066400461213500073 ) ) ;
#60850 = CARTESIAN_POINT ( 'NONE',  ( 10.48133997687999930, -3.815400206859000054, -6.653701289769800020 ) ) ;
#60851 = ORIENTED_EDGE ( 'NONE', *, *, #26608, .T. ) ;
#60852 = CARTESIAN_POINT ( 'NONE',  ( 2.306794735327000190, 2.895272466935999933, -1.424404891072999835 ) ) ;
#60853 = CARTESIAN_POINT ( 'NONE',  ( 17.86534717991289156, -0.5429181307973055537, -12.68438171064090980 ) ) ;
#60854 = FACE_OUTER_BOUND ( 'NONE', #65799, .T. ) ;
#60855 = DIRECTION ( 'NONE',  ( 0.7071082394066439125, 0.7071053229634438608, -3.846805239771239731E-11 ) ) ;
#60856 = SHAPE_REPRESENTATION ( 'O Ring Seal 2', ( #9676 ), #57795 ) ;
#60857 = DIRECTION ( 'NONE',  ( 0.000000000000000000, 0.000000000000000000, -1.000000000000000000 ) ) ;
#60858 = CARTESIAN_POINT ( 'NONE',  ( 4.900006121742001675, -1.229093439949833444, -1.599333684796358401 ) ) ;
#60859 = CARTESIAN_POINT ( 'NONE',  ( 7.933148997457998952, 5.167567567567999731, 6.822293592207000934 ) ) ;
#60860 = LINE ( 'NONE', #18905, #46674 ) ;
#60861 = CARTESIAN_POINT ( 'NONE',  ( 13.64495723965300122, -12.20594327342000085, -2.556931772870000064 ) ) ;
#60862 = EDGE_LOOP ( 'NONE', ( #34928, #68603, #7172, #35537 ) ) ;
#60863 = CARTESIAN_POINT ( 'NONE',  ( 9.216851002545999094, -2.832432432432000269, 6.822293592207000934 ) ) ;
#60864 = ADVANCED_FACE ( 'NONE', ( #53702 ), #38552, .T. ) ;
#60865 = CARTESIAN_POINT ( 'NONE',  ( 30.60000000000000142, 2.052081123290000139E-07, -7.720759220056000238 ) ) ;
#60866 = CARTESIAN_POINT ( 'NONE',  ( 7.424973819922880303, -2.343829071653882323, 8.032060285052104120 ) ) ;
#60867 = LINE ( 'NONE', #7727, #43748 ) ;
#60868 = CARTESIAN_POINT ( 'NONE',  ( 0.8945193373687000404, -0.3804460121770000258, -3.739470302966999782 ) ) ;
#60869 = ORIENTED_EDGE ( 'NONE', *, *, #16170, .F. ) ;
#60870 = CARTESIAN_POINT ( 'NONE',  ( 10.71922080291976265, 4.353435520373844625, -8.814860677227555286 ) ) ;
#60871 = EDGE_CURVE ( 'NONE', #54548, #25005, #53504, .T. ) ;
#60872 = CARTESIAN_POINT ( 'NONE',  ( 10.87955921103774237, -5.549441030678586628, -8.346382036815052530 ) ) ;
#60873 = DIRECTION ( 'NONE',  ( -0.000000000000000000, 1.000000000000000000, 0.000000000000000000 ) ) ;
#60874 = AXIS2_PLACEMENT_3D ( 'NONE', #13021, #7766, #44151 ) ;
#60875 = CARTESIAN_POINT ( 'NONE',  ( 11.56025819896753859, 3.013900664291200293, 7.314099615601099558 ) ) ;
#60876 = CARTESIAN_POINT ( 'NONE',  ( 11.87299956498129916, -5.207010770456999893, 7.825000000000000178 ) ) ;
#60877 = CARTESIAN_POINT ( 'NONE',  ( 10.61442944038000036, -5.287639274524000399, -7.937245019889999753 ) ) ;
#60878 = CARTESIAN_POINT ( 'NONE',  ( 10.98953890776378906, -5.566676525139746978, 4.946116539698106607 ) ) ;
#60879 = CARTESIAN_POINT ( 'NONE',  ( 24.54688887196200042, 12.52317552374000087, 3.000792222368999784 ) ) ;
#60880 = CARTESIAN_POINT ( 'NONE',  ( 12.18136627099996439, -2.541785745019590426, 12.44176459540337376 ) ) ;
#60881 = ORIENTED_EDGE ( 'NONE', *, *, #48296, .T. ) ;
#60882 = CARTESIAN_POINT ( 'NONE',  ( 8.229134761907859641, 5.632572539116967647, 8.109682519133768253 ) ) ;
#60883 = ORIENTED_EDGE ( 'NONE', *, *, #50499, .T. ) ;
#60884 = CARTESIAN_POINT ( 'NONE',  ( 18.26121249471884411, -2.684743402744603991, 13.74018592865772703 ) ) ;
#60885 = CARTESIAN_POINT ( 'NONE',  ( 11.08425954179440076, -3.017023678917100327, -8.316745941391600283 ) ) ;
#60886 = ORIENTED_EDGE ( 'NONE', *, *, #47858, .F. ) ;
#60887 = FACE_OUTER_BOUND ( 'NONE', #37667, .T. ) ;
#60888 = CARTESIAN_POINT ( 'NONE',  ( 18.49996808500599599, 0.9036517550248718278, 11.64999999991244017 ) ) ;
#60889 = CARTESIAN_POINT ( 'NONE',  ( 9.646013540183334456, 4.999583552997728830, -6.731816600031361730 ) ) ;
#60890 = EDGE_CURVE ( 'NONE', #44629, #44553, #30971, .T. ) ;
#60891 = CARTESIAN_POINT ( 'NONE',  ( 0.2000000000000000389, 2.149999999999999911, 0.000000000000000000 ) ) ;
#60892 = CARTESIAN_POINT ( 'NONE',  ( 10.09197164456000095, 3.841384681542000301, 5.536408945990000774 ) ) ;
#60893 = CARTESIAN_POINT ( 'NONE',  ( 10.98768472625999948, -6.720753154780999772, 5.471698433974999887 ) ) ;
#60894 = CARTESIAN_POINT ( 'NONE',  ( 11.10000012945999970, 9.963297611412999188, -5.844090155092000138 ) ) ;
#60895 = PLANE ( 'NONE',  #1412 ) ;
#60896 = CARTESIAN_POINT ( 'NONE',  ( 10.42081395746000005, -2.488448635474999726, -7.717895569088000229 ) ) ;
#60897 = CARTESIAN_POINT ( 'NONE',  ( 10.16000000000000014, -4.496968146123999865, -8.755198255949000696 ) ) ;
#60898 = AXIS2_PLACEMENT_3D ( 'NONE', #44591, #18695, #8201 ) ;
#60899 = SURFACE_SIDE_STYLE ('',( #55309 ) ) ;
#60900 = ORIENTED_EDGE ( 'NONE', *, *, #56376, .F. ) ;
#60901 = CARTESIAN_POINT ( 'NONE',  ( 9.973631561148998514, 3.315688435009791490, 6.424401362931538628 ) ) ;
#60902 = FILL_AREA_STYLE_COLOUR ( '', #59992 ) ;
#60903 = CARTESIAN_POINT ( 'NONE',  ( 11.09999999999999964, -4.000000000000000000, -7.500000000000000000 ) ) ;
#60904 = CARTESIAN_POINT ( 'NONE',  ( 6.477679953015996084, 8.358404271369996863, 3.996200428631998314 ) ) ;
#60905 = CARTESIAN_POINT ( 'NONE',  ( 9.248087964304160025, 4.327168543240619947, 8.717422821756878548 ) ) ;
#60906 = CARTESIAN_POINT ( 'NONE',  ( 12.80505043854143388, 1.874999999999999556, 13.78627172894481667 ) ) ;
#60907 = CARTESIAN_POINT ( 'NONE',  ( 10.92717634842000152, -5.023656093247000243, 8.718039182945998888 ) ) ;
#60908 = ORIENTED_EDGE ( 'NONE', *, *, #6291, .F. ) ;
#60909 = CARTESIAN_POINT ( 'NONE',  ( 21.60000012424471194, 3.970157536060000036E-13, 1.776356839399999796E-13 ) ) ;
#60910 = CARTESIAN_POINT ( 'NONE',  ( 12.44955560269364803, -0.5141525164327368502, 13.88720023103246248 ) ) ;
#60911 = ORIENTED_EDGE ( 'NONE', *, *, #38982, .F. ) ;
#60912 = CARTESIAN_POINT ( 'NONE',  ( 0.2000000000000000389, 0.000000000000000000, 0.000000000000000000 ) ) ;
#60913 = CARTESIAN_POINT ( 'NONE',  ( 11.10000000009000054, -5.300000000088999741, -6.571291220400000022 ) ) ;
#60914 = CARTESIAN_POINT ( 'NONE',  ( 8.948279512853625661, 4.474797027487648293, 8.234914996158446243 ) ) ;
#60915 = FACE_OUTER_BOUND ( 'NONE', #17910, .T. ) ;
#60916 = CARTESIAN_POINT ( 'NONE',  ( 9.228345280414000484, 2.481540185810000132, -7.878707153279001396 ) ) ;
#60917 = VECTOR ( 'NONE', #28023, 1000.000000000000000 ) ;
#60918 = CARTESIAN_POINT ( 'NONE',  ( 11.09999999999999964, 4.000000000000000000, -7.500000000000000000 ) ) ;
#60919 = CARTESIAN_POINT ( 'NONE',  ( 11.00865415830999972, 8.467328835748000770, -6.608351749142999942 ) ) ;
#60920 = EDGE_CURVE ( 'NONE', #19641, #68613, #26762, .T. ) ;
#60921 = EDGE_CURVE ( 'NONE', #49079, #54494, #45261, .T. ) ;
#60922 = DIRECTION ( 'NONE',  ( 1.000000000000000000, 0.000000000000000000, 0.000000000000000000 ) ) ;
#60923 = CARTESIAN_POINT ( 'NONE',  ( 17.55505043854147118, -2.500000000000000000, -25.00000000000000000 ) ) ;
#60924 = CYLINDRICAL_SURFACE ( 'NONE', #41086, 0.6999999999999992895 ) ;
#60925 = CARTESIAN_POINT ( 'NONE',  ( 9.570737326637999587, -4.261100936929000049, -5.979198511086000423 ) ) ;
#60926 = EDGE_CURVE ( 'NONE', #6549, #7747, #43211, .T. ) ;
#60927 = EDGE_CURVE ( 'NONE', #55462, #67010, #46815, .T. ) ;
#60928 = CARTESIAN_POINT ( 'NONE',  ( 10.30903300763299946, 4.597717337857299746, -8.126922218169600143 ) ) ;
#60929 = CARTESIAN_POINT ( 'NONE',  ( 12.57114114720731557, 0.6824382159985146190, 12.58151825845911809 ) ) ;
#60930 = B_SPLINE_CURVE_WITH_KNOTS ( 'NONE', 3,
 ( #44098, #65397, #1090, #58776, #32230, #22404, #17516, #65042, #38490, #59813, #64350, #37800, #59123, #11915, #5976, #27316, #33257, #48642, #742, #64700, #6670, #16811, #38137, #34986, #66785, #1781 ),
 .UNSPECIFIED., .F., .F.,
 ( 4, 2, 2, 2, 2, 2, 2, 2, 2, 2, 2, 2, 4 ),
 ( 0.000000000000000000, 0.06249999999999833467, 0.09374999999999844569, 0.1249999999999985567, 0.2499999999999987788, 0.3749999999999990008, 0.4999999999999992228, 0.6249999999999994449, 0.7499999999999996669, 0.8124999999999995559, 0.8437500000000000000, 0.8750000000000005551, 1.000000000000000000 ),
 .UNSPECIFIED. ) ;
#60931 = CARTESIAN_POINT ( 'NONE',  ( 10.77879632507499785, 4.423544049216699747, -8.285174533868300273 ) ) ;
#60932 = CARTESIAN_POINT ( 'NONE',  ( 8.898101285863999621, 3.264788442324599860, -6.626387721327399838 ) ) ;
#60934 = LINE ( 'NONE', #33679, #28421 ) ;
#60933 = CARTESIAN_POINT ( 'NONE',  ( 9.469113844317998741, -3.781046324972699768, 8.338908357746399602 ) ) ;
#60935 = CARTESIAN_POINT ( 'NONE',  ( 9.099999886593998610, -12.39999890530000037, 0.000000000000000000 ) ) ;
#60936 = ORIENTED_EDGE ( 'NONE', *, *, #54718, .F. ) ;
#60937 = CARTESIAN_POINT ( 'NONE',  ( 10.68546886766499959, 3.433493735705800187, 8.529286361367999447 ) ) ;
#60938 = CARTESIAN_POINT ( 'NONE',  ( 10.87021507563000000, -2.226042145532000305, 7.782753277595999997 ) ) ;
#60939 = CARTESIAN_POINT ( 'NONE',  ( 9.074455549952999078, 4.888629236328500660, 8.216988513669100769 ) ) ;
#60940 = CARTESIAN_POINT ( 'NONE',  ( 10.68559687351635112, -2.907767014557174790, -6.870476274536379435 ) ) ;
#60941 = CARTESIAN_POINT ( 'NONE',  ( 9.538434317036999843, -5.620900626097999897, 7.423100105894999245 ) ) ;
#60942 = CARTESIAN_POINT ( 'NONE',  ( 10.89999835797000038, -1.382741308456999940, -11.26545887848999961 ) ) ;
#60943 = UNCERTAINTY_MEASURE_WITH_UNIT (LENGTH_MEASURE( 1.000000000000000082E-05 ), #20656, 'distance_accuracy_value', 'NONE');
#60944 = VERTEX_POINT ( 'NONE', #11729 ) ;
#60945 = PRESENTATION_LAYER_ASSIGNMENT (  '', '', ( #32994 ) ) ;
#60946 = CARTESIAN_POINT ( 'NONE',  ( 8.695468108405998819, -2.901397043998999781, -7.811136554427399403 ) ) ;
#60947 = CARTESIAN_POINT ( 'NONE',  ( 9.698096873516668381, -3.672815144550895639, -6.282534154164608253 ) ) ;
#60948 = CARTESIAN_POINT ( 'NONE',  ( 5.145433571222000069, -1.346921469446999975, 0.5851709088685000948 ) ) ;
#60949 = CARTESIAN_POINT ( 'NONE',  ( 8.432767466320006733, -2.913363525153000566, -6.617750919463998294 ) ) ;
#60950 = VECTOR ( 'NONE', #25591, 1000.000000000000000 ) ;
#60951 = DIRECTION ( 'NONE',  ( -1.000000000000000000, 0.000000000000000000, 0.000000000000000000 ) ) ;
#60952 = CARTESIAN_POINT ( 'NONE',  ( 11.53564291764652872, 3.004110626587600308, -7.376893506359599506 ) ) ;
#60953 = CARTESIAN_POINT ( 'NONE',  ( 11.37299956498129916, 2.792989229543000107, -7.174999999999999822 ) ) ;
#60954 = CARTESIAN_POINT ( 'NONE',  ( 9.172139116365000788, -4.730747404809998891, -8.668230005597001409 ) ) ;
#60955 = CARTESIAN_POINT ( 'NONE',  ( 0.9155567992084958640, -0.4581489286485083134, -3.500000000000000888 ) ) ;
#60956 = ORIENTED_EDGE ( 'NONE', *, *, #51959, .F. ) ;
#60957 = PLANE ( 'NONE',  #63387 ) ;
#60958 = CARTESIAN_POINT ( 'NONE',  ( 12.40062321164033499, 0.4766231184928879094, -13.88900205690511136 ) ) ;
#60959 = DIRECTION ( 'NONE',  ( 1.000000000000000000, -4.255854927730000031E-14, 1.480297366167000132E-14 ) ) ;
#60960 = CARTESIAN_POINT ( 'NONE',  ( 25.19211255715600117, -8.466231870115001001, -8.226678917617000764 ) ) ;
#60961 = CARTESIAN_POINT ( 'NONE',  ( 13.56457200097585591, -11.48338024779226707, -1.964390585072006257 ) ) ;
#60962 = CARTESIAN_POINT ( 'NONE',  ( 7.000000000000000888, 8.490173021533447439, 4.467909175706600067 ) ) ;
#60963 = CARTESIAN_POINT ( 'NONE',  ( 5.200000000000000178, 0.2500000000000000000, 9.776630298829998011 ) ) ;
#60964 = EDGE_LOOP ( 'NONE', ( #66904, #36184 ) ) ;
#60965 = AXIS2_PLACEMENT_3D ( 'NONE', #35152, #45643, #25329 ) ;
#60966 = CARTESIAN_POINT ( 'NONE',  ( 18.09820959019764075, 2.190632709185573734, -13.73422630893085561 ) ) ;
#60967 = VERTEX_POINT ( 'NONE', #6837 ) ;
#60968 = CARTESIAN_POINT ( 'NONE',  ( 24.60000000000000142, 0.000000000000000000, 0.000000000000000000 ) ) ;
#60969 = CARTESIAN_POINT ( 'NONE',  ( 16.10005255078199937, -3.632778330393000132, -11.06917548872000090 ) ) ;
#60970 = CIRCLE ( 'NONE', #54268, 1.825000327749000117 ) ;
#60971 = EDGE_CURVE ( 'NONE', #45043, #44536, #16975, .T. ) ;
#60972 = CARTESIAN_POINT ( 'NONE',  ( 9.301695280414000067, 5.619431609641999614, -8.115423117607999615 ) ) ;
#60973 = CARTESIAN_POINT ( 'NONE',  ( 11.48937577273788690, -4.461177266722074819, 6.300114087089553117 ) ) ;
#60974 = CARTESIAN_POINT ( 'NONE',  ( 17.72088406261400451, 1.806772466812846867, -13.88292461265716327 ) ) ;
#60975 = CARTESIAN_POINT ( 'NONE',  ( 18.09811783085399028, 0.3100350603811417027, -12.69492243000556364 ) ) ;
#60976 = EDGE_CURVE ( 'NONE', #56759, #1011, #123, .T. ) ;
#60977 = CARTESIAN_POINT ( 'NONE',  ( 10.28976354018233152, -4.327184855449096368, 8.717465845835395299 ) ) ;
#60978 = ORIENTED_EDGE ( 'NONE', *, *, #30017, .T. ) ;
#60979 = CARTESIAN_POINT ( 'NONE',  ( 9.634027193201999850, -3.042970193091000031, 8.588108172435999776 ) ) ;
#60980 = CARTESIAN_POINT ( 'NONE',  ( 18.16281717209332314, -2.646070499629755268, -13.64134067086682656 ) ) ;
#60981 = CARTESIAN_POINT ( 'NONE',  ( 9.395239158775000377, 5.045571591548999812, -9.086294919530001124 ) ) ;
#60982 = ORIENTED_EDGE ( 'NONE', *, *, #41104, .F. ) ;
#60983 = CARTESIAN_POINT ( 'NONE',  ( 9.910156421876999744, 2.531070993918000056, -7.917736616860999277 ) ) ;
#60984 = ORIENTED_EDGE ( 'NONE', *, *, #18087, .T. ) ;
#60985 = CARTESIAN_POINT ( 'NONE',  ( 9.860608878791998322, 3.741427262966100287, 8.612148635591999835 ) ) ;
#60986 = CARTESIAN_POINT ( 'NONE',  ( 18.24542859620203572, -2.700577031380342330, -12.30719352326003779 ) ) ;
#60987 = CARTESIAN_POINT ( 'NONE',  ( 10.98768472567999943, 5.449702577258999980, -4.945212061305999107 ) ) ;
#60988 = CARTESIAN_POINT ( 'NONE',  ( 24.30000000000000071, -9.305479840184000651, -8.315530346521999405 ) ) ;
#60989 = CARTESIAN_POINT ( 'NONE',  ( 11.72772918458500158, -11.64671933177000085, -1.861692232596000141 ) ) ;
#60990 = CARTESIAN_POINT ( 'NONE',  ( 9.662000818238999145, 3.232852935619000334, 7.096028062709999418 ) ) ;
#60991 = CARTESIAN_POINT ( 'NONE',  ( 9.353051448577010873, -3.388693121031217448, 9.128448243495800085 ) ) ;
#60992 = ORIENTED_EDGE ( 'NONE', *, *, #13050, .F. ) ;
#60993 = CARTESIAN_POINT ( 'NONE',  ( 8.320275543017386255, -5.099114840939221516, 6.576957048925175187 ) ) ;
#60994 = CARTESIAN_POINT ( 'NONE',  ( 10.88760471959000142, 5.634847467408999222, -7.088990678556999825 ) ) ;
#60995 = CARTESIAN_POINT ( 'NONE',  ( 24.30001123418010778, 8.895961323370999096, -8.895961323370999096 ) ) ;
#60996 = CARTESIAN_POINT ( 'NONE',  ( 12.44048633593776643, 3.149516123668032908, -13.64113935299650926 ) ) ;
#60997 = CARTESIAN_POINT ( 'NONE',  ( 10.39358376188600097, -5.078750111091999919, -8.187519150726398465 ) ) ;
#60998 = CARTESIAN_POINT ( 'NONE',  ( 9.815199780373001559, -2.813634733202999616, 8.848854270764999086 ) ) ;
#60999 = CARTESIAN_POINT ( 'NONE',  ( 17.71666486338982338, 0.6040897852209331509, 13.88232707694115398 ) ) ;
#61000 = AXIS2_PLACEMENT_3D ( 'NONE', #42561, #20544, #62495 ) ;
#61001 = CARTESIAN_POINT ( 'NONE',  ( 10.17905590578999941, 2.899999999999999911, 6.571291218949999902 ) ) ;
#61002 = EDGE_CURVE ( 'NONE', #22542, #46692, #56383, .T. ) ;
#61003 = VERTEX_POINT ( 'NONE', #32726 ) ;
#61004 = EDGE_LOOP ( 'NONE', ( #30756, #19802, #13929, #23988, #45091, #42610, #62953, #50364, #43772, #31465 ) ) ;
#61005 = CARTESIAN_POINT ( 'NONE',  ( 8.699089158774000907, 4.178200486578000472, -5.608493638783999202 ) ) ;
#61006 = CARTESIAN_POINT ( 'NONE',  ( 12.26246717652413309, -0.3103928945121602334, 13.89533876751213448 ) ) ;
#61007 = B_SPLINE_CURVE_WITH_KNOTS ( 'NONE', 3,
 ( #2505, #66472, #18596, #13356 ),
 .UNSPECIFIED., .F., .F.,
 ( 4, 4 ),
 ( 0.000000000000000000, 1.000000000000000000 ),
 .UNSPECIFIED. ) ;
#61008 = EDGE_CURVE ( 'NONE', #23338, #68419, #9277, .T. ) ;
#61009 = EDGE_CURVE ( 'NONE', #8323, #18734, #48415, .T. ) ;
#61010 = CARTESIAN_POINT ( 'NONE',  ( 12.26191093051546588, -2.190091418679299906, 13.73433605229447707 ) ) ;
#61011 = CARTESIAN_POINT ( 'NONE',  ( -0.2999999999999999889, -0.5773502691895999739, 1.000000000000000000 ) ) ;
#61012 = CARTESIAN_POINT ( 'NONE',  ( 7.165495559622000243, -2.688354259407999880, 8.140021027181001401 ) ) ;
#61013 = CARTESIAN_POINT ( 'NONE',  ( 15.95377458853735853, -3.445704530244193098, -11.33538647441605640 ) ) ;
#61015 = DIRECTION ( 'NONE',  ( -1.000000000000000000, 0.000000000000000000, 0.000000000000000000 ) ) ;
#61014 = CARTESIAN_POINT ( 'NONE',  ( 10.99288779216199963, -2.943881405003000218, 7.119137915499500480 ) ) ;
#61016 = CARTESIAN_POINT ( 'NONE',  ( 10.76426088462129904, 4.002719309691810778, -6.221990224628999755 ) ) ;
#61017 = EDGE_LOOP ( 'NONE', ( #6532, #67319, #64973 ) ) ;
#61018 = CONICAL_SURFACE ( 'NONE', #62104, 12.72499970924999957, 0.7853981386146715593 ) ;
#61019 = CARTESIAN_POINT ( 'NONE',  ( 12.15760927739264297, 0.3803681712231598011, 13.99548972734121577 ) ) ;
#61020 = CARTESIAN_POINT ( 'NONE',  ( 9.356851002546999752, 2.832432432432000269, -6.822293592207000934 ) ) ;
#61021 = CARTESIAN_POINT ( 'NONE',  ( 17.81340500845573871, 0.5691963043021754931, 12.68282590392938047 ) ) ;
#61022 = CARTESIAN_POINT ( 'NONE',  ( 12.80505043854144276, -0.6250000000000001110, 12.67928921589117586 ) ) ;
#61023 = CARTESIAN_POINT ( 'NONE',  ( 4.149992563291999836, -1.947893036340042849, 0.5234817089163666948 ) ) ;
#61024 = ORIENTED_EDGE ( 'NONE', *, *, #13586, .T. ) ;
#61026 = CARTESIAN_POINT ( 'NONE',  ( 11.09999999999999964, -5.299999999999999822, -5.157071272631999825 ) ) ;
#61025 = CARTESIAN_POINT ( 'NONE',  ( 11.78830977893788301, -4.976598135215292373, 8.326430086672807818 ) ) ;
#61027 = CARTESIAN_POINT ( 'NONE',  ( 8.854170280414001226, 4.902869380824999901, -8.978557145469999057 ) ) ;
#61028 = CARTESIAN_POINT ( 'NONE',  ( 24.63329222613833380, 10.83443034969673846, 3.855530961822280833 ) ) ;
#61029 = EDGE_CURVE ( 'NONE', #40878, #68681, #24648, .T. ) ;
#61030 = CARTESIAN_POINT ( 'NONE',  ( 10.17349413291699811, 5.162701151235999930, 8.030511425625498134 ) ) ;
#61031 = DIRECTION ( 'NONE',  ( 0.000000000000000000, 0.000000000000000000, -1.000000000000000000 ) ) ;
#61032 = CARTESIAN_POINT ( 'NONE',  ( 10.14393020684900115, -2.750000000000000000, 7.500000000000000000 ) ) ;
#61033 = CARTESIAN_POINT ( 'NONE',  ( 2.495155415437999569, -3.073701342168999595, -1.512342069823999990 ) ) ;
#61034 = ORIENTED_EDGE ( 'NONE', *, *, #31325, .F. ) ;
#61035 = CARTESIAN_POINT ( 'NONE',  ( 12.30048768357419853, 0.5166535389540172218, -12.58940585649086863 ) ) ;
#61036 = CARTESIAN_POINT ( 'NONE',  ( 4.699998537092440642, 0.000000000000000000, 0.000000000000000000 ) ) ;
#61037 = DIRECTION ( 'NONE',  ( -1.000000000000000000, 0.000000000000000000, 0.000000000000000000 ) ) ;
#61038 = CARTESIAN_POINT ( 'NONE',  ( 7.807364158771999740, 3.650414032626000171, 6.083147621602999600 ) ) ;
#61039 = CARTESIAN_POINT ( 'NONE',  ( 18.29999744860992905, -2.794302574217387924, -11.51706234583375732 ) ) ;
#61040 = ORIENTED_EDGE ( 'NONE', *, *, #58437, .T. ) ;
#61041 = CARTESIAN_POINT ( 'NONE',  ( 6.501421824151000450, 0.7188269793800999841, -0.9308427218166001049 ) ) ;
#61042 = CARTESIAN_POINT ( 'NONE',  ( 10.91882084328970670, 9.640838713336684407, 5.933495657908773424 ) ) ;
#61044 = CARTESIAN_POINT ( 'NONE',  ( 10.64831157502399073, 4.679757719901597390, -8.679446014678214638 ) ) ;
#61043 = CARTESIAN_POINT ( 'NONE',  ( 5.500000000000000000, 12.65263727151999795, 3.063503113339999917 ) ) ;
#61045 = CARTESIAN_POINT ( 'NONE',  ( 11.01041369783139956, 3.935522326596939902, 6.223614866029000048 ) ) ;
#61046 = CARTESIAN_POINT ( 'NONE',  ( 11.09590547754519996, 5.315605332491999846, -7.541753805330609239 ) ) ;
#61047 = VERTEX_POINT ( 'NONE', #35148 ) ;
#61048 = AXIS2_PLACEMENT_3D ( 'NONE', #51256, #56847, #67657 ) ;
#61049 = CYLINDRICAL_SURFACE ( 'NONE', #35076, 1.350000000000000089 ) ;
#61050 = VERTEX_POINT ( 'NONE', #61362 ) ;
#61051 = DIRECTION ( 'NONE',  ( 0.000000000000000000, -1.000000000000000000, 0.000000000000000000 ) ) ;
#61052 = CARTESIAN_POINT ( 'NONE',  ( 7.956793146791999227, -4.524489047957000132, 9.047757046927999980 ) ) ;
#61053 = CIRCLE ( 'NONE', #32018, 1.000000000000000222 ) ;
#61054 = CARTESIAN_POINT ( 'NONE',  ( 18.18297552798362560, -0.3652063536484516648, -13.99523956222174448 ) ) ;
#61055 = ORIENTED_EDGE ( 'NONE', *, *, #67967, .T. ) ;
#61056 = CARTESIAN_POINT ( 'NONE',  ( 6.790909542087999462, -9.291477070232998514, 5.323632131722000338 ) ) ;
#61057 = FACE_OUTER_BOUND ( 'NONE', #18702, .T. ) ;
#61058 = CARTESIAN_POINT ( 'NONE',  ( 8.170639158770999444, 4.727211190310000255, -8.622645617656999661 ) ) ;
#61059 = ADVANCED_FACE ( 'NONE', ( #13137 ), #51742, .F. ) ;
#61060 = CARTESIAN_POINT ( 'NONE',  ( 24.63333006944293402, 2.078227422262555635, -11.31065739827893779 ) ) ;
#61061 = CARTESIAN_POINT ( 'NONE',  ( 11.09999999999999964, 4.000000000000000000, 7.500000000000000000 ) ) ;
#61062 = ORIENTED_EDGE ( 'NONE', *, *, #65013, .T. ) ;
#61063 = DIRECTION ( 'NONE',  ( -0.7071068156326932863, 0.000000000000000000, -0.7071067467404001938 ) ) ;
#61064 = B_SPLINE_CURVE_WITH_KNOTS ( 'NONE', 3,
 ( #25288, #30540, #50831, #56770, #46622, #14803, #3609, #52198, #61660, #46276 ),
 .UNSPECIFIED., .F., .F.,
 ( 4, 2, 2, 2, 4 ),
 ( 0.000000000000000000, 0.2500000000000000000, 0.5000000000000000000, 0.7500000000000000000, 1.000000000000000000 ),
 .UNSPECIFIED. ) ;
#61065 = CARTESIAN_POINT ( 'NONE',  ( 23.64132706837899889, -13.18685377439000028, -4.069706785829999340 ) ) ;
#61066 = CARTESIAN_POINT ( 'NONE',  ( 9.716846873515667227, 4.768183399968648040, 8.499583552997721725 ) ) ;
#61067 = CARTESIAN_POINT ( 'NONE',  ( 9.739312519577287830, -2.650230560758064069, 7.263871480528514724 ) ) ;
#61068 = ORIENTED_EDGE ( 'NONE', *, *, #56965, .T. ) ;
#61069 = DIRECTION ( 'NONE',  ( 0.000000000000000000, -0.1218274111675001353, -0.9925512993736016476 ) ) ;
#61070 = CARTESIAN_POINT ( 'NONE',  ( 10.95460932063975790, -2.828099631735832453, -6.694244964707101175 ) ) ;
#61071 = B_SPLINE_CURVE_WITH_KNOTS ( 'NONE', 3,
 ( #58493, #37859, #48701, #802, #26693, #11624, #22118, #17224, #38549, #27374, #54633, #43463, #16188, #1151, #16874, #5354, #38198, #48008, #59528, #108, #10596, #32964, #21096, #22460, #6728, #48347, #31938, #49378, #59183, #54278, #53596, #53248, #63729, #37512, #21771, #58836, #15841, #43805, #65101, #59872, #11977, #11283, #37173, #10944, #32622, #21424, #5692, #453, #43107, #6036, #64408, #12332, #18616, #54981, #29469, #60914, #13380, #39591, #44508, #17929, #33663, #45188, #8468, #44159, #2192 ),
 .UNSPECIFIED., .F., .F.,
 ( 4, 1, 1, 1, 1, 1, 1, 1, 1, 1, 1, 1, 1, 1, 1, 1, 1, 1, 1, 1, 1, 1, 1, 1, 1, 1, 1, 1, 1, 1, 1, 1, 1, 1, 1, 1, 1, 1, 1, 1, 1, 1, 1, 1, 1, 1, 1, 1, 1, 1, 1, 1, 1, 1, 1, 1, 1, 1, 1, 1, 1, 1, 4 ),
 ( 0.000000000000000000, 0.01249986222369732156, 0.02874986775682976045, 0.04499987328996220282, 0.06124987882309464171, 0.07749988435622708061, 0.09374988988935951950, 0.1099998954224919584, 0.1262499009556244112, 0.1424999064887568501, 0.1587499120218892890, 0.1749999175550217279, 0.1912499230881541668, 0.2074999286212866056, 0.2237499341544190445, 0.2399999396875514834, 0.2562499452206838946, 0.2724999507538163890, 0.2887499562869488279, 0.3049999618200812668, 0.3212499673532136502, 0.3374999728863461446, 0.3537499784194785835, 0.3699999839526110224, 0.3862499894857434612, 0.4024999950188759001, 0.4187500005520083390, 0.4350000060851407779, 0.4512500116182732168, 0.4675000171514057112, 0.4837500226845380946, 0.5000000282176705335, 0.5162500337508029169, 0.5325000392839353003, 0.5487500448170677947, 0.5650000503502001781, 0.5812500558833327835, 0.5975000614164651669, 0.6137500669495975503, 0.6300000724827300447, 0.6462500780158624281, 0.6625000835489948114, 0.6787500890821273059, 0.6950000946152596892, 0.7112501001483922947, 0.7275001056815246780, 0.7437501112146570614, 0.7600001167477895558, 0.7762501222809219392, 0.7925001278140544336, 0.8087501333471868170, 0.8250001388803192004, 0.8412501444134518058, 0.8575001499465841892, 0.8737501554797166836, 0.8900001610128490670, 0.9062501665459814504, 0.9225001720791139448, 0.9387501776122463282, 0.9550001831453788226, 0.9712501886785112060, 0.9875001942116437004, 1.000000000000000000 ),
 .UNSPECIFIED. ) ;
#61072 = CARTESIAN_POINT ( 'NONE',  ( 8.398903073012702336, 5.292594335792998095, -8.672717482341102624 ) ) ;
#61073 = CARTESIAN_POINT ( 'NONE',  ( 24.53428985175800037, 12.47024902693999948, -3.026245299674999778 ) ) ;
#61074 = CARTESIAN_POINT ( 'NONE',  ( 24.39664795268166841, 3.240506188470991145, 12.09373373761089177 ) ) ;
#61075 = AXIS2_PLACEMENT_3D ( 'NONE', #21733, #43066, #32927 ) ;
#61076 = CARTESIAN_POINT ( 'NONE',  ( 12.33448524795695711, -0.4118363585311515807, -13.89180007025484720 ) ) ;
#61077 = CARTESIAN_POINT ( 'NONE',  ( 18.02812495262685744, -2.091428156338118960, 12.53745402072848592 ) ) ;
#61078 = VERTEX_POINT ( 'NONE', #50529 ) ;
#61079 = CARTESIAN_POINT ( 'NONE',  ( 10.76857802013509868, -5.174568897094999897, -7.472656658230009796 ) ) ;
#61080 = EDGE_LOOP ( 'NONE', ( #23708, #2741, #28120, #9265, #58958 ) ) ;
#61081 = FACE_BOUND ( 'NONE', #42631, .T. ) ;
#61082 = CARTESIAN_POINT ( 'NONE',  ( 9.278070280414000948, 2.546924812613000189, -6.918870225297999887 ) ) ;
#61083 = CARTESIAN_POINT ( 'NONE',  ( 2.915571724536000442, -1.477002359740999804, 2.855699589946999684 ) ) ;
#61084 = CARTESIAN_POINT ( 'NONE',  ( 9.937415816209998809, -3.510658118802999716, -6.227041669085999764 ) ) ;
#61085 = CARTESIAN_POINT ( 'NONE',  ( 7.858269739253733732, 2.859091829101807480, -6.771441901864826640 ) ) ;
#61086 = CARTESIAN_POINT ( 'NONE',  ( 9.041114232695017350, -4.912826217066823986, 8.494526172176604106 ) ) ;
#61087 = ORIENTED_EDGE ( 'NONE', *, *, #7962, .T. ) ;
#61088 = EDGE_CURVE ( 'NONE', #25113, #31044, #19395, .T. ) ;
#61089 = CARTESIAN_POINT ( 'NONE',  ( 12.03564291764652872, -4.995889373412399692, 7.623106493640399606 ) ) ;
#61090 = CARTESIAN_POINT ( 'NONE',  ( 10.06843885510000014, 4.148608506723999945, 8.941445591976998841 ) ) ;
#61091 = EDGE_CURVE ( 'NONE', #5290, #63702, #2825, .T. ) ;
#61092 = DIRECTION ( 'NONE',  ( 0.000000000000000000, 0.000000000000000000, -1.000000000000000000 ) ) ;
#61093 = CARTESIAN_POINT ( 'NONE',  ( 10.45551210286900279, 3.782771630962270759, -8.756187319522085843 ) ) ;
#61094 = CARTESIAN_POINT ( 'NONE',  ( 11.09999999999999964, -4.000000000000000000, 7.500000000000000000 ) ) ;
#61095 = CARTESIAN_POINT ( 'NONE',  ( 11.41256651104150066, 4.098999650273559503, -6.501426055769400136 ) ) ;
#61096 = CONICAL_SURFACE ( 'NONE', #65522, 12.37499919541000004, 0.7853980884875938484 ) ;
#61097 = CARTESIAN_POINT ( 'NONE',  ( 10.92117502560267361, 2.832205961051685428, -6.780502835040467247 ) ) ;
#61098 = PRESENTATION_LAYER_ASSIGNMENT (  '', '', ( #4139 ) ) ;
#61099 = CARTESIAN_POINT ( 'NONE',  ( 8.922480666858998433, 4.380700808321400075, -8.576476893896000320 ) ) ;
#61100 = CARTESIAN_POINT ( 'NONE',  ( 18.25531039711339432, -0.1866745257715827222, 12.59862229962904046 ) ) ;
#61101 = CARTESIAN_POINT ( 'NONE',  ( 11.02319144466311052, 5.119973997747526262, -7.824989718906223857 ) ) ;
#61102 = CARTESIAN_POINT ( 'NONE',  ( 0.9500156295917255855, 2.823650222959981804, -2.106025417230501962 ) ) ;
#61103 = CIRCLE ( 'NONE', #32065, 14.00000000000000000 ) ;
#61104 = CARTESIAN_POINT ( 'NONE',  ( 10.16008584122999991, 4.812959680871000678, -8.526582921144999716 ) ) ;
#61105 = EDGE_LOOP ( 'NONE', ( #55395, #27959, #65086 ) ) ;
#61106 = CARTESIAN_POINT ( 'NONE',  ( 8.116918146793999256, -5.773185758034999893, 7.141496747382000798 ) ) ;
#61107 = CARTESIAN_POINT ( 'NONE',  ( 18.18357137170425020, 2.882057337525661289, 13.70014066609292058 ) ) ;
#61108 = ADVANCED_FACE ( 'NONE', ( #28880 ), #26536, .F. ) ;
#61109 = CARTESIAN_POINT ( 'NONE',  ( 24.54688887196200042, 8.860350057919001543, -9.344992028423000363 ) ) ;
#61110 = DIRECTION ( 'NONE',  ( -4.331025598861020273E-21, -3.276905820014099985E-06, 0.9999999999946310725 ) ) ;
#61111 = ORIENTED_EDGE ( 'NONE', *, *, #54614, .F. ) ;
#61112 = CONICAL_SURFACE ( 'NONE', #27571, 13.04999934368000147, 0.7853981075146502233 ) ;
#61113 = B_SPLINE_CURVE_WITH_KNOTS ( 'NONE', 3,
 ( #1540, #13078, #22858, #62670 ),
 .UNSPECIFIED., .F., .F.,
 ( 4, 4 ),
 ( 0.000000000000000000, 0.1253179912170450105 ),
 .UNSPECIFIED. ) ;
#61114 = EDGE_CURVE ( 'NONE', #55782, #57373, #53028, .T. ) ;
#61115 = CARTESIAN_POINT ( 'NONE',  ( 8.604017219593000476, 5.165497731316000873, 8.645531386060000045 ) ) ;
#61117 = CYLINDRICAL_SURFACE ( 'NONE', #66648, 12.50000000000000000 ) ;
#61116 = CARTESIAN_POINT ( 'NONE',  ( 10.14325461470300027, -4.840245908677600184, -7.713763321667399531 ) ) ;
#61118 = CARTESIAN_POINT ( 'NONE',  ( 9.900934992105000276, 4.883852641422000040, -9.070888919673000927 ) ) ;
#61119 = ORIENTED_EDGE ( 'NONE', *, *, #61266, .F. ) ;
#61120 = CARTESIAN_POINT ( 'NONE',  ( 9.576488281553999116, 4.593976206186999534, 5.662041230125000268 ) ) ;
#61121 = CIRCLE ( 'NONE', #30986, 1.250000000000000444 ) ;
#61122 = CARTESIAN_POINT ( 'NONE',  ( 9.766851002543001314, 2.832432432432000269, 6.822293592207000934 ) ) ;
#61123 = CARTESIAN_POINT ( 'NONE',  ( 11.08841369783139896, 3.942447888101379583, 6.360711682373000109 ) ) ;
#61124 = CARTESIAN_POINT ( 'NONE',  ( 9.667080975990000269, -4.541622198376999542, 5.824041840233000755 ) ) ;
#61125 = CARTESIAN_POINT ( 'NONE',  ( 8.228219317832992985, 3.441361860949001539, 6.127431671619995690 ) ) ;
#61126 = EDGE_LOOP ( 'NONE', ( #47049, #56173, #50969, #64124 ) ) ;
#61127 = DIRECTION ( 'NONE',  ( 1.000000000000000000, 0.000000000000000000, 0.000000000000000000 ) ) ;
#61128 = CARTESIAN_POINT ( 'NONE',  ( 10.46297944037999983, -3.993164663709000362, -6.140164943008000087 ) ) ;
#61129 = CARTESIAN_POINT ( 'NONE',  ( 7.975403604543350511, -2.344124067439634640, 6.939139580511310079 ) ) ;
#61130 = CARTESIAN_POINT ( 'NONE',  ( 9.972852379787999766, -5.044471434015000533, 6.258101649750000384 ) ) ;
#61131 = CARTESIAN_POINT ( 'NONE',  ( 10.76346886766499900, -4.634677072395899877, -6.346853961441000003 ) ) ;
#61132 = CARTESIAN_POINT ( 'NONE',  ( 9.197480666858998788, -3.665111009453500213, 6.553061479084200336 ) ) ;
#61133 = VERTEX_POINT ( 'NONE', #37195 ) ;
#61134 = CARTESIAN_POINT ( 'NONE',  ( 17.80000000005199823, 3.345268251980999974, -11.86064071431999878 ) ) ;
#61135 = CARTESIAN_POINT ( 'NONE',  ( 11.92887348028849992, -5.124210964533999935, 6.892162778124999889 ) ) ;
#61136 = EDGE_LOOP ( 'NONE', ( #38973, #54000, #7941, #13161 ) ) ;
#61137 = CARTESIAN_POINT ( 'NONE',  ( 4.000000000000000000, 2.750000000000000000, 0.000000000000000000 ) ) ;
#61138 = ORIENTED_EDGE ( 'NONE', *, *, #62564, .F. ) ;
#61139 = CARTESIAN_POINT ( 'NONE',  ( 11.09999999999999964, -5.299999999999999822, -5.157071272631999825 ) ) ;
#61140 = CARTESIAN_POINT ( 'NONE',  ( 9.442010841233001273, 5.045571591548999812, -9.086294919530001124 ) ) ;
#61141 = DIRECTION ( 'NONE',  ( -1.000000000000000000, 0.000000000000000000, 0.000000000000000000 ) ) ;
#61142 = DIRECTION ( 'NONE',  ( 0.000000000000000000, -0.8648648648648720183, 0.5020047465136825426 ) ) ;
#61143 = CARTESIAN_POINT ( 'NONE',  ( 12.36741688735892986, 2.053674487412246563, -12.54445365011033786 ) ) ;
#61144 = CARTESIAN_POINT ( 'NONE',  ( 11.56795257254739973, -4.963546614172099858, 7.219770138693499817 ) ) ;
#61145 = CARTESIAN_POINT ( 'NONE',  ( 12.02677869730533011, -4.403502086956500250, 8.295667533166499297 ) ) ;
#61146 =( BOUNDED_SURFACE ( )  B_SPLINE_SURFACE ( 3, 3, ( 
 ( #54705, #16261, #53332, #5432, #59602, #22537, #48425 ),
 ( #881, #54352, #21846, #38626, #33389, #10672, #43181 ),
 ( #12057, #58918, #6804, #32019, #32695, #17301, #47747 ),
 ( #53674, #59947, #69062, #58568, #22197, #21168, #43533 ) ),
 .UNSPECIFIED., .F., .F., .T. ) 
 B_SPLINE_SURFACE_WITH_KNOTS ( ( 4, 4 ),
 ( 4, 1, 1, 1, 4 ),
 ( 0.000000000000000000, 1.000000000000000000 ),
 ( 0.8949772423043999003, 0.9056938526918999477, 0.9344431701380999655, 0.9658387281735000274, 0.9801003582285999771 ),
 .UNSPECIFIED. ) 
 GEOMETRIC_REPRESENTATION_ITEM ( )  RATIONAL_B_SPLINE_SURFACE ( (
 ( 1.200981758128000010, 1.200981758128000010, 1.200981758128000010, 1.200981758128000010, 1.200981758128000010, 1.200981758128000010, 1.200981758128000010),
 ( 0.9330060806240999538, 0.9330060806240999538, 0.9330060806240999538, 0.9330060806240999538, 0.9330060806240999538, 0.9330060806240999538, 0.9330060806240999538),
 ( 0.9330060806240999538, 0.9330060806240999538, 0.9330060806240999538, 0.9330060806240999538, 0.9330060806240999538, 0.9330060806240999538, 0.9330060806240999538),
 ( 1.200981758128000010, 1.200981758128000010, 1.200981758128000010, 1.200981758128000010, 1.200981758128000010, 1.200981758128000010, 1.200981758128000010) ) ) 
 REPRESENTATION_ITEM ( '' )  SURFACE ( )  );
#61147 = ORIENTED_EDGE ( 'NONE', *, *, #53574, .F. ) ;
#61148 = CARTESIAN_POINT ( 'NONE',  ( 25.60000000000000142, 0.000000000000000000, 0.000000000000000000 ) ) ;
#61149 = ORIENTED_EDGE ( 'NONE', *, *, #2690, .T. ) ;
#61150 = CARTESIAN_POINT ( 'NONE',  ( 7.700043146791999860, -3.346260729029000291, 6.002247316312999459 ) ) ;
#61151 = CARTESIAN_POINT ( 'NONE',  ( 7.931011803055000975, 3.387313518888000363, -6.297038610257000180 ) ) ;
#61152 = ORIENTED_EDGE ( 'NONE', *, *, #36578, .F. ) ;
#61153 = CARTESIAN_POINT ( 'NONE',  ( 12.10480575880364107, -2.667436721895846130, -12.31441907085211973 ) ) ;
#61154 = CARTESIAN_POINT ( 'NONE',  ( 11.01456785386839954, 3.053605396817899997, 6.863111178199799767 ) ) ;
#61155 = PRESENTATION_LAYER_ASSIGNMENT (  '', '', ( #9788 ) ) ;
#61156 = CARTESIAN_POINT ( 'NONE',  ( 9.926183059621999760, -4.356410583133000003, -9.313949118577001585 ) ) ;
#61157 = FACE_OUTER_BOUND ( 'NONE', #7488, .T. ) ;
#61158 = CARTESIAN_POINT ( 'NONE',  ( 17.69476807989700262, -11.38964709781999929, 4.572869473993000256 ) ) ;
#61159 = CARTESIAN_POINT ( 'NONE',  ( 9.934999999999998721, 4.640430492595999823, -9.117542781427999898 ) ) ;
#61160 = CARTESIAN_POINT ( 'NONE',  ( 12.19342855462631370, -2.370970601743436212, -13.69993124892199354 ) ) ;
#61161 = CARTESIAN_POINT ( 'NONE',  ( 18.17602447836047475, 0.07155418421575511501, -12.69973420405193032 ) ) ;
#61162 = CARTESIAN_POINT ( 'NONE',  ( 11.46595122972049907, -3.656201404350900130, -6.704952129760900270 ) ) ;
#61163 = CARTESIAN_POINT ( 'NONE',  ( 10.17349413291699811, -2.837298848764000514, -6.969488574374499201 ) ) ;
#61164 = CARTESIAN_POINT ( 'NONE',  ( 7.994579719591000000, 2.263558315407000254, 8.007442119518000112 ) ) ;
#61165 = ORIENTED_EDGE ( 'NONE', *, *, #698, .T. ) ;
#61166 = CIRCLE ( 'NONE', #36602, 0.6999999999999992895 ) ;
#61167 = CARTESIAN_POINT ( 'NONE',  ( 23.60000000000000142, 1.954456641860109256, -13.79170062071063008 ) ) ;
#61168 = CARTESIAN_POINT ( 'NONE',  ( 8.017297003156361512, 5.179978819780632016, 8.180934229233717048 ) ) ;
#61169 = CARTESIAN_POINT ( 'NONE',  ( 24.03158564178600187, -3.727259782881000127, 13.01535860997999983 ) ) ;
#61170 = CARTESIAN_POINT ( 'NONE',  ( 17.96242084756261193, 2.025889508701483877, 12.54946620628462206 ) ) ;
#61171 = CARTESIAN_POINT ( 'NONE',  ( 18.26123302403700066, 2.828310120379999848, -11.95646042099000006 ) ) ;
#61172 = CARTESIAN_POINT ( 'NONE',  ( 10.09197164456000095, 3.841384681542000301, 5.536408945990000774 ) ) ;
#61173 = VECTOR ( 'NONE', #59746, 1000.000000000000114 ) ;
#61174 = CARTESIAN_POINT ( 'NONE',  ( 8.023148997453999343, 5.167567567567999731, -6.822293592207000934 ) ) ;
#61175 = CARTESIAN_POINT ( 'NONE',  ( 1.700000000000000178, 2.149999999999999911, 0.000000000000000000 ) ) ;
#61176 = EDGE_CURVE ( 'NONE', #31977, #50708, #59308, .T. ) ;
#61177 = ORIENTED_EDGE ( 'NONE', *, *, #17117, .F. ) ;
#61178 = CARTESIAN_POINT ( 'NONE',  ( 12.64184255386822464, -1.896331190223615515, 12.57194050387411899 ) ) ;
#61179 = EDGE_CURVE ( 'NONE', #13153, #13611, #4675, .T. ) ;
#61180 = CARTESIAN_POINT ( 'NONE',  ( 9.855633995697999694, -3.138280386550500012, -7.595641268826199166 ) ) ;
#61181 = CARTESIAN_POINT ( 'NONE',  ( 10.14750576281000072, 2.602962605360999770, 6.738577830910999822 ) ) ;
#61182 = CARTESIAN_POINT ( 'NONE',  ( 12.30233327354039830, -5.101536739857000846, 8.220500279733599314 ) ) ;
#61183 = PRODUCT ( 'Insulator', 'Insulator', '', ( #19765 ) ) ;
#61184 = CARTESIAN_POINT ( 'NONE',  ( 11.55194988689359903, 4.580487242693600081, -8.638573882912000457 ) ) ;
#61185 = CARTESIAN_POINT ( 'NONE',  ( 12.72331806630341156, 0.6199686954221025337, 12.67962180225517876 ) ) ;
#61186 = CARTESIAN_POINT ( 'NONE',  ( 7.481079719589999399, 2.374037589774999901, 8.293392681990997772 ) ) ;
#61187 = CARTESIAN_POINT ( 'NONE',  ( 9.290193290418001126, 2.377818438998999806, 7.540992072119000689 ) ) ;
#61188 = CARTESIAN_POINT ( 'NONE',  ( 12.23381074371944877, 2.246196888878373432, 12.50707970526073254 ) ) ;
#61189 = ORIENTED_EDGE ( 'NONE', *, *, #24272, .F. ) ;
#61190 = CARTESIAN_POINT ( 'NONE',  ( 25.40548315682400116, 8.312246831039999506, 8.369343040493999908 ) ) ;
#61191 = CARTESIAN_POINT ( 'NONE',  ( 10.56733863405299800, 4.788475529394700558, -8.505794571537999005 ) ) ;
#61192 = CARTESIAN_POINT ( 'NONE',  ( 10.73166211313188256, -5.609524154758663173, 8.188827626220106737 ) ) ;
#61194 = CARTESIAN_POINT ( 'NONE',  ( 10.22934687351566474, 3.836375382625535124, 8.750000000000000000 ) ) ;
#61193 = CARTESIAN_POINT ( 'NONE',  ( 8.085168146793000332, -2.431397064767999439, 7.958394431095000776 ) ) ;
#61195 = CARTESIAN_POINT ( 'NONE',  ( 9.830709346416998784, -3.092687088662700035, 7.930842873041400232 ) ) ;
#61196 = CARTESIAN_POINT ( 'NONE',  ( 11.02287616594229824, -4.261927842557799551, -6.674353346984900348 ) ) ;
#61197 = ORIENTED_EDGE ( 'NONE', *, *, #55402, .F. ) ;
#61198 = B_SPLINE_CURVE_WITH_KNOTS ( 'NONE', 3,
 ( #48535, #59707, #27552, #49216 ),
 .UNSPECIFIED., .F., .F.,
 ( 4, 4 ),
 ( 0.000000000000000000, 1.000000000000000000 ),
 .UNSPECIFIED. ) ;
#61199 = CARTESIAN_POINT ( 'NONE',  ( 2.120840275626000082, -0.2760264376601999636, -3.247374627496999899 ) ) ;
#61200 = ADVANCED_FACE ( 'NONE', ( #9582 ), #18267, .F. ) ;
#61201 = CARTESIAN_POINT ( 'NONE',  ( 18.10291658814850990, -0.3009529450547471785, -12.69520353502832677 ) ) ;
#61202 = CARTESIAN_POINT ( 'NONE',  ( 0.8183045265946674585, 2.967694544611792828, -1.300349661452710803 ) ) ;
#61204 = B_SPLINE_CURVE_WITH_KNOTS ( 'NONE', 3,
 ( #62771, #30983, #42159, #14894 ),
 .UNSPECIFIED., .F., .F.,
 ( 4, 4 ),
 ( 0.000000000000000000, 1.000000000000000000 ),
 .UNSPECIFIED. ) ;
#61203 = CARTESIAN_POINT ( 'NONE',  ( 17.99250848601378650, -2.946479007108954828, 13.56856542436122659 ) ) ;
#61205 = CARTESIAN_POINT ( 'NONE',  ( 24.46580263758400164, -12.16839033388000146, 3.168637029940999827 ) ) ;
#61207 = CARTESIAN_POINT ( 'NONE',  ( 12.68593947922895460, -3.238585582162124776, 13.62026383368923454 ) ) ;
#61206 = COLOUR_RGB ( '', 0.09019608, 0.27058824, 0.51372549) ;
#61208 = CARTESIAN_POINT ( 'NONE',  ( 4.599999999999999645, 0.000000000000000000, 0.000000000000000000 ) ) ;
#61209 = CARTESIAN_POINT ( 'NONE',  ( 16.39999999485600313, 3.595156957901000094, 11.99794989424000136 ) ) ;
#61210 = CARTESIAN_POINT ( 'NONE',  ( 13.07616489729400122, -12.32806027643999869, -1.877794484342000025 ) ) ;
#61211 = ORIENTED_EDGE ( 'NONE', *, *, #43797, .T. ) ;
#61212 = CARTESIAN_POINT ( 'NONE',  ( 8.625073341231001223, 3.117378429069999957, 8.662179062556001341 ) ) ;
#61213 = CARTESIAN_POINT ( 'NONE',  ( 11.05220172920000010, 5.231347787620000744, 4.974789424501000923 ) ) ;
#61214 = CARTESIAN_POINT ( 'NONE',  ( 7.417028609100216663, -2.407073382786591775, 8.200060021492962647 ) ) ;
#61215 = AXIS2_PLACEMENT_3D ( 'NONE', #8848, #41007, #32249 ) ;
#61216 = CARTESIAN_POINT ( 'NONE',  ( 10.51720455738115412, -5.205742106671480407, 8.206130011351941533 ) ) ;
#61217 = CARTESIAN_POINT ( 'NONE',  ( 0.9278812726222999130, -0.1441893070566999946, 3.255843074068999865 ) ) ;
#61218 = ORIENTED_EDGE ( 'NONE', *, *, #44778, .T. ) ;
#61219 = CARTESIAN_POINT ( 'NONE',  ( 10.72963504510710564, 4.176677120266796273, -8.849854844400319109 ) ) ;
#61220 = FACE_OUTER_BOUND ( 'NONE', #34698, .T. ) ;
#61221 = CARTESIAN_POINT ( 'NONE',  ( 10.53734212242000012, 2.992816679959000137, 8.731689474572998932 ) ) ;
#61222 = CARTESIAN_POINT ( 'NONE',  ( 11.21564426047340035, 4.539962866738299851, 6.654192128557399499 ) ) ;
#61223 = B_SPLINE_CURVE_WITH_KNOTS ( 'NONE', 3,
 ( #54659, #8491, #30173, #18980, #29495, #56388 ),
 .UNSPECIFIED., .F., .F.,
 ( 4, 2, 4 ),
 ( 0.000000000000000000, 0.5000000000000000000, 1.000000000000000000 ),
 .UNSPECIFIED. ) ;
#61224 = CARTESIAN_POINT ( 'NONE',  ( 9.624831031536459136, -2.894183647071444376, 8.301356454185306433 ) ) ;
#61225 = CARTESIAN_POINT ( 'NONE',  ( 10.95519194037999888, -3.860335380237000180, -6.147338954930000376 ) ) ;
#61226 = CARTESIAN_POINT ( 'NONE',  ( 15.89979320884932967, -4.771864030974223958, -11.40757335769646552 ) ) ;
#61227 = CARTESIAN_POINT ( 'NONE',  ( 0.4843736936024935491, 2.045128573188879972, -2.872081862618736547 ) ) ;
#61228 = CARTESIAN_POINT ( 'NONE',  ( 12.21592886434220482, -2.708773148185487756, 12.40049785804586691 ) ) ;
#61229 = CARTESIAN_POINT ( 'NONE',  ( 8.274731576662917476, 5.048784206079365511, 8.903984921411593589 ) ) ;
#61230 = VERTEX_POINT ( 'NONE', #11647 ) ;
#61231 = CARTESIAN_POINT ( 'NONE',  ( 17.71798387292789556, -1.896258650311507310, 13.78312406285442293 ) ) ;
#61232 = CARTESIAN_POINT ( 'NONE',  ( 10.32118582084299874, -4.836160649475099937, -6.533484739457099622 ) ) ;
#61233 = ORIENTED_EDGE ( 'NONE', *, *, #46002, .T. ) ;
#61234 = ORIENTED_EDGE ( 'NONE', *, *, #18620, .F. ) ;
#61235 = CARTESIAN_POINT ( 'NONE',  ( 24.72675015352175620, -3.119025593723015355, -11.78403009279797864 ) ) ;
#61236 = CARTESIAN_POINT ( 'NONE',  ( 10.90000000000000036, 0.000000000000000000, 0.000000000000000000 ) ) ;
#61237 = EDGE_CURVE ( 'NONE', #34497, #65244, #20059, .T. ) ;
#61238 = CARTESIAN_POINT ( 'NONE',  ( 9.215291255903000689, 4.861981595026999337, 8.938817176893000038 ) ) ;
#61239 = ADVANCED_FACE ( 'NONE', ( #49754 ), #21508, .T. ) ;
#61240 = CARTESIAN_POINT ( 'NONE',  ( 10.01597178489000051, 4.792666960550000077, -6.390258598531999290 ) ) ;
#61241 = CARTESIAN_POINT ( 'NONE',  ( 8.706911754519369495, 3.704150863171606467, -8.842717511604519132 ) ) ;
#61242 = CARTESIAN_POINT ( 'NONE',  ( 10.25888544622000076, -4.512389816463000081, 5.993697694029000544 ) ) ;
#61243 = CARTESIAN_POINT ( 'NONE',  ( 11.84006751466700180, 3.254324250158000087, -11.33670592834999979 ) ) ;
#61244 = CARTESIAN_POINT ( 'NONE',  ( 10.28773706650000008, -5.077599250153999932, -5.991350640809000261 ) ) ;
#61245 = CARTESIAN_POINT ( 'NONE',  ( 11.60948876160955479, -4.695527826393099957, -8.223320049540498999 ) ) ;
#61246 =( LENGTH_UNIT ( ) NAMED_UNIT ( * ) SI_UNIT ( .MILLI., .METRE. ) );
#61247 = EDGE_LOOP ( 'NONE', ( #30008, #28695, #64877, #57667 ) ) ;
#61248 = CARTESIAN_POINT ( 'NONE',  ( 8.837278925393345475, 4.883321897350202612, -6.987098574663183292 ) ) ;
#61249 = CARTESIAN_POINT ( 'NONE',  ( 24.51106053578591926, 8.765536724423055759, 8.765535773142982379 ) ) ;
#61250 = AXIS2_PLACEMENT_3D ( 'NONE', #14304, #62858, #46458 ) ;
#61251 = CARTESIAN_POINT ( 'NONE',  ( 5.000030787343000327, 2.045306479342561268, -0.5496608443529887866 ) ) ;
#61252 = CARTESIAN_POINT ( 'NONE',  ( 10.57088779216199903, 5.183207142131999845, -7.926693309523199282 ) ) ;
#61253 = CARTESIAN_POINT ( 'NONE',  ( 12.18091821863271207, 2.461361028094612546, 13.68154568029715890 ) ) ;
#61254 = CARTESIAN_POINT ( 'NONE',  ( 9.945535518573000999, -2.906050966242999856, 8.880386511481999534 ) ) ;
#61255 = ORIENTED_EDGE ( 'NONE', *, *, #22958, .F. ) ;
#61256 = STYLED_ITEM ( 'NONE', ( #34814 ), #53935 ) ;
#61257 = CARTESIAN_POINT ( 'NONE',  ( 12.23478064045376534, 0.2559538865055897561, -12.69653251249011205 ) ) ;
#61258 = CARTESIAN_POINT ( 'NONE',  ( 12.72332061973729012, -0.6199690124688027604, 13.88138352397878705 ) ) ;
#61259 = ORIENTED_EDGE ( 'NONE', *, *, #42921, .T. ) ;
#61260 = CARTESIAN_POINT ( 'NONE',  ( 24.14470051247585403, 12.92580021110792643, -3.214654389895091224 ) ) ;
#61261 = ADVANCED_FACE ( 'NONE', ( #52852 ), #40986, .T. ) ;
#61262 = LINE ( 'NONE', #9142, #42945 ) ;
#61263 = CARTESIAN_POINT ( 'NONE',  ( 23.91164119559400092, -3.265432764442000035, -12.84207651524999960 ) ) ;
#61264 = AXIS2_PLACEMENT_3D ( 'NONE', #18931, #61577, #35022 ) ;
#61265 = CARTESIAN_POINT ( 'NONE',  ( 7.000000000000000000, 8.307879248642999315, -4.307879248643000203 ) ) ;
#61266 = EDGE_CURVE ( 'NONE', #64893, #29332, #39260, .T. ) ;
#61267 = CARTESIAN_POINT ( 'NONE',  ( 23.60000000000000497, 12.92119138974382864, -5.203241264448742243 ) ) ;
#61268 = FACE_OUTER_BOUND ( 'NONE', #69115, .T. ) ;
#61269 = CARTESIAN_POINT ( 'NONE',  ( 10.90000000000000036, -0.2500000000000000000, 4.902439024389999567 ) ) ;
#61270 = DIRECTION ( 'NONE',  ( 2.709094309399999753E-09, -3.458058237665000178E-11, 1.000000000000000000 ) ) ;
#61271 = CARTESIAN_POINT ( 'NONE',  ( 12.36135608140797615, 3.049327969019413498, 12.22544940668144875 ) ) ;
#61272 = LINE ( 'NONE', #45199, #39713 ) ;
#61273 = CARTESIAN_POINT ( 'NONE',  ( 10.82595391537419971, 4.716560378569699452, -7.986661909549199301 ) ) ;
#61274 = CARTESIAN_POINT ( 'NONE',  ( 12.15762345757557661, -0.3746922850240320679, 12.59513687151645200 ) ) ;
#61275 = CARTESIAN_POINT ( 'NONE',  ( 10.94846415877000112, 3.841064079579000090, -9.341816855317999213 ) ) ;
#61276 = CARTESIAN_POINT ( 'NONE',  ( 9.024747021775999301, 3.141778309999299967, -8.253120162257399528 ) ) ;
#61278 = CARTESIAN_POINT ( 'NONE',  ( 11.12299956498149811, 5.207010770456999893, -7.825000000000000178 ) ) ;
#61277 = CARTESIAN_POINT ( 'NONE',  ( 15.95481756226799952, -8.457314961363000094, -8.223455601337001042 ) ) ;
#61279 = VECTOR ( 'NONE', #54105, 1000.000000000000114 ) ;
#61280 = CARTESIAN_POINT ( 'NONE',  ( 23.66004879239100234, -13.39256420742000131, 3.813548264891000183 ) ) ;
#61281 = VERTEX_POINT ( 'NONE', #52155 ) ;
#61282 = ADVANCED_FACE ( 'NONE', ( #9162 ), #30499, .F. ) ;
#61283 = CARTESIAN_POINT ( 'NONE',  ( 9.785087710366283886, -4.544774531727020062, -8.875930998700511054 ) ) ;
#61284 = CARTESIAN_POINT ( 'NONE',  ( 10.24961784311999935, -4.184221496660999406, 9.286877953065999947 ) ) ;
#61285 = CARTESIAN_POINT ( 'NONE',  ( 9.604355082327998616, 3.550486524676900402, 8.398209294002699110 ) ) ;
#61286 = CARTESIAN_POINT ( 'NONE',  ( 10.21473687196862734, 3.686226525417862998, -8.316748708918906274 ) ) ;
#61287 = B_SPLINE_CURVE_WITH_KNOTS ( 'NONE', 3,
 ( #17368, #59671, #64555, #5836 ),
 .UNSPECIFIED., .F., .F.,
 ( 4, 4 ),
 ( 0.000000000000000000, 1.000000000000000000 ),
 .UNSPECIFIED. ) ;
#61288 = CARTESIAN_POINT ( 'NONE',  ( 10.56492304196000021, -4.212244324161999565, 8.933470634735002136 ) ) ;
#61289 = DIRECTION ( 'NONE',  ( 1.000000000000000000, 0.000000000000000000, 0.000000000000000000 ) ) ;
#61290 = ORIENTED_EDGE ( 'NONE', *, *, #14445, .T. ) ;
#61291 = CARTESIAN_POINT ( 'NONE',  ( 9.328696787962998727, -3.803923679411099990, -6.375149554610999303 ) ) ;
#61292 = CARTESIAN_POINT ( 'NONE',  ( 4.650000881942629505, 3.375077994860000042E-14, 1.048050535245999973E-13 ) ) ;
#61293 = CARTESIAN_POINT ( 'NONE',  ( 18.02779610229248064, 1.934613261143887319, -12.45059556317631788 ) ) ;
#61294 = CARTESIAN_POINT ( 'NONE',  ( 6.966665878460972294, 12.09896511371893446, 3.276379751798347506 ) ) ;
#61295 = FACE_OUTER_BOUND ( 'NONE', #33953, .T. ) ;
#61296 = CARTESIAN_POINT ( 'NONE',  ( 11.36333594839950045, 4.659759757475400832, -6.743912759487099784 ) ) ;
#61297 = CARTESIAN_POINT ( 'NONE',  ( 12.21068878750229381, 2.693668765628876027, -13.63048043068445381 ) ) ;
#61299 = CARTESIAN_POINT ( 'NONE',  ( 9.480151033051999576, -4.233164088428999605, -6.141918726850000176 ) ) ;
#61298 = VECTOR ( 'NONE', #37286, 1000.000000000000000 ) ;
#61300 = CARTESIAN_POINT ( 'NONE',  ( 25.29574884316900096, 11.38516889222999851, 3.114186424562000344 ) ) ;
#61301 = ORIENTED_EDGE ( 'NONE', *, *, #65261, .T. ) ;
#61302 = CARTESIAN_POINT ( 'NONE',  ( 9.883148997457000817, -5.167567567567999731, 6.822293592207000934 ) ) ;
#61303 = CARTESIAN_POINT ( 'NONE',  ( 12.38211732427673439, -0.5935699150349511566, -13.98741755999924941 ) ) ;
#61304 = DIRECTION ( 'NONE',  ( -1.000000000000000000, 0.000000000000000000, 0.000000000000000000 ) ) ;
#61305 = CARTESIAN_POINT ( 'NONE',  ( 2.250973465874000379, -3.500000000000000000, 0.000000000000000000 ) ) ;
#61306 = CARTESIAN_POINT ( 'NONE',  ( 8.142589158771000868, 5.074768364528000397, -8.296267706722000312 ) ) ;
#61307 = CARTESIAN_POINT ( 'NONE',  ( 6.670294783753479173, -0.1881139380374373116, -1.513300629325556201 ) ) ;
#61308 = ORIENTED_EDGE ( 'NONE', *, *, #30805, .T. ) ;
#61309 = CARTESIAN_POINT ( 'NONE',  ( 9.365000000002998704, -2.649999999999999911, -7.500000000000000000 ) ) ;
#61310 = CARTESIAN_POINT ( 'NONE',  ( 18.18010564875746837, 2.481546250174181623, -13.67737493447379293 ) ) ;
#61311 = ORIENTED_EDGE ( 'NONE', *, *, #43087, .F. ) ;
#61312 = CYLINDRICAL_SURFACE ( 'NONE', #46250, 1.350000000000000089 ) ;
#61313 = CARTESIAN_POINT ( 'NONE',  ( 24.72250568140215421, 3.121164773874959497, 11.78765955954131606 ) ) ;
#61314 = CARTESIAN_POINT ( 'NONE',  ( 8.912754719595000097, 2.481540185810000132, -7.878707153279001396 ) ) ;
#61315 = EDGE_CURVE ( 'NONE', #53307, #55375, #4258, .T. ) ;
#61316 = CARTESIAN_POINT ( 'NONE',  ( 9.143927823787139531, 5.249988444743198812, 7.500000155056751439 ) ) ;
#61317 = EDGE_CURVE ( 'NONE', #59495, #14714, #37640, .T. ) ;
#61318 = CARTESIAN_POINT ( 'NONE',  ( 11.10612378248509913, -4.482960757953799558, -6.586279795136899651 ) ) ;
#61319 = CARTESIAN_POINT ( 'NONE',  ( 1.699999999999999956, 0.000000000000000000, 0.000000000000000000 ) ) ;
#61320 = ADVANCED_FACE ( 'NONE', ( #57741 ), #53543, .F. ) ;
#61321 = CARTESIAN_POINT ( 'NONE',  ( 10.34184687351566545, -4.999583552997724389, 8.268183399968647151 ) ) ;
#61322 = ORIENTED_EDGE ( 'NONE', *, *, #36484, .T. ) ;
#61323 = CARTESIAN_POINT ( 'NONE',  ( 7.700135044850973998, 4.657064392362385341, -8.696559172435133434 ) ) ;
#61324 = LINE ( 'NONE', #51512, #42894 ) ;
#61325 = CARTESIAN_POINT ( 'NONE',  ( 18.12577783848301038, -2.244501219366055622, 13.72435250368118531 ) ) ;
#61326 = EDGE_LOOP ( 'NONE', ( #59214, #2840, #42514, #5542 ) ) ;
#61327 = CARTESIAN_POINT ( 'NONE',  ( 10.13381533919000077, 5.176445833090999926, -8.189798585019000043 ) ) ;
#61328 = DIRECTION ( 'NONE',  ( 0.000000000000000000, -1.000000000000000000, 0.000000000000000000 ) ) ;
#61329 = VERTEX_POINT ( 'NONE', #22748 ) ;
#61330 = CARTESIAN_POINT ( 'NONE',  ( 9.556659112603998807, 3.503852111758100296, 6.471616938597000157 ) ) ;
#61331 = B_SPLINE_CURVE_WITH_KNOTS ( 'NONE', 3,
 ( #45520, #66830, #7064, #60211, #12317, #33648, #49365, #8108, #28054, #33300, #18256, #23144, #1478, #61248, #39576, #29452 ),
 .UNSPECIFIED., .F., .F.,
 ( 4, 2, 2, 2, 2, 2, 2, 4 ),
 ( 0.000000000000000000, 0.1250000000000004718, 0.2500000000000009437, 0.3750000000000014433, 0.5000000000000018874, 0.6250000000000015543, 0.7500000000000012212, 1.000000000000000000 ),
 .UNSPECIFIED. ) ;
#61332 = CARTESIAN_POINT ( 'NONE',  ( 18.16391642019722141, -2.089583161048361948, -12.42552483951006614 ) ) ;
#61333 = CARTESIAN_POINT ( 'NONE',  ( 24.30000000000000071, -8.756202924575998026, -7.455126447192999883 ) ) ;
#61334 = CARTESIAN_POINT ( 'NONE',  ( 23.89320776801300283, 1.894218448865001792, 11.32736289216000536 ) ) ;
#61335 = B_SPLINE_CURVE_WITH_KNOTS ( 'NONE', 3,
 ( #46624, #62683, #35785, #45930, #18676, #9199, #45251, #51853, #30542, #40339 ),
 .UNSPECIFIED., .F., .F.,
 ( 4, 2, 2, 2, 4 ),
 ( 0.000000000000000000, 0.2500000000000000000, 0.5000000000000000000, 0.7500000000000000000, 1.000000000000000000 ),
 .UNSPECIFIED. ) ;
#61336 = CARTESIAN_POINT ( 'NONE',  ( 8.440795537699267825, 5.100000000000000533, 6.662590550601105832 ) ) ;
#61337 = CARTESIAN_POINT ( 'NONE',  ( 9.382636167377327752, -2.846367580966820299, 8.802155020956973885 ) ) ;
#61338 = ORIENTED_EDGE ( 'NONE', *, *, #62690, .F. ) ;
#61339 = CARTESIAN_POINT ( 'NONE',  ( 24.54174074851747989, -3.611931245578916094, 12.30360799784193837 ) ) ;
#61340 = CARTESIAN_POINT ( 'NONE',  ( 10.41025778040999938, 4.690688562647999937, -6.142866736126999960 ) ) ;
#61341 = CARTESIAN_POINT ( 'NONE',  ( 10.96543126312000105, -5.152333517825000264, -5.068250443055999810 ) ) ;
#61342 = CARTESIAN_POINT ( 'NONE',  ( 12.11838997910883720, 2.753273141185786255, -13.72661716423428935 ) ) ;
#61343 = CARTESIAN_POINT ( 'NONE',  ( 10.01163399569799850, -2.865156490077000129, -7.625954975973699312 ) ) ;
#61344 = CARTESIAN_POINT ( 'NONE',  ( 10.00137895011999944, -3.855365288061999962, 5.709482985498999241 ) ) ;
#61345 = CARTESIAN_POINT ( 'NONE',  ( 17.60287317832943543, -0.7290248443971262260, 13.98100598729141097 ) ) ;
#61346 = CARTESIAN_POINT ( 'NONE',  ( 7.838687487314834890, 4.995567223853333516, 6.525491811874558401 ) ) ;
#61347 = B_SPLINE_CURVE_WITH_KNOTS ( 'NONE', 3,
 ( #39877, #13315, #40218, #61535, #40548, #35318, #13650, #46145, #67451, #41924, #63584, #5203, #17336, #69174, #38665, #15360, #21284, #58342 ),
 .UNSPECIFIED., .F., .F.,
 ( 4, 2, 2, 2, 2, 2, 2, 2, 4 ),
 ( 0.000000000000000000, 0.1249999999999999445, 0.2499999999999998890, 0.3749999999999998335, 0.4999999999999997780, 0.6249999999999997780, 0.7499999999999998890, 0.8749999999999998890, 1.000000000000000000 ),
 .UNSPECIFIED. ) ;
#61348 = ORIENTED_EDGE ( 'NONE', *, *, #67496, .T. ) ;
#61349 = ORIENTED_EDGE ( 'NONE', *, *, #48260, .F. ) ;
#61350 = CARTESIAN_POINT ( 'NONE',  ( 8.789679719592999874, 4.162493982103000256, -5.775210092227999858 ) ) ;
#61351 = CARTESIAN_POINT ( 'NONE',  ( 10.57314899745999881, 5.167567567567999731, -6.822293592207000934 ) ) ;
#61352 = CARTESIAN_POINT ( 'NONE',  ( 12.48799821679275546, -1.955167389913696763, 13.77408040568291803 ) ) ;
#61353 = CARTESIAN_POINT ( 'NONE',  ( 9.285047233936884581, -4.827112843486829341, 9.039507299413969577 ) ) ;
#61354 = CARTESIAN_POINT ( 'NONE',  ( 24.22025221778200077, 8.983854323373000383, -8.868431746691999962 ) ) ;
#61355 = CARTESIAN_POINT ( 'NONE',  ( 10.29522949779699914, 4.480999174483200065, -8.221351791991999391 ) ) ;
#61357 = CARTESIAN_POINT ( 'NONE',  ( 11.07071157029000119, -6.643654070931000355, 5.582937608692000175 ) ) ;
#61356 = CARTESIAN_POINT ( 'NONE',  ( 10.94222949779799947, -3.366547096154099972, 6.550014196338999284 ) ) ;
#61358 = CARTESIAN_POINT ( 'NONE',  ( 8.489692067425998800, -4.486659167649003521, -6.565674902303003435 ) ) ;
#61359 = ORIENTED_EDGE ( 'NONE', *, *, #14327, .F. ) ;
#61360 = CARTESIAN_POINT ( 'NONE',  ( 10.26195635248000038, -3.348682106447000262, 4.591198220724000301 ) ) ;
#61361 = ADVANCED_FACE ( 'NONE', ( #5633 ), #11561, .T. ) ;
#61362 = CARTESIAN_POINT ( 'NONE',  ( 7.000000000000000000, -6.255435840762999966, 3.000000000000000000 ) ) ;
#61363 = CARTESIAN_POINT ( 'NONE',  ( 8.573148997459998810, 5.167567567567999731, -6.822293592207000934 ) ) ;
#61364 = CARTESIAN_POINT ( 'NONE',  ( 12.18504239631809405, 0.08143391461294853528, 12.69966978410897518 ) ) ;
#61365 = EDGE_CURVE ( 'NONE', #11513, #31652, #40993, .T. ) ;
#61366 = DIRECTION ( 'NONE',  ( 0.000000000000000000, 0.9553735099700839672, 0.2954005017724949389 ) ) ;
#61367 = ORIENTED_EDGE ( 'NONE', *, *, #66052, .F. ) ;
#61369 = CARTESIAN_POINT ( 'NONE',  ( 9.924988015501618577, 5.349815781279066762, 7.500001845592777272 ) ) ;
#61368 = DIRECTION ( 'NONE',  ( 1.000000000000000000, 0.000000000000000000, 0.000000000000000000 ) ) ;
#61370 = CARTESIAN_POINT ( 'NONE',  ( 24.44496356299600137, 12.03536643057000077, 3.224849944858999784 ) ) ;
#61371 = DIRECTION ( 'NONE',  ( 0.000000000000000000, 0.000000000000000000, -1.000000000000000000 ) ) ;
#61372 = AXIS2_PLACEMENT_3D ( 'NONE', #40578, #45147, #17888 ) ;
#61373 = CARTESIAN_POINT ( 'NONE',  ( 10.88733729122639993, 2.722429312291999803, 7.533608309972310124 ) ) ;
#61374 = DIRECTION ( 'NONE',  ( 1.000000000000000000, 0.000000000000000000, 0.000000000000000000 ) ) ;
#61375 = B_SPLINE_SURFACE_WITH_KNOTS ( 'NONE', 1, 3, ( 
 ( #42835, #26770, #11355, #16940, #15912, #11698, #59600, #6454, #58916, #37582, #184, #27804, #22534, #43873, #65179, #5081, #21502, #69060, #21166, #42494, #63803, #37246, #64144, #16259, #32356, #17999, #23237, #50841, #44917, #34082, #44581, #38978, #66221, #23925, #65527, #61332, #18344, #39663, #39318, #60640, #33735, #13101, #34433, #55749, #50156, #59944, #60296, #7849, #29540, #12751, #6802, #29184, #55397, #50493, #45260, #12404, #2938, #2594, #12055, #66565, #55051, #60986, #28139, #23574, #18684, #7154, #40017, #28489, #24267, #33388, #49807, #1917, #13451, #65873, #34772, #54704, #49453, #7493, #28848, #45604, #56081, #2260, #8190, #17298, #38623, #1562, #22884, #44235, #17655, #14129, #19023, #8534, #9905, #3619, #35456, #20395, #67590, #30894, #66908, #56781, #46632, #25297, #25642, #35793 ),
 ( #46972, #62689, #3958, #3285, #13786, #57108, #30548, #24954, #46286, #36131, #24615, #67938, #20054, #41721, #8879, #9206, #29882, #45938, #51189, #51862, #67249, #30214, #14812, #19364, #40349, #51519, #15152, #63022, #62357, #36473, #31244, #9553, #41382, #57445, #52207, #25988, #19714, #57793, #40687, #4308, #35118, #68275, #61670, #52551, #4648, #56430, #62016, #41034, #14475, #16177, #37503, #63721, #11272, #15500, #42753, #47316, #42068, #99, #64056, #5683, #43450, #64746, #53588, #11612, #27024, #68974, #53923, #10589, #4998, #444, #48001, #16519, #52902, #36828, #68621, #54267, #16860, #21087, #21759, #58826, #31928, #10935, #6024, #43096, #48338, #26336, #63376, #32277, #64398, #5341, #26685, #37848, #47659, #59171, #32613, #791, #15834, #27364, #10245, #42414, #31583, #48687, #37164, #53241 ) ),
 .UNSPECIFIED., .F., .F., .F.,
 ( 2, 2 ),
 ( 4, 2, 2, 2, 2, 2, 2, 2, 2, 2, 2, 2, 2, 2, 2, 2, 2, 2, 2, 2, 2, 2, 2, 2, 2, 2, 2, 2, 2, 2, 2, 2, 2, 2, 2, 2, 2, 2, 2, 2, 2, 2, 2, 2, 2, 2, 2, 2, 2, 2, 2, 4 ),
 ( 0.000000000000000000, 1.000000000000000000 ),
 ( 0.000000000000000000, 7.157017711320847928E-05, 0.0001431403542264169586, 0.0002147105313396254378, 0.0002326030756179275644, 0.0002504956198962296639, 0.0002862807084528339171, 0.0003220657970094381703, 0.0003578508855660424235, 0.0003936359741226466225, 0.0004294210626792508757, 0.0004652061512358551289, 0.0005009912397924593279, 0.0005367763283490635268, 0.0005725614169056678342, 0.0006441315940188763406, 0.0006799166825754805396, 0.0007157017711320848470, 0.0007335943154103870007, 0.0007514868596886890460, 0.0007872719482452932450, 0.0008588421253585017514, 0.0008946272139151059503, 0.0009304123024717102577, 0.0009661973910283144567, 0.001001982479584918656, 0.001073552656698127054, 0.001145122833811335668, 0.001216693010924544283, 0.001288263188037752681, 0.001359833365150961079, 0.001395618453707565387, 0.001431403542264169694, 0.001467188630820774001, 0.001502973719377378092, 0.001574543896490586490, 0.001646114073603795105, 0.001681899162160399412, 0.001717684250717003503, 0.001735576794995305656, 0.001753469339273607593, 0.001789254427830211901, 0.001860824604943420515, 0.001896609693500024823, 0.001932394782056628913, 0.001968179870613233004, 0.001986072414891535375, 0.002003964959169837311, 0.002075535136283045493, 0.002147105313396254107, 0.002218675490509462722, 0.002290245667622671337 ),
 .UNSPECIFIED. ) ;
#61376 = CARTESIAN_POINT ( 'NONE',  ( 8.205992358813000820, 3.399999999999999911, 6.138278517057000450 ) ) ;
#61377 = CARTESIAN_POINT ( 'NONE',  ( 2.070791208532999583, 2.973679562143999533, -2.014976181196999949 ) ) ;
#61378 = ORIENTED_EDGE ( 'NONE', *, *, #50916, .T. ) ;
#61379 = CARTESIAN_POINT ( 'NONE',  ( 12.45211143562937117, 0.6284163952874691761, -12.58432055988357767 ) ) ;
#61380 = CARTESIAN_POINT ( 'NONE',  ( 11.00000000000000000, 2.941427501403999667, -7.825000000000000178 ) ) ;
#61381 = CARTESIAN_POINT ( 'NONE',  ( 23.80948493899275675, -13.00802406696185543, -3.693054094325271652 ) ) ;
#61382 = CARTESIAN_POINT ( 'NONE',  ( 24.43232361759900328, 3.176382763002000509, -12.00226528444000174 ) ) ;
#61383 = DIRECTION ( 'NONE',  ( 1.000000000000000000, 0.000000000000000000, 0.000000000000000000 ) ) ;
#61384 = ORIENTED_EDGE ( 'NONE', *, *, #26917, .F. ) ;
#61385 = CARTESIAN_POINT ( 'NONE',  ( 6.602250463385000323, 1.103230901197000069, 0.4075104821199000416 ) ) ;
#61386 = CARTESIAN_POINT ( 'NONE',  ( 7.291685841229000431, 2.836301549691000012, -8.273864296493000481 ) ) ;
#61387 = CARTESIAN_POINT ( 'NONE',  ( 17.55505043854143565, 2.500000000000000000, -25.00000000000000000 ) ) ;
#61388 = CARTESIAN_POINT ( 'NONE',  ( 10.09964828895399869, 5.121614868497999851, 6.887384543790600056 ) ) ;
#61389 = CARTESIAN_POINT ( 'NONE',  ( 11.84388784977539899, 2.744254309011999737, -7.428242901739219306 ) ) ;
#61390 = VERTEX_POINT ( 'NONE', #43745 ) ;
#61391 = CARTESIAN_POINT ( 'NONE',  ( 9.869049086607999399, -5.575175898444999945, 7.724300702620999104 ) ) ;
#61392 = ORIENTED_EDGE ( 'NONE', *, *, #47801, .F. ) ;
#61393 = CARTESIAN_POINT ( 'NONE',  ( 9.842711596872401714, -5.100000000000000533, -6.305985889525932642 ) ) ;
#61394 = CARTESIAN_POINT ( 'NONE',  ( 8.689254440380000943, -2.550228841911000188, 7.666975032000999946 ) ) ;
#61395 = CARTESIAN_POINT ( 'NONE',  ( 18.03319344185666040, -0.5490318484135096044, -13.98923259457975732 ) ) ;
#61396 = B_SPLINE_CURVE_WITH_KNOTS ( 'NONE', 3,
 ( #37069, #4207, #57344, #41282, #42324, #30791, #26583, #62591, #58048, #58381, #25545, #46870, #16073, #68177 ),
 .UNSPECIFIED., .F., .F.,
 ( 4, 2, 2, 2, 2, 2, 4 ),
 ( 0.000000000000000000, 0.1250000000000009159, 0.2500000000000018319, 0.5000000000000023315, 0.6250000000000025535, 0.7500000000000026645, 1.000000000000000000 ),
 .UNSPECIFIED. ) ;
#61397 = EDGE_LOOP ( 'NONE', ( #59759, #43695, #44794, #65391 ) ) ;
#61398 = CARTESIAN_POINT ( 'NONE',  ( 9.140753410162000492, 5.100000000000000533, 6.175944241622000064 ) ) ;
#61399 = EDGE_CURVE ( 'NONE', #48015, #43460, #16131, .T. ) ;
#61400 = CARTESIAN_POINT ( 'NONE',  ( 25.59997255263800042, -11.07537722176000017, -3.096069202785999952 ) ) ;
#61401 = CARTESIAN_POINT ( 'NONE',  ( 10.30226354018333268, -5.092232985442821658, 8.129523725463625894 ) ) ;
#61402 = CARTESIAN_POINT ( 'NONE',  ( 25.29995734509200034, 8.533537492639000632, -7.925519463018001254 ) ) ;
#61403 = EDGE_CURVE ( 'NONE', #43301, #64554, #48983, .T. ) ;
#61404 = CARTESIAN_POINT ( 'NONE',  ( 23.60000000000000142, 2.204728229456999866, 11.99913219504999873 ) ) ;
#61405 = ORIENTED_EDGE ( 'NONE', *, *, #53352, .T. ) ;
#61406 = CARTESIAN_POINT ( 'NONE',  ( 11.59999999999999964, 3.182579051151299687, -7.174999999999999822 ) ) ;
#61407 = EDGE_CURVE ( 'NONE', #9344, #67932, #38845, .T. ) ;
#61408 = CARTESIAN_POINT ( 'NONE',  ( 12.36816014208256043, -2.947033975326387445, -13.56836638442085530 ) ) ;
#61409 = CARTESIAN_POINT ( 'NONE',  ( 10.39393020684999946, 2.750000000000000000, 7.500000000000000000 ) ) ;
#61410 =( NAMED_UNIT ( * ) PLANE_ANGLE_UNIT ( ) SI_UNIT ( $, .RADIAN. ) );
#61411 = B_SPLINE_CURVE_WITH_KNOTS ( 'NONE', 3,
 ( #33548, #16757, #5925, #48936 ),
 .UNSPECIFIED., .F., .F.,
 ( 4, 4 ),
 ( 0.000000000000000000, 1.000000000000000000 ),
 .UNSPECIFIED. ) ;
#61412 = DIRECTION ( 'NONE',  ( 0.000000000000000000, 0.000000000000000000, -1.000000000000000000 ) ) ;
#61413 = VERTEX_POINT ( 'NONE', #22054 ) ;
#61414 = CARTESIAN_POINT ( 'NONE',  ( 23.66004879239100234, -3.393652723963000106, -13.50507488346000073 ) ) ;
#61415 = CARTESIAN_POINT ( 'NONE',  ( 10.93937577273821482, 3.538822733277925181, -8.699885912910445995 ) ) ;
#61416 = CARTESIAN_POINT ( 'NONE',  ( 6.944122165046020534, 4.487799988764965775, -9.291988751869498131 ) ) ;
#61417 = CARTESIAN_POINT ( 'NONE',  ( 9.957691290288998687, -4.889436474118637577, -8.413289387078533466 ) ) ;
#61418 = CARTESIAN_POINT ( 'NONE',  ( 11.49999672495000169, -3.632761979779000061, 11.06912554803999882 ) ) ;
#61419 = CARTESIAN_POINT ( 'NONE',  ( 12.33502240264713379, 0.4124479947379849909, -13.89177559470775236 ) ) ;
#61420 = CARTESIAN_POINT ( 'NONE',  ( 18.08840168032791951, -2.173540213500963159, 12.52169971385178471 ) ) ;
#61421 = ORIENTED_EDGE ( 'NONE', *, *, #38258, .T. ) ;
#61422 = CARTESIAN_POINT ( 'NONE',  ( 10.64902344389989963, -4.883530143601199747, -6.963800219468099684 ) ) ;
#61423 = ORIENTED_EDGE ( 'NONE', *, *, #62643, .T. ) ;
#61424 = EDGE_CURVE ( 'NONE', #68269, #252, #60930, .T. ) ;
#61425 = AXIS2_PLACEMENT_3D ( 'NONE', #20886, #15980, #11084 ) ;
#61426 = CARTESIAN_POINT ( 'NONE',  ( 18.16413073598318917, 2.358269131826202791, 13.70246680370518710 ) ) ;
#61427 = CARTESIAN_POINT ( 'NONE',  ( 8.731095280410999138, 2.469361196073999842, -7.826019481986000059 ) ) ;
#61428 = CARTESIAN_POINT ( 'NONE',  ( 3.131913175787999659, -2.986881754985999837, -1.580751239308999967 ) ) ;
#61429 = CARTESIAN_POINT ( 'NONE',  ( 10.27571314244999989, -5.689440078020999714, -7.562019725378000601 ) ) ;
#61430 = DIRECTION ( 'NONE',  ( 0.000000000000000000, -0.7071067811865475727, -0.7071067811865475727 ) ) ;
#61431 = CARTESIAN_POINT ( 'NONE',  ( 23.64073796900200364, 13.18743409422000035, 4.071803983738000454 ) ) ;
#61432 = VERTEX_POINT ( 'NONE', #23792 ) ;
#61433 = CARTESIAN_POINT ( 'NONE',  ( 11.73610538575739959, -2.890527834009000152, 7.765257665594799796 ) ) ;
#61434 = CARTESIAN_POINT ( 'NONE',  ( 10.37873747135000002, 4.882725050998000249, 6.350806206758999650 ) ) ;
#61435 = CARTESIAN_POINT ( 'NONE',  ( 25.30000327618300204, -10.36736154742121130, -5.168041346173475326 ) ) ;
#61436 = CARTESIAN_POINT ( 'NONE',  ( 7.822379440378000481, -4.636725880537000855, 9.378965771357000492 ) ) ;
#61438 = CARTESIAN_POINT ( 'NONE',  ( 9.084332157886041870, 4.271970605703780066, 8.830901773243875041 ) ) ;
#61437 = CARTESIAN_POINT ( 'NONE',  ( 9.414312736919001168, 3.941041961981000430, 5.878350450964999752 ) ) ;
#61439 = CARTESIAN_POINT ( 'NONE',  ( 11.13764426047339917, 4.613828180779599997, -8.461511872390000022 ) ) ;
#61440 = DIRECTION ( 'NONE',  ( -1.000000000000000000, 0.000000000000000000, 0.000000000000000000 ) ) ;
#61441 = EDGE_CURVE ( 'NONE', #4376, #64614, #18556, .T. ) ;
#61442 = CARTESIAN_POINT ( 'NONE',  ( 9.731000818238999983, 3.111278474435999808, -7.967991827203400490 ) ) ;
#61443 = CARTESIAN_POINT ( 'NONE',  ( 17.85445698522930869, -0.6551943188411679664, 12.58295456804123091 ) ) ;
#61444 = FACE_OUTER_BOUND ( 'NONE', #17672, .T. ) ;
#61445 = CARTESIAN_POINT ( 'NONE',  ( 8.061933748689000367, 4.603465626214999773, -6.221450782568999749 ) ) ;
#61446 = EDGE_CURVE ( 'NONE', #12771, #21149, #10652, .T. ) ;
#61447 = CARTESIAN_POINT ( 'NONE',  ( 11.29596084123000210, 2.828872990872000059, -8.191118698770999629 ) ) ;
#61448 = ORIENTED_EDGE ( 'NONE', *, *, #24242, .F. ) ;
#61449 = CARTESIAN_POINT ( 'NONE',  ( 8.758793146794999984, -3.977267280662000193, 9.308921106447000327 ) ) ;
#61450 = CARTESIAN_POINT ( 'NONE',  ( 18.14726809210091218, 2.096144380837180243, 13.84220294531915485 ) ) ;
#61451 = DIRECTION ( 'NONE',  ( -1.000000000000000000, -5.329070518030000242E-14, 1.243449787539999965E-13 ) ) ;
#61452 = CARTESIAN_POINT ( 'NONE',  ( 10.37835931248476662, 5.126777126150539488, 6.752018918811991455 ) ) ;
#61453 = ORIENTED_EDGE ( 'NONE', *, *, #52394, .F. ) ;
#61454 = CARTESIAN_POINT ( 'NONE',  ( 8.705989158774000813, 2.542862824481000317, 7.419808961972999661 ) ) ;
#61455 = AXIS2_PLACEMENT_3D ( 'NONE', #15504, #68625, #31246 ) ;
#61457 = FACE_OUTER_BOUND ( 'NONE', #10426, .T. ) ;
#61456 = CARTESIAN_POINT ( 'NONE',  ( 9.044210841233001119, 2.773858540272000184, -8.951250717848999727 ) ) ;
#61458 = CARTESIAN_POINT ( 'NONE',  ( 9.508545572907237897, -8.547664595580219071, -6.555873143209844933 ) ) ;
#61459 = VERTEX_POINT ( 'NONE', #49672 ) ;
#61460 = DIRECTION ( 'NONE',  ( -1.000000000000000000, 0.000000000000000000, 0.000000000000000000 ) ) ;
#61461 = CARTESIAN_POINT ( 'NONE',  ( 9.457462135716001583, -5.100000000000000533, -6.571291218949999902 ) ) ;
#61462 = CARTESIAN_POINT ( 'NONE',  ( 11.53148876160955005, 3.209326035813000022, 6.677731919207799294 ) ) ;
#61463 = CARTESIAN_POINT ( 'NONE',  ( 10.13340376756999994, -5.653635692335999607, 6.501829690795999817 ) ) ;
#61464 = PLANE ( 'NONE',  #65602 ) ;
#61465 = ORIENTED_EDGE ( 'NONE', *, *, #16084, .T. ) ;
#61466 = CARTESIAN_POINT ( 'NONE',  ( 11.80852891948700290, -3.296364302329999774, 11.83491796280999964 ) ) ;
#61467 = CARTESIAN_POINT ( 'NONE',  ( 10.16007944038000055, -4.812966563646999596, -8.526591612524001107 ) ) ;
#61468 =( REPRESENTATION_RELATIONSHIP ('NONE','NONE', #10823, #22871 ) REPRESENTATION_RELATIONSHIP_WITH_TRANSFORMATION ( #27773 )SHAPE_REPRESENTATION_RELATIONSHIP( ) );
#61469 = VECTOR ( 'NONE', #25166, 1000.000000000000114 ) ;
#61470 = CARTESIAN_POINT ( 'NONE',  ( 7.906377990995630434, -2.507223990358470989, 8.393237994738566243 ) ) ;
#61471 = CARTESIAN_POINT ( 'NONE',  ( 10.53138988903999973, -5.607755226963999640, 7.280101849877000042 ) ) ;
#61472 = CARTESIAN_POINT ( 'NONE',  ( 10.64391429142989765, -3.977620450637519678, -6.325326139450999641 ) ) ;
#61473 = CARTESIAN_POINT ( 'NONE',  ( 10.41126717315600025, -4.869050473540199597, 8.240598219300300897 ) ) ;
#61474 = ORIENTED_EDGE ( 'NONE', *, *, #9775, .T. ) ;
#61475 = CARTESIAN_POINT ( 'NONE',  ( 9.074999999999999289, -4.417172942406000224, 8.783926296998000538 ) ) ;
#61476 = CARTESIAN_POINT ( 'NONE',  ( 11.24379975933729980, -2.921317947059999920, 7.871126858273000515 ) ) ;
#61477 = EDGE_LOOP ( 'NONE', ( #38194, #35741, #45258, #47230 ) ) ;
#61478 = CARTESIAN_POINT ( 'NONE',  ( 10.67500447327519097, 2.650284540010591439, 7.500001951671590561 ) ) ;
#61479 = ORIENTED_EDGE ( 'NONE', *, *, #37255, .F. ) ;
#61480 = CARTESIAN_POINT ( 'NONE',  ( 9.927742433789001453, -5.651611919872999934, -7.935921913274999184 ) ) ;
#61481 = CARTESIAN_POINT ( 'NONE',  ( 8.903895280414001689, 3.867331042029999999, -9.227339949050001877 ) ) ;
#61482 = CARTESIAN_POINT ( 'NONE',  ( 11.71922412107039868, 4.069539071394910223, -6.185573549454999487 ) ) ;
#61483 = CARTESIAN_POINT ( 'NONE',  ( 18.30008632280270930, 2.887848135250621385E-14, -11.85014035451981762 ) ) ;
#61484 = CARTESIAN_POINT ( 'NONE',  ( 12.18012697958976709, 2.522451323245131771, -12.44635604318887445 ) ) ;
#61485 = EDGE_CURVE ( 'NONE', #48209, #35693, #33442, .T. ) ;
#61486 = CARTESIAN_POINT ( 'NONE',  ( 10.80487885159599948, -3.003595720052600448, 7.618867373350600047 ) ) ;
#61487 = CARTESIAN_POINT ( 'NONE',  ( 11.36190547754509872, -3.108323067758099967, 7.471700551735359852 ) ) ;
#61488 = EDGE_CURVE ( 'NONE', #10241, #2158, #3467, .T. ) ;
#61489 = ORIENTED_EDGE ( 'NONE', *, *, #19877, .F. ) ;
#61490 = CARTESIAN_POINT ( 'NONE',  ( 7.633428764671157829, 3.449330106466649060, 8.750263298858765637 ) ) ;
#61491 = CARTESIAN_POINT ( 'NONE',  ( 8.122956853208000538, -3.566638198986999964, 5.743608852252999775 ) ) ;
#61492 = CARTESIAN_POINT ( 'NONE',  ( 24.07543051757465946, 9.249134803097012636, 9.196971017846948371 ) ) ;
#61493 = ORIENTED_EDGE ( 'NONE', *, *, #67732, .F. ) ;
#61494 = CARTESIAN_POINT ( 'NONE',  ( 12.35979995375152463, -1.912019040637401135, -12.45409236230133843 ) ) ;
#61495 = CARTESIAN_POINT ( 'NONE',  ( 11.69559063708295987, 5.086518862378000883, 7.194517870904999945 ) ) ;
#61496 = CARTESIAN_POINT ( 'NONE',  ( 10.28180685320999999, -3.991526694881000203, -5.814304247846999729 ) ) ;
#61497 = CARTESIAN_POINT ( 'NONE',  ( 10.67726354018259904, 4.629523725463628558, 8.592232985442819881 ) ) ;
#61498 = CARTESIAN_POINT ( 'NONE',  ( 17.97370160627000146, -12.15014996206000042, 3.198998983672000307 ) ) ;
#61499 = CARTESIAN_POINT ( 'NONE',  ( 9.866200267984439165, 5.673313433347823675, -8.064784397742297273 ) ) ;
#61500 = FACE_OUTER_BOUND ( 'NONE', #14899, .T. ) ;
#61501 = CARTESIAN_POINT ( 'NONE',  ( 18.50001572531400029, 2.908166856580999937, -12.18270046149000052 ) ) ;
#61502 = DIRECTION ( 'NONE',  ( -0.000000000000000000, -0.000000000000000000, 1.000000000000000000 ) ) ;
#61503 = CARTESIAN_POINT ( 'NONE',  ( 10.49349279008999858, -4.332388355267299929, -8.734031750754999379 ) ) ;
#61504 = CARTESIAN_POINT ( 'NONE',  ( 17.77301286688680904, -3.166510366255906650, 12.19562279494696178 ) ) ;
#61505 = ORIENTED_EDGE ( 'NONE', *, *, #32993, .F. ) ;
#61506 = ORIENTED_EDGE ( 'NONE', *, *, #38982, .T. ) ;
#61507 = EDGE_CURVE ( 'NONE', #29684, #52776, #15112, .T. ) ;
#61508 =( NAMED_UNIT ( * ) PLANE_ANGLE_UNIT ( ) SI_UNIT ( $, .RADIAN. ) );
#61509 = CARTESIAN_POINT ( 'NONE',  ( 8.417227077245023281, -3.802951429257032334, 6.016322095508296108 ) ) ;
#61510 = CARTESIAN_POINT ( 'NONE',  ( 8.048510972020503473, 4.829207235971519907, 8.579008051763146625 ) ) ;
#61511 = CARTESIAN_POINT ( 'NONE',  ( 10.64447074117000014, 5.073827170570999634, -8.340679549192000053 ) ) ;
#61512 = VECTOR ( 'NONE', #13288, 1000.000000000000114 ) ;
#61513 = CARTESIAN_POINT ( 'NONE',  ( 10.08521345716899908, 4.924890298941200228, 6.659120737011199331 ) ) ;
#61514 = CARTESIAN_POINT ( 'NONE',  ( 17.72206310054079381, 3.180756431682058682, 12.19191584669666462 ) ) ;
#61515 = FACE_OUTER_BOUND ( 'NONE', #63860, .T. ) ;
#61516 = CARTESIAN_POINT ( 'NONE',  ( 10.46432998405999903, 2.042755206296999582, 7.723699495214000343 ) ) ;
#61517 = CIRCLE ( 'NONE', #46990, 2.100000000000000977 ) ;
#61518 = CARTESIAN_POINT ( 'NONE',  ( 9.625583543129627273, -4.871885936991885657, 7.426875573188317148 ) ) ;
#61519 = ORIENTED_EDGE ( 'NONE', *, *, #10835, .F. ) ;
#61520 = CARTESIAN_POINT ( 'NONE',  ( 12.41357648242118294, -2.012680472106853191, 12.55187634341709035 ) ) ;
#61521 = CARTESIAN_POINT ( 'NONE',  ( 9.300405316139999101, -4.213249376011100722, -8.481512610189300361 ) ) ;
#61522 = CARTESIAN_POINT ( 'NONE',  ( 9.444315208305999576, 2.927258006877999641, 8.897018628538001295 ) ) ;
#61523 = CARTESIAN_POINT ( 'NONE',  ( 9.110163692916374956, 5.234200089434220438, 7.754438396796453858 ) ) ;
#61524 = CARTESIAN_POINT ( 'NONE',  ( 10.76841504065829902, 4.914510326623699576, -6.818119527508899935 ) ) ;
#61525 = CARTESIAN_POINT ( 'NONE',  ( 12.24904276456879160, 0.2856309244984035489, 12.69568149856437067 ) ) ;
#61526 = CARTESIAN_POINT ( 'NONE',  ( 7.968176658772001097, 2.280568568659000483, 6.510284508622999233 ) ) ;
#61527 = CARTESIAN_POINT ( 'NONE',  ( 10.43579914648999996, 2.587602126999999808, 6.390037244031000263 ) ) ;
#61528 = CARTESIAN_POINT ( 'NONE',  ( 12.66096866354269856, 1.891485216129971114, 12.57270334283925450 ) ) ;
#61529 = EDGE_CURVE ( 'NONE', #21554, #64636, #21783, .T. ) ;
#61530 = ORIENTED_EDGE ( 'NONE', *, *, #25957, .F. ) ;
#61531 = CARTESIAN_POINT ( 'NONE',  ( 25.48313734979400280, 8.422747986984999713, 7.953661500581000965 ) ) ;
#61532 = CARTESIAN_POINT ( 'NONE',  ( 11.20733594839949809, 4.840266102192999575, -6.537051788466999191 ) ) ;
#61533 = FACE_OUTER_BOUND ( 'NONE', #57257, .T. ) ;
#61535 = CARTESIAN_POINT ( 'NONE',  ( 3.292477888231665872, -3.061624279823272232, -1.756338733055054835 ) ) ;
#61534 = CARTESIAN_POINT ( 'NONE',  ( 11.72003495739535595, -3.351648276372030555, 11.15746180793239795 ) ) ;
#61536 = CARTESIAN_POINT ( 'NONE',  ( 10.28663399569799886, -3.001718438313799808, 7.389201877599999690 ) ) ;
#61537 = CARTESIAN_POINT ( 'NONE',  ( 11.78179573085659904, -3.026866171144600326, -7.668383662421899061 ) ) ;
#61538 = ORIENTED_EDGE ( 'NONE', *, *, #56324, .F. ) ;
#61539 = CARTESIAN_POINT ( 'NONE',  ( 1.391291019826000008, -0.3804460121770000258, -3.739470302966999782 ) ) ;
#61540 = CARTESIAN_POINT ( 'NONE',  ( 17.95718847876655033, -0.4784641821339099543, -12.68786700121472855 ) ) ;
#61541 = LINE ( 'NONE', #56301, #14018 ) ;
#61542 = CARTESIAN_POINT ( 'NONE',  ( 11.79999999771000141, -3.595163221087000149, 11.99793848941000007 ) ) ;
#61543 = CARTESIAN_POINT ( 'NONE',  ( 24.30857393682200041, -12.13191889299999815, 3.290345171485999920 ) ) ;
#61544 = CARTESIAN_POINT ( 'NONE',  ( 15.40000000001299973, 8.815237407733999220, 7.616696375847999967 ) ) ;
#61545 = FACE_OUTER_BOUND ( 'NONE', #25698, .T. ) ;
#61546 = CARTESIAN_POINT ( 'NONE',  ( 9.417725536554337751, -5.345107907813670067, 7.385006124088557833 ) ) ;
#61547 = CARTESIAN_POINT ( 'NONE',  ( 7.373066940378000034, -3.394845988290999816, 9.388942682504000103 ) ) ;
#61548 = VERTEX_POINT ( 'NONE', #2467 ) ;
#61549 = CARTESIAN_POINT ( 'NONE',  ( 8.341920280410999311, 5.601795057054999916, 7.176148573050999957 ) ) ;
#61550 =( BOUNDED_SURFACE ( )  B_SPLINE_SURFACE ( 3, 3, ( 
 ( #41486, #47423, #47081, #15262 ),
 ( #36585, #9314, #4066, #68731 ),
 ( #40795, #62118, #20850, #14236 ),
 ( #8979, #42183, #56535, #67695 ) ),
 .UNSPECIFIED., .F., .F., .T. ) 
 B_SPLINE_SURFACE_WITH_KNOTS ( ( 4, 4 ),
 ( 4, 4 ),
 ( 0.000000000000000000, 1.000000000000000000 ),
 ( 0.000000000000000000, 1.000000000000000000 ),
 .UNSPECIFIED. ) 
 GEOMETRIC_REPRESENTATION_ITEM ( )  RATIONAL_B_SPLINE_SURFACE ( (
 ( 1.512182578520000042, 1.160176301760999840, 1.160176301760999840, 1.512182578520000042),
 ( 1.111288591041000196, 0.8526025270081000196, 0.8526025270081000196, 1.111288591041000196),
 ( 1.111288591041000196, 0.8526025270081000196, 0.8526025270081000196, 1.111288591041000196),
 ( 1.512182578520000042, 1.160176301760999840, 1.160176301760999840, 1.512182578520000042) ) ) 
 REPRESENTATION_ITEM ( '' )  SURFACE ( )  );
#61551 = CARTESIAN_POINT ( 'NONE',  ( 11.59999999999999964, 3.182579051151299687, -7.174999999999999822 ) ) ;
#61552 = DIRECTION ( 'NONE',  ( 0.000000000000000000, -1.000000000000000000, 0.000000000000000000 ) ) ;
#61553 = CARTESIAN_POINT ( 'NONE',  ( 17.83817875645617690, -0.5572864141904814161, 13.88496202738737217 ) ) ;
#61554 = CARTESIAN_POINT ( 'NONE',  ( 1.028018509565999938, -2.208354302538000358, -2.618776384398000090 ) ) ;
#61556 = VERTEX_POINT ( 'NONE', #23097 ) ;
#61555 = B_SPLINE_CURVE_WITH_KNOTS ( 'NONE', 3,
 ( #48057, #37220, #10302, #503, #36884, #58537, #37905, #21819, #43152, #64457 ),
 .UNSPECIFIED., .F., .F.,
 ( 4, 2, 2, 2, 4 ),
 ( 0.000000000000000000, 0.2500000000000001665, 0.5000000000000003331, 0.7500000000000001110, 1.000000000000000000 ),
 .UNSPECIFIED. ) ;
#61557 = DIRECTION ( 'NONE',  ( 0.000000000000000000, 0.000000000000000000, -1.000000000000000000 ) ) ;
#61558 = CARTESIAN_POINT ( 'NONE',  ( 10.79692742076994527, -5.515504571040683146, -6.594679436486475588 ) ) ;
#61559 = CARTESIAN_POINT ( 'NONE',  ( 9.869051220224999810, 5.575171928796999410, 7.724300137354000562 ) ) ;
#61560 = CARTESIAN_POINT ( 'NONE',  ( 11.78179573085659904, 4.973133828855400118, 7.331616337578100051 ) ) ;
#61562 = CARTESIAN_POINT ( 'NONE',  ( 8.712568288355884150, -5.100000000000000533, 6.329675358928077422 ) ) ;
#61561 = VECTOR ( 'NONE', #4568, 1000.000000000000114 ) ;
#61563 = DIRECTION ( 'NONE',  ( 0.000000000000000000, 0.9693731749023103417, -0.2455924424322025734 ) ) ;
#61564 = FACE_OUTER_BOUND ( 'NONE', #44734, .T. ) ;
#61565 = CARTESIAN_POINT ( 'NONE',  ( 18.47825479160223239, 3.085175724107807493, -12.13916519603725419 ) ) ;
#61566 = EDGE_CURVE ( 'NONE', #52202, #41699, #30116, .T. ) ;
#61567 = CARTESIAN_POINT ( 'NONE',  ( 12.19239630168272726, -2.623612345332759777, 12.42193400450689289 ) ) ;
#61568 = ADVANCED_FACE ( 'NONE', ( #60854 ), #34645, .T. ) ;
#61569 = CARTESIAN_POINT ( 'NONE',  ( 7.907666719952700873, 2.506162197551407012, 8.397413729663252724 ) ) ;
#61570 = ORIENTED_EDGE ( 'NONE', *, *, #2747, .T. ) ;
#61571 = CARTESIAN_POINT ( 'NONE',  ( 17.97976423439218507, -3.110159202364634723, 13.65016833014880682 ) ) ;
#61572 = DIRECTION ( 'NONE',  ( 0.000000000000000000, 0.000000000000000000, -1.000000000000000000 ) ) ;
#61573 = ORIENTED_EDGE ( 'NONE', *, *, #52955, .F. ) ;
#61574 = ORIENTED_EDGE ( 'NONE', *, *, #46799, .T. ) ;
#61575 = CARTESIAN_POINT ( 'NONE',  ( 10.73724174883999893, 3.975468761016990094, 6.608211443991299561 ) ) ;
#61576 = CARTESIAN_POINT ( 'NONE',  ( 5.292049206183823351, -1.006254710013267717, 0.5206924512979714814 ) ) ;
#61577 = DIRECTION ( 'NONE',  ( 1.000000000000000000, 0.000000000000000000, 0.000000000000000000 ) ) ;
#61578 = CARTESIAN_POINT ( 'NONE',  ( 10.03490996941999924, 5.615906393494999982, 7.351455918368999143 ) ) ;
#61579 = CARTESIAN_POINT ( 'NONE',  ( 9.701722306758000514, 4.253749110891999585, -8.839930742927998963 ) ) ;
#61580 = CARTESIAN_POINT ( 'NONE',  ( 9.784141369869628235, -3.576408136849907216, -8.265573120213877800 ) ) ;
#61581 = CARTESIAN_POINT ( 'NONE',  ( 9.534903635507999908, -3.030945724184999968, 8.761987396837000119 ) ) ;
#61582 = CARTESIAN_POINT ( 'NONE',  ( 18.23353331006402911, 0.2537702651956263988, -12.59744904646397679 ) ) ;
#61583 = CARTESIAN_POINT ( 'NONE',  ( 10.24845588172999911, -4.234132110154000372, -5.660862927546999934 ) ) ;
#61584 = CARTESIAN_POINT ( 'NONE',  ( 10.87518447801629939, -3.134012688501500055, -7.480906371072489236 ) ) ;
#61585 = CARTESIAN_POINT ( 'NONE',  ( 10.61503919148196218, -5.349978903665073560, -7.499997722305344006 ) ) ;
#61586 = ORIENTED_EDGE ( 'NONE', *, *, #14716, .T. ) ;
#61587 = EDGE_CURVE ( 'NONE', #4653, #20297, #18208, .T. ) ;
#61588 = CARTESIAN_POINT ( 'NONE',  ( 11.02035356290999957, -6.428762174806000651, -5.279064955367999801 ) ) ;
#61589 = CARTESIAN_POINT ( 'NONE',  ( 6.899999691988000450, -12.43893545635000031, -2.828937028792000152 ) ) ;
#61590 = EDGE_CURVE ( 'NONE', #36450, #53853, #5073, .T. ) ;
#61591 = CARTESIAN_POINT ( 'NONE',  ( 9.002599499754321499, 5.050337702473633783, 7.001638755957637628 ) ) ;
#61592 = CARTESIAN_POINT ( 'NONE',  ( 9.785684229509998389, 3.098260518542999886, -6.592668585875199661 ) ) ;
#61593 = CARTESIAN_POINT ( 'NONE',  ( 12.47114117431408076, 3.166196762519381647, 13.63727363649663538 ) ) ;
#61594 = CARTESIAN_POINT ( 'NONE',  ( 11.20563089100999932, -3.509133048232999652, 6.118191305996999674 ) ) ;
#61595 = ORIENTED_EDGE ( 'NONE', *, *, #34469, .F. ) ;
#61596 = CARTESIAN_POINT ( 'NONE',  ( 12.23478131644321998, -0.2564338550251593074, -12.69653134296677699 ) ) ;
#61597 = CARTESIAN_POINT ( 'NONE',  ( 12.78109991897669673, 0.7302151993337113733, 13.98094363222392467 ) ) ;
#61598 = ORIENTED_EDGE ( 'NONE', *, *, #20481, .T. ) ;
#61599 = CARTESIAN_POINT ( 'NONE',  ( 3.500000000000000000, 0.000000000000000000, 0.000000000000000000 ) ) ;
#61600 = CARTESIAN_POINT ( 'NONE',  ( 18.49993212792200126, 2.908182645667999999, 12.18276646858999968 ) ) ;
#61601 = CARTESIAN_POINT ( 'NONE',  ( 24.23189443787899933, -3.402543883684999937, -12.43221920717999929 ) ) ;
#61602 = CARTESIAN_POINT ( 'NONE',  ( 8.379867906096000851, 2.923743482149999906, 6.439439799146000176 ) ) ;
#61603 = CARTESIAN_POINT ( 'NONE',  ( 24.30000000000000071, -2.258942858049999725, -12.29419282279000036 ) ) ;
#61604 = CARTESIAN_POINT ( 'NONE',  ( -0.06014317643898999671, -2.101315454803999838, -2.652019770012000066 ) ) ;
#61605 = VECTOR ( 'NONE', #1024, 1000.000000000000114 ) ;
#61606 = DIRECTION ( 'NONE',  ( 1.000000000000000000, 0.000000000000000000, 0.000000000000000000 ) ) ;
#61607 = LINE ( 'NONE', #51800, #58949 ) ;
#61608 = B_SPLINE_CURVE_WITH_KNOTS ( 'NONE', 3,
 ( #54229, #38147, #17880, #33614 ),
 .UNSPECIFIED., .F., .F.,
 ( 4, 4 ),
 ( 0.000000000000000000, 1.000000000000000000 ),
 .UNSPECIFIED. ) ;
#61609 = CARTESIAN_POINT ( 'NONE',  ( 18.29995268966800026, 2.861739928647000220, 11.98821236628000086 ) ) ;
#61610 = CARTESIAN_POINT ( 'NONE',  ( 10.97364560330029981, 4.265439025801100570, -6.675475461903199736 ) ) ;
#61611 = CARTESIAN_POINT ( 'NONE',  ( 18.28771851938432036, 2.987294196519939327, 11.95930572916780754 ) ) ;
#61612 = CARTESIAN_POINT ( 'NONE',  ( 11.11123293495519881, 3.108594079907299967, -7.464165716332529676 ) ) ;
#61613 = CARTESIAN_POINT ( 'NONE',  ( 9.733963142879998642, 5.117257953482000410, -7.264481182560499128 ) ) ;
#61615 = CARTESIAN_POINT ( 'NONE',  ( 12.18199593246769119, 2.449686698290863163, 12.46314100316935480 ) ) ;
#61614 = CARTESIAN_POINT ( 'NONE',  ( 15.86001156276200064, -8.572187346067000391, -8.239473968622000655 ) ) ;
#61616 = CARTESIAN_POINT ( 'NONE',  ( 23.57927802539584405, -13.36787453502657819, 4.109736056796153392 ) ) ;
#61617 = VERTEX_POINT ( 'NONE', #24485 ) ;
#61618 = CARTESIAN_POINT ( 'NONE',  ( 10.52946886766499901, 3.569835351907400423, 8.281567006984099422 ) ) ;
#61619 = AXIS2_PLACEMENT_3D ( 'NONE', #38368, #21591, #6894 ) ;
#61620 = CARTESIAN_POINT ( 'NONE',  ( 9.972852379787999766, -5.044471434015000533, 6.258101649750000384 ) ) ;
#61621 = EDGE_CURVE ( 'NONE', #19330, #37826, #61541, .T. ) ;
#61622 = EDGE_CURVE ( 'NONE', #8057, #23202, #9416, .T. ) ;
#61623 = CARTESIAN_POINT ( 'NONE',  ( 9.427051052051998781, 4.985712601322500603, 7.307093369932900373 ) ) ;
#61624 = CARTESIAN_POINT ( 'NONE',  ( 10.90540321535548429, -2.790089835004903041, -6.887843015913232669 ) ) ;
#61625 = CARTESIAN_POINT ( 'NONE',  ( 24.44496482743900145, 12.03536723905999928, -3.224852005146999989 ) ) ;
#61626 = LINE ( 'NONE', #60942, #57606 ) ;
#61627 = DIRECTION ( 'NONE',  ( -8.952907862884472301E-11, -0.2714597137497840040, -0.9624498032681421122 ) ) ;
#61628 = ORIENTED_EDGE ( 'NONE', *, *, #34023, .F. ) ;
#61629 = CARTESIAN_POINT ( 'NONE',  ( 8.974088727410999056, -5.137817193984000497, -7.595427884080399927 ) ) ;
#61630 = CARTESIAN_POINT ( 'NONE',  ( 8.620740978634000129, 4.599999999999999645, 5.898823289756999877 ) ) ;
#61631 = B_SPLINE_CURVE_WITH_KNOTS ( 'NONE', 3,
 ( #58450, #62990, #57756, #15803 ),
 .UNSPECIFIED., .F., .F.,
 ( 4, 4 ),
 ( 0.000000000000000000, 1.000000000000000000 ),
 .UNSPECIFIED. ) ;
#61632 = CARTESIAN_POINT ( 'NONE',  ( 18.27597346048318627, 2.401680171065123659, -12.36899652916222436 ) ) ;
#61633 = CARTESIAN_POINT ( 'NONE',  ( 10.96922972661000095, -2.855437608211000011, 5.027789437851001075 ) ) ;
#61634 = CARTESIAN_POINT ( 'NONE',  ( 5.000000000000000000, -1.199999999999999956, 9.776630298829998011 ) ) ;
#61635 = CARTESIAN_POINT ( 'NONE',  ( 7.726096713366001900, 2.834812733921999062, 6.825604963486997079 ) ) ;
#61636 = CARTESIAN_POINT ( 'NONE',  ( 9.751909913808001207, -4.316974633926000671, -5.653758079558000027 ) ) ;
#61637 = CARTESIAN_POINT ( 'NONE',  ( 9.023148997459999876, 5.167567567567999731, -6.822293592207000934 ) ) ;
#61638 = VERTEX_POINT ( 'NONE', #41247 ) ;
#61639 = CARTESIAN_POINT ( 'NONE',  ( 5.500000000000000000, -12.87590651766999983, 2.791353855799999728 ) ) ;
#61640 = CARTESIAN_POINT ( 'NONE',  ( 12.32690743522622334, 0.5490318484135059407, -13.98923259457975732 ) ) ;
#61641 = CARTESIAN_POINT ( 'NONE',  ( 13.59015267864900345, -8.992820872206999994, -7.631366745126000772 ) ) ;
#61642 = EDGE_CURVE ( 'NONE', #16931, #34575, #65396, .T. ) ;
#61643 = DIRECTION ( 'NONE',  ( 1.000000000000000000, 0.000000000000000000, 0.000000000000000000 ) ) ;
#61644 = EDGE_CURVE ( 'NONE', #19777, #39380, #22526, .T. ) ;
#61645 = CARTESIAN_POINT ( 'NONE',  ( 2.335432296257125451, -1.713969392196469377, -3.070236115647940078 ) ) ;
#61646 = CARTESIAN_POINT ( 'NONE',  ( 9.170239158775000732, 4.769103072373000352, -8.666849124598000387 ) ) ;
#61647 = CARTESIAN_POINT ( 'NONE',  ( 12.01518179236249040, -4.180996681294200101, 8.347076615013298451 ) ) ;
#61648 = ORIENTED_EDGE ( 'NONE', *, *, #30234, .F. ) ;
#61649 = CIRCLE ( 'NONE', #60504, 1.649999999999999911 ) ;
#61650 = ADVANCED_FACE ( 'NONE', ( #47531 ), #27114, .T. ) ;
#61651 = CARTESIAN_POINT ( 'NONE',  ( 3.999971066382000284, 2.149963194831999935, 0.000000000000000000 ) ) ;
#61652 = CARTESIAN_POINT ( 'NONE',  ( 18.24190944330472419, 2.752675741764504025, -13.72673684790926529 ) ) ;
#61653 = ORIENTED_EDGE ( 'NONE', *, *, #56436, .T. ) ;
#61654 = CARTESIAN_POINT ( 'NONE',  ( 10.03535508232799955, -4.388021368982800041, 8.275336934318801241 ) ) ;
#61655 = FACE_OUTER_BOUND ( 'NONE', #68107, .T. ) ;
#61656 = CARTESIAN_POINT ( 'NONE',  ( 9.749220280410998640, 5.656948148960999845, -6.994239053114000626 ) ) ;
#61657 = CARTESIAN_POINT ( 'NONE',  ( 9.129282595918651211, 5.249943393780838186, 7.269976573734645342 ) ) ;
#61658 = CARTESIAN_POINT ( 'NONE',  ( 10.89835090130999973, -3.121033016283800254, -8.043647632228999811 ) ) ;
#61659 = CARTESIAN_POINT ( 'NONE',  ( 27.64127793187000037, -5.599999999999999645, 6.571291218949999902 ) ) ;
#61660 = CARTESIAN_POINT ( 'NONE',  ( 8.832144816391009456, -3.783447583457012264, -8.465905425056138967 ) ) ;
#61661 = ORIENTED_EDGE ( 'NONE', *, *, #15554, .F. ) ;
#61662 = CARTESIAN_POINT ( 'NONE',  ( 7.748782164940981154, 3.848159210716703971, -8.857024363427377978 ) ) ;
#61663 = CARTESIAN_POINT ( 'NONE',  ( 10.67726354018233259, -3.370476274536371442, 8.592232985442818105 ) ) ;
#61664 = CARTESIAN_POINT ( 'NONE',  ( 8.649364158774000444, 3.038023536984999939, -5.861661709981000001 ) ) ;
#61665 = VERTEX_POINT ( 'NONE', #39100 ) ;
#61666 = VECTOR ( 'NONE', #15430, 1000.000000000000114 ) ;
#61667 = CARTESIAN_POINT ( 'NONE',  ( 10.18512471524999974, 5.526143977810000329, -7.556025088797999167 ) ) ;
#61668 = ORIENTED_EDGE ( 'NONE', *, *, #19134, .T. ) ;
#61669 = CARTESIAN_POINT ( 'NONE',  ( 9.252709346416999381, 5.031430618794000331, 7.989780896525600085 ) ) ;
#61670 = CARTESIAN_POINT ( 'NONE',  ( 18.12635565526709769, -2.245741716918843611, -12.50718761097852116 ) ) ;
#61671 = ADVANCED_FACE ( 'NONE', ( #23705 ), #25185, .F. ) ;
#61672 = AXIS2_PLACEMENT_3D ( 'NONE', #60829, #2108, #28325 ) ;
#61673 = CARTESIAN_POINT ( 'NONE',  ( 11.53713099069000059, -11.52702260260000067, -1.399766873409999945 ) ) ;
#61674 = LINE ( 'NONE', #56433, #36910 ) ;
#61675 = CARTESIAN_POINT ( 'NONE',  ( 9.408936720234443385, -2.481771157840773512, 8.348873588805004076 ) ) ;
#61676 = ORIENTED_EDGE ( 'NONE', *, *, #68079, .F. ) ;
#61677 = CARTESIAN_POINT ( 'NONE',  ( 11.59999999999999964, 5.064318446328999634, 6.844464917182299324 ) ) ;
#61678 = CARTESIAN_POINT ( 'NONE',  ( 9.907296092384241248, -5.171595203895851256, -8.821442009999598710 ) ) ;
#61679 = CARTESIAN_POINT ( 'NONE',  ( 10.88207481814999866, -5.063049640536999796, -5.075897427045000576 ) ) ;
#61680 = CARTESIAN_POINT ( 'NONE',  ( 12.18685148345900338, 2.135865664097131855, -13.83612956354243906 ) ) ;
#61681 = CARTESIAN_POINT ( 'NONE',  ( 10.06229229006299875, -3.012566816337000297, -6.926667499798199401 ) ) ;
#61682 = B_SPLINE_CURVE_WITH_KNOTS ( 'NONE', 3,
 ( #44910, #17992, #12397, #45599 ),
 .UNSPECIFIED., .F., .F.,
 ( 4, 4 ),
 ( 0.000000000000000000, 1.000000000000000000 ),
 .UNSPECIFIED. ) ;
#61683 = CARTESIAN_POINT ( 'NONE',  ( 9.691080333872001518, -5.335644368206000188, 8.701217921043999937 ) ) ;
#61684 = DIRECTION ( 'NONE',  ( 0.000000000000000000, 0.000000000000000000, -1.000000000000000000 ) ) ;
#61685 = CARTESIAN_POINT ( 'NONE',  ( 10.90000000000000036, -2.899999999999999911, 6.414037451299000381 ) ) ;
#61686 = ORIENTED_EDGE ( 'NONE', *, *, #13825, .T. ) ;
#61687 = VERTEX_POINT ( 'NONE', #34895 ) ;
#61688 = CARTESIAN_POINT ( 'NONE',  ( 10.07367028041000090, 4.905765359186999852, -8.776126235875999271 ) ) ;
#61689 = CARTESIAN_POINT ( 'NONE',  ( 9.272336283620196795, 5.086552246568830427, 8.869404539491238637 ) ) ;
#61690 = CARTESIAN_POINT ( 'NONE',  ( 12.18127175124231165, -2.459544125572825646, 13.68195797703611305 ) ) ;
#61691 = CARTESIAN_POINT ( 'NONE',  ( 23.59999443371599881, 2.915558930973999985, 13.58549620949000136 ) ) ;
#61692 = CARTESIAN_POINT ( 'NONE',  ( 25.46375152665800101, -2.879425814940999917, -11.30951176145000048 ) ) ;
#61693 = CARTESIAN_POINT ( 'NONE',  ( 16.39999999231800132, -3.216285993016000155, -11.40340220863999932 ) ) ;
#61695 = CARTESIAN_POINT ( 'NONE',  ( 8.936935970859920531, 2.275488567576319010, 7.787316285718978826 ) ) ;
#61694 = CARTESIAN_POINT ( 'NONE',  ( 10.20768422950999899, -4.804883439508000897, 8.309874741421300115 ) ) ;
#61696 = CARTESIAN_POINT ( 'NONE',  ( 8.734653236333999260, -4.846210315537001101, -6.250999225331006492 ) ) ;
#61697 = ORIENTED_EDGE ( 'NONE', *, *, #46287, .F. ) ;
#61698 = VECTOR ( 'NONE', #6661, 1000.000000000000000 ) ;
#61699 = CARTESIAN_POINT ( 'NONE',  ( 12.61731565720671000, -0.7069209314891412577, 13.98214394338193678 ) ) ;
#61700 = DIRECTION ( 'NONE',  ( 1.000000000000000000, 0.000000000000000000, 0.000000000000000000 ) ) ;
#61701 = ADVANCED_FACE ( 'NONE', ( #33861 ), #59483, .F. ) ;
#61702 = EDGE_CURVE ( 'NONE', #62483, #22269, #16704, .T. ) ;
#61703 = CARTESIAN_POINT ( 'NONE',  ( 9.490308298768001194, -5.536248950452999473, -7.355084988757000453 ) ) ;
#61704 = CARTESIAN_POINT ( 'NONE',  ( 18.15028814309356520, 0.1908418880314464161, 12.69807545005479810 ) ) ;
#61705 = FACE_OUTER_BOUND ( 'NONE', #59099, .T. ) ;
#61706 = FACE_OUTER_BOUND ( 'NONE', #45936, .T. ) ;
#61707 = CARTESIAN_POINT ( 'NONE',  ( 9.972410841228999345, 4.357364160690000432, -9.282962013144999247 ) ) ;
#61708 = CARTESIAN_POINT ( 'NONE',  ( 8.328787166962994704, -5.102611464338999703, 6.655261220345003004 ) ) ;
#61709 = VECTOR ( 'NONE', #21331, 1000.000000000000000 ) ;
#61710 = LINE ( 'NONE', #44962, #40054 ) ;
#61711 = CARTESIAN_POINT ( 'NONE',  ( 0.3011869175822131095, -0.4312571925403625994, 3.301166135663313295 ) ) ;
#61712 = DIRECTION ( 'NONE',  ( 0.000000000000000000, -0.7198977633594747516, 0.6940801180771756229 ) ) ;
#61713 = ORIENTED_EDGE ( 'NONE', *, *, #30419, .F. ) ;
#61714 = CARTESIAN_POINT ( 'NONE',  ( 12.63954751664500797, 0.7006927685645021331, -12.58050281163331796 ) ) ;
#61715 = CARTESIAN_POINT ( 'NONE',  ( 7.810193361277576685, -3.081125311113132703, 6.468046414883829698 ) ) ;
#61716 = CARTESIAN_POINT ( 'NONE',  ( 24.44496356267099912, -8.810485190366000197, 8.810508100388000585 ) ) ;
#61717 = CARTESIAN_POINT ( 'NONE',  ( 9.026926658770998202, 4.852728889087999598, 8.683917172082999514 ) ) ;
#61718 = CARTESIAN_POINT ( 'NONE',  ( 10.01293113571299997, -5.100000000000000533, 6.444141223344916014 ) ) ;
#61719 = EDGE_LOOP ( 'NONE', ( #5222, #49872, #15988, #15177, #39161 ) ) ;
#61720 = CARTESIAN_POINT ( 'NONE',  ( 6.076234045860000599, 0.7526323975856999970, -1.087207638099000118 ) ) ;
#61721 = CARTESIAN_POINT ( 'NONE',  ( 10.94020963518341460, 9.314146368041843260, 6.233663971910207380 ) ) ;
#61722 = CARTESIAN_POINT ( 'NONE',  ( 10.63789391302369580, 4.829717262113647713, -8.579596796882025700 ) ) ;
#61723 = CARTESIAN_POINT ( 'NONE',  ( 1.584306799206999905, 1.762666431298138825, 3.058252359239908014 ) ) ;
#61724 = CARTESIAN_POINT ( 'NONE',  ( 11.68277869730536977, 3.468607053297499743, -6.452143920160000157 ) ) ;
#61725 = ORIENTED_EDGE ( 'NONE', *, *, #16417, .F. ) ;
#61726 = EDGE_CURVE ( 'NONE', #5681, #34720, #44226, .T. ) ;
#61727 = CARTESIAN_POINT ( 'NONE',  ( 9.778462793022999477, -5.743713977826000239, 7.748300060190000060 ) ) ;
#61728 = ORIENTED_EDGE ( 'NONE', *, *, #65217, .T. ) ;
#61729 = CARTESIAN_POINT ( 'NONE',  ( 21.72233714749290101, 0.000000000000000000, 0.000000000000000000 ) ) ;
#61730 = FACE_OUTER_BOUND ( 'NONE', #38179, .T. ) ;
#61731 = CARTESIAN_POINT ( 'NONE',  ( 18.05115593671926888, 0.5330308249010425881, -13.98985951701901520 ) ) ;
#61732 = VERTEX_POINT ( 'NONE', #6324 ) ;
#61733 = CARTESIAN_POINT ( 'NONE',  ( 10.93864331818477176, 9.341686757170215571, -6.213842809792356370 ) ) ;
#61734 = CARTESIAN_POINT ( 'NONE',  ( 11.08380555355832620, -3.999999927290649460, -9.033895164528411570 ) ) ;
#61735 = DIRECTION ( 'NONE',  ( -1.000000000000000000, 0.000000000000000000, 0.000000000000000000 ) ) ;
#61736 = B_SPLINE_CURVE_WITH_KNOTS ( 'NONE', 3,
 ( #43813, #65108, #49740, #17233 ),
 .UNSPECIFIED., .F., .F.,
 ( 4, 4 ),
 ( 0.000000000000000000, 0.1254138569076999055 ),
 .UNSPECIFIED. ) ;
#61737 = LINE ( 'NONE', #44988, #39844 ) ;
#61738 = CARTESIAN_POINT ( 'NONE',  ( 18.10321044368077281, -2.800384070978154671, 12.37651499848969650 ) ) ;
#61739 = ORIENTED_EDGE ( 'NONE', *, *, #34188, .T. ) ;
#61740 = CARTESIAN_POINT ( 'NONE',  ( 10.15402496696000156, -5.267980706381999667, 5.992344456606999437 ) ) ;
#61741 = CARTESIAN_POINT ( 'NONE',  ( 11.59999999999999787, 4.834915812642035959, 8.298683811023389367 ) ) ;
#61742 = CARTESIAN_POINT ( 'NONE',  ( 10.46684687351657672, 3.231816600031355069, -8.499583552997723501 ) ) ;
#61743 = CARTESIAN_POINT ( 'NONE',  ( 9.883513540182333301, 2.750000000000000000, 7.663624617374469317 ) ) ;
#61744 = AXIS2_PLACEMENT_3D ( 'NONE', #57222, #9324, #17338 ) ;
#61745 = CARTESIAN_POINT ( 'NONE',  ( 11.03775575519999919, -8.050335494570999728, 6.914609630061999468 ) ) ;
#61746 = VERTEX_POINT ( 'NONE', #7031 ) ;
#61747 = PRODUCT ( 'Terminal Screw 1', 'Terminal Screw 1', '', ( #11324 ) ) ;
#61748 = CARTESIAN_POINT ( 'NONE',  ( 23.65871028981190349, 13.20934072687480310, -3.970311354682951155 ) ) ;
#61749 = ADVANCED_FACE ( 'NONE', ( #49329 ), #17166, .F. ) ;
#61750 = CARTESIAN_POINT ( 'NONE',  ( 8.863694533038728451, -3.488685518255360662, -6.614578276768173559 ) ) ;
#61751 = CARTESIAN_POINT ( 'NONE',  ( 3.500000000000000000, 3.126788493178761730, 1.462720483632788060 ) ) ;
#61752 = CARTESIAN_POINT ( 'NONE',  ( 24.11212198533107909, -3.334560347335004948, -12.54180816139383126 ) ) ;
#61753 = CARTESIAN_POINT ( 'NONE',  ( 11.79999999550100220, 3.351258778187000242, -11.15757272551999968 ) ) ;
#61754 = CARTESIAN_POINT ( 'NONE',  ( 12.18532581790793401, 0.08167545936615711044, -13.89968205666727386 ) ) ;
#61755 = CARTESIAN_POINT ( 'NONE',  ( 18.17899100331062101, -2.462234907104897896, 12.46031481527572282 ) ) ;
#61756 = EDGE_LOOP ( 'NONE', ( #53825, #19454, #16675, #13816 ) ) ;
#61757 = CARTESIAN_POINT ( 'NONE',  ( 10.44999293566599974, -3.279967330949900450, -8.383280442119700027 ) ) ;
#61758 = VERTEX_POINT ( 'NONE', #16481 ) ;
#61759 = CARTESIAN_POINT ( 'NONE',  ( 10.53734212242000012, 2.992816679959000137, 8.731689474572998932 ) ) ;
#61760 = PRESENTATION_LAYER_ASSIGNMENT (  '', '', ( #22678 ) ) ;
#61761 = CARTESIAN_POINT ( 'NONE',  ( 25.34480240682214003, -11.16380505725911298, 3.340444239295249584 ) ) ;
#61762 = CARTESIAN_POINT ( 'NONE',  ( 8.441604719589999917, 5.473983809665999622, -8.180077404516000072 ) ) ;
#61763 = CARTESIAN_POINT ( 'NONE',  ( 3.145426443515999981, 0.1831839624298000069, 3.703521834897999909 ) ) ;
#61764 = B_SPLINE_CURVE_WITH_KNOTS ( 'NONE', 3,
 ( #50353, #40889, #18195, #60842 ),
 .UNSPECIFIED., .F., .F.,
 ( 4, 4 ),
 ( 0.000000000000000000, 1.000000000000000000 ),
 .UNSPECIFIED. ) ;
#61765 = CARTESIAN_POINT ( 'NONE',  ( 10.07930721860999945, -2.718124813223000036, -6.397797539448999871 ) ) ;
#61766 = AXIS2_PLACEMENT_3D ( 'NONE', #21005, #52468, #32193 ) ;
#61767 = CARTESIAN_POINT ( 'NONE',  ( 9.660601868375998436, -2.901236202253999696, -6.151180522693000086 ) ) ;
#61768 = VERTEX_POINT ( 'NONE', #17528 ) ;
#61769 = CARTESIAN_POINT ( 'NONE',  ( 11.68687482311540116, -2.942322404451000128, 7.072673169413499217 ) ) ;
#61770 = CARTESIAN_POINT ( 'NONE',  ( 10.19255830160000009, 2.560287027313000063, 7.664549200117999561 ) ) ;
#61771 = LINE ( 'NONE', #55155, #42706 ) ;
#61772 = CARTESIAN_POINT ( 'NONE',  ( 7.437254440376999121, -2.216884807317999861, 8.370075800106999253 ) ) ;
#61773 = B_SPLINE_CURVE_WITH_KNOTS ( 'NONE', 3,
 ( #17677, #39000, #7180, #38296 ),
 .UNSPECIFIED., .F., .F.,
 ( 4, 4 ),
 ( 0.000000000000000000, 1.000000000000000000 ),
 .UNSPECIFIED. ) ;
#61775 = CARTESIAN_POINT ( 'NONE',  ( 11.07299956498199833, -2.792989229543000107, -7.825000000000000178 ) ) ;
#61774 = CARTESIAN_POINT ( 'NONE',  ( 9.194604681486000075, 5.157771204918000230, 8.637848577075999401 ) ) ;
#61776 = CARTESIAN_POINT ( 'NONE',  ( 10.40333997687999990, 4.213854445120500003, -6.519583185858300212 ) ) ;
#61777 = CYLINDRICAL_SURFACE ( 'NONE', #57065, 0.6999999999999992895 ) ;
#61778 = CARTESIAN_POINT ( 'NONE',  ( 8.998468108405997867, 5.098602956001000663, -7.811136554427399403 ) ) ;
#61779 = EDGE_CURVE ( 'NONE', #67987, #51205, #4939, .T. ) ;
#61780 = ADVANCED_FACE ( 'NONE', ( #5985 ), #37810, .T. ) ;
#61781 = CARTESIAN_POINT ( 'NONE',  ( 17.99623368854100036, -0.5708113556792879795, 12.58706429964239071 ) ) ;
#61782 = DIRECTION ( 'NONE',  ( -1.000000000000000000, 0.000000000000000000, 0.000000000000000000 ) ) ;
#61783 = DIRECTION ( 'NONE',  ( -0.7071067811859638175, 0.6115524522396686979, -0.3549698552841819010 ) ) ;
#61784 = CARTESIAN_POINT ( 'NONE',  ( 23.64081946308400362, 10.11970730052999912, 9.384831229972000699 ) ) ;
#61785 = ORIENTED_EDGE ( 'NONE', *, *, #56493, .F. ) ;
#61786 = CARTESIAN_POINT ( 'NONE',  ( 8.347269353210000631, -2.741638482234999952, 6.457327039244000311 ) ) ;
#61787 = EDGE_CURVE ( 'NONE', #30625, #54024, #53367, .T. ) ;
#61788 = EDGE_CURVE ( 'NONE', #26090, #53272, #52493, .T. ) ;
#61789 = AXIS2_PLACEMENT_3D ( 'NONE', #54518, #34514, #24692 ) ;
#61790 = CARTESIAN_POINT ( 'NONE',  ( 18.23517937092938368, 2.264898893658550794, 13.81558401759068744 ) ) ;
#61791 = CARTESIAN_POINT ( 'NONE',  ( 5.000015393671500163, -2.571712834666313134E-16, -2.099962892531002545 ) ) ;
#61792 = CYLINDRICAL_SURFACE ( 'NONE', #43704, 0.5000000000000002220 ) ;
#61793 = ORIENTED_EDGE ( 'NONE', *, *, #36784, .F. ) ;
#61794 = CIRCLE ( 'NONE', #9283, 1.900000000000000577 ) ;
#61795 = CARTESIAN_POINT ( 'NONE',  ( 7.058509992104999853, 4.314040636970999820, 8.819134391732999845 ) ) ;
#61797 = CARTESIAN_POINT ( 'NONE',  ( 11.31389666366019853, 3.954123449088899900, 6.467512203247999913 ) ) ;
#61796 = CARTESIAN_POINT ( 'NONE',  ( 8.952784697134999803, -3.529509552262100058, -6.771750947090999340 ) ) ;
#61798 = CARTESIAN_POINT ( 'NONE',  ( 8.131285109058133287, -8.951598720774811113, -5.991666729276850845 ) ) ;
#61799 = ORIENTED_EDGE ( 'NONE', *, *, #45540, .F. ) ;
#61800 = CARTESIAN_POINT ( 'NONE',  ( 1.540556799207333238, 3.500000000000000888, -0.4581489286485045387 ) ) ;
#61801 = CARTESIAN_POINT ( 'NONE',  ( 10.40685100253999984, -2.832432432432000269, -6.822293592207000934 ) ) ;
#61802 = CARTESIAN_POINT ( 'NONE',  ( 11.60533460557258323, 4.184174550317700358, 6.374224726731999802 ) ) ;
#61803 = CARTESIAN_POINT ( 'NONE',  ( 10.98768538770000092, -2.700669876604000041, 4.945210823433001224 ) ) ;
#61804 = LINE ( 'NONE', #7986, #64489 ) ;
#61805 = ORIENTED_EDGE ( 'NONE', *, *, #27794, .F. ) ;
#61806 = CARTESIAN_POINT ( 'NONE',  ( 10.98768472639999949, -0.3876847264043000174, 4.945212061661000469 ) ) ;
#61807 = CARTESIAN_POINT ( 'NONE',  ( 10.14521814679000045, -3.576528389491000048, -8.962725485696999783 ) ) ;
#61808 = CARTESIAN_POINT ( 'NONE',  ( 8.064837199433295467, -3.781904628662576151, 5.773930963923838533 ) ) ;
#61809 = CIRCLE ( 'NONE', #24931, 12.39999890530000037 ) ;
#61810 = CARTESIAN_POINT ( 'NONE',  ( 11.56322412107030928, -3.945399343424460525, -6.467939235001000320 ) ) ;
#61811 = CARTESIAN_POINT ( 'NONE',  ( 9.702051052051999136, -2.879444846832000415, 7.280704316743199733 ) ) ;
#61812 = VERTEX_POINT ( 'NONE', #64707 ) ;
#61813 = CARTESIAN_POINT ( 'NONE',  ( 10.98974733714999985, -5.155859329793999635, -5.102561852530000053 ) ) ;
#61814 = CARTESIAN_POINT ( 'NONE',  ( 11.16579975933730040, -2.791514215189000225, 7.915786590091300035 ) ) ;
#61815 = VERTEX_POINT ( 'NONE', #43754 ) ;
#61816 = CARTESIAN_POINT ( 'NONE',  ( 9.041999884715581359, 3.843103124197280618, 6.308000049678228471 ) ) ;
#61817 = CONICAL_SURFACE ( 'NONE', #27231, 5.886037960926999268, 0.3217505543965463732 ) ;
#61818 = ORIENTED_EDGE ( 'NONE', *, *, #28353, .F. ) ;
#61819 = CARTESIAN_POINT ( 'NONE',  ( 9.710316810687000810, -2.624921803719999946, -8.200122328058998988 ) ) ;
#61820 = CARTESIAN_POINT ( 'NONE',  ( 9.898395280408998076, 3.987760651117999711, -9.123263301387000368 ) ) ;
#61821 = DIRECTION ( 'NONE',  ( 0.000000000000000000, -1.000000000000000000, 0.000000000000000000 ) ) ;
#61822 = CARTESIAN_POINT ( 'NONE',  ( 25.44993977744900349, 9.517611874540000017, 8.103398312166998352 ) ) ;
#61823 = CARTESIAN_POINT ( 'NONE',  ( 12.21195445704740656, 2.302603597045699946, -12.49539791649142906 ) ) ;
#61824 = CARTESIAN_POINT ( 'NONE',  ( 11.27256919669530077, -3.037654633983899899, 7.215672285280100517 ) ) ;
#61825 = CARTESIAN_POINT ( 'NONE',  ( 8.592635841230999105, 3.856772556595000179, 5.521246073317000125 ) ) ;
#61826 = VERTEX_POINT ( 'NONE', #16819 ) ;
#61827 = CARTESIAN_POINT ( 'NONE',  ( 9.698096873516668381, 4.327184855449106138, 8.717465845835393523 ) ) ;
#61828 = CARTESIAN_POINT ( 'NONE',  ( 8.598668146794999245, -2.376522687267000222, 7.686981355459999499 ) ) ;
#61829 = CARTESIAN_POINT ( 'NONE',  ( 24.17206818058083329, 9.108188618978893203, 9.092704695918069291 ) ) ;
#61830 = ORIENTED_EDGE ( 'NONE', *, *, #46926, .T. ) ;
#61831 = CARTESIAN_POINT ( 'NONE',  ( 12.08482599452297812, -2.564444806221819473, -12.33627826672298866 ) ) ;
#61832 = CARTESIAN_POINT ( 'NONE',  ( 10.44841638348500013, 2.891666689023999925, 7.769976643522699788 ) ) ;
#61833 = EDGE_CURVE ( 'NONE', #12035, #60646, #58667, .T. ) ;
#61834 = CARTESIAN_POINT ( 'NONE',  ( 11.15264435320999858, -2.317067032475999877, -7.596564138533999255 ) ) ;
#61835 = CARTESIAN_POINT ( 'NONE',  ( 6.544609839683332986, -1.500000000000000444, 0.1963495408493560745 ) ) ;
#61836 = CARTESIAN_POINT ( 'NONE',  ( 17.56813658992500393, -11.93194907420999940, 3.261335586771000106 ) ) ;
#61837 = CARTESIAN_POINT ( 'NONE',  ( 9.242292592096250203, 3.634505416671740097, -6.294013902202234334 ) ) ;
#61838 = CARTESIAN_POINT ( 'NONE',  ( 12.43878596651945401, -1.993461161472737775, -13.76788477248720355 ) ) ;
#61839 = ADVANCED_FACE ( 'NONE', ( #54931 ), #38498, .T. ) ;
#61840 = CARTESIAN_POINT ( 'NONE',  ( 11.78594988689359901, -3.606563555963900214, -8.271690446953899212 ) ) ;
#61841 = CARTESIAN_POINT ( 'NONE',  ( 10.44426222744799837, -4.986443098259000450, -8.312555471636301263 ) ) ;
#61842 = VECTOR ( 'NONE', #39690, 1000.000000000000000 ) ;
#61843 = CARTESIAN_POINT ( 'NONE',  ( 17.74426251268377186, -3.174930969421385196, 12.19343357469032085 ) ) ;
#61844 = ORIENTED_EDGE ( 'NONE', *, *, #21000, .F. ) ;
#61845 = ORIENTED_EDGE ( 'NONE', *, *, #9775, .F. ) ;
#61846 = CIRCLE ( 'NONE', #16070, 0.6999999999999992895 ) ;
#61847 = CARTESIAN_POINT ( 'NONE',  ( 5.200000002601999682, 0.2500000026021999555, 3.150000007068999963 ) ) ;
#61848 = CARTESIAN_POINT ( 'NONE',  ( 18.16782992319337708, 2.622990445277169513, 13.64655204326457927 ) ) ;
#61849 = CARTESIAN_POINT ( 'NONE',  ( 10.42081182385000027, 2.488452444780999695, -7.717895019962999648 ) ) ;
#61850 = DIRECTION ( 'NONE',  ( 0.000000000000000000, 1.000000000000000000, 0.000000000000000000 ) ) ;
#61851 = CARTESIAN_POINT ( 'NONE',  ( 18.06549347002469474, 2.139198186095363052, 12.52833527917195866 ) ) ;
#61852 = DIRECTION ( 'NONE',  ( 0.8660254037844289376, 0.000000000000000000, 0.5000000000000169864 ) ) ;
#61853 = CARTESIAN_POINT ( 'NONE',  ( 10.59344747867000081, 5.297752619853000944, 8.474195539311001113 ) ) ;
#61854 = CARTESIAN_POINT ( 'NONE',  ( 10.22963300084641780, -4.176697648610067759, -8.850191834421890391 ) ) ;
#61855 = ORIENTED_EDGE ( 'NONE', *, *, #59036, .F. ) ;
#61856 = CARTESIAN_POINT ( 'NONE',  ( 12.66183496498647365, -1.891282299343450601, 12.57277654391869248 ) ) ;
#61857 = CARTESIAN_POINT ( 'NONE',  ( 8.996455549952997899, -3.218304396998100003, -6.869290649434700136 ) ) ;
#61858 = CARTESIAN_POINT ( 'NONE',  ( 9.590596677641999079, 2.445964682955000136, 7.841184989245001624 ) ) ;
#61859 = CARTESIAN_POINT ( 'NONE',  ( 12.22433327354039889, -4.983220429128399687, 8.143111181492699302 ) ) ;
#61860 = VECTOR ( 'NONE', #19927, 1000.000000000000114 ) ;
#61861 = CARTESIAN_POINT ( 'NONE',  ( 10.47303166480599934, 2.862083839376000416, -7.580230465881790280 ) ) ;
#61862 = CARTESIAN_POINT ( 'NONE',  ( 12.18829625149018803, -0.1017072266180455709, 12.69945743039634856 ) ) ;
#61863 = VECTOR ( 'NONE', #66368, 1000.000000000000227 ) ;
#61864 = CARTESIAN_POINT ( 'NONE',  ( 7.673642219589999591, 4.696238830159999544, 5.830273622963999536 ) ) ;
#61865 = CARTESIAN_POINT ( 'NONE',  ( 10.03490996941999924, 5.615906393494999982, 7.351455918368999143 ) ) ;
#61866 = CARTESIAN_POINT ( 'NONE',  ( 12.69127452969527603, 1.885356761727419173, 12.57371515106196114 ) ) ;
#61867 = ORIENTED_EDGE ( 'NONE', *, *, #35794, .F. ) ;
#61868 = VECTOR ( 'NONE', #43838, 1000.000000000000227 ) ;
#61869 = CARTESIAN_POINT ( 'NONE',  ( 10.19741084123000086, 4.262870449202000422, -8.811513791423999820 ) ) ;
#61870 = B_SPLINE_CURVE_WITH_KNOTS ( 'NONE', 3,
 ( #63548, #59337, #21928, #15997 ),
 .UNSPECIFIED., .F., .F.,
 ( 4, 4 ),
 ( 0.000000000000000000, 1.000000000000000000 ),
 .UNSPECIFIED. ) ;
#61871 = CARTESIAN_POINT ( 'NONE',  ( -0.000000000000000000, 2.824612379753681513, 0.7585797238568994239 ) ) ;
#61872 = EDGE_CURVE ( 'NONE', #39743, #68200, #49682, .T. ) ;
#61873 = EDGE_CURVE ( 'NONE', #45267, #6955, #49150, .T. ) ;
#61874 = CARTESIAN_POINT ( 'NONE',  ( 5.391115032920665406, 0.7145727369020858921, 1.339076430445264032 ) ) ;
#61876 = CARTESIAN_POINT ( 'NONE',  ( 10.11476354018233081, 5.217465845835394411, 7.827184855449092815 ) ) ;
#61875 = CARTESIAN_POINT ( 'NONE',  ( 8.277730646792999636, -4.874569256861000177, 6.119503992241999590 ) ) ;
#61877 = CARTESIAN_POINT ( 'NONE',  ( 10.29184687351566652, 3.000416447002276943, -6.731816600031355513 ) ) ;
#61878 = B_SPLINE_CURVE_WITH_KNOTS ( 'NONE', 3,
 ( #5132, #47107, #32407, #10718 ),
 .UNSPECIFIED., .F., .F.,
 ( 4, 4 ),
 ( 0.000000000000000000, 1.000000000000000000 ),
 .UNSPECIFIED. ) ;
#61879 = CARTESIAN_POINT ( 'NONE',  ( 11.21564426047340035, -3.460037133261700149, -8.345807871442598724 ) ) ;
#61880 = EDGE_LOOP ( 'NONE', ( #11846, #68599, #22019, #49984 ) ) ;
#61881 = CARTESIAN_POINT ( 'NONE',  ( 1.200563222062999813, -2.255103325128000158, 3.007138987545999953 ) ) ;
#61882 = DIRECTION ( 'NONE',  ( 0.000000000000000000, 0.000000000000000000, 1.000000000000000000 ) ) ;
#61884 = CARTESIAN_POINT ( 'NONE',  ( 5.440293001548999641, -12.88483958404999896, -2.133988467673999967 ) ) ;
#61883 = CARTESIAN_POINT ( 'NONE',  ( 9.893930206848999376, -5.250000000000000000, 7.500000000000000000 ) ) ;
#61885 = CARTESIAN_POINT ( 'NONE',  ( 11.79999999116810727, -3.511856242852832377, 11.95218832016636945 ) ) ;
#61886 = CARTESIAN_POINT ( 'NONE',  ( 10.23809632363000155, 2.752447932331000047, 6.820051270595000048 ) ) ;
#61887 = CARTESIAN_POINT ( 'NONE',  ( 12.58176516051273630, -3.212719125873755299, 13.62638797003613966 ) ) ;
#61888 = CARTESIAN_POINT ( 'NONE',  ( 8.476023596135332738, 2.899999999999999911, -6.562910362702667477 ) ) ;
#61889 = DIRECTION ( 'NONE',  ( 1.000000000000000000, 0.000000000000000000, -0.000000000000000000 ) ) ;
#61890 = CARTESIAN_POINT ( 'NONE',  ( 8.528441940379998698, -2.472358291268000219, 6.234202627038999189 ) ) ;
#61891 = ORIENTED_EDGE ( 'NONE', *, *, #25587, .T. ) ;
#61892 = CARTESIAN_POINT ( 'NONE',  ( 7.930392219590000735, 3.164805384346000228, 9.104735843897000080 ) ) ;
#61893 = EDGE_CURVE ( 'NONE', #62696, #3420, #2477, .T. ) ;
#61894 = CARTESIAN_POINT ( 'NONE',  ( 13.43979992210467067, -11.65095899958523340, -2.173573044049637470 ) ) ;
#61895 = CARTESIAN_POINT ( 'NONE',  ( 7.450093581731485060, -2.260954841078268274, 7.477861549239195327 ) ) ;
#61896 = AXIS2_PLACEMENT_3D ( 'NONE', #5792, #32041, #53356 ) ;
#61897 = FACE_OUTER_BOUND ( 'NONE', #35181, .T. ) ;
#61898 = CARTESIAN_POINT ( 'NONE',  ( 1.981657498383000204, -3.284887521161000024, -0.9717780471415999877 ) ) ;
#61899 = ORIENTED_EDGE ( 'NONE', *, *, #14220, .F. ) ;
#61900 = CARTESIAN_POINT ( 'NONE',  ( 23.56665657357900301, 3.064215547964999882E-13, 1.261213355973999610E-13 ) ) ;
#61901 = CARTESIAN_POINT ( 'NONE',  ( 11.51872200990539952, -4.947480442174099657, 7.830502140005199507 ) ) ;
#61902 = LINE ( 'NONE', #8423, #48682 ) ;
#61903 = CARTESIAN_POINT ( 'NONE',  ( 9.555697025339000561, 2.440752375194999768, 6.680879724048000234 ) ) ;
#61904 = CARTESIAN_POINT ( 'NONE',  ( 11.24025954179439957, 4.771812902496799680, 6.858707791728399172 ) ) ;
#61905 = CARTESIAN_POINT ( 'NONE',  ( 7.110192589515543560, 5.350273814425614560, -7.415195716910538692 ) ) ;
#61906 = CYLINDRICAL_SURFACE ( 'NONE', #13720, 1.250000000000000222 ) ;
#61907 = FACE_OUTER_BOUND ( 'NONE', #34830, .T. ) ;
#61908 = CARTESIAN_POINT ( 'NONE',  ( 11.36660992314014784, 3.674321412135251652, -11.19575788941673267 ) ) ;
#61909 = CARTESIAN_POINT ( 'NONE',  ( 12.18517285595739175, -2.419552247691227453, 12.46997200859748389 ) ) ;
#61910 = B_SPLINE_CURVE_WITH_KNOTS ( 'NONE', 3,
 ( #16973, #17685, #59633, #54386, #28524, #49836, #5795, #56808, #35147, #39350, #8905, #39697, #7523, #28879 ),
 .UNSPECIFIED., .F., .F.,
 ( 4, 2, 2, 2, 2, 2, 4 ),
 ( 0.000000000000000000, 0.2499999999999995559, 0.3749999999999995559, 0.4999999999999995559, 0.6249999999999995559, 0.7499999999999995559, 1.000000000000000000 ),
 .UNSPECIFIED. ) ;
#61911 = CARTESIAN_POINT ( 'NONE',  ( 7.765771671202282178, 5.188776208877133200, 8.801183839191253355 ) ) ;
#61912 = ORIENTED_EDGE ( 'NONE', *, *, #25957, .T. ) ;
#61913 = CARTESIAN_POINT ( 'NONE',  ( 17.57587346436487152, -1.875000586273749992, 13.78631940097168673 ) ) ;
#61914 = CARTESIAN_POINT ( 'NONE',  ( 10.20271159698171815, -5.100000000000000533, 6.305985889763628727 ) ) ;
#61915 = ORIENTED_EDGE ( 'NONE', *, *, #68001, .T. ) ;
#61916 = ORIENTED_EDGE ( 'NONE', *, *, #68744, .F. ) ;
#61917 = CARTESIAN_POINT ( 'NONE',  ( 24.89163398232695812, -3.022263450368753990, -11.64683128245694554 ) ) ;
#61918 = DIRECTION ( 'NONE',  ( 0.000000000000000000, 0.9659258262890756397, -0.2588190451024932059 ) ) ;
#61920 = CARTESIAN_POINT ( 'NONE',  ( 10.97364560330029981, 4.265439025801100570, 8.324524538096799375 ) ) ;
#61919 = CONICAL_SURFACE ( 'NONE', #45211, 13.94232985059000107, 1.233427423217456464 ) ;
#61921 = CARTESIAN_POINT ( 'NONE',  ( 10.09696969267000100, 5.253376380222999131, 8.530663119653999260 ) ) ;
#61922 = DIRECTION ( 'NONE',  ( -1.000000000000000000, 0.000000000000000000, 0.000000000000000000 ) ) ;
#61923 = CARTESIAN_POINT ( 'NONE',  ( 8.998937807218627682, -4.055078665241000024, -6.626788336335921237 ) ) ;
#61924 = CARTESIAN_POINT ( 'NONE',  ( 10.29378083128999855, -3.483628580733000302, 6.176326635498999629 ) ) ;
#61925 = CARTESIAN_POINT ( 'NONE',  ( 18.24182894713847602, -0.2307628456012796592, -12.59789151516662997 ) ) ;
#61926 = EDGE_CURVE ( 'NONE', #53120, #32339, #18910, .T. ) ;
#61927 = DIRECTION ( 'NONE',  ( 0.000000000000000000, -1.000000000000000000, 0.000000000000000000 ) ) ;
#61928 = CARTESIAN_POINT ( 'NONE',  ( 10.29262282008599882, -3.548418513060800361, -8.228386593078399258 ) ) ;
#61929 = CARTESIAN_POINT ( 'NONE',  ( 12.80505043854146940, -1.875000000000000444, 12.57545641911172396 ) ) ;
#61930 = EDGE_LOOP ( 'NONE', ( #63593, #23447, #4794, #4791, #39802 ) ) ;
#61931 = AXIS2_PLACEMENT_3D ( 'NONE', #12728, #34058, #1892 ) ;
#61932 = CARTESIAN_POINT ( 'NONE',  ( 25.60000000000000142, -2.976419018679000050, -11.10814700232000085 ) ) ;
#61933 =( NAMED_UNIT ( * ) PLANE_ANGLE_UNIT ( ) SI_UNIT ( $, .RADIAN. ) );
#61934 = CARTESIAN_POINT ( 'NONE',  ( 24.69609520272172176, 8.660953915096069267, 8.619378635578760495 ) ) ;
#61935 = B_SPLINE_CURVE_WITH_KNOTS ( 'NONE', 3,
 ( #63662, #58423, #25926, #32218 ),
 .UNSPECIFIED., .F., .F.,
 ( 4, 4 ),
 ( 0.000000000000000000, 1.000000000000000000 ),
 .UNSPECIFIED. ) ;
#61936 = CARTESIAN_POINT ( 'NONE',  ( 10.73165287102650822, -3.320185038362776897, -8.679412628036383026 ) ) ;
#61937 = CARTESIAN_POINT ( 'NONE',  ( 9.836342523874998633, 2.735516931877000513, -7.306436165809000016 ) ) ;
#61938 = CARTESIAN_POINT ( 'NONE',  ( 12.15443728026460946, 2.840296387118482091, 13.70885984368922017 ) ) ;
#61939 = FACE_OUTER_BOUND ( 'NONE', #12297, .T. ) ;
#61940 = ORIENTED_EDGE ( 'NONE', *, *, #45724, .F. ) ;
#61941 = CARTESIAN_POINT ( 'NONE',  ( 12.29893172089695952, -0.3669524142237010622, -12.69287054297889483 ) ) ;
#61942 = CARTESIAN_POINT ( 'NONE',  ( 24.67921580255100267, 8.727633792449999817, 9.158312800479000870 ) ) ;
#61943 = ORIENTED_EDGE ( 'NONE', *, *, #54290, .F. ) ;
#61944 = CARTESIAN_POINT ( 'NONE',  ( 11.39393020684959978, -5.250000000000000000, 7.500000000000000000 ) ) ;
#61945 = CARTESIAN_POINT ( 'NONE',  ( 10.39393020684999946, 2.750000000000000000, 7.500000000000000000 ) ) ;
#61946 = CARTESIAN_POINT ( 'NONE',  ( 8.620740978634000129, -4.599999999999999645, 5.898823289756999877 ) ) ;
#61947 = DIRECTION ( 'NONE',  ( 0.000000000000000000, -0.7506664619968553831, 0.6606813625592322659 ) ) ;
#61948 = AXIS2_PLACEMENT_3D ( 'NONE', #44440, #65738, #60848 ) ;
#61949 = B_SPLINE_SURFACE_WITH_KNOTS ( 'NONE', 3, 3, ( 
 ( #63396, #48016, #32296, #15517 ),
 ( #11291, #54285, #58501, #21104 ),
 ( #37181, #47334, #32631, #10604 ),
 ( #68638, #59536, #20758, #43114 ),
 ( #58845, #10954, #42429, #42087 ),
 ( #811, #15850, #5702, #10264 ) ),
 .UNSPECIFIED., .F., .F., .F.,
 ( 4, 1, 1, 4 ),
 ( 4, 4 ),
 ( 0.8990819262081000129, 0.9285714285714000704, 1.000000000000000000, 1.007603470489000008 ),
 ( -0.1835655481301000091, 1.183565547943999929 ),
 .UNSPECIFIED. ) ;
#61950 = FACE_OUTER_BOUND ( 'NONE', #54945, .T. ) ;
#61951 = AXIS2_PLACEMENT_3D ( 'NONE', #20916, #37000, #58661 ) ;
#61952 = B_SPLINE_CURVE_WITH_KNOTS ( 'NONE', 3,
 ( #25132, #62193, #45438, #52035, #67089, #4138, #36310, #51362, #9729, #46465, #19892, #31080 ),
 .UNSPECIFIED., .F., .F.,
 ( 4, 2, 2, 2, 2, 4 ),
 ( 0.000000000000000000, 0.2500000000000149880, 0.3750000000000213163, 0.4375000000000214828, 0.5000000000000216493, 1.000000000000000000 ),
 .UNSPECIFIED. ) ;
#61953 = CARTESIAN_POINT ( 'NONE',  ( 25.46373329105799854, 11.23406619596999967, -3.161081784610999978 ) ) ;
#61954 = CARTESIAN_POINT ( 'NONE',  ( 8.122851870746000458, 2.921728982776850003, 8.328193042680714697 ) ) ;
#61955 = CARTESIAN_POINT ( 'NONE',  ( 5.000000000000000000, 0.2500000000000000000, 3.149999999999999911 ) ) ;
#61956 = CARTESIAN_POINT ( 'NONE',  ( 5.599999999999999645, -0.4000000000000000222, -6.406472342878999804 ) ) ;
#61957 = CARTESIAN_POINT ( 'NONE',  ( 11.63825819896753977, 3.148796120250299868, -7.660469764776300039 ) ) ;
#61958 = CARTESIAN_POINT ( 'NONE',  ( 8.335548758400999958, 2.897657723982001166, -6.653323589456997311 ) ) ;
#61959 = EDGE_CURVE ( 'NONE', #54862, #33733, #15153, .T. ) ;
#61960 = EDGE_CURVE ( 'NONE', #57124, #46963, #24149, .T. ) ;
#61961 = CARTESIAN_POINT ( 'NONE',  ( 11.02418915877000138, 2.407889430138999920, -8.439554272735000140 ) ) ;
#61962 = CARTESIAN_POINT ( 'NONE',  ( 10.18144474310099845, 5.015709705366000470, -7.992914665944799602 ) ) ;
#61964 = CARTESIAN_POINT ( 'NONE',  ( 9.262289945692000259, -4.238022715896200054, 6.588711079851200303 ) ) ;
#61963 = CARTESIAN_POINT ( 'NONE',  ( 15.65609597790000151, -8.788746246889001412, -7.589637905006999752 ) ) ;
#61965 = CARTESIAN_POINT ( 'NONE',  ( 23.56934271467462594, -13.33981148175788434, 4.212069331298350150 ) ) ;
#61966 = EDGE_LOOP ( 'NONE', ( #63541, #20409, #7491, #67859, #30562, #50113 ) ) ;
#61967 = ADVANCED_BREP_SHAPE_REPRESENTATION ( '', ( #52802, #9676 ), #67766 ) ;
#61968 = CARTESIAN_POINT ( 'NONE',  ( 10.32169598648999909, 4.766524664146899681, 7.043598424555200133 ) ) ;
#61969 = CONICAL_SURFACE ( 'NONE', #63089, 0.9999998338055000602, 0.7853981908209605178 ) ;
#61970 = CARTESIAN_POINT ( 'NONE',  ( 9.848732933287999813, -2.769734897491000325, 6.441850735262000249 ) ) ;
#61971 = CARTESIAN_POINT ( 'NONE',  ( 10.08560887879199797, 3.772542739612499751, 8.478317686146800369 ) ) ;
#61972 = CARTESIAN_POINT ( 'NONE',  ( 23.61814127931500096, -2.884265323764000133, 13.53884956573999965 ) ) ;
#61973 = CARTESIAN_POINT ( 'NONE',  ( 11.10000000009000054, -2.699999999911000259, 6.571291220400000022 ) ) ;
#61974 = CARTESIAN_POINT ( 'NONE',  ( 12.54566616138316526, 3.068981097031269201, 13.53612220331575600 ) ) ;
#61975 = CARTESIAN_POINT ( 'NONE',  ( 6.983066493190000834, -12.13287627744000119, 3.076835272540999977 ) ) ;
#61976 = ORIENTED_EDGE ( 'NONE', *, *, #49435, .T. ) ;
#61977 = EDGE_CURVE ( 'NONE', #46269, #67865, #50896, .T. ) ;
#61978 = CARTESIAN_POINT ( 'NONE',  ( 8.577265421554999492, -4.214287043487900064, -8.608472884860999486 ) ) ;
#61979 = DIRECTION ( 'NONE',  ( 0.000000000000000000, 0.000000000000000000, -1.000000000000000000 ) ) ;
#61980 = CARTESIAN_POINT ( 'NONE',  ( 10.93614141025500075, -3.450366949021700158, 6.521048559232099251 ) ) ;
#61981 = ADVANCED_FACE ( 'NONE', ( #12116 ), #23981, .F. ) ;
#61982 = CARTESIAN_POINT ( 'NONE',  ( 17.59659125555221948, 3.123958135111998491, -12.28406395290800468 ) ) ;
#61983 = CARTESIAN_POINT ( 'NONE',  ( 8.538555273383003907, -3.514476186897000254, -6.517616047691000780 ) ) ;
#61984 = DIRECTION ( 'NONE',  ( 0.000000000000000000, 0.000000000000000000, -1.000000000000000000 ) ) ;
#61985 = CARTESIAN_POINT ( 'NONE',  ( 12.18008982747168112, 2.511713771612850810, -13.67097129483465068 ) ) ;
#61986 = CARTESIAN_POINT ( 'NONE',  ( 9.040134009213000255, -5.099406281193999746, -6.669356233738001016 ) ) ;
#61987 = CARTESIAN_POINT ( 'NONE',  ( 25.27036577661199956, 11.11618949463999861, 3.474359096894000132 ) ) ;
#61988 = ORIENTED_EDGE ( 'NONE', *, *, #61399, .F. ) ;
#61989 = DIRECTION ( 'NONE',  ( -1.000000000000000000, 0.000000000000000000, 0.000000000000000000 ) ) ;
#61990 = DIRECTION ( 'NONE',  ( 0.000000000000000000, 0.000000000000000000, -1.000000000000000000 ) ) ;
#61991 = CYLINDRICAL_SURFACE ( 'NONE', #10881, 11.29999999999999893 ) ;
#61992 = DIRECTION ( 'NONE',  ( 0.000000000000000000, -1.000000000000000000, 0.000000000000000000 ) ) ;
#61993 = CARTESIAN_POINT ( 'NONE',  ( 18.16429560769915952, 2.358968865796700065, 12.48332026670510864 ) ) ;
#61994 = CARTESIAN_POINT ( 'NONE',  ( 8.523814158775000038, 4.920236664407999783, -6.448229650796999834 ) ) ;
#61995 = CARTESIAN_POINT ( 'NONE',  ( 6.584068549836916695, -1.425304930403541004, -0.5415159910133545695 ) ) ;
#61996 = ORIENTED_EDGE ( 'NONE', *, *, #54008, .F. ) ;
#61997 = CARTESIAN_POINT ( 'NONE',  ( 3.999971066382000284, -2.149963194831999935, 0.000000000000000000 ) ) ;
#61998 = CARTESIAN_POINT ( 'NONE',  ( 18.18368263331577594, 2.882378207881307386, -13.70008584495759152 ) ) ;
#61999 = ORIENTED_EDGE ( 'NONE', *, *, #65166, .F. ) ;
#62000 = CARTESIAN_POINT ( 'NONE',  ( 5.500000000000000000, 13.87069231928999891, 4.225386915259999654 ) ) ;
#62001 = DIRECTION ( 'NONE',  ( 1.000000000000000000, 0.000000000000000000, 0.000000000000000000 ) ) ;
#62002 = CARTESIAN_POINT ( 'NONE',  ( 8.962479719595000560, 2.546924812613000189, -6.918870225297999887 ) ) ;
#62003 = CARTESIAN_POINT ( 'NONE',  ( 9.414763540182331525, 2.782534154164605589, -7.827184855449099921 ) ) ;
#62004 = CARTESIAN_POINT ( 'NONE',  ( 11.41301932002725650, -5.250000000000000888, 7.200148911387370454 ) ) ;
#62005 = CARTESIAN_POINT ( 'NONE',  ( 10.60235971519489873, -3.394698737128500010, -6.493038401303000029 ) ) ;
#62006 = DIRECTION ( 'NONE',  ( 0.000000000000000000, 0.000000000000000000, -1.000000000000000000 ) ) ;
#62007 = CARTESIAN_POINT ( 'NONE',  ( 13.73712493497300180, 11.35980872612999804, 2.405726353896999736 ) ) ;
#62008 = ORIENTED_EDGE ( 'NONE', *, *, #48044, .F. ) ;
#62009 = CARTESIAN_POINT ( 'NONE',  ( 3.500000000000000000, 1.113524292603000010, -3.231029921506000324 ) ) ;
#62010 = CARTESIAN_POINT ( 'NONE',  ( 10.70851354018233437, -3.836375382625528019, 8.749999999999996447 ) ) ;
#62011 = CARTESIAN_POINT ( 'NONE',  ( 9.386379719595000282, 5.673443217382001080, -7.051790060464000476 ) ) ;
#62012 = ORIENTED_EDGE ( 'NONE', *, *, #57623, .F. ) ;
#62013 = CARTESIAN_POINT ( 'NONE',  ( 9.856715971886000460, 4.814120192353000149, -8.929574926876000518 ) ) ;
#62014 = ORIENTED_EDGE ( 'NONE', *, *, #56097, .T. ) ;
#62015 = CARTESIAN_POINT ( 'NONE',  ( 8.948759580228999866, 2.889471124893000287, 7.765443149353999708 ) ) ;
#62016 = CARTESIAN_POINT ( 'NONE',  ( 18.15128053492060900, -2.312280642761794791, -12.49331763295500863 ) ) ;
#62017 = AXIS2_PLACEMENT_3D ( 'NONE', #1976, #55456, #65588 ) ;
#62018 = CARTESIAN_POINT ( 'NONE',  ( 9.314928906318884927, 2.650140463285438397, -7.499996151983930659 ) ) ;
#62019 = CARTESIAN_POINT ( 'NONE',  ( 17.55505043854144276, 0.6250000000000001110, 13.88107975066923316 ) ) ;
#62020 = CARTESIAN_POINT ( 'NONE',  ( 8.611367346726332528, 2.905107952767239876, 6.370216469110514979 ) ) ;
#62021 = VERTEX_POINT ( 'NONE', #65929 ) ;
#62022 = CARTESIAN_POINT ( 'NONE',  ( 10.31905590579000176, 2.899999999999999911, -6.571291218949999902 ) ) ;
#62023 = CARTESIAN_POINT ( 'NONE',  ( 10.42512334122999995, 3.371064118627999928, -6.294343971198999910 ) ) ;
#62024 = DIRECTION ( 'NONE',  ( 0.000000000000000000, 1.000000000000000000, 0.000000000000000000 ) ) ;
#62025 = CARTESIAN_POINT ( 'NONE',  ( 12.09788000779844630, 2.355563551342471751, -13.80043034480240216 ) ) ;
#62026 = CARTESIAN_POINT ( 'NONE',  ( 10.48444474310099928, -2.984290294633999974, -7.992914665944799602 ) ) ;
#62027 = CARTESIAN_POINT ( 'NONE',  ( 17.71954595323150627, 0.7115697451011995245, 13.98190580764195978 ) ) ;
#62028 = CARTESIAN_POINT ( 'NONE',  ( 17.89162860438300129, 3.376692001085000339, 11.11057855219999979 ) ) ;
#62029 = CARTESIAN_POINT ( 'NONE',  ( 10.84088306584999906, -2.636277440143000472, -7.512643837511999934 ) ) ;
#62030 = ORIENTED_EDGE ( 'NONE', *, *, #46345, .T. ) ;
#62031 = ORIENTED_EDGE ( 'NONE', *, *, #28320, .F. ) ;
#62032 = CARTESIAN_POINT ( 'NONE',  ( 8.830545280412000153, 3.207599814920999659, -6.150466394809999571 ) ) ;
#62033 = DIRECTION ( 'NONE',  ( 0.000000000000000000, -0.8734457522908377625, -0.4869214698543208875 ) ) ;
#62034 = CARTESIAN_POINT ( 'NONE',  ( 10.43353630809279942, 2.899999999999999911, -6.665341197380437066 ) ) ;
#62035 = CARTESIAN_POINT ( 'NONE',  ( 25.31008644117000372, 8.472729765048999440, -8.045102513582000014 ) ) ;
#62036 = ADVANCED_FACE ( 'NONE', ( #54759 ), #18057, .T. ) ;
#62037 = EDGE_CURVE ( 'NONE', #38406, #44536, #19604, .T. ) ;
#62038 = CARTESIAN_POINT ( 'NONE',  ( 23.58435503226500174, 10.35630177538000041, -9.330313185629002248 ) ) ;
#62039 = CARTESIAN_POINT ( 'NONE',  ( 18.23176382712000176, -2.916721637292999603, -11.52766586543999949 ) ) ;
#62041 = DIRECTION ( 'NONE',  ( 0.000000000000000000, -1.000000000000000000, 0.000000000000000000 ) ) ;
#62040 = CARTESIAN_POINT ( 'NONE',  ( 9.903734463322999559, -3.881063085044400118, 6.364399516445999438 ) ) ;
#62042 = CARTESIAN_POINT ( 'NONE',  ( 10.90000000000000036, 5.100000000000000533, -6.436740704805999691 ) ) ;
#62043 = ORIENTED_EDGE ( 'NONE', *, *, #15529, .F. ) ;
#62044 = CYLINDRICAL_SURFACE ( 'NONE', #26934, 0.4999999999999998335 ) ;
#62045 = VECTOR ( 'NONE', #128, 1000.000000000000114 ) ;
#62046 = CARTESIAN_POINT ( 'NONE',  ( 23.89320776801300283, -10.87822567738999346, -3.284864823361000941 ) ) ;
#62047 = CARTESIAN_POINT ( 'NONE',  ( 9.578311703535998589, -4.818302824158000597, -8.808202952968999355 ) ) ;
#62048 = CARTESIAN_POINT ( 'NONE',  ( 7.924408822415808018, 4.759987200975432486, 6.322386952704928120 ) ) ;
#62049 = CARTESIAN_POINT ( 'NONE',  ( 11.30000000000000071, 0.000000000000000000, 0.000000000000000000 ) ) ;
#62050 = CARTESIAN_POINT ( 'NONE',  ( 23.56665676678100141, 1.192379528446999839E-13, -4.982680934517999418E-13 ) ) ;
#62051 = CARTESIAN_POINT ( 'NONE',  ( 9.690635841230999858, 2.927176851028000293, -5.932007155957999878 ) ) ;
#62052 = B_SPLINE_CURVE_WITH_KNOTS ( 'NONE', 3,
 ( #39633, #23545, #30184, #18990 ),
 .UNSPECIFIED., .F., .F.,
 ( 4, 4 ),
 ( 0.000000000000000000, 1.000000000000000000 ),
 .UNSPECIFIED. ) ;
#62053 = CARTESIAN_POINT ( 'NONE',  ( 7.990070311382211798, 3.072494164717982201, -6.390217723318725618 ) ) ;
#62054 = CARTESIAN_POINT ( 'NONE',  ( 11.00000000000000000, 2.941427501403999667, 7.174999999999999822 ) ) ;
#62055 = EDGE_CURVE ( 'NONE', #41440, #12705, #12918, .T. ) ;
#62056 = CARTESIAN_POINT ( 'NONE',  ( 4.000000000000000000, 0.000000000000000000, 0.000000000000000000 ) ) ;
#62057 = CARTESIAN_POINT ( 'NONE',  ( 3.623628218870999618, 1.587559571644000078, -2.882103889560999832 ) ) ;
#62058 = ORIENTED_EDGE ( 'NONE', *, *, #62349, .F. ) ;
#62059 = B_SPLINE_CURVE_WITH_KNOTS ( 'NONE', 3,
 ( #29620, #50236, #44662, #60722, #24352, #7582, #8274, #13532, #2340, #28931, #46020, #61750, #23658, #33820, #45684, #66990 ),
 .UNSPECIFIED., .F., .F.,
 ( 4, 2, 2, 2, 2, 2, 2, 4 ),
 ( 0.000000000000000000, 0.1249999999999996669, 0.2499999999999993339, 0.3749999999999990008, 0.4999999999999986677, 0.6249999999999991118, 0.7499999999999995559, 1.000000000000000000 ),
 .UNSPECIFIED. ) ;
#62060 = CARTESIAN_POINT ( 'NONE',  ( 12.37769715316224506, -0.4561785182478235723, -12.68897339690747295 ) ) ;
#62061 = CARTESIAN_POINT ( 'NONE',  ( 12.19116924868947471, -2.617374923999068681, -12.42344294665103988 ) ) ;
#62062 = DIRECTION ( 'NONE',  ( 0.000000000000000000, -0.8075584957945176612, 0.5897874836499127360 ) ) ;
#62063 = CARTESIAN_POINT ( 'NONE',  ( 8.641801658773999861, 2.933833973450999721, 8.496479443567000800 ) ) ;
#62064 = DIRECTION ( 'NONE',  ( 0.7071193432624600650, 0.7070942188874600465, 1.398349818569919760E-09 ) ) ;
#62065 = ORIENTED_EDGE ( 'NONE', *, *, #41609, .T. ) ;
#62066 = CARTESIAN_POINT ( 'NONE',  ( 6.025819726242999330, -0.03703453004475999732, -1.321780775251000017 ) ) ;
#62067 = CARTESIAN_POINT ( 'NONE',  ( 10.98768472638000127, 7.408460511344000743, 6.159405790617999976 ) ) ;
#62068 = CARTESIAN_POINT ( 'NONE',  ( 10.92594639162300041, 5.087027437888981929, 4.995424258306049303 ) ) ;
#62069 = CARTESIAN_POINT ( 'NONE',  ( 7.844613792771893301, 2.729327499216226194, -7.000868400899764588 ) ) ;
#62070 = CARTESIAN_POINT ( 'NONE',  ( 10.51414141025500015, 4.615773412711500434, -8.596754040696000132 ) ) ;
#62071 = ORIENTED_EDGE ( 'NONE', *, *, #21851, .T. ) ;
#62072 = CARTESIAN_POINT ( 'NONE',  ( 10.53733998880999856, -2.992814141720000265, 8.731692578598000409 ) ) ;
#62073 = EDGE_LOOP ( 'NONE', ( #40298, #9568, #66869, #1860, #16989, #47377 ) ) ;
#62074 = CARTESIAN_POINT ( 'NONE',  ( 9.205773468340201049, 5.100000000000000533, -6.304440313902172299 ) ) ;
#62075 = CARTESIAN_POINT ( 'NONE',  ( 7.854816940377000734, -4.561648098548999997, 6.153050355516999304 ) ) ;
#62076 = CARTESIAN_POINT ( 'NONE',  ( 18.00570828977290461, -0.5721320424853957309, -13.98830666644471599 ) ) ;
#62077 = ORIENTED_EDGE ( 'NONE', *, *, #11448, .T. ) ;
#62078 = CARTESIAN_POINT ( 'NONE',  ( 8.624544496487235534, 2.406435347409131786, -6.761471569661993364 ) ) ;
#62079 = DIRECTION ( 'NONE',  ( -1.000000000000000000, 0.000000000000000000, 0.000000000000000000 ) ) ;
#62080 = CARTESIAN_POINT ( 'NONE',  ( 8.178354719590000599, 5.563172860439999923, -7.424303164651000486 ) ) ;
#62081 = DIRECTION ( 'NONE',  ( 1.000000000000000000, 0.000000000000000000, 0.000000000000000000 ) ) ;
#62082 = CARTESIAN_POINT ( 'NONE',  ( 24.60115017391931502, 3.453285473742774947, 12.10347684623337550 ) ) ;
#62083 = VERTEX_POINT ( 'NONE', #1623 ) ;
#62084 = CARTESIAN_POINT ( 'NONE',  ( 2.198890132540458175, -2.798833948393640192, 2.150913519912191152 ) ) ;
#62085 = DIRECTION ( 'NONE',  ( 0.000000000000000000, 1.000000000000000000, 0.000000000000000000 ) ) ;
#62086 = CARTESIAN_POINT ( 'NONE',  ( 12.37550370467830696, 11.46556593385748357, -4.499409319921212180 ) ) ;
#62087 = CARTESIAN_POINT ( 'NONE',  ( 10.53865751177000121, -3.647233463439000012, -6.014125921456000334 ) ) ;
#62088 = CARTESIAN_POINT ( 'NONE',  ( 4.000000000000000000, 0.000000000000000000, 0.000000000000000000 ) ) ;
#62089 = VERTEX_POINT ( 'NONE', #39375 ) ;
#62090 = CARTESIAN_POINT ( 'NONE',  ( 17.95719809541170520, 0.4784561393452470557, -13.88891570267007403 ) ) ;
#62091 = AXIS2_PLACEMENT_3D ( 'NONE', #42481, #12040, #6095 ) ;
#62092 = DIRECTION ( 'NONE',  ( 1.000000000000000000, 0.000000000000000000, 0.000000000000000000 ) ) ;
#62093 = EDGE_CURVE ( 'NONE', #32306, #25573, #65349, .T. ) ;
#62094 = CARTESIAN_POINT ( 'NONE',  ( 23.60000657692131654, -2.996625413523755110, -13.56987347963171686 ) ) ;
#62095 = CARTESIAN_POINT ( 'NONE',  ( 3.146806799210916772, -0.9161175952574931447, 3.408904368339100710 ) ) ;
#62096 = ADVANCED_FACE ( 'NONE', ( #12811 ), #2313, .F. ) ;
#62097 = CARTESIAN_POINT ( 'NONE',  ( 12.42411034028606309, -0.4959091552601235242, -13.88809952003718173 ) ) ;
#62098 = CARTESIAN_POINT ( 'NONE',  ( 18.15862102414880042, -2.662578152609975213, 12.41223253473083155 ) ) ;
#62099 = EDGE_LOOP ( 'NONE', ( #56945, #21962, #52753, #27660 ) ) ;
#62100 = CARTESIAN_POINT ( 'NONE',  ( 10.52435971519499880, -3.467537960339900138, -6.614211617270199461 ) ) ;
#62101 = ORIENTED_EDGE ( 'NONE', *, *, #25572, .F. ) ;
#62102 = CARTESIAN_POINT ( 'NONE',  ( 10.87148757351999961, 5.567567343464999929, 7.772413227960999649 ) ) ;
#62103 = DIRECTION ( 'NONE',  ( 0.000000000000000000, -0.9659258262890757507, -0.2588190451024934835 ) ) ;
#62104 = AXIS2_PLACEMENT_3D ( 'NONE', #35749, #2894, #24220 ) ;
#62105 = CARTESIAN_POINT ( 'NONE',  ( 8.458179719589999479, 5.332332124071999857, -8.487089944253000340 ) ) ;
#62106 = B_SPLINE_CURVE_WITH_KNOTS ( 'NONE', 3,
 ( #9699, #67392, #19514, #52354, #63527, #25786 ),
 .UNSPECIFIED., .F., .F.,
 ( 4, 2, 4 ),
 ( 0.000000000000000000, 0.5000000000000000000, 1.000000000000000000 ),
 .UNSPECIFIED. ) ;
#62107 = CARTESIAN_POINT ( 'NONE',  ( 3.480762151334999555, 3.165347270645999966, -1.931374428620000083 ) ) ;
#62108 = CARTESIAN_POINT ( 'NONE',  ( 11.03407957707000087, -2.992853177526999975, -9.056567163506000995 ) ) ;
#62109 = LINE ( 'NONE', #68035, #404 ) ;
#62110 = CARTESIAN_POINT ( 'NONE',  ( 18.18005043824376443, -1.329523415562850021E-10, -12.70000000088146486 ) ) ;
#62111 = VERTEX_POINT ( 'NONE', #61043 ) ;
#62112 = CARTESIAN_POINT ( 'NONE',  ( 12.20379573085659963, -2.893744357957000357, 7.308581953418300081 ) ) ;
#62113 = DIRECTION ( 'NONE',  ( 0.000000000000000000, -0.3118250626419980520, 0.9501395320205942019 ) ) ;
#62114 = CARTESIAN_POINT ( 'NONE',  ( 15.91587707751000025, 9.040653309694000939, 8.458480061295000851 ) ) ;
#62115 = EDGE_CURVE ( 'NONE', #24689, #10513, #12508, .T. ) ;
#62116 = DIRECTION ( 'NONE',  ( -0.5000000000000169864, 0.000000000000000000, -0.8660254037844288266 ) ) ;
#62118 = CARTESIAN_POINT ( 'NONE',  ( 23.89320776801300283, -2.594336453666000075, -11.06325219639999347 ) ) ;
#62117 = CARTESIAN_POINT ( 'NONE',  ( 9.939321360490000146, 2.638097915594000309, 6.328629954376999933 ) ) ;
#62119 = CARTESIAN_POINT ( 'NONE',  ( 10.50180110216399854, 3.143606124884799957, -6.976989117212499814 ) ) ;
#62120 = EDGE_CURVE ( 'NONE', #5301, #41119, #49737, .T. ) ;
#62121 = CARTESIAN_POINT ( 'NONE',  ( 24.56892856850300078, -12.04602458699000067, 3.139954038541999726 ) ) ;
#62122 = CARTESIAN_POINT ( 'NONE',  ( 9.123101285863999266, 3.353260484332500013, -6.731514281717299930 ) ) ;
#62123 = CARTESIAN_POINT ( 'NONE',  ( 18.26152580467099540, 0.1632583333441799678, 12.59896334813831764 ) ) ;
#62124 = CARTESIAN_POINT ( 'NONE',  ( 24.36958145701300182, 3.196690648311999894, 12.07804156775000060 ) ) ;
#62125 = CARTESIAN_POINT ( 'NONE',  ( 10.63880513895979973, 5.150451045932999961, 8.139542779846600240 ) ) ;
#62126 = PLANE ( 'NONE',  #46636 ) ;
#62127 = VERTEX_POINT ( 'NONE', #48018 ) ;
#62128 = CARTESIAN_POINT ( 'NONE',  ( 9.079730646793999327, -5.421531391267000011, 6.381128921159999301 ) ) ;
#62129 = CARTESIAN_POINT ( 'NONE',  ( 17.81237950545464699, 3.200707792931475559, 13.62921448194399154 ) ) ;
#62130 = FACE_OUTER_BOUND ( 'NONE', #43708, .T. ) ;
#62131 = CARTESIAN_POINT ( 'NONE',  ( 24.30001682246400208, -8.938702682732001747, -8.938676171235998780 ) ) ;
#62132 = ORIENTED_EDGE ( 'NONE', *, *, #8835, .T. ) ;
#62133 = CARTESIAN_POINT ( 'NONE',  ( 7.871551658771999804, 4.780986922229000236, 6.267222470044999660 ) ) ;
#62134 = ADVANCED_FACE ( 'NONE', ( #58848, #6390 ), #42771, .T. ) ;
#62135 = MECHANICAL_DESIGN_GEOMETRIC_PRESENTATION_REPRESENTATION (  '', ( #14143 ), #58794 ) ;
#62137 = CARTESIAN_POINT ( 'NONE',  ( 11.39189666366029918, 3.947847673382490541, 6.326270943800999191 ) ) ;
#62136 = CARTESIAN_POINT ( 'NONE',  ( 9.662000818238999145, -4.767147064380999666, -7.903971937289999694 ) ) ;
#62138 = CARTESIAN_POINT ( 'NONE',  ( 10.44812028041000040, 5.235600787608000850, -6.609970743661000903 ) ) ;
#62139 = ORIENTED_EDGE ( 'NONE', *, *, #18479, .T. ) ;
#62140 = DIRECTION ( 'NONE',  ( 2.186053604475938581E-10, -0.8077514394224775129, 0.5895232074404836986 ) ) ;
#62142 = CARTESIAN_POINT ( 'NONE',  ( 17.74396022931449934, -3.223333129201646052, -13.62388254889262029 ) ) ;
#62141 = B_SPLINE_CURVE_WITH_KNOTS ( 'NONE', 3,
 ( #16805, #43740, #44092, #33250 ),
 .UNSPECIFIED., .F., .F.,
 ( 4, 4 ),
 ( 0.000000000000000000, 1.000000000000000000 ),
 .UNSPECIFIED. ) ;
#62143 = CARTESIAN_POINT ( 'NONE',  ( 10.88733729122639993, 2.722429312291999803, 7.533608309972310124 ) ) ;
#62144 = CARTESIAN_POINT ( 'NONE',  ( 17.60000000357355532, -10.99221148292035544, 4.481504242813237227 ) ) ;
#62146 = CARTESIAN_POINT ( 'NONE',  ( 8.455992358812000731, 3.399999999999999911, 6.571291218949999902 ) ) ;
#62145 = VECTOR ( 'NONE', #66876, 1000.000000000000000 ) ;
#62147 = VERTEX_POINT ( 'NONE', #11634 ) ;
#62148 = CARTESIAN_POINT ( 'NONE',  ( 5.100000001045000175, 0.000000000000000000, 0.000000000000000000 ) ) ;
#62149 = CARTESIAN_POINT ( 'NONE',  ( 8.014414158768000007, 2.494419548310999879, -8.658783402411998509 ) ) ;
#62150 = CARTESIAN_POINT ( 'NONE',  ( 8.254401249163198173, -5.347345989532893640, 8.600472902534793462 ) ) ;
#62151 = CARTESIAN_POINT ( 'NONE',  ( 10.55569598648999907, -2.869047858956000230, -8.173387776112500447 ) ) ;
#62152 = CARTESIAN_POINT ( 'NONE',  ( 9.776025935146000378, -4.185743043590700374, 8.765655525501999890 ) ) ;
#62153 = ORIENTED_EDGE ( 'NONE', *, *, #55322, .T. ) ;
#62154 = CARTESIAN_POINT ( 'NONE',  ( 10.88897495225000078, -5.158582900058999776, -5.064471961637000419 ) ) ;
#62155 = CARTESIAN_POINT ( 'NONE',  ( 10.84580110216399973, -5.090698144635000588, 8.166103548914600552 ) ) ;
#62156 = EDGE_LOOP ( 'NONE', ( #26403, #49761, #7073, #56899, #68008, #15295, #7473, #19898, #57196, #48507, #34959, #33135 ) ) ;
#62157 = CARTESIAN_POINT ( 'NONE',  ( 11.30000000000000071, 3.090860900556000105E-13, -1.000866056699999936E-13 ) ) ;
#62158 = ORIENTED_EDGE ( 'NONE', *, *, #49991, .F. ) ;
#62159 = CARTESIAN_POINT ( 'NONE',  ( 9.265134009212999899, -5.494586520014999920, -6.370782351137999733 ) ) ;
#62160 = CARTESIAN_POINT ( 'NONE',  ( 2.436390132543208686, 0.4581489286485155299, -3.499999999999999556 ) ) ;
#62161 = DIRECTION ( 'NONE',  ( 1.000000000000000000, 0.000000000000000000, 0.000000000000000000 ) ) ;
#62162 = CARTESIAN_POINT ( 'NONE',  ( 10.20000099824999928, 12.50000000000000000, 0.000000000000000000 ) ) ;
#62163 = CARTESIAN_POINT ( 'NONE',  ( 12.44669855353769350, 1.987833209345827967, -12.55628527126821226 ) ) ;
#62164 = CARTESIAN_POINT ( 'NONE',  ( 11.07149279008999976, -4.296686446741600385, 6.398515879103999993 ) ) ;
#62165 = CARTESIAN_POINT ( 'NONE',  ( 8.656823341231000057, 5.329437560656000272, 6.027391099688998999 ) ) ;
#62166 = EDGE_LOOP ( 'NONE', ( #49232, #15908, #40704 ) ) ;
#62167 = CARTESIAN_POINT ( 'NONE',  ( 7.474999999999999645, 5.349999999999999645, 7.500000000000000000 ) ) ;
#62168 = CARTESIAN_POINT ( 'NONE',  ( 8.251331853209000755, -5.773185758034999893, 7.141496747382000798 ) ) ;
#62169 = CARTESIAN_POINT ( 'NONE',  ( 11.79999998956225937, 3.428554832065389135, -11.90642801602077228 ) ) ;
#62170 = ORIENTED_EDGE ( 'NONE', *, *, #61644, .F. ) ;
#62171 = CARTESIAN_POINT ( 'NONE',  ( 12.55429323164601207, -3.072583267488711023, -12.29953727834259958 ) ) ;
#62172 = CARTESIAN_POINT ( 'NONE',  ( 11.05964426047339799, 4.687693494822500639, 6.422784126663999338 ) ) ;
#62173 = CARTESIAN_POINT ( 'NONE',  ( 10.84974435320999930, -5.265000209383999596, -6.385811305909999902 ) ) ;
#62174 = CARTESIAN_POINT ( 'NONE',  ( 10.69809687351599869, 4.327184855449106138, 8.717465845835393523 ) ) ;
#62175 = CARTESIAN_POINT ( 'NONE',  ( 2.457156007037999856, 3.012404793772358591, -1.845954168039164678 ) ) ;
#62176 = EDGE_CURVE ( 'NONE', #38467, #41893, #17397, .T. ) ;
#62177 = CARTESIAN_POINT ( 'NONE',  ( 24.62773497369100184, -8.736972494141998169, 9.042113496788999782 ) ) ;
#62178 = CARTESIAN_POINT ( 'NONE',  ( 12.30715842069481702, -2.122066859011513262, -13.74633992746440292 ) ) ;
#62179 = EDGE_CURVE ( 'NONE', #66731, #42529, #36653, .T. ) ;
#62180 = DIRECTION ( 'NONE',  ( 0.000000000000000000, 1.000000000000000000, 0.000000000000000000 ) ) ;
#62181 = CARTESIAN_POINT ( 'NONE',  ( 10.61656919669529842, -2.774362666861999838, -7.862118085997298778 ) ) ;
#62182 = EDGE_CURVE ( 'NONE', #52150, #56420, #31947, .T. ) ;
#62183 = DIRECTION ( 'NONE',  ( 0.000000000000000000, 1.000000000000000000, 0.000000000000000000 ) ) ;
#62184 = ORIENTED_EDGE ( 'NONE', *, *, #56493, .T. ) ;
#62185 = B_SPLINE_CURVE_WITH_KNOTS ( 'NONE', 3,
 ( #21729, #16149, #32924, #37136, #64368, #68943, #63692, #43063, #16491, #27334, #65058, #17179, #5994, #42386, #15807, #48658 ),
 .UNSPECIFIED., .F., .F.,
 ( 4, 2, 2, 2, 2, 2, 2, 4 ),
 ( 0.000000000000000000, 0.06249999999999930611, 0.1249999999999986122, 0.2499999999999994449, 0.4999999999999997780, 0.7500000000000001110, 0.8750000000000000000, 1.000000000000000000 ),
 .UNSPECIFIED. ) ;
#62186 = ORIENTED_EDGE ( 'NONE', *, *, #564, .T. ) ;
#62187 = DIRECTION ( 'NONE',  ( -1.000000000000000000, 0.000000000000000000, 0.000000000000000000 ) ) ;
#62188 = VECTOR ( 'NONE', #64143, 1000.000000000000000 ) ;
#62189 = FACE_OUTER_BOUND ( 'NONE', #33978, .T. ) ;
#62190 = CARTESIAN_POINT ( 'NONE',  ( 18.07078568656085338, 2.853178104762410072, 13.59212922196301143 ) ) ;
#62191 = CARTESIAN_POINT ( 'NONE',  ( 10.38153063908000107, 2.772139908660999907, -8.408082511401000048 ) ) ;
#62192 = B_SPLINE_CURVE_WITH_KNOTS ( 'NONE', 3,
 ( #5077, #57526, #14208, #20132, #62767 ),
 .UNSPECIFIED., .F., .F.,
 ( 4, 1, 4 ),
 ( 0.000000000000000000, 0.5000000000000000000, 1.000000000000000000 ),
 .UNSPECIFIED. ) ;
#62193 = CARTESIAN_POINT ( 'NONE',  ( 8.731512351913153225, 5.100000000000000533, 6.372362022305052776 ) ) ;
#62194 = CARTESIAN_POINT ( 'NONE',  ( 8.871383953235001840, -4.600000082569999371, -6.206578679665999410 ) ) ;
#62195 = DIRECTION ( 'NONE',  ( 0.000000000000000000, 1.000000000000000000, 0.000000000000000000 ) ) ;
#62196 = CARTESIAN_POINT ( 'NONE',  ( 10.99433665574000152, 3.697618584609999814, 5.729302299903000772 ) ) ;
#62197 = CARTESIAN_POINT ( 'NONE',  ( 10.36503728015203230, -2.650011783303574564, -7.500002219258004921 ) ) ;
#62198 = ORIENTED_EDGE ( 'NONE', *, *, #29144, .T. ) ;
#62199 = CARTESIAN_POINT ( 'NONE',  ( 12.52605318029424275, -1.940633248599432203, 12.56447441435821943 ) ) ;
#62200 = CARTESIAN_POINT ( 'NONE',  ( 9.197076168957998732, -4.439974903344300117, -8.247081005603298820 ) ) ;
#62201 = CARTESIAN_POINT ( 'NONE',  ( 10.96207813434000045, 5.399835028078000754, 7.743264559064000352 ) ) ;
#62202 = CARTESIAN_POINT ( 'NONE',  ( 11.26346886766499900, -4.634677072395899877, 8.653146038559000885 ) ) ;
#62203 = CARTESIAN_POINT ( 'NONE',  ( 10.11453584122999949, 5.322769172805999816, -7.951018786192998178 ) ) ;
#62204 = AXIS2_PLACEMENT_3D ( 'NONE', #38404, #38056, #64618 ) ;
#62205 = CARTESIAN_POINT ( 'NONE',  ( 10.12426357027499790, 5.254871132332000094, -7.742104041724699570 ) ) ;
#62206 = CARTESIAN_POINT ( 'NONE',  ( 12.18127380957210271, -0.04040257046694565451, 12.69991905489010442 ) ) ;
#62207 = CARTESIAN_POINT ( 'NONE',  ( 7.609454719589999527, 3.276311362504999991, 5.841989464160999290 ) ) ;
#62208 = B_SPLINE_CURVE_WITH_KNOTS ( 'NONE', 3,
 ( #58594, #22564, #53011, #37611 ),
 .UNSPECIFIED., .F., .F.,
 ( 4, 4 ),
 ( 0.000000000000000000, 1.000000000000000000 ),
 .UNSPECIFIED. ) ;
#62209 = CARTESIAN_POINT ( 'NONE',  ( 9.724611353170001138, 2.928305163963000446, 8.718478150869000132 ) ) ;
#62210 = VECTOR ( 'NONE', #41357, 1000.000000000000000 ) ;
#62211 = CARTESIAN_POINT ( 'NONE',  ( 12.24247500090512553, 2.227530134987963706, 12.51087939115179104 ) ) ;
#62212 = VERTEX_POINT ( 'NONE', #1159 ) ;
#62213 = CARTESIAN_POINT ( 'NONE',  ( 9.237204719595000668, 3.071719032003000116, -6.037263251225000182 ) ) ;
#62214 = CYLINDRICAL_SURFACE ( 'NONE', #4506, 1.350000000000000533 ) ;
#62215 = CARTESIAN_POINT ( 'NONE',  ( 9.153455117183014522, 2.649843614532819469, 7.852866721134448724 ) ) ;
#62217 = DIRECTION ( 'NONE',  ( 1.000000000000000000, 0.000000000000000000, 0.000000000000000000 ) ) ;
#62216 = CARTESIAN_POINT ( 'NONE',  ( 8.058769353207999586, -2.432121990576000314, 6.597519606637999523 ) ) ;
#62218 = CARTESIAN_POINT ( 'NONE',  ( 10.19809687351566474, 4.327184855449106138, -6.282534154164607365 ) ) ;
#62219 = CARTESIAN_POINT ( 'NONE',  ( 11.77359063708300013, -3.044227915785300276, -7.768721787835699999 ) ) ;
#62220 = ORIENTED_EDGE ( 'NONE', *, *, #21380, .T. ) ;
#62221 = CARTESIAN_POINT ( 'NONE',  ( 1.968247751176999794, 3.260257002997999809, 1.508168810892000167 ) ) ;
#62222 = CARTESIAN_POINT ( 'NONE',  ( 18.06139130775558854, -0.3666439886896704636, -12.69288249682903569 ) ) ;
#62223 = EDGE_CURVE ( 'NONE', #22085, #61617, #5804, .T. ) ;
#62225 = CARTESIAN_POINT ( 'NONE',  ( 13.67476513888300005, -9.526862765824999357, -8.046751417967000108 ) ) ;
#62224 = CARTESIAN_POINT ( 'NONE',  ( 9.468589158772999781, 4.034680274230000308, -6.102912434217000026 ) ) ;
#62226 = DIRECTION ( 'NONE',  ( 1.000000000000000000, 1.776356839362000177E-14, 5.329070518085999900E-14 ) ) ;
#62227 = CARTESIAN_POINT ( 'NONE',  ( 17.60000001994400165, -11.53041320601000130, 4.891397783926000109 ) ) ;
#62228 = ADVANCED_FACE ( 'NONE', ( #38558 ), #27383, .F. ) ;
#62229 = CARTESIAN_POINT ( 'NONE',  ( 12.57032717430624480, -3.208883835765893533, 13.62729181966624026 ) ) ;
#62230 = DIRECTION ( 'NONE',  ( -0.7071067759742961645, 0.7071067863987962054, 5.966942998097971758E-08 ) ) ;
#62231 = CARTESIAN_POINT ( 'NONE',  ( 24.92745128319736736, -11.55994776411245262, 3.214489235262763867 ) ) ;
#62232 = CARTESIAN_POINT ( 'NONE',  ( 8.630418146794999856, -5.808258301303999893, 7.446016267012000256 ) ) ;
#62233 = ORIENTED_EDGE ( 'NONE', *, *, #23440, .F. ) ;
#62234 = CARTESIAN_POINT ( 'NONE',  ( 7.956795280408998750, 4.524487726177000013, 9.047753146378999745 ) ) ;
#62236 = CARTESIAN_POINT ( 'NONE',  ( 10.98435104515999861, 5.105444214897000066, 4.879787924579000347 ) ) ;
#62235 = CARTESIAN_POINT ( 'NONE',  ( 5.347090849689999814, 0.7718853692621999718, -1.249287881180999982 ) ) ;
#62237 = CARTESIAN_POINT ( 'NONE',  ( 7.580200994261414138, -4.132977011570006631, 5.765716077822864882 ) ) ;
#62238 = AXIS2_PLACEMENT_3D ( 'NONE', #57082, #20028, #19688 ) ;
#62239 = DIRECTION ( 'NONE',  ( 0.8843050097021416533, -0.1786785991673574547, -0.4313682974156609062 ) ) ;
#62240 = CARTESIAN_POINT ( 'NONE',  ( 1.318883544274000119, -2.924745949230000086, 2.085595834630999956 ) ) ;
#62241 = ORIENTED_EDGE ( 'NONE', *, *, #17839, .F. ) ;
#62242 = CARTESIAN_POINT ( 'NONE',  ( 0.7716437780931045820, 3.201127686947116580, -0.2025159996193092726 ) ) ;
#62243 = CARTESIAN_POINT ( 'NONE',  ( 10.79262282008599882, -3.548418513060800361, 6.771613406921599854 ) ) ;
#62244 = CARTESIAN_POINT ( 'NONE',  ( 11.57240408529958842, 3.267527001822357224, 7.982112976485220557 ) ) ;
#62245 = CARTESIAN_POINT ( 'NONE',  ( 10.37026939687000038, 5.571553923009999743, 7.748385725654999945 ) ) ;
#62246 =( GEOMETRIC_REPRESENTATION_CONTEXT ( 3 ) GLOBAL_UNCERTAINTY_ASSIGNED_CONTEXT ( ( #26892 ) ) GLOBAL_UNIT_ASSIGNED_CONTEXT ( ( #36045, #61933, #52466 ) ) REPRESENTATION_CONTEXT ( 'NONE', 'WORKASPACE' ) );
#62247 = CARTESIAN_POINT ( 'NONE',  ( 11.55610404293055993, 3.497163090439000310, 6.476063885290000322 ) ) ;
#62248 = CARTESIAN_POINT ( 'NONE',  ( 24.17201600611014101, -3.320432398031667898, 12.43436857130917161 ) ) ;
#62249 = CARTESIAN_POINT ( 'NONE',  ( 8.620740978634000129, -4.599999999999999645, 5.898823289756999877 ) ) ;
#62250 = CARTESIAN_POINT ( 'NONE',  ( 11.19955063476130164, 4.976598135215295038, -6.673569913327196623 ) ) ;
#62251 = CARTESIAN_POINT ( 'NONE',  ( 8.246455660830299905, 5.453956472524233767, 8.461650011249977510 ) ) ;
#62252 = ORIENTED_EDGE ( 'NONE', *, *, #49752, .T. ) ;
#62253 = CIRCLE ( 'NONE', #27676, 0.9999999999999993339 ) ;
#62254 = CARTESIAN_POINT ( 'NONE',  ( 18.18368263331580437, -2.882378207881296284, 13.70008584495759152 ) ) ;
#62255 = DIRECTION ( 'NONE',  ( 0.5000000000000169864, 0.000000000000000000, -0.8660254037844288266 ) ) ;
#62256 = VERTEX_POINT ( 'NONE', #16883 ) ;
#62257 = DIRECTION ( 'NONE',  ( 1.000000000000000000, 0.000000000000000000, 0.000000000000000000 ) ) ;
#62258 = DIRECTION ( 'NONE',  ( 0.000000000000000000, 1.000000000000000000, 0.000000000000000000 ) ) ;
#62259 = CARTESIAN_POINT ( 'NONE',  ( 8.486008579191000933, 3.399999999999999911, 5.976611076844000614 ) ) ;
#62260 = CARTESIAN_POINT ( 'NONE',  ( 10.75210807141120029, 4.040019166404060336, 6.634727177901499573 ) ) ;
#62261 = CARTESIAN_POINT ( 'NONE',  ( 9.476372460169001144, 5.098395626600999542, 6.305536056092000408 ) ) ;
#62262 = CARTESIAN_POINT ( 'NONE',  ( 10.77434248675000106, 4.612886656332999991, -8.898793847069001117 ) ) ;
#62263 = CARTESIAN_POINT ( 'NONE',  ( 9.961445400145626294, -3.652722274830687343, -6.696924380570436597 ) ) ;
#62264 = CARTESIAN_POINT ( 'NONE',  ( 11.07345355053000091, -3.998673159585000025, 8.920828114954002075 ) ) ;
#62265 = EDGE_CURVE ( 'NONE', #18362, #65751, #48711, .T. ) ;
#62266 = CARTESIAN_POINT ( 'NONE',  ( 18.26112048795755172, 0.1637242582067865437, -12.59894148523290802 ) ) ;
#62267 = AXIS2_PLACEMENT_3D ( 'NONE', #25980, #27969, #25635 ) ;
#62268 = CARTESIAN_POINT ( 'NONE',  ( 11.39975833414730033, 4.796537143354000499, 7.825000000000000178 ) ) ;
#62269 = CARTESIAN_POINT ( 'NONE',  ( 11.29364426047339975, -3.533902447304699823, -8.230103870496201068 ) ) ;
#62270 = EDGE_CURVE ( 'NONE', #23992, #4182, #28365, .T. ) ;
#62271 = EDGE_CURVE ( 'NONE', #27423, #63357, #49390, .T. ) ;
#62272 = CARTESIAN_POINT ( 'NONE',  ( 6.899999438051000133, 1.266765207443000030, 0.8033093483900000109 ) ) ;
#62273 = ORIENTED_EDGE ( 'NONE', *, *, #27643, .T. ) ;
#62274 = CARTESIAN_POINT ( 'NONE',  ( 10.96507314189000049, -5.561950019225000652, -4.905737662152000134 ) ) ;
#62275 = SURFACE_SIDE_STYLE ('',( #17913 ) ) ;
#62276 = CARTESIAN_POINT ( 'NONE',  ( 24.57937622054645033, -3.599767751962166251, -12.25814915832331842 ) ) ;
#62277 = LINE ( 'NONE', #14394, #24728 ) ;
#62278 = CARTESIAN_POINT ( 'NONE',  ( 17.74439936569994813, 1.785463535057948636, 12.47285731025143463 ) ) ;
#62279 = CARTESIAN_POINT ( 'NONE',  ( 9.633709346416999608, 5.155548326249999924, -6.951281079990299538 ) ) ;
#62280 = CARTESIAN_POINT ( 'NONE',  ( 12.30654613137381759, 1.987682873648402015, 13.85818111229403016 ) ) ;
#62281 = DIRECTION ( 'NONE',  ( 0.000000000000000000, 0.9925108176925445669, 0.1221567712543053380 ) ) ;
#62282 = EDGE_LOOP ( 'NONE', ( #42560, #11859, #35146, #943 ) ) ;
#62283 = CARTESIAN_POINT ( 'NONE',  ( 12.33180295249681713, 0.4082649242943290346, -12.69116688078651833 ) ) ;
#62284 = AXIS2_PLACEMENT_3D ( 'NONE', #18165, #29355, #50666 ) ;
#62285 = CARTESIAN_POINT ( 'NONE',  ( 12.30932141792787959, -0.5329747956504982120, 13.98985355243729245 ) ) ;
#62286 = ORIENTED_EDGE ( 'NONE', *, *, #47801, .T. ) ;
#62287 = CARTESIAN_POINT ( 'NONE',  ( 25.49994615423647204, 2.042074767856997042, -11.11389836053589875 ) ) ;
#62288 = CARTESIAN_POINT ( 'NONE',  ( 18.36651216305128997, 2.877244130631058106, 12.05316132863762846 ) ) ;
#62289 = ADVANCED_FACE ( 'NONE', ( #65465 ), #38915, .F. ) ;
#62290 = CARTESIAN_POINT ( 'NONE',  ( 10.73976354018279977, -4.327184855449098144, -6.282534154164605589 ) ) ;
#62291 = CARTESIAN_POINT ( 'NONE',  ( 11.94133594839949986, -3.430493414882899827, 8.152656755002400502 ) ) ;
#62292 = B_SPLINE_CURVE_WITH_KNOTS ( 'NONE', 3,
 ( #35272, #35617, #14626, #5160 ),
 .UNSPECIFIED., .F., .F.,
 ( 4, 4 ),
 ( 0.8745867815654175814, 1.000000000000000000 ),
 .UNSPECIFIED. ) ;
#62293 = VECTOR ( 'NONE', #51987, 1000.000000000000114 ) ;
#62294 = CARTESIAN_POINT ( 'NONE',  ( 10.26685100253999927, -2.832432432432000269, 6.822293592207000934 ) ) ;
#62295 = DIRECTION ( 'NONE',  ( 0.000000000000000000, 1.000000000000000000, 0.000000000000000000 ) ) ;
#62296 = CARTESIAN_POINT ( 'NONE',  ( 11.32299956498189886, 2.792989229543000107, 7.825000000000000178 ) ) ;
#62297 = CARTESIAN_POINT ( 'NONE',  ( 10.34393020684899867, -5.250000000000000000, -7.500000000000000000 ) ) ;
#62298 = FACE_OUTER_BOUND ( 'NONE', #62282, .T. ) ;
#62299 = CARTESIAN_POINT ( 'NONE',  ( 11.24025954179439957, 4.771812902496799680, -8.141292208271599051 ) ) ;
#62300 = CARTESIAN_POINT ( 'NONE',  ( 10.97499895057999986, -2.398081733189999864E-14, -12.37499919541000004 ) ) ;
#62301 = CARTESIAN_POINT ( 'NONE',  ( 10.38052665877000003, 5.283793195606000026, -8.830196380017000024 ) ) ;
#62302 = CARTESIAN_POINT ( 'NONE',  ( 8.695468108405998819, 5.098602956001000663, -7.811136554427399403 ) ) ;
#62304 = DIRECTION ( 'NONE',  ( 0.000000000000000000, 1.000000000000000000, 0.000000000000000000 ) ) ;
#62303 = CARTESIAN_POINT ( 'NONE',  ( 16.13573769406199787, -8.400696156758000299, -8.016340154447000543 ) ) ;
#62305 = CARTESIAN_POINT ( 'NONE',  ( -0.2999999999999999889, 0.5773502691895999739, 1.000000000000000000 ) ) ;
#62306 = VERTEX_POINT ( 'NONE', #56372 ) ;
#62307 = AXIS2_PLACEMENT_3D ( 'NONE', #53892, #21057, #11244 ) ;
#62308 = CARTESIAN_POINT ( 'NONE',  ( 10.28014141025500017, 4.417352327511700594, 6.756653759087999589 ) ) ;
#62309 = CARTESIAN_POINT ( 'NONE',  ( 9.334658571019252449, 5.771500264757192689, -7.375358915183060304 ) ) ;
#62310 = CARTESIAN_POINT ( 'NONE',  ( 10.33890035061499901, 4.267716286314199969, 6.531924610394499453 ) ) ;
#62311 = CARTESIAN_POINT ( 'NONE',  ( 9.353545867770625577, 4.858658389798049981, -7.668041776205901883 ) ) ;
#62312 = AXIS2_PLACEMENT_3D ( 'NONE', #66373, #39822, #61142 ) ;
#62313 = DIRECTION ( 'NONE',  ( 0.7071067388045961799, 0.7071068235684964121, -1.176037761303994353E-10 ) ) ;
#62314 = EDGE_CURVE ( 'NONE', #24123, #59800, #41955, .T. ) ;
#62315 = CARTESIAN_POINT ( 'NONE',  ( 12.76382664777360354, 3.124999999999999112, 13.52078629068864757 ) ) ;
#62316 = CARTESIAN_POINT ( 'NONE',  ( 9.496463691918865635, -5.100000000000000533, -6.665341197415688868 ) ) ;
#62317 = VERTEX_POINT ( 'NONE', #29820 ) ;
#62318 = B_SPLINE_CURVE_WITH_KNOTS ( 'NONE', 3,
 ( #53038, #19848, #10720, #46765, #20529, #41177, #62484, #5134, #9339, #15969, #53384, #35925, #57238, #68068, #20184, #36267 ),
 .UNSPECIFIED., .F., .F.,
 ( 4, 2, 2, 1, 1, 2, 2, 2, 4 ),
 ( 0.000000000000000000, 0.2499999999999763522, 0.3749999999999656941, 0.4374999999999591438, 0.4687499999999563127, 0.4843749999999565903, 0.4999999999999568123, 0.7499999999999784617, 1.000000000000000000 ),
 .UNSPECIFIED. ) ;
#62319 = CARTESIAN_POINT ( 'NONE',  ( 9.581988259785999773, -4.149395984695000372, -8.631996151823999597 ) ) ;
#62320 = CARTESIAN_POINT ( 'NONE',  ( 6.649999999999999467, 5.221516520829000640, -8.074802043613001246 ) ) ;
#62321 = CARTESIAN_POINT ( 'NONE',  ( 10.89969598649000027, -3.111999510220800236, 6.971269690999399415 ) ) ;
#62322 = PRODUCT_DEFINITION_SHAPE ( 'NONE', 'NONE',  #51754 ) ;
#62323 = CARTESIAN_POINT ( 'NONE',  ( 17.57923549477748537, 1.761145725279485541, -12.47631219955854043 ) ) ;
#62324 = CARTESIAN_POINT ( 'NONE',  ( 11.13500760274999912, -2.665983503042999914, 5.187970728494999406 ) ) ;
#62325 = LINE ( 'NONE', #40313, #19451 ) ;
#62326 = CARTESIAN_POINT ( 'NONE',  ( 12.20440283767314327, 2.672818874493718244, -13.63528575822274469 ) ) ;
#62327 = CARTESIAN_POINT ( 'NONE',  ( 11.64975833414749928, -4.796537143354000499, 7.174999999999999822 ) ) ;
#62328 = CARTESIAN_POINT ( 'NONE',  ( 24.84742972624900403, 11.95752699856999968, 2.993660429748000062 ) ) ;
#62329 = CARTESIAN_POINT ( 'NONE',  ( 9.475279990687656806, -5.350441389720279162, 7.499985493516659218 ) ) ;
#62330 = CARTESIAN_POINT ( 'NONE',  ( 12.08616987952486532, 0.09542514088230683034, -13.99967976774382272 ) ) ;
#62331 = CARTESIAN_POINT ( 'NONE',  ( 23.56664311700400205, 13.31365802054999925, 4.296923094388999331 ) ) ;
#62332 = CARTESIAN_POINT ( 'NONE',  ( 11.10000000432000000, 9.172263358062000549, 6.560374562178000524 ) ) ;
#62333 = CARTESIAN_POINT ( 'NONE',  ( 9.115000000004000569, -5.349999999999999645, -7.500000000000000000 ) ) ;
#62334 = CARTESIAN_POINT ( 'NONE',  ( 9.319414158774000256, 2.656512020013999997, -7.884832994446999699 ) ) ;
#62335 = CARTESIAN_POINT ( 'NONE',  ( 15.90006914250094461, 3.698856701507908795, 11.75540275481943020 ) ) ;
#62336 = ORIENTED_EDGE ( 'NONE', *, *, #4952, .T. ) ;
#62337 = CARTESIAN_POINT ( 'NONE',  ( 8.632946129846605032, -2.796778970782837437, 8.203843119991294230 ) ) ;
#62338 = CARTESIAN_POINT ( 'NONE',  ( 18.16658511877954751, 2.125673232124648759, -13.83768827471936724 ) ) ;
#62339 = EDGE_LOOP ( 'NONE', ( #14977, #1936, #36423, #57878 ) ) ;
#62340 = CARTESIAN_POINT ( 'NONE',  ( 9.807392757686999474, -3.414780058706799792, 6.860292594369099106 ) ) ;
#62341 = CARTESIAN_POINT ( 'NONE',  ( 24.83134246164797787, 3.060673188834726499, 11.69614408486561352 ) ) ;
#62342 = CARTESIAN_POINT ( 'NONE',  ( 9.442010841233001273, 5.045571591548999812, -9.086294919530001124 ) ) ;
#62343 = CARTESIAN_POINT ( 'NONE',  ( 12.80505043854144276, -0.7192913403693027563, 12.57945229203838267 ) ) ;
#62344 = CARTESIAN_POINT ( 'NONE',  ( 10.56080513895999928, -2.973119161490000106, -6.929150654994399083 ) ) ;
#62345 = CARTESIAN_POINT ( 'NONE',  ( 8.970944094206998898, 5.100000000000000533, 6.571291218949999902 ) ) ;
#62346 = CARTESIAN_POINT ( 'NONE',  ( 11.66883611783287655, -12.15999240571540696, -2.000270994041519756 ) ) ;
#62347 = ORIENTED_EDGE ( 'NONE', *, *, #47994, .T. ) ;
#62348 = CARTESIAN_POINT ( 'NONE',  ( 25.30000327618300204, -6.604245036507551141E-15, -11.49994408209238017 ) ) ;
#62349 = EDGE_CURVE ( 'NONE', #68412, #43577, #17459, .T. ) ;
#62350 = CARTESIAN_POINT ( 'NONE',  ( 24.34832162680337575, -12.03537037244042374, 3.224867771903811242 ) ) ;
#62351 = CARTESIAN_POINT ( 'NONE',  ( 9.874770280412001000, 4.038835765825999680, -5.935509327774999733 ) ) ;
#62352 = ORIENTED_EDGE ( 'NONE', *, *, #2747, .F. ) ;
#62353 = CARTESIAN_POINT ( 'NONE',  ( 10.71983649979000042, 3.571741329336999726, -5.696148467328000287 ) ) ;
#62354 =( LENGTH_UNIT ( ) NAMED_UNIT ( * ) SI_UNIT ( .MILLI., .METRE. ) );
#62355 = ORIENTED_EDGE ( 'NONE', *, *, #41065, .F. ) ;
#62356 = CARTESIAN_POINT ( 'NONE',  ( 10.06122949779699915, 4.709679768527199606, 6.435697190503999465 ) ) ;
#62357 = CARTESIAN_POINT ( 'NONE',  ( 17.99268395210761540, -2.053674450599853873, -12.54441556206896990 ) ) ;
#62358 = CARTESIAN_POINT ( 'NONE',  ( 16.09997386696500143, 8.350085070477001992, 8.123950967096998710 ) ) ;
#62359 = AXIS2_PLACEMENT_3D ( 'NONE', #39229, #60552, #3201 ) ;
#62360 = CARTESIAN_POINT ( 'NONE',  ( 4.400000000000000355, 0.5526513453421999511, 1.394480724316999876 ) ) ;
#62361 = CARTESIAN_POINT ( 'NONE',  ( 8.558656770618505050, 3.294700107201707695, 5.942504245731808687 ) ) ;
#62362 = EDGE_LOOP ( 'NONE', ( #15481, #10462, #52087, #48104, #13449 ) ) ;
#62363 = CARTESIAN_POINT ( 'NONE',  ( 24.66708179678231261, -3.571422468857847310, 12.15221134872180997 ) ) ;
#62364 = CARTESIAN_POINT ( 'NONE',  ( 11.25809834123000108, 3.275514549383000240, -8.650774600386998969 ) ) ;
#62365 = EDGE_CURVE ( 'NONE', #21989, #56231, #61272, .T. ) ;
#62366 = AXIS2_PLACEMENT_3D ( 'NONE', #20835, #14904, #57198 ) ;
#62367 = CARTESIAN_POINT ( 'NONE',  ( 19.89999890908300273, 0.000000000000000000, 0.000000000000000000 ) ) ;
#62368 = CARTESIAN_POINT ( 'NONE',  ( 12.63927634677108713, 3.229167277941579872, -13.62249984660984303 ) ) ;
#62369 = ADVANCED_FACE ( 'NONE', ( #8130 ), #17059, .F. ) ;
#62370 = CARTESIAN_POINT ( 'NONE',  ( 17.81056431323685629, 0.6834693007276584353, 13.98330741474946315 ) ) ;
#62371 = CARTESIAN_POINT ( 'NONE',  ( 17.87778689823928246, 11.54766097721278229, -4.850486155499411645 ) ) ;
#62372 = CARTESIAN_POINT ( 'NONE',  ( 10.56591477248000110, -5.293237054095000005, -7.067083954277999958 ) ) ;
#62373 = VERTEX_POINT ( 'NONE', #52141 ) ;
#62374 = ORIENTED_EDGE ( 'NONE', *, *, #52096, .T. ) ;
#62375 = CARTESIAN_POINT ( 'NONE',  ( 9.766460841231999979, 3.135494838036999798, -8.598037907310999373 ) ) ;
#62376 = CARTESIAN_POINT ( 'NONE',  ( 9.643930206848999376, -2.750000000000000000, -7.500000000000000000 ) ) ;
#62377 = CARTESIAN_POINT ( 'NONE',  ( 1.165556799207875249, 0.4581489286485003198, 3.500000000000000444 ) ) ;
#62378 = CARTESIAN_POINT ( 'NONE',  ( 25.57777390266700124, 8.344452479015000534, -8.014498661339999330 ) ) ;
#62379 = CARTESIAN_POINT ( 'NONE',  ( 24.38453586173000076, 8.887473727858999695, -8.991251287490998223 ) ) ;
#62380 = CARTESIAN_POINT ( 'NONE',  ( 18.49055856039300139, -2.949841519493000330, -11.23086453091999992 ) ) ;
#62382 = CARTESIAN_POINT ( 'NONE',  ( 11.09999999999999964, 4.000000000000000000, 7.500000000000000000 ) ) ;
#62381 = CARTESIAN_POINT ( 'NONE',  ( 10.91690035061499842, -3.695660922043800145, 6.399494776650000105 ) ) ;
#62383 = CARTESIAN_POINT ( 'NONE',  ( 12.80505043854143388, 3.124999999999999556, 12.28373071562070074 ) ) ;
#62384 = EDGE_LOOP ( 'NONE', ( #51856, #21113, #20814, #2635, #31019, #36989, #4366 ) ) ;
#62385 = CARTESIAN_POINT ( 'NONE',  ( 25.46373024410000241, -11.23407150414000100, 3.161076981347000103 ) ) ;
#62386 = CARTESIAN_POINT ( 'NONE',  ( 10.38001771741999946, -3.294294314927000311, -5.012847088973000353 ) ) ;
#62387 = CARTESIAN_POINT ( 'NONE',  ( 9.353137413980999071, -5.679455740088000582, -8.329752476417999318 ) ) ;
#62388 = CARTESIAN_POINT ( 'NONE',  ( 7.940355219341154402, 4.833259259596939472, 6.348670065445725541 ) ) ;
#62389 = CIRCLE ( 'NONE', #67927, 2.149999999999999911 ) ;
#62390 = CARTESIAN_POINT ( 'NONE',  ( 18.17998003037035204, -2.509683781248572387, -12.44929946634871953 ) ) ;
#62391 = EDGE_CURVE ( 'NONE', #35353, #2331, #13392, .T. ) ;
#62392 = DIRECTION ( 'NONE',  ( -1.000000000000000000, 0.000000000000000000, 0.000000000000000000 ) ) ;
#62393 = CARTESIAN_POINT ( 'NONE',  ( 9.442010841233001273, 5.045571591548999812, -9.086294919530001124 ) ) ;
#62394 = CARTESIAN_POINT ( 'NONE',  ( 14.04004776902899998, 8.829547661313998930, 7.819892149868999276 ) ) ;
#62395 = CARTESIAN_POINT ( 'NONE',  ( 7.978216579186597990, 3.009178048233850156, -6.462117657976292229 ) ) ;
#62396 = CARTESIAN_POINT ( 'NONE',  ( 6.462873758167999583, 0.02828639361845000297, -1.175746811673999970 ) ) ;
#62397 = CARTESIAN_POINT ( 'NONE',  ( 0.2021281585065432262, 3.118434889361825668, -0.8389436472200255679 ) ) ;
#62398 = CARTESIAN_POINT ( 'NONE',  ( 3.634748863956000164, -1.556094637422999805, -2.863599491026000088 ) ) ;
#62399 = ORIENTED_EDGE ( 'NONE', *, *, #28841, .F. ) ;
#62400 = CARTESIAN_POINT ( 'NONE',  ( 12.78111495345091697, 0.7189971323193988795, -12.57946912511938109 ) ) ;
#62401 = CARTESIAN_POINT ( 'NONE',  ( 12.19222608800083663, -2.622765415629520813, -12.42211422045274105 ) ) ;
#62402 = FACE_OUTER_BOUND ( 'NONE', #36058, .T. ) ;
#62403 = CARTESIAN_POINT ( 'NONE',  ( 24.50399615158200106, 3.502219942208999903, -12.23695409027999936 ) ) ;
#62404 =( LENGTH_UNIT ( ) NAMED_UNIT ( * ) SI_UNIT ( .MILLI., .METRE. ) );
#62405 = EDGE_LOOP ( 'NONE', ( #32094, #24323, #14736, #64547, #30957, #66280, #54056, #3142, #62674, #12911, #54828, #627 ) ) ;
#62406 = FACE_OUTER_BOUND ( 'NONE', #12372, .T. ) ;
#62407 = APPLICATION_PROTOCOL_DEFINITION ( 'draft international standard', 'automotive_design', 1998, #15925 ) ;
#62408 = CARTESIAN_POINT ( 'NONE',  ( 17.69809845384140701, 0.6087666915464966522, 12.68035271361765126 ) ) ;
#62409 = CARTESIAN_POINT ( 'NONE',  ( 12.96427412810700197, -11.57018092489999894, -1.758708699944000031 ) ) ;
#62410 = CARTESIAN_POINT ( 'NONE',  ( 17.55505043854143565, 3.199698446519375850, 12.18695736643652694 ) ) ;
#62411 = CARTESIAN_POINT ( 'NONE',  ( 10.72702344389999851, 2.995605560827999891, -6.890449684422599752 ) ) ;
#62412 = ORIENTED_EDGE ( 'NONE', *, *, #15939, .T. ) ;
#62413 = CARTESIAN_POINT ( 'NONE',  ( 11.27765354842000001, -3.273798832483999721, 6.368296067120999382 ) ) ;
#62414 = VERTEX_POINT ( 'NONE', #46223 ) ;
#62415 = CARTESIAN_POINT ( 'NONE',  ( 9.152931135682532471, 5.100000000000000533, -6.444141223442171551 ) ) ;
#62416 = CARTESIAN_POINT ( 'NONE',  ( 9.266941940380000631, -3.049610585291000042, 6.392533570808999421 ) ) ;
#62417 = CARTESIAN_POINT ( 'NONE',  ( 15.83176382712000319, 8.647155996545000889, 8.162171193140999037 ) ) ;
#62418 = ORIENTED_EDGE ( 'NONE', *, *, #18176, .T. ) ;
#62419 = CARTESIAN_POINT ( 'NONE',  ( -0.000000000000000000, 1.460960874861672698, -2.533832635912068199 ) ) ;
#62420 = CARTESIAN_POINT ( 'NONE',  ( 5.500000000000000000, 1.600000000000000089, 0.000000000000000000 ) ) ;
#62421 = CARTESIAN_POINT ( 'NONE',  ( 6.993814158770001121, 4.468431922689999780, -6.183326950307000303 ) ) ;
#62422 = CARTESIAN_POINT ( 'NONE',  ( 0.000000000000000000, 0.000000000000000000, 0.000000000000000000 ) ) ;
#62423 = CARTESIAN_POINT ( 'NONE',  ( 5.500000000000000000, 12.43893545635000031, 2.828937028792000152 ) ) ;
#62424 = VERTEX_POINT ( 'NONE', #25583 ) ;
#62425 = CARTESIAN_POINT ( 'NONE',  ( 11.27109998545999936, -5.469594811916000054, 8.504700858852999090 ) ) ;
#62426 = EDGE_CURVE ( 'NONE', #5439, #26882, #44163, .T. ) ;
#62427 = EDGE_CURVE ( 'NONE', #54502, #44042, #57560, .T. ) ;
#62428 = CARTESIAN_POINT ( 'NONE',  ( 12.19551626500196839, -2.360211740052808427, -13.70208339272018350 ) ) ;
#62429 = FACE_OUTER_BOUND ( 'NONE', #47108, .T. ) ;
#62430 = VERTEX_POINT ( 'NONE', #25924 ) ;
#62431 = CARTESIAN_POINT ( 'NONE',  ( 10.25166529434999951, -3.418639857622999934, -8.733652610425998830 ) ) ;
#62432 = DIRECTION ( 'NONE',  ( -0.7071067759742961645, -0.7071067863987962054, -5.966942998097971758E-08 ) ) ;
#62433 = ORIENTED_EDGE ( 'NONE', *, *, #2855, .T. ) ;
#62434 = CARTESIAN_POINT ( 'NONE',  ( 11.37299956498129916, -5.207010770456999893, -7.174999999999999822 ) ) ;
#62435 = DIRECTION ( 'NONE',  ( 0.000000000000000000, -0.9466492601157000530, 0.3222656952305000266 ) ) ;
#62436 = CARTESIAN_POINT ( 'NONE',  ( 17.55505043854143565, 2.500000000000000000, -25.00000000000000000 ) ) ;
#62437 = CARTESIAN_POINT ( 'NONE',  ( 8.933148997457999840, 5.167567567567999731, 6.822293592207000934 ) ) ;
#62438 = CARTESIAN_POINT ( 'NONE',  ( 12.37030616679614070, 0.4491394412341185860, -13.89023495843588840 ) ) ;
#62439 = CARTESIAN_POINT ( 'NONE',  ( 17.88838831427751686, -1.971212373206994384, 12.55919681887186456 ) ) ;
#62440 = ORIENTED_EDGE ( 'NONE', *, *, #13666, .T. ) ;
#62441 = CARTESIAN_POINT ( 'NONE',  ( 7.915155411429996235, -5.089315853099998677, 6.494606418034001294 ) ) ;
#62442 = ORIENTED_EDGE ( 'NONE', *, *, #25137, .T. ) ;
#62443 = CARTESIAN_POINT ( 'NONE',  ( 9.736878146978000359, 2.742182981761000171, 6.839230404018000087 ) ) ;
#62444 = EDGE_CURVE ( 'NONE', #40213, #17921, #25881, .T. ) ;
#62445 = CARTESIAN_POINT ( 'NONE',  ( 11.25962254157670905, -3.830327337663943510, -8.360248390549317676 ) ) ;
#62446 = CARTESIAN_POINT ( 'NONE',  ( 8.690229719593000723, 2.414630869937000046, -6.801495146585999407 ) ) ;
#62447 = CARTESIAN_POINT ( 'NONE',  ( 3.313094297425999812, -3.277373826264000201, -1.734488728539000046 ) ) ;
#62448 = ADVANCED_FACE ( 'NONE', ( #62298 ), #63311, .T. ) ;
#62449 = CARTESIAN_POINT ( 'NONE',  ( 17.33333333083533390, -3.216308279608389054, -11.40341444610950283 ) ) ;
#62450 = CARTESIAN_POINT ( 'NONE',  ( 10.93769855012999948, 2.936883479403999964, 4.920828759365000415 ) ) ;
#62451 = CARTESIAN_POINT ( 'NONE',  ( 23.54916660312699861, 13.36550856414000066, 4.293655460768000864 ) ) ;
#62452 = EDGE_LOOP ( 'NONE', ( #22935, #37915, #68807, #14807 ) ) ;
#62453 = CARTESIAN_POINT ( 'NONE',  ( 11.14533863405319991, -3.296214805808900028, 6.602238051205399749 ) ) ;
#62454 = CARTESIAN_POINT ( 'NONE',  ( 10.35096486449576503, 5.732427394192054493, -7.739054094300635178 ) ) ;
#62455 = CARTESIAN_POINT ( 'NONE',  ( 11.09999999999999964, -2.274006712557999688, -7.281956340829000673 ) ) ;
#62456 = CARTESIAN_POINT ( 'NONE',  ( 10.90000000162999960, 2.899999999992999733, -5.160242739096000619 ) ) ;
#62457 = VECTOR ( 'NONE', #48655, 1000.000000000000227 ) ;
#62459 = DIRECTION ( 'NONE',  ( 0.000000000000000000, -1.000000000000000000, 0.000000000000000000 ) ) ;
#62458 = CARTESIAN_POINT ( 'NONE',  ( 10.24961997674000003, 4.184221916050000267, 9.286882020979000174 ) ) ;
#62460 = CARTESIAN_POINT ( 'NONE',  ( 11.58071932425156980, 3.832730087831799803, -8.628410767520000135 ) ) ;
#62461 = CARTESIAN_POINT ( 'NONE',  ( -17.56123417799999942, 13.94845324556000143, 4.312847325879000770 ) ) ;
#62462 = CARTESIAN_POINT ( 'NONE',  ( 8.947809814040999399, 4.698458605182900705, -8.403266072559899769 ) ) ;
#62463 = CARTESIAN_POINT ( 'NONE',  ( 17.72055336043788287, 0.7006927685644959158, 12.58050281163332151 ) ) ;
#62464 = FACE_OUTER_BOUND ( 'NONE', #2278, .T. ) ;
#62465 = CARTESIAN_POINT ( 'NONE',  ( 11.68277869730536977, 3.468607053297499743, 8.547856079839998955 ) ) ;
#62466 = CARTESIAN_POINT ( 'NONE',  ( 23.81909306311399988, 9.670551759768001077, 9.332972164518999136 ) ) ;
#62467 = ORIENTED_EDGE ( 'NONE', *, *, #12009, .T. ) ;
#62468 = CARTESIAN_POINT ( 'NONE',  ( 8.064120559623999540, -4.228293421747000735, 8.941387937291999322 ) ) ;
#62469 = CARTESIAN_POINT ( 'NONE',  ( 17.67416556365684244, 3.238622530711260605, 13.62025504818856625 ) ) ;
#62470 = CARTESIAN_POINT ( 'NONE',  ( 5.000030787343001215, -1.290525307673963118, -1.679270695423619175 ) ) ;
#62471 = ORIENTED_EDGE ( 'NONE', *, *, #51689, .F. ) ;
#62472 = CARTESIAN_POINT ( 'NONE',  ( 18.17677363193000062, 3.419785592864999835, 11.99291007725999947 ) ) ;
#62473 = CARTESIAN_POINT ( 'NONE',  ( 11.75203632436369894, 2.890282938442000127, 7.759151359668400083 ) ) ;
#62474 = CARTESIAN_POINT ( 'NONE',  ( 10.84974221959000218, 5.265003089217000998, -6.385808769407000263 ) ) ;
#62475 = ADVANCED_FACE ( 'NONE', ( #40974 ), #40624, .T. ) ;
#62476 = ORIENTED_EDGE ( 'NONE', *, *, #3881, .F. ) ;
#62477 = ADVANCED_FACE ( 'NONE', ( #56720 ), #8815, .F. ) ;
#62478 = CARTESIAN_POINT ( 'NONE',  ( 1.373890132540666720, -2.150913519912200922, -2.798833948393631754 ) ) ;
#62479 = CARTESIAN_POINT ( 'NONE',  ( 18.27937482164658789, -2.670364552392027857, 12.31525491564956809 ) ) ;
#62480 = CARTESIAN_POINT ( 'NONE',  ( 10.12841772631199966, 4.490588993294299947, 6.490165927606000196 ) ) ;
#62481 = DIRECTION ( 'NONE',  ( -1.000000000000000000, 0.000000000000000000, 0.000000000000000000 ) ) ;
#62482 = CARTESIAN_POINT ( 'NONE',  ( 5.500000000000000000, -11.95749337870000062, -3.642574926947999892 ) ) ;
#62483 = VERTEX_POINT ( 'NONE', #3559 ) ;
#62484 = CARTESIAN_POINT ( 'NONE',  ( 7.834511717026050093, -4.924825534011793238, 6.461662825486788719 ) ) ;
#62485 = CARTESIAN_POINT ( 'NONE',  ( 15.88832047282411075, 8.582214862760459084, 8.173711952084858012 ) ) ;
#62486 = CARTESIAN_POINT ( 'NONE',  ( 8.276895518193162715, -4.975196787739221804, 8.941828154844815302 ) ) ;
#62487 = CARTESIAN_POINT ( 'NONE',  ( 9.600734463322998735, -3.881063085044400118, 6.364399516445999438 ) ) ;
#62488 = ORIENTED_EDGE ( 'NONE', *, *, #64336, .T. ) ;
#62489 = PLANE ( 'NONE',  #43362 ) ;
#62490 = B_SPLINE_CURVE_WITH_KNOTS ( 'NONE', 3,
 ( #4000, #41763, #56472, #36515 ),
 .UNSPECIFIED., .F., .F.,
 ( 4, 4 ),
 ( 0.000000000000000000, 0.4999999997918080918 ),
 .UNSPECIFIED. ) ;
#62491 = CARTESIAN_POINT ( 'NONE',  ( 13.49980696793000057, -9.514462421839999351, -7.834836582454001608 ) ) ;
#62492 = VERTEX_POINT ( 'NONE', #24894 ) ;
#62493 = CARTESIAN_POINT ( 'NONE',  ( 7.307500000000000107, -0.2999999999999999889, -3.149999999999999911 ) ) ;
#62494 = VERTEX_POINT ( 'NONE', #67531 ) ;
#62495 = DIRECTION ( 'NONE',  ( 0.000000000000000000, 1.000000000000000000, 0.000000000000000000 ) ) ;
#62496 = LINE ( 'NONE', #41524, #19340 ) ;
#62497 = CARTESIAN_POINT ( 'NONE',  ( 10.51414141025500015, 4.615773412711500434, -8.596754040696000132 ) ) ;
#62498 = CARTESIAN_POINT ( 'NONE',  ( 12.21922412107039868, -3.930460928605089777, 8.814426450544999625 ) ) ;
#62499 = CARTESIAN_POINT ( 'NONE',  ( 12.48995884033423032, 1.960141145868676382, -12.56111957647685351 ) ) ;
#62500 = CARTESIAN_POINT ( 'NONE',  ( 10.89918582084299992, -4.746348444722899629, 8.362701637490498996 ) ) ;
#62501 = CARTESIAN_POINT ( 'NONE',  ( 8.079135841228998416, 3.524748802314000340, 5.573833469815000718 ) ) ;
#62502 = EDGE_CURVE ( 'NONE', #3171, #28855, #19653, .T. ) ;
#62503 = ADVANCED_FACE ( 'NONE', ( #30130 ), #47752, .T. ) ;
#62504 = ORIENTED_EDGE ( 'NONE', *, *, #39392, .T. ) ;
#62505 = CIRCLE ( 'NONE', #7822, 13.17499999999999893 ) ;
#62506 = DIRECTION ( 'NONE',  ( -1.000000000000000000, 0.000000000000000000, 0.000000000000000000 ) ) ;
#62507 = EDGE_CURVE ( 'NONE', #5914, #60441, #66744, .T. ) ;
#62508 = CARTESIAN_POINT ( 'NONE',  ( 8.610058059625000482, -5.329429281359999493, 6.027400270608000099 ) ) ;
#62509 = LINE ( 'NONE', #52713, #20091 ) ;
#62510 = ORIENTED_EDGE ( 'NONE', *, *, #2276, .F. ) ;
#62511 = B_SPLINE_SURFACE_WITH_KNOTS ( 'NONE', 3, 3, ( 
 ( #1076, #1766, #28693, #39516, #17143, #32891, #59797, #65381, #38825, #2117, #23084, #59450, #65729, #60493, #12953, #60152, #33238, #54903, #7006, #27997, #49306, #1418, #28338, #12257, #17852, #49657, #39170, #12602, #2452, #7348, #50006, #23434, #44773, #66073, #18194 ),
 ( #60841, #38475, #34280, #55600, #7701, #29042, #23777, #45112, #38123, #54201, #6302, #27649, #48968, #65026, #35653, #25150, #8391, #13985, #19910, #24121, #35311, #61527, #56628, #24812, #35982, #19566, #57300, #34969, #40888, #8732, #34629, #3476, #18541, #56967, #46482 ),
 ( #9068, #29735, #30406, #55942, #61187, #51038, #13642, #25496, #41235, #30076, #62546, #62209, #51718, #51377, #14330, #67106, #61865, #24468, #56286, #3811, #67788, #45793, #3140, #14669, #19214, #9403, #39867, #40541, #67443, #46137, #30745, #52054, #4157, #8044, #46826 ),
 ( #13307, #29388, #45456, #50698, #2795, #66768, #18885, #40211, #37359, #4498, #5195, #69167, #21616, #36680, #10439, #31099, #25839, #52405, #37024, #47167, #31435, #16029, #68470, #41575, #15352, #16373, #42951, #63578, #58001, #10100, #52751, #63917, #32128, #26190, #32467 ) ),
 .UNSPECIFIED., .F., .F., .F.,
 ( 4, 4 ),
 ( 4, 1, 1, 1, 1, 1, 1, 1, 1, 1, 1, 1, 1, 1, 1, 1, 1, 1, 1, 1, 1, 1, 1, 1, 1, 1, 1, 1, 1, 1, 1, 1, 4 ),
 ( -0.1039370721279000015, 1.103937072127999963 ),
 ( -0.01933701211302999920, 0.01208563257065999909, 0.04350827725433999843, 0.07493092193802000645, 0.1063535666217000075, 0.1377762113054000204, 0.1691988559891000055, 0.2006215006727000150, 0.2320441453564000001, 0.2634667900400999851, 0.2948894347238000258, 0.3263120794074999553, 0.3577347240911999959, 0.3891573687748000054, 0.4205800134584999905, 0.4520026581421999756, 0.4834253028259000162, 0.5148479475096000568, 0.5462705921932000663, 0.5776932368768999959, 0.6091158815606000365, 0.6405385262443000771, 0.6719611709280000067, 0.7033838156117000473, 0.7348064602953000568, 0.7662291049789999864, 0.7976517496627000270, 0.8290743943464000676, 0.8604970390300999972, 0.8919196837138000378, 0.9233423283974000473, 0.9547649730810999769, 0.9861876177648000175 ),
 .UNSPECIFIED. ) ;
#62512 = CARTESIAN_POINT ( 'NONE',  ( 12.63789105315733075, -1.779885672808168895, -12.47365341745800649 ) ) ;
#62513 = CARTESIAN_POINT ( 'NONE',  ( 11.47810404293059960, 3.436653965247300047, 6.352848032645000309 ) ) ;
#62514 = CARTESIAN_POINT ( 'NONE',  ( 10.97819314679000158, -5.476828481365000556, -7.128717489481000591 ) ) ;
#62515 = CARTESIAN_POINT ( 'NONE',  ( 6.345434501008996975, 9.270874106397998915, -4.897694007782000369 ) ) ;
#62516 = CARTESIAN_POINT ( 'NONE',  ( 17.72467941260600099, -11.93112142875000004, 3.264904591444000026 ) ) ;
#62517 = CARTESIAN_POINT ( 'NONE',  ( 24.56500367260400353, -8.792450275132999593, 9.097562848838000704 ) ) ;
#62518 = CARTESIAN_POINT ( 'NONE',  ( 12.37528356179629441, -2.046093867836326297, -13.75926687192407094 ) ) ;
#62519 = CARTESIAN_POINT ( 'NONE',  ( 10.43210941423799909, -3.358814833524500276, -6.917608226833099394 ) ) ;
#62520 = CARTESIAN_POINT ( 'NONE',  ( 11.23195122972050086, -3.492749840905900349, -6.326963915009999440 ) ) ;
#62521 = CARTESIAN_POINT ( 'NONE',  ( 8.517841509200911432, -5.092672768596408162, 6.425478427622871358 ) ) ;
#62522 = VERTEX_POINT ( 'NONE', #38798 ) ;
#62523 = ORIENTED_EDGE ( 'NONE', *, *, #57603, .F. ) ;
#62524 = CARTESIAN_POINT ( 'NONE',  ( 12.43971800581059739, -0.6379138416578148396, -13.98550699733554303 ) ) ;
#62525 = SHAPE_REPRESENTATION_RELATIONSHIP ( 'NONE' , 'NONE' ,  #46027, #46907 ) ;
#62526 = DIRECTION ( 'NONE',  ( -1.000000000000000000, 0.000000000000000000, 0.000000000000000000 ) ) ;
#62527 = CARTESIAN_POINT ( 'NONE',  ( 17.92070696553032505, 3.007249353054399332, 13.55264287719425376 ) ) ;
#62528 = CARTESIAN_POINT ( 'NONE',  ( 9.831594052344000190, 3.539229510464000139, -8.956011942092999334 ) ) ;
#62529 = EDGE_CURVE ( 'NONE', #15832, #67326, #49628, .T. ) ;
#62530 = CARTESIAN_POINT ( 'NONE',  ( 6.999998782146999332, 0.000000000000000000, 0.000000000000000000 ) ) ;
#62531 = CARTESIAN_POINT ( 'NONE',  ( 17.89623257347365382, 3.023758741516315407, 12.31397229722846731 ) ) ;
#62532 = CARTESIAN_POINT ( 'NONE',  ( 17.95534550153200115, 3.277905616156999713, -11.84067279748999901 ) ) ;
#62533 = CARTESIAN_POINT ( 'NONE',  ( 9.323722176100000425, 3.947350570199999797, 6.051869652381999920 ) ) ;
#62534 = CARTESIAN_POINT ( 'NONE',  ( 8.665068710487354053, -4.836047963814035455, -6.439919795970022065 ) ) ;
#62535 = EDGE_LOOP ( 'NONE', ( #2805, #67133, #36904, #48864 ) ) ;
#62536 = CARTESIAN_POINT ( 'NONE',  ( 10.21609109105999913, 5.961715741921000067, 7.319666990313999477 ) ) ;
#62537 = CARTESIAN_POINT ( 'NONE',  ( 8.766480666858997850, -3.710922827228400056, -8.317400147935998689 ) ) ;
#62538 = CARTESIAN_POINT ( 'NONE',  ( 10.31457848836000046, 5.362142879234999882, 6.677781064327999339 ) ) ;
#62539 = CARTESIAN_POINT ( 'NONE',  ( 11.43479632507519916, -3.442212747724900268, 6.465962698293999722 ) ) ;
#62540 = CARTESIAN_POINT ( 'NONE',  ( 9.716735841232001292, 3.941185585667000169, -8.896279800194999865 ) ) ;
#62541 = CARTESIAN_POINT ( 'NONE',  ( 10.59393020684899867, 5.250000000000000000, 7.500000000000000000 ) ) ;
#62542 = CARTESIAN_POINT ( 'NONE',  ( 24.46225921258299962, 8.785799836126999551, 8.709231069799999503 ) ) ;
#62543 = CARTESIAN_POINT ( 'NONE',  ( 12.70318068537855893, 0.6169782284476045264, 12.67981870385669652 ) ) ;
#62544 = B_SPLINE_CURVE_WITH_KNOTS ( 'NONE', 3,
 ( #18737, #28544, #66958, #19065 ),
 .UNSPECIFIED., .F., .F.,
 ( 4, 4 ),
 ( 0.000000000000000000, 1.000000000000000000 ),
 .UNSPECIFIED. ) ;
#62545 = CARTESIAN_POINT ( 'NONE',  ( 5.656849040861676059, -12.07883750123030708, -3.735095616319062284 ) ) ;
#62546 = CARTESIAN_POINT ( 'NONE',  ( 9.662551629919999385, 4.094830335839000135, 9.119946295870999364 ) ) ;
#62547 = PLANE ( 'NONE',  #53416 ) ;
#62548 = ORIENTED_EDGE ( 'NONE', *, *, #63952, .T. ) ;
#62549 = CARTESIAN_POINT ( 'NONE',  ( 8.830545280412000153, 3.207599814920999659, -6.150466394809999571 ) ) ;
#62550 = CARTESIAN_POINT ( 'NONE',  ( 10.12426357027499790, 5.254871132332000094, -7.742104041724699570 ) ) ;
#62551 = CARTESIAN_POINT ( 'NONE',  ( 9.007644528442998677, 4.705791426005982991, 8.704816259181130889 ) ) ;
#62552 = CARTESIAN_POINT ( 'NONE',  ( 17.55505043854147118, -3.125000000000000000, 12.28374638332999780 ) ) ;
#62553 = CARTESIAN_POINT ( 'NONE',  ( 12.10000000000000142, -4.794859953698269450, 7.924485708373448567 ) ) ;
#62554 = AXIS2_PLACEMENT_3D ( 'NONE', #1435, #64701, #16812 ) ;
#62555 = CARTESIAN_POINT ( 'NONE',  ( 11.06795257254739973, -4.963546614172099858, -7.780229861306499295 ) ) ;
#62556 = ORIENTED_EDGE ( 'NONE', *, *, #42525, .F. ) ;
#62557 = CARTESIAN_POINT ( 'NONE',  ( 1.772746615351999955, -3.758001540264999996, 0.07616889274500000806 ) ) ;
#62558 = CARTESIAN_POINT ( 'NONE',  ( 11.49999672495000169, -3.632761979779000061, 11.06912554803999882 ) ) ;
#62561 = CARTESIAN_POINT ( 'NONE',  ( 13.82798078375900275, -9.420238147574000465, -8.170996254510999535 ) ) ;
#62560 = CARTESIAN_POINT ( 'NONE',  ( 9.808929255601938735, 4.355736776651455422, 9.240861898867757773 ) ) ;
#62559 = PRODUCT_DEFINITION_CONTEXT ( 'detailed design', #43610, 'design' ) ;
#62562 = LINE ( 'NONE', #57318, #25736 ) ;
#62563 = EDGE_CURVE ( 'NONE', #26452, #23033, #27968, .T. ) ;
#62564 = EDGE_CURVE ( 'NONE', #14826, #44907, #3960, .T. ) ;
#62565 = DIRECTION ( 'NONE',  ( 1.000000000000000000, 0.000000000000000000, 0.000000000000000000 ) ) ;
#62566 = CARTESIAN_POINT ( 'NONE',  ( 18.01266241223994768, -2.926178784092879681, -13.57373383468747186 ) ) ;
#62567 = CARTESIAN_POINT ( 'NONE',  ( 11.19518313518939934, 3.462699341914400097, 6.820583637845799352 ) ) ;
#62568 = CARTESIAN_POINT ( 'NONE',  ( 27.64127793187000037, -5.599999999999999645, 6.571291218949999902 ) ) ;
#62569 = CARTESIAN_POINT ( 'NONE',  ( 8.052730646792999991, -4.968144979409999884, 5.971795951526999602 ) ) ;
#62570 = ORIENTED_EDGE ( 'NONE', *, *, #31576, .T. ) ;
#62571 = CARTESIAN_POINT ( 'NONE',  ( 8.791232780412000736, 5.095085596809999728, 6.286981168432999922 ) ) ;
#62573 = CARTESIAN_POINT ( 'NONE',  ( 9.964045559621999004, -3.485908552077000344, -9.275738075927998594 ) ) ;
#62572 = CARTESIAN_POINT ( 'NONE',  ( 6.377250463384999790, 1.514695785805999950, 0.5594970275663000425 ) ) ;
#62574 = CARTESIAN_POINT ( 'NONE',  ( 7.590451290858640121, -4.346862521704085935, 5.795392881046511846 ) ) ;
#62575 = FACE_OUTER_BOUND ( 'NONE', #40682, .T. ) ;
#62576 = CARTESIAN_POINT ( 'NONE',  ( 0.7371534748590999886, 2.178673723483000035, -2.162625512369000358 ) ) ;
#62577 = ORIENTED_EDGE ( 'NONE', *, *, #61317, .F. ) ;
#62578 = DIRECTION ( 'NONE',  ( 1.000000000000000000, 0.000000000000000000, 0.000000000000000000 ) ) ;
#62579 = CARTESIAN_POINT ( 'NONE',  ( 10.85826357027499967, -3.149486845331399998, 7.335909308151700614 ) ) ;
#62580 = CARTESIAN_POINT ( 'NONE',  ( 9.657553581808000942, 5.333455947841000189, 6.049916795084000043 ) ) ;
#62581 = CARTESIAN_POINT ( 'NONE',  ( 9.646287586158999616, 2.591467678478000192, 6.760055064032999717 ) ) ;
#62582 = CARTESIAN_POINT ( 'NONE',  ( 11.13764426047339917, 4.613828180779599997, 6.538488127609999978 ) ) ;
#62583 = CARTESIAN_POINT ( 'NONE',  ( 10.10000000000000142, 0.000000000000000000, 0.000000000000000000 ) ) ;
#62584 = CARTESIAN_POINT ( 'NONE',  ( 18.50001572531400029, 2.908166856580999937, -12.18270046149000052 ) ) ;
#62585 = CARTESIAN_POINT ( 'NONE',  ( 24.53429015151300163, -3.614318902553999902, -12.31267542782000035 ) ) ;
#62586 = CARTESIAN_POINT ( 'NONE',  ( 24.63408906255500241, -3.094015452922999732, -11.81699230461000028 ) ) ;
#62587 = CARTESIAN_POINT ( 'NONE',  ( 18.00853468083869302, -1.948185427393968716, 13.86378859567400568 ) ) ;
#62589 = EDGE_CURVE ( 'NONE', #52961, #25295, #50032, .T. ) ;
#62588 = FACE_OUTER_BOUND ( 'NONE', #22603, .T. ) ;
#62590 = VERTEX_POINT ( 'NONE', #64997 ) ;
#62591 = CARTESIAN_POINT ( 'NONE',  ( 15.92727146503378499, -9.312591611299774641, -8.375703117199135406 ) ) ;
#62592 = DIRECTION ( 'NONE',  ( 0.000000000000000000, 1.000000000000000000, 0.000000000000000000 ) ) ;
#62593 = ORIENTED_EDGE ( 'NONE', *, *, #66317, .F. ) ;
#62594 = CARTESIAN_POINT ( 'NONE',  ( 11.58902763632552002, 3.213494089586499847, 7.862914650060299770 ) ) ;
#62595 = CARTESIAN_POINT ( 'NONE',  ( 9.972850246170999355, 5.044468801812000081, 6.258104779495000436 ) ) ;
#62596 = CARTESIAN_POINT ( 'NONE',  ( 10.27571527605999968, 5.689443924112000062, -7.562019866568999049 ) ) ;
#62597 = CARTESIAN_POINT ( 'NONE',  ( 10.01210369451062654, -4.198138975488563851, -6.647783351891156656 ) ) ;
#62598 = CARTESIAN_POINT ( 'NONE',  ( 10.51654446536000087, -4.930670681812999945, 8.573593359022000371 ) ) ;
#62599 = CARTESIAN_POINT ( 'NONE',  ( 18.28005836700934239, -0.01123479547583286324, -12.60000044989513590 ) ) ;
#62600 = CARTESIAN_POINT ( 'NONE',  ( 10.60198654464000079, -2.164987663130000239, -7.764523632348000248 ) ) ;
#62601 = CARTESIAN_POINT ( 'NONE',  ( 10.38287885159599888, -3.139900861731399928, -7.397393329751199786 ) ) ;
#62602 = DIRECTION ( 'NONE',  ( 0.9999999999985111909, -8.580731922641101058E-07, -1.497129875399016346E-06 ) ) ;
#62603 = VERTEX_POINT ( 'NONE', #39489 ) ;
#62604 = AXIS2_PLACEMENT_3D ( 'NONE', #19756, #40387, #61712 ) ;
#62605 = B_SPLINE_CURVE_WITH_KNOTS ( 'NONE', 3,
 ( #32419, #42222, #58286, #53395, #5145, #26481, #42557, #63866, #5494, #26829, #21565, #23642, #1288, #44980, #22258, #44301, #28915, #66285, #18409, #60360, #48837, #11764 ),
 .UNSPECIFIED., .F., .F.,
 ( 4, 2, 2, 1, 1, 2, 2, 2, 2, 2, 2, 4 ),
 ( 0.000000000000000000, 0.1249999999999863998, 0.1874999999999805433, 0.2187499999999784062, 0.2343749999999749367, 0.2421874999999744926, 0.2499999999999740208, 0.3749999999999827360, 0.4374999999999875655, 0.4687499999999886202, 0.4999999999999896749, 1.000000000000000000 ),
 .UNSPECIFIED. ) ;
#62606 = CARTESIAN_POINT ( 'NONE',  ( 11.12373728587000166, -6.332991536706000346, -5.421362649029999758 ) ) ;
#62607 = DIRECTION ( 'NONE',  ( 0.000000000000000000, -0.2461538461537955691, -0.9692307692307821076 ) ) ;
#62608 = FACE_OUTER_BOUND ( 'NONE', #29961, .T. ) ;
#62609 = PLANE ( 'NONE',  #48183 ) ;
#62610 = EDGE_CURVE ( 'NONE', #798, #52567, #44217, .T. ) ;
#62611 = CARTESIAN_POINT ( 'NONE',  ( 7.000000000000000000, 8.307879248642999315, -4.307879248643000203 ) ) ;
#62612 = CARTESIAN_POINT ( 'NONE',  ( 12.11707904423852966, 2.286486548259629714, 13.81204227851268840 ) ) ;
#62613 = FACE_OUTER_BOUND ( 'NONE', #47438, .T. ) ;
#62614 = ORIENTED_EDGE ( 'NONE', *, *, #10559, .F. ) ;
#62615 = CARTESIAN_POINT ( 'NONE',  ( 12.42340696030921521, 0.4949990735619317905, -12.68701406540670540 ) ) ;
#62616 = CARTESIAN_POINT ( 'NONE',  ( 12.30074708396108996, -0.5247499651446895230, 13.99016470477802265 ) ) ;
#62617 = ORIENTED_EDGE ( 'NONE', *, *, #1617, .T. ) ;
#62618 = CARTESIAN_POINT ( 'NONE',  ( 12.53584957871194128, -1.812149883874480505, 12.46900695079345489 ) ) ;
#62619 = CARTESIAN_POINT ( 'NONE',  ( 9.883148997457000817, 5.167567567567999731, 6.822293592207000934 ) ) ;
#62620 = CARTESIAN_POINT ( 'NONE',  ( 16.00806624337635142, 9.235483320791411543, 8.460674029563245213 ) ) ;
#62621 = CARTESIAN_POINT ( 'NONE',  ( 11.39979975933730039, -3.180925410802600162, 7.781807394638899922 ) ) ;
#62622 = CARTESIAN_POINT ( 'NONE',  ( 9.817462135711998883, 5.100000000000000533, 6.571291218949999902 ) ) ;
#62623 = FACE_OUTER_BOUND ( 'NONE', #30447, .T. ) ;
#62624 = CARTESIAN_POINT ( 'NONE',  ( 8.969356963619999235, 2.880642974985999860, 7.500000000085178087 ) ) ;
#62625 = CARTESIAN_POINT ( 'NONE',  ( 12.21223476585295487, 2.065380716993680199, 12.42958554107382163 ) ) ;
#62626 = CARTESIAN_POINT ( 'NONE',  ( 9.883915020958999875, -5.811247906278000031, -7.978055797018001272 ) ) ;
#62627 = TOROIDAL_SURFACE ( 'NONE', #54807, 8.250000000000000000, 1.000000000000000000 ) ;
#62628 = CARTESIAN_POINT ( 'NONE',  ( 10.28026357027499849, 4.985299147223100746, -7.690095141806899903 ) ) ;
#62629 = CYLINDRICAL_SURFACE ( 'NONE', #46226, 1.350000000000000533 ) ;
#62630 = CARTESIAN_POINT ( 'NONE',  ( 9.978904719591000116, 5.007782080444000528, -8.772599239991000886 ) ) ;
#62631 = CARTESIAN_POINT ( 'NONE',  ( 9.098721904869998767, 5.115452802765999785, -8.126218358304999612 ) ) ;
#62633 = CARTESIAN_POINT ( 'NONE',  ( 12.80505043854143388, 1.875000000000000000, 12.57541666120756041 ) ) ;
#62632 = CARTESIAN_POINT ( 'NONE',  ( 10.16966711471859952, 2.650353857333680896, 7.590422934968386492 ) ) ;
#62634 = CARTESIAN_POINT ( 'NONE',  ( 11.30000285318000230, -11.76356368987999979, -1.428410073821000159 ) ) ;
#62635 = ORIENTED_EDGE ( 'NONE', *, *, #51447, .F. ) ;
#62636 = AXIS2_PLACEMENT_3D ( 'NONE', #39666, #66567, #50843 ) ;
#62637 = CARTESIAN_POINT ( 'NONE',  ( 1.700000811628999964, 0.000000000000000000, 0.000000000000000000 ) ) ;
#62638 = DIRECTION ( 'NONE',  ( 1.000000000000000000, 0.000000000000000000, 0.000000000000000000 ) ) ;
#62639 = CARTESIAN_POINT ( 'NONE',  ( 10.06844525594999951, -4.148609764890999863, 8.941457795715999524 ) ) ;
#62640 = CARTESIAN_POINT ( 'NONE',  ( 8.945797255587999430, 5.003512473869000665, 7.542485555928779561 ) ) ;
#62641 = CARTESIAN_POINT ( 'NONE',  ( 8.973608660036624940, 4.220957842099207546, -6.653412791890684019 ) ) ;
#62642 = EDGE_CURVE ( 'NONE', #68200, #10649, #55850, .T. ) ;
#62643 = EDGE_CURVE ( 'NONE', #25251, #64076, #33904, .T. ) ;
#62644 = AXIS2_PLACEMENT_3D ( 'NONE', #43449, #12319, #60558 ) ;
#62645 = DIRECTION ( 'NONE',  ( 1.000000000000000000, 0.000000000000000000, 0.000000000000000000 ) ) ;
#62646 = CARTESIAN_POINT ( 'NONE',  ( 12.29043182814385560, -2.854820394136933004, 13.59177665069740470 ) ) ;
#62647 = CARTESIAN_POINT ( 'NONE',  ( 12.18947262544869048, 2.391368178646923415, 13.69585133611195005 ) ) ;
#62648 = CARTESIAN_POINT ( 'NONE',  ( 23.51706216425600360, 2.929165934761999601, -13.82547941210000175 ) ) ;
#62649 = EDGE_LOOP ( 'NONE', ( #62273, #52881, #9595, #60054, #56529, #7314 ) ) ;
#62650 = EDGE_CURVE ( 'NONE', #28311, #7747, #18334, .T. ) ;
#62651 = ADVANCED_FACE ( 'NONE', ( #3783 ), #63919, .F. ) ;
#62652 = B_SPLINE_CURVE_WITH_KNOTS ( 'NONE', 3,
 ( #53926, #52903, #6026, #22109, #21418, #42416, #63722, #37165, #58485, #17918 ),
 .UNSPECIFIED., .F., .F.,
 ( 4, 2, 2, 2, 4 ),
 ( 0.5007402250167770630, 0.6255551687625827695, 0.7503701125083885870, 0.8751850562541942935, 1.000000000000000000 ),
 .UNSPECIFIED. ) ;
#62653 = CARTESIAN_POINT ( 'NONE',  ( 4.661160569768000528, 0.5205051299898000305, 1.007958462633000041 ) ) ;
#62654 = CARTESIAN_POINT ( 'NONE',  ( 9.377342523874999003, -5.264483068122999931, -7.306436165809000016 ) ) ;
#62655 = CARTESIAN_POINT ( 'NONE',  ( 10.42787890655380600, -4.833579956562179980, -4.974657529990448523 ) ) ;
#62656 = CARTESIAN_POINT ( 'NONE',  ( 11.35679632507500081, -3.509334349252600127, 6.590394082213600235 ) ) ;
#62657 = CARTESIAN_POINT ( 'NONE',  ( 17.81328364446394019, 1.807903055951886273, -12.46962321666120665 ) ) ;
#62658 = CARTESIAN_POINT ( 'NONE',  ( 10.86297706979999944, -2.934528160336999925, 5.173578227060000145 ) ) ;
#62659 = CARTESIAN_POINT ( 'NONE',  ( 8.763353253171903390, -4.132446745988498371, -8.413353309630901222 ) ) ;
#62660 = CARTESIAN_POINT ( 'NONE',  ( 12.32889761174196863, 2.904977411718398184, -13.57918629439654978 ) ) ;
#62661 = CARTESIAN_POINT ( 'NONE',  ( 11.13224602605999891, -2.668757901739000182, -5.057295448712999963 ) ) ;
#62662 = CARTESIAN_POINT ( 'NONE',  ( 9.900941392955999731, -4.883847137081999357, -9.070879136699002032 ) ) ;
#62663 = DIRECTION ( 'NONE',  ( -1.000000000000000000, -3.552713678992000385E-14, 7.105427357983999508E-14 ) ) ;
#62664 = CARTESIAN_POINT ( 'NONE',  ( 12.33591485593542281, 0.5568603909045817257, -13.98892293345220139 ) ) ;
#62665 = CARTESIAN_POINT ( 'NONE',  ( 13.55266668291200105, -9.123246021508000680, -7.477861434740999513 ) ) ;
#62666 = CARTESIAN_POINT ( 'NONE',  ( 9.188234083221837878, -2.648243641808896598, 7.263637137173924785 ) ) ;
#62667 = CARTESIAN_POINT ( 'NONE',  ( 18.15926133226627925, 2.338854968114922883, 12.48766092794227589 ) ) ;
#62668 = EDGE_CURVE ( 'NONE', #29897, #22158, #30826, .T. ) ;
#62669 = CARTESIAN_POINT ( 'NONE',  ( 9.251970280414001380, 5.673443217382001080, -7.051790060464000476 ) ) ;
#62670 = CARTESIAN_POINT ( 'NONE',  ( 10.22514748322308797, 2.649941783575544108, 7.500008211948054893 ) ) ;
#62671 = VERTEX_POINT ( 'NONE', #14299 ) ;
#62672 = CARTESIAN_POINT ( 'NONE',  ( 8.434805295391802460, -5.349284795551668914, 7.676787393164613782 ) ) ;
#62673 = CARTESIAN_POINT ( 'NONE',  ( 18.19085350567997139, 2.166991405623370337, -13.83127841112310996 ) ) ;
#62674 = ORIENTED_EDGE ( 'NONE', *, *, #8449, .F. ) ;
#62675 = CARTESIAN_POINT ( 'NONE',  ( 10.49127973160899963, -3.922199073804859992, 8.363513150096299142 ) ) ;
#62676 = CARTESIAN_POINT ( 'NONE',  ( 9.099999931440999390, -2.750000000000000000, -7.500000000000000000 ) ) ;
#62677 = CARTESIAN_POINT ( 'NONE',  ( 9.193385841233000733, 2.981992329588000423, -5.895876591910999664 ) ) ;
#62678 = CARTESIAN_POINT ( 'NONE',  ( 11.39393020684959978, -5.250000000000000000, 7.500000000000000000 ) ) ;
#62679 = CARTESIAN_POINT ( 'NONE',  ( 10.52435971519499880, -3.467537960339900138, -6.614211617270199461 ) ) ;
#62680 = CARTESIAN_POINT ( 'NONE',  ( 24.53428993882599940, 8.855929947951999281, -9.286429770520999938 ) ) ;
#62681 = CARTESIAN_POINT ( 'NONE',  ( 12.80505043854143388, 1.875000000000000000, 12.57541666120756041 ) ) ;
#62682 = ORIENTED_EDGE ( 'NONE', *, *, #39147, .T. ) ;
#62683 = CARTESIAN_POINT ( 'NONE',  ( 10.06927318630900103, 4.756452637475338641, -8.526145288591964189 ) ) ;
#62684 = CARTESIAN_POINT ( 'NONE',  ( 8.938854719593997800, 5.597201461420000967, -8.171008079894999554 ) ) ;
#62685 = VERTEX_POINT ( 'NONE', #35954 ) ;
#62686 = CARTESIAN_POINT ( 'NONE',  ( 10.32702465212000043, 5.663794543395000325, -6.682030833630000721 ) ) ;
#62687 = ORIENTED_EDGE ( 'NONE', *, *, #63908, .F. ) ;
#62688 = CARTESIAN_POINT ( 'NONE',  ( 9.858596320338998353, 2.815618218644000414, 7.983346856269500691 ) ) ;
#62689 = CARTESIAN_POINT ( 'NONE',  ( 17.57591033989428908, -1.875000590519982246, -12.57541652832150447 ) ) ;
#62690 = EDGE_CURVE ( 'NONE', #58563, #16266, #29018, .T. ) ;
#62691 = DIRECTION ( 'NONE',  ( 1.000000000000000000, 0.000000000000000000, 0.000000000000000000 ) ) ;
#62692 = VECTOR ( 'NONE', #53922, 1000.000000000000000 ) ;
#62693 = EDGE_CURVE ( 'NONE', #41892, #46269, #35786, .T. ) ;
#62694 = CARTESIAN_POINT ( 'NONE',  ( 24.50549018585800098, -12.34681877080999968, -3.084981659446000002 ) ) ;
#62695 = CARTESIAN_POINT ( 'NONE',  ( 23.60000000000000142, 0.000000000000000000, 0.000000000000000000 ) ) ;
#62696 = VERTEX_POINT ( 'NONE', #40856 ) ;
#62697 = CARTESIAN_POINT ( 'NONE',  ( 24.45617574099272673, 3.500160185366723908, -12.27858218217408925 ) ) ;
#62698 = CARTESIAN_POINT ( 'NONE',  ( 11.22023584123000006, 3.883089684441999978, -8.854806321849000739 ) ) ;
#62699 = LINE ( 'NONE', #57804, #20712 ) ;
#62700 = DIRECTION ( 'NONE',  ( 1.000000000000000000, 0.000000000000000000, 0.000000000000000000 ) ) ;
#62701 = CARTESIAN_POINT ( 'NONE',  ( 17.57900089668073917, 0.7302151644511168938, 13.98094363559787823 ) ) ;
#62702 = CARTESIAN_POINT ( 'NONE',  ( 18.07439970769999960, 3.110573872314000177, 11.47478625844000177 ) ) ;
#62703 = AXIS2_PLACEMENT_3D ( 'NONE', #3545, #3214, #30144 ) ;
#62704 = CARTESIAN_POINT ( 'NONE',  ( 11.06133683778999988, -2.503914237677999921, -6.712780725818999983 ) ) ;
#62705 = ORIENTED_EDGE ( 'NONE', *, *, #23940, .F. ) ;
#62706 = VERTEX_POINT ( 'NONE', #23748 ) ;
#62707 = CARTESIAN_POINT ( 'NONE',  ( 9.120035841232999374, 5.288433695693000480, -8.041290150997999930 ) ) ;
#62708 = CYLINDRICAL_SURFACE ( 'NONE', #22112, 0.5000000000000004441 ) ;
#62709 = CARTESIAN_POINT ( 'NONE',  ( 12.64149076266971328, -3.109019952252448871, 13.52530492583600541 ) ) ;
#62710 = CARTESIAN_POINT ( 'NONE',  ( 25.36443153939400119, 8.489939778973999651, -7.945402963458000123 ) ) ;
#62711 = CARTESIAN_POINT ( 'NONE',  ( 23.54917043075800009, 10.40012418511999925, -9.429198771629000220 ) ) ;
#62712 = CARTESIAN_POINT ( 'NONE',  ( 9.028772138681999238, 3.677371150249499898, -6.695252480703800302 ) ) ;
#62714 = DIRECTION ( 'NONE',  ( 0.000000000000000000, -0.1218274111675001492, -0.9925512993736016476 ) ) ;
#62713 = CARTESIAN_POINT ( 'NONE',  ( 9.851063610504999346, -3.588011994494999968, 6.583971515917899531 ) ) ;
#62715 = CARTESIAN_POINT ( 'NONE',  ( 21.59999946634000167, -13.89999946622000060, -2.316958215196000280E-09 ) ) ;
#62716 = EDGE_LOOP ( 'NONE', ( #54742, #31705, #45296, #56762 ) ) ;
#62717 = DIRECTION ( 'NONE',  ( 0.000000000000000000, 0.3352635608502960163, 0.9421243786071880066 ) ) ;
#62718 = CARTESIAN_POINT ( 'NONE',  ( 8.205380712518003605, -3.106081630192000009, 6.107045428706002532 ) ) ;
#62719 = CARTESIAN_POINT ( 'NONE',  ( 10.19095058442699830, 4.507735863714500191, 8.674133161175999973 ) ) ;
#62720 = CARTESIAN_POINT ( 'NONE',  ( 6.949659606017999813, -12.16386295504999993, -3.090546161407999648 ) ) ;
#62721 = CARTESIAN_POINT ( 'NONE',  ( 18.18005043873318982, -2.501166356684528580, -12.45128845098599335 ) ) ;
#62722 = DIRECTION ( 'NONE',  ( 1.000000000000000000, 0.000000000000000000, 0.000000000000000000 ) ) ;
#62723 = CARTESIAN_POINT ( 'NONE',  ( 8.745860841232000027, 4.178200486578000472, -5.608493638783999202 ) ) ;
#62724 = EDGE_CURVE ( 'NONE', #27484, #10323, #50771, .T. ) ;
#62725 = EDGE_CURVE ( 'NONE', #5638, #26310, #38242, .T. ) ;
#62726 = CARTESIAN_POINT ( 'NONE',  ( 15.83777337640989202, -9.021763928136902422, -8.400065602738662207 ) ) ;
#62727 = CARTESIAN_POINT ( 'NONE',  ( 16.13125657744143737, -3.735736757528830054, -11.95504925864019441 ) ) ;
#62728 = VECTOR ( 'NONE', #15887, 999.9999999999998863 ) ;
#62729 = CARTESIAN_POINT ( 'NONE',  ( 10.86501009699205866, -2.649983380499685737, -7.500000587580680111 ) ) ;
#62730 = CARTESIAN_POINT ( 'NONE',  ( 0.3209986693645116018, -1.671708792466147120, 2.902155973540134326 ) ) ;
#62731 = DIRECTION ( 'NONE',  ( 0.7071065576627081350, 0.000000000000000000, -0.7071070047103161782 ) ) ;
#62732 = CARTESIAN_POINT ( 'NONE',  ( 9.870826602350810219, 2.650039321431383765, -7.402527530260877953 ) ) ;
#62733 = ORIENTED_EDGE ( 'NONE', *, *, #16717, .T. ) ;
#62734 = CARTESIAN_POINT ( 'NONE',  ( 12.40062372901866894, -0.4766234715920634746, -12.68796191786314154 ) ) ;
#62735 = CARTESIAN_POINT ( 'NONE',  ( 12.18124154974851336, -2.460017072494863122, -12.46078795777972736 ) ) ;
#62736 = LINE ( 'NONE', #8581, #34265 ) ;
#62737 = DIRECTION ( 'NONE',  ( 0.000000000000000000, -1.000000000000000000, 0.000000000000000000 ) ) ;
#62738 = CARTESIAN_POINT ( 'NONE',  ( 1.571806799207417393, 3.408904368339104263, 0.9161175952574878156 ) ) ;
#62739 = ORIENTED_EDGE ( 'NONE', *, *, #50752, .T. ) ;
#62740 = DIRECTION ( 'NONE',  ( -0.1522489053782972723, 0.9525130357304880668, -0.2637028395269958025 ) ) ;
#62741 = PRODUCT_CONTEXT ( 'NONE', #42282, 'mechanical' ) ;
#62742 = CARTESIAN_POINT ( 'NONE',  ( 10.96620111615414928, 8.758729369432925793, 6.500226485814697419 ) ) ;
#62743 = EDGE_CURVE ( 'NONE', #15849, #24516, #46794, .T. ) ;
#62744 = CARTESIAN_POINT ( 'NONE',  ( 10.35434687351662575, -5.250000000000000000, 7.336375382625534236 ) ) ;
#62745 = CARTESIAN_POINT ( 'NONE',  ( 1.709306799206499861, -3.058252359239909790, 1.762666431298136382 ) ) ;
#62747 = AXIS2_PLACEMENT_3D ( 'NONE', #17935, #66161, #33324 ) ;
#62746 = CARTESIAN_POINT ( 'NONE',  ( 11.01790547754519878, 5.174295865741999734, -7.537269019642879542 ) ) ;
#62748 = ORIENTED_EDGE ( 'NONE', *, *, #29004, .F. ) ;
#62749 = CARTESIAN_POINT ( 'NONE',  ( 10.20319453770999907, -3.421758889707999796, 6.017729046583999875 ) ) ;
#62750 = VERTEX_POINT ( 'NONE', #30714 ) ;
#62751 = CARTESIAN_POINT ( 'NONE',  ( 11.86486084871759950, -5.207010770456999893, 7.174999999999999822 ) ) ;
#62752 = CARTESIAN_POINT ( 'NONE',  ( 9.368918146792999835, -5.618388245857000030, 7.727743016644000207 ) ) ;
#62753 = CONICAL_SURFACE ( 'NONE', #11399, 0.8999999993279991228, 0.7853981633972997312 ) ;
#62754 = CARTESIAN_POINT ( 'NONE',  ( 15.95192027319500205, 8.515023616297000331, 8.165096030563999463 ) ) ;
#62755 = EDGE_LOOP ( 'NONE', ( #3029, #2717, #44422, #15649 ) ) ;
#62756 = CARTESIAN_POINT ( 'NONE',  ( 8.427194650706185897, 4.807287621755191864, -9.060105673721203345 ) ) ;
#62757 = CARTESIAN_POINT ( 'NONE',  ( 11.10000057264999995, 0.4999994248636999705, 9.776630284457000997 ) ) ;
#62758 = CARTESIAN_POINT ( 'NONE',  ( 6.645739158770999744, 5.086541985415000688, -8.378805615758999181 ) ) ;
#62759 = CARTESIAN_POINT ( 'NONE',  ( 11.00000000000000000, 4.991767524623399233, 7.825000000000000178 ) ) ;
#62760 = CARTESIAN_POINT ( 'NONE',  ( 18.12484680923011382, -2.757022365768678096, 12.38798834872858556 ) ) ;
#62761 = ORIENTED_EDGE ( 'NONE', *, *, #11992, .T. ) ;
#62762 = CARTESIAN_POINT ( 'NONE',  ( 2.240556799207291672, -3.500000000000003109, 0.4581489286484972667 ) ) ;
#62763 = CARTESIAN_POINT ( 'NONE',  ( 12.21587634999234595, -2.708625115319929666, -13.62694294269819117 ) ) ;
#62764 = CARTESIAN_POINT ( 'NONE',  ( 9.575651506909606425, -2.765563590215046830, 7.432209138388947700 ) ) ;
#62765 = ORIENTED_EDGE ( 'NONE', *, *, #44146, .T. ) ;
#62766 = CARTESIAN_POINT ( 'NONE',  ( 10.99693800072000016, -2.980603239157999962, -6.418614998350999912 ) ) ;
#62767 = CARTESIAN_POINT ( 'NONE',  ( 8.316694475082000437, 2.898380349184999982, 6.611503672649000407 ) ) ;
#62768 = ORIENTED_EDGE ( 'NONE', *, *, #49221, .T. ) ;
#62769 = CARTESIAN_POINT ( 'NONE',  ( 17.55505043854144276, 0.6250000000000001110, -13.88107975066922428 ) ) ;
#62770 = CARTESIAN_POINT ( 'NONE',  ( 17.59627748481874221, -0.6237239846186468650, -12.67937377942301502 ) ) ;
#62771 = CARTESIAN_POINT ( 'NONE',  ( 8.687922088694000067, 3.419384128876999718, -5.860036257779999147 ) ) ;
#62772 = FACE_OUTER_BOUND ( 'NONE', #9113, .T. ) ;
#62773 = CARTESIAN_POINT ( 'NONE',  ( 11.09999999999999964, 4.000000000000000000, 7.500000000000000000 ) ) ;
#62774 = EDGE_CURVE ( 'NONE', #52369, #16060, #48280, .T. ) ;
#62775 = CARTESIAN_POINT ( 'NONE',  ( 12.33367687689867687, 2.910531109056639032, 13.57771726184491357 ) ) ;
#62776 = CARTESIAN_POINT ( 'NONE',  ( 18.39984528086700166, 2.531308496144999716E-14, 2.131628207279999844E-14 ) ) ;
#62777 = ORIENTED_EDGE ( 'NONE', *, *, #35203, .T. ) ;
#62778 = CARTESIAN_POINT ( 'NONE',  ( 7.810726116476000236, -5.086048788582002267, 6.527219528731996512 ) ) ;
#62779 = B_SPLINE_CURVE_WITH_KNOTS ( 'NONE', 3,
 ( #29440, #44821, #45840, #2843 ),
 .UNSPECIFIED., .F., .F.,
 ( 4, 4 ),
 ( 0.000000000000000000, 1.000000000000000000 ),
 .UNSPECIFIED. ) ;
#62780 = ORIENTED_EDGE ( 'NONE', *, *, #16417, .T. ) ;
#62781 = CARTESIAN_POINT ( 'NONE',  ( 10.40516904918000129, 5.216391323504000255, 6.765759859247999941 ) ) ;
#62782 = CARTESIAN_POINT ( 'NONE',  ( 11.27531844363630320, -3.660964894626073107, -8.308695084076106241 ) ) ;
#62783 = CARTESIAN_POINT ( 'NONE',  ( 12.54469325725303541, 1.931433442391065070, -13.77773667378076361 ) ) ;
#62784 = CARTESIAN_POINT ( 'NONE',  ( 2.432838064400999922, 1.445961631832999972, -3.231775658717000344 ) ) ;
#62785 = B_SPLINE_CURVE_WITH_KNOTS ( 'NONE', 3,
 ( #21950, #54115, #17408, #11460 ),
 .UNSPECIFIED., .F., .F.,
 ( 4, 4 ),
 ( 0.000000000000000000, 1.000000000000000000 ),
 .UNSPECIFIED. ) ;
#62786 = CARTESIAN_POINT ( 'NONE',  ( 9.856713838269000050, -4.814118338972999567, -8.929571672388000536 ) ) ;
#62787 = LINE ( 'NONE', #14228, #32804 ) ;
#62788 = CARTESIAN_POINT ( 'NONE',  ( 9.316610756102749136, -5.674809202490012083, -6.995745383024254416 ) ) ;
#62789 = VERTEX_POINT ( 'NONE', #52024 ) ;
#62790 = CARTESIAN_POINT ( 'NONE',  ( 12.15456516821461008, -3.197083038490000195, 6.689681884064299311 ) ) ;
#62791 = CARTESIAN_POINT ( 'NONE',  ( 11.09999999999999964, 4.000000000000000000, -7.500000000000000000 ) ) ;
#62792 = LINE ( 'NONE', #19815, #46051 ) ;
#62793 = LINE ( 'NONE', #25400, #7546 ) ;
#62795 = LINE ( 'NONE', #8639, #1608 ) ;
#62794 = CARTESIAN_POINT ( 'NONE',  ( 10.06344080699000010, 5.156228702401000952, 6.125219923432000613 ) ) ;
#62796 = CIRCLE ( 'NONE', #25984, 1.099999999999999867 ) ;
#62797 = CARTESIAN_POINT ( 'NONE',  ( 10.21462282008599942, 4.523146351753199568, -8.343818446627699004 ) ) ;
#62798 = DIRECTION ( 'NONE',  ( 0.000000000000000000, -0.9553735099700839672, -0.2954005017724949389 ) ) ;
#62799 = CARTESIAN_POINT ( 'NONE',  ( 9.425038493598998812, 4.627468580434300094, -6.901676404381399621 ) ) ;
#62800 = B_SPLINE_CURVE_WITH_KNOTS ( 'NONE', 3,
 ( #67236, #3273, #42059, #20384 ),
 .UNSPECIFIED., .F., .F.,
 ( 4, 4 ),
 ( 0.000000000000000000, 1.000000000000000000 ),
 .UNSPECIFIED. ) ;
#62801 = B_SPLINE_CURVE_WITH_KNOTS ( 'NONE', 3,
 ( #12976, #56647, #46158, #67462 ),
 .UNSPECIFIED., .F., .F.,
 ( 4, 4 ),
 ( 0.000000000000000000, 1.000000000000000000 ),
 .UNSPECIFIED. ) ;
#62802 = CARTESIAN_POINT ( 'NONE',  ( 17.90798944145350902, 0.6284163952874703973, 12.58432055988358123 ) ) ;
#62803 = CARTESIAN_POINT ( 'NONE',  ( 7.193698479222000230, -0.8911225501965001072, 0.9093353740403999907 ) ) ;
#62804 = CARTESIAN_POINT ( 'NONE',  ( 24.45625628206627766, -8.883598553532051412, 9.170492330253466662 ) ) ;
#62805 = CARTESIAN_POINT ( 'NONE',  ( 23.85182611390700202, 9.643708492127998966, 9.632179236076000350 ) ) ;
#62806 = ORIENTED_EDGE ( 'NONE', *, *, #8279, .T. ) ;
#62807 = CARTESIAN_POINT ( 'NONE',  ( 7.127706853208000126, -4.698358408974000255, 8.789434435623999065 ) ) ;
#62808 = EDGE_CURVE ( 'NONE', #44937, #5174, #26626, .T. ) ;
#62809 = ADVANCED_FACE ( 'NONE', ( #42577 ), #53069, .T. ) ;
#62810 = CARTESIAN_POINT ( 'NONE',  ( 17.77834352330034307, 3.212755074437993130, 13.62637949436378015 ) ) ;
#62811 = DIRECTION ( 'NONE',  ( -0.000000000000000000, 0.9659258262890756397, 0.2588190451024934280 ) ) ;
#62812 = ORIENTED_EDGE ( 'NONE', *, *, #63517, .T. ) ;
#62813 = CARTESIAN_POINT ( 'NONE',  ( 18.30830001818700126, 3.300182612895000478, 12.02694835946000040 ) ) ;
#62814 = CARTESIAN_POINT ( 'NONE',  ( 11.30878751119029957, 2.958974835389999836, 6.955365841266999638 ) ) ;
#62815 = CARTESIAN_POINT ( 'NONE',  ( 10.58470471959000037, 2.966809777448999874, -8.831980808885999679 ) ) ;
#62816 = ORIENTED_EDGE ( 'NONE', *, *, #36972, .F. ) ;
#62817 = CARTESIAN_POINT ( 'NONE',  ( 1.300973465874000201, -3.500000000000000000, 0.000000000000000000 ) ) ;
#62818 = CARTESIAN_POINT ( 'NONE',  ( 24.84557120767344429, -8.580242956840624657, 9.011385558522297501 ) ) ;
#62819 = CARTESIAN_POINT ( 'NONE',  ( 10.64118447801629941, 5.277702140407999565, 7.528171279442569919 ) ) ;
#62820 = CARTESIAN_POINT ( 'NONE',  ( 13.99999999485600277, -9.471999751521998689, -8.194948195317001804 ) ) ;
#62821 = CARTESIAN_POINT ( 'NONE',  ( 8.785198341231000185, 5.414918126383000185, 8.890678916765999418 ) ) ;
#62822 = VERTEX_POINT ( 'NONE', #26501 ) ;
#62823 = CARTESIAN_POINT ( 'NONE',  ( 25.37955899411765159, -11.36924665038260329, -3.069077516866383082 ) ) ;
#62824 = CARTESIAN_POINT ( 'NONE',  ( 7.119364158768999751, 2.502464354543000091, -6.330838737160999763 ) ) ;
#62825 = EDGE_CURVE ( 'NONE', #68596, #7028, #25461, .T. ) ;
#62826 = CARTESIAN_POINT ( 'NONE',  ( 8.255343399658274350, -5.333771483169611471, 8.616868296190860477 ) ) ;
#62827 = CARTESIAN_POINT ( 'NONE',  ( 10.05464655415100061, -3.380689388027600106, 6.380697202105999999 ) ) ;
#62828 = ORIENTED_EDGE ( 'NONE', *, *, #52081, .T. ) ;
#62829 = CARTESIAN_POINT ( 'NONE',  ( 10.36332605023000042, -4.728604826508999714, -4.865787476787999388 ) ) ;
#62830 = CARTESIAN_POINT ( 'NONE',  ( 10.74733997688000109, -3.727636250918499705, 8.748653021963999521 ) ) ;
#62831 = ORIENTED_EDGE ( 'NONE', *, *, #32832, .T. ) ;
#62832 = ADVANCED_FACE ( 'NONE', ( #63192 ), #2922, .T. ) ;
#62833 = CARTESIAN_POINT ( 'NONE',  ( 8.810863317747999801, 4.960863370448500120, -7.500000000073117512 ) ) ;
#62834 = ORIENTED_EDGE ( 'NONE', *, *, #56040, .T. ) ;
#62835 = VECTOR ( 'NONE', #23864, 1000.000000000000000 ) ;
#62836 = FACE_OUTER_BOUND ( 'NONE', #55087, .T. ) ;
#62837 = CARTESIAN_POINT ( 'NONE',  ( 2.530140132543583498, 3.408904368339106483, -0.9161175952574748260 ) ) ;
#62838 = CARTESIAN_POINT ( 'NONE',  ( 11.76588784977539781, 2.879134238109999799, -7.435950347916509884 ) ) ;
#62839 = CARTESIAN_POINT ( 'NONE',  ( 11.47635090131019986, -3.000792947412299849, 6.881982988766500497 ) ) ;
#62840 = FACE_OUTER_BOUND ( 'NONE', #26051, .T. ) ;
#62841 = CARTESIAN_POINT ( 'NONE',  ( 11.51456785386839954, -4.946394603182100447, 6.863111178199799767 ) ) ;
#62842 = DIRECTION ( 'NONE',  ( -0.000000000000000000, 0.9127899773906427150, 0.4084292560226189250 ) ) ;
#62843 = ORIENTED_EDGE ( 'NONE', *, *, #29143, .F. ) ;
#62844 = CARTESIAN_POINT ( 'NONE',  ( 16.39999999379500295, -3.351248059343999941, -11.15756683833000018 ) ) ;
#62845 = STYLED_ITEM ( 'NONE', ( #37314 ), #29488 ) ;
#62846 = CARTESIAN_POINT ( 'NONE',  ( 8.674245559624999657, -5.983034890242000081, 7.440798487724999966 ) ) ;
#62847 = CARTESIAN_POINT ( 'NONE',  ( 11.79999999771000141, 3.595163221087000149, -11.99793848941000007 ) ) ;
#62848 = ORIENTED_EDGE ( 'NONE', *, *, #47275, .F. ) ;
#62849 = CARTESIAN_POINT ( 'NONE',  ( 12.78086743291011551, -1.761210985583074207, -12.47630298729255216 ) ) ;
#62850 = CARTESIAN_POINT ( 'NONE',  ( 11.37964291764649971, 2.731641218595000087, 7.656787697937099679 ) ) ;
#62851 = CARTESIAN_POINT ( 'NONE',  ( 10.71315564678999976, -2.619204038425999581, -8.142086897834001746 ) ) ;
#62852 = CARTESIAN_POINT ( 'NONE',  ( 7.946130483458992977, 8.084765295500995208, -4.735587142431003649 ) ) ;
#62853 = CARTESIAN_POINT ( 'NONE',  ( 17.76900185986900027, -3.411877013825000304, -11.89794217324999970 ) ) ;
#62854 = CARTESIAN_POINT ( 'NONE',  ( 10.74809687351632448, 4.327184855449106138, 8.717465845835393523 ) ) ;
#62855 = CARTESIAN_POINT ( 'NONE',  ( 12.40968101568429383, -3.130119464836099485, -13.64559997174500872 ) ) ;
#62856 = CARTESIAN_POINT ( 'NONE',  ( 11.26487482311540056, -3.069598554678400149, -7.875904247640098887 ) ) ;
#62857 = CARTESIAN_POINT ( 'NONE',  ( 11.39975833414730033, 4.796537143354000499, -7.174999999999999822 ) ) ;
#62858 = DIRECTION ( 'NONE',  ( -1.000000000000000000, 0.000000000000000000, 0.000000000000000000 ) ) ;
#62859 = ORIENTED_EDGE ( 'NONE', *, *, #17890, .T. ) ;
#62860 = ORIENTED_EDGE ( 'NONE', *, *, #26944, .T. ) ;
#62861 = CARTESIAN_POINT ( 'NONE',  ( 12.61475641025121774, -0.7110419930699988234, -13.98197980709423760 ) ) ;
#62862 = DIRECTION ( 'NONE',  ( 0.000000000000000000, 0.000000000000000000, 1.000000000000000000 ) ) ;
#62863 = DIRECTION ( 'NONE',  ( -1.000000000000000000, 0.000000000000000000, 0.000000000000000000 ) ) ;
#62864 = CARTESIAN_POINT ( 'NONE',  ( 12.08457173739308388, -3.062774903199518839, 6.638117766810081477 ) ) ;
#62865 = CARTESIAN_POINT ( 'NONE',  ( 10.55068356942999941, 2.412177153420000053, -6.919581319869999803 ) ) ;
#62866 = DIRECTION ( 'NONE',  ( -0.8660254037844289376, 0.000000000000000000, 0.5000000000000169864 ) ) ;
#62867 = CARTESIAN_POINT ( 'NONE',  ( 17.69900574642232272, 3.108543425041114805, 12.28872856983837458 ) ) ;
#62868 = CARTESIAN_POINT ( 'NONE',  ( 18.12310803393399894, 3.320912951897000198, -11.92519506916999994 ) ) ;
#62869 = CARTESIAN_POINT ( 'NONE',  ( 10.80815748598999981, 2.937526572573000205, 8.948458885032000154 ) ) ;
#62870 = ORIENTED_EDGE ( 'NONE', *, *, #63984, .T. ) ;
#62871 = CARTESIAN_POINT ( 'NONE',  ( 8.798416552063660134, 5.540558544858231294, -6.616773852782482201 ) ) ;
#62872 = ORIENTED_EDGE ( 'NONE', *, *, #31105, .F. ) ;
#62873 = CARTESIAN_POINT ( 'NONE',  ( 12.42229329081243705, -2.994506204212080469, 12.32251488760203628 ) ) ;
#62874 = CARTESIAN_POINT ( 'NONE',  ( 23.56665676678100141, -10.37811504717999966, -9.381458738969000066 ) ) ;
#62875 = CARTESIAN_POINT ( 'NONE',  ( 9.298033738970000073, 4.087077023028999001, 9.429414864145000408 ) ) ;
#62876 = CARTESIAN_POINT ( 'NONE',  ( 11.01414141025500015, -3.384226587288500010, 6.403245959303999868 ) ) ;
#62877 = DIRECTION ( 'NONE',  ( 0.000000000000000000, 1.000000000000000000, 0.000000000000000000 ) ) ;
#62878 = CIRCLE ( 'NONE', #52862, 12.35000000006999876 ) ;
#62879 = CARTESIAN_POINT ( 'NONE',  ( 25.59994555223599733, 8.527741194213000142, 7.260611644044000279 ) ) ;
#62880 = CARTESIAN_POINT ( 'NONE',  ( 24.56892835520400098, 8.742292411382999617, 8.862186445043999328 ) ) ;
#62881 = CARTESIAN_POINT ( 'NONE',  ( 12.54669586862715214, -0.5691963043021777136, 12.68282590392938047 ) ) ;
#62882 = CARTESIAN_POINT ( 'NONE',  ( 9.316114158771000575, 3.677414437776999723, 9.250745771096999803 ) ) ;
#62883 = CARTESIAN_POINT ( 'NONE',  ( 18.30003129332100187, -2.732683818840999646, -11.53064095373000164 ) ) ;
#62884 = CARTESIAN_POINT ( 'NONE',  ( 11.48831242699000121, -3.364143239851999923, 11.30418287150000012 ) ) ;
#62885 = ORIENTED_EDGE ( 'NONE', *, *, #28758, .F. ) ;
#62886 = CARTESIAN_POINT ( 'NONE',  ( 10.02394528041000044, 5.481267232667000222, -8.005061172455999241 ) ) ;
#62887 = DIRECTION ( 'NONE',  ( 1.000000000000000000, 0.000000000000000000, 0.000000000000000000 ) ) ;
#62888 = EDGE_CURVE ( 'NONE', #57184, #5900, #21249, .T. ) ;
#62889 = EDGE_CURVE ( 'NONE', #64076, #28965, #34927, .T. ) ;
#62890 = CARTESIAN_POINT ( 'NONE',  ( 10.95387080750653652, -2.254039244220492844, 7.421505705631724403 ) ) ;
#62891 = CARTESIAN_POINT ( 'NONE',  ( 14.39999999734000191, 11.41071763148134544, -4.623975354790890613 ) ) ;
#62892 = CARTESIAN_POINT ( 'NONE',  ( 12.09999999999999964, -2.820501972398000046, 7.825000000000000178 ) ) ;
#62893 = CARTESIAN_POINT ( 'NONE',  ( 11.50687348028854906, -5.003459210197000573, -8.042549288197099244 ) ) ;
#62894 = ORIENTED_EDGE ( 'NONE', *, *, #67081, .F. ) ;
#62895 = EDGE_CURVE ( 'NONE', #13607, #63587, #12971, .T. ) ;
#62896 = CARTESIAN_POINT ( 'NONE',  ( 1.629700767030000108, 0.9191385115525000371, 3.644662079466999938 ) ) ;
#62897 = CARTESIAN_POINT ( 'NONE',  ( 11.29998636608000062, -3.695122995756999984, 11.25914041192000070 ) ) ;
#62899 = CARTESIAN_POINT ( 'NONE',  ( 13.46395943152100116, -9.515552291263999152, -7.774702642439999423 ) ) ;
#62898 = CARTESIAN_POINT ( 'NONE',  ( 9.743692251747383182, 5.492527719313065937, 8.410238609252001396 ) ) ;
#62900 = CYLINDRICAL_SURFACE ( 'NONE', #21286, 1.350000000000000089 ) ;
#62901 = EDGE_LOOP ( 'NONE', ( #6520, #23632, #51251, #41224 ) ) ;
#62902 = DIRECTION ( 'NONE',  ( 0.000000000000000000, 0.000000000000000000, -1.000000000000000000 ) ) ;
#62903 = CARTESIAN_POINT ( 'NONE',  ( 17.99238080566778564, -2.053374525523686156, -13.75805324639250493 ) ) ;
#62904 = CARTESIAN_POINT ( 'NONE',  ( 11.04749144726329924, 3.499163784537000055, 8.206726025856399431 ) ) ;
#62905 = CARTESIAN_POINT ( 'NONE',  ( 24.94504657985486418, -11.54140607358216286, 3.218788503616806906 ) ) ;
#62906 = CARTESIAN_POINT ( 'NONE',  ( 7.239688980126000040, -4.389298280625000714, 9.135255728583000945 ) ) ;
#62907 = ORIENTED_EDGE ( 'NONE', *, *, #4656, .T. ) ;
#62908 = CARTESIAN_POINT ( 'NONE',  ( 7.283509992105000386, 4.426928431836000044, 9.293321981113999541 ) ) ;
#62910 = CARTESIAN_POINT ( 'NONE',  ( 10.41839555962000041, -4.531908721143000029, -9.270473926467998282 ) ) ;
#62909 = CARTESIAN_POINT ( 'NONE',  ( 10.98768472639999949, 0.3876847264043000174, 4.945212061661000469 ) ) ;
#62911 = CARTESIAN_POINT ( 'NONE',  ( 7.576990885774728568, -4.064377392965215385, 5.762023686569064829 ) ) ;
#62912 = CARTESIAN_POINT ( 'NONE',  ( 18.07980642413443917, -0.3396162601792407920, 13.89441893193904676 ) ) ;
#62913 = CARTESIAN_POINT ( 'NONE',  ( 23.83637964422599964, 3.383983541727000333, 13.10295583586000134 ) ) ;
#62914 = ORIENTED_EDGE ( 'NONE', *, *, #30478, .T. ) ;
#62915 = CARTESIAN_POINT ( 'NONE',  ( 2.096960091860043285, -2.086971693014386897, -2.559869209799199741 ) ) ;
#62916 = CARTESIAN_POINT ( 'NONE',  ( 11.35056919669530018, -3.169300617545700138, 7.254567470917099747 ) ) ;
#62917 = EDGE_CURVE ( 'NONE', #12815, #12021, #10068, .T. ) ;
#62918 = DIRECTION ( 'NONE',  ( 1.000000000000000000, 0.000000000000000000, 0.000000000000000000 ) ) ;
#62919 = CARTESIAN_POINT ( 'NONE',  ( 8.801820635884373800, -3.939853377893446584, -8.450403350428134175 ) ) ;
#62920 = CARTESIAN_POINT ( 'NONE',  ( 10.84226088462129844, 4.002427228022017225, 8.640738455926999961 ) ) ;
#62921 = CARTESIAN_POINT ( 'NONE',  ( 23.72389859521504007, -3.247326028998003267, 13.28501015257995910 ) ) ;
#62922 = CARTESIAN_POINT ( 'NONE',  ( 8.724024145839392119, -4.217522721361648408, -8.345440805164775711 ) ) ;
#62923 = LINE ( 'NONE', #9442, #55532 ) ;
#62924 = DIRECTION ( 'NONE',  ( 1.000000000000000000, 0.000000000000000000, 0.000000000000000000 ) ) ;
#62925 = AXIS2_PLACEMENT_3D ( 'NONE', #18098, #39073, #39417 ) ;
#62926 = CARTESIAN_POINT ( 'NONE',  ( 17.77845184731634021, -1.823244735605234812, 13.88077056497939843 ) ) ;
#62927 = CARTESIAN_POINT ( 'NONE',  ( 17.96066850193498965, 2.975608638399078743, -13.56100830560624360 ) ) ;
#62928 = EDGE_LOOP ( 'NONE', ( #23256, #19855, #2288, #35546 ) ) ;
#62929 = DIRECTION ( 'NONE',  ( 1.000000000000000000, 0.000000000000000000, 1.649474208015000260E-14 ) ) ;
#62930 = CARTESIAN_POINT ( 'NONE',  ( 9.201637546194751494, -3.727464796005204750, -6.269669426086102781 ) ) ;
#62931 = ORIENTED_EDGE ( 'NONE', *, *, #39815, .F. ) ;
#62932 = CARTESIAN_POINT ( 'NONE',  ( 11.61364291764652812, 3.140345330584100036, 7.606265891492399511 ) ) ;
#62933 = CARTESIAN_POINT ( 'NONE',  ( 10.68403803949000164, 5.436614310638000269, 8.578436083822998270 ) ) ;
#62934 = CARTESIAN_POINT ( 'NONE',  ( 10.55068356942999941, 2.412177153420000053, -6.919581319869999803 ) ) ;
#62935 = CARTESIAN_POINT ( 'NONE',  ( 9.556179045228626379, -4.616765641734932757, -6.879409626165266189 ) ) ;
#62936 = CARTESIAN_POINT ( 'NONE',  ( 10.89228096335999929, -3.998355205482000851, 9.261304730013998565 ) ) ;
#62937 = CARTESIAN_POINT ( 'NONE',  ( 18.25578817174764978, -0.1860047152749900456, -12.59864695008083046 ) ) ;
#62938 = CARTESIAN_POINT ( 'NONE',  ( 9.032940059871402028, 5.014669081864663980, 8.393627007547543428 ) ) ;
#62939 = CARTESIAN_POINT ( 'NONE',  ( 10.23103300763299828, -3.307558760216100069, -8.226274395107198600 ) ) ;
#62940 = CARTESIAN_POINT ( 'NONE',  ( 12.80505043854146940, -1.836948468694464820, 12.54242247073720051 ) ) ;
#62941 = ORIENTED_EDGE ( 'NONE', *, *, #27244, .F. ) ;
#62942 = FACE_OUTER_BOUND ( 'NONE', #17875, .T. ) ;
#62943 = CYLINDRICAL_SURFACE ( 'NONE', #45062, 2.000000000000000444 ) ;
#62944 = CARTESIAN_POINT ( 'NONE',  ( 10.35226354018316108, -5.092232985442820770, -6.870476274536370553 ) ) ;
#62945 = CARTESIAN_POINT ( 'NONE',  ( 10.91900351868999408, 8.255374249431000067, 7.037317811674005164 ) ) ;
#62946 = ADVANCED_FACE ( 'NONE', ( #9368 ), #15321, .T. ) ;
#62947 = CARTESIAN_POINT ( 'NONE',  ( 12.22832816813797585, 2.961039467707558437, 13.68329631872641095 ) ) ;
#62948 = ADVANCED_FACE ( 'NONE', ( #5851 ), #22279, .F. ) ;
#62949 = CARTESIAN_POINT ( 'NONE',  ( 10.41185831014999863, -2.101597930377999912, 7.856264717901999539 ) ) ;
#62950 = CARTESIAN_POINT ( 'NONE',  ( 12.44244977473554492, -0.5091670849982490310, -12.68626057781829175 ) ) ;
#62951 = AXIS2_PLACEMENT_3D ( 'NONE', #57075, #3583, #13412 ) ;
#62952 = CARTESIAN_POINT ( 'NONE',  ( 12.17712534909926880, -0.3652063536484373985, 13.99523956222174270 ) ) ;
#62953 = ORIENTED_EDGE ( 'NONE', *, *, #34544, .T. ) ;
#62954 = CARTESIAN_POINT ( 'NONE',  ( 12.75685216135446964, -1.762044409276920076, 12.47618552084819399 ) ) ;
#62955 = CARTESIAN_POINT ( 'NONE',  ( 8.814947692958833514, 2.650138447187985413, -7.499997389691697158 ) ) ;
#62956 = CARTESIAN_POINT ( 'NONE',  ( 9.228135700785001561, -2.875364528161000077, 8.669943154892999715 ) ) ;
#62957 = DIRECTION ( 'NONE',  ( -0.5000000000000150990, -0.08222066253632250021, 0.8621135439442261239 ) ) ;
#62958 = CARTESIAN_POINT ( 'NONE',  ( 10.88287885159599888, -3.139900861731399928, 7.602606670248799325 ) ) ;
#62959 = CARTESIAN_POINT ( 'NONE',  ( 12.75734966356159994, 0.7181168112306464124, 12.57951960855070261 ) ) ;
#62960 = DIRECTION ( 'NONE',  ( 1.000000000000000000, 0.000000000000000000, 0.000000000000000000 ) ) ;
#62961 = CARTESIAN_POINT ( 'NONE',  ( 11.15221028326116048, 3.091096528151293210, -7.175011397899978327 ) ) ;
#62962 = CARTESIAN_POINT ( 'NONE',  ( 12.41832178632828310, 1.871654022356042502, 12.46021467525213744 ) ) ;
#62963 = CARTESIAN_POINT ( 'NONE',  ( 9.971918425727000823, -4.365624317997999881, -9.242254741729000855 ) ) ;
#62964 = CARTESIAN_POINT ( 'NONE',  ( 11.28949010443639978, 5.000675062740000065, -7.574834962826040297 ) ) ;
#62965 = LINE ( 'NONE', #67533, #25809 ) ;
#62966 = EDGE_CURVE ( 'NONE', #50185, #49185, #32438, .T. ) ;
#62967 = CARTESIAN_POINT ( 'NONE',  ( 9.964039158770999549, 3.485905350467000119, -9.275749134703000109 ) ) ;
#62968 = CARTESIAN_POINT ( 'NONE',  ( 9.554646554150998838, 4.619310611972400338, -8.619302797893999113 ) ) ;
#62970 = CARTESIAN_POINT ( 'NONE',  ( 9.220712484379999907, -4.219532685969900498, 6.659501631675699862 ) ) ;
#62969 = CARTESIAN_POINT ( 'NONE',  ( 9.924988015501618577, 5.349815781279066762, 7.500001845592777272 ) ) ;
#62971 = CARTESIAN_POINT ( 'NONE',  ( 11.32299956498189886, -5.207010770456999893, -7.174999999999999822 ) ) ;
#62972 = EDGE_LOOP ( 'NONE', ( #12465, #41165 ) ) ;
#62973 = AXIS2_PLACEMENT_3D ( 'NONE', #33067, #21530, #26445 ) ;
#62974 = EDGE_CURVE ( 'NONE', #6526, #23153, #4062, .T. ) ;
#62975 = CARTESIAN_POINT ( 'NONE',  ( 12.38195926916771583, -0.4608195502960515388, 12.68876479730130313 ) ) ;
#62976 = CARTESIAN_POINT ( 'NONE',  ( 24.14474077035201915, -9.246824227896013326, 9.586721910999997931 ) ) ;
#62977 = DIRECTION ( 'NONE',  ( -1.000000000000000000, 0.000000000000000000, 0.000000000000000000 ) ) ;
#62978 = CARTESIAN_POINT ( 'NONE',  ( 9.779646554150998483, 4.419749732651400365, 6.741370903243699253 ) ) ;
#62979 = CARTESIAN_POINT ( 'NONE',  ( 21.59999987243000064, -1.749711486808999826E-13, -3.819167204710999825E-14 ) ) ;
#62980 = CARTESIAN_POINT ( 'NONE',  ( 12.39110436774228141, -2.968713941934962630, 13.56281002627122945 ) ) ;
#62981 = CARTESIAN_POINT ( 'NONE',  ( 12.28991563249832808, 2.854049639532288296, 13.59191281879116708 ) ) ;
#62982 = CARTESIAN_POINT ( 'NONE',  ( 8.191498566858999908, 3.399962487441000381, 6.146646668338000552 ) ) ;
#62983 = ORIENTED_EDGE ( 'NONE', *, *, #36301, .T. ) ;
#62984 = CARTESIAN_POINT ( 'NONE',  ( 4.284853625320999448, -0.9992745876934998606, 0.5369886066053000118 ) ) ;
#62985 = CARTESIAN_POINT ( 'NONE',  ( 9.959912909067998754, -4.809406943772300380, -8.490578012456198920 ) ) ;
#62986 = CARTESIAN_POINT ( 'NONE',  ( 10.48676300414402185, -4.912662277004227640, -4.994045588562562088 ) ) ;
#62987 = CARTESIAN_POINT ( 'NONE',  ( 11.52301463001509951, -3.452642973349600464, 8.376661845795100092 ) ) ;
#62988 = EDGE_CURVE ( 'NONE', #1808, #24606, #50940, .T. ) ;
#62989 = CARTESIAN_POINT ( 'NONE',  ( 17.76260332629189165, 3.089553855563651918, -12.29447117690774505 ) ) ;
#62990 = CARTESIAN_POINT ( 'NONE',  ( 13.99999999439439335, -9.377150629848445718, -8.201012428486357919 ) ) ;
#62991 = VECTOR ( 'NONE', #65935, 1000.000000000000114 ) ;
#62992 = CARTESIAN_POINT ( 'NONE',  ( 18.17985377383957157, 2.516953534566725104, 12.44759707711947883 ) ) ;
#62993 = CARTESIAN_POINT ( 'NONE',  ( 7.540307192462002206, 2.929979193199001575, 6.558004150875995641 ) ) ;
#62994 = CARTESIAN_POINT ( 'NONE',  ( 11.04647087182000043, -2.754739992437999607, -5.117584562748000110 ) ) ;
#62995 = CARTESIAN_POINT ( 'NONE',  ( 11.17788601987000163, -2.412142864687000010, -7.075602314719000141 ) ) ;
#62996 = CARTESIAN_POINT ( 'NONE',  ( 29.60000000000000142, 0.000000000000000000, 8.250000000000000000 ) ) ;
#62997 = CARTESIAN_POINT ( 'NONE',  ( 12.39267642948476222, 0.6007076874295218527, -13.98710814480368114 ) ) ;
#62998 = CARTESIAN_POINT ( 'NONE',  ( 13.73862479881500143, -8.949604875896001843, -7.398842444207000213 ) ) ;
#62999 = FACE_OUTER_BOUND ( 'NONE', #47135, .T. ) ;
#63000 = CARTESIAN_POINT ( 'NONE',  ( 9.101049665823000012, -5.350000000000001421, -7.263338156157798764 ) ) ;
#63001 = ORIENTED_EDGE ( 'NONE', *, *, #28097, .T. ) ;
#63002 = CARTESIAN_POINT ( 'NONE',  ( 8.564679719593000229, 4.146787477634999775, -5.941926545671999627 ) ) ;
#63003 = CARTESIAN_POINT ( 'NONE',  ( 11.54749144726329924, -4.500836215462999945, 8.206726025856399431 ) ) ;
#63004 = ORIENTED_EDGE ( 'NONE', *, *, #13606, .F. ) ;
#63005 = DIRECTION ( 'NONE',  ( 1.000000000000000000, 0.000000000000000000, 0.000000000000000000 ) ) ;
#63006 = CARTESIAN_POINT ( 'NONE',  ( 18.25313429507006546, 2.320711718358090536, -13.80631856085854992 ) ) ;
#63007 = ORIENTED_EDGE ( 'NONE', *, *, #66088, .F. ) ;
#63008 = CARTESIAN_POINT ( 'NONE',  ( 11.43345123989529810, 4.540230239159599890, 6.456682674800999777 ) ) ;
#63009 = CARTESIAN_POINT ( 'NONE',  ( 17.89176949848240028, 3.347044352179603610, -11.15884716666442600 ) ) ;
#63010 = DIRECTION ( 'NONE',  ( 1.000000000000000000, 0.000000000000000000, 0.000000000000000000 ) ) ;
#63011 = CARTESIAN_POINT ( 'NONE',  ( 10.52946886766499901, -4.430164648092599577, -6.718432993015899690 ) ) ;
#63012 = CARTESIAN_POINT ( 'NONE',  ( 17.55505043854147118, -1.875000000000000000, -25.00000000000000000 ) ) ;
#63013 = DIRECTION ( 'NONE',  ( 0.000000000000000000, 1.000000000000000000, 0.000000000000000000 ) ) ;
#63014 = ORIENTED_EDGE ( 'NONE', *, *, #22830, .F. ) ;
#63015 = FACE_OUTER_BOUND ( 'NONE', #42546, .T. ) ;
#63016 = CARTESIAN_POINT ( 'NONE',  ( 9.286929719595001131, 4.102804347295999854, -5.770625657082999460 ) ) ;
#63017 = ORIENTED_EDGE ( 'NONE', *, *, #68895, .T. ) ;
#63018 = AXIS2_PLACEMENT_3D ( 'NONE', #34996, #56310, #2141 ) ;
#63019 = CARTESIAN_POINT ( 'NONE',  ( 11.03408597791999846, 2.992846905312999795, -9.056576857348998644 ) ) ;
#63020 = ORIENTED_EDGE ( 'NONE', *, *, #17670, .F. ) ;
#63021 = CARTESIAN_POINT ( 'NONE',  ( 9.453329965421998438, 3.111510091554099855, 6.579690231462300254 ) ) ;
#63022 = CARTESIAN_POINT ( 'NONE',  ( 17.98531014845341858, -2.046560857067137640, -12.54571659797611360 ) ) ;
#63023 = CARTESIAN_POINT ( 'NONE',  ( 9.328814160995289484, 2.650569397798120619, -7.263217323294509420 ) ) ;
#63024 = ADVANCED_FACE ( 'NONE', ( #17741 ), #39061, .T. ) ;
#63025 = EDGE_CURVE ( 'NONE', #10995, #62306, #39767, .T. ) ;
#63026 = CARTESIAN_POINT ( 'NONE',  ( 24.30000000000000071, 2.078227429405999693, 11.31065739696999906 ) ) ;
#63027 = EDGE_CURVE ( 'NONE', #24880, #47459, #25748, .T. ) ;
#63028 = CARTESIAN_POINT ( 'NONE',  ( 11.11772401304000013, -8.026951646845001065, -6.811579381709000458 ) ) ;
#63029 = ORIENTED_EDGE ( 'NONE', *, *, #16777, .T. ) ;
#63030 = CARTESIAN_POINT ( 'NONE',  ( 11.59999999999999964, 4.924024592270519918, 6.664392815890117561 ) ) ;
#63031 = CARTESIAN_POINT ( 'NONE',  ( 10.61443584123000150, 5.287628373050000441, -7.937241318065001217 ) ) ;
#63032 = AXIS2_PLACEMENT_3D ( 'NONE', #23504, #7078, #1493 ) ;
#63033 = CARTESIAN_POINT ( 'NONE',  ( 9.975298369746390392, 5.350379160513678123, 7.499985214262784083 ) ) ;
#63034 = DIRECTION ( 'NONE',  ( 0.000000000000000000, -0.9516627692381158798, 0.3071448740351048756 ) ) ;
#63035 = CARTESIAN_POINT ( 'NONE',  ( 17.97713831050996447, 0.5938246120522454596, 13.98740230410797558 ) ) ;
#63036 = AXIS2_PLACEMENT_3D ( 'NONE', #35107, #35783, #68264 ) ;
#63037 = CARTESIAN_POINT ( 'NONE',  ( 17.99211270977099986, 3.227071166021000082, 11.34499727797000013 ) ) ;
#63038 = CARTESIAN_POINT ( 'NONE',  ( 10.89218817467000200, -2.661900611977999986, -8.236035141896001832 ) ) ;
#63039 = ORIENTED_EDGE ( 'NONE', *, *, #29688, .T. ) ;
#63040 = EDGE_LOOP ( 'NONE', ( #6172, #4233, #39817, #49702 ) ) ;
#63041 = CARTESIAN_POINT ( 'NONE',  ( 9.667010841233000917, 4.769103072373000352, -8.666849124598000387 ) ) ;
#63042 = DIRECTION ( 'NONE',  ( 7.373249170895999531E-10, 7.373245149945000197E-10, -1.000000000000000000 ) ) ;
#63043 = LINE ( 'NONE', #31600, #59200 ) ;
#63044 = CARTESIAN_POINT ( 'NONE',  ( 24.56658884197400283, 8.743998557975999120, -8.863912221221001531 ) ) ;
#63045 = CARTESIAN_POINT ( 'NONE',  ( 11.80233327354039830, 2.898463260143000042, -6.779499720266399798 ) ) ;
#63047 = AXIS2_PLACEMENT_3D ( 'NONE', #25799, #10060, #25110 ) ;
#63046 = CARTESIAN_POINT ( 'NONE',  ( 8.978113844317999082, 4.218953675027299788, -6.661091642253600398 ) ) ;
#63049 = CARTESIAN_POINT ( 'NONE',  ( 8.735210106471628322, 5.610874584628978923, 8.247390189602128885 ) ) ;
#63048 = CARTESIAN_POINT ( 'NONE',  ( 10.76291290906799958, -4.635529777446699917, 6.722218404915299317 ) ) ;
#63050 = CARTESIAN_POINT ( 'NONE',  ( 8.076856445596000356, -2.879480170456998778, 6.727212843387002650 ) ) ;
#63051 = ORIENTED_EDGE ( 'NONE', *, *, #51165, .T. ) ;
#63052 = FACE_OUTER_BOUND ( 'NONE', #15669, .T. ) ;
#63053 = CARTESIAN_POINT ( 'NONE',  ( 10.39853701727000157, -3.107293017143999858, -4.742114626611999562 ) ) ;
#63054 = CARTESIAN_POINT ( 'NONE',  ( 9.861671671056999600, 2.738456190347000163, 7.288123611975898974 ) ) ;
#63055 = CARTESIAN_POINT ( 'NONE',  ( 21.59999946634000167, 13.89999946622000060, 2.316962009661000178E-09 ) ) ;
#63056 = B_SPLINE_CURVE_WITH_KNOTS ( 'NONE', 3,
 ( #18031, #55774, #7877, #60666 ),
 .UNSPECIFIED., .F., .F.,
 ( 4, 4 ),
 ( 0.000000000000000000, 1.000000000000000000 ),
 .UNSPECIFIED. ) ;
#63057 = CARTESIAN_POINT ( 'NONE',  ( 9.194602547868999665, -5.157768569202000108, 8.637845986715998237 ) ) ;
#63058 = DIRECTION ( 'NONE',  ( -7.774844867625903451E-08, 7.808575926866904497E-08, -0.9999999999999940048 ) ) ;
#63059 = CARTESIAN_POINT ( 'NONE',  ( 16.04514873068900016, -3.655338946640000142, -11.11851555082999887 ) ) ;
#63060 = CARTESIAN_POINT ( 'NONE',  ( 13.46222979673600051, 9.132942286732999904, 7.608635239113000104 ) ) ;
#63061 = CARTESIAN_POINT ( 'NONE',  ( 7.995055131332884812, 3.139660977872365422, -6.336962724805712988 ) ) ;
#63062 = CARTESIAN_POINT ( 'NONE',  ( 11.12309687351639020, -2.782534154164605145, 7.172815144550900968 ) ) ;
#63063 = B_SPLINE_SURFACE_WITH_KNOTS ( 'NONE', 3, 3, ( 
 ( #22541, #54012, #540, #1571 ),
 ( #26777, #37592, #22889, #6463 ),
 ( #43187, #27810, #53338, #21852 ),
 ( #64154, #16612, #65185, #6809 ) ),
 .UNSPECIFIED., .F., .F., .F.,
 ( 4, 4 ),
 ( 4, 4 ),
 ( -0.01349945606786999951, 0.08053609420915000539 ),
 ( -0.0005287450254680999126, 0.02696599629895000266 ),
 .UNSPECIFIED. ) ;
#63064 = ADVANCED_FACE ( 'NONE', ( #968 ), #48859, .F. ) ;
#63065 = CARTESIAN_POINT ( 'NONE',  ( 0.2087320758492651196, 3.208711876255013529, -0.4208838518088701131 ) ) ;
#63066 = PRODUCT_DEFINITION_FORMATION_WITH_SPECIFIED_SOURCE ( 'ANY', '', #51713, .NOT_KNOWN. ) ;
#63067 = DIRECTION ( 'NONE',  ( 0.000000000000000000, -0.7158784314710772145, 0.6982249432342778617 ) ) ;
#63068 = CARTESIAN_POINT ( 'NONE',  ( 3.157929369547999965, -0.6681045838537000847, -3.189815491325000085 ) ) ;
#63069 = EDGE_LOOP ( 'NONE', ( #39199, #13702, #64381, #24371 ) ) ;
#63070 = CARTESIAN_POINT ( 'NONE',  ( 12.58454787187813650, 0.5848996845204771367, -12.68186405703079167 ) ) ;
#63071 = CARTESIAN_POINT ( 'NONE',  ( 12.19364288166475063, -2.630035214363327434, -12.42031982033429038 ) ) ;
#63072 = EDGE_CURVE ( 'NONE', #24435, #49203, #67470, .T. ) ;
#63073 = DIRECTION ( 'NONE',  ( 1.000000000000000000, 0.000000000000000000, 0.000000000000000000 ) ) ;
#63074 = DIRECTION ( 'NONE',  ( -1.000000000000000000, 0.000000000000000000, 0.000000000000000000 ) ) ;
#63075 = DIRECTION ( 'NONE',  ( -1.000000000000000000, 0.000000000000000000, 0.000000000000000000 ) ) ;
#63076 = ORIENTED_EDGE ( 'NONE', *, *, #6401, .T. ) ;
#63077 = DIRECTION ( 'NONE',  ( 0.000000000000000000, 0.8648648648648720183, -0.5020047465136825426 ) ) ;
#63078 =( LENGTH_UNIT ( ) NAMED_UNIT ( * ) SI_UNIT ( .MILLI., .METRE. ) );
#63079 = CARTESIAN_POINT ( 'NONE',  ( 10.96940393808957381, 8.671713867168650225, 6.520930117690211247 ) ) ;
#63080 = CARTESIAN_POINT ( 'NONE',  ( 11.09392659058483233, 2.706073409411867914, 6.603326177255940621 ) ) ;
#63081 = FACE_OUTER_BOUND ( 'NONE', #35243, .T. ) ;
#63082 = CARTESIAN_POINT ( 'NONE',  ( 13.07616489729400122, 12.32806027643999869, 1.877794484342000025 ) ) ;
#63083 = EDGE_LOOP ( 'NONE', ( #21487, #63187, #12049, #23361 ) ) ;
#63084 = B_SPLINE_CURVE_WITH_KNOTS ( 'NONE', 3,
 ( #58957, #63842, #5122, #11063, #42535, #922, #10708, #43573, #26457, #37971 ),
 .UNSPECIFIED., .F., .F.,
 ( 4, 2, 2, 2, 4 ),
 ( 0.000000000000000000, 0.2500000000000009992, 0.3750000000000014988, 0.5000000000000019984, 1.000000000000000000 ),
 .UNSPECIFIED. ) ;
#63085 = CARTESIAN_POINT ( 'NONE',  ( 11.11504459742000073, -3.456612073675000119, 5.970342812640000218 ) ) ;
#63086 = ORIENTED_EDGE ( 'NONE', *, *, #42614, .T. ) ;
#63087 = CARTESIAN_POINT ( 'NONE',  ( 8.495897545620808344, -3.117844663886039758, 6.071417532389746796 ) ) ;
#63088 = CARTESIAN_POINT ( 'NONE',  ( 7.481081853206999810, -2.374041291348000016, 8.293390875797999939 ) ) ;
#63089 = AXIS2_PLACEMENT_3D ( 'NONE', #5001, #47661, #101 ) ;
#63090 = CARTESIAN_POINT ( 'NONE',  ( 17.57900089668074273, -0.7302151644511190032, -13.98094363559787290 ) ) ;
#63091 = ORIENTED_EDGE ( 'NONE', *, *, #6551, .T. ) ;
#63092 = CARTESIAN_POINT ( 'NONE',  ( 16.39999999393278429, 3.428567374516922506, 11.90640519000895559 ) ) ;
#63093 = CARTESIAN_POINT ( 'NONE',  ( 23.60000000000000142, 9.305479840184000651, 8.315530346521999405 ) ) ;
#63094 = CARTESIAN_POINT ( 'NONE',  ( 7.581654719587999303, 4.473304741848999733, -6.008315738301999609 ) ) ;
#63095 = CARTESIAN_POINT ( 'NONE',  ( 11.11486084871780022, 5.207010770456999893, 7.825000000000000178 ) ) ;
#63096 = CARTESIAN_POINT ( 'NONE',  ( 17.94531445438002848, -2.988940031718063217, 12.32413547815666277 ) ) ;
#63097 = ORIENTED_EDGE ( 'NONE', *, *, #49248, .F. ) ;
#63098 = CARTESIAN_POINT ( 'NONE',  ( 9.504901164121001500, -3.934733502342999678, 5.704835336325999151 ) ) ;
#63099 = CARTESIAN_POINT ( 'NONE',  ( 12.21323965719961180, -2.701097326009253230, -13.62869820424139178 ) ) ;
#63100 = CARTESIAN_POINT ( 'NONE',  ( 9.356495485442707150, -3.650546589001255171, 6.546761994161411913 ) ) ;
#63101 = VERTEX_POINT ( 'NONE', #38714 ) ;
#63102 = DIRECTION ( 'NONE',  ( 0.000000000000000000, -0.7071067811865474617, -0.7071067811865474617 ) ) ;
#63103 = CARTESIAN_POINT ( 'NONE',  ( 7.956697741658004475, 3.406302814652999889, -6.282208831379191949 ) ) ;
#63104 = ORIENTED_EDGE ( 'NONE', *, *, #33962, .T. ) ;
#63105 = CARTESIAN_POINT ( 'NONE',  ( 11.79999999684100054, 12.15995044155999949, 2.000340912084999978 ) ) ;
#63106 = CARTESIAN_POINT ( 'NONE',  ( 23.89491057039001731, 12.87866800254527888, -3.584029398659131616 ) ) ;
#63107 = CARTESIAN_POINT ( 'NONE',  ( 5.034865712291000328, -1.474529322351999960, 0.5016153125228000054 ) ) ;
#63108 = CARTESIAN_POINT ( 'NONE',  ( 12.80505043854146940, -2.500000000000000444, -25.00000000000000000 ) ) ;
#63109 = DIRECTION ( 'NONE',  ( -1.000000000000000000, 0.000000000000000000, 0.000000000000000000 ) ) ;
#63110 = CARTESIAN_POINT ( 'NONE',  ( 25.46375345652300126, 2.879422156700999658, -11.30951020355999859 ) ) ;
#63111 = EDGE_CURVE ( 'NONE', #59076, #42164, #66608, .T. ) ;
#63112 = CARTESIAN_POINT ( 'NONE',  ( 12.39904396558114463, 2.975276281382167376, 13.56103672317924769 ) ) ;
#63113 = EDGE_CURVE ( 'NONE', #49620, #49843, #10759, .T. ) ;
#63114 = AXIS2_PLACEMENT_3D ( 'NONE', #47327, #42076, #31591 ) ;
#63116 = EDGE_CURVE ( 'NONE', #67674, #28175, #51622, .T. ) ;
#63115 = CARTESIAN_POINT ( 'NONE',  ( 4.650001602240106280, 2.000000000000000000, 2.043842969622812301E-09 ) ) ;
#63117 = EDGE_LOOP ( 'NONE', ( #35291, #37162, #40109, #11497 ) ) ;
#63118 = CARTESIAN_POINT ( 'NONE',  ( 10.52946886766499901, -4.430164648092599577, -6.718432993015899690 ) ) ;
#63119 = ORIENTED_EDGE ( 'NONE', *, *, #22867, .F. ) ;
#63120 = CARTESIAN_POINT ( 'NONE',  ( 9.298033738970000073, 4.087077023028999001, 9.429414864145000408 ) ) ;
#63121 = CARTESIAN_POINT ( 'NONE',  ( 0.7000000000000000666, 0.000000000000000000, 0.5999999999999999778 ) ) ;
#63122 = CARTESIAN_POINT ( 'NONE',  ( 8.871410841230998656, 2.721111233225000259, -6.936528696292000085 ) ) ;
#63123 = CARTESIAN_POINT ( 'NONE',  ( 2.342247503581000423, 1.381879776714000085, -3.088550434077999896 ) ) ;
#63124 = CARTESIAN_POINT ( 'NONE',  ( 25.20345855277900071, 2.651890812380999662, 11.40160123550000115 ) ) ;
#63125 = CARTESIAN_POINT ( 'NONE',  ( 15.90018573812399971, 8.493548356068000516, 8.263529029821000904 ) ) ;
#63126 = VERTEX_POINT ( 'NONE', #66218 ) ;
#63127 = CARTESIAN_POINT ( 'NONE',  ( 9.274684250042126266, -5.195247215952409903, -6.222724923390055451 ) ) ;
#63128 = ORIENTED_EDGE ( 'NONE', *, *, #20398, .T. ) ;
#63129 = CARTESIAN_POINT ( 'NONE',  ( 12.46489557882766341, 0.5244061151666827847, 13.88668399599068870 ) ) ;
#63130 = CARTESIAN_POINT ( 'NONE',  ( 10.91964694612699915, -5.186980343482999523, 7.026297514493899499 ) ) ;
#63131 = CARTESIAN_POINT ( 'NONE',  ( 3.300973465876999580, -3.500000000000000000, 0.000000000000000000 ) ) ;
#63132 = DIRECTION ( 'NONE',  ( -1.000000000000000000, 0.000000000000000000, 0.000000000000000000 ) ) ;
#63133 = EDGE_CURVE ( 'NONE', #8000, #54361, #29622, .T. ) ;
#63134 = CARTESIAN_POINT ( 'NONE',  ( 7.448644353207000357, -4.628942671846000501, 5.991663889842000046 ) ) ;
#63135 = CARTESIAN_POINT ( 'NONE',  ( 9.447841622600000377, 5.447457912891000120, 7.431328695644999982 ) ) ;
#63136 = CARTESIAN_POINT ( 'NONE',  ( 10.66995391537419913, 4.943675741382899780, -8.140910455049299443 ) ) ;
#63137 = AXIS2_PLACEMENT_3D ( 'NONE', #41416, #61368, #29916 ) ;
#63138 = B_SPLINE_CURVE_WITH_KNOTS ( 'NONE', 3,
 ( #64441, #6763, #60603, #55362, #7457, #6414, #12714, #491, #11315, #44194 ),
 .UNSPECIFIED., .F., .F.,
 ( 4, 2, 2, 2, 4 ),
 ( 0.000000000000000000, 0.2500000000000000555, 0.5000000000000000000, 0.7499999999999998890, 1.000000000000000000 ),
 .UNSPECIFIED. ) ;
#63139 = DIRECTION ( 'NONE',  ( 1.000000000000000000, 0.000000000000000000, 0.000000000000000000 ) ) ;
#63140 = AXIS2_PLACEMENT_3D ( 'NONE', #6274, #27616, #6630 ) ;
#63141 = CARTESIAN_POINT ( 'NONE',  ( 8.802265421554999136, 3.811499292588199861, -8.475084258675400051 ) ) ;
#63142 = CARTESIAN_POINT ( 'NONE',  ( 18.03335409833309555, 0.5406785836137698587, 12.58839662496522749 ) ) ;
#63143 = CARTESIAN_POINT ( 'NONE',  ( 6.961241552806000321, 1.068399614603999792, -0.6924786331873999945 ) ) ;
#63144 = CYLINDRICAL_SURFACE ( 'NONE', #33355, 0.5500000000000000444 ) ;
#63145 = CARTESIAN_POINT ( 'NONE',  ( 0.3043556721781856544, 1.649503828942506578, -2.894701909231111703 ) ) ;
#63146 = VERTEX_POINT ( 'NONE', #46021 ) ;
#63147 = CARTESIAN_POINT ( 'NONE',  ( 7.448644353207000357, -4.628942671846000501, 5.991663889842000046 ) ) ;
#63148 = CARTESIAN_POINT ( 'NONE',  ( 17.74396022931447092, 3.223333129201660707, 13.62388254889261496 ) ) ;
#63149 = DIRECTION ( 'NONE',  ( 1.000000000000000000, 0.000000000000000000, 0.000000000000000000 ) ) ;
#63150 = ORIENTED_EDGE ( 'NONE', *, *, #31654, .F. ) ;
#63151 = CARTESIAN_POINT ( 'NONE',  ( 0.08797697758023999282, -1.491878233134000142, -2.734521550864000172 ) ) ;
#63152 = CARTESIAN_POINT ( 'NONE',  ( 10.63880513895979973, 5.150451045932999961, 8.139542779846600240 ) ) ;
#63153 = CARTESIAN_POINT ( 'NONE',  ( 10.59957028040999916, 4.438147096284001059, -8.958385582135001357 ) ) ;
#63154 = VERTEX_POINT ( 'NONE', #46369 ) ;
#63155 = CARTESIAN_POINT ( 'NONE',  ( 9.258504216683469679, 4.163629870566138536, -6.250027056024106464 ) ) ;
#63156 = CARTESIAN_POINT ( 'NONE',  ( 17.65323508305261768, -1.760912828005723130, 12.47634505842160735 ) ) ;
#63157 = CARTESIAN_POINT ( 'NONE',  ( 10.59195391537400077, 5.057233422790000432, 6.781965272201699868 ) ) ;
#63158 = EDGE_CURVE ( 'NONE', #16743, #46332, #52311, .T. ) ;
#63159 = CARTESIAN_POINT ( 'NONE',  ( 24.67921139482200132, 8.727627377900999406, -9.158314240160001063 ) ) ;
#63160 = FACE_OUTER_BOUND ( 'NONE', #7646, .T. ) ;
#63161 = ORIENTED_EDGE ( 'NONE', *, *, #11840, .T. ) ;
#63162 = CARTESIAN_POINT ( 'NONE',  ( 13.99999999347100044, 9.187456302440001110, 8.213201953411001455 ) ) ;
#63163 = CARTESIAN_POINT ( 'NONE',  ( 7.964689158768001320, 3.456780951359999854, -9.320567109458000488 ) ) ;
#63164 = CARTESIAN_POINT ( 'NONE',  ( 8.236412180507333147, -5.557254354115385375, 8.275240123836031358 ) ) ;
#63165 = CARTESIAN_POINT ( 'NONE',  ( 10.51057120343299900, -4.062009413492949861, 6.222291352336999815 ) ) ;
#63166 = ORIENTED_EDGE ( 'NONE', *, *, #18959, .F. ) ;
#63167 = CARTESIAN_POINT ( 'NONE',  ( 6.999999691988000095, -2.604139126561000230E-12, 1.310063169058000104E-14 ) ) ;
#63168 = CARTESIAN_POINT ( 'NONE',  ( 5.700000000000000178, 12.50865771883999855, -2.924687089724999911 ) ) ;
#63169 = ORIENTED_EDGE ( 'NONE', *, *, #23684, .F. ) ;
#63170 = FACE_OUTER_BOUND ( 'NONE', #59164, .T. ) ;
#63171 = CARTESIAN_POINT ( 'NONE',  ( 6.949657512459999964, 12.16386489619000066, 3.090547023080999711 ) ) ;
#63172 = AXIS2_PLACEMENT_3D ( 'NONE', #6821, #6124, #38290 ) ;
#63173 = VERTEX_POINT ( 'NONE', #8956 ) ;
#63174 = CARTESIAN_POINT ( 'NONE',  ( 18.12876426765905791, 0.2481576080865483258, -13.89702325994032783 ) ) ;
#63175 = LINE ( 'NONE', #47465, #34208 ) ;
#63176 = CARTESIAN_POINT ( 'NONE',  ( 2.321806799209417793, -3.408904368339104263, -0.9161175952574813763 ) ) ;
#63177 = CARTESIAN_POINT ( 'NONE',  ( 11.72433327354039889, 3.016779570871600313, -6.856888818507299810 ) ) ;
#63178 = CARTESIAN_POINT ( 'NONE',  ( 11.72567835872029995, -4.993948309075300074, 8.126439557340900066 ) ) ;
#63179 = DIRECTION ( 'NONE',  ( 0.000000000000000000, -1.000000000000000000, 0.000000000000000000 ) ) ;
#63180 = CARTESIAN_POINT ( 'NONE',  ( 11.92887348028849992, -5.124210964533999935, 6.892162778124999889 ) ) ;
#63181 = DIRECTION ( 'NONE',  ( 1.000000000000000000, 0.000000000000000000, 0.000000000000000000 ) ) ;
#63182 = VERTEX_POINT ( 'NONE', #24354 ) ;
#63183 = CARTESIAN_POINT ( 'NONE',  ( 9.154341692891295068, -2.749999283195044164, -7.336371291557481022 ) ) ;
#63184 = AXIS2_PLACEMENT_3D ( 'NONE', #25475, #46807, #61850 ) ;
#63185 = CARTESIAN_POINT ( 'NONE',  ( 11.43028911132391379, -5.144000659054666080, -8.059011948032955175 ) ) ;
#63186 = CARTESIAN_POINT ( 'NONE',  ( 15.90000000000000036, -8.729799320958107955, -8.474717466973274327 ) ) ;
#63187 = ORIENTED_EDGE ( 'NONE', *, *, #15919, .T. ) ;
#63188 = CARTESIAN_POINT ( 'NONE',  ( 12.20147980349672601, -2.662577969174665604, -12.41220455913370380 ) ) ;
#63189 = VECTOR ( 'NONE', #47058, 1000.000000000000114 ) ;
#63190 = DIRECTION ( 'NONE',  ( -1.000000000000000000, 0.000000000000000000, 0.000000000000000000 ) ) ;
#63191 = FACE_OUTER_BOUND ( 'NONE', #54076, .T. ) ;
#63192 = FACE_OUTER_BOUND ( 'NONE', #32691, .T. ) ;
#63193 = CARTESIAN_POINT ( 'NONE',  ( 12.21194158638448002, -2.301857635319168427, -13.71345735897203610 ) ) ;
#63194 = CARTESIAN_POINT ( 'NONE',  ( 11.73256516821459883, -3.293702443348299980, -8.212808089543500500 ) ) ;
#63195 = B_SPLINE_CURVE_WITH_KNOTS ( 'NONE', 3,
 ( #12639, #12994, #61227, #38510, #13343, #34318 ),
 .UNSPECIFIED., .F., .F.,
 ( 4, 2, 4 ),
 ( 0.000000000000000000, 0.1860062838997574297, 0.3720125677995148594 ),
 .UNSPECIFIED. ) ;
#63196 = DIRECTION ( 'NONE',  ( -1.000000000000000000, 0.000000000000000000, 0.000000000000000000 ) ) ;
#63198 = EDGE_CURVE ( 'NONE', #31672, #3964, #53179, .T. ) ;
#63197 = CARTESIAN_POINT ( 'NONE',  ( 18.27387565520749391, -2.575953525795620092, 12.33388021351436947 ) ) ;
#63199 = ORIENTED_EDGE ( 'NONE', *, *, #43653, .T. ) ;
#63200 = ORIENTED_EDGE ( 'NONE', *, *, #65837, .F. ) ;
#63201 = CARTESIAN_POINT ( 'NONE',  ( 0.000000000000000000, 0.000000000000000000, 0.000000000000000000 ) ) ;
#63202 = DIRECTION ( 'NONE',  ( -1.000000000000000000, 0.000000000000000000, 0.000000000000000000 ) ) ;
#63203 = CARTESIAN_POINT ( 'NONE',  ( 4.900006121741999010, 2.000000000000000000, 0.000000000000000000 ) ) ;
#63204 = CARTESIAN_POINT ( 'NONE',  ( 10.99693586709999948, 2.980605808171000071, -6.418617723582000778 ) ) ;
#63205 = DIRECTION ( 'NONE',  ( 1.000000000000000000, 3.552713678845000257E-14, 1.776356839423000267E-14 ) ) ;
#63206 = CARTESIAN_POINT ( 'NONE',  ( 17.77739983953768643, 3.084473828682777974, 12.29598274197195806 ) ) ;
#63207 = CARTESIAN_POINT ( 'NONE',  ( 23.73691858855699977, -13.28034100689999875, 3.697799110653999577 ) ) ;
#63208 = CARTESIAN_POINT ( 'NONE',  ( 18.27948916824812287, -2.669673601445818889, -12.31540264490818615 ) ) ;
#63209 = VERTEX_POINT ( 'NONE', #23661 ) ;
#63210 = CARTESIAN_POINT ( 'NONE',  ( 9.099999999999999645, 0.000000000000000000, 0.000000000000000000 ) ) ;
#63211 = ORIENTED_EDGE ( 'NONE', *, *, #44983, .F. ) ;
#63212 = CARTESIAN_POINT ( 'NONE',  ( 12.58270105247236970, -3.084473834238325107, 12.29599965897949865 ) ) ;
#63213 = CARTESIAN_POINT ( 'NONE',  ( 9.653000818238998804, -4.767147064380999666, -7.903971937289999694 ) ) ;
#63214 = CARTESIAN_POINT ( 'NONE',  ( 9.260906466624998501, 4.901388651757999426, 9.090324495507999814 ) ) ;
#63215 = EDGE_CURVE ( 'NONE', #21757, #20699, #40675, .T. ) ;
#63216 = CARTESIAN_POINT ( 'NONE',  ( 11.09725056272499977, -2.683866746800999792, 7.480494252843770120 ) ) ;
#63217 = CARTESIAN_POINT ( 'NONE',  ( 9.169760841232999837, 4.728328492779000136, -8.692725459657999920 ) ) ;
#63218 = CARTESIAN_POINT ( 'NONE',  ( 10.95123343040000030, 9.911362171613999905, -5.636329857493000084 ) ) ;
#63219 = AXIS2_PLACEMENT_3D ( 'NONE', #3182, #40246, #20288 ) ;
#63220 = B_SPLINE_CURVE_WITH_KNOTS ( 'NONE', 3,
 ( #28197, #55806, #18746, #7554 ),
 .UNSPECIFIED., .F., .F.,
 ( 4, 4 ),
 ( 0.000000000000000000, 1.000000000000000000 ),
 .UNSPECIFIED. ) ;
#63221 = EDGE_CURVE ( 'NONE', #15621, #17417, #41544, .T. ) ;
#63222 = CARTESIAN_POINT ( 'NONE',  ( 10.46887750876899936, 3.307728619566300043, -8.574279626736998949 ) ) ;
#63223 = CARTESIAN_POINT ( 'NONE',  ( 10.92101570304880909, 4.925410080013705283, -9.003883028371625130 ) ) ;
#63224 = VECTOR ( 'NONE', #37474, 1000.000000000000000 ) ;
#63225 = CARTESIAN_POINT ( 'NONE',  ( 11.59999999999999609, 3.168976350368595263, -7.997379651729209726 ) ) ;
#63226 = DIRECTION ( 'NONE',  ( 0.000000000000000000, -0.1218274111675002463, 0.9925512993736016476 ) ) ;
#63227 = CARTESIAN_POINT ( 'NONE',  ( 11.35180279716000129, -3.678144743825999985, 11.20807767738999949 ) ) ;
#63228 = VERTEX_POINT ( 'NONE', #45686 ) ;
#63229 = CARTESIAN_POINT ( 'NONE',  ( 8.590779719591999708, 2.836879604150999601, -8.783908972046001296 ) ) ;
#63230 = FACE_OUTER_BOUND ( 'NONE', #56261, .T. ) ;
#63231 = CARTESIAN_POINT ( 'NONE',  ( 20.07256264693999981, 0.000000000000000000, 0.000000000000000000 ) ) ;
#63232 = DIRECTION ( 'NONE',  ( -1.000000000000000000, 0.000000000000000000, 0.000000000000000000 ) ) ;
#63233 = CARTESIAN_POINT ( 'NONE',  ( 5.000000000000000000, -1.199999999999999956, -9.776630298829998011 ) ) ;
#63234 = B_SPLINE_CURVE_WITH_KNOTS ( 'NONE', 3,
 ( #42948, #37021, #53093, #4844, #58679, #26877, #41915, #52051, #64257, #63223, #20247, #4496, #25836, #15350, #68817, #20939, #43295, #21956 ),
 .UNSPECIFIED., .F., .F.,
 ( 4, 2, 2, 2, 2, 2, 2, 2, 4 ),
 ( 0.000000000000000000, 0.1250000000000000833, 0.2500000000000001665, 0.3750000000000002220, 0.5000000000000003331, 0.6250000000000004441, 0.7500000000000004441, 0.8750000000000002220, 1.000000000000000000 ),
 .UNSPECIFIED. ) ;
#63235 = CARTESIAN_POINT ( 'NONE',  ( 10.47303166480599934, -5.137916160623999140, -7.580230465881790280 ) ) ;
#63236 = ORIENTED_EDGE ( 'NONE', *, *, #35028, .F. ) ;
#63237 = CIRCLE ( 'NONE', #29798, 13.10000000000000320 ) ;
#63238 = CARTESIAN_POINT ( 'NONE',  ( 10.12435795695566476, -2.750000000000000000, -7.807440182398264206 ) ) ;
#63239 = CARTESIAN_POINT ( 'NONE',  ( 8.400073341230999802, 2.800103557244999930, 9.079946116129001155 ) ) ;
#63242 = DIRECTION ( 'NONE',  ( 1.000000000000000000, 0.000000000000000000, 0.000000000000000000 ) ) ;
#63241 = CARTESIAN_POINT ( 'NONE',  ( 9.988331016203231272, 2.447533665446552043, 6.696458009942619860 ) ) ;
#63240 = PRODUCT_DEFINITION_CONTEXT ( 'detailed design', #54308, 'design' ) ;
#63243 = CARTESIAN_POINT ( 'NONE',  ( 24.67921569845699992, 12.29514839105000057, -2.979196030862000022 ) ) ;
#63244 = EDGE_LOOP ( 'NONE', ( #59260, #39814, #12834, #32401, #52056 ) ) ;
#63245 = CARTESIAN_POINT ( 'NONE',  ( 9.848259964010999568, 4.436917881843999822, 6.148031614254000132 ) ) ;
#63246 = CARTESIAN_POINT ( 'NONE',  ( 18.15591411656202325, -2.672312740310635260, -13.63535347231577077 ) ) ;
#63247 = CARTESIAN_POINT ( 'NONE',  ( 10.33364828895399867, 4.760196147278000112, 7.084788038520800413 ) ) ;
#63248 = CARTESIAN_POINT ( 'NONE',  ( 10.71685100253999856, -2.832432432432000269, 6.822293592207000934 ) ) ;
#63249 = CARTESIAN_POINT ( 'NONE',  ( 7.705394353206999725, -3.245532552444000185, 8.949627348471000943 ) ) ;
#63250 = ORIENTED_EDGE ( 'NONE', *, *, #30844, .T. ) ;
#63251 = CARTESIAN_POINT ( 'NONE',  ( 9.214142219592000416, 5.421534627450999899, 6.381126373995999579 ) ) ;
#63252 = B_SPLINE_CURVE_WITH_KNOTS ( 'NONE', 3,
 ( #43814, #23512, #34019, #28076 ),
 .UNSPECIFIED., .F., .F.,
 ( 4, 4 ),
 ( 0.000000000000000000, 0.4999999998439638160 ),
 .UNSPECIFIED. ) ;
#63254 = CARTESIAN_POINT ( 'NONE',  ( 9.926183059621999760, -4.356410583133000003, -9.313949118577001585 ) ) ;
#63253 = CARTESIAN_POINT ( 'NONE',  ( 13.70003001321900449, 12.06139972930709270, 3.524828382075550604 ) ) ;
#63255 = CARTESIAN_POINT ( 'NONE',  ( 7.484823115406580740, -2.425454210375729502, 6.760261958790284353 ) ) ;
#63256 = CARTESIAN_POINT ( 'NONE',  ( 18.01649462512370903, -0.4224288469488072795, 13.89137824130979126 ) ) ;
#63257 = CARTESIAN_POINT ( 'NONE',  ( 24.25866820969800131, 3.167022761916999940, 12.13987262450000060 ) ) ;
#63258 = VERTEX_POINT ( 'NONE', #8277 ) ;
#63259 = CARTESIAN_POINT ( 'NONE',  ( 9.508513540182335078, 3.836375382625529795, -8.749999999999998224 ) ) ;
#63260 = CARTESIAN_POINT ( 'NONE',  ( 11.66641369783139837, -4.050626550392200542, 6.497808498716000081 ) ) ;
#63261 = CARTESIAN_POINT ( 'NONE',  ( 11.46253286130405691, 4.338994305312701805, 8.308656198582323071 ) ) ;
#63262 = CARTESIAN_POINT ( 'NONE',  ( 8.789886373836322875, -3.999992178805580334, -8.439846342473931173 ) ) ;
#63263 = CARTESIAN_POINT ( 'NONE',  ( 11.35918179236250047, 3.761636028845500412, 8.615559381441000752 ) ) ;
#63264 = EDGE_LOOP ( 'NONE', ( #31698, #10035, #30280, #20375, #46970 ) ) ;
#63265 = FACE_OUTER_BOUND ( 'NONE', #20445, .T. ) ;
#63266 = CARTESIAN_POINT ( 'NONE',  ( 12.56405804856026442, 1.801709437036786099, -12.47051912880706404 ) ) ;
#63267 = CARTESIAN_POINT ( 'NONE',  ( 12.30233327354039830, -5.101536739857000846, 8.220500279733599314 ) ) ;
#63268 = CARTESIAN_POINT ( 'NONE',  ( 25.36444459794699924, -2.635932456649999978, -11.32519762123999918 ) ) ;
#63269 = AXIS2_PLACEMENT_3D ( 'NONE', #59878, #38207, #11984 ) ;
#63270 = B_SPLINE_CURVE_WITH_KNOTS ( 'NONE', 3,
 ( #13954, #56596, #8703, #2087 ),
 .UNSPECIFIED., .F., .F.,
 ( 4, 4 ),
 ( 0.000000000000000000, 1.000000000000000000 ),
 .UNSPECIFIED. ) ;
#63271 = CARTESIAN_POINT ( 'NONE',  ( 18.26447107791332058, -2.367226376531796461, 13.79841952404521166 ) ) ;
#63272 = LINE ( 'NONE', #68865, #22712 ) ;
#63273 = EDGE_LOOP ( 'NONE', ( #33582, #6179, #32754, #13511 ) ) ;
#63274 = CARTESIAN_POINT ( 'NONE',  ( 9.599999931441001166, -4.000000000000000000, 7.500000000000000000 ) ) ;
#63275 = CARTESIAN_POINT ( 'NONE',  ( 23.59999441188499958, 10.30760541648000128, -9.317696302454001156 ) ) ;
#63276 = ORIENTED_EDGE ( 'NONE', *, *, #47045, .T. ) ;
#63277 = DIRECTION ( 'NONE',  ( 0.000000000000000000, -1.000000000000000000, 0.000000000000000000 ) ) ;
#63278 = CARTESIAN_POINT ( 'NONE',  ( 9.509901345851000443, 5.077442745148000647, 8.469003100811999474 ) ) ;
#63279 = CARTESIAN_POINT ( 'NONE',  ( 10.43284001513000092, 3.279325423736999756, -9.029279369994000604 ) ) ;
#63280 = CARTESIAN_POINT ( 'NONE',  ( 8.244330716364007827, 4.955554988691996954, 6.175165069893004954 ) ) ;
#63281 = CARTESIAN_POINT ( 'NONE',  ( 9.332935524889000689, -5.100347267927999972, 8.693464469215999912 ) ) ;
#63282 = CARTESIAN_POINT ( 'NONE',  ( 17.94855945389787877, -0.6042324041877072949, -12.58550538354983672 ) ) ;
#63283 = AXIS2_PLACEMENT_3D ( 'NONE', #67984, #36523, #45653 ) ;
#63284 = CARTESIAN_POINT ( 'NONE',  ( 9.038697134104578979, 4.943501910544378042, 8.465380656488354916 ) ) ;
#63285 = CARTESIAN_POINT ( 'NONE',  ( 10.52641638348499953, -4.974961480482700260, -7.262511127784999410 ) ) ;
#63286 = EDGE_CURVE ( 'NONE', #6824, #54765, #46447, .T. ) ;
#63288 = EDGE_CURVE ( 'NONE', #32586, #31711, #58717, .T. ) ;
#63287 = CARTESIAN_POINT ( 'NONE',  ( 7.352704719590999360, 4.773081973066999772, 8.927402469597002010 ) ) ;
#63289 = ORIENTED_EDGE ( 'NONE', *, *, #38135, .F. ) ;
#63290 = AXIS2_PLACEMENT_3D ( 'NONE', #39363, #3657, #13830 ) ;
#63291 = CARTESIAN_POINT ( 'NONE',  ( 9.625409048293999348, -2.899999999999999911, -6.226580113766999602 ) ) ;
#63292 = CARTESIAN_POINT ( 'NONE',  ( 24.34833292450100117, 8.895958855249167740, 8.895958855249167740 ) ) ;
#63293 = LINE ( 'NONE', #36746, #61561 ) ;
#63294 = CARTESIAN_POINT ( 'NONE',  ( 9.236022032864006803, 9.967515357128998943, 5.897776175397996035 ) ) ;
#63295 = CARTESIAN_POINT ( 'NONE',  ( 12.51429325950072169, 1.848987300417678226, 13.87736530974562754 ) ) ;
#63296 = CARTESIAN_POINT ( 'NONE',  ( 13.70005190196300227, 9.005348107749998832, 7.391036106496999381 ) ) ;
#63297 = AXIS2_PLACEMENT_3D ( 'NONE', #56405, #22597, #13758 ) ;
#63298 = CARTESIAN_POINT ( 'NONE',  ( 12.47664625021882046, -0.5322368320764085947, -12.68499235032976102 ) ) ;
#63299 = CARTESIAN_POINT ( 'NONE',  ( 12.38296256657291394, -0.5938246120522429061, 13.98740230410797558 ) ) ;
#63300 = VERTEX_POINT ( 'NONE', #26773 ) ;
#63301 = CARTESIAN_POINT ( 'NONE',  ( 12.43945954148919064, -1.858853511423144145, 12.46213071393705007 ) ) ;
#63302 = CARTESIAN_POINT ( 'NONE',  ( 9.456405316140999773, -4.271593136661399726, -8.750048621292000561 ) ) ;
#63303 = LINE ( 'NONE', #4927, #61666 ) ;
#63304 = CARTESIAN_POINT ( 'NONE',  ( 10.90374822854000136, -3.726845778959999578, 5.900452123196999743 ) ) ;
#63305 = CARTESIAN_POINT ( 'NONE',  ( 11.69518313518939934, -4.537300658085600347, 6.820583637845799352 ) ) ;
#63306 = ADVANCED_FACE ( 'NONE', ( #48085 ), #5085, .F. ) ;
#63307 = CARTESIAN_POINT ( 'NONE',  ( 12.30074667651850184, 0.5168989769797244227, 12.58939571008426839 ) ) ;
#63308 = CARTESIAN_POINT ( 'NONE',  ( 0.07157952889540999952, -0.5148121778627998690, -3.334029978310999898 ) ) ;
#63309 = CARTESIAN_POINT ( 'NONE',  ( 9.762727031004574840, 2.920691866409497184, -8.329517998611422058 ) ) ;
#63310 = CARTESIAN_POINT ( 'NONE',  ( 12.27207149905416550, 1.992391748285591513, 12.44148121715491584 ) ) ;
#63311 = CYLINDRICAL_SURFACE ( 'NONE', #34127, 0.5000000000000002220 ) ;
#63312 = CARTESIAN_POINT ( 'NONE',  ( 11.38795122972049967, 4.398282450130399646, -6.578956058177199751 ) ) ;
#63313 = CARTESIAN_POINT ( 'NONE',  ( 8.045433776029998540, 2.903894639863001892, -6.425841880607995549 ) ) ;
#63314 = CARTESIAN_POINT ( 'NONE',  ( 11.03905471959000018, 3.855072614532999875, -9.179480010827999692 ) ) ;
#63315 = CARTESIAN_POINT ( 'NONE',  ( 9.276025935145998602, 3.814256956409300070, -6.234344474498000110 ) ) ;
#63317 = CARTESIAN_POINT ( 'NONE',  ( 18.14887404799286230, -0.1995702674007985011, 12.69797248607370754 ) ) ;
#63316 = CARTESIAN_POINT ( 'NONE',  ( 17.77443075273995277, -11.85817042883088845, 3.314254474333838907 ) ) ;
#63318 = CARTESIAN_POINT ( 'NONE',  ( 8.099999999999999645, -11.84999999999999964, 0.000000000000000000 ) ) ;
#63319 = ORIENTED_EDGE ( 'NONE', *, *, #13632, .T. ) ;
#63320 = AXIS2_PLACEMENT_3D ( 'NONE', #29467, #35045, #40282 ) ;
#63321 = CARTESIAN_POINT ( 'NONE',  ( 12.49508659866806859, 0.5431048945666756556, 12.68437082640543245 ) ) ;
#63322 = CARTESIAN_POINT ( 'NONE',  ( 23.66004879239100234, -9.998911572074998588, 9.691526907171001071 ) ) ;
#63323 = CARTESIAN_POINT ( 'NONE',  ( 9.497627230745894877, 3.288461954788812758, -9.126428113227261107 ) ) ;
#63324 = CARTESIAN_POINT ( 'NONE',  ( 9.602342523874998648, 3.142972170141900001, 7.631191628371899682 ) ) ;
#63325 = FACE_OUTER_BOUND ( 'NONE', #3567, .T. ) ;
#63326 = CARTESIAN_POINT ( 'NONE',  ( 12.26319456176233125, -2.811641923064096993, 13.60240885908115516 ) ) ;
#63327 = CARTESIAN_POINT ( 'NONE',  ( 12.24918480870364945, 2.785872542152070697, 13.60860763679485075 ) ) ;
#63328 = CARTESIAN_POINT ( 'NONE',  ( 23.55075434807899981, 2.914196937700999968, -13.72993838155000113 ) ) ;
#63329 = B_SPLINE_CURVE_WITH_KNOTS ( 'NONE', 3,
 ( #66525, #49070, #18645, #44189 ),
 .UNSPECIFIED., .F., .F.,
 ( 4, 4 ),
 ( 0.000000000000000000, 1.000000000000000000 ),
 .UNSPECIFIED. ) ;
#63330 = ORIENTED_EDGE ( 'NONE', *, *, #1037, .F. ) ;
#63331 = CARTESIAN_POINT ( 'NONE',  ( 4.626950847545000300, 0.8932343018606000440, 0.6993127588698000441 ) ) ;
#63332 = CARTESIAN_POINT ( 'NONE',  ( 9.757279731608999640, -3.885210315895800015, -6.225948307210999566 ) ) ;
#63333 = AXIS2_PLACEMENT_3D ( 'NONE', #53980, #31636, #52958 ) ;
#63334 = CARTESIAN_POINT ( 'NONE',  ( 9.856851002545999663, 2.832432432432000269, -6.822293592207000934 ) ) ;
#63335 = CARTESIAN_POINT ( 'NONE',  ( 11.77745123989519982, -3.589787500396900199, 6.707778874960499849 ) ) ;
#63336 = CARTESIAN_POINT ( 'NONE',  ( 18.16006747845239744, 2.341920795209952555, -12.48703680160761209 ) ) ;
#63337 = CARTESIAN_POINT ( 'NONE',  ( 8.589811424367198356, 5.008283254081848490, 6.160546554369722649 ) ) ;
#63338 = CARTESIAN_POINT ( 'NONE',  ( 18.15919311622385024, 2.661142131363571028, 12.41257606650292011 ) ) ;
#63339 = EDGE_CURVE ( 'NONE', #17653, #7995, #37249, .T. ) ;
#63340 = EDGE_CURVE ( 'NONE', #40048, #59800, #52635, .T. ) ;
#63342 = AXIS2_PLACEMENT_3D ( 'NONE', #58571, #52636, #58229 ) ;
#63341 = CARTESIAN_POINT ( 'NONE',  ( 8.146781841545999825, 3.121749852590999907, 6.130949854565998614 ) ) ;
#63343 = CARTESIAN_POINT ( 'NONE',  ( 9.443897997121000643, -4.993413662857000723, -9.088148847710000311 ) ) ;
#63344 = CARTESIAN_POINT ( 'NONE',  ( 10.68343305961999867, -3.810133104029999718, -5.661126601970999594 ) ) ;
#63345 = CARTESIAN_POINT ( 'NONE',  ( 9.174642513462206495, -2.649442673322992103, 7.499981897072125925 ) ) ;
#63346 = CARTESIAN_POINT ( 'NONE',  ( 7.896812975353013186, -5.287194663100612146, 7.026484571482168207 ) ) ;
#63347 = CARTESIAN_POINT ( 'NONE',  ( 23.67309711513813397, 9.998428628671371499, -9.464667082479147453 ) ) ;
#63348 = CARTESIAN_POINT ( 'NONE',  ( -17.56123417799999942, 11.06886219213000011, 1.536526853569999851 ) ) ;
#63349 = CARTESIAN_POINT ( 'NONE',  ( 23.73832405981900351, 13.27898672761999954, -3.695569413652000534 ) ) ;
#63350 = VERTEX_POINT ( 'NONE', #19796 ) ;
#63351 = CARTESIAN_POINT ( 'NONE',  ( 8.962479719595000560, 2.546924812613000189, -6.918870225297999887 ) ) ;
#63352 = CARTESIAN_POINT ( 'NONE',  ( 12.01102763632551884, -4.911148285670300595, 7.920427941950599404 ) ) ;
#63353 = ORIENTED_EDGE ( 'NONE', *, *, #32023, .F. ) ;
#63354 = LINE ( 'NONE', #31909, #19492 ) ;
#63355 = CARTESIAN_POINT ( 'NONE',  ( 11.28118179236249929, -4.267047616085000605, -6.250199235344999771 ) ) ;
#63357 = VERTEX_POINT ( 'NONE', #20136 ) ;
#63356 = B_SPLINE_CURVE_WITH_KNOTS ( 'NONE', 3,
 ( #15706, #32142, #37035, #53456 ),
 .UNSPECIFIED., .F., .F.,
 ( 4, 4 ),
 ( 0.000000000000000000, 1.000000000000000000 ),
 .UNSPECIFIED. ) ;
#63358 = CARTESIAN_POINT ( 'NONE',  ( 11.22567835872029995, 3.006051690924700370, 8.126439557340900066 ) ) ;
#63359 = CARTESIAN_POINT ( 'NONE',  ( 9.044210841233001119, 2.773858540272000184, -8.951250717848999727 ) ) ;
#63360 = CARTESIAN_POINT ( 'NONE',  ( 10.20000099824999928, 0.000000000000000000, 0.000000000000000000 ) ) ;
#63361 = CARTESIAN_POINT ( 'NONE',  ( 10.81499708368651369, -2.650004840405617124, -7.499999822193714749 ) ) ;
#63362 = CARTESIAN_POINT ( 'NONE',  ( 12.40639171139639885, 0.4813567170340031232, -13.88878047999878440 ) ) ;
#63363 = CARTESIAN_POINT ( 'NONE',  ( 10.98768472639999949, 5.139099012905000485, 4.945212061661000469 ) ) ;
#63364 = CARTESIAN_POINT ( 'NONE',  ( 11.33810207955129812, 4.796537143354000499, -7.825000000000000178 ) ) ;
#63365 = ORIENTED_EDGE ( 'NONE', *, *, #28985, .F. ) ;
#63366 = CARTESIAN_POINT ( 'NONE',  ( 13.50567905817900183, 9.332645239999999731, 7.987984570204999635 ) ) ;
#63367 = AXIS2_PLACEMENT_3D ( 'NONE', #49196, #18772, #12836 ) ;
#63369 = EDGE_CURVE ( 'NONE', #43973, #14135, #60970, .T. ) ;
#63368 = CARTESIAN_POINT ( 'NONE',  ( 9.635004719593998956, 2.334550724494000029, -7.977056617806000283 ) ) ;
#63370 = ORIENTED_EDGE ( 'NONE', *, *, #216, .T. ) ;
#63371 = B_SPLINE_CURVE_WITH_KNOTS ( 'NONE', 3,
 ( #37050, #22679, #1708, #43330 ),
 .UNSPECIFIED., .F., .F.,
 ( 4, 4 ),
 ( 0.000000000000000000, 1.000000000000000000 ),
 .UNSPECIFIED. ) ;
#63372 = CARTESIAN_POINT ( 'NONE',  ( 9.843622243630001378, 5.021682716044000294, -8.761466596873999535 ) ) ;
#63373 = EDGE_CURVE ( 'NONE', #14790, #12749, #684, .T. ) ;
#63374 = ORIENTED_EDGE ( 'NONE', *, *, #19624, .T. ) ;
#63375 = CARTESIAN_POINT ( 'NONE',  ( 9.276025935145998602, 3.814256956409300070, 8.765655525501999890 ) ) ;
#63376 = CARTESIAN_POINT ( 'NONE',  ( 17.88765289689609972, -3.029249243711964468, -12.31236272700674839 ) ) ;
#63377 = CONICAL_SURFACE ( 'NONE', #28936, 2.824973347946000413, 0.7853886971611369061 ) ;
#63378 = LINE ( 'NONE', #20742, #20692 ) ;
#63379 = AXIS2_PLACEMENT_3D ( 'NONE', #27044, #5017, #25659 ) ;
#63380 = CARTESIAN_POINT ( 'NONE',  ( 18.17882542849182315, -2.459571230369202333, -12.46089164812839378 ) ) ;
#63381 = CARTESIAN_POINT ( 'NONE',  ( 24.39664322086668946, -3.224866850466631796, 12.03536693359005483 ) ) ;
#63382 = B_SPLINE_CURVE_WITH_KNOTS ( 'NONE', 3,
 ( #42352, #21353, #53520, #47245 ),
 .UNSPECIFIED., .F., .F.,
 ( 4, 4 ),
 ( 0.000000000000000000, 1.000000000000000000 ),
 .UNSPECIFIED. ) ;
#63383 = ORIENTED_EDGE ( 'NONE', *, *, #52838, .F. ) ;
#63384 = DIRECTION ( 'NONE',  ( 1.000000000000000000, 0.000000000000000000, 0.000000000000000000 ) ) ;
#63385 = CARTESIAN_POINT ( 'NONE',  ( 10.93769906950999982, 5.063122007744000008, 4.920829195600999739 ) ) ;
#63386 = DIRECTION ( 'NONE',  ( 0.000000000000000000, -1.000000000000000000, 0.000000000000000000 ) ) ;
#63387 = AXIS2_PLACEMENT_3D ( 'NONE', #2232, #44887, #2566 ) ;
#63388 = CARTESIAN_POINT ( 'NONE',  ( 8.857090631127384484, 4.619515535681817830, 8.304725771527001754 ) ) ;
#63389 = ADVANCED_FACE ( 'NONE', ( #62772 ), #68360, .F. ) ;
#63390 = CARTESIAN_POINT ( 'NONE',  ( 9.983079719591000156, 5.002683760508999988, -8.912673867568997821 ) ) ;
#63391 = CARTESIAN_POINT ( 'NONE',  ( 12.79999999975700042, -11.86189249994999884, 3.298671769835999967 ) ) ;
#63392 = CARTESIAN_POINT ( 'NONE',  ( 11.08752429429999964, -2.871531501602999636, -6.302910744985999791 ) ) ;
#63393 = ORIENTED_EDGE ( 'NONE', *, *, #4016, .F. ) ;
#63394 = EDGE_LOOP ( 'NONE', ( #4022, #62132, #51275, #15895 ) ) ;
#63395 = CIRCLE ( 'NONE', #35524, 1.999999999999999556 ) ;
#63396 = CARTESIAN_POINT ( 'NONE',  ( 11.12921181452999875, 5.272412031865999715, -4.816967985768999760 ) ) ;
#63397 = CARTESIAN_POINT ( 'NONE',  ( 11.64459549376230285, 11.53034370889877813, 1.666360518327090201 ) ) ;
#63398 = LINE ( 'NONE', #15519, #1320 ) ;
#63399 = CARTESIAN_POINT ( 'NONE',  ( 0.1499942179680000265, 2.678379783547567339, -0.7197945678028350169 ) ) ;
#63400 = CARTESIAN_POINT ( 'NONE',  ( 11.72433327354039889, 3.016779570871600313, -6.856888818507299810 ) ) ;
#63401 = CARTESIAN_POINT ( 'NONE',  ( 9.434038493598999153, 4.627468580434300094, -6.901676404381399621 ) ) ;
#63403 = CARTESIAN_POINT ( 'NONE',  ( 8.345403361566443579, 4.924247179573619349, -6.195500497232360182 ) ) ;
#63402 = CARTESIAN_POINT ( 'NONE',  ( 10.58560887879199974, -4.227457260387500249, 8.478317686146800369 ) ) ;
#63404 = CARTESIAN_POINT ( 'NONE',  ( 7.559219638201004621, -3.224407481241000628, 6.403792276147000528 ) ) ;
#63405 = ORIENTED_EDGE ( 'NONE', *, *, #64369, .F. ) ;
#63406 = CARTESIAN_POINT ( 'NONE',  ( 24.30000000000000071, 11.49391741900999975, -4.090215442373000165 ) ) ;
#63407 = CARTESIAN_POINT ( 'NONE',  ( 11.09999999999999964, -5.767038119064999968, 5.145156729235000448 ) ) ;
#63408 = CARTESIAN_POINT ( 'NONE',  ( 9.583051052052001140, 5.255397705012999410, 7.254315263553399618 ) ) ;
#63409 = CARTESIAN_POINT ( 'NONE',  ( 3.999999836924999386, -2.524999836911000273, -2.479015424680000399E-10 ) ) ;
#63410 = CARTESIAN_POINT ( 'NONE',  ( 11.14698053895999941, -5.129799765052999838, 5.886044098803999702 ) ) ;
#63411 = CARTESIAN_POINT ( 'NONE',  ( 18.17920460086783407, 2.538974944925445509, -12.44245230915264955 ) ) ;
#63412 = DIRECTION ( 'NONE',  ( -1.000000000000000000, 0.000000000000000000, 0.000000000000000000 ) ) ;
#63413 = CARTESIAN_POINT ( 'NONE',  ( 15.52628979459880298, -9.187490316955878811, -8.213190486479959418 ) ) ;
#63414 = CARTESIAN_POINT ( 'NONE',  ( 7.974268290630120326, 2.993798921748313635, -6.483333862739654840 ) ) ;
#63415 = CARTESIAN_POINT ( 'NONE',  ( 9.940621437244999470, -3.424116261072899903, -6.851875117168399143 ) ) ;
#63416 = DIRECTION ( 'NONE',  ( -1.000000000000000000, 0.000000000000000000, 0.000000000000000000 ) ) ;
#63417 = CARTESIAN_POINT ( 'NONE',  ( 11.00145247700548268, -4.082536117276985621, 8.370216864706282678 ) ) ;
#63418 = CARTESIAN_POINT ( 'NONE',  ( 0.1499942179680000265, -2.678379783547564674, -0.7197945678028442318 ) ) ;
#63419 = VERTEX_POINT ( 'NONE', #68707 ) ;
#63420 = ADVANCED_FACE ( 'NONE', ( #10673 ), #57190, .T. ) ;
#63421 = ADVANCED_FACE ( 'NONE', ( #31667 ), #41123, .F. ) ;
#63422 = CARTESIAN_POINT ( 'NONE',  ( 12.18107318252211613, -0.04114048977874555646, -12.69993211551499535 ) ) ;
#63423 = CARTESIAN_POINT ( 'NONE',  ( 12.26360295036286452, -2.812350523742413788, -12.37328769147676155 ) ) ;
#63424 = CARTESIAN_POINT ( 'NONE',  ( 24.30000000000000071, 3.224868684338999980, -12.03537377768999939 ) ) ;
#63426 = CARTESIAN_POINT ( 'NONE',  ( 7.325000000000000178, -4.000000000000000000, 9.239711431703000244 ) ) ;
#63425 = VECTOR ( 'NONE', #2202, 1000.000000000000114 ) ;
#63427 = CARTESIAN_POINT ( 'NONE',  ( 10.22963300084732552, 4.176697648610399938, -8.850191834421025305 ) ) ;
#63428 = ORIENTED_EDGE ( 'NONE', *, *, #42141, .F. ) ;
#63429 = CARTESIAN_POINT ( 'NONE',  ( 11.82299956498189886, -5.207010770456999893, 7.825000000000000178 ) ) ;
#63430 = ADVANCED_FACE ( 'NONE', ( #14895 ), #20823, .F. ) ;
#63431 = CARTESIAN_POINT ( 'NONE',  ( 0.000000000000000000, 0.000000000000000000, 0.000000000000000000 ) ) ;
#63432 = CARTESIAN_POINT ( 'NONE',  ( 11.18412378248529926, -4.549028353065900809, -6.461285588983000316 ) ) ;
#63433 = LINE ( 'NONE', #847, #56365 ) ;
#63434 = CARTESIAN_POINT ( 'NONE',  ( 13.46087891924500113, -11.63300053112000043, -2.447944685581000090 ) ) ;
#63435 = CARTESIAN_POINT ( 'NONE',  ( 21.00000012402660232, -1.355091984497000173E-13, 1.088018564133000035E-14 ) ) ;
#63436 = AXIS2_PLACEMENT_3D ( 'NONE', #31305, #42479, #63443 ) ;
#63437 = CYLINDRICAL_SURFACE ( 'NONE', #27330, 0.5000000000000002220 ) ;
#63438 = ORIENTED_EDGE ( 'NONE', *, *, #58166, .F. ) ;
#63439 = CARTESIAN_POINT ( 'NONE',  ( 1.300973465874000201, -3.500000000000000000, 0.000000000000000000 ) ) ;
#63440 = ORIENTED_EDGE ( 'NONE', *, *, #21019, .T. ) ;
#63441 = CARTESIAN_POINT ( 'NONE',  ( 6.960910042590000124, -9.225299970787000703, 5.198333362044999184 ) ) ;
#63442 = CARTESIAN_POINT ( 'NONE',  ( 7.711433059622000208, -5.797088532631000213, 8.340479314546998424 ) ) ;
#63443 = DIRECTION ( 'NONE',  ( 0.000000000000000000, 1.000000000000000000, 0.000000000000000000 ) ) ;
#63444 =( GEOMETRIC_REPRESENTATION_CONTEXT ( 3 ) GLOBAL_UNCERTAINTY_ASSIGNED_CONTEXT ( ( #12704 ) ) GLOBAL_UNIT_ASSIGNED_CONTEXT ( ( #872, #22186, #27797 ) ) REPRESENTATION_CONTEXT ( 'NONE', 'WORKASPACE' ) );
#63445 = ORIENTED_EDGE ( 'NONE', *, *, #60720, .F. ) ;
#63446 = DIRECTION ( 'NONE',  ( -1.000000000000000000, 0.000000000000000000, 0.000000000000000000 ) ) ;
#63447 = CARTESIAN_POINT ( 'NONE',  ( 8.228079719590001062, 5.311932732455999506, -8.353077699453999472 ) ) ;
#63448 = CARTESIAN_POINT ( 'NONE',  ( 25.60000000000000142, -2.258942858049999725, 10.99402034467349232 ) ) ;
#63449 = CARTESIAN_POINT ( 'NONE',  ( 8.154573290672269437, -3.060691178947356761, 6.318599490783953776 ) ) ;
#63450 = ORIENTED_EDGE ( 'NONE', *, *, #8547, .F. ) ;
#63451 = CARTESIAN_POINT ( 'NONE',  ( 9.228135700785001561, -2.875364528161000077, 8.669943154892999715 ) ) ;
#63452 = CARTESIAN_POINT ( 'NONE',  ( 11.09999999999999964, 2.700000000000000178, -6.461133846875999787 ) ) ;
#63453 = CARTESIAN_POINT ( 'NONE',  ( 12.10004069261200677, 11.60802777289553411, -4.146429405016670344 ) ) ;
#63454 = ORIENTED_EDGE ( 'NONE', *, *, #1654, .T. ) ;
#63455 = DIRECTION ( 'NONE',  ( 0.000000000000000000, 1.000000000000000000, 0.000000000000000000 ) ) ;
#63456 = ORIENTED_EDGE ( 'NONE', *, *, #10275, .F. ) ;
#63457 = DIRECTION ( 'NONE',  ( -1.000000000000000000, 0.000000000000000000, -1.233561263588000078E-14 ) ) ;
#63458 = CARTESIAN_POINT ( 'NONE',  ( 24.13789454551274005, 12.48572713186856831, -3.365239671874099781 ) ) ;
#63459 = CARTESIAN_POINT ( 'NONE',  ( 5.445382378960999858, -0.1840109337218999719, 1.546599278641000108 ) ) ;
#63460 = CARTESIAN_POINT ( 'NONE',  ( 5.146693173016833711, -1.310679582531386611, -0.7554284705563495406 ) ) ;
#63461 = CARTESIAN_POINT ( 'NONE',  ( 10.14393020684899938, 5.250000000000000000, 7.500000000000000000 ) ) ;
#63462 = CARTESIAN_POINT ( 'NONE',  ( 24.26287088544855308, 12.27454670750946697, 3.288953945731635464 ) ) ;
#63463 = DIRECTION ( 'NONE',  ( 1.000000000000000000, 0.000000000000000000, 3.552713678810000077E-14 ) ) ;
#63464 = ORIENTED_EDGE ( 'NONE', *, *, #66781, .F. ) ;
#63465 = CARTESIAN_POINT ( 'NONE',  ( 7.874998340266000874, -5.143395304206999974, 6.784086671025002069 ) ) ;
#63466 = VERTEX_POINT ( 'NONE', #30633 ) ;
#63467 = CARTESIAN_POINT ( 'NONE',  ( 10.33536974457000035, 5.153692264686000613, 8.830864265869999841 ) ) ;
#63468 = CARTESIAN_POINT ( 'NONE',  ( 4.400000000000000355, 1.266759534686000110, 0.8033182938792000627 ) ) ;
#63469 = DIRECTION ( 'NONE',  ( 1.000000000000000000, 0.000000000000000000, 0.000000000000000000 ) ) ;
#63470 = CARTESIAN_POINT ( 'NONE',  ( 12.34612353109747573, 2.075598726024749929, -13.75436385846648157 ) ) ;
#63471 = CARTESIAN_POINT ( 'NONE',  ( 10.36409408021999923, -4.600000090830000943, -4.954046131267999087 ) ) ;
#63472 = CARTESIAN_POINT ( 'NONE',  ( 12.80000000000000071, 11.23412379136000006, -3.084957477885999833 ) ) ;
#63473 = EDGE_CURVE ( 'NONE', #43200, #23962, #42160, .T. ) ;
#63474 = CARTESIAN_POINT ( 'NONE',  ( 18.01189197849806334, -0.4270206790917105422, 13.89118144889039286 ) ) ;
#63475 = VECTOR ( 'NONE', #59522, 1000.000000000000000 ) ;
#63476 = CARTESIAN_POINT ( 'NONE',  ( 9.375307864587574258, -5.578557532607083758, -8.254778991542760735 ) ) ;
#63477 = VERTEX_POINT ( 'NONE', #4042 ) ;
#63478 = EDGE_CURVE ( 'NONE', #11589, #27875, #15584, .T. ) ;
#63479 = AXIS2_PLACEMENT_3D ( 'NONE', #4599, #25935, #394 ) ;
#63480 = CARTESIAN_POINT ( 'NONE',  ( 12.53679426224900162, -11.40784081139999984, 4.532785132108998916 ) ) ;
#63481 = CARTESIAN_POINT ( 'NONE',  ( 11.65810538575740019, -2.757018958839999812, 7.797177576385699638 ) ) ;
#63482 = CARTESIAN_POINT ( 'NONE',  ( 3.071806799211250549, 3.408904368339104263, 0.9161175952574878156 ) ) ;
#63483 = CARTESIAN_POINT ( 'NONE',  ( 17.59542397721386209, -0.6249999999999998890, -13.88107975724990695 ) ) ;
#63484 = CARTESIAN_POINT ( 'NONE',  ( 7.769581853207999877, -2.431397064767999439, 7.958394431095000776 ) ) ;
#63486 = CARTESIAN_POINT ( 'NONE',  ( 13.63331750507211559, 9.617283495289667528, 7.919506078536236338 ) ) ;
#63485 = CARTESIAN_POINT ( 'NONE',  ( 9.758140238852000437, 2.901378080241999946, 6.555076849497999625 ) ) ;
#63487 = CARTESIAN_POINT ( 'NONE',  ( 11.62579573085663043, 5.239377455231000624, -7.714452430741599365 ) ) ;
#63488 = B_SPLINE_CURVE_WITH_KNOTS ( 'NONE', 3,
 ( #4665, #15169, #42770, #53605 ),
 .UNSPECIFIED., .F., .F.,
 ( 4, 4 ),
 ( 0.000000000000000000, 1.000000000000000000 ),
 .UNSPECIFIED. ) ;
#63489 = CARTESIAN_POINT ( 'NONE',  ( 10.47253786429000044, -2.899999999999999911, -6.571291218949999902 ) ) ;
#63490 = CARTESIAN_POINT ( 'NONE',  ( 9.222405316139999698, 3.815922504313999930, -8.347244604637999998 ) ) ;
#63491 = CARTESIAN_POINT ( 'NONE',  ( 18.24552617758596540, 0.2196334679052291683, 12.59809060309703277 ) ) ;
#63492 = B_SPLINE_SURFACE_WITH_KNOTS ( 'NONE', 3, 3, ( 
 ( #35482, #50521, #67611, #57133 ),
 ( #56803, #7874, #51544, #2621 ),
 ( #13811, #50867, #9230, #24293 ),
 ( #62380, #8217, #45630, #62039 ),
 ( #46657, #25319, #29906, #3640 ),
 ( #8900, #24977, #45962, #29210 ),
 ( #51211, #46310, #40372, #2964 ),
 ( #19738, #30239, #67962, #30569 ),
 ( #13475, #66934, #41060, #35142 ),
 ( #56106, #34795, #3307, #29565 ) ),
 .UNSPECIFIED., .F., .F., .F.,
 ( 4, 1, 1, 1, 1, 1, 1, 4 ),
 ( 4, 4 ),
 ( 0.04183311431307000505, 0.1428571428570999946, 0.2857142857143000203, 0.4285714285713999594, 0.5714285714286000406, 0.7142857142856999797, 0.8571428571429000609, 0.9292981235707000742 ),
 ( -0.1917799910644999994, 1.191756862851000021 ),
 .UNSPECIFIED. ) ;
#63493 = CARTESIAN_POINT ( 'NONE',  ( 6.861617155770999510, -0.3226229809382999969, -1.231632514461999950 ) ) ;
#63494 = CARTESIAN_POINT ( 'NONE',  ( 24.32785187986800324, 9.022984283431000563, 9.340288652106000455 ) ) ;
#63495 = ORIENTED_EDGE ( 'NONE', *, *, #8016, .F. ) ;
#63496 = CARTESIAN_POINT ( 'NONE',  ( 9.475897313459000770, -4.122021308488999836, 9.013573548576999883 ) ) ;
#63497 = CARTESIAN_POINT ( 'NONE',  ( 9.658629719592001450, 5.496789211521000418, -7.043125396300999874 ) ) ;
#63498 = CARTESIAN_POINT ( 'NONE',  ( 17.78978190923676550, 3.208919636066285719, 13.62728338959921359 ) ) ;
#63499 = PLANE ( 'NONE',  #4340 ) ;
#63500 = B_SPLINE_CURVE_WITH_KNOTS ( 'NONE', 3,
 ( #24277, #56787, #19720, #46640 ),
 .UNSPECIFIED., .F., .F.,
 ( 4, 4 ),
 ( 0.000000000000000000, 1.000000000000000000 ),
 .UNSPECIFIED. ) ;
#63501 = EDGE_LOOP ( 'NONE', ( #40485, #33116, #15167, #40343, #36223, #37292 ) ) ;
#63502 = AXIS2_PLACEMENT_3D ( 'NONE', #15928, #63469, #19806 ) ;
#63503 = FACE_OUTER_BOUND ( 'NONE', #43350, .T. ) ;
#63504 = CARTESIAN_POINT ( 'NONE',  ( 10.60746886766490071, 3.501664543805500074, 8.405426684175299812 ) ) ;
#63505 = CARTESIAN_POINT ( 'NONE',  ( 10.54684221959000112, 3.691673619534999951, -9.157283848447001162 ) ) ;
#63506 = ORIENTED_EDGE ( 'NONE', *, *, #57773, .F. ) ;
#63507 = ADVANCED_FACE ( 'NONE', ( #36217 ), #36410, .T. ) ;
#63508 = EDGE_CURVE ( 'NONE', #54024, #60220, #4390, .T. ) ;
#63509 = PLANE ( 'NONE',  #68534 ) ;
#63510 = CARTESIAN_POINT ( 'NONE',  ( -15.86200481174999943, 2.399999999999999911, -6.571291218949999902 ) ) ;
#63511 = CARTESIAN_POINT ( 'NONE',  ( 11.30579707368350029, 3.365167912142600137, 8.609190966793999422 ) ) ;
#63512 = CARTESIAN_POINT ( 'NONE',  ( 5.695281798973955034, 12.04221271193345189, 3.723442287067866729 ) ) ;
#63513 = CARTESIAN_POINT ( 'NONE',  ( 8.400073341230999802, 2.800103557244999930, 9.079946116129001155 ) ) ;
#63514 = ORIENTED_EDGE ( 'NONE', *, *, #6125, .T. ) ;
#63515 = FACE_OUTER_BOUND ( 'NONE', #11998, .T. ) ;
#63516 = EDGE_CURVE ( 'NONE', #62306, #30294, #20494, .T. ) ;
#63517 = EDGE_CURVE ( 'NONE', #25932, #20015, #39819, .T. ) ;
#63518 = B_SPLINE_CURVE_WITH_KNOTS ( 'NONE', 3,
 ( #39573, #33296, #54612, #60897 ),
 .UNSPECIFIED., .F., .F.,
 ( 4, 4 ),
 ( 0.000000000000000000, 1.000000000000000000 ),
 .UNSPECIFIED. ) ;
#63519 = CARTESIAN_POINT ( 'NONE',  ( 8.502804719591001259, 4.586183217919999500, -9.013777652867000612 ) ) ;
#63520 = CARTESIAN_POINT ( 'NONE',  ( 8.127481833579825121, -5.069078398454679224, 6.127575109768734762 ) ) ;
#63521 = CARTESIAN_POINT ( 'NONE',  ( 9.016151519676999015, -3.972335373863620234, 6.221087886525999089 ) ) ;
#63522 = ORIENTED_EDGE ( 'NONE', *, *, #21002, .T. ) ;
#63523 = CARTESIAN_POINT ( 'NONE',  ( 16.39967273502900014, -3.641490841173999904, -12.02437761214999945 ) ) ;
#63524 = B_SPLINE_CURVE_WITH_KNOTS ( 'NONE', 3,
 ( #1942, #23261, #12429, #29562, #28162, #39341, #60662, #33760 ),
 .UNSPECIFIED., .F., .F.,
 ( 4, 2, 2, 4 ),
 ( 0.000000000000000000, 0.2500000000000002220, 0.5000000000000004441, 1.000000000000000000 ),
 .UNSPECIFIED. ) ;
#63525 = CARTESIAN_POINT ( 'NONE',  ( 11.48394322905000031, 11.59615457572999908, 1.579582225534999829 ) ) ;
#63526 = ORIENTED_EDGE ( 'NONE', *, *, #56537, .F. ) ;
#63527 = CARTESIAN_POINT ( 'NONE',  ( 16.09997386696500143, -7.697446472043792731, -8.794756076490951813 ) ) ;
#63528 = PLANE ( 'NONE',  #66949 ) ;
#63529 = FACE_OUTER_BOUND ( 'NONE', #66293, .T. ) ;
#63530 = B_SPLINE_CURVE_WITH_KNOTS ( 'NONE', 3,
 ( #19991, #68204, #20323, #51115, #57041, #41650, #45871, #15081, #67179, #62620, #57723, #14742, #9831, #19293 ),
 .UNSPECIFIED., .F., .F.,
 ( 4, 2, 2, 2, 2, 2, 4 ),
 ( 0.000000000000000000, 0.1249999999999997502, 0.2499999999999995004, 0.4999999999999976685, 0.6249999999999990008, 0.7500000000000002220, 1.000000000000000000 ),
 .UNSPECIFIED. ) ;
#63531 = CARTESIAN_POINT ( 'NONE',  ( 7.773264358664000007, -2.859518314699000197, 6.768377407145999669 ) ) ;
#63532 = CARTESIAN_POINT ( 'NONE',  ( 9.764473719840861321, -3.575759230362629104, -8.840579835172658107 ) ) ;
#63533 = AXIS2_PLACEMENT_3D ( 'NONE', #40038, #56102, #8211 ) ;
#63534 = CARTESIAN_POINT ( 'NONE',  ( 11.64122412107036908, 4.062069863985690255, -6.326756392227999015 ) ) ;
#63535 = CARTESIAN_POINT ( 'NONE',  ( 11.38813259637009878, -5.155817667926999803, 6.870201387206400057 ) ) ;
#63536 = CARTESIAN_POINT ( 'NONE',  ( 8.751262507007865565, -5.414309366961505887, 8.580389789711265536 ) ) ;
#63537 = CARTESIAN_POINT ( 'NONE',  ( 11.71149010443640037, -2.862435565199000109, 7.414927836855409460 ) ) ;
#63538 = VERTEX_POINT ( 'NONE', #38276 ) ;
#63539 = CARTESIAN_POINT ( 'NONE',  ( 7.101301658771000724, 3.554857159507999853, 8.889479859586000288 ) ) ;
#63540 = EDGE_CURVE ( 'NONE', #13916, #35486, #60671, .T. ) ;
#63541 = ORIENTED_EDGE ( 'NONE', *, *, #67079, .F. ) ;
#63542 = FACE_OUTER_BOUND ( 'NONE', #33789, .T. ) ;
#63543 = CARTESIAN_POINT ( 'NONE',  ( 9.316120559621998254, -3.677416446733000388, 9.250734868033999803 ) ) ;
#63544 = LINE ( 'NONE', #25454, #26793 ) ;
#63545 = EDGE_LOOP ( 'NONE', ( #17980, #14179, #28651, #9362, #56446 ) ) ;
#63546 = CARTESIAN_POINT ( 'NONE',  ( 12.22009801487426550, -2.720357631080354999, -12.39749406087475947 ) ) ;
#63547 = CARTESIAN_POINT ( 'NONE',  ( 10.91914189278999636, 8.255337631213995664, -7.037376568592996762 ) ) ;
#63548 = CARTESIAN_POINT ( 'NONE',  ( 7.921841810112000282, 2.875629839593000003, -6.725486766668000271 ) ) ;
#63549 = CARTESIAN_POINT ( 'NONE',  ( 10.72726354018300121, 4.629523725463627670, 8.592232985442818105 ) ) ;
#63550 = CARTESIAN_POINT ( 'NONE',  ( 12.22752497338540145, -2.076440593937393775, -13.84516123709150826 ) ) ;
#63551 = CARTESIAN_POINT ( 'NONE',  ( 11.53564291764652872, -4.995889373412399692, -7.376893506359599506 ) ) ;
#63552 = CARTESIAN_POINT ( 'NONE',  ( 7.090737316147470715, 0.3434952630163173315, -1.274854790665578941 ) ) ;
#63553 = CARTESIAN_POINT ( 'NONE',  ( 18.25703273071139421, -2.298329627318190571, 12.38863175403534989 ) ) ;
#63554 = ORIENTED_EDGE ( 'NONE', *, *, #27708, .T. ) ;
#63555 = EDGE_LOOP ( 'NONE', ( #25986, #2219, #4704, #51844 ) ) ;
#63556 = DIRECTION ( 'NONE',  ( 0.000000000000000000, 0.000000000000000000, 1.000000000000000000 ) ) ;
#63557 = FACE_BOUND ( 'NONE', #6342, .T. ) ;
#63558 = CARTESIAN_POINT ( 'NONE',  ( 12.80505043854144276, -0.6250000000000001110, -13.88107975066922428 ) ) ;
#63559 = CARTESIAN_POINT ( 'NONE',  ( 9.922184613163000932, 3.489926301007000298, -9.111807643819000546 ) ) ;
#63560 = CARTESIAN_POINT ( 'NONE',  ( 18.19991693152165979, 3.160411602603945269, -11.91446363486501703 ) ) ;
#63561 = ADVANCED_FACE ( 'NONE', ( #48773 ), #42725, .F. ) ;
#63562 = CARTESIAN_POINT ( 'NONE',  ( 17.55505043854143565, 1.875000000000000000, -12.57545641911172751 ) ) ;
#63563 = CARTESIAN_POINT ( 'NONE',  ( 7.805976048735002948, 2.918573024645998881, -6.499545638216004839 ) ) ;
#63564 = CARTESIAN_POINT ( 'NONE',  ( 9.972537864286000087, 2.899999999999999911, -6.571291218949999902 ) ) ;
#63565 = VERTEX_POINT ( 'NONE', #16608 ) ;
#63566 = EDGE_CURVE ( 'NONE', #38268, #14826, #54043, .T. ) ;
#63567 = CARTESIAN_POINT ( 'NONE',  ( 10.32322131289000033, -4.654255525074000310, -4.621083567265000802 ) ) ;
#63568 = ORIENTED_EDGE ( 'NONE', *, *, #534, .T. ) ;
#63569 = CARTESIAN_POINT ( 'NONE',  ( 9.843732751558000871, 4.115124343450999866, 9.466620196856998959 ) ) ;
#63570 = CARTESIAN_POINT ( 'NONE',  ( 8.741151519676998660, -3.981249765141819719, -8.366807394121199337 ) ) ;
#63571 = CARTESIAN_POINT ( 'NONE',  ( 9.576488281553999116, 4.593976206186999534, 5.662041230125000268 ) ) ;
#63572 = CARTESIAN_POINT ( 'NONE',  ( 11.27879632507499963, -3.576455950783300253, 6.714825466131699727 ) ) ;
#63573 = CARTESIAN_POINT ( 'NONE',  ( 10.16426084122999995, 4.808846957865000604, -8.639578604182998944 ) ) ;
#63574 = CARTESIAN_POINT ( 'NONE',  ( 11.53979707368350027, 3.569730287184500472, -6.748224392138099326 ) ) ;
#63575 = CARTESIAN_POINT ( 'NONE',  ( 24.69899870589400237, 8.733950678133000523, 9.243023888125000198 ) ) ;
#63576 = CARTESIAN_POINT ( 'NONE',  ( 12.66237550623657171, -0.6088395004560435142, 12.68034807294329269 ) ) ;
#63577 = CARTESIAN_POINT ( 'NONE',  ( 11.59999999999999964, 3.137911629819546189, -7.912526219123482640 ) ) ;
#63578 = CARTESIAN_POINT ( 'NONE',  ( 10.62697636434999993, 3.142921793056999924, 8.668445734229999644 ) ) ;
#63579 = CARTESIAN_POINT ( 'NONE',  ( 11.44749694427000186, -3.679776032594999968, 11.11060924501999914 ) ) ;
#63580 = ORIENTED_EDGE ( 'NONE', *, *, #46793, .T. ) ;
#63581 = CARTESIAN_POINT ( 'NONE',  ( 8.639360841228999277, 5.074768364528000397, -8.296267706722000312 ) ) ;
#63582 = CARTESIAN_POINT ( 'NONE',  ( 7.028203291589999679, 0.2006192615549000080, -1.234405135879000026 ) ) ;
#63583 = CARTESIAN_POINT ( 'NONE',  ( 17.69888641710118549, 1.891428316105117746, 13.78380564104364936 ) ) ;
#63584 = CARTESIAN_POINT ( 'NONE',  ( 3.396238944115833824, 0.8916813559738958617, -3.415138845704721149 ) ) ;
#63585 = DIRECTION ( 'NONE',  ( 0.000000000000000000, 0.8445063564576198445, 0.5355455292528128464 ) ) ;
#63586 = CARTESIAN_POINT ( 'NONE',  ( 11.58071932425156980, -4.167269912168199753, -8.628410767520000135 ) ) ;
#63587 = VERTEX_POINT ( 'NONE', #2262 ) ;
#63588 = CARTESIAN_POINT ( 'NONE',  ( 5.601974509046187656, -12.13172069192463987, 3.749825701181730420 ) ) ;
#63589 = FACE_OUTER_BOUND ( 'NONE', #52378, .T. ) ;
#63591 = DIRECTION ( 'NONE',  ( 0.000000000000000000, 0.8684118361392316743, -0.4958436072526178351 ) ) ;
#63590 = CARTESIAN_POINT ( 'NONE',  ( 9.111654719595000174, 4.989193221215000307, -6.287302145481000082 ) ) ;
#63592 = CARTESIAN_POINT ( 'NONE',  ( 15.89994436294300151, 8.847904542234999781, 8.580301953175000662 ) ) ;
#63593 = ORIENTED_EDGE ( 'NONE', *, *, #23348, .F. ) ;
#63594 = CARTESIAN_POINT ( 'NONE',  ( 10.87148757351999961, 5.567567343464999929, 7.772413227960999649 ) ) ;
#63595 = CARTESIAN_POINT ( 'NONE',  ( 18.14022514731439628, -2.720460039646586115, -13.62418930002215589 ) ) ;
#63596 = CARTESIAN_POINT ( 'NONE',  ( 10.48133997687999930, 4.184599793140999502, 8.346298710230199092 ) ) ;
#63597 = CARTESIAN_POINT ( 'NONE',  ( 24.69611861387416951, -11.79505474561326039, 3.190916355391951509 ) ) ;
#63598 = CARTESIAN_POINT ( 'NONE',  ( 7.358058059621999547, -4.561648098548999997, 6.153050355516999304 ) ) ;
#63599 = VERTEX_POINT ( 'NONE', #14731 ) ;
#63600 = CARTESIAN_POINT ( 'NONE',  ( 9.149954719592001240, 4.175915362023999933, 5.699506188181000077 ) ) ;
#63601 = B_SPLINE_CURVE_WITH_KNOTS ( 'NONE', 3,
 ( #50568, #34842, #56153, #8261, #24342, #31650, #37234, #48069, #47041, #32004, #42483, #31309, #41791, #68694, #69047, #20808, #26755, #173 ),
 .UNSPECIFIED., .F., .F.,
 ( 4, 2, 2, 2, 2, 2, 2, 2, 4 ),
 ( 0.000000000000000000, 0.1250000000000000000, 0.2500000000000000000, 0.3750000000000000000, 0.5000000000000000000, 0.6250000000000000000, 0.7500000000000000000, 0.8750000000000000000, 1.000000000000000000 ),
 .UNSPECIFIED. ) ;
#63602 = EDGE_CURVE ( 'NONE', #31811, #52040, #39667, .T. ) ;
#63603 = EDGE_CURVE ( 'NONE', #61665, #57654, #9468, .T. ) ;
#63605 = DIRECTION ( 'NONE',  ( 0.000000000000000000, 0.000000000000000000, -1.000000000000000000 ) ) ;
#63604 = DIRECTION ( 'NONE',  ( 0.000000000000000000, -0.8648648648648720183, -0.5020047465136825426 ) ) ;
#63606 = CONICAL_SURFACE ( 'NONE', #30148, 13.04999927352999833, 0.7853981075146502233 ) ;
#63607 = CARTESIAN_POINT ( 'NONE',  ( 7.467982099739825408, -2.305963387369412754, 7.104575083399867097 ) ) ;
#63608 = CARTESIAN_POINT ( 'NONE',  ( 18.10291897062741029, -0.3009486141072659215, 13.89561788111045182 ) ) ;
#63609 = CARTESIAN_POINT ( 'NONE',  ( 1.070927120944999755, -3.140063525497999830, -0.8725182546194000244 ) ) ;
#63610 = EDGE_LOOP ( 'NONE', ( #3289, #5999, #36352, #56401 ) ) ;
#63611 = CARTESIAN_POINT ( 'NONE',  ( 9.623096873515669003, 5.217465845835395299, -7.827184855449101697 ) ) ;
#63612 = CARTESIAN_POINT ( 'NONE',  ( 11.29718447801629999, -2.996774412198000448, 7.522119512433738997 ) ) ;
#63613 = CARTESIAN_POINT ( 'NONE',  ( 9.687870098586998324, 5.912263966150999472, 7.772301113561999486 ) ) ;
#63614 = CARTESIAN_POINT ( 'NONE',  ( 10.40333997687999990, 4.213854445120500003, 8.480416814141699788 ) ) ;
#63615 = ORIENTED_EDGE ( 'NONE', *, *, #8365, .T. ) ;
#63616 = B_SPLINE_CURVE_WITH_KNOTS ( 'NONE', 3,
 ( #27433, #27093, #21488, #22517 ),
 .UNSPECIFIED., .F., .F.,
 ( 4, 4 ),
 ( 0.000000000000000000, 1.000000000000000000 ),
 .UNSPECIFIED. ) ;
#63617 = CARTESIAN_POINT ( 'NONE',  ( 24.13225220766125645, -3.329780019911785960, 12.50570657898502702 ) ) ;
#63618 = CARTESIAN_POINT ( 'NONE',  ( 24.30001696810800027, 12.21047201856000086, 3.271805692349999628 ) ) ;
#63619 = CARTESIAN_POINT ( 'NONE',  ( 11.18546886766499959, -4.566506264294200257, 8.529286361367999447 ) ) ;
#63620 = EDGE_CURVE ( 'NONE', #21235, #52300, #34868, .T. ) ;
#63621 = CARTESIAN_POINT ( 'NONE',  ( 24.60115017431256490, -12.20856115934854635, -3.061105476207797160 ) ) ;
#63622 = CARTESIAN_POINT ( 'NONE',  ( 18.24299778933912819, -2.286486205740230204, 13.81204233372298340 ) ) ;
#63623 = CARTESIAN_POINT ( 'NONE',  ( 25.34480285809352296, -8.474813500079264372, -7.997915891567656033 ) ) ;
#63624 = ORIENTED_EDGE ( 'NONE', *, *, #28020, .T. ) ;
#63625 = DIRECTION ( 'NONE',  ( -1.000000000000000000, 0.000000000000000000, 0.000000000000000000 ) ) ;
#63626 = B_SPLINE_CURVE_WITH_KNOTS ( 'NONE', 3,
 ( #27992, #61523, #60835, #66069, #39165, #39862, #34275, #60488, #49652, #8040, #18879, #12598, #55595, #28330, #34625, #1757, #50348, #33925 ),
 .UNSPECIFIED., .F., .F.,
 ( 4, 2, 2, 2, 2, 2, 2, 2, 4 ),
 ( 0.000000000000000000, 0.1250000000000000000, 0.2500000000000000000, 0.3750000000000000000, 0.5000000000000000000, 0.6250000000000000000, 0.7500000000000000000, 0.8750000000000000000, 1.000000000000000000 ),
 .UNSPECIFIED. ) ;
#63627 = DIRECTION ( 'NONE',  ( 0.000000000000000000, 0.000000000000000000, -1.000000000000000000 ) ) ;
#63628 = ORIENTED_EDGE ( 'NONE', *, *, #66295, .T. ) ;
#63629 = CARTESIAN_POINT ( 'NONE',  ( 11.06795257254739973, 3.036453385827900142, 7.219770138693499817 ) ) ;
#63630 = DIRECTION ( 'NONE',  ( 0.000000000000000000, -0.7198977633595244896, -0.6940801180771239975 ) ) ;
#63631 = CARTESIAN_POINT ( 'NONE',  ( 11.10062015617000064, 3.093053541899000169, -6.153678467293999255 ) ) ;
#63632 = CARTESIAN_POINT ( 'NONE',  ( 7.903774407030003779, 5.139635483293002238, 6.776036904885998524 ) ) ;
#63633 = CARTESIAN_POINT ( 'NONE',  ( 9.260912867475999732, -4.901383038209000453, 9.090314591495999963 ) ) ;
#63634 = CARTESIAN_POINT ( 'NONE',  ( 18.05961319350869232, -0.5166535389540217738, -12.58940585649086508 ) ) ;
#63635 = CARTESIAN_POINT ( 'NONE',  ( 9.040001050027107965, 4.926961961734873441, 8.481263526778137773 ) ) ;
#63636 = CARTESIAN_POINT ( 'NONE',  ( 10.25564828895399927, -3.119330945648699949, -7.981013126389099099 ) ) ;
#63637 = CARTESIAN_POINT ( 'NONE',  ( 7.481079719589999399, 2.374037589774999901, 8.293392681990997772 ) ) ;
#63638 = EDGE_LOOP ( 'NONE', ( #21821, #66891, #58881, #8147, #59510, #13373 ) ) ;
#63639 = CARTESIAN_POINT ( 'NONE',  ( 11.10391045180383962, 5.129049487418003928, 6.885461205208883051 ) ) ;
#63640 = CARTESIAN_POINT ( 'NONE',  ( 11.09999999999999964, 5.299316147296000423, -5.124965750789000296 ) ) ;
#63641 = CARTESIAN_POINT ( 'NONE',  ( 10.27934687351620724, -4.163624617374463988, -6.249999999999999112 ) ) ;
#63642 = CARTESIAN_POINT ( 'NONE',  ( 11.48791672854001433, 9.860991908751987722, 5.543179905927000384 ) ) ;
#63643 = CARTESIAN_POINT ( 'NONE',  ( 11.43330331963142044, -3.865571928678541269, 11.84352938576710734 ) ) ;
#63644 = CARTESIAN_POINT ( 'NONE',  ( 10.90070920260000165, 9.357678590204999480, 6.160837872949999294 ) ) ;
#63645 = EDGE_CURVE ( 'NONE', #58173, #26251, #67344, .T. ) ;
#63646 = CARTESIAN_POINT ( 'NONE',  ( 10.90000000000000036, 0.2999999999999999889, -4.902439024389999567 ) ) ;
#63647 = CARTESIAN_POINT ( 'NONE',  ( 9.210288521113000115, -4.352953559891299840, 6.715449042252499723 ) ) ;
#63648 = ORIENTED_EDGE ( 'NONE', *, *, #17757, .F. ) ;
#63649 = CARTESIAN_POINT ( 'NONE',  ( 24.43232361759900328, 8.806075257782000065, 8.751960807121999864 ) ) ;
#63650 = CARTESIAN_POINT ( 'NONE',  ( 9.279101285863998072, -4.823683599683300294, -6.521261160937499746 ) ) ;
#63651 = DIRECTION ( 'NONE',  ( 2.888199747633069555E-10, 0.5897878662160149776, 0.8075582163933199276 ) ) ;
#63652 = VECTOR ( 'NONE', #511, 999.9999999999998863 ) ;
#63653 = CARTESIAN_POINT ( 'NONE',  ( 9.571967469951999874, -4.084684048989999816, 8.946621592834999248 ) ) ;
#63654 = CARTESIAN_POINT ( 'NONE',  ( 12.03979707368350027, -4.430269712815499972, 8.251775607861899786 ) ) ;
#63655 = B_SPLINE_SURFACE_WITH_KNOTS ( 'NONE', 3, 3, ( 
 ( #37679, #27198, #54449, #39067, #55142, #7245, #277, #43972, #16351, #60388, #65276, #28230, #49545, #22626, #59693, #17747, #33480, #1658, #22974, #21935, #60040, #17390, #38720, #64234, #43273, #42929, #32787, #59009, #44324, #65622, #11794, #1311, #22286, #43627, #11111 ),
 ( #12492, #64921, #49204, #33827, #32446, #12152, #5857, #53760, #48517, #54795, #626, #64581, #16691, #38019, #59346, #11446, #54102, #6197, #17036, #33134, #6550, #27892, #34171, #56174, #66999, #61079, #24360, #2347, #29628, #3368, #56517, #45005, #8962, #61757, #24706 ),
 ( #7590, #67335, #45692, #19455, #13199, #50931, #23329, #39760, #2691, #55491, #55836, #40431, #29971, #19109, #56865, #44669, #50590, #13876, #35207, #8623, #65963, #51274, #18779, #7940, #46028, #3030, #61422, #34526, #40776, #62100, #8284, #14219, #35547, #66311, #23667 ),
 ( #49897, #18435, #66660, #29276, #24016, #2006, #18088, #45350, #40110, #13540, #34859, #39409, #60730, #12844, #28940, #50243, #14900, #36224, #4047, #42503, #31329, #47407, #52641, #57538, #30990, #68026, #58233, #63118, #5089, #25730, #15588, #4734, #52993, #36567, #26425 ) ),
 .UNSPECIFIED., .F., .F., .F.,
 ( 4, 4 ),
 ( 4, 1, 1, 1, 1, 1, 1, 1, 1, 1, 1, 1, 1, 1, 1, 1, 1, 1, 1, 1, 1, 1, 1, 1, 1, 1, 1, 1, 1, 1, 1, 1, 4 ),
 ( -0.02000000000000000042, 1.020000000000000018 ),
 ( 0.1633025096610999927, 0.1899619885200000136, 0.2166214673788000034, 0.2432809462376999965, 0.2699404250964999585, 0.2965999039553000038, 0.3232593828141999692, 0.3499188616730000145, 0.3765783405318000043, 0.4032378193906999697, 0.4298972982494999595, 0.4565567771083000048, 0.4832162559671999702, 0.5098757348260000155, 0.5365352136848999809, 0.5631946925437000262, 0.5898541714025000715, 0.6165136502614000369, 0.6431731291201999712, 0.6698326079790000165, 0.6964920868378999819, 0.7231515656967000272, 0.7498110445554999615, 0.7764705234143999268, 0.8031300022731999722, 0.8297894811320000175, 0.8564489599908999828, 0.8831084388497000282, 0.9097679177085999935, 0.9364273965674000388, 0.9630868754261999731, 0.9897463542851000495, 1.016405833144000015 ),
 .UNSPECIFIED. ) ;
#63656 = CARTESIAN_POINT ( 'NONE',  ( 12.71024088650322525, 0.7135009822674867053, 12.57978225961208807 ) ) ;
#63657 = CARTESIAN_POINT ( 'NONE',  ( 21.65000086032551252, 3.970157536060000036E-13, -13.94999929344982448 ) ) ;
#63658 = CARTESIAN_POINT ( 'NONE',  ( 8.817462135714999150, 5.100000000000000533, 6.571291218949999902 ) ) ;
#63659 = CARTESIAN_POINT ( 'NONE',  ( 12.08628615590296995, 2.575951425301598263, 12.33388065128748323 ) ) ;
#63660 = CARTESIAN_POINT ( 'NONE',  ( 10.16360887879199915, 3.741427262966100287, -6.387851364408000165 ) ) ;
#63661 = CARTESIAN_POINT ( 'NONE',  ( 11.41256651104150066, 4.098999650273559503, -6.501426055769400136 ) ) ;
#63662 = CARTESIAN_POINT ( 'NONE',  ( 25.59997324745700098, 8.218963665694001719, 8.043524865688999270 ) ) ;
#63663 = CARTESIAN_POINT ( 'NONE',  ( 10.69829221958999987, 2.534027248431999890, -6.667786804432999759 ) ) ;
#63664 = CARTESIAN_POINT ( 'NONE',  ( 9.909254614703000286, 2.760277452415999644, -7.815392442832299835 ) ) ;
#63666 = CARTESIAN_POINT ( 'NONE',  ( 11.09999233421999953, -1.199999999999999956, -9.776630298829998011 ) ) ;
#63665 = CARTESIAN_POINT ( 'NONE',  ( 15.35917414208899956, -8.811049802147000065, -7.563839685023999948 ) ) ;
#63667 = CARTESIAN_POINT ( 'NONE',  ( 8.971882233721794719, 5.348858080848509999, 7.441238387768498441 ) ) ;
#63668 = ORIENTED_EDGE ( 'NONE', *, *, #29465, .F. ) ;
#63669 = DIRECTION ( 'NONE',  ( 0.000000000000000000, -0.7071067811864953923, -0.7071067811865995312 ) ) ;
#63670 = CARTESIAN_POINT ( 'NONE',  ( 15.90000000000314451, 3.738168175168965046, 11.41174933108808176 ) ) ;
#63671 = CARTESIAN_POINT ( 'NONE',  ( 10.75110221171000013, -2.822135527917999820, 6.655890318096999714 ) ) ;
#63672 = CARTESIAN_POINT ( 'NONE',  ( 8.920468108405998464, 4.966402032527499344, 7.226304214866999587 ) ) ;
#63673 = B_SPLINE_CURVE_WITH_KNOTS ( 'NONE', 3,
 ( #44557, #65849, #17973, #23898, #28820, #6775, #66538, #18658, #39991, #39292 ),
 .UNSPECIFIED., .F., .F.,
 ( 4, 2, 2, 2, 4 ),
 ( 0.000000000000000000, 0.2499999999999995559, 0.4999999999999991118, 0.7499999999999995559, 1.000000000000000000 ),
 .UNSPECIFIED. ) ;
#63674 = B_SPLINE_CURVE_WITH_KNOTS ( 'NONE', 3,
 ( #62969, #15096, #15444, #9845, #25239, #20002, #9494, #62632, #14757 ),
 .UNSPECIFIED., .F., .F.,
 ( 4, 1, 1, 1, 1, 1, 4 ),
 ( 0.1253704142480318307, 0.1591342569109579497, 0.3260226980931646423, 0.4929111392759626398, 0.6597995804581695545, 0.8266880216409677740, 0.8746094594482839435 ),
 .UNSPECIFIED. ) ;
#63675 = LINE ( 'NONE', #58436, #6441 ) ;
#63676 = CARTESIAN_POINT ( 'NONE',  ( 12.34743845434969067, -2.926178772989072030, 13.57378949252271028 ) ) ;
#63677 = CARTESIAN_POINT ( 'NONE',  ( 12.18524893064656744, 2.418966797248156553, 13.69026124204055783 ) ) ;
#63678 = CARTESIAN_POINT ( 'NONE',  ( 8.807788144226000426, -3.909067355573210278, -8.453461841935100196 ) ) ;
#63679 = ORIENTED_EDGE ( 'NONE', *, *, #17404, .F. ) ;
#63680 = EDGE_CURVE ( 'NONE', #47157, #56428, #12666, .T. ) ;
#63681 = EDGE_CURVE ( 'NONE', #24788, #64129, #51731, .T. ) ;
#63682 = CARTESIAN_POINT ( 'NONE',  ( 4.432228487644000126, -1.190661282979999847, -0.4572756141791000095 ) ) ;
#63683 = CARTESIAN_POINT ( 'NONE',  ( 9.630633995698000049, -2.728594541839999721, -7.641111829547599932 ) ) ;
#63684 = DIRECTION ( 'NONE',  ( 0.8660254037844289376, 0.000000000000000000, -0.5000000000000169864 ) ) ;
#63685 = CARTESIAN_POINT ( 'NONE',  ( 11.09999999999999964, -4.000000000000000000, 7.500000000000000000 ) ) ;
#63686 = AXIS2_PLACEMENT_3D ( 'NONE', #25865, #67816, #68720 ) ;
#63687 = CARTESIAN_POINT ( 'NONE',  ( 18.13803896488298761, 2.274492816832913267, -12.50128160305151859 ) ) ;
#63688 = CARTESIAN_POINT ( 'NONE',  ( 8.647284337624714823, 3.603316920592619876, -5.883498474299047487 ) ) ;
#63689 = CARTESIAN_POINT ( 'NONE',  ( 17.99291067209865957, 2.946084426705852355, 12.33636513593942752 ) ) ;
#63690 = CARTESIAN_POINT ( 'NONE',  ( 10.87221764200999985, -2.934320605648999880, -5.123881828670999283 ) ) ;
#63691 = CARTESIAN_POINT ( 'NONE',  ( 10.56984555961999916, -2.152868447761999704, -7.425101130468999777 ) ) ;
#63692 = CARTESIAN_POINT ( 'NONE',  ( 12.35624619795302515, 1.936672541213169119, 13.86556857871777027 ) ) ;
#63693 = CARTESIAN_POINT ( 'NONE',  ( 9.766851002543001314, 2.832432432432000269, 6.822293592207000934 ) ) ;
#63694 = CARTESIAN_POINT ( 'NONE',  ( 13.00000000009400303, -11.69118001589999878, -1.923222888683999932 ) ) ;
#63695 = CARTESIAN_POINT ( 'NONE',  ( 4.500000000000000000, 3.200000000000000178, 0.000000000000000000 ) ) ;
#63696 = LINE ( 'NONE', #15811, #27019 ) ;
#63697 = ADVANCED_FACE ( 'NONE', ( #20311 ), #62943, .T. ) ;
#63698 = CIRCLE ( 'NONE', #45856, 13.10000000000000142 ) ;
#63699 = ORIENTED_EDGE ( 'NONE', *, *, #51829, .F. ) ;
#63700 = CARTESIAN_POINT ( 'NONE',  ( 8.307195280408999238, 5.473983809665999622, -8.180077404516000072 ) ) ;
#63701 = CARTESIAN_POINT ( 'NONE',  ( 12.15871932425157098, -4.147141405561299621, 6.507377093516500288 ) ) ;
#63702 = VERTEX_POINT ( 'NONE', #57030 ) ;
#63703 = B_SPLINE_CURVE_WITH_KNOTS ( 'NONE', 3,
 ( #57948, #31727, #57591, #31383, #9017, #52695 ),
 .UNSPECIFIED., .F., .F.,
 ( 4, 2, 4 ),
 ( 0.000000000000000000, 0.5000000000000000000, 1.000000000000000000 ),
 .UNSPECIFIED. ) ;
#63704 = CARTESIAN_POINT ( 'NONE',  ( 13.21911358530772773, 12.38522838340865562, 1.866030466704203583 ) ) ;
#63705 = CARTESIAN_POINT ( 'NONE',  ( 10.15303300763299887, -3.212834858289399964, -8.325626572044798834 ) ) ;
#63706 = ORIENTED_EDGE ( 'NONE', *, *, #61566, .T. ) ;
#63707 = ADVANCED_FACE ( 'NONE', ( #36393 ), #63995, .F. ) ;
#63708 = CARTESIAN_POINT ( 'NONE',  ( 12.79999999734009464, -10.99220013531737372, 4.481500379774075782 ) ) ;
#63709 = CARTESIAN_POINT ( 'NONE',  ( 8.696135841231001251, 3.038023536984999939, -5.861661709981000001 ) ) ;
#63710 = CARTESIAN_POINT ( 'NONE',  ( 18.35192688406300121, -2.803631260452999818, 11.45923525916999886 ) ) ;
#63711 = CARTESIAN_POINT ( 'NONE',  ( 9.383148997457999130, -5.167567567567999731, 6.822293592207000934 ) ) ;
#63712 = CARTESIAN_POINT ( 'NONE',  ( 12.27345183613374147, 0.3288514423020141852, -13.89476819318362999 ) ) ;
#63713 = FACE_OUTER_BOUND ( 'NONE', #48959, .T. ) ;
#63714 = CARTESIAN_POINT ( 'NONE',  ( 13.64382898362900143, 11.47858090575000034, 2.288513382665999796 ) ) ;
#63715 = ORIENTED_EDGE ( 'NONE', *, *, #50623, .T. ) ;
#63716 = CARTESIAN_POINT ( 'NONE',  ( 8.731095280410999138, 2.469361196073999842, -7.826019481986000059 ) ) ;
#63717 = ORIENTED_EDGE ( 'NONE', *, *, #30253, .T. ) ;
#63718 = CARTESIAN_POINT ( 'NONE',  ( 10.16989991304999918, 2.594216849811000092, -6.291257009166999481 ) ) ;
#63719 = EDGE_LOOP ( 'NONE', ( #45381, #50209, #38325, #49170 ) ) ;
#63720 = CARTESIAN_POINT ( 'NONE',  ( 9.402671671056999969, 2.738456190347000163, 7.288123611975898974 ) ) ;
#63721 = CARTESIAN_POINT ( 'NONE',  ( 18.17259031544353931, -2.401600790900606963, -12.47395980848748742 ) ) ;
#63722 = CARTESIAN_POINT ( 'NONE',  ( 17.94511861457986868, 11.84188429194256109, -3.380847647125635014 ) ) ;
#63723 = CARTESIAN_POINT ( 'NONE',  ( 18.14123990137488818, -2.282196115462137520, -12.49965818828723840 ) ) ;
#63724 = AXIS2_PLACEMENT_3D ( 'NONE', #53277, #48726, #11307 ) ;
#63725 = CARTESIAN_POINT ( 'NONE',  ( 12.34820889858482040, 0.4270206790917077111, 13.89118144889039286 ) ) ;
#63726 = EDGE_LOOP ( 'NONE', ( #21509, #43657 ) ) ;
#63727 = CARTESIAN_POINT ( 'NONE',  ( 11.59999999999999964, 4.738901876697420690, 6.529275711103850632 ) ) ;
#63728 = CARTESIAN_POINT ( 'NONE',  ( 18.31073753479499899, 11.62544123506999938, -4.252388861798999997 ) ) ;
#63729 = CARTESIAN_POINT ( 'NONE',  ( 9.530849898046625412, 3.608426922415753690, 8.282433891029866047 ) ) ;
#63730 = DIRECTION ( 'NONE',  ( 0.000000000000000000, 0.9916377111174248249, 0.1290528957048032721 ) ) ;
#63731 = VECTOR ( 'NONE', #18001, 1000.000000000000114 ) ;
#63732 = CARTESIAN_POINT ( 'NONE',  ( 9.544414158773999901, 2.173570076733999823, -8.023168429484000441 ) ) ;
#63733 = CARTESIAN_POINT ( 'NONE',  ( 17.79055474012400140, -3.643253463509999790, 12.02383756773999934 ) ) ;
#63734 = CARTESIAN_POINT ( 'NONE',  ( 10.30297040315999979, -4.081263557776000361, -9.025012210052000938 ) ) ;
#63735 = EDGE_CURVE ( 'NONE', #61638, #56759, #23240, .T. ) ;
#63736 = EDGE_CURVE ( 'NONE', #14947, #60334, #65683, .T. ) ;
#63737 = ORIENTED_EDGE ( 'NONE', *, *, #60051, .T. ) ;
#63738 = EDGE_LOOP ( 'NONE', ( #14230, #2338, #63370 ) ) ;
#63739 = AXIS2_PLACEMENT_3D ( 'NONE', #26100, #32043, #5110 ) ;
#63740 = CARTESIAN_POINT ( 'NONE',  ( 9.349999778958000718, -4.000000000000000000, 7.500000000000000000 ) ) ;
#63741 = CARTESIAN_POINT ( 'NONE',  ( 7.924878289113897800, 5.349357204871084903, 7.500005630225526687 ) ) ;
#63742 = CARTESIAN_POINT ( 'NONE',  ( 11.43320385462400424, 12.36501045767315077, 1.521867244384402129 ) ) ;
#63743 = CARTESIAN_POINT ( 'NONE',  ( 0.1499942179679999987, 1.384928887584815138, -2.402872127494067644 ) ) ;
#63744 = CARTESIAN_POINT ( 'NONE',  ( 11.76077869730539938, 3.404661623424200201, -6.326049646822999861 ) ) ;
#63745 = CARTESIAN_POINT ( 'NONE',  ( 8.750151519676999001, 4.018750234858180725, -8.366807394121199337 ) ) ;
#63747 = CARTESIAN_POINT ( 'NONE',  ( 8.339548841713925853, 4.878437372552390627, -6.158507291990058086 ) ) ;
#63746 = CARTESIAN_POINT ( 'NONE',  ( 9.498468108405999644, -2.901397043998999781, 7.188863445572599709 ) ) ;
#63748 = CARTESIAN_POINT ( 'NONE',  ( 4.721693173016666023, 0.7554284705563509839, -1.310679582531386167 ) ) ;
#63749 = ORIENTED_EDGE ( 'NONE', *, *, #33393, .F. ) ;
#63750 = DIRECTION ( 'NONE',  ( -1.000000000000000000, 0.000000000000000000, 0.000000000000000000 ) ) ;
#63751 = CARTESIAN_POINT ( 'NONE',  ( 8.200208800211990834, -2.889590298673998081, 6.692105494707000446 ) ) ;
#63752 = CARTESIAN_POINT ( 'NONE',  ( 10.49490035061499782, 4.340961869598300105, 6.267064942904999825 ) ) ;
#63753 = FACE_OUTER_BOUND ( 'NONE', #58548, .T. ) ;
#63754 = CARTESIAN_POINT ( 'NONE',  ( 9.843726350706999639, -4.115123626494000320, 9.466607949400000166 ) ) ;
#63755 = CARTESIAN_POINT ( 'NONE',  ( 18.16572637360205889, 2.633126309616273808, -12.41957822412274837 ) ) ;
#63756 = CARTESIAN_POINT ( 'NONE',  ( 10.72422653164066730, -2.899999999999999911, -6.304440313833583609 ) ) ;
#63757 = EDGE_CURVE ( 'NONE', #17154, #15110, #5618, .T. ) ;
#63758 = ADVANCED_FACE ( 'NONE', ( #60642 ), #3879, .F. ) ;
#63759 = DIRECTION ( 'NONE',  ( 0.000000000000000000, -0.2461538461537955413, -0.9692307692307819966 ) ) ;
#63760 = CYLINDRICAL_SURFACE ( 'NONE', #27477, 0.5000000000000004441 ) ;
#63761 = CARTESIAN_POINT ( 'NONE',  ( 9.256734463322999318, -3.909687748588949852, -8.362294405496898619 ) ) ;
#63762 = ADVANCED_FACE ( 'NONE', ( #62608 ), #12754, .T. ) ;
#63763 = CARTESIAN_POINT ( 'NONE',  ( 5.980603783354000669, 1.250196283310000211, -0.4306799594067000081 ) ) ;
#63764 = CARTESIAN_POINT ( 'NONE',  ( 7.000000000000000000, 8.491849194844679261, -4.464079820575392432 ) ) ;
#63765 = CARTESIAN_POINT ( 'NONE',  ( 8.786046699800500903, 4.845411057630703233, -7.961595344540238095 ) ) ;
#63766 = VERTEX_POINT ( 'NONE', #23578 ) ;
#63767 = CARTESIAN_POINT ( 'NONE',  ( 12.18829625149018447, 0.1017072266180437112, -12.69945743039636099 ) ) ;
#63768 = CARTESIAN_POINT ( 'NONE',  ( 11.29364426047339975, 4.466097552695299733, -8.230103870496201068 ) ) ;
#63769 = FACE_OUTER_BOUND ( 'NONE', #21777, .T. ) ;
#63770 = CARTESIAN_POINT ( 'NONE',  ( 8.523148997455999520, 5.167567567567999731, -6.822293592207000934 ) ) ;
#63771 = CARTESIAN_POINT ( 'NONE',  ( 1.800973465875000068, -3.500000000000000000, 0.000000000000000000 ) ) ;
#63772 = EDGE_LOOP ( 'NONE', ( #55835, #56228, #18584, #50315, #69177, #19847, #55881, #40366, #57173, #24448 ) ) ;
#63773 = CARTESIAN_POINT ( 'NONE',  ( 5.000000000000000000, 0.6769230769231000533, 2.665384615385000266 ) ) ;
#63775 = CARTESIAN_POINT ( 'NONE',  ( 10.73213259636989925, -4.907524392912299582, -7.994504989494399361 ) ) ;
#63774 =( BOUNDED_SURFACE ( )  B_SPLINE_SURFACE ( 3, 3, ( 
 ( #60758, #66339, #56206, #12875 ),
 ( #34202, #7622, #38749, #12180 ),
 ( #54826, #13228, #1687, #65654 ),
 ( #23004, #17776, #18463, #39788 ) ),
 .UNSPECIFIED., .F., .F., .T. ) 
 B_SPLINE_SURFACE_WITH_KNOTS ( ( 4, 4 ),
 ( 4, 4 ),
 ( 0.000000000000000000, 1.000000000000000000 ),
 ( 0.000000000000000000, 1.000000000000000000 ),
 .UNSPECIFIED. ) 
 GEOMETRIC_REPRESENTATION_ITEM ( )  RATIONAL_B_SPLINE_SURFACE ( (
 ( 1.512182578520000042, 1.160176301760999840, 1.160176301760999840, 1.512182578520000042),
 ( 1.111288591041000196, 0.8526025270081000196, 0.8526025270081000196, 1.111288591041000196),
 ( 1.111288591041000196, 0.8526025270081000196, 0.8526025270081000196, 1.111288591041000196),
 ( 1.512182578520000042, 1.160176301760999840, 1.160176301760999840, 1.512182578520000042) ) ) 
 REPRESENTATION_ITEM ( '' )  SURFACE ( )  );
#63776 = CARTESIAN_POINT ( 'NONE',  ( 18.18005043853714398, 0.02024571650141320303, 12.69999991888671076 ) ) ;
#63777 = CARTESIAN_POINT ( 'NONE',  ( 10.57309687351575000, -2.782534154164605589, 7.172815144550900968 ) ) ;
#63778 = PLANE ( 'NONE',  #65201 ) ;
#63779 = CARTESIAN_POINT ( 'NONE',  ( 10.60746886766490071, 3.501664543805500074, -6.594573315824700188 ) ) ;
#63780 = ORIENTED_EDGE ( 'NONE', *, *, #15854, .T. ) ;
#63781 = CARTESIAN_POINT ( 'NONE',  ( 11.05935368890999904, -2.480241580537000168, 6.610077204591000566 ) ) ;
#63782 = CARTESIAN_POINT ( 'NONE',  ( 17.88731995174120826, 3.029458325253038264, -13.54679862780130151 ) ) ;
#63783 = ORIENTED_EDGE ( 'NONE', *, *, #57474, .F. ) ;
#63784 = ADVANCED_FACE ( 'NONE', ( #44919 ), #18346, .F. ) ;
#63785 = CARTESIAN_POINT ( 'NONE',  ( 6.900019030169000089, 12.43894676821000012, 2.828897736577999922 ) ) ;
#63786 = CARTESIAN_POINT ( 'NONE',  ( 8.829019353210000531, -5.290204991635000020, 8.768102264518001121 ) ) ;
#63787 = CARTESIAN_POINT ( 'NONE',  ( 15.86087891924500148, 8.502609378008999741, 8.308114605954999732 ) ) ;
#63788 = B_SPLINE_CURVE_WITH_KNOTS ( 'NONE', 3,
 ( #51181, #67930, #23914, #66557, #13441, #61323, #56072, #8182, #61662, #29531, #50833, #19356, #2929, #24257, #8525, #3277, #19015, #30207 ),
 .UNSPECIFIED., .F., .F.,
 ( 4, 2, 2, 2, 2, 2, 2, 2, 4 ),
 ( 0.000000000000000000, 0.1250000000000000000, 0.2500000000000000000, 0.3750000000000000000, 0.5000000000000000000, 0.6250000000000000000, 0.7500000000000000000, 0.8750000000000000000, 1.000000000000000000 ),
 .UNSPECIFIED. ) ;
#63789 = VERTEX_POINT ( 'NONE', #47922 ) ;
#63790 = CARTESIAN_POINT ( 'NONE',  ( 12.79999999914999975, -12.11987927271999865, 3.159802730921999814 ) ) ;
#63791 = CIRCLE ( 'NONE', #39253, 0.5000000000000000000 ) ;
#63792 = CARTESIAN_POINT ( 'NONE',  ( 7.473345280404999791, 2.591432452475999515, -8.508584064833998539 ) ) ;
#63793 = CARTESIAN_POINT ( 'NONE',  ( 9.934999999999998721, 4.640430492595999823, -9.117542781427999898 ) ) ;
#63794 = CARTESIAN_POINT ( 'NONE',  ( 7.323364960633568899, 2.795155525963220366, -8.204923913533448854 ) ) ;
#63795 = ORIENTED_EDGE ( 'NONE', *, *, #13587, .F. ) ;
#63796 = CARTESIAN_POINT ( 'NONE',  ( 9.476374593785998002, -5.098398394707999159, 6.305533045879999854 ) ) ;
#63797 = CARTESIAN_POINT ( 'NONE',  ( 25.26979655960100146, 11.11692128343999997, -3.473710019957000128 ) ) ;
#63798 = CARTESIAN_POINT ( 'NONE',  ( 11.20596535229475776, 3.091087823720314987, 7.175015064079871330 ) ) ;
#63799 = ORIENTED_EDGE ( 'NONE', *, *, #1823, .F. ) ;
#63800 = CARTESIAN_POINT ( 'NONE',  ( 11.29998578400000042, -3.824193979571000046, 11.71675423233000046 ) ) ;
#63801 = ORIENTED_EDGE ( 'NONE', *, *, #32793, .T. ) ;
#63802 = CARTESIAN_POINT ( 'NONE',  ( 11.79999999713069947, 12.23671679745269181, 1.944304699248228685 ) ) ;
#63803 = CARTESIAN_POINT ( 'NONE',  ( 17.95101261602637166, -1.877525629946219965, -12.45933154191684444 ) ) ;
#63804 = CARTESIAN_POINT ( 'NONE',  ( 18.36662463489988184, 2.877217017167648550, -12.05304703251516152 ) ) ;
#63805 = AXIS2_PLACEMENT_3D ( 'NONE', #961, #22272, #43614 ) ;
#63806 = CARTESIAN_POINT ( 'NONE',  ( 11.60000000000000142, 3.327218134278213668, -6.851153339015914945 ) ) ;
#63807 = DIRECTION ( 'NONE',  ( -1.000000000000000000, 0.000000000000000000, 0.000000000000000000 ) ) ;
#63808 = CARTESIAN_POINT ( 'NONE',  ( 9.365090231804463983, 2.650133164351947013, -7.500005474590564880 ) ) ;
#63809 = CARTESIAN_POINT ( 'NONE',  ( 24.14104127787211240, 12.48046602493499080, 3.363062335187216867 ) ) ;
#63810 = ORIENTED_EDGE ( 'NONE', *, *, #4070, .F. ) ;
#63811 = CARTESIAN_POINT ( 'NONE',  ( 3.364061264882832969, -2.483906522064658784, -2.527484337399751091 ) ) ;
#63812 = ORIENTED_EDGE ( 'NONE', *, *, #26356, .T. ) ;
#63813 = CARTESIAN_POINT ( 'NONE',  ( 9.687870098586998324, 5.912263966150999472, 7.772301113561999486 ) ) ;
#63814 = CARTESIAN_POINT ( 'NONE',  ( 10.34266415877000078, 5.750490533313000086, -8.094415907623000450 ) ) ;
#63815 = CARTESIAN_POINT ( 'NONE',  ( 10.98768472639999949, -0.3876847264043000174, -4.945212061661000469 ) ) ;
#63816 = CARTESIAN_POINT ( 'NONE',  ( 8.970860841232001448, 4.131080973160000447, -6.108642999115999395 ) ) ;
#63817 = CARTESIAN_POINT ( 'NONE',  ( 24.67921310950000091, -12.29514723793999842, -2.979192343402000009 ) ) ;
#63818 = DIRECTION ( 'NONE',  ( 3.927529531862125126E-06, -0.2588384783032084413, -0.9659206189611307947 ) ) ;
#63819 = CARTESIAN_POINT ( 'NONE',  ( 18.18005725403618911, -0.009762789003249691330, 13.90000041479089532 ) ) ;
#63820 = CARTESIAN_POINT ( 'NONE',  ( 18.01482774839357859, 0.4234772792570224986, 13.89131919812331439 ) ) ;
#63821 = EDGE_CURVE ( 'NONE', #4653, #10847, #31515, .T. ) ;
#63822 = ADVANCED_FACE ( 'NONE', ( #48606 ), #26942, .F. ) ;
#63823 = ORIENTED_EDGE ( 'NONE', *, *, #55402, .T. ) ;
#63824 = CARTESIAN_POINT ( 'NONE',  ( 12.78082384918899983, -11.55157311154999888, 4.942237549596000257 ) ) ;
#63825 = CARTESIAN_POINT ( 'NONE',  ( 11.55964426047339977, -3.312306505177499805, 6.422784126663999338 ) ) ;
#63826 = CARTESIAN_POINT ( 'NONE',  ( 18.03351232765111334, -0.4021407113407378109, -13.89217057782752818 ) ) ;
#63827 = CARTESIAN_POINT ( 'NONE',  ( 8.437855646795000553, -2.606998386752999775, 6.345764833140000505 ) ) ;
#63829 = CARTESIAN_POINT ( 'NONE',  ( 9.688891943908508608, 2.651205815580220282, 7.263338752445344326 ) ) ;
#63828 = CARTESIAN_POINT ( 'NONE',  ( 10.56491664109999995, 4.212242527248999835, 8.933458498617000032 ) ) ;
#63830 = CARTESIAN_POINT ( 'NONE',  ( 11.10887482311539998, 5.184953745778000389, -7.978749413531599721 ) ) ;
#63831 = AXIS2_PLACEMENT_3D ( 'NONE', #52527, #36449, #35768 ) ;
#63832 = B_SPLINE_CURVE_WITH_KNOTS ( 'NONE', 3,
 ( #5131, #53721, #69108, #5818, #933, #37979, #6509, #59303 ),
 .UNSPECIFIED., .F., .F.,
 ( 4, 2, 2, 4 ),
 ( 0.000000000000000000, 0.2499999999999998890, 0.4999999999999997780, 1.000000000000000000 ),
 .UNSPECIFIED. ) ;
#63833 = CARTESIAN_POINT ( 'NONE',  ( 25.19214535676100297, -11.35759380094999926, 3.218642521839000015 ) ) ;
#63834 = CARTESIAN_POINT ( 'NONE',  ( 9.703659112603999048, 3.623260508844300176, -8.280881105104999307 ) ) ;
#63835 = CARTESIAN_POINT ( 'NONE',  ( 17.91054845552245922, -0.5141503178158091103, 12.68598964581896738 ) ) ;
#63836 = CARTESIAN_POINT ( 'NONE',  ( 7.226906611567000205, -1.149357487460000105, 0.4566943152281999763 ) ) ;
#63837 = CARTESIAN_POINT ( 'NONE',  ( 24.08694690297700092, 9.258999421897000204, 9.302244280904000462 ) ) ;
#63838 = VERTEX_POINT ( 'NONE', #26600 ) ;
#63839 = CARTESIAN_POINT ( 'NONE',  ( 9.278331853207999913, -5.791549888895000109, 7.752110689268000954 ) ) ;
#63840 = CARTESIAN_POINT ( 'NONE',  ( 9.717214158771000143, 3.990126737362999609, -8.809457313313998839 ) ) ;
#63841 = FACE_OUTER_BOUND ( 'NONE', #40959, .T. ) ;
#63842 = CARTESIAN_POINT ( 'NONE',  ( 10.98960529798009489, 6.634415940184054783, 5.386686141248282489 ) ) ;
#63843 = ORIENTED_EDGE ( 'NONE', *, *, #39616, .F. ) ;
#63844 = AXIS2_PLACEMENT_3D ( 'NONE', #6387, #31945, #27043 ) ;
#63845 = ADVANCED_FACE ( 'NONE', ( #36745 ), #37086, .F. ) ;
#63846 = CARTESIAN_POINT ( 'NONE',  ( 0.4444555633787999893, -2.390579753276000030, 2.141564200098999837 ) ) ;
#63847 = CARTESIAN_POINT ( 'NONE',  ( 10.35814141025499957, 4.483492689244800822, 6.638851159159999682 ) ) ;
#63848 = CARTESIAN_POINT ( 'NONE',  ( 10.69016084123000176, 4.391264627567999845, -8.802335896973000118 ) ) ;
#63849 = EDGE_LOOP ( 'NONE', ( #63169, #44126, #44057, #45159 ) ) ;
#63850 = CARTESIAN_POINT ( 'NONE',  ( 5.284193173016667799, 1.460959015002474493, -0.3926218265389176953 ) ) ;
#63851 = CARTESIAN_POINT ( 'NONE',  ( 11.07299956498199833, -2.792989229543000107, -7.825000000000000178 ) ) ;
#63852 = CARTESIAN_POINT ( 'NONE',  ( 10.05862282008599884, 4.666276081381299790, 6.425317846273999933 ) ) ;
#63853 = FACE_OUTER_BOUND ( 'NONE', #4209, .T. ) ;
#63854 = CARTESIAN_POINT ( 'NONE',  ( 7.475045280409000625, 3.276311362504999991, 5.841989464160999290 ) ) ;
#63855 = ORIENTED_EDGE ( 'NONE', *, *, #57288, .T. ) ;
#63856 = CARTESIAN_POINT ( 'NONE',  ( 25.46372779695100164, -11.23407511953000082, -3.161075425950000017 ) ) ;
#63857 = CARTESIAN_POINT ( 'NONE',  ( 7.259679719586999980, 3.516145570366999706, -5.836512876186000121 ) ) ;
#63858 = CARTESIAN_POINT ( 'NONE',  ( 8.326548857933062209, -3.968851420165860233, 9.244526958411647399 ) ) ;
#63859 = CARTESIAN_POINT ( 'NONE',  ( 9.598721904869998767, -2.884547197234000215, 6.873781641694999500 ) ) ;
#63860 = EDGE_LOOP ( 'NONE', ( #67605, #35528, #41115, #54133 ) ) ;
#63861 = CARTESIAN_POINT ( 'NONE',  ( 3.000973465876999757, 3.500000000000000000, 0.000000000000000000 ) ) ;
#63862 = DIRECTION ( 'NONE',  ( 0.000000000000000000, -0.9620913858416644260, -0.2727272727272901376 ) ) ;
#63863 = VERTEX_POINT ( 'NONE', #20658 ) ;
#63864 = ADVANCED_FACE ( 'NONE', ( #58066 ), #19, .T. ) ;
#63865 = CARTESIAN_POINT ( 'NONE',  ( 24.90040311280328567, 3.015665883976863526, -11.63994628420445032 ) ) ;
#63866 = CARTESIAN_POINT ( 'NONE',  ( 24.70906580553056742, -8.654462107696843987, -8.608367302003138377 ) ) ;
#63867 = CARTESIAN_POINT ( 'NONE',  ( 7.890669427268998781, -4.660296165433000404, 6.322498843348999920 ) ) ;
#63868 = ORIENTED_EDGE ( 'NONE', *, *, #20348, .F. ) ;
#63869 = CARTESIAN_POINT ( 'NONE',  ( 9.534310001152000780, -5.383415012847999392, -8.183490493635000362 ) ) ;
#63870 = CARTESIAN_POINT ( 'NONE',  ( 7.616545958352999968, 8.192027149378999340, 4.617357713344999226 ) ) ;
#63871 = CARTESIAN_POINT ( 'NONE',  ( 11.35545123989519922, 4.475221369382300196, -8.417769225118700405 ) ) ;
#63872 = CARTESIAN_POINT ( 'NONE',  ( 4.574515983791000080E-07, 2.400000066501999818, 0.000000000000000000 ) ) ;
#63873 = CARTESIAN_POINT ( 'NONE',  ( 11.06733863405299800, -3.211524470605299886, 6.494205428462000107 ) ) ;
#63874 = ORIENTED_EDGE ( 'NONE', *, *, #66995, .F. ) ;
#63875 = CARTESIAN_POINT ( 'NONE',  ( 7.833767219591000419, 2.583668273793999770, 6.684750595573999199 ) ) ;
#63876 = VERTEX_POINT ( 'NONE', #41984 ) ;
#63877 = CARTESIAN_POINT ( 'NONE',  ( 3.000973465876999757, 3.500000000000000000, 0.000000000000000000 ) ) ;
#63878 = B_SPLINE_CURVE_WITH_KNOTS ( 'NONE', 3,
 ( #48585, #12561, #65342, #6964, #16753, #5921, #32852, #11171, #48234, #32507, #54163, #42989, #38434, #27956, #22351, #11508 ),
 .UNSPECIFIED., .F., .F.,
 ( 4, 2, 2, 2, 2, 2, 2, 4 ),
 ( 0.1254192006116268687, 0.2190632745348801147, 0.3127073484581333607, 0.4999954963046393530, 0.5936395702278924880, 0.6872836441511454009, 0.7809277180743985358, 0.8745717919976516708 ),
 .UNSPECIFIED. ) ;
#63879 = AXIS2_PLACEMENT_3D ( 'NONE', #907, #18029, #7518 ) ;
#63880 = CARTESIAN_POINT ( 'NONE',  ( 8.930995559624999913, -2.019079883662000086, 7.390983468784999566 ) ) ;
#63881 = DIRECTION ( 'NONE',  ( 1.000000000000000000, 0.000000000000000000, 0.000000000000000000 ) ) ;
#63882 = ORIENTED_EDGE ( 'NONE', *, *, #48924, .T. ) ;
#63883 = CARTESIAN_POINT ( 'NONE',  ( 12.79462099885205184, -1.875000035136121568, -12.57541665307954659 ) ) ;
#63884 = CARTESIAN_POINT ( 'NONE',  ( 11.00774031427000033, 7.361568041487994485, -6.124472886188995879 ) ) ;
#63885 = FACE_OUTER_BOUND ( 'NONE', #41781, .T. ) ;
#63886 = DIRECTION ( 'NONE',  ( 1.000000000000000000, 0.000000000000000000, 0.000000000000000000 ) ) ;
#63887 = CARTESIAN_POINT ( 'NONE',  ( 12.18844676753248457, -2.902714632704707309, -13.69578956119810620 ) ) ;
#63888 = CARTESIAN_POINT ( 'NONE',  ( 10.35826357027499789, -3.149486845331399998, -7.664090691848299386 ) ) ;
#63889 = CARTESIAN_POINT ( 'NONE',  ( 18.32727125556129977, 3.363648366952159297, 12.06493410109839637 ) ) ;
#63890 = CARTESIAN_POINT ( 'NONE',  ( 18.13398081625437541, -2.046400819240521418, 12.43272243325427873 ) ) ;
#63891 = ORIENTED_EDGE ( 'NONE', *, *, #58437, .F. ) ;
#63892 = CARTESIAN_POINT ( 'NONE',  ( 11.12483852207999924, -5.434422895407000631, -5.164705231992000378 ) ) ;
#63893 = ORIENTED_EDGE ( 'NONE', *, *, #47610, .T. ) ;
#63894 = AXIS2_PLACEMENT_3D ( 'NONE', #9703, #52358, #4451 ) ;
#63895 = CARTESIAN_POINT ( 'NONE',  ( 0.000000000000000000, 0.000000000000000000, 0.000000000000000000 ) ) ;
#63896 = LINE ( 'NONE', #16011, #50101 ) ;
#63897 = CARTESIAN_POINT ( 'NONE',  ( 4.900006121741999898, -1.007237960741797389, 1.747572776708516740 ) ) ;
#63898 = CARTESIAN_POINT ( 'NONE',  ( 10.36630583688000051, 5.852743870412999705, -7.568014644338999730 ) ) ;
#63899 = DIRECTION ( 'NONE',  ( 1.000000000000000000, 0.000000000000000000, 0.000000000000000000 ) ) ;
#63900 = CARTESIAN_POINT ( 'NONE',  ( 18.17891623993478944, 2.457256301271274257, -12.46146663851731340 ) ) ;
#63901 = AXIS2_PLACEMENT_3D ( 'NONE', #6909, #50602, #44339 ) ;
#63902 = CARTESIAN_POINT ( 'NONE',  ( 23.73417960609100064, -13.39756163216000040, 3.632377255137999583 ) ) ;
#63903 = EDGE_CURVE ( 'NONE', #40828, #32947, #34002, .T. ) ;
#63905 = EDGE_CURVE ( 'NONE', #30682, #11605, #9836, .T. ) ;
#63904 = CARTESIAN_POINT ( 'NONE',  ( 8.768793171737998549, 3.595811914175000013, -8.374125585548998885 ) ) ;
#63906 = ORIENTED_EDGE ( 'NONE', *, *, #62725, .T. ) ;
#63907 = CARTESIAN_POINT ( 'NONE',  ( 11.58810207955109917, -4.796537143354000499, -7.174999999999999822 ) ) ;
#63908 = EDGE_CURVE ( 'NONE', #426, #58024, #68437, .T. ) ;
#63909 = EDGE_CURVE ( 'NONE', #57343, #46556, #22345, .T. ) ;
#63910 = CARTESIAN_POINT ( 'NONE',  ( 10.09197164456000095, 3.841384681542000301, 5.536408945990000774 ) ) ;
#63911 = CARTESIAN_POINT ( 'NONE',  ( 2.050973465875999935, 3.500000000000000000, 0.000000000000000000 ) ) ;
#63912 = CARTESIAN_POINT ( 'NONE',  ( 11.98011496860029901, -3.080230834057799960, 7.971338736265699332 ) ) ;
#63913 = CARTESIAN_POINT ( 'NONE',  ( 18.26087544840899923, 2.716371057353000218, -11.57326339378999869 ) ) ;
#63914 = CARTESIAN_POINT ( 'NONE',  ( 11.31825954179440075, 4.666231193203100425, -8.053565341712399572 ) ) ;
#63915 = CARTESIAN_POINT ( 'NONE',  ( 12.40045920100465082, -0.4764818960106725343, 12.68796903437992540 ) ) ;
#63916 = CARTESIAN_POINT ( 'NONE',  ( 11.60000000000000142, 3.186931496511416828, -8.037608584222629915 ) ) ;
#63917 = CARTESIAN_POINT ( 'NONE',  ( 10.87521525736000072, 4.831064930369000088, 6.312796576761000367 ) ) ;
#63918 = CARTESIAN_POINT ( 'NONE',  ( 24.67921580188599862, 3.567514645466999923, -12.13750897870000145 ) ) ;
#63919 = B_SPLINE_SURFACE_WITH_KNOTS ( 'NONE', 3, 3, ( 
 ( #51685, #9036, #62177, #18515 ),
 ( #50669, #45428, #8705, #30377 ),
 ( #56940, #2769, #62517, #40511 ),
 ( #13956, #3109, #25121, #35283 ),
 ( #3443, #40183, #24095, #66392 ),
 ( #24780, #46453, #46107, #14636 ) ),
 .UNSPECIFIED., .F., .F., .F.,
 ( 4, 1, 1, 4 ),
 ( 4, 4 ),
 ( 0.1423941212541000034, 0.3333333333333000081, 0.6666666666667000474, 0.8219462477342999174 ),
 ( -0.1256563615234000120, 1.125656361508000192 ),
 .UNSPECIFIED. ) ;
#63920 = ORIENTED_EDGE ( 'NONE', *, *, #23066, .T. ) ;
#63921 = CARTESIAN_POINT ( 'NONE',  ( 9.368660841232999914, 2.702406276695999754, -6.981052078638000147 ) ) ;
#63922 = CARTESIAN_POINT ( 'NONE',  ( 6.961914452361000372, 0.1816583604578000111, -1.117739201043999930 ) ) ;
#63923 = CARTESIAN_POINT ( 'NONE',  ( 17.84240044433949990, 3.055120806185297244, 13.53986419860029145 ) ) ;
#63924 = CARTESIAN_POINT ( 'NONE',  ( 10.91620964606000044, -2.818413279081999789, -6.814156272943999504 ) ) ;
#63925 = CARTESIAN_POINT ( 'NONE',  ( 24.50549018585800098, 8.845081872695999436, -9.150167881723000107 ) ) ;
#63926 = CARTESIAN_POINT ( 'NONE',  ( 11.40841235500449891, -4.841138636481000290, -6.729431436870699557 ) ) ;
#63927 = ORIENTED_EDGE ( 'NONE', *, *, #9861, .F. ) ;
#63928 = AXIS2_PLACEMENT_3D ( 'NONE', #37621, #65223, #59290 ) ;
#63929 = FACE_OUTER_BOUND ( 'NONE', #7629, .T. ) ;
#63930 = DIRECTION ( 'NONE',  ( 0.000000000000000000, 0.8075584957945176612, -0.5897874836499127360 ) ) ;
#63933 = UNCERTAINTY_MEASURE_WITH_UNIT (LENGTH_MEASURE( 1.000000000000000082E-05 ), #8267, 'distance_accuracy_value', 'NONE');
#63932 = CARTESIAN_POINT ( 'NONE',  ( 5.600023899775999681, 13.94845324556000143, 4.312847325879000770 ) ) ;
#63931 = CARTESIAN_POINT ( 'NONE',  ( 9.881820280408998514, 4.325866256860000369, -9.125812605905000652 ) ) ;
#63934 = CARTESIAN_POINT ( 'NONE',  ( 3.400291169224110011, 0.03804497073930836887, 3.257691641818311279 ) ) ;
#63935 = VERTEX_POINT ( 'NONE', #22022 ) ;
#63936 = CARTESIAN_POINT ( 'NONE',  ( 10.70441484796999987, 3.444517850837000239, 6.009055070331999815 ) ) ;
#63937 = CARTESIAN_POINT ( 'NONE',  ( 18.09690629521218241, -2.811641957965457905, -13.60235445620236128 ) ) ;
#63938 = CARTESIAN_POINT ( 'NONE',  ( 10.77672335273219950, 4.301522290735800169, 6.687976048055599421 ) ) ;
#63939 = CARTESIAN_POINT ( 'NONE',  ( 9.532671748231999587, -4.663050389319001177, 8.669823109968998409 ) ) ;
#63940 = CARTESIAN_POINT ( 'NONE',  ( 8.128308059623998716, -3.117370956513999758, 8.662188901935000018 ) ) ;
#63941 = VERTEX_POINT ( 'NONE', #47233 ) ;
#63942 = CARTESIAN_POINT ( 'NONE',  ( 7.454676658771000497, 2.138190256467000339, 6.814770510101999967 ) ) ;
#63944 = CARTESIAN_POINT ( 'NONE',  ( 10.52384314678999999, -5.441919393629000012, -7.989634081859001036 ) ) ;
#63943 = CARTESIAN_POINT ( 'NONE',  ( 10.74760529021567734, 4.040385281810796592, -8.373188771871163283 ) ) ;
#63945 = CARTESIAN_POINT ( 'NONE',  ( 7.754788148867381992, -5.333023120641254167, 8.617227868399091051 ) ) ;
#63946 = CIRCLE ( 'NONE', #33829, 2.000000000000000444 ) ;
#63947 = CARTESIAN_POINT ( 'NONE',  ( 18.15698508547025369, -0.1703860850750339440, 13.89862588397355658 ) ) ;
#63948 = CARTESIAN_POINT ( 'NONE',  ( 24.33654969819199820, 3.364569167692000207, 12.26690921096999887 ) ) ;
#63949 = ORIENTED_EDGE ( 'NONE', *, *, #12968, .T. ) ;
#63950 = CARTESIAN_POINT ( 'NONE',  ( 5.605026506349999771, -1.500000000000000000, 0.000000000000000000 ) ) ;
#63951 = CARTESIAN_POINT ( 'NONE',  ( 11.37103032197929942, -3.416314376401300201, 8.316248703309600643 ) ) ;
#63952 = EDGE_CURVE ( 'NONE', #25385, #45676, #7366, .T. ) ;
#63953 = CARTESIAN_POINT ( 'NONE',  ( 11.55194988689359903, 4.580487242693600081, 6.361426117087999543 ) ) ;
#63954 = ORIENTED_EDGE ( 'NONE', *, *, #67686, .T. ) ;
#63955 = CARTESIAN_POINT ( 'NONE',  ( 8.424364158774000799, 3.292387953886000140, -6.294868737226000377 ) ) ;
#63956 = EDGE_CURVE ( 'NONE', #9331, #47642, #43142, .T. ) ;
#63957 = CARTESIAN_POINT ( 'NONE',  ( 12.10652924560087307, 2.286704390305608570, -12.39076728011198725 ) ) ;
#63958 = CARTESIAN_POINT ( 'NONE',  ( 11.01925056272500036, -2.825232917634000085, 7.482589369563879877 ) ) ;
#63959 = CARTESIAN_POINT ( 'NONE',  ( 24.84742874851600192, -3.386177995241999916, -11.85235341148000110 ) ) ;
#63960 = CARTESIAN_POINT ( 'NONE',  ( 18.14470825313953739, 2.707255376642708100, -13.62731588235574698 ) ) ;
#63961 = VERTEX_POINT ( 'NONE', #16773 ) ;
#63962 = FACE_OUTER_BOUND ( 'NONE', #7879, .T. ) ;
#63963 = CARTESIAN_POINT ( 'NONE',  ( 23.77345882393642995, 9.774756027420808735, 9.437281717087342869 ) ) ;
#63964 = ORIENTED_EDGE ( 'NONE', *, *, #44538, .F. ) ;
#63965 = CARTESIAN_POINT ( 'NONE',  ( 11.56025819896753859, 3.013900664291200293, 7.314099615601099558 ) ) ;
#63966 = DIRECTION ( 'NONE',  ( 0.000000000000000000, -1.000000000000000000, 0.000000000000000000 ) ) ;
#63967 = CARTESIAN_POINT ( 'NONE',  ( 10.34224945431000009, 3.348985101650000296, -8.881460768006000706 ) ) ;
#63968 = FACE_OUTER_BOUND ( 'NONE', #55827, .T. ) ;
#63969 = CARTESIAN_POINT ( 'NONE',  ( 10.98286725694000054, -3.998514182530999772, 9.091066422484001208 ) ) ;
#63970 = CARTESIAN_POINT ( 'NONE',  ( 17.94350157889105901, 0.4896501542853345379, -12.68729270499358108 ) ) ;
#63971 = CARTESIAN_POINT ( 'NONE',  ( 9.042739452581361803, 4.892140300096698979, 8.513365777369095611 ) ) ;
#63972 = CARTESIAN_POINT ( 'NONE',  ( 10.87103032197929942, -3.416314376401300201, -6.683751296690399357 ) ) ;
#63973 = CARTESIAN_POINT ( 'NONE',  ( 8.881823341230997926, 4.977909614887999545, 6.416776202806000029 ) ) ;
#63974 = ORIENTED_EDGE ( 'NONE', *, *, #9654, .F. ) ;
#63975 =( NAMED_UNIT ( * ) SI_UNIT ( $, .STERADIAN. ) SOLID_ANGLE_UNIT ( ) );
#63976 = CARTESIAN_POINT ( 'NONE',  ( 24.68353817070021705, -3.140007193288423704, 11.82111472263500218 ) ) ;
#63977 = CARTESIAN_POINT ( 'NONE',  ( 10.98768472639999949, 5.139096889661000311, -4.945212061661000469 ) ) ;
#63978 = CARTESIAN_POINT ( 'NONE',  ( 24.92740991898443426, 8.563816619416252607, 8.404006304129723048 ) ) ;
#63979 = CARTESIAN_POINT ( 'NONE',  ( 17.98022888730379165, 3.063516777430822735, 12.22190850126833972 ) ) ;
#63980 = DIRECTION ( 'NONE',  ( 1.000000000000000000, 0.000000000000000000, 0.000000000000000000 ) ) ;
#63982 = EDGE_CURVE ( 'NONE', #8257, #38701, #3157, .T. ) ;
#63981 = DIRECTION ( 'NONE',  ( 0.000000000000000000, 0.000000000000000000, 1.000000000000000000 ) ) ;
#63983 = CARTESIAN_POINT ( 'NONE',  ( 8.610944094208999644, 5.100000000000000533, -6.571291218949999902 ) ) ;
#63984 = EDGE_CURVE ( 'NONE', #56577, #50051, #15419, .T. ) ;
#63985 = CARTESIAN_POINT ( 'NONE',  ( 8.158337976294000900E-06, 0.000000000000000000, 0.000000000000000000 ) ) ;
#63986 = ADVANCED_FACE ( 'NONE', ( #27977 ), #33219, .F. ) ;
#63987 = VERTEX_POINT ( 'NONE', #34259 ) ;
#63988 = CARTESIAN_POINT ( 'NONE',  ( 12.36031510016529822, -1.911905511008638259, 12.45410252665035600 ) ) ;
#63989 = CARTESIAN_POINT ( 'NONE',  ( 10.26291290906799958, -4.635529777446699917, -8.277781595084700683 ) ) ;
#63990 = FACE_OUTER_BOUND ( 'NONE', #36915, .T. ) ;
#63991 = DIRECTION ( 'NONE',  ( 1.000000000000000000, 0.000000000000000000, 0.000000000000000000 ) ) ;
#63992 = CARTESIAN_POINT ( 'NONE',  ( 11.81410538575740077, -3.024036709177600368, 7.733337754805098996 ) ) ;
#63993 = CARTESIAN_POINT ( 'NONE',  ( 10.79718447801629999, 5.003225587801999552, -7.477880487566260115 ) ) ;
#63994 = CARTESIAN_POINT ( 'NONE',  ( 12.35444711458465505, 0.5635217852606908551, 12.58739276154098086 ) ) ;
#63995 = CONICAL_SURFACE ( 'NONE', #56182, 1.150066570905000196, 0.7854484257638207900 ) ;
#63996 = CARTESIAN_POINT ( 'NONE',  ( 0.3595045405019000051, -1.072119470989999934, 3.198702759649999727 ) ) ;
#63997 = FACE_OUTER_BOUND ( 'NONE', #17334, .T. ) ;
#63998 = CARTESIAN_POINT ( 'NONE',  ( 12.43868857148325269, 1.859375588728223505, 12.46205283878464876 ) ) ;
#64000 = CARTESIAN_POINT ( 'NONE',  ( 8.304135841228999837, 3.650414032626000171, 6.083147621602999600 ) ) ;
#63999 = CARTESIAN_POINT ( 'NONE',  ( 9.327747021775998348, 3.141778309999299967, -8.253120162257399528 ) ) ;
#64001 = CARTESIAN_POINT ( 'NONE',  ( 10.66995391537419913, 4.943675741382899780, -8.140910455049299443 ) ) ;
#64002 = CARTESIAN_POINT ( 'NONE',  ( 7.577053541547003945, 3.182130936862002102, -6.424376193309997873 ) ) ;
#64003 = CARTESIAN_POINT ( 'NONE',  ( 10.05462971959000029, 3.531217403581000003, -9.119235467071000301 ) ) ;
#64004 = ADVANCED_FACE ( 'NONE', ( #54884 ), #2432, .F. ) ;
#64005 = CARTESIAN_POINT ( 'NONE',  ( 9.959912909067998754, 3.190593056227700064, -8.490578012456198920 ) ) ;
#64007 = CARTESIAN_POINT ( 'NONE',  ( 12.33520056822022148, 2.912263648515628134, 12.34589992753487664 ) ) ;
#64006 = LINE ( 'NONE', #10531, #25228 ) ;
#64008 = CARTESIAN_POINT ( 'NONE',  ( 11.14955063476181607, -3.023401864784705850, -6.673569913327194847 ) ) ;
#64009 = ORIENTED_EDGE ( 'NONE', *, *, #34943, .F. ) ;
#64010 = CARTESIAN_POINT ( 'NONE',  ( 12.26246716466153863, 0.3103928898581689300, 12.69489813901718911 ) ) ;
#64011 = CARTESIAN_POINT ( 'NONE',  ( 10.16476354018241501, 5.217465845835396188, 7.827184855449094592 ) ) ;
#64012 = CARTESIAN_POINT ( 'NONE',  ( 17.55505043854144631, -0.7192913403693119712, -12.57945229203838267 ) ) ;
#64013 = CARTESIAN_POINT ( 'NONE',  ( 8.715822372493999382, 3.750788346126100237, 6.684745346084599582 ) ) ;
#64014 = CARTESIAN_POINT ( 'NONE',  ( 12.51770044094180534, -3.055120810438262335, 13.53992139506082459 ) ) ;
#64015 = CARTESIAN_POINT ( 'NONE',  ( 12.18032316971016193, 2.521073842666304632, 13.66891947081129111 ) ) ;
#64016 = CARTESIAN_POINT ( 'NONE',  ( 8.982564767455606614, -5.103418008754404767, -7.795647801703331936 ) ) ;
#64017 = ORIENTED_EDGE ( 'NONE', *, *, #32078, .T. ) ;
#64018 = CARTESIAN_POINT ( 'NONE',  ( 4.797999458657999483, -1.073975598522000086, 0.3653522499201999896 ) ) ;
#64019 = CARTESIAN_POINT ( 'NONE',  ( 8.896088727410999653, -5.274736981944999847, -7.606911245136100064 ) ) ;
#64020 = VECTOR ( 'NONE', #12158, 1000.000000000000000 ) ;
#64021 = CARTESIAN_POINT ( 'NONE',  ( 18.28832092577789581, -2.855728055076846683, 11.50255606648410200 ) ) ;
#64022 = CARTESIAN_POINT ( 'NONE',  ( 17.89176949849500886, -3.347044352179931792, 11.15884716666432475 ) ) ;
#64023 = CARTESIAN_POINT ( 'NONE',  ( 17.92103372721321364, 3.006741473881710647, -12.31895748915804489 ) ) ;
#64024 = CARTESIAN_POINT ( 'NONE',  ( 9.772783876522375124, -4.789858247946766845, 8.481892410946455740 ) ) ;
#64025 = CARTESIAN_POINT ( 'NONE',  ( 11.09999999999999964, -5.340540540541000247, -6.721892642903999793 ) ) ;
#64026 = CARTESIAN_POINT ( 'NONE',  ( 10.11501430098066656, 5.350017391163124358, -7.499999134156894343 ) ) ;
#64027 = CARTESIAN_POINT ( 'NONE',  ( 10.33453064679000200, -3.295701412239999684, -6.149875347297999895 ) ) ;
#64028 = EDGE_CURVE ( 'NONE', #32816, #58368, #66401, .T. ) ;
#64029 = CARTESIAN_POINT ( 'NONE',  ( 4.771693173016333667, 0.7554284705563509839, -1.310679582531385945 ) ) ;
#64030 = CARTESIAN_POINT ( 'NONE',  ( 11.14393020684970104, -2.750000000000000000, 7.500000000000000000 ) ) ;
#64031 = CARTESIAN_POINT ( 'NONE',  ( 23.78804094696696581, 9.744952014918238703, -9.430323830586468503 ) ) ;
#64032 = CARTESIAN_POINT ( 'NONE',  ( -15.86200481174999943, -2.399999999999999911, 6.571291218949999902 ) ) ;
#64033 = ORIENTED_EDGE ( 'NONE', *, *, #68351, .F. ) ;
#64034 = CARTESIAN_POINT ( 'NONE',  ( 9.972410841228999345, 4.357364160690000432, -9.282962013144999247 ) ) ;
#64036 = COLOUR_RGB ( '', 0.31764706, 0.68627451, 0.89019608) ;
#64035 = CARTESIAN_POINT ( 'NONE',  ( 11.64595257254739913, -4.831736303435800295, 7.258104750172799768 ) ) ;
#64037 = ORIENTED_EDGE ( 'NONE', *, *, #36325, .F. ) ;
#64038 = CYLINDRICAL_SURFACE ( 'NONE', #67489, 1.350000000000000089 ) ;
#64039 = CARTESIAN_POINT ( 'NONE',  ( 11.06379841651039797, -4.401637675674300532, -8.567697191971999970 ) ) ;
#64040 = VERTEX_POINT ( 'NONE', #28673 ) ;
#64041 = CARTESIAN_POINT ( 'NONE',  ( 10.72191429142990060, 4.025072603369280522, 8.816028813488999916 ) ) ;
#64043 = CARTESIAN_POINT ( 'NONE',  ( 24.13559297464179565, 3.329017028593327598, -12.49970664374816565 ) ) ;
#64042 = AXIS2_PLACEMENT_3D ( 'NONE', #50063, #2171, #66473 ) ;
#64044 = CARTESIAN_POINT ( 'NONE',  ( 18.35481935287100086, -2.723593151845999927, 11.47751840123000022 ) ) ;
#64045 = CARTESIAN_POINT ( 'NONE',  ( 10.73724174883999893, -4.024531238983009906, -8.391788556008700439 ) ) ;
#64046 = CARTESIAN_POINT ( 'NONE',  ( 12.38151006065648296, 0.4597209100133001214, -13.88976952606943271 ) ) ;
#64047 = CARTESIAN_POINT ( 'NONE',  ( 11.53937265905000054, 3.642773248484000082, -11.02530338024999956 ) ) ;
#64048 = CARTESIAN_POINT ( 'NONE',  ( 13.73573769406200107, 11.39043216638999922, 2.256426478477000064 ) ) ;
#64049 = EDGE_LOOP ( 'NONE', ( #41598, #5229, #60804, #46084 ) ) ;
#64050 = CARTESIAN_POINT ( 'NONE',  ( 8.780820280412001466, 2.567871051582000241, -6.869011921437000012 ) ) ;
#64051 = ORIENTED_EDGE ( 'NONE', *, *, #9860, .T. ) ;
#64052 = CARTESIAN_POINT ( 'NONE',  ( 0.1431889841876702318, -0.3267341222390062194, -3.196183395200867139 ) ) ;
#64053 =( LENGTH_UNIT ( ) NAMED_UNIT ( * ) SI_UNIT ( .MILLI., .METRE. ) );
#64054 = ORIENTED_EDGE ( 'NONE', *, *, #59112, .F. ) ;
#64055 = CARTESIAN_POINT ( 'NONE',  ( 8.499265421555000088, 3.759926620436100375, 6.258138488953999712 ) ) ;
#64056 = CARTESIAN_POINT ( 'NONE',  ( 18.17176891181421539, -2.603394967838110308, -12.42689558795375326 ) ) ;
#64057 = CARTESIAN_POINT ( 'NONE',  ( 24.89163395459006978, -8.575320083348136890, 8.440772679311232096 ) ) ;
#64058 = CARTESIAN_POINT ( 'NONE',  ( 10.16476354018241501, 5.217465845835396188, -7.172815144550905408 ) ) ;
#64059 = B_SPLINE_SURFACE_WITH_KNOTS ( 'NONE', 3, 3, ( 
 ( #15349, #57996, #41570, #63575 ),
 ( #62542, #62880, #10096, #19907 ),
 ( #37956, #31431, #52747, #51715 ),
 ( #3807, #46477, #67785, #14663 ),
 ( #35979, #57297, #9399, #61190 ),
 ( #44434, #54906, #2120, #33936 ),
 ( #8048, #45796, #45116, #50701 ),
 ( #55255, #67109, #61531, #29045 ) ),
 .UNSPECIFIED., .F., .F., .F.,
 ( 4, 1, 1, 1, 1, 4 ),
 ( 4, 4 ),
 ( 0.008355517289528000338, 0.05882352941176000050, 0.1176470588234999892, 0.1764705882353000133, 0.2352941176471000095, 0.2534843112964000333 ),
 ( -0.1830816879725000179, 1.182949857028000151 ),
 .UNSPECIFIED. ) ;
#64060 = B_SPLINE_CURVE_WITH_KNOTS ( 'NONE', 3,
 ( #6839, #37964, #915, #33075 ),
 .UNSPECIFIED., .F., .F.,
 ( 4, 4 ),
 ( 0.000000000000000000, 1.000000000000000000 ),
 .UNSPECIFIED. ) ;
#64061 = DIRECTION ( 'NONE',  ( -1.000000000000000000, 0.000000000000000000, 0.000000000000000000 ) ) ;
#64062 = EDGE_CURVE ( 'NONE', #15478, #57225, #59866, .T. ) ;
#64063 = CARTESIAN_POINT ( 'NONE',  ( 11.66544712921906779, -4.732401051283384952, 7.017906594554381705 ) ) ;
#64064 = EDGE_CURVE ( 'NONE', #4640, #10323, #29058, .T. ) ;
#64065 = VERTEX_POINT ( 'NONE', #23760 ) ;
#64066 = CARTESIAN_POINT ( 'NONE',  ( 11.95023821374600104, 11.77429045505000005, -4.110796463462000006 ) ) ;
#64067 = AXIS2_PLACEMENT_3D ( 'NONE', #14754, #36071, #3561 ) ;
#64068 = CARTESIAN_POINT ( 'NONE',  ( 18.44976178625400109, 11.77429045505000005, -4.110796463462000006 ) ) ;
#64069 = FACE_OUTER_BOUND ( 'NONE', #16517, .T. ) ;
#64070 = CARTESIAN_POINT ( 'NONE',  ( 4.604558767843999867, 1.154756044014000116, 0.2749155220972999691 ) ) ;
#64071 = VECTOR ( 'NONE', #5782, 1000.000000000000000 ) ;
#64072 = CARTESIAN_POINT ( 'NONE',  ( 8.897989158775001073, 4.990139824845000405, -9.121472988377998803 ) ) ;
#64073 = CARTESIAN_POINT ( 'NONE',  ( 18.23019412026599895, -3.031170125296999807, 11.90979123982999965 ) ) ;
#64074 = CARTESIAN_POINT ( 'NONE',  ( 10.57793869653000129, -4.393380534095000733, -6.024358525186999991 ) ) ;
#64075 = VERTEX_POINT ( 'NONE', #22372 ) ;
#64076 = VERTEX_POINT ( 'NONE', #1398 ) ;
#64077 = DIRECTION ( 'NONE',  ( 0.000000000000000000, 0.000000000000000000, -1.000000000000000000 ) ) ;
#64078 = CARTESIAN_POINT ( 'NONE',  ( 24.53429015151300163, -3.614318902553999902, -12.31267542782000035 ) ) ;
#64079 = CARTESIAN_POINT ( 'NONE',  ( 18.28051081950330570, -2.330210462394771476, 13.80606256597843995 ) ) ;
#64080 = DIRECTION ( 'NONE',  ( -1.000000000000000000, 0.000000000000000000, 0.000000000000000000 ) ) ;
#64081 = CARTESIAN_POINT ( 'NONE',  ( 18.30000000000000071, 0.000000000000000000, 0.000000000000000000 ) ) ;
#64082 = CARTESIAN_POINT ( 'NONE',  ( 10.36503728015203230, -2.650011783303574564, -7.500002219258004921 ) ) ;
#64083 = EDGE_CURVE ( 'NONE', #40232, #14053, #65711, .T. ) ;
#64084 = CARTESIAN_POINT ( 'NONE',  ( 8.724822372493999723, 3.750788346126100237, -8.315254653915399530 ) ) ;
#64086 = DIRECTION ( 'NONE',  ( -1.000000000000000000, 0.000000000000000000, 0.000000000000000000 ) ) ;
#64085 = CARTESIAN_POINT ( 'NONE',  ( 9.775076168957999911, -4.509700402263200125, 6.634524523592600254 ) ) ;
#64087 = CONICAL_SURFACE ( 'NONE', #4961, 1.349999998858999906, 0.7853981633972997312 ) ;
#64088 = CARTESIAN_POINT ( 'NONE',  ( 4.575859839683333874, -1.460959015002473826, -0.3926218265389207485 ) ) ;
#64089 = ORIENTED_EDGE ( 'NONE', *, *, #29718, .T. ) ;
#64090 = B_SPLINE_CURVE_WITH_KNOTS ( 'NONE', 3,
 ( #17714, #33795, #28908, #65930, #45659, #39376, #34140, #66966, #23297, #12812, #7907, #61044, #61722, #40400, #44974, #66625, #19072, #2654 ),
 .UNSPECIFIED., .F., .F.,
 ( 4, 2, 2, 2, 2, 2, 2, 2, 4 ),
 ( 0.1254181127249429095, 0.2190640428433491271, 0.3127099729617552892, 0.4063559030801615068, 0.5000018331985677245, 0.5936477633169741086, 0.6872936934353806038, 0.7809396235537870989, 0.8745855536721935941 ),
 .UNSPECIFIED. ) ;
#64091 = EDGE_CURVE ( 'NONE', #13916, #38357, #38457, .T. ) ;
#64092 = AXIS2_PLACEMENT_3D ( 'NONE', #66972, #44979, #39043 ) ;
#64093 = CARTESIAN_POINT ( 'NONE',  ( 7.475100008705002352, -3.230432416208002699, 6.447622763416998914 ) ) ;
#64094 = CARTESIAN_POINT ( 'NONE',  ( 9.405747021775999528, 3.038503783616799847, 6.656252755052399550 ) ) ;
#64095 = DIRECTION ( 'NONE',  ( -1.000000000000000000, 0.000000000000000000, 0.000000000000000000 ) ) ;
#64096 = CARTESIAN_POINT ( 'NONE',  ( 9.380781717619999682, -2.204246399534000034, 7.545378188773000261 ) ) ;
#64097 = CARTESIAN_POINT ( 'NONE',  ( 18.13004437684510961, 2.745098799910168808, -12.39110308483444634 ) ) ;
#64098 = CARTESIAN_POINT ( 'NONE',  ( 16.31144947526900069, -3.254927130315000028, -11.33654363332999893 ) ) ;
#64099 = CIRCLE ( 'NONE', #33989, 12.59999999999999964 ) ;
#64100 = CARTESIAN_POINT ( 'NONE',  ( 13.55168611684300117, -12.14221570691000096, -2.415203473206000151 ) ) ;
#64101 = CARTESIAN_POINT ( 'NONE',  ( 10.65896891525000001, 7.495473220363000344, -6.019650519997999716 ) ) ;
#64102 = CARTESIAN_POINT ( 'NONE',  ( 10.01660887879199890, -4.196341783741199372, -6.655513263298900029 ) ) ;
#64103 = CARTESIAN_POINT ( 'NONE',  ( 6.081432422588000541, 0.7848946462383999956, 1.064150538460000073 ) ) ;
#64104 = CARTESIAN_POINT ( 'NONE',  ( 12.80505043854146940, -1.760845406083394016, 12.47635457398814829 ) ) ;
#64105 = DIRECTION ( 'NONE',  ( 0.000000000000000000, -0.7071067811865475727, -0.7071067811865475727 ) ) ;
#64106 = ORIENTED_EDGE ( 'NONE', *, *, #11784, .F. ) ;
#64107 = CARTESIAN_POINT ( 'NONE',  ( 12.19004707749462924, 0.1118057330073172623, -12.69934308675517620 ) ) ;
#64108 = CARTESIAN_POINT ( 'NONE',  ( 10.82595391537419971, 4.716560378569699452, -7.986661909549199301 ) ) ;
#64109 = DIRECTION ( 'NONE',  ( 0.7071067811865709984, -0.7011937528853720014, -0.09125415560123631420 ) ) ;
#64110 = DIRECTION ( 'NONE',  ( 0.000000000000000000, 0.000000000000000000, -1.000000000000000000 ) ) ;
#64111 = CARTESIAN_POINT ( 'NONE',  ( 1.790556799208292027, -3.500000000000002220, 0.4581489286484968781 ) ) ;
#64112 = ORIENTED_EDGE ( 'NONE', *, *, #38884, .T. ) ;
#64113 = CARTESIAN_POINT ( 'NONE',  ( 7.714733813452927969, -2.650598945404480045, 7.676825647508595196 ) ) ;
#64114 = APPLICATION_PROTOCOL_DEFINITION ( 'draft international standard', 'automotive_design', 1998, #20833 ) ;
#64115 = CARTESIAN_POINT ( 'NONE',  ( 11.15278751119019773, -4.790480620979200133, -7.913556523549700294 ) ) ;
#64116 = CARTESIAN_POINT ( 'NONE',  ( 24.45617572375350690, -3.500160191032958945, 12.27858220308102766 ) ) ;
#64117 = CARTESIAN_POINT ( 'NONE',  ( 10.86180282789683460, -2.874603711584073462, -6.749639981064807337 ) ) ;
#64118 = CARTESIAN_POINT ( 'NONE',  ( 7.613624210631964040, 5.119274190779043998, -8.282492918286559203 ) ) ;
#64119 = CARTESIAN_POINT ( 'NONE',  ( 10.44125056272499918, 5.033400911533000510, -7.515315513715298934 ) ) ;
#64120 = ORIENTED_EDGE ( 'NONE', *, *, #67550, .T. ) ;
#64121 = AXIS2_PLACEMENT_3D ( 'NONE', #210, #64172, #58250 ) ;
#64122 = CARTESIAN_POINT ( 'NONE',  ( 9.576494682405000347, -4.593972507100000158, 5.662052676321000177 ) ) ;
#64123 = DIRECTION ( 'NONE',  ( -0.8660254018730039194, -3.203742570879014573E-12, 0.5000000033107019348 ) ) ;
#64124 = ORIENTED_EDGE ( 'NONE', *, *, #65257, .T. ) ;
#64125 = CARTESIAN_POINT ( 'NONE',  ( 23.66004879239100234, -3.393653467490999720, 13.50507469661999949 ) ) ;
#64126 = CARTESIAN_POINT ( 'NONE',  ( 8.058769353207999586, -2.432121990576000314, 6.597519606637999523 ) ) ;
#64127 = CARTESIAN_POINT ( 'NONE',  ( 9.170239158775000732, 4.769103072373000352, -8.666849124598000387 ) ) ;
#64128 = PRODUCT_RELATED_PRODUCT_CATEGORY ( 'part', '', ( #61183 ) ) ;
#64129 = VERTEX_POINT ( 'NONE', #12240 ) ;
#64130 = CARTESIAN_POINT ( 'NONE',  ( 6.520684977710001107, -0.7452859457610933047, 1.338676382078441307 ) ) ;
#64131 = CARTESIAN_POINT ( 'NONE',  ( 6.867785841228999821, 5.777496342847000754, -7.598381660561000395 ) ) ;
#64132 = CARTESIAN_POINT ( 'NONE',  ( 11.09999999999999964, -5.350000000000000533, 7.500000000000000000 ) ) ;
#64133 = CARTESIAN_POINT ( 'NONE',  ( 8.180537356029997653, -3.349941516901878025, 6.152975253528285116 ) ) ;
#64134 = VERTEX_POINT ( 'NONE', #17833 ) ;
#64135 = CARTESIAN_POINT ( 'NONE',  ( 9.380781717619999682, -2.204246399534000034, 7.545378188773000261 ) ) ;
#64136 = CARTESIAN_POINT ( 'NONE',  ( 24.63779784258400340, 11.77742452909999926, -3.228730981588999960 ) ) ;
#64137 = CARTESIAN_POINT ( 'NONE',  ( 5.500000000000000000, -1.300000000000000044, -10.46294468575700165 ) ) ;
#64138 = ORIENTED_EDGE ( 'NONE', *, *, #10045, .F. ) ;
#64139 = AXIS2_PLACEMENT_3D ( 'NONE', #23852, #32963, #49377 ) ;
#64140 = CARTESIAN_POINT ( 'NONE',  ( 6.169609839683334762, -0.1963495408493606265, -1.500000000000000222 ) ) ;
#64141 = CARTESIAN_POINT ( 'NONE',  ( 10.34939194037999854, -2.653148377029999949, -7.312413909354000374 ) ) ;
#64142 = EDGE_LOOP ( 'NONE', ( #39275, #68700 ) ) ;
#64143 = DIRECTION ( 'NONE',  ( -3.710543846949000018E-09, 3.726597655970000124E-11, -1.000000000000000000 ) ) ;
#64144 = CARTESIAN_POINT ( 'NONE',  ( 17.98055108453616668, -1.897673117161889467, -12.45627908894455338 ) ) ;
#64145 = CARTESIAN_POINT ( 'NONE',  ( 4.487510156732001043, -0.9398597281081001453, 1.241979931278999860 ) ) ;
#64146 = AXIS2_PLACEMENT_3D ( 'NONE', #61061, #65258, #34843 ) ;
#64147 = CARTESIAN_POINT ( 'NONE',  ( 11.60000000000000142, 3.244119941477265456, -6.982116912833853384 ) ) ;
#64148 = CARTESIAN_POINT ( 'NONE',  ( 16.04731601457200085, 3.899361801049999965, 11.84592592973999992 ) ) ;
#64149 = CARTESIAN_POINT ( 'NONE',  ( 7.100000000000000533, -11.06886219213000011, 1.536526853569999851 ) ) ;
#64150 = CARTESIAN_POINT ( 'NONE',  ( 24.14062698496121939, 12.48115957962327904, 3.363346990936225911 ) ) ;
#64151 = B_SPLINE_CURVE_WITH_KNOTS ( 'NONE', 3,
 ( #19230, #1870, #61884, #17252, #23189, #28445 ),
 .UNSPECIFIED., .F., .F.,
 ( 4, 1, 1, 4 ),
 ( 0.000000000000000000, 0.3333333333333000081, 0.6666666666667000474, 1.000000000000000000 ),
 .UNSPECIFIED. ) ;
#64152 = ORIENTED_EDGE ( 'NONE', *, *, #28809, .F. ) ;
#64153 = EDGE_CURVE ( 'NONE', #41105, #12259, #39152, .T. ) ;
#64154 = CARTESIAN_POINT ( 'NONE',  ( 8.734200250017998712, 4.093844212487689482, -8.386722339907899837 ) ) ;
#64155 = EDGE_CURVE ( 'NONE', #57180, #13267, #59003, .T. ) ;
#64156 = VERTEX_POINT ( 'NONE', #19890 ) ;
#64157 = CARTESIAN_POINT ( 'NONE',  ( 10.89227882974000039, 3.998355201738000630, 9.261308739708001170 ) ) ;
#64158 = CARTESIAN_POINT ( 'NONE',  ( 11.09991415876999987, 2.373387781209999936, -6.776601845694000481 ) ) ;
#64159 = AXIS2_PLACEMENT_3D ( 'NONE', #17272, #59573, #64804 ) ;
#64160 = CARTESIAN_POINT ( 'NONE',  ( 13.00000000005200107, 12.15994572112000149, 2.000334444851999738 ) ) ;
#64161 = CARTESIAN_POINT ( 'NONE',  ( 9.418385841233000377, 3.251172436837000301, -6.320036569851000152 ) ) ;
#64162 = CARTESIAN_POINT ( 'NONE',  ( 11.09999999999999964, 2.700688487044999864, -5.124965750789000296 ) ) ;
#64163 =( LENGTH_UNIT ( ) NAMED_UNIT ( * ) SI_UNIT ( .MILLI., .METRE. ) );
#64164 = CARTESIAN_POINT ( 'NONE',  ( 18.17177275037307638, 0.1018973686818568924, 13.89950237059086291 ) ) ;
#64165 = CARTESIAN_POINT ( 'NONE',  ( 9.366922563375464250, -5.649238375891439290, -8.083220911872984971 ) ) ;
#64166 = VERTEX_POINT ( 'NONE', #56949 ) ;
#64167 = CARTESIAN_POINT ( 'NONE',  ( 12.76431812838242230, 0.6240106079350378199, 13.88114051191589660 ) ) ;
#64168 = CARTESIAN_POINT ( 'NONE',  ( 10.63662282008600002, -3.405288783432600219, 6.540749699823199315 ) ) ;
#64169 = CARTESIAN_POINT ( 'NONE',  ( 13.59982064663300072, 2.566835632933000434E-13, 1.354472090042999897E-14 ) ) ;
#64170 = CARTESIAN_POINT ( 'NONE',  ( 9.272293146792000229, -3.705847642455000202, 9.096432253453999195 ) ) ;
#64172 = DIRECTION ( 'NONE',  ( 1.000000000000000000, 0.000000000000000000, 0.000000000000000000 ) ) ;
#64171 = CARTESIAN_POINT ( 'NONE',  ( 10.65550720192000078, 4.237674045823999869, 9.105219676299999065 ) ) ;
#64173 = CARTESIAN_POINT ( 'NONE',  ( 10.37457053952199892, 3.551693493661699730, -6.451042711717000167 ) ) ;
#64174 = EDGE_CURVE ( 'NONE', #6106, #31059, #56528, .T. ) ;
#64175 = CARTESIAN_POINT ( 'NONE',  ( 12.09999999999999787, -4.689830048140305685, 6.761031184901315605 ) ) ;
#64176 = AXIS2_PLACEMENT_3D ( 'NONE', #21083, #36128, #10932 ) ;
#64177 = CARTESIAN_POINT ( 'NONE',  ( 9.804975701332999449, 4.636077325177999420, -8.089163458558500608 ) ) ;
#64178 = CARTESIAN_POINT ( 'NONE',  ( 18.17607568152034148, 0.07112609253419145683, 12.69973757146476245 ) ) ;
#64179 = CARTESIAN_POINT ( 'NONE',  ( 6.815869870238000061, 0.2268263219687999821, -1.395656501875000011 ) ) ;
#64180 = DIRECTION ( 'NONE',  ( 0.000000000000000000, 1.000000000000000000, 0.000000000000000000 ) ) ;
#64181 = ORIENTED_EDGE ( 'NONE', *, *, #61787, .T. ) ;
#64182 = CARTESIAN_POINT ( 'NONE',  ( 7.416894353206999746, -3.448181789123000218, 9.222458996124998976 ) ) ;
#64183 = CARTESIAN_POINT ( 'NONE',  ( 9.216851002545999094, -2.832432432432000269, 6.822293592207000934 ) ) ;
#64184 = DIRECTION ( 'NONE',  ( 1.000000000000000000, 0.000000000000000000, 0.000000000000000000 ) ) ;
#64185 = CARTESIAN_POINT ( 'NONE',  ( 8.599999986286999132, -3.249999986289399789, -7.500000000038047787 ) ) ;
#64186 = VERTEX_POINT ( 'NONE', #14647 ) ;
#64187 = CARTESIAN_POINT ( 'NONE',  ( 11.01356641589999974, -2.786433584103999994, 6.253463831328000211 ) ) ;
#64188 = CIRCLE ( 'NONE', #50842, 12.60000000000000142 ) ;
#64189 = CARTESIAN_POINT ( 'NONE',  ( 11.60988784977536348, 3.148894096305599799, 7.548634759728509280 ) ) ;
#64190 = CARTESIAN_POINT ( 'NONE',  ( 11.22023584123000006, 3.883089684441999978, -8.854806321849000739 ) ) ;
#64191 = ORIENTED_EDGE ( 'NONE', *, *, #12414, .T. ) ;
#64192 = FACE_OUTER_BOUND ( 'NONE', #55661, .T. ) ;
#64193 = DIRECTION ( 'NONE',  ( 0.000000000000000000, 0.2461538461537955413, 0.9692307692307821076 ) ) ;
#64194 = CARTESIAN_POINT ( 'NONE',  ( 18.23375231277518083, 2.733957939387004821, -12.29982111303847958 ) ) ;
#64195 = CARTESIAN_POINT ( 'NONE',  ( 5.598857209342392949, 12.13471601159925406, 3.750691118698490811 ) ) ;
#64196 = CARTESIAN_POINT ( 'NONE',  ( 7.346670280409000497, 2.374037589774999901, 8.293392681990997772 ) ) ;
#64197 = ORIENTED_EDGE ( 'NONE', *, *, #11001, .T. ) ;
#64198 = CARTESIAN_POINT ( 'NONE',  ( 7.040773995485999137, -1.461948210420000116, 0.3790019357670000311 ) ) ;
#64199 = CARTESIAN_POINT ( 'NONE',  ( 7.508304719586000431, 4.512523768570999572, -9.154878768564000069 ) ) ;
#64200 = CARTESIAN_POINT ( 'NONE',  ( 8.551242329018723609, -3.500793602214988365, 5.833163798001932854 ) ) ;
#64201 = CARTESIAN_POINT ( 'NONE',  ( 10.94452754078378121, -3.491551460122512385, -6.788965764111623002 ) ) ;
#64202 = ORIENTED_EDGE ( 'NONE', *, *, #30875, .F. ) ;
#64203 = CARTESIAN_POINT ( 'NONE',  ( 11.53935620825160768, 11.69940330537452589, 1.870140110077450402 ) ) ;
#64204 = CARTESIAN_POINT ( 'NONE',  ( 11.25913316395000052, 11.80170809442000035, 1.433206434934999995 ) ) ;
#64205 = ORIENTED_EDGE ( 'NONE', *, *, #34615, .T. ) ;
#64206 = CARTESIAN_POINT ( 'NONE',  ( 24.44496487975900223, 3.224879802562000464, -12.03535984693000138 ) ) ;
#64207 = DIRECTION ( 'NONE',  ( -1.000000000000000000, 0.000000000000000000, 0.000000000000000000 ) ) ;
#64208 = CARTESIAN_POINT ( 'NONE',  ( 17.81345962944524075, 0.5694488842926277439, -13.88429844810376323 ) ) ;
#64209 = EDGE_CURVE ( 'NONE', #44214, #16046, #30058, .T. ) ;
#64210 = EDGE_CURVE ( 'NONE', #42806, #35474, #48103, .T. ) ;
#64211 = ORIENTED_EDGE ( 'NONE', *, *, #47919, .T. ) ;
#64212 = CARTESIAN_POINT ( 'NONE',  ( 10.64418092495376378, -2.624263734258304837, -6.377679599447885650 ) ) ;
#64213 = CARTESIAN_POINT ( 'NONE',  ( 11.48522412107029922, 4.047131449166419870, -6.609122077774299164 ) ) ;
#64214 = CARTESIAN_POINT ( 'NONE',  ( 11.35399482404719329, 3.445326802703547742, -11.33548354870907637 ) ) ;
#64216 = CIRCLE ( 'NONE', #43020, 0.5000000000000004441 ) ;
#64215 = CARTESIAN_POINT ( 'NONE',  ( 11.04272335273199879, -3.555125495332600138, 6.301916924546999255 ) ) ;
#64217 = VERTEX_POINT ( 'NONE', #19548 ) ;
#64218 = CARTESIAN_POINT ( 'NONE',  ( 8.822982780412001347, 2.678331728353000152, 8.735281589464001684 ) ) ;
#64219 = VERTEX_POINT ( 'NONE', #36307 ) ;
#64220 = LINE ( 'NONE', #64908, #58579 ) ;
#64221 = CARTESIAN_POINT ( 'NONE',  ( 16.00156003475500199, -9.132520755637999699, -8.493756974768999157 ) ) ;
#64222 = DIRECTION ( 'NONE',  ( 0.000000000000000000, 1.000000000000000000, 0.000000000000000000 ) ) ;
#64223 = ORIENTED_EDGE ( 'NONE', *, *, #12087, .F. ) ;
#64224 = B_SPLINE_SURFACE_WITH_KNOTS ( 'NONE', 3, 3, ( 
 ( #7166, #22547, #39331, #65886, #2609, #13118, #49818, #66578, #60997, #18356, #11711, #1577, #60652, #50169, #54366, #23250, #33050, #34447, #43890, #17311, #44593, #38636, #7862, #29196, #59958, #18698, #33401, #40031, #12069, #22895, #44246, #38990, #56442, #42351, #4926, #36403, #51201, #31855, #13461, #8204, #19032, #10515, #58076, #53170, #24629, #63302, #34784, #3294, #14141, #45616, #67259, #52829, #63650, #56093, #29553, #40359, #5272, #10180, #26612, #45949, #15429, #50854, #19376, #57720, #66922, #40697, #26262 ),
 ( #2949, #62026, #31507, #47592, #68899, #24282, #36756, #31176, #9828, #21014, #15768, #4576, #52480, #37097, #58410, #68547, #47931, #30, #61681, #21352, #61343, #13798, #35128, #29894, #8546, #25913, #47244, #20669, #41997, #10859, #65017, #49297, #43379, #33576, #65373, #43722, #38818, #26953, #22032, #48961, #16447, #37431, #27641, #12250, #28328, #49649, #1754, #17134, #58753, #54896, #38469, #1409, #22726, #59789, #54550, #5954, #372, #37776, #44072, #64325, #33232, #11892, #48619, #6647, #1070, #27988, #27295 ),
 ( #22381, #60144, #6996, #17494, #42680, #54194, #720, #63989, #64679, #16106, #32205, #53519, #5606, #48265, #21689, #43023, #59101, #11204, #32540, #53855, #16786, #38116, #59441, #11540, #32883, #6296, #55244, #7341, #23428, #28683, #29379, #40203, #50000, #44424, #44766, #13978, #45787, #29727, #18186, #51370, #34961, #67098, #18877, #51031, #50690, #61521, #35303, #66067, #8724, #56278, #60486, #30067, #60832, #2111, #39508, #12945, #33923, #61857, #12595, #45447, #3130, #23769, #56619, #19208, #24113, #40532, #34273 ),
 ( #2787, #24462, #55936, #23075, #18532, #8385, #66760, #65722, #13636, #17846, #55592, #39163, #7694, #29036, #50345, #8038, #2445, #45104, #66413, #39859, #61180, #13299, #34623, #19900, #41565, #31089, #52397, #9060, #63213, #4489, #68810, #20930, #9741, #37016, #14994, #35974, #10091, #4148, #25829, #15682, #31771, #41908, #30399, #40880, #24802, #68458, #62200, #52742, #67434, #4836, #14321, #56958, #46472, #42266, #35646, #51707, #3803, #25141, #67778, #47159, #20581, #41226, #46127, #62537, #63570, #26178, #31426 ) ),
 .UNSPECIFIED., .F., .F., .F.,
 ( 4, 4 ),
 ( 4, 1, 1, 1, 1, 1, 1, 1, 1, 1, 1, 1, 1, 1, 1, 1, 1, 1, 1, 1, 1, 1, 1, 1, 1, 1, 1, 1, 1, 1, 1, 1, 1, 1, 1, 1, 1, 1, 1, 1, 1, 1, 1, 1, 1, 1, 1, 1, 1, 1, 1, 1, 1, 1, 1, 1, 1, 1, 1, 1, 1, 1, 1, 1, 4 ),
 ( -0.02000000000000000042, 1.020000000000000018 ),
 ( -0.02000000000000000042, -0.003749999999999999861, 0.01250000000000000069, 0.02875000000000000125, 0.04499999999999999833, 0.06124999999999999889, 0.07749999999999999944, 0.09375000000000000000, 0.1100000000000000006, 0.1262500000000000011, 0.1424999999999999878, 0.1587500000000000022, 0.1749999999999999889, 0.1912500000000000033, 0.2074999999999999900, 0.2237500000000000044, 0.2399999999999999911, 0.2562499999999999778, 0.2725000000000000200, 0.2887500000000000067, 0.3049999999999999933, 0.3212499999999999800, 0.3375000000000000222, 0.3537500000000000089, 0.3699999999999999956, 0.3862499999999999822, 0.4025000000000000244, 0.4187500000000000111, 0.4349999999999999978, 0.4512499999999999845, 0.4675000000000000266, 0.4837500000000000133, 0.5000000000000000000, 0.5162499999999999867, 0.5324999999999999734, 0.5487499999999999600, 0.5649999999999999467, 0.5812500000000000444, 0.5975000000000000311, 0.6137500000000000178, 0.6300000000000000044, 0.6462499999999999911, 0.6624999999999999778, 0.6787499999999999645, 0.6949999999999999512, 0.7112500000000000488, 0.7275000000000000355, 0.7437500000000000222, 0.7600000000000000089, 0.7762499999999999956, 0.7924999999999999822, 0.8087499999999999689, 0.8249999999999999556, 0.8412500000000000533, 0.8575000000000000400, 0.8737500000000000266, 0.8900000000000000133, 0.9062500000000000000, 0.9224999999999999867, 0.9387499999999999734, 0.9549999999999999600, 0.9712499999999999467, 0.9875000000000000444, 1.003749999999999920, 1.020000000000000018 ),
 .UNSPECIFIED. ) ;
#64225 = CARTESIAN_POINT ( 'NONE',  ( 12.80505043854146940, -1.874999999999999778, -12.57541666120756396 ) ) ;
#64226 = DIRECTION ( 'NONE',  ( 0.000000000000000000, -1.000000000000000000, 0.000000000000000000 ) ) ;
#64227 = CARTESIAN_POINT ( 'NONE',  ( 8.960616452296999768, 2.899999999999999911, 6.279946362737000243 ) ) ;
#64228 = CARTESIAN_POINT ( 'NONE',  ( 21.65000086032565108, -2.247091401841000284E-13, 4.272138198758000206E-13 ) ) ;
#64229 = CARTESIAN_POINT ( 'NONE',  ( 12.58164121395691559, -1.823227133926378585, -13.88077287699123197 ) ) ;
#64230 = CARTESIAN_POINT ( 'NONE',  ( 10.94487616594229884, -4.303437140848100029, -6.543508100188799581 ) ) ;
#64231 = CARTESIAN_POINT ( 'NONE',  ( 7.100000000000000533, -4.000000000000000000, -7.500000000000000000 ) ) ;
#64232 = CARTESIAN_POINT ( 'NONE',  ( 17.87828936854287676, -3.124432504806129440, 12.20647160316251068 ) ) ;
#64233 = ORIENTED_EDGE ( 'NONE', *, *, #5726, .T. ) ;
#64234 = CARTESIAN_POINT ( 'NONE',  ( 10.92968717260509948, -4.687649763627899979, -8.622362941748999532 ) ) ;
#64235 = EDGE_CURVE ( 'NONE', #68711, #2919, #552, .T. ) ;
#64236 = EDGE_LOOP ( 'NONE', ( #24960, #51819, #18942, #22637, #25339 ) ) ;
#64237 = B_SPLINE_CURVE_WITH_KNOTS ( 'NONE', 1,
 ( #40022, #62019 ),
 .UNSPECIFIED., .F., .F.,
 ( 2, 2 ),
 ( 0.000000000000000000, 1.000000000000000000 ),
 .UNSPECIFIED. ) ;
#64238 = CARTESIAN_POINT ( 'NONE',  ( 25.34478631770858925, 2.688917760716752703, -11.33837770301359527 ) ) ;
#64239 = CARTESIAN_POINT ( 'NONE',  ( 4.900006121741999898, -1.599333684796359956, 1.229093439949830557 ) ) ;
#64240 = EDGE_CURVE ( 'NONE', #13432, #51187, #58135, .T. ) ;
#64241 = CARTESIAN_POINT ( 'NONE',  ( 10.91624242361999997, 5.459834480072999874, -8.642877574935999618 ) ) ;
#64242 = CARTESIAN_POINT ( 'NONE',  ( 10.76232069631999977, -3.259150589222000072, -8.644998763029001054 ) ) ;
#64243 = VECTOR ( 'NONE', #29760, 1000.000000000000000 ) ;
#64244 = DIRECTION ( 'NONE',  ( 0.000000000000000000, 0.000000000000000000, -1.000000000000000000 ) ) ;
#64245 = CARTESIAN_POINT ( 'NONE',  ( 7.964620641636996901, 2.867893108869000507, -6.758951315555000505 ) ) ;
#64246 = CARTESIAN_POINT ( 'NONE',  ( 10.00637913184999839, 5.119263020957999899, 8.420380450036001108 ) ) ;
#64247 = ORIENTED_EDGE ( 'NONE', *, *, #2748, .T. ) ;
#64248 = CARTESIAN_POINT ( 'NONE',  ( 18.53573769406200356, 2.787008136214999876, 11.27235516822999983 ) ) ;
#64249 = CARTESIAN_POINT ( 'NONE',  ( 11.11845610223999969, 5.767025078915000158, 7.178418469370999588 ) ) ;
#64250 = B_SPLINE_CURVE_WITH_KNOTS ( 'NONE', 3,
 ( #67583, #67240, #40680, #56422, #3278, #50835, #61663, #2930, #62010, #8527, #35447, #24258, #56073, #13442, #14467, #46279, #45598, #14122 ),
 .UNSPECIFIED., .F., .F.,
 ( 4, 2, 2, 2, 2, 2, 2, 2, 4 ),
 ( 0.000000000000000000, 0.1250000000000003331, 0.2500000000000006661, 0.3750000000000009992, 0.5000000000000013323, 0.6250000000000009992, 0.7500000000000006661, 0.8750000000000003331, 1.000000000000000000 ),
 .UNSPECIFIED. ) ;
#64251 = B_SPLINE_CURVE_WITH_KNOTS ( 'NONE', 3,
 ( #11969, #22800, #34695, #23844 ),
 .UNSPECIFIED., .F., .F.,
 ( 4, 4 ),
 ( 0.000000000000000000, 1.000000000000000000 ),
 .UNSPECIFIED. ) ;
#64252 = CARTESIAN_POINT ( 'NONE',  ( 24.30001682246400208, -8.938702682732001747, -8.938676171235998780 ) ) ;
#64253 = CARTESIAN_POINT ( 'NONE',  ( 11.94366954483529852, -3.514796851401900124, 8.248643701125299543 ) ) ;
#64254 = CARTESIAN_POINT ( 'NONE',  ( 17.77441288034700051, 3.189751316310999840, -11.45074679932000095 ) ) ;
#64255 = CARTESIAN_POINT ( 'NONE',  ( 11.12133729122639991, 3.134101783108900197, -7.477221318588949117 ) ) ;
#64256 = ADVANCED_FACE ( 'NONE', ( #16354 ), #42798, .F. ) ;
#64257 = CARTESIAN_POINT ( 'NONE',  ( 10.94856425838729841, 4.366288724067763916, -9.227056792578350652 ) ) ;
#64258 = CARTESIAN_POINT ( 'NONE',  ( 24.51195315439300160, -8.843582221221000239, -9.168329703202999781 ) ) ;
#64259 = DIRECTION ( 'NONE',  ( 0.000000000000000000, 0.7198977633594745296, -0.6940801180771756229 ) ) ;
#64260 =( LENGTH_UNIT ( ) NAMED_UNIT ( * ) SI_UNIT ( .MILLI., .METRE. ) );
#64261 = ORIENTED_EDGE ( 'NONE', *, *, #61315, .T. ) ;
#64262 = CARTESIAN_POINT ( 'NONE',  ( 11.09999938828999966, 12.24999938819000000, 1.815300846655999940E-09 ) ) ;
#64263 = LINE ( 'NONE', #16715, #24642 ) ;
#64264 = CARTESIAN_POINT ( 'NONE',  ( 18.13779378220191063, 2.273859756726421377, 13.71877938508613326 ) ) ;
#64265 = CARTESIAN_POINT ( 'NONE',  ( 24.62773497368900166, 8.736972494143998347, -9.042113496790999960 ) ) ;
#64266 = CARTESIAN_POINT ( 'NONE',  ( 10.66995391537419913, -3.056324258617099776, -8.140910455049299443 ) ) ;
#64267 = EDGE_LOOP ( 'NONE', ( #37604, #50009, #40815, #9358 ) ) ;
#64268 = CARTESIAN_POINT ( 'NONE',  ( 6.950045635439000336, -13.87069231928999891, -4.225386915259999654 ) ) ;
#64269 = CARTESIAN_POINT ( 'NONE',  ( 8.758795280412000395, 3.977267228909999730, 9.308925224542001331 ) ) ;
#64270 = CIRCLE ( 'NONE', #10686, 12.50000000000000178 ) ;
#64272 = CARTESIAN_POINT ( 'NONE',  ( 10.97028665956023019, -4.742415037725370652, -8.549395343567622874 ) ) ;
#64271 = CARTESIAN_POINT ( 'NONE',  ( 9.202245280414000916, 5.095038542659000136, -6.157541456184000062 ) ) ;
#64273 = CARTESIAN_POINT ( 'NONE',  ( 10.84289849785072590, -2.713620053740499305, -7.026897974086598886 ) ) ;
#64274 = VERTEX_POINT ( 'NONE', #59013 ) ;
#64275 = CARTESIAN_POINT ( 'NONE',  ( 11.12915085989000019, 3.083869275439000024, 8.585995236726001067 ) ) ;
#64276 = CARTESIAN_POINT ( 'NONE',  ( 18.20194470744738524, -2.188139888162251800, -13.82794850388582475 ) ) ;
#64277 = CARTESIAN_POINT ( 'NONE',  ( 11.75718044953559804, 4.889766368533900120, 7.036033215662999218 ) ) ;
#64278 = CARTESIAN_POINT ( 'NONE',  ( 9.479212726990999371, -4.071727350623000063, 9.089303488377000306 ) ) ;
#64279 = CARTESIAN_POINT ( 'NONE',  ( 8.860769353209001054, -2.935738482289000029, 6.259841087764999479 ) ) ;
#64280 = ORIENTED_EDGE ( 'NONE', *, *, #53898, .F. ) ;
#64281 = CARTESIAN_POINT ( 'NONE',  ( 8.957392219593000249, 2.678331728353000152, 8.735281589464001684 ) ) ;
#64283 = CARTESIAN_POINT ( 'NONE',  ( 10.58470685321000104, -2.966812129551000154, -8.831977776575000050 ) ) ;
#64282 = CARTESIAN_POINT ( 'NONE',  ( 10.91991225946278199, 4.700767082376348327, -6.977491532540834207 ) ) ;
#64284 = CARTESIAN_POINT ( 'NONE',  ( 7.829206492768003400, -3.883838858848270181, 9.258058093495069585 ) ) ;
#64285 = CARTESIAN_POINT ( 'NONE',  ( 10.83668192271000130, -4.288535286065000562, 9.448729895547000268 ) ) ;
#64286 = CARTESIAN_POINT ( 'NONE',  ( 1.213972969267000046, 1.556166911672999920, -2.863499806755999799 ) ) ;
#64287 = VERTEX_POINT ( 'NONE', #37683 ) ;
#64288 = CARTESIAN_POINT ( 'NONE',  ( 5.688359839683333696, -0.7554284705563480973, -1.310679582531387277 ) ) ;
#64289 = CARTESIAN_POINT ( 'NONE',  ( 10.85410941423799791, -3.257202320419700037, 8.174686939644999484 ) ) ;
#64290 = CARTESIAN_POINT ( 'NONE',  ( 11.35502763632549872, 2.839566963815999934, 8.035454525731699604 ) ) ;
#64291 = ORIENTED_EDGE ( 'NONE', *, *, #6880, .F. ) ;
#64292 = EDGE_CURVE ( 'NONE', #51764, #21230, #40540, .T. ) ;
#64293 = ADVANCED_FACE ( 'NONE', ( #41554 ), #42255, .F. ) ;
#64294 = CARTESIAN_POINT ( 'NONE',  ( 9.807804719590000886, 3.988943694240999704, -8.966360307350999648 ) ) ;
#64295 = EDGE_CURVE ( 'NONE', #24787, #49573, #16012, .T. ) ;
#64296 = CARTESIAN_POINT ( 'NONE',  ( 12.23408645687631591, 2.036599147259922749, -12.43432143783615729 ) ) ;
#64297 = CARTESIAN_POINT ( 'NONE',  ( 11.85034208742530026, -4.630634088820300143, 6.508707709313799050 ) ) ;
#64298 = CARTESIAN_POINT ( 'NONE',  ( 7.399999875133000060, 0.9999998751120001694, 1.219901821080000081E-10 ) ) ;
#64299 = CARTESIAN_POINT ( 'NONE',  ( 18.16777246613359154, 2.623276685346445980, -13.64654026446401502 ) ) ;
#64300 = VERTEX_POINT ( 'NONE', #57626 ) ;
#64301 = CARTESIAN_POINT ( 'NONE',  ( 8.239941940377999430, -2.735207418315000361, 6.771977475428999860 ) ) ;
#64302 = CARTESIAN_POINT ( 'NONE',  ( 5.555026506349999948, -1.500000000000000000, 0.000000000000000000 ) ) ;
#64303 = ORIENTED_EDGE ( 'NONE', *, *, #66051, .T. ) ;
#64304 = CARTESIAN_POINT ( 'NONE',  ( 12.35197574246973673, -3.042005152232414744, -12.22727356655694209 ) ) ;
#64305 = CARTESIAN_POINT ( 'NONE',  ( 10.43210941423799909, 4.641185166475500168, 8.082391773166900606 ) ) ;
#64306 = CARTESIAN_POINT ( 'NONE',  ( 9.820199962102000413, 3.883325513302000154, 6.055618835924000187 ) ) ;
#64307 = CARTESIAN_POINT ( 'NONE',  ( 11.05675868087999980, 2.811466576753000268, -4.847348033755999985 ) ) ;
#64308 = CARTESIAN_POINT ( 'NONE',  ( 9.643930206848999376, 5.250000000000000000, 7.500000000000000000 ) ) ;
#64309 = CARTESIAN_POINT ( 'NONE',  ( 10.66951732929000052, -4.592671928130000580, 5.841406818427000047 ) ) ;
#64310 = CARTESIAN_POINT ( 'NONE',  ( 17.99694387276892726, -0.5707228546307235861, -12.58707662888203771 ) ) ;
#64311 = CARTESIAN_POINT ( 'NONE',  ( 12.31573549167064030, 2.888971355165489197, -12.35241121502826545 ) ) ;
#64312 = CARTESIAN_POINT ( 'NONE',  ( 10.30487885159599770, -3.003595720052600448, -7.381132626649399064 ) ) ;
#64313 = CARTESIAN_POINT ( 'NONE',  ( 9.475899447075999404, 4.122021000979000149, 9.013569734175000292 ) ) ;
#64314 = VERTEX_POINT ( 'NONE', #42933 ) ;
#64315 = DIRECTION ( 'NONE',  ( 1.000000000000000000, 0.000000000000000000, 0.000000000000000000 ) ) ;
#64316 = CARTESIAN_POINT ( 'NONE',  ( 9.260957905557225089, 2.777225843657625592, 6.918122793223488998 ) ) ;
#64317 = CARTESIAN_POINT ( 'NONE',  ( 11.56571517796000137, 12.12283255502000046, 1.989142034170999995 ) ) ;
#64318 = CARTESIAN_POINT ( 'NONE',  ( 18.02766945781917585, 1.934589073148402116, 12.45059934707292726 ) ) ;
#64319 = CARTESIAN_POINT ( 'NONE',  ( 11.12439302932000018, 6.497997223551999824, 5.557915343071999636 ) ) ;
#64320 = CARTESIAN_POINT ( 'NONE',  ( 10.96245900765000059, 7.417179809027999227, 6.111322237281999747 ) ) ;
#64321 = CARTESIAN_POINT ( 'NONE',  ( 12.39828795418346274, -0.4745523467757941094, -12.68806523616956206 ) ) ;
#64322 = DIRECTION ( 'NONE',  ( 1.000000000000000000, 0.000000000000000000, 0.000000000000000000 ) ) ;
#64323 = ORIENTED_EDGE ( 'NONE', *, *, #66706, .T. ) ;
#64324 = CARTESIAN_POINT ( 'NONE',  ( 12.07980306947244031, -2.459616342362513919, 12.35762317364248020 ) ) ;
#64325 = CARTESIAN_POINT ( 'NONE',  ( 9.023797255587998833, -2.859210004667000149, -7.451702546394010085 ) ) ;
#64326 = CARTESIAN_POINT ( 'NONE',  ( 9.525000000000000355, -4.417172942406000224, 8.783926296998000538 ) ) ;
#64327 = B_SPLINE_CURVE_WITH_KNOTS ( 'NONE', 3,
 ( #48492, #32080, #16322, #10389, #597, #16667 ),
 .UNSPECIFIED., .F., .F.,
 ( 4, 2, 4 ),
 ( 0.000000000000000000, 0.5000000000000000000, 1.000000000000000000 ),
 .UNSPECIFIED. ) ;
#64328 = CARTESIAN_POINT ( 'NONE',  ( 4.599999999999999645, -1.760845406083394682, 12.47635457398814829 ) ) ;
#64329 = CARTESIAN_POINT ( 'NONE',  ( 10.79262282008599882, -3.548418513060800361, 6.771613406921599854 ) ) ;
#64330 = AXIS2_PLACEMENT_3D ( 'NONE', #13336, #34660, #55973 ) ;
#64331 = CARTESIAN_POINT ( 'NONE',  ( 10.57564694612699974, 3.068007311611700150, -7.871941502982999772 ) ) ;
#64332 = EDGE_CURVE ( 'NONE', #41105, #62590, #53078, .T. ) ;
#64333 = CARTESIAN_POINT ( 'NONE',  ( 12.64055030734119001, 0.7009231686363525116, 12.58048995873113896 ) ) ;
#64334 = CARTESIAN_POINT ( 'NONE',  ( 0.5323593903514999282, -3.136585174263000209, 0.6804425983637999442 ) ) ;
#64335 = CARTESIAN_POINT ( 'NONE',  ( 5.214996238499456815, -0.1443403793638295407, 1.113928983458401856 ) ) ;
#64336 = EDGE_CURVE ( 'NONE', #56866, #16567, #65547, .T. ) ;
#64337 = CARTESIAN_POINT ( 'NONE',  ( 12.55429323164597299, 3.072583267488710579, 12.29953727834259603 ) ) ;
#64339 = CARTESIAN_POINT ( 'NONE',  ( 7.533885841228999958, 4.623631324973000112, 8.651459902566999816 ) ) ;
#64338 = CARTESIAN_POINT ( 'NONE',  ( 10.36624205625100004, 3.590523439766200031, -8.565862728991998409 ) ) ;
#64340 = CARTESIAN_POINT ( 'NONE',  ( 10.98995257254739855, 2.904643075091000171, -7.818564472783199548 ) ) ;
#64341 = CARTESIAN_POINT ( 'NONE',  ( 12.68562097720201898, 12.11848650044656672, -3.165127050490344374 ) ) ;
#64342 = CARTESIAN_POINT ( 'NONE',  ( 10.69016084123000176, 4.391264627567999845, -8.802335896973000118 ) ) ;
#64343 = DIRECTION ( 'NONE',  ( -0.7071067040009368920, 0.000000000000000000, -0.7071068583721498158 ) ) ;
#64345 = DIRECTION ( 'NONE',  ( -1.000000000000000000, 0.000000000000000000, 0.000000000000000000 ) ) ;
#64344 = CARTESIAN_POINT ( 'NONE',  ( 10.34365768245000083, -4.000000000000000000, -4.787564842381000219 ) ) ;
#64346 = DIRECTION ( 'NONE',  ( 1.000000000000000000, 0.000000000000000000, 0.000000000000000000 ) ) ;
#64347 = VERTEX_POINT ( 'NONE', #48175 ) ;
#64348 = CARTESIAN_POINT ( 'NONE',  ( 12.29893172067548690, 0.3669524139187689271, 12.69287054299043227 ) ) ;
#64349 = CARTESIAN_POINT ( 'NONE',  ( 23.85399087666008811, -9.637233594680219895, 9.713115531358498700 ) ) ;
#64350 = CARTESIAN_POINT ( 'NONE',  ( 12.01556330254184601, -11.99897551495956272, 3.593484177663201606 ) ) ;
#64351 = CARTESIAN_POINT ( 'NONE',  ( 18.27937482164660565, 2.670364552387198387, -12.31525491565053798 ) ) ;
#64352 = CARTESIAN_POINT ( 'NONE',  ( 12.25686392147160220, -2.040034559784666968, 13.85057184956195542 ) ) ;
#64353 = CARTESIAN_POINT ( 'NONE',  ( 10.85987047770900382, -5.250000000000000000, 7.249610810850630749 ) ) ;
#64354 = CARTESIAN_POINT ( 'NONE',  ( 11.00000000000000000, 3.031410575668799900, 7.825000000000000178 ) ) ;
#64355 = ORIENTED_EDGE ( 'NONE', *, *, #52874, .T. ) ;
#64356 = CARTESIAN_POINT ( 'NONE',  ( 23.60000000000000142, 0.000000000000000000, 0.000000000000000000 ) ) ;
#64357 = CARTESIAN_POINT ( 'NONE',  ( 18.01246087681489172, -10.82907928505310124, 4.296547899025035200 ) ) ;
#64358 = AXIS2_PLACEMENT_3D ( 'NONE', #30617, #52621, #4026 ) ;
#64359 = CARTESIAN_POINT ( 'NONE',  ( 27.64127793187000037, -5.599999999999999645, 6.571291218949999902 ) ) ;
#64360 = DIRECTION ( 'NONE',  ( -1.000000000000000000, 0.000000000000000000, 0.000000000000000000 ) ) ;
#64361 = CARTESIAN_POINT ( 'NONE',  ( 17.96930180488788409, 2.968443477542578979, -12.33001868694669589 ) ) ;
#64362 = CARTESIAN_POINT ( 'NONE',  ( 10.33253786428999987, -2.899999999999999911, 6.571291218949999902 ) ) ;
#64363 = CARTESIAN_POINT ( 'NONE',  ( 8.314979508587148516, 2.649972834346558059, -7.499998738096613771 ) ) ;
#64364 = ADVANCED_FACE ( 'NONE', ( #47147 ), #26029, .F. ) ;
#64365 = FACE_OUTER_BOUND ( 'NONE', #53728, .T. ) ;
#64366 = CARTESIAN_POINT ( 'NONE',  ( 10.05463185321000097, -3.531218470783999752, -9.119231780812000920 ) ) ;
#64367 = AXIS2_PLACEMENT_3D ( 'NONE', #40737, #4005, #67637 ) ;
#64368 = CARTESIAN_POINT ( 'NONE',  ( 12.56925896342638183, 1.825837054105086787, 13.88044190432479041 ) ) ;
#64369 = EDGE_CURVE ( 'NONE', #43864, #57137, #19747, .T. ) ;
#64370 = CARTESIAN_POINT ( 'NONE',  ( 25.39990883465370430, 2.060145121004215873, 11.21224557561489910 ) ) ;
#64371 = EDGE_CURVE ( 'NONE', #2412, #19919, #28935, .T. ) ;
#64372 = CARTESIAN_POINT ( 'NONE',  ( 24.70869262301700076, 12.32777590421999925, 2.948351121266000074 ) ) ;
#64373 = CARTESIAN_POINT ( 'NONE',  ( 8.786046699800500903, -3.154588942369298099, -7.961595344540238095 ) ) ;
#64374 = ORIENTED_EDGE ( 'NONE', *, *, #4803, .T. ) ;
#64375 = CARTESIAN_POINT ( 'NONE',  ( 7.355268297462892235, 3.356766528212881795, 9.118107836026387858 ) ) ;
#64376 = CARTESIAN_POINT ( 'NONE',  ( 11.57210672858429845, -4.692204557952299737, 8.020722037455799480 ) ) ;
#64377 = VERTEX_POINT ( 'NONE', #32108 ) ;
#64378 = AXIS2_PLACEMENT_3D ( 'NONE', #5882, #59718, #64609 ) ;
#64379 = CARTESIAN_POINT ( 'NONE',  ( 24.30000000000000071, 10.83443035398000021, -3.855530949778000149 ) ) ;
#64380 = CARTESIAN_POINT ( 'NONE',  ( 11.45348876160960039, -4.885820101980599794, -8.421216112044099589 ) ) ;
#64381 = ORIENTED_EDGE ( 'NONE', *, *, #26355, .F. ) ;
#64382 = CARTESIAN_POINT ( 'NONE',  ( 10.85679632507500081, 4.490665650747399873, 6.590394082213600235 ) ) ;
#64383 = CARTESIAN_POINT ( 'NONE',  ( 6.778816671981999775, -0.8882170986559999593, 0.6661914818925001036 ) ) ;
#64384 = CARTESIAN_POINT ( 'NONE',  ( 8.748305582559998683, -3.908727042518870043, -8.362426869835999810 ) ) ;
#64385 = CARTESIAN_POINT ( 'NONE',  ( 18.07439970769999960, -3.110573872314000177, 11.47478625844000177 ) ) ;
#64386 = CARTESIAN_POINT ( 'NONE',  ( 11.02812378248509795, -4.416893162838900544, -6.711274001288999536 ) ) ;
#64387 = CARTESIAN_POINT ( 'NONE',  ( 12.18504202264279712, 0.08143095636433357598, -13.89969831568923020 ) ) ;
#64388 = CARTESIAN_POINT ( 'NONE',  ( 6.967819507915497645, 0.1833634693192602583, -1.128230691838603805 ) ) ;
#64389 = CARTESIAN_POINT ( 'NONE',  ( 9.662447522843001124, -4.824180051339999942, -8.517611033492999084 ) ) ;
#64390 = CARTESIAN_POINT ( 'NONE',  ( 12.99518154839200257, 11.72294562696999876, 1.966205464704999795 ) ) ;
#64391 = ORIENTED_EDGE ( 'NONE', *, *, #52184, .T. ) ;
#64392 = CARTESIAN_POINT ( 'NONE',  ( 10.11453584122999949, 5.322769172805999816, -7.951018786192998178 ) ) ;
#64393 = ORIENTED_EDGE ( 'NONE', *, *, #26837, .F. ) ;
#64394 = EDGE_CURVE ( 'NONE', #65751, #17545, #1417, .T. ) ;
#64395 = CARTESIAN_POINT ( 'NONE',  ( 9.973493989215999278, 4.344963986309999804, -9.321593970653999861 ) ) ;
#64396 = ORIENTED_EDGE ( 'NONE', *, *, #57372, .T. ) ;
#64397 = CARTESIAN_POINT ( 'NONE',  ( 18.20180239440930947, -2.898381337075406794, -13.69738341131825266 ) ) ;
#64398 = CARTESIAN_POINT ( 'NONE',  ( 17.86131849338084265, -3.044913046804099466, -12.30775201372483885 ) ) ;
#64399 = CARTESIAN_POINT ( 'NONE',  ( 10.57529832096847677, 3.253995305422127782, 7.955594773867785463 ) ) ;
#64400 = CARTESIAN_POINT ( 'NONE',  ( 13.49980696792483137, 10.14812545701388657, 7.065329385613729585 ) ) ;
#64401 = B_SPLINE_CURVE_WITH_KNOTS ( 'NONE', 3,
 ( #44107, #33611, #39195, #54930 ),
 .UNSPECIFIED., .F., .F.,
 ( 4, 4 ),
 ( 0.8745714697001524263, 1.000000000000000000 ),
 .UNSPECIFIED. ) ;
#64402 = CARTESIAN_POINT ( 'NONE',  ( 9.848253563160000112, -4.436921580929999998, 6.148020168057000134 ) ) ;
#64403 = CARTESIAN_POINT ( 'NONE',  ( 17.88333207268022917, -1.943312949537261636, -12.56472734206913522 ) ) ;
#64404 = CARTESIAN_POINT ( 'NONE',  ( 12.64263601961789263, 0.6038715862870271955, 13.88233985103439494 ) ) ;
#64405 = EDGE_LOOP ( 'NONE', ( #49544, #26133, #7635, #9921, #50615, #52072, #19693, #4805, #25424 ) ) ;
#64406 = CARTESIAN_POINT ( 'NONE',  ( 12.18555568849200021, 11.56145208044000050, -4.416819796118000241 ) ) ;
#64407 = CARTESIAN_POINT ( 'NONE',  ( 18.26809521658400115, 11.96733320521999921, -3.503025077341000326 ) ) ;
#64408 = CARTESIAN_POINT ( 'NONE',  ( 9.074925248765625341, 3.255423617190434271, 7.959497855362744012 ) ) ;
#64409 = CARTESIAN_POINT ( 'NONE',  ( 4.902164461081000013, 0.3345035914287000089, -1.292002046660999826 ) ) ;
#64410 = AXIS2_PLACEMENT_3D ( 'NONE', #60912, #51113, #3889 ) ;
#64411 = ADVANCED_BREP_SHAPE_REPRESENTATION ( '', ( #31079, #9676 ), #52154 ) ;
#64412 = CARTESIAN_POINT ( 'NONE',  ( 8.798539158775000146, 5.851083642416999631, -7.072167224702999633 ) ) ;
#64413 = CARTESIAN_POINT ( 'NONE',  ( 18.40156003475500057, -3.148349829928000165, 12.06792178657999948 ) ) ;
#64414 = CARTESIAN_POINT ( 'NONE',  ( 9.856713838269000050, -4.814118338972999567, -8.929571672388000536 ) ) ;
#64415 = ORIENTED_EDGE ( 'NONE', *, *, #41401, .F. ) ;
#64416 = ORIENTED_EDGE ( 'NONE', *, *, #30611, .T. ) ;
#64417 = DIRECTION ( 'NONE',  ( 1.000000000000000000, 0.000000000000000000, 0.000000000000000000 ) ) ;
#64418 = ADVANCED_FACE ( 'NONE', ( #44673 ), #53893, .T. ) ;
#64419 = AXIS2_PLACEMENT_3D ( 'NONE', #57547, #48440, #20492 ) ;
#64420 = DIRECTION ( 'NONE',  ( 0.7071059447853028646, -0.7071076175868028502, 3.669598041139013828E-09 ) ) ;
#64421 = DIRECTION ( 'NONE',  ( 0.000000000000000000, -1.000000000000000000, 0.000000000000000000 ) ) ;
#64422 = DIRECTION ( 'NONE',  ( 0.000000000000000000, -1.000000000000000000, 0.000000000000000000 ) ) ;
#64423 = FACE_OUTER_BOUND ( 'NONE', #12476, .T. ) ;
#64424 = CARTESIAN_POINT ( 'NONE',  ( 9.178734463322998138, 4.104624583183299258, -8.498947444525299488 ) ) ;
#64426 = CARTESIAN_POINT ( 'NONE',  ( 8.334999384030673752, 4.800016001909910734, -6.110656516449306075 ) ) ;
#64425 = CARTESIAN_POINT ( 'NONE',  ( 10.78622949779699880, -3.519000825516800379, 6.778648208007999720 ) ) ;
#64427 = CARTESIAN_POINT ( 'NONE',  ( 11.14393020684970104, -2.750000000000000000, 7.500000000000000000 ) ) ;
#64428 = ORIENTED_EDGE ( 'NONE', *, *, #32833, .F. ) ;
#64429 = VECTOR ( 'NONE', #16898, 1000.000000000000114 ) ;
#64430 = FACE_OUTER_BOUND ( 'NONE', #63545, .T. ) ;
#64431 = CARTESIAN_POINT ( 'NONE',  ( 8.062814847549001129, -3.480055400096998319, 6.228346641557002350 ) ) ;
#64432 = CARTESIAN_POINT ( 'NONE',  ( 8.958265421554999719, 3.759926620436100375, 6.258138488953999712 ) ) ;
#64433 = CARTESIAN_POINT ( 'NONE',  ( 5.694051797832758055, -13.02176618664603502, -2.006311339876389432 ) ) ;
#64434 = CIRCLE ( 'NONE', #4158, 11.79499999999999993 ) ;
#64435 = CARTESIAN_POINT ( 'NONE',  ( 9.629020610622001541, -5.794331084664000819, 7.414872097535999629 ) ) ;
#64436 = CARTESIAN_POINT ( 'NONE',  ( 17.77858768906835962, 3.083996659899494563, -12.29614209097632838 ) ) ;
#64437 = CARTESIAN_POINT ( 'NONE',  ( 16.13869549901199818, -3.415897281711999689, -11.19349503352999875 ) ) ;
#64438 = CARTESIAN_POINT ( 'NONE',  ( 10.01459632033899894, -4.929952350555500296, -7.120485934352199564 ) ) ;
#64439 = CARTESIAN_POINT ( 'NONE',  ( 6.283089701056000287, -1.251891003439999928, -0.4257286625704000405 ) ) ;
#64440 = CARTESIAN_POINT ( 'NONE',  ( 11.44452754078377588, -3.491551460122512385, 8.211034235888378774 ) ) ;
#64441 = CARTESIAN_POINT ( 'NONE',  ( 11.50029455687000102, 11.65000000000000036, 0.000000000000000000 ) ) ;
#64442 = EDGE_LOOP ( 'NONE', ( #45804, #38162, #37846 ) ) ;
#64443 = CARTESIAN_POINT ( 'NONE',  ( 12.22352039041727245, 0.2292434675627110230, -12.69722039463305840 ) ) ;
#64444 = CARTESIAN_POINT ( 'NONE',  ( 11.44133594839949986, 4.569506585117100173, -6.847343244997600387 ) ) ;
#64445 = LINE ( 'NONE', #15880, #65534 ) ;
#64446 = CYLINDRICAL_SURFACE ( 'NONE', #29006, 0.5000000000000002220 ) ;
#64447 = CARTESIAN_POINT ( 'NONE',  ( 7.000000000000000000, 6.255435840762999966, -3.000000000000000000 ) ) ;
#64448 = ORIENTED_EDGE ( 'NONE', *, *, #30159, .T. ) ;
#64449 = CARTESIAN_POINT ( 'NONE',  ( 10.90000000000000036, 2.899999999999999911, 6.414037451299000381 ) ) ;
#64450 = B_SPLINE_CURVE_WITH_KNOTS ( 'NONE', 3,
 ( #2847, #11008, #24175, #53659, #6789, #61241, #66823, #59932, #32682, #40260 ),
 .UNSPECIFIED., .F., .F.,
 ( 4, 2, 2, 2, 4 ),
 ( 0.1844766778621776404, 0.3883575083966332442, 0.5922383389310887924, 0.7961191694655445072, 1.000000000000000000 ),
 .UNSPECIFIED. ) ;
#64451 = ADVANCED_FACE ( 'NONE', ( #51952 ), #15250, .T. ) ;
#64452 = CONTEXT_DEPENDENT_SHAPE_REPRESENTATION ( #7452, #41272 ) ;
#64453 = ADVANCED_FACE ( 'NONE', ( #9995 ), #43300, .T. ) ;
#64454 = CARTESIAN_POINT ( 'NONE',  ( 11.06967835872019812, -4.754733798270200928, -7.024326263066900111 ) ) ;
#64455 = CARTESIAN_POINT ( 'NONE',  ( 18.15698397290777777, 0.1703900906530151915, 12.69849596186095297 ) ) ;
#64456 = FACE_OUTER_BOUND ( 'NONE', #44701, .T. ) ;
#64457 = CARTESIAN_POINT ( 'NONE',  ( 10.89393020684959978, 2.750000000000000000, -7.500000000000000000 ) ) ;
#64458 = CARTESIAN_POINT ( 'NONE',  ( 10.98656920625009903, 4.032067152264009913, -6.608450613814399688 ) ) ;
#64459 = EDGE_LOOP ( 'NONE', ( #58149, #45682, #30408, #27346 ) ) ;
#64460 = CIRCLE ( 'NONE', #52203, 1.300164684427999706 ) ;
#64461 = CARTESIAN_POINT ( 'NONE',  ( 10.80169466977000070, -3.998196228428999355, 9.431543037543999475 ) ) ;
#64462 = CARTESIAN_POINT ( 'NONE',  ( 18.15894044208799230, 2.662322226546016246, -13.63771003692132311 ) ) ;
#64463 = ORIENTED_EDGE ( 'NONE', *, *, #22070, .T. ) ;
#64464 = CARTESIAN_POINT ( 'NONE',  ( 10.98768538770000092, -2.700669876604000041, 4.945210823433001224 ) ) ;
#64465 = CARTESIAN_POINT ( 'NONE',  ( 24.57714555854880345, 8.720582753219940031, -8.720580432860286280 ) ) ;
#64466 = CARTESIAN_POINT ( 'NONE',  ( 15.39229341877100232, 8.812225371893999792, 7.562487140343000291 ) ) ;
#64467 = ORIENTED_EDGE ( 'NONE', *, *, #61926, .F. ) ;
#64468 = DIRECTION ( 'NONE',  ( 1.000000000000000000, 0.000000000000000000, 0.000000000000000000 ) ) ;
#64469 = CARTESIAN_POINT ( 'NONE',  ( 18.17614054500835508, 0.08113966114449443212, -12.69973816841072178 ) ) ;
#64470 = CARTESIAN_POINT ( 'NONE',  ( 10.32309687351566652, -5.217465845835395299, -7.172815144550894750 ) ) ;
#64471 = CARTESIAN_POINT ( 'NONE',  ( 9.441296348250521220, 5.329048545047487373, 7.778931234571383690 ) ) ;
#64472 = ORIENTED_EDGE ( 'NONE', *, *, #63603, .F. ) ;
#64473 = CARTESIAN_POINT ( 'NONE',  ( 10.34521071928999980, -2.724119865955000108, 6.497322598008000050 ) ) ;
#64474 = CARTESIAN_POINT ( 'NONE',  ( 24.59232787866800152, 12.25045818421999932, -3.053350602882999976 ) ) ;
#64475 = CARTESIAN_POINT ( 'NONE',  ( 7.100000000000000533, 11.06886219213000011, -1.536526853569999851 ) ) ;
#64476 = EDGE_LOOP ( 'NONE', ( #4811, #3674, #13310, #16681, #21153 ) ) ;
#64477 = ADVANCED_FACE ( 'NONE', ( #14820 ), #20065, .F. ) ;
#64478 = CARTESIAN_POINT ( 'NONE',  ( 16.03350391962103316, 3.653603504000401792, 11.13263026093595975 ) ) ;
#64479 = CARTESIAN_POINT ( 'NONE',  ( 11.06877944038000017, -5.318813217120000658, -7.168443364726000411 ) ) ;
#64480 = ORIENTED_EDGE ( 'NONE', *, *, #61179, .T. ) ;
#64481 = CARTESIAN_POINT ( 'NONE',  ( 9.761304848515999666, 4.913464051101100516, 7.082356937474298952 ) ) ;
#64482 = CARTESIAN_POINT ( 'NONE',  ( 5.000000000000000000, 0.000000000000000000, 0.000000000000000000 ) ) ;
#64483 = EDGE_CURVE ( 'NONE', #25042, #19870, #18884, .T. ) ;
#64484 = CARTESIAN_POINT ( 'NONE',  ( 5.400636683305999775, -0.7159326393614999784, 1.172178427657000199 ) ) ;
#64485 = CARTESIAN_POINT ( 'NONE',  ( 11.59999999999999964, 5.179498027601999510, -7.174999999999999822 ) ) ;
#64486 = CARTESIAN_POINT ( 'NONE',  ( 16.43986884071599874, 3.414349888938000177, 11.89720686373000191 ) ) ;
#64487 = CARTESIAN_POINT ( 'NONE',  ( 5.600000001140999828, 0.000000000000000000, 0.000000000000000000 ) ) ;
#64488 = CARTESIAN_POINT ( 'NONE',  ( 24.08707324615214418, 12.57025408754081752, 3.402056317565807397 ) ) ;
#64489 = VECTOR ( 'NONE', #56904, 999.9999999999998863 ) ;
#64490 = B_SPLINE_SURFACE_WITH_KNOTS ( 'NONE', 3, 3, ( 
 ( #61252, #34349, #49723, #55668, #2517, #45179, #7413, #66484, #13370, #49033, #33998, #2181, #7070, #1141, #23496, #33305, #65092, #1832, #17569, #17215, #38896, #33653, #54970, #28762, #23150, #44499, #65792, #24877, #40609, #45524, #61937, #56352, #61592, #24187, #45861, #19284, #3540, #56699, #62279, #8799, #14397, #14050, #30139, #19635, #51444, #67170, #8458, #40956, #66833, #18946, #50765, #35378, #46207, #51106, #24534, #29457, #2859, #40275, #13709, #35038, #67514, #29802, #3208, #21025, #55162, #55512, #42359 ),
 ( #7612, #48276, #22995, #17413, #382, #60751, #64338, #60411, #18112, #32215, #26962, #44345, #21361, #10870, #63660, #65985, #58420, #44691, #65642, #60067, #38737, #12865, #17769, #39087, #12517, #54817, #33848, #21698, #7267, #28606, #31865, #49918, #43034, #26622, #2030, #23347, #42691, #28960, #33502, #53182, #6917, #12172, #39430, #28249, #5280, #49569, #53529, #63999, #10525, #1679, #34194, #50263, #15776, #37106, #47941, #41, #16117, #37443, #58764, #5621, #61778, #13561, #62462, #61099, #29299, #45026, #40453 ),
 ( #23691, #35899, #25063, #51632, #35568, #13219, #40129, #24036, #13899, #67020, #39778, #46052, #45370, #57215, #46395, #9317, #29651, #3389, #19129, #50952, #41154, #45712, #40799, #67698, #34879, #8305, #24725, #2712, #61442, #66331, #19825, #34545, #14582, #67356, #35227, #56539, #30659, #2368, #18455, #8643, #19476, #55857, #7960, #56197, #14241, #3050, #24381, #29993, #50610, #66678, #18801, #51293, #62122, #56884, #8982, #30322, #3728, #10359, #10013, #5112, #11052, #21534, #53016, #4418, #58255, #63141, #25756 ),
 ( #15948, #42189, #68386, #26799, #4069, #31693, #68048, #36243, #26448, #47085, #10699, #47780, #20506, #69088, #15266, #41832, #32044, #42868, #36590, #21194, #52323, #41489, #64177, #37277, #52664, #42523, #63834, #53360, #58597, #5462, #48113, #214, #15609, #16291, #31351, #37614, #58946, #62799, #51968, #4760, #57562, #25408, #46742, #57914, #20162, #63490, #14920, #36940, #26101, #9663, #31011, #47427, #68736, #20853, #54037, #567, #49142, #65213, #12436, #49487, #18035, #1597, #39351, #38657, #44267, #1949, #22914 ) ),
 .UNSPECIFIED., .F., .F., .F.,
 ( 4, 4 ),
 ( 4, 1, 1, 1, 1, 1, 1, 1, 1, 1, 1, 1, 1, 1, 1, 1, 1, 1, 1, 1, 1, 1, 1, 1, 1, 1, 1, 1, 1, 1, 1, 1, 1, 1, 1, 1, 1, 1, 1, 1, 1, 1, 1, 1, 1, 1, 1, 1, 1, 1, 1, 1, 1, 1, 1, 1, 1, 1, 1, 1, 1, 1, 1, 1, 4 ),
 ( -0.02000000000000000042, 1.020000000000000018 ),
 ( -0.02000000000000000042, -0.003749999999999999861, 0.01250000000000000069, 0.02875000000000000125, 0.04499999999999999833, 0.06124999999999999889, 0.07749999999999999944, 0.09375000000000000000, 0.1100000000000000006, 0.1262500000000000011, 0.1424999999999999878, 0.1587500000000000022, 0.1749999999999999889, 0.1912500000000000033, 0.2074999999999999900, 0.2237500000000000044, 0.2399999999999999911, 0.2562499999999999778, 0.2725000000000000200, 0.2887500000000000067, 0.3049999999999999933, 0.3212499999999999800, 0.3375000000000000222, 0.3537500000000000089, 0.3699999999999999956, 0.3862499999999999822, 0.4025000000000000244, 0.4187500000000000111, 0.4349999999999999978, 0.4512499999999999845, 0.4675000000000000266, 0.4837500000000000133, 0.5000000000000000000, 0.5162499999999999867, 0.5324999999999999734, 0.5487499999999999600, 0.5649999999999999467, 0.5812500000000000444, 0.5975000000000000311, 0.6137500000000000178, 0.6300000000000000044, 0.6462499999999999911, 0.6624999999999999778, 0.6787499999999999645, 0.6949999999999999512, 0.7112500000000000488, 0.7275000000000000355, 0.7437500000000000222, 0.7600000000000000089, 0.7762499999999999956, 0.7924999999999999822, 0.8087499999999999689, 0.8249999999999999556, 0.8412500000000000533, 0.8575000000000000400, 0.8737500000000000266, 0.8900000000000000133, 0.9062500000000000000, 0.9224999999999999867, 0.9387499999999999734, 0.9549999999999999600, 0.9712499999999999467, 0.9875000000000000444, 1.003749999999999920, 1.020000000000000018 ),
 .UNSPECIFIED. ) ;
#64491 = ORIENTED_EDGE ( 'NONE', *, *, #56184, .T. ) ;
#64492 = CARTESIAN_POINT ( 'NONE',  ( 9.323387100380815085, -4.033245596547300416, 9.239790378170226859 ) ) ;
#64493 = EDGE_LOOP ( 'NONE', ( #17799, #4663, #26015, #13566 ) ) ;
#64494 = CARTESIAN_POINT ( 'NONE',  ( 9.834151567923001380, 5.173929249342999803, 8.813048229486998508 ) ) ;
#64495 = CARTESIAN_POINT ( 'NONE',  ( 10.60770165877000082, 2.392327800351000011, -6.587345916039000215 ) ) ;
#64496 = LINE ( 'NONE', #48095, #49715 ) ;
#64497 = CARTESIAN_POINT ( 'NONE',  ( 12.64218892536043093, 3.103760129324341310, -13.52669845179790364 ) ) ;
#64498 = CARTESIAN_POINT ( 'NONE',  ( 3.732263932199000322, -3.201230512442000187, 1.871170248239000022 ) ) ;
#64499 = CARTESIAN_POINT ( 'NONE',  ( 11.09999999999999964, 4.000000000000000000, 7.500000000000000000 ) ) ;
#64500 = CARTESIAN_POINT ( 'NONE',  ( 18.17808105194527002, -0.05063168410658782509, 13.89988098555966012 ) ) ;
#64501 = CARTESIAN_POINT ( 'NONE',  ( 17.86525158951534209, 0.5426919696039526064, 13.88574006265539396 ) ) ;
#64502 = ORIENTED_EDGE ( 'NONE', *, *, #34469, .T. ) ;
#64503 = EDGE_CURVE ( 'NONE', #2358, #58209, #4317, .T. ) ;
#64504 = CARTESIAN_POINT ( 'NONE',  ( 12.27274360194281755, 0.3282986408611026641, 13.89479914613944267 ) ) ;
#64505 = CARTESIAN_POINT ( 'NONE',  ( 12.58523710839113008, -0.5851630251701737118, -13.88341719038490929 ) ) ;
#64506 = CARTESIAN_POINT ( 'NONE',  ( 9.696086916451999826, -2.554404004330999900, 7.600685922079000179 ) ) ;
#64507 = CARTESIAN_POINT ( 'NONE',  ( 17.89454199023491299, -0.5248377731598605767, -13.88666204733997134 ) ) ;
#64508 = B_SPLINE_CURVE_WITH_KNOTS ( 'NONE', 3,
 ( #24170, #2500, #19265, #23482, #50746, #55301, #39565, #8096, #66819, #29786 ),
 .UNSPECIFIED., .F., .F.,
 ( 4, 2, 2, 2, 4 ),
 ( 0.4999999999999994449, 0.6249999999999996669, 0.7499999999999997780, 0.8750000000000000000, 1.000000000000000000 ),
 .UNSPECIFIED. ) ;
#64509 = CARTESIAN_POINT ( 'NONE',  ( 8.245293146793999384, -4.282999948634999221, 9.286791354293999490 ) ) ;
#64511 = CARTESIAN_POINT ( 'NONE',  ( 12.79999999202000005, -11.41069016990000051, 4.623987642516999230 ) ) ;
#64510 = CARTESIAN_POINT ( 'NONE',  ( 10.10838019923399855, -2.730774061183999901, 7.659530259549099718 ) ) ;
#64512 = CARTESIAN_POINT ( 'NONE',  ( 10.76841504065829902, 4.914510326623699576, -6.818119527508899935 ) ) ;
#64513 = DIRECTION ( 'NONE',  ( 0.000000000000000000, -1.000000000000000000, 0.000000000000000000 ) ) ;
#64514 = AXIS2_PLACEMENT_3D ( 'NONE', #8754, #39889, #17873 ) ;
#64515 = B_SPLINE_CURVE_WITH_KNOTS ( 'NONE', 3,
 ( #39320, #12753, #31165, #37764, #32192, #63976, #42669, #10504, #4566, #16094, #37420, #20657, #4912, #48252, #30807, #25561, #36392, #52120, #43011, #41638, #15418 ),
 .UNSPECIFIED., .F., .F.,
 ( 4, 2, 2, 1, 1, 2, 2, 2, 1, 2, 2, 4 ),
 ( 0.000000000000000000, 0.1250000000000165978, 0.1875000000000261180, 0.2187500000000308920, 0.2343750000000332512, 0.2421875000000328071, 0.2500000000000323075, 0.3750000000000177081, 0.4375000000000116573, 0.4687500000000097700, 0.5000000000000078826, 1.000000000000000000 ),
 .UNSPECIFIED. ) ;
#64516 = CARTESIAN_POINT ( 'NONE',  ( 23.58838885791947249, 10.19767132316656522, -9.565245332708771642 ) ) ;
#64517 = CARTESIAN_POINT ( 'NONE',  ( 17.83159136582988680, -0.5605836838512557874, 12.68334204399184273 ) ) ;
#64518 = CARTESIAN_POINT ( 'NONE',  ( 8.348430368788083200, -2.904639935713019039, 6.526593578780762073 ) ) ;
#64519 = VECTOR ( 'NONE', #23695, 1000.000000000000114 ) ;
#64520 = DIRECTION ( 'NONE',  ( 0.000000000000000000, -0.9905022095861402143, -0.1374968101629056305 ) ) ;
#64521 = ORIENTED_EDGE ( 'NONE', *, *, #6692, .F. ) ;
#64522 = CARTESIAN_POINT ( 'NONE',  ( 9.497293146791999874, -3.734278838175999482, 8.942129638874000364 ) ) ;
#64523 = CARTESIAN_POINT ( 'NONE',  ( 8.672989158774999652, 4.728328492779000136, -8.692725459657999920 ) ) ;
#64524 = CARTESIAN_POINT ( 'NONE',  ( 9.266851002542999538, 2.832432432432000269, 6.822293592207000934 ) ) ;
#64525 = PLANE ( 'NONE',  #6590 ) ;
#64526 = VECTOR ( 'NONE', #35089, 1000.000000000000114 ) ;
#64527 = CARTESIAN_POINT ( 'NONE',  ( 0.7490331185628000821, -2.413104819777999843, -2.586865767356999690 ) ) ;
#64528 = CARTESIAN_POINT ( 'NONE',  ( 10.85679632507500081, 4.490665650747399873, 6.590394082213600235 ) ) ;
#64529 = CARTESIAN_POINT ( 'NONE',  ( 2.218610394918000051, -2.772870583375000031, 2.537629777733000136 ) ) ;
#64530 = ORIENTED_EDGE ( 'NONE', *, *, #23750, .T. ) ;
#64531 = B_SPLINE_CURVE_WITH_KNOTS ( 'NONE', 3,
 ( #34039, #32989, #54305, #6408 ),
 .UNSPECIFIED., .F., .F.,
 ( 4, 4 ),
 ( 0.000000000000000000, 1.000000000000000000 ),
 .UNSPECIFIED. ) ;
#64532 = CARTESIAN_POINT ( 'NONE',  ( 12.42221671361157043, -0.6112845611542921942, -12.58516990776527500 ) ) ;
#64533 = AXIS2_PLACEMENT_3D ( 'NONE', #12986, #2146, #23465 ) ;
#64534 = CARTESIAN_POINT ( 'NONE',  ( 10.93937577273821482, -4.461177266722074819, -8.699885912910445995 ) ) ;
#64535 = CARTESIAN_POINT ( 'NONE',  ( 10.17349413291699811, 5.162701151235999930, 8.030511425625498134 ) ) ;
#64536 = CARTESIAN_POINT ( 'NONE',  ( 5.630370665535105346, 12.10426712533993232, 3.742487578857858654 ) ) ;
#64537 = CARTESIAN_POINT ( 'NONE',  ( 9.208107780409999776, 5.057081813675999626, 8.967637988488998957 ) ) ;
#64538 = ORIENTED_EDGE ( 'NONE', *, *, #54147, .T. ) ;
#64539 = CARTESIAN_POINT ( 'NONE',  ( 5.528344406978000336, -1.481027812490000040, 0.6434334968688999457 ) ) ;
#64540 = EDGE_CURVE ( 'NONE', #34343, #46967, #33129, .T. ) ;
#64541 = EDGE_CURVE ( 'NONE', #866, #19742, #42423, .T. ) ;
#64542 = CARTESIAN_POINT ( 'NONE',  ( 8.245320280407000268, 2.435784185744999775, -7.548665584409000040 ) ) ;
#64543 = CARTESIAN_POINT ( 'NONE',  ( 8.499790797351490568, -2.599905373318510460, 6.452158339067893600 ) ) ;
#64544 = EDGE_CURVE ( 'NONE', #28653, #16735, #59559, .T. ) ;
#64545 = CARTESIAN_POINT ( 'NONE',  ( 9.168126402770999661, -2.803062940908000122, 7.951360234587600218 ) ) ;
#64547 = ORIENTED_EDGE ( 'NONE', *, *, #55055, .T. ) ;
#64546 = AXIS2_PLACEMENT_3D ( 'NONE', #20761, #42091, #5368 ) ;
#64548 = CARTESIAN_POINT ( 'NONE',  ( 2.948890132543457998, 2.798833948393634863, -2.150913519912196925 ) ) ;
#64549 = CARTESIAN_POINT ( 'NONE',  ( 11.35179910620000143, 11.71014626380999957, 1.422059914427000082 ) ) ;
#64550 = ORIENTED_EDGE ( 'NONE', *, *, #659, .T. ) ;
#64551 = CARTESIAN_POINT ( 'NONE',  ( 12.56879673640925077, 1.798456840536528434, -12.47100214317278954 ) ) ;
#64552 = DIRECTION ( 'NONE',  ( 0.000000000000000000, -0.9421243786071880066, 0.3352635608502960163 ) ) ;
#64553 = CARTESIAN_POINT ( 'NONE',  ( 18.17001922193490415, -0.1119984579798035534, -13.89939774083725688 ) ) ;
#64554 = VERTEX_POINT ( 'NONE', #52912 ) ;
#64555 = CARTESIAN_POINT ( 'NONE',  ( 13.50000000000303224, 9.278109357271722146, 7.623553959385361622 ) ) ;
#64556 = FILL_AREA_STYLE_COLOUR ( '', #15944 ) ;
#64557 = CARTESIAN_POINT ( 'NONE',  ( 24.53429010005800137, -12.47024913742999885, 3.026245653581999928 ) ) ;
#64558 = CARTESIAN_POINT ( 'NONE',  ( 8.902961428628096030, -2.546297866003439214, 8.472527682318533593 ) ) ;
#64559 = CARTESIAN_POINT ( 'NONE',  ( 11.16579975933730040, -2.791514215189000225, 7.915786590091300035 ) ) ;
#64560 = ORIENTED_EDGE ( 'NONE', *, *, #4774, .F. ) ;
#64561 = CARTESIAN_POINT ( 'NONE',  ( 8.668204719592999652, 3.979464555644999901, 9.134076336209998814 ) ) ;
#64562 = ORIENTED_EDGE ( 'NONE', *, *, #42947, .T. ) ;
#64563 = EDGE_CURVE ( 'NONE', #56639, #8998, #50586, .T. ) ;
#64564 = CARTESIAN_POINT ( 'NONE',  ( 9.279336721442293268, -4.163631234563185401, -6.250006800841094723 ) ) ;
#64565 = B_SPLINE_CURVE_WITH_KNOTS ( 'NONE', 3,
 ( #39631, #1189, #44549, #59910, #22498, #7120, #43842, #17263, #38586, #12018, #17966, #6766, #28105, #65842, #49418, #60264, #12369, #28458, #60606, #55364, #67557, #3252, #3925, #61985, #24581, #30182, #25263, #57077, #46939, #30861, #24921, #35085, #41349, #35761, #8158, #19681, #19327, #14441, #20363, #52175, #62326, #34736, #61297, #9519, #40652, #45904, #29504, #46601, #51489, #13417, #14096, #51155, #41002, #50810, #45571, #9177, #13751, #20023, #62660, #67216, #25611, #30517, #67906, #51830, #68242, #4276, #24232 ),
 .UNSPECIFIED., .F., .F.,
 ( 4, 2, 2, 2, 2, 2, 2, 2, 2, 2, 2, 2, 2, 2, 1, 1, 1, 2, 2, 2, 2, 2, 2, 2, 2, 2, 2, 2, 2, 2, 2, 2, 2, 2, 4 ),
 ( 0.000000000000000000, 0.1249999999998060995, 0.2499999999996121991, 0.3124999999995152766, 0.3437499999994663713, 0.3749999999994174660, 0.4062499999993685607, 0.4218749999993443023, 0.4374999999993200994, 0.4687499999992710831, 0.4843749999992468247, 0.4999999999992225108, 0.5156249999991983080, 0.5312499999991739941, 0.5468749999991497912, 0.5546874999991379118, 0.5585937499991319166, 0.5605468749991289190, 0.5624999999991259214, 0.5781249999991577848, 0.5859374999991732169, 0.5898437499991809885, 0.5937499999991886490, 0.6093749999992187361, 0.6171874999992340571, 0.6249999999992492672, 0.6406249999992801314, 0.6562499999993109956, 0.6718749999993418598, 0.6874999999993726130, 0.7187499999994347855, 0.7343749999994649835, 0.7499999999994952926, 0.8749999999997475353, 1.000000000000000000 ),
 .UNSPECIFIED. ) ;
#64566 = FACE_OUTER_BOUND ( 'NONE', #30041, .T. ) ;
#64567 = CARTESIAN_POINT ( 'NONE',  ( 9.112942518363999156, -5.100000000000000533, 6.192000867487999827 ) ) ;
#64568 = ORIENTED_EDGE ( 'NONE', *, *, #25570, .T. ) ;
#64569 = CARTESIAN_POINT ( 'NONE',  ( 12.32534826942435835, -2.099231811413891258, -12.53595023114330687 ) ) ;
#64570 = EDGE_CURVE ( 'NONE', #26914, #46748, #57454, .T. ) ;
#64571 = CIRCLE ( 'NONE', #38940, 2.524999655449999825 ) ;
#64572 = CARTESIAN_POINT ( 'NONE',  ( 10.61476354018239832, 5.217465845835394411, -7.172815144550904520 ) ) ;
#64573 = CYLINDRICAL_SURFACE ( 'NONE', #32671, 1.350000000000000089 ) ;
#64574 = CARTESIAN_POINT ( 'NONE',  ( 24.23080321643887558, -3.300949962372413005, -12.33052574769844156 ) ) ;
#64575 = CARTESIAN_POINT ( 'NONE',  ( 12.18713711904778130, -2.135907760014724488, -13.83611243771405874 ) ) ;
#64576 = VECTOR ( 'NONE', #52668, 1000.000000000000000 ) ;
#64577 = CARTESIAN_POINT ( 'NONE',  ( 10.89564560330029863, -3.692495237344800341, -6.544808043482999160 ) ) ;
#64578 = CARTESIAN_POINT ( 'NONE',  ( 12.43681290826173225, -1.853313662595208688, 12.46300903944178984 ) ) ;
#64579 = CARTESIAN_POINT ( 'NONE',  ( 18.01279894578404495, -3.038334268486861944, 12.22818629355008468 ) ) ;
#64580 = VERTEX_POINT ( 'NONE', #15842 ) ;
#64581 = CARTESIAN_POINT ( 'NONE',  ( 11.35034208742529849, -4.630634088820300143, -8.491292290686200062 ) ) ;
#64582 = VERTEX_POINT ( 'NONE', #5009 ) ;
#64583 = CONICAL_SURFACE ( 'NONE', #37797, 12.42515511468000078, 0.7854106315584118425 ) ;
#64584 = CARTESIAN_POINT ( 'NONE',  ( 17.10000442166958123, -12.52500000000000036, -4.938443340346877723E-11 ) ) ;
#64585 = CARTESIAN_POINT ( 'NONE',  ( 9.693589158772999426, 4.047146749018000200, -5.600703114891000034 ) ) ;
#64586 = CARTESIAN_POINT ( 'NONE',  ( 10.20918109782000016, 3.334760637131999772, -5.769467581755999497 ) ) ;
#64587 = CARTESIAN_POINT ( 'NONE',  ( 12.80505043854143388, 1.875000000000000000, -25.00000000000000000 ) ) ;
#64588 = DIRECTION ( 'NONE',  ( 0.000000000000000000, -0.1218274111675002463, -0.9925512993736016476 ) ) ;
#64589 = CARTESIAN_POINT ( 'NONE',  ( 23.74239655349000344, -13.04589975639999899, 3.828642821684999920 ) ) ;
#64590 = AXIS2_PLACEMENT_3D ( 'NONE', #24528, #35031, #14389 ) ;
#64591 = FACE_OUTER_BOUND ( 'NONE', #492, .T. ) ;
#64592 = ORIENTED_EDGE ( 'NONE', *, *, #68078, .F. ) ;
#64593 = CARTESIAN_POINT ( 'NONE',  ( 1.877754220768333537, -2.003492624900453212, -2.889646723249190696 ) ) ;
#64594 = CARTESIAN_POINT ( 'NONE',  ( 9.414312736919001168, 3.941041961981000430, 5.878350450964999752 ) ) ;
#64595 = CARTESIAN_POINT ( 'NONE',  ( 2.186390132542666898, -0.4581489286485234680, 3.499999999999998668 ) ) ;
#64596 = CARTESIAN_POINT ( 'NONE',  ( 11.56967835872019990, -4.754733798270200928, 7.975673736933100777 ) ) ;
#64598 = B_SPLINE_CURVE_WITH_KNOTS ( 'NONE', 3,
 ( #69182, #33170, #11148, #58696, #10801, #38057, #32482, #21294, #60083, #43314, #53796, #5893, #53460, #5554, #22320, #48558, #49238, #33517, #1347, #16727, #22665, #44008, #17429, #5214, #663, #59381, #38757, #32822, #54138, #26551, #63934, #7283, #13235, #55178, #40467 ),
 .UNSPECIFIED., .F., .F.,
 ( 4, 1, 1, 1, 1, 1, 1, 1, 1, 1, 1, 1, 1, 1, 1, 1, 1, 1, 1, 1, 1, 1, 1, 1, 1, 1, 1, 1, 1, 1, 1, 1, 4 ),
 ( 0.000000000000000000, 0.01250316081579585549, 0.04500295842620007786, 0.07750275603660429502, 0.1100025536470085330, 0.1425023512574696283, 0.1750021488678738524, 0.2075019464782780765, 0.2400017440886822728, 0.2725015416990865802, 0.3050013393094908043, 0.3375011369198949729, 0.3700009345302991970, 0.4025007321407034766, 0.4350005297511077007, 0.4675003273615118693, 0.5000001249719160379, 0.5324999225823202620, 0.5649997201927245971, 0.5974995178031287102, 0.6299993154135330453, 0.6624991130239372694, 0.6949989106343413825, 0.7274987082447457176, 0.7599985058551499417, 0.7924983034655541658, 0.8249981010759582789, 0.8574978986863625030, 0.8899976962967667271, 0.9224974939071709512, 0.9549972915175752863, 0.9874970891279795104, 1.000000000000000000 ),
 .UNSPECIFIED. ) ;
#64597 = CARTESIAN_POINT ( 'NONE',  ( 17.79514046837899954, 3.190852705101999920, -11.45040944101999969 ) ) ;
#64599 = AXIS2_PLACEMENT_3D ( 'NONE', #40780, #62103, #28942 ) ;
#64600 = CARTESIAN_POINT ( 'NONE',  ( 11.85159063708299954, 4.825025306051200502, -7.731961446576300467 ) ) ;
#64601 = CARTESIAN_POINT ( 'NONE',  ( 10.26001294666571795, 5.278409861158100291, 8.694118350725130284 ) ) ;
#64602 = ADVANCED_FACE ( 'NONE', ( #3968 ), #46643, .T. ) ;
#64603 = ADVANCED_FACE ( 'NONE', ( #9914 ), #52217, .F. ) ;
#64604 = CARTESIAN_POINT ( 'NONE',  ( 23.52037815668899867, -10.38720552913000006, -9.576763669727000661 ) ) ;
#64605 = CARTESIAN_POINT ( 'NONE',  ( 24.08682485015900099, -9.259169203442999319, 9.302355310768000152 ) ) ;
#64606 = B_SPLINE_CURVE_WITH_KNOTS ( 'NONE', 3,
 ( #15098, #42366, #63667, #21369, #15784, #37114, #48636, #26970, #32900, #22743 ),
 .UNSPECIFIED., .F., .F.,
 ( 4, 2, 2, 2, 4 ),
 ( 0.7044197654457721169, 0.7413672947650503664, 0.7783148240843286159, 0.8522098827228861140, 1.000000000000000000 ),
 .UNSPECIFIED. ) ;
#64607 = CARTESIAN_POINT ( 'NONE',  ( 2.250973465874000379, -3.500000000000000000, 0.000000000000000000 ) ) ;
#64608 = ORIENTED_EDGE ( 'NONE', *, *, #36667, .T. ) ;
#64609 = DIRECTION ( 'NONE',  ( 0.000000000000000000, 0.000000000000000000, -1.000000000000000000 ) ) ;
#64610 = CARTESIAN_POINT ( 'NONE',  ( 7.293868350350999563, -0.4381732831389000271, 1.171330428861999895 ) ) ;
#64611 = CARTESIAN_POINT ( 'NONE',  ( 18.17891560871126799, 2.542711950176887559, 13.66427582110434003 ) ) ;
#64612 = CARTESIAN_POINT ( 'NONE',  ( 10.76874784332534141, 4.963431926995326648, 4.838413582109893696 ) ) ;
#64613 = CARTESIAN_POINT ( 'NONE',  ( 11.28118179236249929, -4.267047616085000605, -6.250199235344999771 ) ) ;
#64614 = VERTEX_POINT ( 'NONE', #47328 ) ;
#64615 = CARTESIAN_POINT ( 'NONE',  ( 5.685751648550910531, -12.05129647863330966, 3.726325695169322660 ) ) ;
#64616 = CARTESIAN_POINT ( 'NONE',  ( 8.154704719592000828, 4.255646040929000229, 9.114085578076998928 ) ) ;
#64618 = DIRECTION ( 'NONE',  ( -1.000000000000000000, 0.000000000000000000, 0.000000000000000000 ) ) ;
#64617 = CARTESIAN_POINT ( 'NONE',  ( 9.798945280410000791, 5.639765292528999829, -8.059103558718000215 ) ) ;
#64619 = CARTESIAN_POINT ( 'NONE',  ( 10.83325145537689593, 2.985356913319267669, 4.869878758720406431 ) ) ;
#64620 = ORIENTED_EDGE ( 'NONE', *, *, #13195, .F. ) ;
#64621 = CARTESIAN_POINT ( 'NONE',  ( 9.778460659405999067, 5.743717947473999885, 7.748300625457000379 ) ) ;
#64623 = CARTESIAN_POINT ( 'NONE',  ( 17.79045811871164773, -1.826948899878886534, -13.88028486463507249 ) ) ;
#64622 = VECTOR ( 'NONE', #69175, 999.9999999999998863 ) ;
#64624 = CARTESIAN_POINT ( 'NONE',  ( 10.37872469555899890, 4.502158848185001006, 8.368784980615899372 ) ) ;
#64625 = CARTESIAN_POINT ( 'NONE',  ( 9.681180837610000367, -2.612237299844000216, 7.804680206899999639 ) ) ;
#64626 = CARTESIAN_POINT ( 'NONE',  ( 9.272293146792000229, -3.705847642455000202, 9.096432253453999195 ) ) ;
#64627 = VERTEX_POINT ( 'NONE', #6729 ) ;
#64628 = CARTESIAN_POINT ( 'NONE',  ( 24.53003472522700434, 12.09081557278000041, -3.147842171699999803 ) ) ;
#64629 = ADVANCED_FACE ( 'NONE', ( #43464 ), #32131, .F. ) ;
#64630 = ADVANCED_FACE ( 'NONE', ( #29470 ), #66845, .T. ) ;
#64632 = CARTESIAN_POINT ( 'NONE',  ( 10.35753185321000025, -5.367809014988999650, -6.514738374536999999 ) ) ;
#64631 = CARTESIAN_POINT ( 'NONE',  ( 12.83560584653800163, -12.04942283913000090, 3.198386977700000244 ) ) ;
#64633 = CARTESIAN_POINT ( 'NONE',  ( 7.769665546845473614, -5.098373949222779977, 8.848957063549683255 ) ) ;
#64634 = LINE ( 'NONE', #53808, #61605 ) ;
#64635 = DIRECTION ( 'NONE',  ( 0.000000000000000000, 1.000000000000000000, 0.000000000000000000 ) ) ;
#64636 = VERTEX_POINT ( 'NONE', #60571 ) ;
#64637 = CARTESIAN_POINT ( 'NONE',  ( 24.92845787801541491, -11.55909985197292222, -3.214028671284849370 ) ) ;
#64638 = EDGE_CURVE ( 'NONE', #57947, #45043, #24198, .T. ) ;
#64639 = CARTESIAN_POINT ( 'NONE',  ( 12.00687348028854906, -5.003459210197000573, 6.957450711802899868 ) ) ;
#64640 = CARTESIAN_POINT ( 'NONE',  ( 17.79074592073776628, 3.210128306652872521, 13.62701119232196234 ) ) ;
#64641 = CARTESIAN_POINT ( 'NONE',  ( 10.30072469555899950, 4.570852684939899824, 8.487632181750699445 ) ) ;
#64642 = ORIENTED_EDGE ( 'NONE', *, *, #48137, .F. ) ;
#64643 = B_SPLINE_SURFACE_WITH_KNOTS ( 'NONE', 1, 3, ( 
 ( #55998, #13358, #2507, #45169, #8102, #22788, #29446, #45514, #1819, #17197, #6708, #38528, #59850, #28048, #49357, #44136, #51434, #46194, #30800, #30461, #18938, #3871, #19969, #41631, #3531, #24525, #29793, #66825, #24866, #56688, #25205, #40262, #25554, #51773, #46540, #46880, #68187, #8787, #31159, #41292, #14040, #67505, #61582, #4557, #14723, #4216, #30131, #62266, #20305, #3198, #14386, #40600, #35706, #67846, #15061, #62599, #36384, #35367, #36038, #57023, #13698, #57354, #35027, #9458, #62937, #57700, #61925, #52113, #19623, #9810, #40944, #9123, #52461, #56342, #25897, #8446, #51095, #45850, #67159, #19271, #68879, #11185, #47226, #63634, #26933, #26246, #36738, #64310, #58058, #63282, #32865, #32520, #37079, #52812, #16428, #64662, #6276, #41977, #16766, #37757, #351, #38097, #15751, #26593, #54178, #702, #48247, #16085, #21333, #15412, #53499, #37415 ),
 ( #68529, #59083, #47914, #58392, #58736, #53837, #43004, #20651, #59423, #10842, #20996, #31837, #5934, #42662, #42332, #10497, #53153, #32184, #5255, #21668, #11, #63970, #5589, #11521, #27276, #48599, #22014, #43361, #10160, #31490, #47574, #4905, #28664, #44747, #22707, #33906, #45087, #23410, #66047, #18169, #60468, #13279, #2425, #60125, #1735, #23054, #17114, #39491, #44404, #60813, #55573, #49280, #61161, #43703, #28307, #12576, #64999, #49630, #12926, #34605, #38800, #1391, #7674, #17475, #55918, #38448, #12232, #44051, #34253, #29020, #27619, #55223, #50327, #33557, #65356, #48945, #23751, #17827, #66394, #49977, #18517, #65704, #2092, #6980, #39143, #39839, #1053, #59771, #11872, #22365, #33212, #54532, #6632, #27970, #54877, #7323, #18858, #36909, #26419, #47746, #4728, #24097, #20820, #40185, #56257, #52292, #19190, #69061, #62770, #57530, #31665, #45769 ) ),
 .UNSPECIFIED., .F., .F., .F.,
 ( 2, 2 ),
 ( 4, 2, 2, 2, 2, 2, 2, 2, 2, 2, 2, 2, 2, 2, 2, 2, 2, 2, 2, 2, 2, 2, 2, 2, 2, 2, 2, 2, 2, 2, 2, 2, 2, 2, 2, 2, 2, 2, 2, 2, 2, 2, 2, 2, 2, 2, 2, 2, 2, 2, 2, 2, 2, 2, 2, 4 ),
 ( 0.000000000000000000, 1.000000000000000000 ),
 ( 0.000000000000000000, 7.083325941644366664E-05, 0.0001416665188328873333, 0.0002124997782493309999, 0.0002479164079575528197, 0.0002833330376657746666, 0.0003187496673739965134, 0.0003541662970822183603, 0.0004249995564986619998, 0.0004604161862068838467, 0.0004781245010609947430, 0.0004958328159151056394, 0.0005312494456233274320, 0.0005666660753315493331, 0.0006374993347479930269, 0.0006729159644562148195, 0.0007083325941644367206, 0.0007437492238726585133, 0.0007791658535808803059, 0.0008145824832891022070, 0.0008499991129973239997, 0.0008854157427055457923, 0.0009208323724137676934, 0.0009562490021219894861, 0.0009916656318302112787, 0.001027082261538433180, 0.001062498891246654864, 0.001133332150663098666, 0.001168748780371320567, 0.001204165410079542468, 0.001239582039787764153, 0.001274998669495986054, 0.001345831928912429639, 0.001381248558620651540, 0.001416665188328873441, 0.001452081818037095125, 0.001469790132891206184, 0.001487498447745317027, 0.001558331707161760612, 0.001629164966578204414, 0.001664581596286426098, 0.001699998225994647999, 0.001735414855702869900, 0.001770831485411091585, 0.001841664744827535387, 0.001877081374535757071, 0.001912498004243978972, 0.001947914633952200873, 0.001983331263660422557, 0.002018747893368644242, 0.002054164523076866360, 0.002124997782493309728, 0.002160414412201531846, 0.002195831041909753530, 0.002231247671617975215, 0.002266664301326197332 ),
 .UNSPECIFIED. ) ;
#64644 = CARTESIAN_POINT ( 'NONE',  ( 9.310554719594000161, 3.934138271021000222, -9.063586117809000697 ) ) ;
#64645 = CARTESIAN_POINT ( 'NONE',  ( 12.09524978539961104, 2.332501710336875256, -12.38222815831571566 ) ) ;
#64646 = CARTESIAN_POINT ( 'NONE',  ( 12.09456039236534330, -2.685288321999000249, 7.436015812896529020 ) ) ;
#64647 = ORIENTED_EDGE ( 'NONE', *, *, #3689, .F. ) ;
#64648 = CARTESIAN_POINT ( 'NONE',  ( 7.949316606270907748, 4.924545613133609834, -6.408127913758977279 ) ) ;
#64649 = CARTESIAN_POINT ( 'NONE',  ( 10.39297979612879530, -2.713506317167766468, -7.026950959993343737 ) ) ;
#64650 = VERTEX_POINT ( 'NONE', #50086 ) ;
#64651 = CARTESIAN_POINT ( 'NONE',  ( 9.074379440379999551, -3.981661727120999750, 8.959239802162999311 ) ) ;
#64652 = CARTESIAN_POINT ( 'NONE',  ( 23.80820421035304335, 9.703756284516773079, 9.420712133314477654 ) ) ;
#64653 = ORIENTED_EDGE ( 'NONE', *, *, #9293, .T. ) ;
#64654 = CARTESIAN_POINT ( 'NONE',  ( 9.521013540183334456, 4.768183399968643599, 6.500416447002272946 ) ) ;
#64655 = EDGE_CURVE ( 'NONE', #52670, #15133, #50424, .T. ) ;
#64656 = CARTESIAN_POINT ( 'NONE',  ( 11.51102763632551884, 3.088851714329700293, 7.920427941950599404 ) ) ;
#64657 = CARTESIAN_POINT ( 'NONE',  ( 10.66052890781999984, -2.899999999999999911, -6.152188490330000370 ) ) ;
#64658 = CARTESIAN_POINT ( 'NONE',  ( 11.04798050650000008, 2.753316326401999969, -5.092742990910999801 ) ) ;
#64659 = CARTESIAN_POINT ( 'NONE',  ( 7.758693699415004197, 5.085317049932003286, 6.543835681441004581 ) ) ;
#64660 = CARTESIAN_POINT ( 'NONE',  ( 5.000000000000000000, -1.199999999999999956, -9.776630298829998011 ) ) ;
#64661 = CARTESIAN_POINT ( 'NONE',  ( 14.04809435262700035, 9.134678144910999720, 8.215103563399999587 ) ) ;
#64662 = CARTESIAN_POINT ( 'NONE',  ( 17.85474174040770023, -0.6550687562476319448, -12.58296113213902423 ) ) ;
#64663 = CARTESIAN_POINT ( 'NONE',  ( 12.19822292018694654, 2.649955819899461495, -12.41539170542472093 ) ) ;
#64664 = CARTESIAN_POINT ( 'NONE',  ( 10.89149144726329865, -4.659577337894599935, -6.569275630703699242 ) ) ;
#64665 = CARTESIAN_POINT ( 'NONE',  ( 8.277732780410000046, 4.874567052833000069, 6.119507471270999588 ) ) ;
#64666 = ORIENTED_EDGE ( 'NONE', *, *, #3165, .T. ) ;
#64667 = SHAPE_REPRESENTATION_RELATIONSHIP ( 'NONE' , 'NONE' ,  #19687, #24370 ) ;
#64668 = CARTESIAN_POINT ( 'NONE',  ( 11.60000000000000142, -4.745632530848085118, -8.163463725006291583 ) ) ;
#64669 = CARTESIAN_POINT ( 'NONE',  ( 11.57299956498156845, 5.207010770456999893, 7.174999999999999822 ) ) ;
#64670 = CARTESIAN_POINT ( 'NONE',  ( 7.921841810112000282, 2.875629839593000003, -6.725486766668000271 ) ) ;
#64671 = CARTESIAN_POINT ( 'NONE',  ( 18.24176189833872996, 2.711585165818143128, 12.30477270241628318 ) ) ;
#64672 = CARTESIAN_POINT ( 'NONE',  ( 12.50340631570014693, 1.853896141579338019, 13.87671057111554340 ) ) ;
#64674 = CARTESIAN_POINT ( 'NONE',  ( 10.97914836376999936, 9.415954400956000114, 6.236115164281000212 ) ) ;
#64673 = B_SPLINE_CURVE_WITH_KNOTS ( 'NONE', 3,
 ( #52412, #20600, #4504, #25845, #47173, #68476, #23964, #13488, #1955, #18723, #50535, #34121, #65913, #50196, #2637, #34473 ),
 .UNSPECIFIED., .F., .F.,
 ( 4, 2, 2, 2, 2, 2, 2, 4 ),
 ( 0.000000000000000000, 0.06249999999999995837, 0.1249999999999999167, 0.2499999999999998335, 0.5000000000000005551, 0.7500000000000012212, 0.8750000000000006661, 1.000000000000000000 ),
 .UNSPECIFIED. ) ;
#64675 = CARTESIAN_POINT ( 'NONE',  ( 10.58809113605762597, -4.810085401003767913, 7.830596297620237678 ) ) ;
#64676 = CARTESIAN_POINT ( 'NONE',  ( 10.96888392554999925, -5.599999999999999645, 6.571291218949999902 ) ) ;
#64677 = VERTEX_POINT ( 'NONE', #2870 ) ;
#64678 = CARTESIAN_POINT ( 'NONE',  ( 12.12616169587831294, -2.733465040722951933, 12.29993066094647958 ) ) ;
#64679 = CARTESIAN_POINT ( 'NONE',  ( 10.23758376188599861, -4.847012523549299345, -8.039825975318500184 ) ) ;
#64680 = CARTESIAN_POINT ( 'NONE',  ( 10.12671450658999994, 3.117528978489000124, 8.613535509676999880 ) ) ;
#64681 = CARTESIAN_POINT ( 'NONE',  ( 9.509907746701999898, -5.077451867123000007, 8.469011304701000498 ) ) ;
#64682 = CARTESIAN_POINT ( 'NONE',  ( 10.98995257254739855, 2.904643075091000171, -7.818564472783199548 ) ) ;
#64683 = CARTESIAN_POINT ( 'NONE',  ( 12.08006680260082888, 0.02395120399003008299, 12.59999907117300033 ) ) ;
#64684 = ADVANCED_FACE ( 'NONE', ( #13033 ), #17930, .T. ) ;
#64685 = ADVANCED_FACE ( 'NONE', ( #60915 ), #45872, .T. ) ;
#64686 = CARTESIAN_POINT ( 'NONE',  ( 9.176357780411999343, 2.935741164366000522, 6.259844213126999790 ) ) ;
#64687 = CARTESIAN_POINT ( 'NONE',  ( 5.227606837614000135, -0.3108367803229999948, 1.065889863396000115 ) ) ;
#64688 = CARTESIAN_POINT ( 'NONE',  ( 12.49051143973448497, 3.040180064579588670, 12.30914836342242680 ) ) ;
#64689 = CARTESIAN_POINT ( 'NONE',  ( 5.700000000000000178, 0.8000000000000000444, -3.149999999999999911 ) ) ;
#64690 = CARTESIAN_POINT ( 'NONE',  ( 10.49764694612699856, 2.940513484064000149, -7.922821994243300914 ) ) ;
#64691 = CARTESIAN_POINT ( 'NONE',  ( 11.71022026213526779, -2.954246606487285209, 7.175001674908393134 ) ) ;
#64692 = CARTESIAN_POINT ( 'NONE',  ( 10.72802334123000101, 3.751278653658999929, -8.836901076820000256 ) ) ;
#64693 = PLANE ( 'NONE',  #37192 ) ;
#64695 = CARTESIAN_POINT ( 'NONE',  ( 18.11245859366771072, -0.2828884610821091883, 12.69576253191529069 ) ) ;
#64694 = LINE ( 'NONE', #33247, #40846 ) ;
#64696 = DIRECTION ( 'NONE',  ( 1.000000000000000000, 0.000000000000000000, 0.000000000000000000 ) ) ;
#64697 = ORIENTED_EDGE ( 'NONE', *, *, #47274, .F. ) ;
#64698 = CARTESIAN_POINT ( 'NONE',  ( 12.53103060003192226, 0.5618114788522101666, 12.68327018738109402 ) ) ;
#64699 = CARTESIAN_POINT ( 'NONE',  ( 23.67741258883705768, -9.992411001872515186, -9.459257071873569345 ) ) ;
#64700 = CARTESIAN_POINT ( 'NONE',  ( 12.33432433144335505, -11.58110100107811746, 4.770114854519521330 ) ) ;
#64701 = DIRECTION ( 'NONE',  ( 0.000000000000000000, 0.9867381147929490393, 0.1623203401144079905 ) ) ;
#64702 = CARTESIAN_POINT ( 'NONE',  ( 12.80505043854146940, -3.125000000000000444, 13.52084414783465860 ) ) ;
#64703 = PLANE ( 'NONE',  #9646 ) ;
#64704 = DIRECTION ( 'NONE',  ( 0.7071067811865475727, 0.7071067811865475727, 0.000000000000000000 ) ) ;
#64705 = VERTEX_POINT ( 'NONE', #34360 ) ;
#64706 = DIRECTION ( 'NONE',  ( -0.000000000000000000, -0.000000000000000000, 1.000000000000000000 ) ) ;
#64707 = CARTESIAN_POINT ( 'NONE',  ( 11.09999999999999964, -2.700688486617000006, 5.124965750789000296 ) ) ;
#64708 = CARTESIAN_POINT ( 'NONE',  ( 0.000000000000000000, 0.000000000000000000, 0.000000000000000000 ) ) ;
#64709 = CARTESIAN_POINT ( 'NONE',  ( 18.30003129334700063, -2.732683817159999862, 11.53064095410000078 ) ) ;
#64710 = CARTESIAN_POINT ( 'NONE',  ( 10.90480513896000048, -3.220259576336399920, 7.933462475324499330 ) ) ;
#64711 = ADVANCED_FACE ( 'NONE', ( #2528 ), #66303, .T. ) ;
#64712 = PLANE ( 'NONE',  #29747 ) ;
#64713 = DIRECTION ( 'NONE',  ( 0.000000000000000000, -0.6664713972123997854, 0.7455306007789026523 ) ) ;
#64714 = CARTESIAN_POINT ( 'NONE',  ( 10.82595391537419971, 4.716560378569699452, 7.013338090450799811 ) ) ;
#64715 = CARTESIAN_POINT ( 'NONE',  ( 7.000000000000000000, -0.2897247358851999799, -3.000000000000000000 ) ) ;
#64716 = CARTESIAN_POINT ( 'NONE',  ( 10.28180685320999999, -3.991526694881000203, -5.814304247846999729 ) ) ;
#64717 = CARTESIAN_POINT ( 'NONE',  ( 3.500000000000000000, 3.499738125128000199, -0.04281419768536000314 ) ) ;
#64718 = DIRECTION ( 'NONE',  ( 0.000000000000000000, 0.000000000000000000, 1.000000000000000000 ) ) ;
#64719 = CARTESIAN_POINT ( 'NONE',  ( 23.80948321181408289, 9.702294094131053370, -9.418753252065425130 ) ) ;
#64720 = FACE_OUTER_BOUND ( 'NONE', #4487, .T. ) ;
#64721 = ORIENTED_EDGE ( 'NONE', *, *, #62693, .F. ) ;
#64722 = CARTESIAN_POINT ( 'NONE',  ( 7.412220152880141022, 2.451433362863415510, 8.294844223128800209 ) ) ;
#64723 = CARTESIAN_POINT ( 'NONE',  ( 11.71564426047340035, -3.460037133261700149, 6.654192128557399499 ) ) ;
#64724 = EDGE_LOOP ( 'NONE', ( #22239, #59356, #419, #51264, #32177, #27802, #35500, #25498 ) ) ;
#64725 = CARTESIAN_POINT ( 'NONE',  ( 18.01376003089018596, -2.074995895013258096, 13.75447352907418619 ) ) ;
#64726 = CARTESIAN_POINT ( 'NONE',  ( 10.64533863405319991, -3.296214805808900028, -8.397761948794601139 ) ) ;
#64727 = VERTEX_POINT ( 'NONE', #44848 ) ;
#64728 = CARTESIAN_POINT ( 'NONE',  ( 10.37199293566600034, 4.633387186021100668, 6.723009541442299231 ) ) ;
#64729 = CARTESIAN_POINT ( 'NONE',  ( 6.520102287872433067, 0.8301889199828892396, -0.7704547082435005967 ) ) ;
#64730 = EDGE_CURVE ( 'NONE', #523, #58875, #49711, .T. ) ;
#64731 = CARTESIAN_POINT ( 'NONE',  ( 24.30001120144517301, -3.256147830695084178, 12.15210914111320939 ) ) ;
#64732 = CARTESIAN_POINT ( 'NONE',  ( 8.642358819840239903, -3.294576102360963876, 8.704493534904289120 ) ) ;
#64733 = PLANE ( 'NONE',  #50012 ) ;
#64734 = CARTESIAN_POINT ( 'NONE',  ( 12.20062805326818278, -0.1603563348589100157, -13.89877286452650829 ) ) ;
#64735 = CARTESIAN_POINT ( 'NONE',  ( 11.59999999999999964, -4.149724965537171073, -6.485689145701417857 ) ) ;
#64736 = B_SPLINE_CURVE_WITH_KNOTS ( 'NONE', 3,
 ( #4404, #5100, #15597, #58586, #36576, #31338, #11038, #26089, #47415, #52308, #10346, #47765, #58934, #32034, #57549, #25743, #47073, #68374, #31682, #63820, #53347, #26786, #48101, #65546, #28865, #33752, #1934, #59619, #1239, #17669, #64501, #16621, #1581, #60655, #44251, #55068, #60313, #50172, #55417, #21863, #7170, #38993 ),
 .UNSPECIFIED., .F., .F.,
 ( 4, 2, 2, 2, 2, 2, 2, 2, 2, 2, 2, 2, 2, 1, 2, 2, 2, 2, 2, 1, 2, 4 ),
 ( 0.4997863768984585620, 0.5623130797861395358, 0.6248397826738204541, 0.6404714583957415996, 0.6561031341176628562, 0.6873664855615074787, 0.7029981612834298454, 0.7186298370053522122, 0.7264456748663133956, 0.7342615127272744679, 0.7498931884491969457, 0.7811565398930446769, 0.7889723777540051941, 0.7967882156149656003, 0.8124198913368909647, 0.8280515670588164401, 0.8436832427807419155, 0.8749465942245924222, 0.8905782699465176755, 0.9062099456684430399, 0.9374732971122935465, 1.000000000000000000 ),
 .UNSPECIFIED. ) ;
#64737 = CARTESIAN_POINT ( 'NONE',  ( 10.07930721860999945, -2.718124813223000036, -6.397797539448999871 ) ) ;
#64738 = CARTESIAN_POINT ( 'NONE',  ( 13.46001156276200028, 11.65487838447000080, 2.352687191044000148 ) ) ;
#64739 = ORIENTED_EDGE ( 'NONE', *, *, #51300, .T. ) ;
#64740 = CARTESIAN_POINT ( 'NONE',  ( 10.90000000000000036, -0.2500000000000000000, -9.776630298829998011 ) ) ;
#64741 = ORIENTED_EDGE ( 'NONE', *, *, #52495, .F. ) ;
#64742 = AXIS2_PLACEMENT_3D ( 'NONE', #52104, #20296, #63627 ) ;
#64743 = CARTESIAN_POINT ( 'NONE',  ( 10.81059687351629961, 3.370476274536378103, -6.407767014557176566 ) ) ;
#64744 = ORIENTED_EDGE ( 'NONE', *, *, #36134, .F. ) ;
#64745 = CARTESIAN_POINT ( 'NONE',  ( 17.60475804966761970, -1.787836225788245414, -13.88537509868912956 ) ) ;
#64746 = CARTESIAN_POINT ( 'NONE',  ( 18.15011669908946601, -2.691369836981456931, -12.40492163541245141 ) ) ;
#64747 = CARTESIAN_POINT ( 'NONE',  ( 10.78622389186427277, -2.904384452724245058, 5.097246023308017016 ) ) ;
#64748 = DIRECTION ( 'NONE',  ( -0.8231338744408063235, -0.5678473604306591982, 0.000000000000000000 ) ) ;
#64749 = CARTESIAN_POINT ( 'NONE',  ( 12.70159504149943430, 3.116720374454505116, 13.52307403002092379 ) ) ;
#64750 = CARTESIAN_POINT ( 'NONE',  ( 17.55505043854147118, -1.874999999999999556, 12.57545641911173107 ) ) ;
#64751 = CARTESIAN_POINT ( 'NONE',  ( 23.89320776801300283, -8.928716006283003992, -8.952507060077003587 ) ) ;
#64752 = CARTESIAN_POINT ( 'NONE',  ( 12.24428838907443229, 0.2761834754990887264, 13.89631168292872587 ) ) ;
#64753 = VERTEX_POINT ( 'NONE', #61265 ) ;
#64754 = CARTESIAN_POINT ( 'NONE',  ( 6.945228317543000074, 4.037115771921000018, -6.023232697733999608 ) ) ;
#64755 = CARTESIAN_POINT ( 'NONE',  ( 10.60454482602940018, -3.072763806055099245, 8.633921737781435013 ) ) ;
#64756 = DIRECTION ( 'NONE',  ( -1.000000000000000000, 0.000000000000000000, 0.000000000000000000 ) ) ;
#64757 = CARTESIAN_POINT ( 'NONE',  ( 5.092181265428000536, -0.6485384500295999777, 1.210768222740999933 ) ) ;
#64758 = CARTESIAN_POINT ( 'NONE',  ( 9.187479719595000205, 2.391443348526999912, -6.856688371964000162 ) ) ;
#64759 = CARTESIAN_POINT ( 'NONE',  ( 17.96055895400804303, 12.10036481531685837, -3.233715407583658052 ) ) ;
#64760 = CARTESIAN_POINT ( 'NONE',  ( 10.83767365324000131, -5.758089526411000136, -6.911472812823999945 ) ) ;
#64761 = EDGE_CURVE ( 'NONE', #18749, #42800, #30577, .T. ) ;
#64762 = ADVANCED_FACE ( 'NONE', ( #13719 ), #14062, .T. ) ;
#64763 = ORIENTED_EDGE ( 'NONE', *, *, #50188, .T. ) ;
#64764 = CARTESIAN_POINT ( 'NONE',  ( 8.210775250489261268, 3.646521065535271333, -8.815119237327296631 ) ) ;
#64765 = FACE_OUTER_BOUND ( 'NONE', #9376, .T. ) ;
#64766 = DIRECTION ( 'NONE',  ( 1.307574445097999928E-09, 5.454265898252000151E-12, -1.000000000000000000 ) ) ;
#64767 = CARTESIAN_POINT ( 'NONE',  ( 8.644633100483858357, -3.089364588649414767, -6.503246041658669263 ) ) ;
#64768 = ADVANCED_FACE ( 'NONE', ( #30481 ), #5314, .F. ) ;
#64769 = EDGE_CURVE ( 'NONE', #2919, #34701, #67282, .T. ) ;
#64770 = CARTESIAN_POINT ( 'NONE',  ( 11.85159063708299954, 4.825025306051200502, -7.731961446576300467 ) ) ;
#64771 = CARTESIAN_POINT ( 'NONE',  ( 5.938359839683334584, 0.7554284705563453217, 1.310679582531389276 ) ) ;
#64772 = CARTESIAN_POINT ( 'NONE',  ( 11.02301463001509774, 4.547357026650399980, -6.623338154204899908 ) ) ;
#64773 = CARTESIAN_POINT ( 'NONE',  ( 9.862621437244998290, 4.667147537636399335, -6.749162825004299648 ) ) ;
#64775 = CARTESIAN_POINT ( 'NONE',  ( 5.500000000000000000, 0.4800000000000000377, 1.889999999999999902 ) ) ;
#64774 = CARTESIAN_POINT ( 'NONE',  ( 9.975696787962998968, -3.851113559088000127, 8.354131589521699652 ) ) ;
#64776 = CARTESIAN_POINT ( 'NONE',  ( 11.15434687351636356, -2.749999999999998668, 7.663624617374463988 ) ) ;
#64777 = ORIENTED_EDGE ( 'NONE', *, *, #67215, .F. ) ;
#64778 = VECTOR ( 'NONE', #37166, 1000.000000000000114 ) ;
#64779 = CARTESIAN_POINT ( 'NONE',  ( 11.10612378248509913, 3.517039242046199998, 8.413720204863100349 ) ) ;
#64780 = CARTESIAN_POINT ( 'NONE',  ( 11.08492081570999943, -3.668392767032000013, 5.558160538745999801 ) ) ;
#64781 = CARTESIAN_POINT ( 'NONE',  ( 9.479721904869998994, 4.995641764568400589, 6.941043897400199114 ) ) ;
#64782 = CYLINDRICAL_SURFACE ( 'NONE', #63724, 1.250000000000000222 ) ;
#64783 = CARTESIAN_POINT ( 'NONE',  ( 9.571967469951999874, -4.084684048989999816, 8.946621592834999248 ) ) ;
#64784 = LINE ( 'NONE', #16897, #44211 ) ;
#64785 = CARTESIAN_POINT ( 'NONE',  ( 10.41476354018330852, 2.782534154164605589, 7.172815144550902744 ) ) ;
#64786 = EDGE_CURVE ( 'NONE', #17417, #54684, #47239, .T. ) ;
#64787 = AXIS2_PLACEMENT_3D ( 'NONE', #51053, #18901, #29057 ) ;
#64788 = CARTESIAN_POINT ( 'NONE',  ( 10.08857120343299840, -4.055348968344419269, -8.640469672413999547 ) ) ;
#64789 = CARTESIAN_POINT ( 'NONE',  ( 5.678117865652999363, -0.7240778834237999728, 1.106429931180000104 ) ) ;
#64790 = B_SPLINE_SURFACE_WITH_KNOTS ( 'NONE', 3, 3, ( 
 ( #21320, #31145, #20983, #53140 ),
 ( #68514, #63268, #37402, #52447 ),
 ( #20636, #41962, #36025, #47903 ),
 ( #32171, #37065, #15399, #42320 ),
 ( #36725, #10146, #15737, #9443 ),
 ( #62586, #42648, #63959, #58377 ),
 ( #30787, #16069, #58723, #10827 ),
 ( #3854, #46524, #19952, #14708 ) ),
 .UNSPECIFIED., .F., .F., .F.,
 ( 4, 1, 1, 1, 1, 4 ),
 ( 4, 4 ),
 ( 0.7453059214372000918, 0.7647058823529000460, 0.8235294117646999590, 0.8823529411764999830, 0.9411764705882000870, 0.9905827220917999831 ),
 ( -0.1830915291640000109, 1.182948984815999971 ),
 .UNSPECIFIED. ) ;
#64791 = CARTESIAN_POINT ( 'NONE',  ( 6.999999999999999112, 8.351195738565051485, -4.351195741810073514 ) ) ;
#64792 = CARTESIAN_POINT ( 'NONE',  ( 24.26682857475500299, -3.229948578041999863, 12.20213974738999951 ) ) ;
#64793 = CARTESIAN_POINT ( 'NONE',  ( 13.50018479229300006, -11.60142623882999935, -2.415183939829000259 ) ) ;
#64794 = CARTESIAN_POINT ( 'NONE',  ( 11.36749010443639918, 4.863785690678500195, -7.564597762509089662 ) ) ;
#64795 = DIRECTION ( 'NONE',  ( 0.000000000000000000, 0.5000000000000168754, -0.8660254037844288266 ) ) ;
#64796 = CARTESIAN_POINT ( 'NONE',  ( 25.29574836898500223, -8.389549047707998142, 8.302753013563000550 ) ) ;
#64797 = CARTESIAN_POINT ( 'NONE',  ( 12.35578833720754055, 1.907710147573941972, 12.45493153469542236 ) ) ;
#64798 = ORIENTED_EDGE ( 'NONE', *, *, #36615, .T. ) ;
#64799 = CARTESIAN_POINT ( 'NONE',  ( 11.09999999999999964, -5.299999999999999822, 5.160242713806000303 ) ) ;
#64800 = CONTEXT_DEPENDENT_SHAPE_REPRESENTATION ( #68595, #8152 ) ;
#64801 = CARTESIAN_POINT ( 'NONE',  ( 10.86190547754509872, -3.108323067758099967, -7.528299448264639260 ) ) ;
#64802 = CARTESIAN_POINT ( 'NONE',  ( 18.12548766255678601, 0.2560639957353438301, 12.69654133872496793 ) ) ;
#64803 = DIRECTION ( 'NONE',  ( 0.000000000000000000, 0.9999830366945593463, 0.005824630728861762523 ) ) ;
#64804 = DIRECTION ( 'NONE',  ( 0.000000000000000000, 1.000000000000000000, 0.000000000000000000 ) ) ;
#64805 = CARTESIAN_POINT ( 'NONE',  ( 13.32310803393400178, 12.20807901729000022, 2.049767542799999731 ) ) ;
#64806 = ORIENTED_EDGE ( 'NONE', *, *, #11821, .T. ) ;
#64807 = CARTESIAN_POINT ( 'NONE',  ( 11.09999999999999964, -6.593648102827000201, 5.598803487171999826 ) ) ;
#64808 = CARTESIAN_POINT ( 'NONE',  ( 17.96105691736157084, 2.975276276409919873, -13.56109295189183328 ) ) ;
#64809 = ORIENTED_EDGE ( 'NONE', *, *, #37952, .T. ) ;
#64810 = CARTESIAN_POINT ( 'NONE',  ( 23.60000000000000142, 11.85420044612000012, -3.901016762742000488 ) ) ;
#64811 = CARTESIAN_POINT ( 'NONE',  ( 25.29995734509200034, 8.533537492639000632, -7.925519463018001254 ) ) ;
#64812 = EDGE_CURVE ( 'NONE', #50185, #4, #68484, .T. ) ;
#64813 = CARTESIAN_POINT ( 'NONE',  ( 8.672989158774999652, 4.728328492779000136, -8.692725459657999920 ) ) ;
#64814 = EDGE_LOOP ( 'NONE', ( #49408, #42813, #6811, #24872 ) ) ;
#64815 = CARTESIAN_POINT ( 'NONE',  ( 23.72390811943373023, -13.12880825172584309, 3.830220858725267519 ) ) ;
#64816 = CARTESIAN_POINT ( 'NONE',  ( 11.30367835872029936, -5.113555564477999305, -6.798177532456199934 ) ) ;
#64817 = CARTESIAN_POINT ( 'NONE',  ( 8.110910841226001367, 2.101036793381999779, -7.559080181511999896 ) ) ;
#64818 = EDGE_CURVE ( 'NONE', #40442, #47396, #56396, .T. ) ;
#64819 = CARTESIAN_POINT ( 'NONE',  ( 10.49646369190723405, -5.100000000000000533, -6.665341197409489382 ) ) ;
#64820 = CARTESIAN_POINT ( 'NONE',  ( 9.454578519446510398, 5.254263437105202605, 7.998700540161328476 ) ) ;
#64821 = EDGE_LOOP ( 'NONE', ( #21590, #3116, #22401 ) ) ;
#64822 = CARTESIAN_POINT ( 'NONE',  ( 0.000000000000000000, 0.000000000000000000, 0.000000000000000000 ) ) ;
#64823 = CARTESIAN_POINT ( 'NONE',  ( 24.98632903739299849, 11.60054622243000111, -3.134150054602000246 ) ) ;
#64824 = ORIENTED_EDGE ( 'NONE', *, *, #55842, .T. ) ;
#64825 = CARTESIAN_POINT ( 'NONE',  ( 6.200859839683334762, 0.3926218265389221362, -1.460959015002473160 ) ) ;
#64826 = PLANE ( 'NONE',  #44302 ) ;
#64827 = B_SPLINE_CURVE_WITH_KNOTS ( 'NONE', 3,
 ( #55094, #24572, #66868, #18981 ),
 .UNSPECIFIED., .F., .F.,
 ( 4, 4 ),
 ( 0.000000000000000000, 1.000000000000000000 ),
 .UNSPECIFIED. ) ;
#64828 = ORIENTED_EDGE ( 'NONE', *, *, #1974, .F. ) ;
#64829 = CARTESIAN_POINT ( 'NONE',  ( 10.01258376188599897, 3.037118682679400106, 6.886327436977599525 ) ) ;
#64830 = CARTESIAN_POINT ( 'NONE',  ( 18.08681467613411442, 0.3285836819253546426, -13.89477675118497935 ) ) ;
#64831 = CARTESIAN_POINT ( 'NONE',  ( 5.298007516638000070, 0.9565531964925000352, 1.044714011268000009 ) ) ;
#64832 = CIRCLE ( 'NONE', #58155, 1.800000000000000266 ) ;
#64833 = AXIS2_PLACEMENT_3D ( 'NONE', #60400, #12505, #43637 ) ;
#64834 = CARTESIAN_POINT ( 'NONE',  ( 11.60000000000000142, 4.420828903570660273, -6.483899970161564497 ) ) ;
#64835 = CARTESIAN_POINT ( 'NONE',  ( 24.71800983586086886, 11.77345325639867113, -3.190795111280438690 ) ) ;
#64836 = CARTESIAN_POINT ( 'NONE',  ( 25.29986734212600297, -2.596989636639000398, 11.35306351421000137 ) ) ;
#64837 = CARTESIAN_POINT ( 'NONE',  ( 9.327378398803991999, -3.946271215605382743, 9.238828740155991426 ) ) ;
#64838 = ORIENTED_EDGE ( 'NONE', *, *, #2664, .F. ) ;
#64839 = DIRECTION ( 'NONE',  ( 0.000000000000000000, 0.000000000000000000, 1.000000000000000000 ) ) ;
#64840 = CARTESIAN_POINT ( 'NONE',  ( 9.888314158772001150, 5.105193280231000053, -8.895607399415000671 ) ) ;
#64841 = CARTESIAN_POINT ( 'NONE',  ( 18.47744389612467941, -11.93152012402699391, 3.811457427748914384 ) ) ;
#64842 = CARTESIAN_POINT ( 'NONE',  ( 12.55463174185018715, 3.072731264995192113, -13.53516186994626658 ) ) ;
#64843 = FACE_OUTER_BOUND ( 'NONE', #18907, .T. ) ;
#64844 = CARTESIAN_POINT ( 'NONE',  ( 9.595487457706001422, -3.928425191288000384, 5.531324308465000783 ) ) ;
#64845 = CARTESIAN_POINT ( 'NONE',  ( 18.15913552218862037, -0.1616183441363965301, 13.89875400931294536 ) ) ;
#64846 = CARTESIAN_POINT ( 'NONE',  ( 24.78225916701600440, -3.612170063153999688, 12.07974787419999885 ) ) ;
#64847 = ORIENTED_EDGE ( 'NONE', *, *, #6880, .T. ) ;
#64848 = ORIENTED_EDGE ( 'NONE', *, *, #30926, .F. ) ;
#64849 = CARTESIAN_POINT ( 'NONE',  ( 9.854942824136999846, 2.800308224477999985, 9.013816726157999781 ) ) ;
#64850 = CARTESIAN_POINT ( 'NONE',  ( 12.20062805325453148, 0.1603563348074356076, 13.89877286452765404 ) ) ;
#64851 = EDGE_CURVE ( 'NONE', #68916, #5127, #13937, .T. ) ;
#64852 = CARTESIAN_POINT ( 'NONE',  ( 10.57503300763299947, -3.118110956362800223, 6.575021251017499679 ) ) ;
#64853 = ADVANCED_FACE ( 'NONE', ( #28395 ), #13010, .F. ) ;
#64854 = CARTESIAN_POINT ( 'NONE',  ( 9.944325809452999820, -5.443013936195000291, 7.367349259341000156 ) ) ;
#64855 = DIRECTION ( 'NONE',  ( 0.000000000000000000, 1.000000000000000000, 0.000000000000000000 ) ) ;
#64856 = CARTESIAN_POINT ( 'NONE',  ( 8.577620559625000141, -3.981661727120999750, 8.959239802162999311 ) ) ;
#64857 = CARTESIAN_POINT ( 'NONE',  ( 27.64127793187000037, 5.599999999999999645, -6.571291218949999902 ) ) ;
#64859 = CARTESIAN_POINT ( 'NONE',  ( 11.59999999999999964, -4.000000000000000000, -7.500000000000000000 ) ) ;
#64858 = CARTESIAN_POINT ( 'NONE',  ( 8.739649184022093564, 2.648220570447237243, 7.263719241076208810 ) ) ;
#64860 = CARTESIAN_POINT ( 'NONE',  ( 10.54272335273199879, 4.444874504667400750, -8.698083075453000745 ) ) ;
#64861 = CARTESIAN_POINT ( 'NONE',  ( 12.10000000000000142, -4.471166781226292741, 6.561154158729442187 ) ) ;
#64862 = CARTESIAN_POINT ( 'NONE',  ( 8.649445371194000032, 5.100000000000000533, -6.459601070175000181 ) ) ;
#64863 = CARTESIAN_POINT ( 'NONE',  ( 17.94350157889105901, -0.4896501542853345379, 12.68729270499356510 ) ) ;
#64864 = CARTESIAN_POINT ( 'NONE',  ( 9.099999999999999645, 0.000000000000000000, 0.000000000000000000 ) ) ;
#64865 = DIRECTION ( 'NONE',  ( 0.000000000000000000, -0.7071067811865474617, -0.7071067811865474617 ) ) ;
#64866 = ORIENTED_EDGE ( 'NONE', *, *, #38092, .T. ) ;
#64867 = FACE_OUTER_BOUND ( 'NONE', #43995, .T. ) ;
#64868 = CARTESIAN_POINT ( 'NONE',  ( 9.170239158775000732, 4.769103072373000352, -8.666849124598000387 ) ) ;
#64869 = VECTOR ( 'NONE', #57477, 1000.000000000000000 ) ;
#64870 = CARTESIAN_POINT ( 'NONE',  ( 10.81021345716900051, -3.363461959113699606, 6.921280946186199934 ) ) ;
#64871 = EDGE_CURVE ( 'NONE', #40612, #48587, #4748, .T. ) ;
#64872 = FACE_OUTER_BOUND ( 'NONE', #33447, .T. ) ;
#64873 = B_SPLINE_CURVE_WITH_KNOTS ( 'NONE', 3,
 ( #49355, #60547, #11953, #65433 ),
 .UNSPECIFIED., .F., .F.,
 ( 4, 4 ),
 ( 0.000000000000000000, 1.000000000000000000 ),
 .UNSPECIFIED. ) ;
#64874 = CARTESIAN_POINT ( 'NONE',  ( 0.4694343787449999916, 2.854424451075999958, -2.356853325602000115 ) ) ;
#64875 = CARTESIAN_POINT ( 'NONE',  ( 10.98146005378009882, 4.911671201000399556, 7.986817550794899745 ) ) ;
#64876 = CARTESIAN_POINT ( 'NONE',  ( 2.933839636531999862, 1.438508091966000046, -3.472617419920999815 ) ) ;
#64877 = ORIENTED_EDGE ( 'NONE', *, *, #67709, .F. ) ;
#64878 = CARTESIAN_POINT ( 'NONE',  ( 12.17126533935443611, -0.3494793053307434505, -12.59515668824706580 ) ) ;
#64880 = VECTOR ( 'NONE', #27022, 1000.000000000000000 ) ;
#64879 = DIRECTION ( 'NONE',  ( -1.000000000000000000, 0.000000000000000000, 0.000000000000000000 ) ) ;
#64881 = CARTESIAN_POINT ( 'NONE',  ( 17.99878237954352400, 3.049368882785695067, -12.22543920180491739 ) ) ;
#64882 = PLANE ( 'NONE',  #2014 ) ;
#64883 = CARTESIAN_POINT ( 'NONE',  ( 9.272295280408998863, 3.705846972803000128, 9.096435887808000942 ) ) ;
#64884 = ORIENTED_EDGE ( 'NONE', *, *, #13366, .T. ) ;
#64885 = CARTESIAN_POINT ( 'NONE',  ( 5.701460587185000151, 1.361663118425000096, -0.5499102030850999689 ) ) ;
#64886 = CARTESIAN_POINT ( 'NONE',  ( 7.607754719585000380, 2.591432452475999515, -8.508584064833998539 ) ) ;
#64888 = CARTESIAN_POINT ( 'NONE',  ( 8.807788144226000426, -3.909067355573210278, -8.453461841935100196 ) ) ;
#64887 = CARTESIAN_POINT ( 'NONE',  ( 8.381640933329739696, -2.862614012586783385, 8.816379852580610077 ) ) ;
#64889 = CARTESIAN_POINT ( 'NONE',  ( 9.396088727410999653, -5.274736981944999847, 7.393088754863899936 ) ) ;
#64890 = EDGE_LOOP ( 'NONE', ( #9498, #11621, #63365, #28036, #17899 ) ) ;
#64891 = CARTESIAN_POINT ( 'NONE',  ( 18.05677685611890126, -2.118334401119843946, -13.74715678131696883 ) ) ;
#64892 = CARTESIAN_POINT ( 'NONE',  ( 11.80890711774500090, 11.72268911462999874, 1.968096114907999628 ) ) ;
#64893 = VERTEX_POINT ( 'NONE', #45168 ) ;
#64894 = CARTESIAN_POINT ( 'NONE',  ( 11.10000000000000320, 2.288692731476340114, -7.672306050762143670 ) ) ;
#64895 = CARTESIAN_POINT ( 'NONE',  ( 16.34806348789000197, 3.378436248652000096, 11.11006988061000023 ) ) ;
#64896 = CONICAL_SURFACE ( 'NONE', #31433, 12.44999944941000081, 0.7853981146832407223 ) ;
#64897 = CARTESIAN_POINT ( 'NONE',  ( 18.16408159376649678, 0.1418539764880162590, -13.89904537328360945 ) ) ;
#64898 = ORIENTED_EDGE ( 'NONE', *, *, #44678, .T. ) ;
#64899 = CARTESIAN_POINT ( 'NONE',  ( 10.30195995176331714, -5.579776588524842929, -6.689560773767187385 ) ) ;
#64900 = CARTESIAN_POINT ( 'NONE',  ( 10.48280513895999988, 4.903310631086600146, -6.997844089834400094 ) ) ;
#64901 = EDGE_CURVE ( 'NONE', #41440, #28381, #9349, .T. ) ;
#64902 = DIRECTION ( 'NONE',  ( 0.000000000000000000, -0.1218274111675001353, -0.9925512993736016476 ) ) ;
#64903 = CARTESIAN_POINT ( 'NONE',  ( 11.53502897915239878, -3.672866099873000056, 6.264564938179000286 ) ) ;
#64904 = EDGE_LOOP ( 'NONE', ( #28352, #7665 ) ) ;
#64905 = PLANE ( 'NONE',  #57715 ) ;
#64906 = DIRECTION ( 'NONE',  ( 1.000000000000000000, 0.000000000000000000, 0.000000000000000000 ) ) ;
#64907 = ORIENTED_EDGE ( 'NONE', *, *, #8445, .F. ) ;
#64908 = CARTESIAN_POINT ( 'NONE',  ( 4.599999999999999645, 3.248147246781390329, 13.61798588129781251 ) ) ;
#64909 = CARTESIAN_POINT ( 'NONE',  ( 11.09999999999999964, -0.5000000000000000000, 9.662944685757000940 ) ) ;
#64910 = CARTESIAN_POINT ( 'NONE',  ( 11.12341687003999979, 6.064977932649999737, -5.276126571066000359 ) ) ;
#64911 = ORIENTED_EDGE ( 'NONE', *, *, #32770, .F. ) ;
#64912 = CARTESIAN_POINT ( 'NONE',  ( 12.33197597414245728, -2.091428098900829369, -12.53741636228080836 ) ) ;
#64913 = DIRECTION ( 'NONE',  ( 1.000000000000000000, 0.000000000000000000, 0.000000000000000000 ) ) ;
#64914 = CARTESIAN_POINT ( 'NONE',  ( 7.739722165042043578, 4.561671897555351407, -5.729814629414840432 ) ) ;
#64915 = CARTESIAN_POINT ( 'NONE',  ( 24.30000000000000071, 0.000000000000000000, 0.000000000000000000 ) ) ;
#64916 = CARTESIAN_POINT ( 'NONE',  ( 12.20666462242727590, -2.105579624229079183, -13.84076000201158152 ) ) ;
#64917 = CARTESIAN_POINT ( 'NONE',  ( 10.52641638348499953, -4.974961480482700260, -7.262511127784999410 ) ) ;
#64918 = CARTESIAN_POINT ( 'NONE',  ( 10.45551210286900279, 3.782771630962270759, 6.243812680477911492 ) ) ;
#64919 = CARTESIAN_POINT ( 'NONE',  ( 17.91108626730883202, -1.853415294216375298, 12.46294044425349767 ) ) ;
#64920 = ORIENTED_EDGE ( 'NONE', *, *, #20313, .F. ) ;
#64921 = CARTESIAN_POINT ( 'NONE',  ( 11.75203632436369894, -5.109717061557999429, -7.240848640331599917 ) ) ;
#64922 = ORIENTED_EDGE ( 'NONE', *, *, #20430, .F. ) ;
#64923 = CARTESIAN_POINT ( 'NONE',  ( 11.50000000000000000, -3.008232475376599879, 7.825000000000000178 ) ) ;
#64924 = CARTESIAN_POINT ( 'NONE',  ( 9.047164158776000775, 2.156584729807999867, -7.959751745006000689 ) ) ;
#64925 = CARTESIAN_POINT ( 'NONE',  ( 9.933148997456999751, 5.167567567567999731, 6.822293592207000934 ) ) ;
#64926 = CARTESIAN_POINT ( 'NONE',  ( 9.662447522843001124, -4.824180051339999942, -8.517611033492999084 ) ) ;
#64927 = DIRECTION ( 'NONE',  ( -0.7071067811865159314, -0.5062022020404108869, 0.4937198908789108831 ) ) ;
#64928 = CARTESIAN_POINT ( 'NONE',  ( 23.81896843540200237, 12.91808259626999877, 3.708628114615999838 ) ) ;
#64929 = CARTESIAN_POINT ( 'NONE',  ( 10.57435795695566583, 5.250000000000000000, -7.807440182398264206 ) ) ;
#64930 = VECTOR ( 'NONE', #31503, 1000.000000000000227 ) ;
#64931 = ORIENTED_EDGE ( 'NONE', *, *, #19735, .T. ) ;
#64932 = CARTESIAN_POINT ( 'NONE',  ( 1.969891126640333390, 1.842658540278710566, -2.994770506591986070 ) ) ;
#64933 = EDGE_CURVE ( 'NONE', #56058, #6251, #56234, .T. ) ;
#64934 = CARTESIAN_POINT ( 'NONE',  ( 9.256664404737000140, 4.025830366070999311, 9.295863330698999505 ) ) ;
#64935 = EDGE_CURVE ( 'NONE', #23807, #33299, #60721, .T. ) ;
#64936 = CARTESIAN_POINT ( 'NONE',  ( 2.196806799209333416, -0.9161175952574931447, 3.408904368339101598 ) ) ;
#64937 = CARTESIAN_POINT ( 'NONE',  ( 11.73078751119019891, -4.915752892793999962, 7.020904658857499925 ) ) ;
#64938 = CARTESIAN_POINT ( 'NONE',  ( 17.88015371777900242, 3.314513509857999640, -11.22393657228000130 ) ) ;
#64939 = CARTESIAN_POINT ( 'NONE',  ( 10.50595525820100029, 3.918212119278319694, -6.637672143048099827 ) ) ;
#64940 = CARTESIAN_POINT ( 'NONE',  ( 10.22737811154219223, 5.662262400723353295, 8.092495838525170626 ) ) ;
#64941 = AXIS2_PLACEMENT_3D ( 'NONE', #62695, #5004, #42071 ) ;
#64942 = CARTESIAN_POINT ( 'NONE',  ( 23.64839641905800249, -10.02576512143000009, -9.635306756802998862 ) ) ;
#64943 = CARTESIAN_POINT ( 'NONE',  ( 5.000000000000000000, -11.35000000000000142, 0.000000000000000000 ) ) ;
#64944 = CARTESIAN_POINT ( 'NONE',  ( 11.71289336965100070, -3.191014699919000108, 11.45041132747999946 ) ) ;
#64945 = ORIENTED_EDGE ( 'NONE', *, *, #54441, .F. ) ;
#64946 = CARTESIAN_POINT ( 'NONE',  ( 9.769471092180999960, 5.100000000000000533, -6.152188490330000370 ) ) ;
#64947 = CARTESIAN_POINT ( 'NONE',  ( 6.994995159244999705, -0.3168999327563999935, -1.209784435933999980 ) ) ;
#64948 = CARTESIAN_POINT ( 'NONE',  ( 17.96899650538950155, 2.968713945236787222, 13.56275387600714311 ) ) ;
#64949 = EDGE_CURVE ( 'NONE', #7451, #2756, #37264, .T. ) ;
#64950 = CARTESIAN_POINT ( 'NONE',  ( 10.73994861681368285, 4.937004252026683915, 4.824365178933474496 ) ) ;
#64951 = CARTESIAN_POINT ( 'NONE',  ( 11.05964426047339799, -3.312306505177499805, -8.577215873335999774 ) ) ;
#64952 = VERTEX_POINT ( 'NONE', #11954 ) ;
#64953 = B_SPLINE_CURVE_WITH_KNOTS ( 'NONE', 3,
 ( #40062, #13148, #19060, #23284 ),
 .UNSPECIFIED., .F., .F.,
 ( 4, 4 ),
 ( 0.000000000000000000, 1.000000000000000000 ),
 .UNSPECIFIED. ) ;
#64954 = CARTESIAN_POINT ( 'NONE',  ( 11.02038275177999971, -5.599999999999999645, -6.571291218949999902 ) ) ;
#64955 = EDGE_CURVE ( 'NONE', #21511, #17545, #33293, .T. ) ;
#64956 = CARTESIAN_POINT ( 'NONE',  ( 8.977760841230999489, 2.019067547072999957, 7.390982789861999969 ) ) ;
#64958 = CARTESIAN_POINT ( 'NONE',  ( 11.12299956498149811, -2.792989229543000107, -7.825000000000000178 ) ) ;
#64957 = CARTESIAN_POINT ( 'NONE',  ( 8.514954719592999766, 3.207599814920999659, -6.150466394809999571 ) ) ;
#64959 = CARTESIAN_POINT ( 'NONE',  ( 24.63332956304826737, -10.83443035036254365, 3.855530959951017689 ) ) ;
#64960 = ORIENTED_EDGE ( 'NONE', *, *, #33142, .F. ) ;
#64961 = CARTESIAN_POINT ( 'NONE',  ( 9.260906466624998501, 4.901388651757999426, 9.090324495507999814 ) ) ;
#64962 = CARTESIAN_POINT ( 'NONE',  ( 18.25201697487001340, -2.719281809836145314, -13.73337690942506129 ) ) ;
#64963 = CARTESIAN_POINT ( 'NONE',  ( 11.31410538575739899, 4.975963290822400076, 7.733337754805098996 ) ) ;
#64964 = CARTESIAN_POINT ( 'NONE',  ( 10.23808992278000041, -2.752437370156000540, 6.820045513931999537 ) ) ;
#64965 = CARTESIAN_POINT ( 'NONE',  ( 7.761763193589995780, 2.840593260277998411, 6.815714094171000603 ) ) ;
#64966 = VERTEX_POINT ( 'NONE', #41808 ) ;
#64967 = CARTESIAN_POINT ( 'NONE',  ( 24.54687940532799928, 12.52318695592999909, -3.000795290450999797 ) ) ;
#64969 = CARTESIAN_POINT ( 'NONE',  ( 10.82674314678999927, -3.167157901876000103, -6.225148200207000215 ) ) ;
#64968 = CARTESIAN_POINT ( 'NONE',  ( 12.11132301796900101, -11.62873132690000055, 4.501748577889000735 ) ) ;
#64970 = CARTESIAN_POINT ( 'NONE',  ( 7.662320246279550773, -5.560547198184215389, 6.711813256769637803 ) ) ;
#64971 = CARTESIAN_POINT ( 'NONE',  ( 9.566960887370999700, -5.215923019114000247, 6.177729435798999802 ) ) ;
#64972 = CARTESIAN_POINT ( 'NONE',  ( 9.991937366751301397, -4.976291841660785309, 8.591989380854540670 ) ) ;
#64973 = ORIENTED_EDGE ( 'NONE', *, *, #48179, .T. ) ;
#64975 = DIRECTION ( 'NONE',  ( 0.000000000000000000, 0.000000000000000000, -1.000000000000000000 ) ) ;
#64974 = AXIS2_PLACEMENT_3D ( 'NONE', #61659, #7141, #51508 ) ;
#64976 = CARTESIAN_POINT ( 'NONE',  ( 11.39564560330030041, -3.692495237344800341, 8.455191956516999952 ) ) ;
#64977 = CARTESIAN_POINT ( 'NONE',  ( 8.332048273611004419, 2.867478057767001154, 6.314276212112998721 ) ) ;
#64978 = CARTESIAN_POINT ( 'NONE',  ( 10.83810672858429847, 2.978701842912999886, 8.268288002587098617 ) ) ;
#64979 = ORIENTED_EDGE ( 'NONE', *, *, #2457, .F. ) ;
#64980 = CARTESIAN_POINT ( 'NONE',  ( 8.971339158776000744, 4.082930418187999955, -6.104944817728999773 ) ) ;
#64981 = CYLINDRICAL_SURFACE ( 'NONE', #66085, 2.149999999999999911 ) ;
#64982 = CARTESIAN_POINT ( 'NONE',  ( 12.25024874575444933, 2.943737818075150336, -12.25130580795035407 ) ) ;
#64983 = CARTESIAN_POINT ( 'NONE',  ( 11.35168717260510007, -4.613789146762799831, 6.498190316041999814 ) ) ;
#64984 = DIRECTION ( 'NONE',  ( -1.000000000000000000, 0.000000000000000000, 0.000000000000000000 ) ) ;
#64985 = CARTESIAN_POINT ( 'NONE',  ( 10.60226354018307937, 5.092232985442822546, -8.129523725463620565 ) ) ;
#64986 = ORIENTED_EDGE ( 'NONE', *, *, #2792, .F. ) ;
#64987 = CARTESIAN_POINT ( 'NONE',  ( 23.60205915885299888, 11.53346724329999873, 4.150849519424002487 ) ) ;
#64988 = CARTESIAN_POINT ( 'NONE',  ( 5.763359839684166985, 1.310679582531388387, -0.7554284705563470981 ) ) ;
#64989 = EDGE_LOOP ( 'NONE', ( #5508, #38933, #68627, #27097 ) ) ;
#64990 = CARTESIAN_POINT ( 'NONE',  ( 12.80505043854146940, -3.199698446519381179, -12.18695736643652516 ) ) ;
#64991 = CARTESIAN_POINT ( 'NONE',  ( 10.96949144726329806, 3.419793223320000131, 8.318725197575499664 ) ) ;
#64992 = VECTOR ( 'NONE', #48097, 1000.000000000000000 ) ;
#64993 = CARTESIAN_POINT ( 'NONE',  ( 10.83488305961999920, -5.800181157098999840, -7.920538492179999501 ) ) ;
#64994 = ADVANCED_FACE ( 'NONE', ( #46719 ), #25726, .F. ) ;
#64995 = CARTESIAN_POINT ( 'NONE',  ( 10.61476354018239832, 5.217465845835394411, 7.827184855449092815 ) ) ;
#64996 = CARTESIAN_POINT ( 'NONE',  ( 17.60804966294600149, -11.49744311106999994, 4.819470927255000703 ) ) ;
#64997 = CARTESIAN_POINT ( 'NONE',  ( 10.90000000000000036, -0.2500000000000000000, 9.776630298829998011 ) ) ;
#64998 = CARTESIAN_POINT ( 'NONE',  ( 13.73899430609700190, 9.712898924749000074, 7.967785796560000300 ) ) ;
#64999 = CARTESIAN_POINT ( 'NONE',  ( 18.17981518646734784, -0.01996654564806030208, -12.69998441237379971 ) ) ;
#65000 = CARTESIAN_POINT ( 'NONE',  ( 12.25748074640750751, 2.187380181871708018, -12.51928400913670814 ) ) ;
#65001 = CARTESIAN_POINT ( 'NONE',  ( 10.15303300763299887, -3.212834858289399964, -8.325626572044798834 ) ) ;
#65002 = CARTESIAN_POINT ( 'NONE',  ( 7.711426658771000753, 5.797099724369999763, 8.340484548805999765 ) ) ;
#65003 = ORIENTED_EDGE ( 'NONE', *, *, #36236, .T. ) ;
#65004 = CARTESIAN_POINT ( 'NONE',  ( 24.35365242081699932, -10.79182034089001796, 4.028979492054000744 ) ) ;
#65005 = DIRECTION ( 'NONE',  ( 1.000000000000000000, 0.000000000000000000, 2.714292073215000052E-14 ) ) ;
#65006 = CARTESIAN_POINT ( 'NONE',  ( 11.44793382097000034, 12.36841772234000025, 1.594008128907999922 ) ) ;
#65007 = CARTESIAN_POINT ( 'NONE',  ( 17.99974802964002762, 1.911958328522579187, 12.45409441785080773 ) ) ;
#65008 = CARTESIAN_POINT ( 'NONE',  ( 11.12487850024999858, 5.426340361321000394, 5.164841153873000579 ) ) ;
#65009 = B_SPLINE_CURVE_WITH_KNOTS ( 'NONE', 3,
 ( #34648, #45129, #66093, #13324, #18211, #60858, #8065, #50717, #34297, #55620 ),
 .UNSPECIFIED., .F., .F.,
 ( 4, 2, 2, 2, 4 ),
 ( 0.000000000000000000, 0.1250000000000003053, 0.2500000000000006106, 0.3750000000000009437, 0.5000000000000011102 ),
 .UNSPECIFIED. ) ;
#65010 = CARTESIAN_POINT ( 'NONE',  ( 11.01763844555000027, 7.435008031470999867, 6.253913913716999673 ) ) ;
#65011 = CARTESIAN_POINT ( 'NONE',  ( 6.953052440528999512, -9.233022020364000326, -5.200634764108000851 ) ) ;
#65012 = LINE ( 'NONE', #26259, #12515 ) ;
#65013 = EDGE_CURVE ( 'NONE', #54684, #62696, #38944, .T. ) ;
#65014 = ORIENTED_EDGE ( 'NONE', *, *, #65753, .T. ) ;
#65015 = CARTESIAN_POINT ( 'NONE',  ( 12.14218285455822333, -2.187615620731410804, 12.40865911928243825 ) ) ;
#65016 = EDGE_CURVE ( 'NONE', #44713, #38686, #43454, .T. ) ;
#65017 = CARTESIAN_POINT ( 'NONE',  ( 9.758342523874999230, -5.128664655368000425, -7.327226901081999699 ) ) ;
#65018 = CARTESIAN_POINT ( 'NONE',  ( 24.50549018585800098, -3.501736898117000063, -12.23514954116999931 ) ) ;
#65019 = APPLICATION_CONTEXT ( 'automotive_design' ) ;
#65020 = CARTESIAN_POINT ( 'NONE',  ( 9.385788300200999856, -4.980873770300999759, 6.433336655958999728 ) ) ;
#65021 = CIRCLE ( 'NONE', #54964, 12.39999890530000037 ) ;
#65022 = ADVANCED_FACE ( 'NONE', ( #10332 ), #298, .T. ) ;
#65023 = CARTESIAN_POINT ( 'NONE',  ( 10.72333863405319931, 4.619094858989799768, -8.289729326049599223 ) ) ;
#65024 = CARTESIAN_POINT ( 'NONE',  ( 12.53820945512841689, -0.6689034848678564460, 12.58223305319197394 ) ) ;
#65025 = CARTESIAN_POINT ( 'NONE',  ( 9.368920280410000245, 5.618384167307999277, 7.727742442702000503 ) ) ;
#65026 = CARTESIAN_POINT ( 'NONE',  ( 9.939321360490000146, 2.638097915594000309, 6.328629954376999933 ) ) ;
#65027 = CARTESIAN_POINT ( 'NONE',  ( 12.54493252275448079, 3.068391087487184254, 12.30078773432381034 ) ) ;
#65028 = ORIENTED_EDGE ( 'NONE', *, *, #24999, .F. ) ;
#65029 = CARTESIAN_POINT ( 'NONE',  ( 18.48260618742725470, -3.086131726334561343, -12.13914505220688689 ) ) ;
#65030 = CARTESIAN_POINT ( 'NONE',  ( 11.58071932425156980, 3.832730087831799803, -8.628410767520000135 ) ) ;
#65031 = CARTESIAN_POINT ( 'NONE',  ( 11.04968150330033438, 2.750318496699665438, -6.534572094925334085 ) ) ;
#65032 = CARTESIAN_POINT ( 'NONE',  ( 11.18114303127866727, 3.379301870158037069, 6.880574739649332194 ) ) ;
#65034 = CARTESIAN_POINT ( 'NONE',  ( 24.97036913652599210, 11.51451018643214042, 3.225694753612683652 ) ) ;
#65033 = CARTESIAN_POINT ( 'NONE',  ( 5.500000000000000000, -0.2500000000000000000, -9.776630298829998011 ) ) ;
#65035 = CARTESIAN_POINT ( 'NONE',  ( 10.85056919669530018, -3.169300617545700138, -7.745432529082900253 ) ) ;
#65036 = CARTESIAN_POINT ( 'NONE',  ( 7.199141827028999963, 0.000000000000000000, 0.000000000000000000 ) ) ;
#65037 = ORIENTED_EDGE ( 'NONE', *, *, #32992, .F. ) ;
#65038 = VECTOR ( 'NONE', #50043, 1000.000000000000000 ) ;
#65039 = CARTESIAN_POINT ( 'NONE',  ( 2.116066937563999772, -3.284887521161000024, -0.9717780471415999877 ) ) ;
#65040 = EDGE_CURVE ( 'NONE', #16477, #12411, #48258, .T. ) ;
#65041 = PLANE ( 'NONE',  #42296 ) ;
#65042 = CARTESIAN_POINT ( 'NONE',  ( 12.35268573730777675, -12.09127048605781241, 3.267865047145097179 ) ) ;
#65043 = CARTESIAN_POINT ( 'NONE',  ( 24.37816253747470441, -3.385900881186148847, -12.24459612271480502 ) ) ;
#65044 = CARTESIAN_POINT ( 'NONE',  ( 12.32403884885184198, -1.971565993173706621, 13.86048321094706814 ) ) ;
#65045 = CARTESIAN_POINT ( 'NONE',  ( 10.90000000011000125, -5.100000000110999743, 6.571291220762999430 ) ) ;
#65046 = CARTESIAN_POINT ( 'NONE',  ( 23.83543860380300217, 3.383577400584000028, -13.10464564587000069 ) ) ;
#65047 = VERTEX_POINT ( 'NONE', #27289 ) ;
#65048 = DIRECTION ( 'NONE',  ( 1.000000000000000000, 0.000000000000000000, 0.000000000000000000 ) ) ;
#65049 = CARTESIAN_POINT ( 'NONE',  ( 9.856851002545999663, 2.832432432432000269, -6.822293592207000934 ) ) ;
#65050 = CARTESIAN_POINT ( 'NONE',  ( 10.89999960551999969, -1.382741157691000033, 11.26545764026000107 ) ) ;
#65051 = CARTESIAN_POINT ( 'NONE',  ( 1.080473797070000019, 3.196468001211000054, -1.639036658905000055 ) ) ;
#65052 = CARTESIAN_POINT ( 'NONE',  ( 13.99999999347100044, -9.187456302440001110, -8.213201953411001455 ) ) ;
#65053 = CARTESIAN_POINT ( 'NONE',  ( 17.55505043854143565, 1.874999999999999556, -12.57545641911173107 ) ) ;
#65054 = CARTESIAN_POINT ( 'NONE',  ( 11.12915085989000019, 3.083869275439000024, 8.585995236726001067 ) ) ;
#65055 = CARTESIAN_POINT ( 'NONE',  ( 11.51518179236248862, 3.819003318705799899, 8.347076615013298451 ) ) ;
#65056 = FACE_OUTER_BOUND ( 'NONE', #37321, .T. ) ;
#65057 = CARTESIAN_POINT ( 'NONE',  ( 10.66043185321000131, -2.315667072036000196, -7.431702410656999547 ) ) ;
#65058 = CARTESIAN_POINT ( 'NONE',  ( 12.15689047918783849, 2.896806234391597012, 13.69773071443709256 ) ) ;
#65059 = B_SPLINE_CURVE_WITH_KNOTS ( 'NONE', 3,
 ( #528, #31318, #32015, #4385, #42493, #21843, #53329, #10326, #36212, #68355, #52290, #47397, #52630, #57528, #9632, #47053, #26070, #20818 ),
 .UNSPECIFIED., .F., .F.,
 ( 4, 2, 1, 2, 2, 2, 1, 2, 2, 4 ),
 ( 0.000000000000000000, 0.2499999999999804601, 0.3749999999999698019, 0.4374999999999593658, 0.4999999999999489297, 0.6249999999999243938, 0.6874999999999182876, 0.7187499999999220623, 0.7499999999999258371, 1.000000000000000000 ),
 .UNSPECIFIED. ) ;
#65060 = CARTESIAN_POINT ( 'NONE',  ( 18.50001572531400029, -0.9783175529277773341, -12.52499999999999503 ) ) ;
#65061 = CARTESIAN_POINT ( 'NONE',  ( 21.60000000000000142, 0.000000000000000000, 0.000000000000000000 ) ) ;
#65062 = FACE_OUTER_BOUND ( 'NONE', #9613, .T. ) ;
#65063 = VERTEX_POINT ( 'NONE', #26604 ) ;
#65064 = CARTESIAN_POINT ( 'NONE',  ( 11.01268131116999882, -8.059163363648998768, -6.866685204375000851 ) ) ;
#65065 = ORIENTED_EDGE ( 'NONE', *, *, #18539, .T. ) ;
#65066 = VECTOR ( 'NONE', #24733, 999.9999999999998863 ) ;
#65067 = CARTESIAN_POINT ( 'NONE',  ( 18.02642401515176829, -2.910531091912870849, 13.57777274349195729 ) ) ;
#65068 = CARTESIAN_POINT ( 'NONE',  ( 11.05964426047339799, -3.312306505177499805, -8.577215873335999774 ) ) ;
#65069 = VERTEX_POINT ( 'NONE', #37424 ) ;
#65070 = CARTESIAN_POINT ( 'NONE',  ( 11.52677869730533011, 3.596497913043499750, 8.295667533166499297 ) ) ;
#65071 = CARTESIAN_POINT ( 'NONE',  ( 5.502110917525607547, 0.6366072631350736533, -0.9373824548834209791 ) ) ;
#65072 = CARTESIAN_POINT ( 'NONE',  ( 8.424688440789140031, 5.350083765069828523, 7.500019236172019710 ) ) ;
#65073 = EDGE_CURVE ( 'NONE', #60256, #40899, #24700, .T. ) ;
#65074 = CARTESIAN_POINT ( 'NONE',  ( 8.579854990165863171, -4.352864158101605874, 8.850923404438391984 ) ) ;
#65075 = EDGE_CURVE ( 'NONE', #20439, #57654, #18304, .T. ) ;
#65076 = CARTESIAN_POINT ( 'NONE',  ( 3.250973465878000290, -3.500000000000000000, 0.000000000000000000 ) ) ;
#65077 = CARTESIAN_POINT ( 'NONE',  ( 11.09999999999999964, 10.03015638309000046, -5.726993439934999763 ) ) ;
#65078 = DIRECTION ( 'NONE',  ( 1.000000000000000000, 0.000000000000000000, 0.000000000000000000 ) ) ;
#65079 = CARTESIAN_POINT ( 'NONE',  ( 10.82564972918999935, -5.331162346451000289, -8.542142527201001201 ) ) ;
#65080 = CARTESIAN_POINT ( 'NONE',  ( 11.53979707368350027, -4.430269712815499972, -6.748224392138099326 ) ) ;
#65081 = ORIENTED_EDGE ( 'NONE', *, *, #4738, .F. ) ;
#65082 = CARTESIAN_POINT ( 'NONE',  ( 10.01508584123000034, 4.845406482350000488, -6.387189183984999907 ) ) ;
#65083 = EDGE_LOOP ( 'NONE', ( #35718, #29248, #50577, #21162 ) ) ;
#65084 = VECTOR ( 'NONE', #28743, 1000.000000000000000 ) ;
#65085 = CARTESIAN_POINT ( 'NONE',  ( 10.78976354018297634, 3.672815144550904076, -6.282534154164603812 ) ) ;
#65086 = ORIENTED_EDGE ( 'NONE', *, *, #28179, .F. ) ;
#65087 = CARTESIAN_POINT ( 'NONE',  ( 17.55505043854147118, -3.248147246781390329, -13.61798588129781074 ) ) ;
#65088 = CARTESIAN_POINT ( 'NONE',  ( 10.55918725779999967, -5.125768249360000084, 4.818464946407000404 ) ) ;
#65089 = B_SPLINE_CURVE_WITH_KNOTS ( 'NONE', 3,
 ( #62297, #24554, #14415, #40973, #8129, #29475, #24893, #23513, #30487, #56371 ),
 .UNSPECIFIED., .F., .F.,
 ( 4, 2, 2, 2, 4 ),
 ( 0.000000000000000000, 0.2500000000000000000, 0.5000000000000000000, 0.7500000000000000000, 1.000000000000000000 ),
 .UNSPECIFIED. ) ;
#65090 = VECTOR ( 'NONE', #65005, 1000.000000000000000 ) ;
#65091 = CARTESIAN_POINT ( 'NONE',  ( 7.971709343838234041, 4.577294333992332653, -6.273541878819468565 ) ) ;
#65092 = CARTESIAN_POINT ( 'NONE',  ( 10.19095058442699830, 4.507735863714500191, -6.325866838823999139 ) ) ;
#65093 = CARTESIAN_POINT ( 'NONE',  ( 12.43888651633844056, 3.006915248264996343, 13.55273156457843697 ) ) ;
#65094 = CARTESIAN_POINT ( 'NONE',  ( 10.07101719722999889, -4.042170815906999337, 8.920201479886998186 ) ) ;
#65095 = CARTESIAN_POINT ( 'NONE',  ( 10.06577346837133291, 5.100000000000000533, 6.304440313804915874 ) ) ;
#65096 = CARTESIAN_POINT ( 'NONE',  ( 12.18528724423033438, 0.08139021474669518030, 13.89968437038781524 ) ) ;
#65097 = ORIENTED_EDGE ( 'NONE', *, *, #66212, .F. ) ;
#65098 = CARTESIAN_POINT ( 'NONE',  ( 10.96132811691999898, 2.899462099209999977, 4.932355079819999766 ) ) ;
#65099 = EDGE_CURVE ( 'NONE', #7987, #7389, #429, .T. ) ;
#65100 = CARTESIAN_POINT ( 'NONE',  ( 10.71093936573047145, 4.907409303783653698, -4.810214324746542758 ) ) ;
#65101 = CARTESIAN_POINT ( 'NONE',  ( 9.378875014952626543, 4.868116531169106587, 7.609114422657746069 ) ) ;
#65102 = CARTESIAN_POINT ( 'NONE',  ( 5.034914323403000047, 0.9510812144104999755, -0.7102707857375000211 ) ) ;
#65103 = EDGE_CURVE ( 'NONE', #65069, #17653, #32197, .T. ) ;
#65104 = CARTESIAN_POINT ( 'NONE',  ( 8.988579719593998263, 4.902869380824999901, -8.978557145469999057 ) ) ;
#65105 = FACE_OUTER_BOUND ( 'NONE', #17716, .T. ) ;
#65106 = CARTESIAN_POINT ( 'NONE',  ( 10.39355669675000016, -4.089958462238000081, -9.188182957628999503 ) ) ;
#65107 = VERTEX_POINT ( 'NONE', #47585 ) ;
#65108 = CARTESIAN_POINT ( 'NONE',  ( 9.537027461449516963, -5.286011494985110026, -7.027146145907680719 ) ) ;
#65109 = DIRECTION ( 'NONE',  ( 0.000000000000000000, 1.000000000000000000, 0.000000000000000000 ) ) ;
#65110 = FILL_AREA_STYLE ('',( #22820 ) ) ;
#65111 = CARTESIAN_POINT ( 'NONE',  ( 29.91622776632000225, -7.451149524158998971E-09, 6.772075922106999712 ) ) ;
#65112 = CARTESIAN_POINT ( 'NONE',  ( 8.627615187423813836, -2.899999999999999911, 6.423404451745915011 ) ) ;
#65113 = CARTESIAN_POINT ( 'NONE',  ( 24.30001680106099826, 12.21047197645999915, -3.271805488357999891 ) ) ;
#65114 = B_SPLINE_CURVE_WITH_KNOTS ( 'NONE', 3,
 ( #7132, #1542, #60620, #55727 ),
 .UNSPECIFIED., .F., .F.,
 ( 4, 4 ),
 ( 0.7545333173052201081, 1.000000000000000000 ),
 .UNSPECIFIED. ) ;
#65115 = AXIS2_PLACEMENT_3D ( 'NONE', #42322, #41964, #20638 ) ;
#65116 = CARTESIAN_POINT ( 'NONE',  ( 11.01790547754519878, 5.174295865741999734, -7.537269019642879542 ) ) ;
#65117 = CARTESIAN_POINT ( 'NONE',  ( 8.925442991499998868, 3.936771438983030169, -6.497580701799000380 ) ) ;
#65119 = CARTESIAN_POINT ( 'NONE',  ( 10.95824452673999971, -2.933481078303000089, 5.181932056174999524 ) ) ;
#65118 = CARTESIAN_POINT ( 'NONE',  ( 9.293822372493998785, -4.288705740401799638, 6.555546982591299532 ) ) ;
#65120 = CARTESIAN_POINT ( 'NONE',  ( 10.90000000000000036, 2.778483479159999714, -6.925197956411000000 ) ) ;
#65121 = VERTEX_POINT ( 'NONE', #42344 ) ;
#65122 = CIRCLE ( 'NONE', #60651, 0.7499999936418002555 ) ;
#65123 = B_SPLINE_CURVE_WITH_KNOTS ( 'NONE', 3,
 ( #26717, #16555, #22486, #480, #43828, #48372 ),
 .UNSPECIFIED., .F., .F.,
 ( 4, 2, 4 ),
 ( 0.000000000000000000, 0.5000000000000000000, 1.000000000000000000 ),
 .UNSPECIFIED. ) ;
#65124 = EDGE_CURVE ( 'NONE', #55522, #23367, #26088, .T. ) ;
#65125 = CARTESIAN_POINT ( 'NONE',  ( 10.69057802013490033, 2.966773425016000054, 7.524052967375959966 ) ) ;
#65126 = CARTESIAN_POINT ( 'NONE',  ( 10.09196524370999981, -3.841385669346000231, 5.536421174581999338 ) ) ;
#65127 = CARTESIAN_POINT ( 'NONE',  ( 9.000480666858997836, 4.426512626096299918, 6.293984733123999753 ) ) ;
#65128 = CARTESIAN_POINT ( 'NONE',  ( 5.667284888080160066, -12.98956018065501894, -2.203076788700562005 ) ) ;
#65129 = CARTESIAN_POINT ( 'NONE',  ( 10.99433452212999818, -3.697619272994999928, 5.729306330972000261 ) ) ;
#65130 = CARTESIAN_POINT ( 'NONE',  ( 10.02052890782000105, -2.899999999999999911, 6.152188490330000370 ) ) ;
#65131 = CARTESIAN_POINT ( 'NONE',  ( 11.83936489023500194, 3.414328975993000004, -11.89720897182000137 ) ) ;
#65132 = VECTOR ( 'NONE', #24351, 1000.000000000000114 ) ;
#65133 = CARTESIAN_POINT ( 'NONE',  ( 10.18988779216199880, -2.943881405003000218, -7.880862084500499520 ) ) ;
#65134 = LINE ( 'NONE', #49412, #59989 ) ;
#65135 = CARTESIAN_POINT ( 'NONE',  ( 6.585575618757999905, 0.7284491026353999699, 1.103547660897999938 ) ) ;
#65136 = CARTESIAN_POINT ( 'NONE',  ( 10.39393020684899938, -5.250000000000000000, 7.500000000000000000 ) ) ;
#65137 = VECTOR ( 'NONE', #33570, 1000.000000000000000 ) ;
#65138 = DIRECTION ( 'NONE',  ( 0.000000000000000000, -0.1333333333333049375, 0.9910712498212376209 ) ) ;
#65139 = B_SPLINE_CURVE_WITH_KNOTS ( 'NONE', 3,
 ( #47520, #51723, #30752, #14674 ),
 .UNSPECIFIED., .F., .F.,
 ( 4, 4 ),
 ( 0.000000000000000000, 1.000000000000000000 ),
 .UNSPECIFIED. ) ;
#65140 = CARTESIAN_POINT ( 'NONE',  ( 12.61341903040855783, 0.5949840079737199749, -12.68123264482376555 ) ) ;
#65141 = CARTESIAN_POINT ( 'NONE',  ( 11.68748876160954886, 3.399618311400500303, -8.124372018288600117 ) ) ;
#65142 = CARTESIAN_POINT ( 'NONE',  ( 10.96985954691664844, 5.113501917432773602, 4.936516852154429813 ) ) ;
#65143 = CARTESIAN_POINT ( 'NONE',  ( 24.84742924726900171, -8.571349809962997668, 8.858692393521000241 ) ) ;
#65144 = CARTESIAN_POINT ( 'NONE',  ( 0.9988901325417289812, 2.798833948393634419, -2.150913519912196925 ) ) ;
#65145 = EDGE_LOOP ( 'NONE', ( #63128, #2474, #55643, #15711 ) ) ;
#65146 = FACE_OUTER_BOUND ( 'NONE', #11338, .T. ) ;
#65147 = CONTEXT_DEPENDENT_SHAPE_REPRESENTATION ( #61468, #67483 ) ;
#65148 = CARTESIAN_POINT ( 'NONE',  ( 10.98146005378009882, -3.088328798999600000, -7.013182449205100255 ) ) ;
#65149 = DIRECTION ( 'NONE',  ( 0.000000000000000000, -0.7180577844781753649, -0.6959834898546763959 ) ) ;
#65150 = CARTESIAN_POINT ( 'NONE',  ( 10.53976354018315753, -3.672815144550900524, -8.717465845835397076 ) ) ;
#65151 = CARTESIAN_POINT ( 'NONE',  ( 10.62120626703515214, 3.646797508062010529, 8.848526273074872606 ) ) ;
#65152 = CARTESIAN_POINT ( 'NONE',  ( 13.43590051321700152, 12.19118104410000036, 2.154281854449000555 ) ) ;
#65153 = ORIENTED_EDGE ( 'NONE', *, *, #49334, .F. ) ;
#65154 = CARTESIAN_POINT ( 'NONE',  ( 24.35365242081699932, 8.948887819794997256, 8.923422014253004519 ) ) ;
#65155 = CARTESIAN_POINT ( 'NONE',  ( 8.776575450301999481, -4.067929031554969654, -8.439408300974900357 ) ) ;
#65156 = ORIENTED_EDGE ( 'NONE', *, *, #40205, .F. ) ;
#65157 = DIRECTION ( 'NONE',  ( -1.000000000000000000, 0.000000000000000000, 0.000000000000000000 ) ) ;
#65158 = CARTESIAN_POINT ( 'NONE',  ( 24.76116842704180598, 8.629365340259456119, -8.563010230132558576 ) ) ;
#65159 = CARTESIAN_POINT ( 'NONE',  ( 9.708354719591000048, 5.481267232667000222, -8.005061172455999241 ) ) ;
#65160 = ADVANCED_FACE ( 'NONE', ( #22025 ), #885, .F. ) ;
#65161 = CARTESIAN_POINT ( 'NONE',  ( 17.60000003185799855, -12.11983897296999935, 3.159727888982000188 ) ) ;
#65162 = EDGE_CURVE ( 'NONE', #33712, #10649, #1064, .T. ) ;
#65163 = CARTESIAN_POINT ( 'NONE',  ( 17.82373361328021488, 1.839709763185447988, -13.87859827090101028 ) ) ;
#65164 = CARTESIAN_POINT ( 'NONE',  ( 7.862285841224999849, 5.899700469177000528, -7.473738753146999869 ) ) ;
#65165 = CARTESIAN_POINT ( 'NONE',  ( 11.59999999999999964, 4.000000000000000000, -7.500000000000000000 ) ) ;
#65166 = EDGE_CURVE ( 'NONE', #24800, #38239, #32266, .T. ) ;
#65167 = CARTESIAN_POINT ( 'NONE',  ( 10.38351354018233508, -5.249999999999998224, 7.663624617374469317 ) ) ;
#65168 = EDGE_LOOP ( 'NONE', ( #18073, #48145, #2346, #6085, #39987 ) ) ;
#65169 = DIRECTION ( 'NONE',  ( 0.000000000000000000, -1.000000000000000000, 0.000000000000000000 ) ) ;
#65170 = VECTOR ( 'NONE', #56104, 1000.000000000000000 ) ;
#65171 = DIRECTION ( 'NONE',  ( 0.000000000000000000, 0.000000000000000000, -1.000000000000000000 ) ) ;
#65172 = CARTESIAN_POINT ( 'NONE',  ( 11.18424042080583369, 4.544092497359196514, -6.342116603374313044 ) ) ;
#65173 = ORIENTED_EDGE ( 'NONE', *, *, #26072, .F. ) ;
#65174 = AXIS2_PLACEMENT_3D ( 'NONE', #25391, #25742, #4403 ) ;
#65175 = CARTESIAN_POINT ( 'NONE',  ( 11.30000000000000071, -3.738146657027650033, 11.41167835205686742 ) ) ;
#65176 = CARTESIAN_POINT ( 'NONE',  ( 11.37167944038000122, -2.803484087760999888, -6.967877228197000505 ) ) ;
#65177 = ORIENTED_EDGE ( 'NONE', *, *, #29225, .T. ) ;
#65178 = CARTESIAN_POINT ( 'NONE',  ( 8.798797255587999189, 5.003512473869000665, 7.542485555928790220 ) ) ;
#65179 = CARTESIAN_POINT ( 'NONE',  ( 17.85722199349619643, -1.826245811740498270, -12.46695042358089012 ) ) ;
#65180 = CARTESIAN_POINT ( 'NONE',  ( 5.024329738858000383, -1.220804671313000078, -0.7183737188287999675 ) ) ;
#65181 = CARTESIAN_POINT ( 'NONE',  ( 11.59999999999999964, 4.834915812642036848, -6.701316188976606192 ) ) ;
#65182 = CARTESIAN_POINT ( 'NONE',  ( 24.90037535684063741, 11.58835108095975563, -3.208324347671906995 ) ) ;
#65183 = DIRECTION ( 'NONE',  ( 1.000000000000000000, 0.000000000000000000, 0.000000000000000000 ) ) ;
#65184 = CARTESIAN_POINT ( 'NONE',  ( 10.16657120343299958, 3.951311476804090006, 6.496769302834999316 ) ) ;
#65185 = CARTESIAN_POINT ( 'NONE',  ( 8.705629240797998492, 3.771058080785100408, -8.376522367004298530 ) ) ;
#65186 = ORIENTED_EDGE ( 'NONE', *, *, #42149, .T. ) ;
#65187 = DIRECTION ( 'NONE',  ( -1.000000000000000000, 0.000000000000000000, 0.000000000000000000 ) ) ;
#65188 = CARTESIAN_POINT ( 'NONE',  ( 10.63743278041000018, 3.721476136598000028, -8.997092462634000753 ) ) ;
#65189 = AXIS2_PLACEMENT_3D ( 'NONE', #51999, #47115, #20192 ) ;
#65190 = CARTESIAN_POINT ( 'NONE',  ( 18.04298231209847359, -12.08956857263229168, 3.273859435796452999 ) ) ;
#65191 = CARTESIAN_POINT ( 'NONE',  ( 12.43914160838490623, 1.887194142572508282, -13.87222517180307868 ) ) ;
#65192 = CARTESIAN_POINT ( 'NONE',  ( 11.27101354018290102, -4.768183399968641822, 8.499583552997725278 ) ) ;
#65193 = CARTESIAN_POINT ( 'NONE',  ( 10.71256247620999957, -5.951803124515000043, 7.233045248871000865 ) ) ;
#65194 = CARTESIAN_POINT ( 'NONE',  ( 18.22055847946775131, -0.2899337805559755732, 13.99700184298317041 ) ) ;
#65195 = AXIS2_PLACEMENT_3D ( 'NONE', #39300, #65157, #7832 ) ;
#65196 = CARTESIAN_POINT ( 'NONE',  ( 25.41802129974299973, -2.807511311350999961, 11.31773419928000024 ) ) ;
#65197 = VERTEX_POINT ( 'NONE', #29029 ) ;
#65198 = ORIENTED_EDGE ( 'NONE', *, *, #21019, .F. ) ;
#65199 = CARTESIAN_POINT ( 'NONE',  ( 10.02201554968999986, 3.298015135926000152, 5.700522662207000657 ) ) ;
#65200 = CARTESIAN_POINT ( 'NONE',  ( 12.32101708573729226, -0.3953980351163901563, 13.89243073565879172 ) ) ;
#65201 = AXIS2_PLACEMENT_3D ( 'NONE', #5739, #4362, #15889 ) ;
#65202 = B_SPLINE_CURVE_WITH_KNOTS ( 'NONE', 3,
 ( #20103, #20444, #151, #26733, #47367, #21469, #37548, #58531, #63427, #20790, #69024, #10986, #41771, #5397, #36183, #31982, #14860, #42120 ),
 .UNSPECIFIED., .F., .F.,
 ( 4, 2, 2, 2, 2, 2, 2, 2, 4 ),
 ( 0.1254150264828375605, 0.2190616449219018325, 0.3127082633609661322, 0.4063548818000304319, 0.5000015002390947316, 0.5936481186781590313, 0.6872947371172232200, 0.7809413555562875198, 0.8745879739953518195 ),
 .UNSPECIFIED. ) ;
#65203 = CARTESIAN_POINT ( 'NONE',  ( 12.33180813479863502, -0.4082709497318060543, -13.89192968283203200 ) ) ;
#65204 = CARTESIAN_POINT ( 'NONE',  ( 10.87522165821000009, -4.831071966430999787, 6.312786525516999703 ) ) ;
#65205 = FACE_OUTER_BOUND ( 'NONE', #51679, .T. ) ;
#65206 = CARTESIAN_POINT ( 'NONE',  ( 10.90000000000000036, -2.778483479159999714, -6.925197956411000000 ) ) ;
#65207 = CARTESIAN_POINT ( 'NONE',  ( 25.27002764979846816, 8.359940994488436417, -8.486676288913415078 ) ) ;
#65209 = DIRECTION ( 'NONE',  ( 0.000000000000000000, 0.9466492601157000530, -0.3222656952305000266 ) ) ;
#65208 = CARTESIAN_POINT ( 'NONE',  ( 10.48831740696900106, -3.762080884004200154, 6.243107450209000042 ) ) ;
#65210 = DIRECTION ( 'NONE',  ( 0.000000000000000000, -0.9466492601157000530, 0.3222656952305000266 ) ) ;
#65211 = CARTESIAN_POINT ( 'NONE',  ( 24.30857393632600250, -8.915481952665000875, -8.861377372684998477 ) ) ;
#65212 = EDGE_CURVE ( 'NONE', #31626, #10089, #30581, .T. ) ;
#65213 = CARTESIAN_POINT ( 'NONE',  ( 8.918455549952998496, 4.674761969675400586, -6.955569812538500152 ) ) ;
#65214 = CARTESIAN_POINT ( 'NONE',  ( 17.59617179617751503, -0.6239794389693676946, 12.67935706666152740 ) ) ;
#65215 = B_SPLINE_SURFACE_WITH_KNOTS ( 'NONE', 3, 3, ( 
 ( #68146, #51396, #46154, #62899 ),
 ( #9764, #68837, #37037, #57660 ),
 ( #40904, #31115, #58352, #25852 ),
 ( #20609, #62225, #31449, #10454 ),
 ( #68486, #35666, #36695, #56981 ),
 ( #15019, #62561, #3491, #57317 ),
 ( #4861, #19925, #9417, #41934 ),
 ( #24827, #9084, #52419, #58016 ),
 ( #52768, #26204, #30423, #51733 ) ),
 .UNSPECIFIED., .F., .F., .F.,
 ( 4, 1, 1, 1, 1, 1, 4 ),
 ( 4, 4 ),
 ( 0.05214259105098999897, 0.1666666666667000196, 0.3333333333333000081, 0.5000000000000000000, 0.6666666666667000474, 0.8333333333333000637, 0.9777068595523999983 ),
 ( -0.1900882580235000174, 1.190231865545000156 ),
 .UNSPECIFIED. ) ;
#65216 = CARTESIAN_POINT ( 'NONE',  ( 8.327311442791936358, -2.900678125132057694, 6.583025523232378440 ) ) ;
#65217 = EDGE_CURVE ( 'NONE', #34701, #42176, #1748, .T. ) ;
#65218 = CARTESIAN_POINT ( 'NONE',  ( 17.92143259511168552, -3.006721712955584991, -12.31894844866650551 ) ) ;
#65219 = ORIENTED_EDGE ( 'NONE', *, *, #44598, .T. ) ;
#65221 = DIRECTION ( 'NONE',  ( 0.000000000000000000, -1.000000000000000000, 0.000000000000000000 ) ) ;
#65220 = CARTESIAN_POINT ( 'NONE',  ( 8.610058059625000482, -5.329429281359999493, 6.027400270608000099 ) ) ;
#65222 = CARTESIAN_POINT ( 'NONE',  ( 8.307195280408999238, 5.473983809665999622, -8.180077404516000072 ) ) ;
#65223 = DIRECTION ( 'NONE',  ( 1.000000000000000000, 0.000000000000000000, 0.000000000000000000 ) ) ;
#65224 = CARTESIAN_POINT ( 'NONE',  ( 23.60205915885299888, 9.230633470682002795, -8.204162215359994903 ) ) ;
#65225 = CIRCLE ( 'NONE', #40683, 10.80000000000000604 ) ;
#65226 = B_SPLINE_CURVE_WITH_KNOTS ( 'NONE', 3,
 ( #41739, #52226, #10606, #4324 ),
 .UNSPECIFIED., .F., .F.,
 ( 4, 4 ),
 ( 0.000000000000000000, 1.000000000000000000 ),
 .UNSPECIFIED. ) ;
#65227 = CARTESIAN_POINT ( 'NONE',  ( 0.5433723959866999520, 0.6801881511091000254, 3.471639432493999866 ) ) ;
#65228 = B_SPLINE_SURFACE_WITH_KNOTS ( 'NONE', 3, 3, ( 
 ( #33924, #55245, #17135, #39509 ),
 ( #22382, #65723, #28684, #65374 ),
 ( #49650, #17847, #44073, #6997 ),
 ( #49298, #11893, #65018, #1755 ),
 ( #33233, #38470, #50001, #22727 ),
 ( #5955, #59790, #54897, #33577 ) ),
 .UNSPECIFIED., .F., .F., .F.,
 ( 4, 1, 1, 4 ),
 ( 4, 4 ),
 ( 0.1423941366080999915, 0.3333333333333000081, 0.6666666666667000474, 0.8219462302419999755 ),
 ( -0.1256563615234000120, 1.125656361508000192 ),
 .UNSPECIFIED. ) ;
#65229 = CARTESIAN_POINT ( 'NONE',  ( 9.401555021597628681, 2.569600868085949674, 8.509762776563993825 ) ) ;
#65230 = CARTESIAN_POINT ( 'NONE',  ( 2.547610702941999872, 2.269953836787999890, -2.784090233961999949 ) ) ;
#65231 = EDGE_LOOP ( 'NONE', ( #24236, #2865, #47999, #22796 ) ) ;
#65232 = CARTESIAN_POINT ( 'NONE',  ( 12.08233499759479912, 0.05827135643914355123, -12.59987075990256855 ) ) ;
#65233 = FACE_OUTER_BOUND ( 'NONE', #47273, .T. ) ;
#65234 = CARTESIAN_POINT ( 'NONE',  ( 18.14576286523417892, 2.898275280820967748, -12.26215340014708488 ) ) ;
#65235 = CARTESIAN_POINT ( 'NONE',  ( 5.500000000000000000, 0.8000000000000000444, 3.149999999999999911 ) ) ;
#65236 = CARTESIAN_POINT ( 'NONE',  ( 7.191892219589999691, 3.501518846194999757, 9.055971388486000251 ) ) ;
#65237 = VERTEX_POINT ( 'NONE', #59781 ) ;
#65238 = CARTESIAN_POINT ( 'NONE',  ( 6.889531036634999772, 0.8895447933473999980, 1.347595971237000256 ) ) ;
#65239 = CARTESIAN_POINT ( 'NONE',  ( 7.101645280409999650, 4.411055010497999973, -9.010057343561001630 ) ) ;
#65241 = CARTESIAN_POINT ( 'NONE',  ( 9.576488281553999116, 4.593976206186999534, 5.662041230125000268 ) ) ;
#65240 = CARTESIAN_POINT ( 'NONE',  ( 8.448578618970964627, -2.260522387638269848, 7.526897675015515432 ) ) ;
#65242 = CONICAL_SURFACE ( 'NONE', #18403, 0.8999999994071996579, 0.7853981633972997312 ) ;
#65243 = CARTESIAN_POINT ( 'NONE',  ( 12.80505043854143388, 1.836970230372604318, 12.54239289408378255 ) ) ;
#65244 = VERTEX_POINT ( 'NONE', #55930 ) ;
#65245 = CARTESIAN_POINT ( 'NONE',  ( 8.599999952505998024, 4.000000000000000000, 6.750000006358199300 ) ) ;
#65246 = SURFACE_STYLE_FILL_AREA ( #65594 ) ;
#65247 = VERTEX_POINT ( 'NONE', #11885 ) ;
#65248 = DIRECTION ( 'NONE',  ( -0.000000000000000000, -0.000000000000000000, 1.000000000000000000 ) ) ;
#65249 = CARTESIAN_POINT ( 'NONE',  ( 16.39965637475000193, 3.313349101483999970, 11.22428178643999885 ) ) ;
#65250 = CARTESIAN_POINT ( 'NONE',  ( 18.11587426570509862, -0.2766185922798718999, -13.89631150889695732 ) ) ;
#65251 = ORIENTED_EDGE ( 'NONE', *, *, #19128, .F. ) ;
#65252 = CARTESIAN_POINT ( 'NONE',  ( 15.58179592144909265, -8.803826609191874653, -7.629963841725977858 ) ) ;
#65253 = EDGE_CURVE ( 'NONE', #47064, #62822, #44416, .T. ) ;
#65254 = FACE_OUTER_BOUND ( 'NONE', #63083, .T. ) ;
#65255 = CARTESIAN_POINT ( 'NONE',  ( 10.39969598649000027, 4.888000489779200208, -8.028730309000598808 ) ) ;
#65256 = CARTESIAN_POINT ( 'NONE',  ( 4.600000127571202135, 3.375077994860000042E-14, 1.048050535245999973E-13 ) ) ;
#65257 = EDGE_CURVE ( 'NONE', #10305, #39016, #48906, .T. ) ;
#65258 = DIRECTION ( 'NONE',  ( 1.000000000000000000, 0.000000000000000000, 0.000000000000000000 ) ) ;
#65259 = VERTEX_POINT ( 'NONE', #54544 ) ;
#65260 = CARTESIAN_POINT ( 'NONE',  ( 8.385051658773999606, 4.977909614887999545, 6.416776202806000029 ) ) ;
#65261 = EDGE_CURVE ( 'NONE', #24634, #60155, #51784, .T. ) ;
#65262 = CARTESIAN_POINT ( 'NONE',  ( 12.54566616139125834, -3.068981097034638950, -13.53612220331446281 ) ) ;
#65263 = AXIS2_PLACEMENT_3D ( 'NONE', #46097, #13945, #18156 ) ;
#65264 = CARTESIAN_POINT ( 'NONE',  ( 9.896013540183334456, -4.999583552997726166, 6.731816600031358178 ) ) ;
#65265 = CARTESIAN_POINT ( 'NONE',  ( 15.39403162610500075, -9.133592062008998980, -8.216350050208999889 ) ) ;
#65266 = VERTEX_POINT ( 'NONE', #1402 ) ;
#65267 = CARTESIAN_POINT ( 'NONE',  ( 12.69127452969531156, -1.885356761727419839, -12.57371515106196114 ) ) ;
#65268 = CARTESIAN_POINT ( 'NONE',  ( 11.09999999999999964, -5.350000000000000533, -7.500000000000000000 ) ) ;
#65269 = CARTESIAN_POINT ( 'NONE',  ( 7.590547165042061728, 2.142854238949568835, -7.493582139438092149 ) ) ;
#65270 = CARTESIAN_POINT ( 'NONE',  ( 5.000030787343000327, 1.834918991542629385, 1.057581170753186806 ) ) ;
#65271 = FACE_OUTER_BOUND ( 'NONE', #54145, .T. ) ;
#65272 = CARTESIAN_POINT ( 'NONE',  ( 10.72333863405319931, -3.380905141010200232, -8.289729326049599223 ) ) ;
#65273 = FACE_OUTER_BOUND ( 'NONE', #16154, .T. ) ;
#65274 = CARTESIAN_POINT ( 'NONE',  ( 17.74533816909192296, -1.785653880132711535, 12.47283005504979059 ) ) ;
#65275 = ORIENTED_EDGE ( 'NONE', *, *, #6773, .T. ) ;
#65276 = CARTESIAN_POINT ( 'NONE',  ( 11.46989666366029859, -4.058428102321880004, -8.814970315645998866 ) ) ;
#65277 = ORIENTED_EDGE ( 'NONE', *, *, #51471, .F. ) ;
#65278 = ADVANCED_FACE ( 'NONE', ( #39156 ), #48891, .F. ) ;
#65279 = CONICAL_SURFACE ( 'NONE', #68617, 2.049999999589000588, 0.7853981633972997312 ) ;
#65280 = CARTESIAN_POINT ( 'NONE',  ( 11.80427293869800032, -12.43391773449000048, -1.801004847141999932 ) ) ;
#65281 = CARTESIAN_POINT ( 'NONE',  ( 9.289886373836322875, -3.999992178805580334, 6.560153657526066162 ) ) ;
#65282 = CARTESIAN_POINT ( 'NONE',  ( 2.545075687104000117, -2.780561538855000236, 1.920602712081999952 ) ) ;
#65283 = CARTESIAN_POINT ( 'NONE',  ( 10.38153277269999997, -2.772136814285999673, -8.408084799892998618 ) ) ;
#65284 = CARTESIAN_POINT ( 'NONE',  ( 6.617301518455933618, -1.500125606900863939, -0.2316530497092380014 ) ) ;
#65285 = AXIS2_PLACEMENT_3D ( 'NONE', #57978, #68796, #42587 ) ;
#65286 = CARTESIAN_POINT ( 'NONE',  ( 24.15333686126099977, 12.81676537908000135, 3.250112501260999931 ) ) ;
#65287 = DIRECTION ( 'NONE',  ( -0.7071067811864999442, 0.09428090792503998618, -0.7007932008808999136 ) ) ;
#65288 = EDGE_LOOP ( 'NONE', ( #38642, #3086, #13297, #47119 ) ) ;
#65289 = CARTESIAN_POINT ( 'NONE',  ( 1.900788447236333445, -1.095349359437870485, -3.341294758621923044 ) ) ;
#65290 = CARTESIAN_POINT ( 'NONE',  ( 10.49785886974000171, 3.776281431161999880, 5.717632172928999168 ) ) ;
#65291 = FACE_BOUND ( 'NONE', #21813, .T. ) ;
#65292 = CARTESIAN_POINT ( 'NONE',  ( 12.80505043854144276, -0.6564304467897706941, -12.64601024127358286 ) ) ;
#65293 = CARTESIAN_POINT ( 'NONE',  ( 18.18404792230800382, 3.205001206845999651, -11.25648540289999922 ) ) ;
#65294 = CARTESIAN_POINT ( 'NONE',  ( 11.02287616594229824, 3.738072157442200005, -6.674353346984900348 ) ) ;
#65295 = B_SPLINE_CURVE_WITH_KNOTS ( 'NONE', 3,
 ( #56078, #2591, #23922, #18681 ),
 .UNSPECIFIED., .F., .F.,
 ( 4, 4 ),
 ( 0.000000000000000000, 1.000000000000000000 ),
 .UNSPECIFIED. ) ;
#65296 = CARTESIAN_POINT ( 'NONE',  ( 7.100000000000139977, 3.928301696086603734, -8.885577256977402527 ) ) ;
#65297 = VECTOR ( 'NONE', #20055, 1000.000000000000000 ) ;
#65298 = CARTESIAN_POINT ( 'NONE',  ( 24.13718290469899941, -9.106000876233000696, -8.983949862985999957 ) ) ;
#65299 = CARTESIAN_POINT ( 'NONE',  ( 24.33639158961700133, -8.941349246732999134, 9.047440025103000494 ) ) ;
#65300 = DIRECTION ( 'NONE',  ( -0.4999999999999719669, 0.6407827956774649891, -0.5825782426110679424 ) ) ;
#65301 = ADVANCED_FACE ( 'NONE', ( #61515 ), #40198, .F. ) ;
#65302 = EDGE_LOOP ( 'NONE', ( #43377, #36895, #20258, #40821 ) ) ;
#65303 = CARTESIAN_POINT ( 'NONE',  ( 7.795980646793000624, -3.164807285701999984, 9.104732190648000767 ) ) ;
#65304 = CARTESIAN_POINT ( 'NONE',  ( 9.399722005181999407, -5.700621988293000264, -7.339579610785999186 ) ) ;
#65305 = CARTESIAN_POINT ( 'NONE',  ( 18.11617320663394892, 2.776000138870930556, 13.61099849375432491 ) ) ;
#65306 = DIRECTION ( 'NONE',  ( -1.000000000000000000, 0.000000000000000000, 0.000000000000000000 ) ) ;
#65307 = CARTESIAN_POINT ( 'NONE',  ( 10.66579975933730040, -2.791514215189000225, -7.084213409908699965 ) ) ;
#65308 = VERTEX_POINT ( 'NONE', #8719 ) ;
#65309 = B_SPLINE_CURVE_WITH_KNOTS ( 'NONE', 3,
 ( #40406, #3001, #65596, #40084 ),
 .UNSPECIFIED., .F., .F.,
 ( 4, 4 ),
 ( 0.000000000000000000, 1.000000000000000000 ),
 .UNSPECIFIED. ) ;
#65310 = CARTESIAN_POINT ( 'NONE',  ( 25.47132134066600173, 2.701728734476000149, -11.27934147707000179 ) ) ;
#65311 = CARTESIAN_POINT ( 'NONE',  ( 7.320267219589999819, 2.466388272391000225, 6.935562100014999842 ) ) ;
#65312 = CARTESIAN_POINT ( 'NONE',  ( 8.605545280412000508, 3.122811675949999977, -6.006064052396999919 ) ) ;
#65313 = CARTESIAN_POINT ( 'NONE',  ( 25.50734665507583188, -11.18386470588408876, 3.138222106905402597 ) ) ;
#65314 = ORIENTED_EDGE ( 'NONE', *, *, #2457, .T. ) ;
#65315 = CARTESIAN_POINT ( 'NONE',  ( 11.00588826681000043, 3.012760565655999923, 5.961496895743000124 ) ) ;
#65316 = CARTESIAN_POINT ( 'NONE',  ( 17.65134488495972676, -1.793858269351544132, -13.88459860980089644 ) ) ;
#65317 = CARTESIAN_POINT ( 'NONE',  ( 10.92026088462129962, 4.002135146349410810, 8.503467136482999678 ) ) ;
#65318 = CARTESIAN_POINT ( 'NONE',  ( 9.848253563160000112, -4.436921580929999998, 6.148020168057000134 ) ) ;
#65319 = CARTESIAN_POINT ( 'NONE',  ( 7.545207810761997536, 3.529659010889000026, 6.570477302111996210 ) ) ;
#65320 = ORIENTED_EDGE ( 'NONE', *, *, #39476, .F. ) ;
#65321 = CARTESIAN_POINT ( 'NONE',  ( 11.30000000000000071, 0.000000000000000000, 0.000000000000000000 ) ) ;
#65322 = DIRECTION ( 'NONE',  ( -1.000000000000000000, 0.000000000000000000, 0.000000000000000000 ) ) ;
#65324 = CARTESIAN_POINT ( 'NONE',  ( 10.63743064679000128, -3.721475434679999861, -8.997096235511000017 ) ) ;
#65323 = CARTESIAN_POINT ( 'NONE',  ( 12.29459504890700039, -12.00990144118000025, 3.349639255392000248 ) ) ;
#65325 = CARTESIAN_POINT ( 'NONE',  ( 7.804884823657623372, -4.430740684302771903, 9.185820566326194481 ) ) ;
#65326 = CARTESIAN_POINT ( 'NONE',  ( 11.02286109245999945, -2.398753588646000079, 6.352476128646999065 ) ) ;
#65327 = CARTESIAN_POINT ( 'NONE',  ( 23.64816362642000414, 3.331185260057999642, 13.50063194398999933 ) ) ;
#65328 = CARTESIAN_POINT ( 'NONE',  ( 10.48725461470299969, -5.106563667948999630, 7.218483930889299849 ) ) ;
#65329 = ORIENTED_EDGE ( 'NONE', *, *, #59478, .T. ) ;
#65330 = CARTESIAN_POINT ( 'NONE',  ( 24.23080253867526679, -9.028074447669709457, 9.023970195626347390 ) ) ;
#65331 = CARTESIAN_POINT ( 'NONE',  ( 10.77610941423800028, -3.155589807313900153, 8.266982106121901097 ) ) ;
#65332 = ORIENTED_EDGE ( 'NONE', *, *, #54309, .F. ) ;
#65333 = CARTESIAN_POINT ( 'NONE',  ( 7.581295643773000137, 2.929975047062999050, 6.543750339501001712 ) ) ;
#65334 = CARTESIAN_POINT ( 'NONE',  ( 11.15810538575740019, 5.242981041160000188, 7.797177576385699638 ) ) ;
#65335 = ORIENTED_EDGE ( 'NONE', *, *, #62988, .T. ) ;
#65336 = CARTESIAN_POINT ( 'NONE',  ( 9.120514158775000269, 5.306366356490000769, -7.996450761531000317 ) ) ;
#65337 = DIRECTION ( 'NONE',  ( 1.000000000000000000, 0.000000000000000000, 0.000000000000000000 ) ) ;
#65338 = CARTESIAN_POINT ( 'NONE',  ( 12.11828080172247724, 2.711598415135494378, -12.30476978351483375 ) ) ;
#65339 = CARTESIAN_POINT ( 'NONE',  ( 11.39835090130999973, -3.121033016283800254, 6.956352367771000189 ) ) ;
#65340 = ADVANCED_FACE ( 'NONE', ( #66754 ), #51364, .F. ) ;
#65342 = CARTESIAN_POINT ( 'NONE',  ( 9.294016886149316647, 2.684778767696973212, -7.853313980369418523 ) ) ;
#65341 = B_SPLINE_CURVE_WITH_KNOTS ( 'NONE', 3,
 ( #9003, #19846, #29672, #18824 ),
 .UNSPECIFIED., .F., .F.,
 ( 4, 4 ),
 ( 0.000000000000000000, 0.1253320266324779719 ),
 .UNSPECIFIED. ) ;
#65343 = CARTESIAN_POINT ( 'NONE',  ( 10.90000053908999966, 9.856474340180000127, -5.627824942316999923 ) ) ;
#65344 = VERTEX_POINT ( 'NONE', #3124 ) ;
#65345 = CARTESIAN_POINT ( 'NONE',  ( 23.89320776801300283, 10.75689324692999804, 4.023240149044999825 ) ) ;
#65346 = CARTESIAN_POINT ( 'NONE',  ( 23.56664318980499928, 10.37807351222000030, 9.381504534996999212 ) ) ;
#65347 = ORIENTED_EDGE ( 'NONE', *, *, #64483, .F. ) ;
#65348 = CARTESIAN_POINT ( 'NONE',  ( 12.63902032760546668, -3.180686373181428106, -12.19193352998605029 ) ) ;
#65350 = CARTESIAN_POINT ( 'NONE',  ( 10.91610672858429965, 3.088399709291500095, 8.185766014210599906 ) ) ;
#65349 = CIRCLE ( 'NONE', #47554, 1.000000000000000666 ) ;
#65351 = CARTESIAN_POINT ( 'NONE',  ( 11.17788601987000163, -2.412142864687000010, -7.075602314719000141 ) ) ;
#65352 = CARTESIAN_POINT ( 'NONE',  ( 11.05576032679999976, 2.800783223368999764, -4.875271127325000009 ) ) ;
#65353 = LINE ( 'NONE', #38797, #60572 ) ;
#65354 = CARTESIAN_POINT ( 'NONE',  ( 8.731616107288068918, 4.000002263255225898, 6.618420992905501343 ) ) ;
#65355 = CARTESIAN_POINT ( 'NONE',  ( 13.59022209853100094, 9.429754002912000388, 8.017367994085999428 ) ) ;
#65356 = CARTESIAN_POINT ( 'NONE',  ( 18.10875687686965563, -0.2899325138666228319, -12.69554708236672980 ) ) ;
#65357 = CARTESIAN_POINT ( 'NONE',  ( 12.21825390184417159, 2.283832253973942183, -12.49935200980489114 ) ) ;
#65358 = CARTESIAN_POINT ( 'NONE',  ( 10.34995525820099971, -4.107710726525199973, -6.364355462479999836 ) ) ;
#65359 = CARTESIAN_POINT ( 'NONE',  ( 7.454676658771000497, 2.138190256467000339, 6.814770510101999967 ) ) ;
#65360 = ORIENTED_EDGE ( 'NONE', *, *, #37605, .F. ) ;
#65361 = EDGE_CURVE ( 'NONE', #43628, #15277, #66489, .T. ) ;
#65362 = CARTESIAN_POINT ( 'NONE',  ( 11.59999999999999787, -4.198022108741683134, -8.571335789050445797 ) ) ;
#65363 = CARTESIAN_POINT ( 'NONE',  ( 4.500000000000000000, 3.200000000000000178, 0.000000000000000000 ) ) ;
#65364 = CARTESIAN_POINT ( 'NONE',  ( 11.53681706333000179, 12.46890164658000089, 1.535189833763999978 ) ) ;
#65365 = EDGE_CURVE ( 'NONE', #31118, #22245, #21628, .T. ) ;
#65366 = CARTESIAN_POINT ( 'NONE',  ( 18.04847759739541857, 3.007479059277873734, 12.23581163759356194 ) ) ;
#65367 = CARTESIAN_POINT ( 'NONE',  ( 13.49980696793000057, -9.514462421839999351, -7.834836582454001608 ) ) ;
#65368 = CARTESIAN_POINT ( 'NONE',  ( 11.05336220499919797, 3.034597079077000270, -7.825000000000000178 ) ) ;
#65369 = CARTESIAN_POINT ( 'NONE',  ( 9.726900131858625898, -4.185762427694958987, 6.645000240129933289 ) ) ;
#65370 = CARTESIAN_POINT ( 'NONE',  ( 12.43982406840033050, 0.6284010951863483463, -12.58437167746805940 ) ) ;
#65371 = VERTEX_POINT ( 'NONE', #56269 ) ;
#65372 = CARTESIAN_POINT ( 'NONE',  ( 12.09524978539964479, -2.332501710336877920, 12.38222815831571566 ) ) ;
#65373 = CARTESIAN_POINT ( 'NONE',  ( 9.657025935145998830, -4.165792341207500193, -6.370288821165999593 ) ) ;
#65374 = CARTESIAN_POINT ( 'NONE',  ( 24.70869262301700076, -3.610540981815000272, -12.15034266584999934 ) ) ;
#65375 = FACE_OUTER_BOUND ( 'NONE', #53810, .T. ) ;
#65376 = B_SPLINE_SURFACE_WITH_KNOTS ( 'NONE', 3, 3, ( 
 ( #5383, #7027, #54581, #60514 ),
 ( #23103, #65750, #12281, #1440 ),
 ( #6676, #61210, #39539, #42790 ),
 ( #44104, #11922, #33263, #66096 ),
 ( #17162, #45132, #28712, #12978 ),
 ( #18563, #13327, #38495, #28362 ),
 ( #39890, #17522, #34651, #59818 ),
 ( #26722, #140, #64100, #50029 ),
 ( #65403, #60175, #49678, #33607 ),
 ( #1787, #60861, #17874, #39191 ) ),
 .UNSPECIFIED., .F., .F., .F.,
 ( 4, 1, 1, 1, 1, 1, 1, 4 ),
 ( 4, 4 ),
 ( 0.07203983506772999867, 0.1428571428570999946, 0.2857142857143000203, 0.4285714285713999594, 0.5714285714286000406, 0.7142857142856999797, 0.8571428571429000609, 0.9589780836993999635 ),
 ( -0.1900620218102000158, 1.190128522698000069 ),
 .UNSPECIFIED. ) ;
#65377 = CARTESIAN_POINT ( 'NONE',  ( 11.43302763632549990, 2.964209339073000216, -7.022058766158599141 ) ) ;
#65378 = CARTESIAN_POINT ( 'NONE',  ( 12.09634453438821566, 0.1521017209118858404, 12.59908727444664045 ) ) ;
#65379 = VECTOR ( 'NONE', #35401, 1000.000000000000000 ) ;
#65380 = CARTESIAN_POINT ( 'NONE',  ( 9.331135841230999262, 4.141907758973999876, 6.047574021139999978 ) ) ;
#65381 = CARTESIAN_POINT ( 'NONE',  ( 9.657553581808000942, 5.333455947841000189, 6.049916795084000043 ) ) ;
#65382 = CARTESIAN_POINT ( 'NONE',  ( 12.44743307598044879, 3.012678875451596738, 12.31720924913609849 ) ) ;
#65383 = ORIENTED_EDGE ( 'NONE', *, *, #40361, .F. ) ;
#65384 = FACE_OUTER_BOUND ( 'NONE', #22125, .T. ) ;
#65385 = CARTESIAN_POINT ( 'NONE',  ( 10.44841638348500013, 2.891666689023999925, -7.230023356477299323 ) ) ;
#65386 = DIRECTION ( 'NONE',  ( 0.000000000000000000, -0.3380467785883188858, -0.9411293085894520960 ) ) ;
#65388 = CARTESIAN_POINT ( 'NONE',  ( 25.26126930374652346, 11.18199973298772498, 3.383911755808009403 ) ) ;
#65387 = CARTESIAN_POINT ( 'NONE',  ( 8.166615904750996080, 4.665939084510003276, 6.165875187757999143 ) ) ;
#65389 = CARTESIAN_POINT ( 'NONE',  ( 10.45672469555900008, -3.566534988568399900, -6.750062220519700062 ) ) ;
#65390 = CARTESIAN_POINT ( 'NONE',  ( 16.40000000000000213, -14.76315775485999993, -50.50083396221000243 ) ) ;
#65391 = ORIENTED_EDGE ( 'NONE', *, *, #34745, .T. ) ;
#65392 = AXIS2_PLACEMENT_3D ( 'NONE', #56737, #51143, #29141 ) ;
#65393 = B_SPLINE_CURVE_WITH_KNOTS ( 'NONE', 3,
 ( #10677, #6114, #49116, #32025, #11362, #32366, #38984, #65536, #5440, #48089, #193, #5773, #21510, #42843 ),
 .UNSPECIFIED., .F., .F.,
 ( 4, 2, 2, 2, 2, 2, 4 ),
 ( 0.000000000000000000, 0.1249999999999986955, 0.2499999999999973910, 0.4999999999999992228, 0.6249999999999998890, 0.7500000000000005551, 1.000000000000000000 ),
 .UNSPECIFIED. ) ;
#65394 = CARTESIAN_POINT ( 'NONE',  ( 2.025476376744999918, -3.125150066150999884, -0.9245224406458000255 ) ) ;
#65395 = DIRECTION ( 'NONE',  ( -1.000000000000000000, 0.000000000000000000, 0.000000000000000000 ) ) ;
#65396 = CIRCLE ( 'NONE', #8471, 1.500000000000000000 ) ;
#65397 = CARTESIAN_POINT ( 'NONE',  ( 12.74229120054538811, -12.11986439831272655, 3.159827838237132092 ) ) ;
#65398 = CARTESIAN_POINT ( 'NONE',  ( 9.095759580228998331, 3.156743194445300382, 7.701558687214699717 ) ) ;
#65399 = CARTESIAN_POINT ( 'NONE',  ( 11.07273594314529142, -2.871094011463778184, -7.175020482857276782 ) ) ;
#65400 = CARTESIAN_POINT ( 'NONE',  ( 12.68500746440623317, -1.797494983113976152, 13.88412888179957427 ) ) ;
#65401 = CARTESIAN_POINT ( 'NONE',  ( 11.05568736508000072, 2.800099964430999844, 4.877315660663000152 ) ) ;
#65402 = CARTESIAN_POINT ( 'NONE',  ( 12.80505043854143388, 1.787797342887042840, 13.88538010501570774 ) ) ;
#65403 = CARTESIAN_POINT ( 'NONE',  ( 13.73936233968600185, -12.30487262812000004, -2.534071019599000163 ) ) ;
#65404 = ORIENTED_EDGE ( 'NONE', *, *, #41655, .T. ) ;
#65405 = CARTESIAN_POINT ( 'NONE',  ( 7.562916666663876519, 5.079550237237543620, -6.670361928033864629 ) ) ;
#65406 = DIRECTION ( 'NONE',  ( 1.000000000000000000, 0.000000000000000000, 0.000000000000000000 ) ) ;
#65407 = CARTESIAN_POINT ( 'NONE',  ( 11.30361999289329944, -4.544092497359196514, -6.342116603374310380 ) ) ;
#65408 = DIRECTION ( 'NONE',  ( 0.9999999999889699343, -2.769066800191914947E-06, -3.793722030192884931E-06 ) ) ;
#65409 = CARTESIAN_POINT ( 'NONE',  ( 20.10000000000000142, 0.000000000000000000, 0.000000000000000000 ) ) ;
#65410 = CARTESIAN_POINT ( 'NONE',  ( 1.980140132539667253, 3.408904368339106927, -0.9161175952574746040 ) ) ;
#65411 = CARTESIAN_POINT ( 'NONE',  ( 25.60000000000000142, -2.023988666086999899, -11.01546541709000060 ) ) ;
#65412 = CARTESIAN_POINT ( 'NONE',  ( 9.736878146978000359, 2.742182981761000171, 6.839230404018000087 ) ) ;
#65413 = CARTESIAN_POINT ( 'NONE',  ( 11.26902897915239876, 4.221721321201099997, 6.662660017635100296 ) ) ;
#65414 = B_SPLINE_CURVE_WITH_KNOTS ( 'NONE', 3,
 ( #44957, #18382, #60336, #34809 ),
 .UNSPECIFIED., .F., .F.,
 ( 4, 4 ),
 ( 0.000000000000000000, 1.000000000000000000 ),
 .UNSPECIFIED. ) ;
#65415 = CARTESIAN_POINT ( 'NONE',  ( 27.64127793187000037, 2.399999999999999911, 6.571291218949999902 ) ) ;
#65416 = CARTESIAN_POINT ( 'NONE',  ( 10.78888064679000003, -2.675723359162999859, -6.748225798259000818 ) ) ;
#65417 = CARTESIAN_POINT ( 'NONE',  ( 4.646693173015832734, -1.310679582531386611, -0.7554284705563495406 ) ) ;
#65418 = CARTESIAN_POINT ( 'NONE',  ( 24.35146665670700017, 12.30647607894000117, 3.205652257177999953 ) ) ;
#65419 = ADVANCED_FACE ( 'NONE', ( #19894 ), #58468, .F. ) ;
#65420 = CARTESIAN_POINT ( 'NONE',  ( 12.21329150903074101, -2.701250043963952852, 12.40242623241618958 ) ) ;
#65421 = ADVANCED_FACE ( 'NONE', ( #45780 ), #9386, .F. ) ;
#65422 = ORIENTED_EDGE ( 'NONE', *, *, #24808, .T. ) ;
#65423 = CARTESIAN_POINT ( 'NONE',  ( 8.397785841227999981, 5.616457598545999907, -8.245813000738998255 ) ) ;
#65424 = ORIENTED_EDGE ( 'NONE', *, *, #62427, .F. ) ;
#65425 = CARTESIAN_POINT ( 'NONE',  ( 18.17249645628719534, -2.401006805677767808, 13.69397427989632909 ) ) ;
#65426 = CARTESIAN_POINT ( 'NONE',  ( 10.78887616594230003, -4.386455737425299262, -6.281817606595999415 ) ) ;
#65427 = ORIENTED_EDGE ( 'NONE', *, *, #50757, .F. ) ;
#65428 = CARTESIAN_POINT ( 'NONE',  ( 10.72702344389999851, 2.995605560827999891, 8.109550315577399360 ) ) ;
#65429 = CARTESIAN_POINT ( 'NONE',  ( 6.358516356071935327, -1.061705381105392032, -0.3968015536708104918 ) ) ;
#65430 = CARTESIAN_POINT ( 'NONE',  ( 23.75089607250696133, 3.269771166517764449, -13.22954999995908487 ) ) ;
#65431 = VECTOR ( 'NONE', #54237, 1000.000000000000000 ) ;
#65432 = CARTESIAN_POINT ( 'NONE',  ( 9.905792474809000936, 2.698958900805999761, 8.979236532123000103 ) ) ;
#65433 = CARTESIAN_POINT ( 'NONE',  ( 24.30000000000000071, -8.810505093353000916, -8.810505093353000916 ) ) ;
#65434 = CARTESIAN_POINT ( 'NONE',  ( 17.33333333119166753, -3.345268056437868953, -11.86064107241928234 ) ) ;
#65435 = CARTESIAN_POINT ( 'NONE',  ( 11.64596081258699911, 3.342173145742999729, -11.21570452027999920 ) ) ;
#65436 = CARTESIAN_POINT ( 'NONE',  ( 11.03407957707000087, -2.992853177526999975, -9.056567163506000995 ) ) ;
#65437 = CARTESIAN_POINT ( 'NONE',  ( 25.49994615399570819, -8.603880941064405263, -7.325437794649179324 ) ) ;
#65438 = EDGE_LOOP ( 'NONE', ( #48808, #29534, #62471, #67037, #13859 ) ) ;
#65439 = CARTESIAN_POINT ( 'NONE',  ( 10.57286587299508440, -3.010279057788120660, -5.022110908762327242 ) ) ;
#65440 = EDGE_LOOP ( 'NONE', ( #67388, #54776, #68761, #48173 ) ) ;
#65441 = VECTOR ( 'NONE', #23797, 1000.000000000000000 ) ;
#65442 = CARTESIAN_POINT ( 'NONE',  ( 0.7431103717477000048, 2.848815883361000001, -1.248255999701999963 ) ) ;
#65443 = B_SPLINE_CURVE_WITH_KNOTS ( 'NONE', 3,
 ( #34579, #23034, #17804, #58285, #42221, #19856, #41185, #26134, #30357, #52001, #51665, #3760, #46085, #3424, #20885, #30692, #35935, #40834 ),
 .UNSPECIFIED., .F., .F.,
 ( 4, 2, 2, 2, 2, 2, 2, 2, 4 ),
 ( 0.000000000000000000, 0.1250000000000000000, 0.2500000000000000000, 0.3750000000000000000, 0.5000000000000000000, 0.6250000000000000000, 0.7500000000000000000, 0.8750000000000000000, 1.000000000000000000 ),
 .UNSPECIFIED. ) ;
#65444 = ORIENTED_EDGE ( 'NONE', *, *, #4916, .T. ) ;
#65445 = CARTESIAN_POINT ( 'NONE',  ( 17.60412247569231425, -3.248108758003541485, -13.61799506159942474 ) ) ;
#65446 = CARTESIAN_POINT ( 'NONE',  ( 10.95390526108000095, -5.337639433354000040, 4.888929981400999658 ) ) ;
#65447 = ADVANCED_FACE ( 'NONE', ( #13969 ), #10905, .F. ) ;
#65448 = CARTESIAN_POINT ( 'NONE',  ( 10.53855965315437082, -2.999267221421852980, 5.023112174284990239 ) ) ;
#65449 = FACE_OUTER_BOUND ( 'NONE', #49603, .T. ) ;
#65450 = CARTESIAN_POINT ( 'NONE',  ( 12.66207816929884444, 1.891226320509242553, 13.78383611977690570 ) ) ;
#65451 = CARTESIAN_POINT ( 'NONE',  ( 10.05691733561000056, -2.453480799114999833, 6.657106310117000270 ) ) ;
#65452 = CARTESIAN_POINT ( 'NONE',  ( 11.12299956498149811, 5.207010770456999893, -7.825000000000000178 ) ) ;
#65453 = CARTESIAN_POINT ( 'NONE',  ( 12.25919481816070267, 0.4811670829680709249, 13.99174107639406017 ) ) ;
#65454 = ORIENTED_EDGE ( 'NONE', *, *, #39309, .F. ) ;
#65455 = CARTESIAN_POINT ( 'NONE',  ( 12.82764013820600013, 11.38891548326999903, -4.574441164091999745 ) ) ;
#65456 = CARTESIAN_POINT ( 'NONE',  ( 9.457462135716001583, 5.100000000000000533, -6.571291218949999902 ) ) ;
#65457 = CARTESIAN_POINT ( 'NONE',  ( 23.55651145941100211, -3.262678050158999810, -13.70323023102000093 ) ) ;
#65458 = CARTESIAN_POINT ( 'NONE',  ( 4.955958905525999825, 1.069320748165000001, -0.7985724841332999535 ) ) ;
#65459 = CARTESIAN_POINT ( 'NONE',  ( 8.491329719591000469, 4.851303550474000303, -9.008742670124000540 ) ) ;
#65460 = DIRECTION ( 'NONE',  ( 0.000000000000000000, 1.000000000000000000, 0.000000000000000000 ) ) ;
#65461 = CARTESIAN_POINT ( 'NONE',  ( 10.91623602276999883, -5.459825388708999583, -8.642870457474998602 ) ) ;
#65462 = FACE_OUTER_BOUND ( 'NONE', #53917, .T. ) ;
#65463 = CARTESIAN_POINT ( 'NONE',  ( 23.73952225791441606, 3.508702178794984139, 13.37374633488916054 ) ) ;
#65464 = DIRECTION ( 'NONE',  ( -4.468462273946190507E-09, 0.2714605545367115846, -0.9624495661231402543 ) ) ;
#65465 = FACE_OUTER_BOUND ( 'NONE', #19392, .T. ) ;
#65466 = CARTESIAN_POINT ( 'NONE',  ( 8.548990840217488341, -3.103435619188711136, 6.042760497454945146 ) ) ;
#65467 = DIRECTION ( 'NONE',  ( 0.000000000000000000, -1.000000000000000000, 0.000000000000000000 ) ) ;
#65468 = CARTESIAN_POINT ( 'NONE',  ( 10.37199293566600034, 4.633387186021100668, -8.276990458557699881 ) ) ;
#65469 = CARTESIAN_POINT ( 'NONE',  ( 8.722809814040999754, 4.614409247670200109, -8.294571108394100278 ) ) ;
#65471 = DIRECTION ( 'NONE',  ( -0.7071101187282218259, 0.000000000000000000, -0.7071034436291199210 ) ) ;
#65470 = CARTESIAN_POINT ( 'NONE',  ( 9.773063610504999943, -3.644370728184199937, 6.709281487801199262 ) ) ;
#65472 = CARTESIAN_POINT ( 'NONE',  ( 11.28976354018297634, -4.327184855449096368, 8.717465845835395299 ) ) ;
#65473 = EDGE_LOOP ( 'NONE', ( #18564, #67734, #33754, #60457, #47293 ) ) ;
#65474 = AXIS2_PLACEMENT_3D ( 'NONE', #39741, #19090, #66291 ) ;
#65475 = CARTESIAN_POINT ( 'NONE',  ( 10.48280513895999988, 4.903310631086600146, 8.002155910165599906 ) ) ;
#65476 = AXIS2_PLACEMENT_3D ( 'NONE', #13447, #50490, #55745 ) ;
#65477 = CARTESIAN_POINT ( 'NONE',  ( 7.411085905969002852, -3.233236485764999113, 6.481842843012996624 ) ) ;
#65478 = EDGE_CURVE ( 'NONE', #66938, #27264, #50650, .T. ) ;
#65479 = CARTESIAN_POINT ( 'NONE',  ( 9.101797255588000013, 5.278067516796999925, 7.554109351283189611 ) ) ;
#65480 = CARTESIAN_POINT ( 'NONE',  ( 9.784141369869628235, 4.423591863150092784, -8.265573120213877800 ) ) ;
#65481 = CARTESIAN_POINT ( 'NONE',  ( 10.22109127278999807, -2.983266195621000261, 8.764707262515999631 ) ) ;
#65482 = CARTESIAN_POINT ( 'NONE',  ( 10.00371413511149932, -2.641056634684001203, 6.398884489502225215 ) ) ;
#65483 = CARTESIAN_POINT ( 'NONE',  ( 11.83124374198900064, 3.528976724670999765, -11.96046730081999954 ) ) ;
#65484 = VERTEX_POINT ( 'NONE', #69156 ) ;
#65485 = CARTESIAN_POINT ( 'NONE',  ( 8.950772138681999834, -4.373757805842100055, -6.567719246739500250 ) ) ;
#65486 = AXIS2_PLACEMENT_3D ( 'NONE', #15964, #931, #59651 ) ;
#65487 = CARTESIAN_POINT ( 'NONE',  ( 8.765417767663000959, 5.029951493281999753, -6.097931603992000404 ) ) ;
#65488 = CARTESIAN_POINT ( 'NONE',  ( 6.074764545683000172, -1.539848055637000002, 0.4860074956841999860 ) ) ;
#65489 = CYLINDRICAL_SURFACE ( 'NONE', #17599, 1.250000000000000222 ) ;
#65490 = CARTESIAN_POINT ( 'NONE',  ( 25.30000327618300204, 8.756202924575998026, 7.455126447192999883 ) ) ;
#65491 = CARTESIAN_POINT ( 'NONE',  ( 11.79364426047339975, -3.533902447304699823, 6.769896129503799820 ) ) ;
#65492 = CARTESIAN_POINT ( 'NONE',  ( 10.60441638348510018, 3.158410350011299883, -7.294998899090099798 ) ) ;
#65493 = CARTESIAN_POINT ( 'NONE',  ( 13.99999999231800096, 8.833253877201999060, 7.896562762484000686 ) ) ;
#65494 = CARTESIAN_POINT ( 'NONE',  ( 25.08240868301900406, -8.543484405703001272, 8.158957461736999761 ) ) ;
#65495 = CARTESIAN_POINT ( 'NONE',  ( 5.700000000000000178, -11.06886219213000011, -1.536526853569999851 ) ) ;
#65496 = ORIENTED_EDGE ( 'NONE', *, *, #29374, .T. ) ;
#65497 = CYLINDRICAL_SURFACE ( 'NONE', #7609, 2.149999999999999911 ) ;
#65498 = CARTESIAN_POINT ( 'NONE',  ( 12.66324396017929388, 0.6090406077983142596, -13.88203505342130661 ) ) ;
#65499 = FACE_OUTER_BOUND ( 'NONE', #11943, .T. ) ;
#65500 = ADVANCED_FACE ( 'NONE', ( #5866 ), #58884, .F. ) ;
#65501 = CARTESIAN_POINT ( 'NONE',  ( 24.87966566241900068, -8.586230768662000301, -8.375222081007999364 ) ) ;
#65502 = CARTESIAN_POINT ( 'NONE',  ( 10.43559687351661758, -5.092232985442824322, -8.129523725463622341 ) ) ;
#65503 = CARTESIAN_POINT ( 'NONE',  ( 7.000000000000000000, 10.13680670596995625, 4.410575858471027288 ) ) ;
#65504 = DIRECTION ( 'NONE',  ( 0.8660254037844968833, -2.665883466949989686E-12, -0.4999999999998989142 ) ) ;
#65505 = EDGE_LOOP ( 'NONE', ( #12151, #51357, #52435, #68391 ) ) ;
#65506 = EDGE_CURVE ( 'NONE', #52017, #34080, #28948, .T. ) ;
#65507 = SURFACE_SIDE_STYLE ('',( #39644 ) ) ;
#65508 = CARTESIAN_POINT ( 'NONE',  ( 18.14140153244917286, 2.282676164818131515, -13.71717056020690606 ) ) ;
#65509 = EDGE_LOOP ( 'NONE', ( #15589, #32713, #40740, #17957, #5336, #29088 ) ) ;
#65510 = DIRECTION ( 'NONE',  ( 0.000000000000000000, 1.000000000000000000, 0.000000000000000000 ) ) ;
#65511 = CARTESIAN_POINT ( 'NONE',  ( 17.92913687483822116, 3.216295279492294767, 11.40344415251901644 ) ) ;
#65512 = CARTESIAN_POINT ( 'NONE',  ( 15.46873602477000276, 8.828190495471000432, 7.821444125541998638 ) ) ;
#65513 = CARTESIAN_POINT ( 'NONE',  ( 11.10000000000000142, -2.495605073370282145, -8.212123196678321690 ) ) ;
#65514 = CARTESIAN_POINT ( 'NONE',  ( 10.51414141025500015, -3.384226587288500010, -8.596754040696000132 ) ) ;
#65515 = CARTESIAN_POINT ( 'NONE',  ( 17.89454609197015600, 0.5248351044407618682, -12.68540052859646217 ) ) ;
#65516 = CARTESIAN_POINT ( 'NONE',  ( 10.98333333333533091, -4.339018939180776080, 8.912414555067401878 ) ) ;
#65517 = ORIENTED_EDGE ( 'NONE', *, *, #1760, .T. ) ;
#65518 = CARTESIAN_POINT ( 'NONE',  ( 10.96580795178999956, -4.930647899304999804, 6.170539049947000088 ) ) ;
#65519 = CARTESIAN_POINT ( 'NONE',  ( 18.17514039570439977, -2.578830837888117067, -13.65637626283699113 ) ) ;
#65520 = CARTESIAN_POINT ( 'NONE',  ( 9.892489158770999325, 5.099602161831000124, -9.049221499261999924 ) ) ;
#65521 = ORIENTED_EDGE ( 'NONE', *, *, #11044, .F. ) ;
#65522 = AXIS2_PLACEMENT_3D ( 'NONE', #30146, #2866, #13377 ) ;
#65523 = CARTESIAN_POINT ( 'NONE',  ( 11.01002959534999981, 3.180718072098000171, -6.283812549199000230 ) ) ;
#65524 = CARTESIAN_POINT ( 'NONE',  ( 11.29595444038000096, -2.828863075736999910, -8.191124550002999882 ) ) ;
#65525 = VERTEX_POINT ( 'NONE', #17044 ) ;
#65526 = CARTESIAN_POINT ( 'NONE',  ( 9.659988259785999176, 3.868581654116200141, 6.504223158184999853 ) ) ;
#65527 = CARTESIAN_POINT ( 'NONE',  ( 18.15405049586277997, -2.074720874654904623, -12.42801810613654823 ) ) ;
#65528 = EDGE_CURVE ( 'NONE', #7896, #4640, #52239, .T. ) ;
#65529 = VECTOR ( 'NONE', #42055, 1000.000000000000000 ) ;
#65530 = CARTESIAN_POINT ( 'NONE',  ( 10.99143984058726353, 6.551946267843069549, -5.305482051232298879 ) ) ;
#65531 = DIRECTION ( 'NONE',  ( 0.000000000000000000, 0.9421243786071880066, -0.3352635608502960163 ) ) ;
#65532 = CARTESIAN_POINT ( 'NONE',  ( 11.74267124137200113, -11.57041781403000158, -1.757356211607000063 ) ) ;
#65533 = B_SPLINE_CURVE_WITH_KNOTS ( 'NONE', 3,
 ( #11584, #37140, #64373, #42728, #48661, #22772 ),
 .UNSPECIFIED., .F., .F.,
 ( 4, 2, 4 ),
 ( 0.000000000000000000, 0.5000000000000000000, 1.000000000000000000 ),
 .UNSPECIFIED. ) ;
#65534 = VECTOR ( 'NONE', #64109, 1000.000000000000114 ) ;
#65535 = CARTESIAN_POINT ( 'NONE',  ( 9.788646554150998824, 4.419749732651400365, 6.741370903243699253 ) ) ;
#65536 = CARTESIAN_POINT ( 'NONE',  ( 13.52727141073796169, -12.35275327559112490, -2.070326479556442667 ) ) ;
#65537 = ORIENTED_EDGE ( 'NONE', *, *, #49559, .T. ) ;
#65538 = CARTESIAN_POINT ( 'NONE',  ( 10.74599736040000053, 5.242718773683000322, 8.978699897073999736 ) ) ;
#65539 = CARTESIAN_POINT ( 'NONE',  ( 10.14522028041000112, 3.576529456695000331, -8.962721799438000403 ) ) ;
#65540 = DIRECTION ( 'NONE',  ( -1.000000000000000000, 0.000000000000000000, 0.000000000000000000 ) ) ;
#65541 = VECTOR ( 'NONE', #29231, 1000.000000000000000 ) ;
#65542 = CARTESIAN_POINT ( 'NONE',  ( 12.21305109721488869, 2.701423549395648216, -13.62869161905334359 ) ) ;
#65543 = CARTESIAN_POINT ( 'NONE',  ( 11.26059687351620298, -4.629523725463621453, 8.592232985442825210 ) ) ;
#65544 = CARTESIAN_POINT ( 'NONE',  ( 9.533427734455999669, -2.564762519363000148, 6.150594768287000136 ) ) ;
#65545 = CARTESIAN_POINT ( 'NONE',  ( 17.91054527438922861, 0.5141525164327357400, 13.88720023103246248 ) ) ;
#65546 = CARTESIAN_POINT ( 'NONE',  ( 17.94896392900171733, 0.4852513397891488056, 13.88859817538062558 ) ) ;
#65547 = B_SPLINE_CURVE_WITH_KNOTS ( 'NONE', 3,
 ( #31414, #26168, #37340, #25817 ),
 .UNSPECIFIED., .F., .F.,
 ( 4, 4 ),
 ( 0.000000000000000000, 1.000000000000000000 ),
 .UNSPECIFIED. ) ;
#65548 = VERTEX_POINT ( 'NONE', #54458 ) ;
#65549 = EDGE_LOOP ( 'NONE', ( #24316, #55059, #17758, #56050, #7998, #24223, #63812, #16235, #68333 ) ) ;
#65550 = VECTOR ( 'NONE', #59770, 1000.000000000000000 ) ;
#65551 = CARTESIAN_POINT ( 'NONE',  ( 9.635004719593998956, 2.334550724494000029, -7.977056617806000283 ) ) ;
#65552 = CARTESIAN_POINT ( 'NONE',  ( 12.19590749973210286, -0.1412517843910542081, 13.89905214520371679 ) ) ;
#65553 = CARTESIAN_POINT ( 'NONE',  ( 12.24303834290234505, -0.2736100115472018257, -13.89637849652428514 ) ) ;
#65554 = CARTESIAN_POINT ( 'NONE',  ( 10.00638553269999953, -5.119272496996000399, 8.420388242270998802 ) ) ;
#65555 = DIRECTION ( 'NONE',  ( 1.000000000000000000, 0.000000000000000000, 0.000000000000000000 ) ) ;
#65556 = LINE ( 'NONE', #6481, #29929 ) ;
#65557 = CARTESIAN_POINT ( 'NONE',  ( 5.699999999836000697, -1.433333331105999919, -10.65401593570999950 ) ) ;
#65559 = CARTESIAN_POINT ( 'NONE',  ( 5.200000000000000178, 0.000000000000000000, 0.000000000000000000 ) ) ;
#65558 = CARTESIAN_POINT ( 'NONE',  ( 10.36167167105699960, -5.261543809652999393, 7.288123611975898974 ) ) ;
#65560 = CARTESIAN_POINT ( 'NONE',  ( 8.663116700034002804, -5.178392435731003829, -6.846672731545002222 ) ) ;
#65561 = DIRECTION ( 'NONE',  ( 0.000000000000000000, 1.000000000000000000, 0.000000000000000000 ) ) ;
#65562 = CARTESIAN_POINT ( 'NONE',  ( 6.999999691988000095, 1.243449787579999883E-13, -1.714942017578999994E-13 ) ) ;
#65563 = ADVANCED_FACE ( 'NONE', ( #11803 ), #61817, .F. ) ;
#65564 = EDGE_CURVE ( 'NONE', #49507, #65786, #12852, .T. ) ;
#65565 = CARTESIAN_POINT ( 'NONE',  ( 17.75635104740699077, 0.5917829749564882391, 12.68143435689271037 ) ) ;
#65566 = DIRECTION ( 'NONE',  ( -1.000000000000000000, 0.000000000000000000, 0.000000000000000000 ) ) ;
#65567 = CARTESIAN_POINT ( 'NONE',  ( 4.149992563291998948, 1.747525841223984910, 1.007210908820209916 ) ) ;
#65568 = ORIENTED_EDGE ( 'NONE', *, *, #5998, .T. ) ;
#65570 = CARTESIAN_POINT ( 'NONE',  ( 9.615109647822677630, 5.349900357012234764, -7.499993490198826329 ) ) ;
#65569 = CARTESIAN_POINT ( 'NONE',  ( 11.64955063476181429, -3.023401864784705850, 8.326430086672806041 ) ) ;
#65571 = CARTESIAN_POINT ( 'NONE',  ( 9.351420280414000530, 4.953415418491999844, -8.946479654552000227 ) ) ;
#65572 = EDGE_CURVE ( 'NONE', #46074, #37636, #6559, .T. ) ;
#65573 = CARTESIAN_POINT ( 'NONE',  ( 12.60210251410538618, -1.908512130997220835, 13.78126077419328510 ) ) ;
#65574 = CARTESIAN_POINT ( 'NONE',  ( 10.25036334590209464, -3.059888261081735727, -8.493457116339172330 ) ) ;
#65575 = CARTESIAN_POINT ( 'NONE',  ( 7.874998340266000874, -5.143395304206999974, 6.784086671025002069 ) ) ;
#65576 = CIRCLE ( 'NONE', #14238, 2.000000000000000888 ) ;
#65577 = CARTESIAN_POINT ( 'NONE',  ( 0.4527818351675000352, 0.6486458134353999538, 3.310649237188999727 ) ) ;
#65578 = DIRECTION ( 'NONE',  ( 0.000000000000000000, 1.000000000000000000, 0.000000000000000000 ) ) ;
#65579 = CARTESIAN_POINT ( 'NONE',  ( 2.590519314319999822, 0.2902467568208999538, -3.413293928950000389 ) ) ;
#65580 = ORIENTED_EDGE ( 'NONE', *, *, #68658, .T. ) ;
#65581 = CARTESIAN_POINT ( 'NONE',  ( 12.30074667651849474, -0.5168989769797315281, -12.58939571008426839 ) ) ;
#65582 = CARTESIAN_POINT ( 'NONE',  ( 24.52301487334444730, -12.12194136125221888, 3.142914510258483229 ) ) ;
#65583 = CARTESIAN_POINT ( 'NONE',  ( 23.60000333624175184, -13.25018707633487658, -4.190178083890355509 ) ) ;
#65584 = CARTESIAN_POINT ( 'NONE',  ( 7.127704719590999716, 4.698356649019999942, 8.789431186081998248 ) ) ;
#65585 = VERTEX_POINT ( 'NONE', #23336 ) ;
#65586 = CARTESIAN_POINT ( 'NONE',  ( 5.444320540949000531, -0.1571859003484000206, 1.535560374452000110 ) ) ;
#65587 = CARTESIAN_POINT ( 'NONE',  ( 8.037560841226000008, 5.122039080790999677, -6.666882531104000087 ) ) ;
#65589 = CARTESIAN_POINT ( 'NONE',  ( 24.57937622088081042, -8.815984698211464021, 9.246564899790328695 ) ) ;
#65588 = DIRECTION ( 'NONE',  ( 0.000000000000000000, 1.000000000000000000, 0.000000000000000000 ) ) ;
#65590 = VECTOR ( 'NONE', #4615, 1000.000000000000000 ) ;
#65591 = CARTESIAN_POINT ( 'NONE',  ( 11.01279632507519857, 4.624908853805600906, -8.658468685623999406 ) ) ;
#65592 = ORIENTED_EDGE ( 'NONE', *, *, #46405, .F. ) ;
#65593 = CARTESIAN_POINT ( 'NONE',  ( 11.09999999999999964, -2.700230688176999738, 5.136744346970999686 ) ) ;
#65594 = FILL_AREA_STYLE ('',( #1629 ) ) ;
#65595 = EDGE_LOOP ( 'NONE', ( #20294, #48391, #13766, #29101 ) ) ;
#65596 = CARTESIAN_POINT ( 'NONE',  ( 15.96683822361880090, -3.674392175451292264, -11.19597380828251687 ) ) ;
#65597 = CARTESIAN_POINT ( 'NONE',  ( 16.07059379716000080, 3.381060347337999872, 11.29912544500000138 ) ) ;
#65598 = CARTESIAN_POINT ( 'NONE',  ( 17.91891929415153228, -0.5082612142235584107, -13.88749228919889767 ) ) ;
#65599 = EDGE_LOOP ( 'NONE', ( #23073, #18807 ) ) ;
#65600 = DIRECTION ( 'NONE',  ( -0.000000000000000000, -0.000000000000000000, 1.000000000000000000 ) ) ;
#65601 = DIRECTION ( 'NONE',  ( -1.000000000000000000, 0.000000000000000000, -2.609704304917999919E-14 ) ) ;
#65602 = AXIS2_PLACEMENT_3D ( 'NONE', #18475, #13583, #50975 ) ;
#65603 = CARTESIAN_POINT ( 'NONE',  ( 7.689964158769000413, 4.459320617394000763, -8.819879155908999735 ) ) ;
#65604 = LINE ( 'NONE', #1294, #54298 ) ;
#65605 = CARTESIAN_POINT ( 'NONE',  ( 18.17230637739242383, -2.598591657424966783, 12.42808133540079574 ) ) ;
#65606 = ORIENTED_EDGE ( 'NONE', *, *, #23935, .T. ) ;
#65607 = DIRECTION ( 'NONE',  ( 0.000000000000000000, -1.000000000000000000, 0.000000000000000000 ) ) ;
#65608 = CARTESIAN_POINT ( 'NONE',  ( 24.42335427832999883, -12.73360904536999882, -3.018931263375000285 ) ) ;
#65609 = CARTESIAN_POINT ( 'NONE',  ( 15.39046541331000029, -9.526477069417000010, -8.190982836632000996 ) ) ;
#65610 = VERTEX_POINT ( 'NONE', #33490 ) ;
#65611 = CARTESIAN_POINT ( 'NONE',  ( 10.47253786429000044, -2.899999999999999911, -6.571291218949999902 ) ) ;
#65612 = ADVANCED_FACE ( 'NONE', ( #39418 ), #16492, .F. ) ;
#65613 = CARTESIAN_POINT ( 'NONE',  ( 10.60434687351569494, 5.250000000000001776, -7.336375382625535124 ) ) ;
#65614 = CARTESIAN_POINT ( 'NONE',  ( 24.67921580316900076, -12.29514843751999997, 2.979196179828000002 ) ) ;
#65615 = CARTESIAN_POINT ( 'NONE',  ( 5.000030787343001215, -0.2748844998327719669, 2.099962892531005654 ) ) ;
#65616 = CARTESIAN_POINT ( 'NONE',  ( 24.30000000000000071, 8.810505093353000916, 8.810505093353000916 ) ) ;
#65617 = CARTESIAN_POINT ( 'NONE',  ( 5.700000000000000178, 0.000000000000000000, -1.250000000000000000 ) ) ;
#65618 = AXIS2_PLACEMENT_3D ( 'NONE', #10752, #27189, #6541 ) ;
#65619 = CARTESIAN_POINT ( 'NONE',  ( 17.80580762821595897, -3.072583274995464464, 12.29955455495395888 ) ) ;
#65620 = VERTEX_POINT ( 'NONE', #46384 ) ;
#65621 =( BOUNDED_SURFACE ( )  B_SPLINE_SURFACE ( 3, 3, ( 
 ( #16734, #17435, #64965, #1701, #2389, #33523, #54842, #22671, #38411, #65667, #17079 ),
 ( #49942, #54144, #23713, #54493, #59735, #33176, #2053, #66009, #27584, #55537, #33869 ),
 ( #38764, #7634, #45048, #6594, #60089, #55184, #38063, #49244, #59388, #44015, #23020 ),
 ( #11488, #32828, #18132, #65319, #12195, #49593, #51988, #39801, #30346, #40820, #61125 ) ),
 .UNSPECIFIED., .F., .F., .T. ) 
 B_SPLINE_SURFACE_WITH_KNOTS ( ( 4, 4 ),
 ( 4, 1, 1, 1, 1, 1, 1, 1, 4 ),
 ( 0.000000000000000000, 1.000000000000000000 ),
 ( 0.8312902889582000077, 0.8338388411866000105, 0.8555869174461000481, 0.8794646334507000285, 0.9056938526918999477, 0.9344431701381999966, 0.9658387281735000274, 1.000000000000000000, 1.004668145018999814 ),
 .UNSPECIFIED. ) 
 GEOMETRIC_REPRESENTATION_ITEM ( )  RATIONAL_B_SPLINE_SURFACE ( (
 ( 1.221026506593000160, 1.221026506593000160, 1.221026506593000160, 1.221026506593000160, 1.221026506593000160, 1.221026506593000160, 1.221026506593000160, 1.221026506593000160, 1.221026506593000160, 1.221026506593000160, 1.221026506593000160),
 ( 0.9263244978021999421, 0.9263244978021999421, 0.9263244978021999421, 0.9263244978021999421, 0.9263244978021999421, 0.9263244978021999421, 0.9263244978021999421, 0.9263244978021999421, 0.9263244978021999421, 0.9263244978021999421, 0.9263244978021999421),
 ( 0.9263244978021999421, 0.9263244978021999421, 0.9263244978021999421, 0.9263244978021999421, 0.9263244978021999421, 0.9263244978021999421, 0.9263244978021999421, 0.9263244978021999421, 0.9263244978021999421, 0.9263244978021999421, 0.9263244978021999421),
 ( 1.221026506593000160, 1.221026506593000160, 1.221026506593000160, 1.221026506593000160, 1.221026506593000160, 1.221026506593000160, 1.221026506593000160, 1.221026506593000160, 1.221026506593000160, 1.221026506593000160, 1.221026506593000160) ) ) 
 REPRESENTATION_ITEM ( '' )  SURFACE ( )  );
#65622 = CARTESIAN_POINT ( 'NONE',  ( 10.68035971519489813, -3.321859513918399731, -6.371865185335000348 ) ) ;
#65623 = VERTEX_POINT ( 'NONE', #55844 ) ;
#65624 = CARTESIAN_POINT ( 'NONE',  ( 0.1499942179679999987, 2.750000000000000000, 0.000000000000000000 ) ) ;
#65625 = CARTESIAN_POINT ( 'NONE',  ( 8.848264158775000610, 5.751585344281000545, -8.235867044345999588 ) ) ;
#65626 = CARTESIAN_POINT ( 'NONE',  ( 3.006162285354999852, -1.552497165750999830, 3.001664479667999874 ) ) ;
#65627 = CARTESIAN_POINT ( 'NONE',  ( 9.898134631442999876, -2.965923230546999800, -6.610863544715000373 ) ) ;
#65628 = AXIS2_PLACEMENT_3D ( 'NONE', #51316, #52342, #62481 ) ;
#65629 = DIRECTION ( 'NONE',  ( 0.000000000000000000, -0.3258275053806940491, 0.9454292341245821296 ) ) ;
#65630 = CARTESIAN_POINT ( 'NONE',  ( 23.86797489265400074, 13.28660945761000001, 3.449435190502999848 ) ) ;
#65631 = CARTESIAN_POINT ( 'NONE',  ( 8.706426979769998908, 3.641148095589300304, -8.276078370613198842 ) ) ;
#65632 = ORIENTED_EDGE ( 'NONE', *, *, #23148, .F. ) ;
#65633 = CARTESIAN_POINT ( 'NONE',  ( 9.893930206848997599, 2.750000000000000000, 7.500000000000000000 ) ) ;
#65634 = CARTESIAN_POINT ( 'NONE',  ( 11.61718313518939993, -4.622449961306399402, 6.712912394634500401 ) ) ;
#65635 = CARTESIAN_POINT ( 'NONE',  ( 10.00138108374000012, 3.855364958793999985, 5.709478909302000638 ) ) ;
#65636 = CARTESIAN_POINT ( 'NONE',  ( 10.79212049823023278, -3.170455386494715810, -8.579526322294743323 ) ) ;
#65637 = CARTESIAN_POINT ( 'NONE',  ( 17.79999999998900151, -3.595165934733000057, 11.99793354950999991 ) ) ;
#65638 = CARTESIAN_POINT ( 'NONE',  ( 9.115731781212220497, 3.733300398746750570, 8.827344556479088666 ) ) ;
#65639 = CONICAL_SURFACE ( 'NONE', #15400, 1.699999998954999869, 0.7853981633972997312 ) ;
#65640 = CARTESIAN_POINT ( 'NONE',  ( 11.21564426047340035, 4.539962866738299851, -8.345807871442598724 ) ) ;
#65641 = CARTESIAN_POINT ( 'NONE',  ( 7.100000000000208367, 2.697694540754497883, -7.975585739598743729 ) ) ;
#65642 = CARTESIAN_POINT ( 'NONE',  ( 10.06229229006299875, 4.987433183662999703, -6.926667499798199401 ) ) ;
#65643 = EDGE_CURVE ( 'NONE', #37994, #55008, #22281, .T. ) ;
#65644 = ADVANCED_FACE ( 'NONE', ( #40785 ), #46038, .T. ) ;
#65645 = CARTESIAN_POINT ( 'NONE',  ( 24.25865867642400175, -8.929940475172999825, 8.812671217186998973 ) ) ;
#65646 = AXIS2_PLACEMENT_3D ( 'NONE', #56240, #55900, #39472 ) ;
#65647 = CARTESIAN_POINT ( 'NONE',  ( 8.114681124177748117, 5.046545375811008149, -6.488671702751082293 ) ) ;
#65648 = VERTEX_POINT ( 'NONE', #62110 ) ;
#65649 = CARTESIAN_POINT ( 'NONE',  ( 8.694605646795000808, -5.290204991635000020, 8.768102264518001121 ) ) ;
#65650 = CARTESIAN_POINT ( 'NONE',  ( 10.19691842572999896, -4.268950419651999617, -8.781589108989999559 ) ) ;
#65651 = EDGE_CURVE ( 'NONE', #29508, #39266, #9768, .T. ) ;
#65652 = EDGE_CURVE ( 'NONE', #53921, #664, #8909, .T. ) ;
#65653 = CARTESIAN_POINT ( 'NONE',  ( 17.85704948507091672, 1.853727412078925330, 13.87673533860537667 ) ) ;
#65654 = CARTESIAN_POINT ( 'NONE',  ( 23.60205915885299888, -2.489696159912998752, 12.09604418629000122 ) ) ;
#65655 = CARTESIAN_POINT ( 'NONE',  ( 10.81349144726329925, -4.738947899111299655, -6.457276458983999490 ) ) ;
#65656 = EDGE_LOOP ( 'NONE', ( #11431, #48263, #13318, #55538 ) ) ;
#65657 = CARTESIAN_POINT ( 'NONE',  ( 24.95781717674400113, 3.530132479599000117, -11.86561275887000022 ) ) ;
#65658 = CARTESIAN_POINT ( 'NONE',  ( 8.566232780412001091, 5.212261578733999201, 6.157186134061999994 ) ) ;
#65660 = CARTESIAN_POINT ( 'NONE',  ( 11.13746005378019888, 5.161099018038999731, 8.120007936598501175 ) ) ;
#65659 = CARTESIAN_POINT ( 'NONE',  ( 8.307195280408999238, 5.473983809665999622, -8.180077404516000072 ) ) ;
#65661 = CARTESIAN_POINT ( 'NONE',  ( 11.09991415876999987, 2.373387781209999936, -6.776601845694000481 ) ) ;
#65662 = ORIENTED_EDGE ( 'NONE', *, *, #27109, .T. ) ;
#65663 = CARTESIAN_POINT ( 'NONE',  ( 10.80168826891999956, 3.998196217194999846, 9.431555066626000183 ) ) ;
#65664 = CARTESIAN_POINT ( 'NONE',  ( 17.81289281796191304, -1.835117743393744671, -13.87920855489149474 ) ) ;
#65665 = CARTESIAN_POINT ( 'NONE',  ( 11.01872200990539952, 3.052519557825900343, 7.830502140005199507 ) ) ;
#65666 = CARTESIAN_POINT ( 'NONE',  ( 10.35616740164000049, -2.777283710737999733, 8.995265811011998736 ) ) ;
#65667 = CARTESIAN_POINT ( 'NONE',  ( 8.493443684196000376, 2.902502839086001263, 6.607649189245996091 ) ) ;
#65668 = ORIENTED_EDGE ( 'NONE', *, *, #27877, .F. ) ;
#65669 = CARTESIAN_POINT ( 'NONE',  ( 24.55996189763800075, 12.50738814877000138, -2.996555333880000394 ) ) ;
#65670 = EDGE_CURVE ( 'NONE', #61281, #41424, #53690, .T. ) ;
#65672 = CARTESIAN_POINT ( 'NONE',  ( 10.42511694037999881, -3.371058793856000158, -6.294333763729999198 ) ) ;
#65671 = CARTESIAN_POINT ( 'NONE',  ( 12.52995381683800247, -11.92229088141000126, 3.300664210127000064 ) ) ;
#65673 = CARTESIAN_POINT ( 'NONE',  ( 7.958764476359821316, -2.272891526873158874, 7.290622470508028030 ) ) ;
#65674 = CARTESIAN_POINT ( 'NONE',  ( 9.781666627457001439, -5.464740618746000145, 8.817321229216000589 ) ) ;
#65675 = DIRECTION ( 'NONE',  ( 0.000000000000000000, -0.8648648648648720183, 0.5020047465136825426 ) ) ;
#65676 = CARTESIAN_POINT ( 'NONE',  ( 10.10731740696899905, -3.787635830142400462, 6.378110563671000044 ) ) ;
#65677 = EDGE_LOOP ( 'NONE', ( #61988, #46930, #44315, #52190 ) ) ;
#65678 = CARTESIAN_POINT ( 'NONE',  ( 24.01967398689980371, -9.335314603828233970, 9.252502456888306526 ) ) ;
#65679 = CARTESIAN_POINT ( 'NONE',  ( 11.73195122972050086, -3.492749840905900349, 8.673036084990000560 ) ) ;
#65680 = ORIENTED_EDGE ( 'NONE', *, *, #51382, .T. ) ;
#65681 = DIRECTION ( 'NONE',  ( -1.000000000000000000, 0.000000000000000000, 0.000000000000000000 ) ) ;
#65682 = ORIENTED_EDGE ( 'NONE', *, *, #48128, .T. ) ;
#65683 = B_SPLINE_CURVE_WITH_KNOTS ( 'NONE', 3,
 ( #9818, #67854, #35712, #34436 ),
 .UNSPECIFIED., .F., .F.,
 ( 4, 4 ),
 ( 0.000000000000000000, 1.000000000000000000 ),
 .UNSPECIFIED. ) ;
#65684 = CARTESIAN_POINT ( 'NONE',  ( 8.307195280408999238, 5.473983809665999622, -8.180077404516000072 ) ) ;
#65685 = CIRCLE ( 'NONE', #2070, 1.000000000000000444 ) ;
#65686 = CARTESIAN_POINT ( 'NONE',  ( 24.08774000868300291, 12.68430291248000152, -3.366812948787999638 ) ) ;
#65687 = DIRECTION ( 'NONE',  ( 0.000000000000000000, -1.000000000000000000, 0.000000000000000000 ) ) ;
#65688 = CARTESIAN_POINT ( 'NONE',  ( 12.70853553880217568, 3.193755089013868620, -12.18851650745940240 ) ) ;
#65689 = CARTESIAN_POINT ( 'NONE',  ( 10.85814141025499957, -3.516507310755200066, 6.638851159159999682 ) ) ;
#65690 = CARTESIAN_POINT ( 'NONE',  ( 7.953777748866911246, 4.974397447652631143, -6.453194790817486926 ) ) ;
#65691 = CIRCLE ( 'NONE', #13266, 5.760713961201000544 ) ;
#65692 = ORIENTED_EDGE ( 'NONE', *, *, #16171, .T. ) ;
#65693 = CARTESIAN_POINT ( 'NONE',  ( 23.56666365135700403, 11.61524011585000160, 3.333188920242000197 ) ) ;
#65694 = CARTESIAN_POINT ( 'NONE',  ( 18.28019269455628404, -0.1906559479456389483, 14.00000681886698928 ) ) ;
#65695 = ORIENTED_EDGE ( 'NONE', *, *, #659, .F. ) ;
#65696 = CARTESIAN_POINT ( 'NONE',  ( 12.25813800312572432, -2.953224329521601188, -12.24903309118795214 ) ) ;
#65697 = CARTESIAN_POINT ( 'NONE',  ( 10.69456919669529960, 5.093991349577000172, 7.176777099639999768 ) ) ;
#65698 = EDGE_CURVE ( 'NONE', #57495, #23524, #15254, .T. ) ;
#65699 = CARTESIAN_POINT ( 'NONE',  ( 10.87274555961999845, -5.407608219159000029, -8.698392243238998844 ) ) ;
#65700 = CARTESIAN_POINT ( 'NONE',  ( 10.56271176071999918, 2.509373760909999973, -8.602415192333999983 ) ) ;
#65701 = CARTESIAN_POINT ( 'NONE',  ( 18.44490890441100106, -11.76218143194999755, 4.145213721498999249 ) ) ;
#65702 = CARTESIAN_POINT ( 'NONE',  ( 8.048510972020597620, -4.829207235971667345, 8.579008051763574727 ) ) ;
#65703 = CARTESIAN_POINT ( 'NONE',  ( 12.29585337184159499, -2.862976231886636302, -13.58970269765488403 ) ) ;
#65704 = CARTESIAN_POINT ( 'NONE',  ( 18.01167108103433279, -0.4268810874232039088, -12.69034564040270396 ) ) ;
#65705 = ADVANCED_FACE ( 'NONE', ( #41479 ), #3761, .T. ) ;
#65706 = CARTESIAN_POINT ( 'NONE',  ( 6.999998782146999332, -11.95749337870000062, 3.642574926947999892 ) ) ;
#65707 = CARTESIAN_POINT ( 'NONE',  ( 11.18687482311539938, -2.942322404451000128, -7.927326830586499007 ) ) ;
#65708 = CARTESIAN_POINT ( 'NONE',  ( 8.160739158772001289, 5.944584532500000407, 7.106843289410999631 ) ) ;
#65709 = VERTEX_POINT ( 'NONE', #10687 ) ;
#65710 = CARTESIAN_POINT ( 'NONE',  ( 11.59999999999999964, -3.075975407729480526, -8.335607184109880663 ) ) ;
#65711 = LINE ( 'NONE', #43711, #65090 ) ;
#65712 = CARTESIAN_POINT ( 'NONE',  ( 9.848259964010999568, 4.436917881843999822, 6.148031614254000132 ) ) ;
#65713 = B_SPLINE_CURVE_WITH_KNOTS ( 'NONE', 3,
 ( #50862, #25315, #20073, #13126 ),
 .UNSPECIFIED., .F., .F.,
 ( 4, 4 ),
 ( 0.000000000000000000, 1.000000000000000000 ),
 .UNSPECIFIED. ) ;
#65714 = CARTESIAN_POINT ( 'NONE',  ( 24.38582837070600107, -3.342331292268000187, 12.19039702797000047 ) ) ;
#65715 = CARTESIAN_POINT ( 'NONE',  ( 17.97018005872493518, 2.032669421145251842, 12.54824173908127527 ) ) ;
#65716 = CARTESIAN_POINT ( 'NONE',  ( 10.85685100254000091, 2.832432432432000269, -6.822293592207000934 ) ) ;
#65717 = CARTESIAN_POINT ( 'NONE',  ( 9.504903297738000134, 3.934733353759999552, 5.704831249548000471 ) ) ;
#65718 = DIRECTION ( 'NONE',  ( 2.887534672467944307E-10, -0.4812251768484908099, 0.8765970164032835799 ) ) ;
#65719 = CARTESIAN_POINT ( 'NONE',  ( 12.61731147763009631, -0.6963438834283414147, -12.58074676375338896 ) ) ;
#65720 = ORIENTED_EDGE ( 'NONE', *, *, #58395, .T. ) ;
#65721 = CARTESIAN_POINT ( 'NONE',  ( 12.11689977649202099, -2.253070615825701228, 12.39692697851452330 ) ) ;
#65722 = CARTESIAN_POINT ( 'NONE',  ( 10.18491290906799840, -4.548591194283900130, -8.171383386399000415 ) ) ;
#65723 = CARTESIAN_POINT ( 'NONE',  ( 24.51327040776200050, -3.324719603035999782, -12.06512239505999950 ) ) ;
#65724 = CARTESIAN_POINT ( 'NONE',  ( 8.392489902862999784, -5.100228725471000146, 6.589622881798000265 ) ) ;
#65725 = CARTESIAN_POINT ( 'NONE',  ( 11.08425954179440076, 4.982976321082899673, -8.316745941391600283 ) ) ;
#65726 = CARTESIAN_POINT ( 'NONE',  ( 12.08965323865565011, 0.1172743548790619733, 12.59945959730644027 ) ) ;
#65727 = CIRCLE ( 'NONE', #35604, 1.350000000000000533 ) ;
#65728 = CARTESIAN_POINT ( 'NONE',  ( 9.566490007895001924, 4.108964550738000376, 8.851615252874999840 ) ) ;
#65729 = CARTESIAN_POINT ( 'NONE',  ( 9.967852198058999136, 2.034774058634999605, 7.636878205663998997 ) ) ;
#65730 = CARTESIAN_POINT ( 'NONE',  ( 12.63789105315729877, 1.779885672808162678, 12.47365341745800471 ) ) ;
#65731 = ORIENTED_EDGE ( 'NONE', *, *, #51859, .T. ) ;
#65732 = CARTESIAN_POINT ( 'NONE',  ( 8.351014158771000950, 5.616457598545999907, -8.245813000738998255 ) ) ;
#65733 = CARTESIAN_POINT ( 'NONE',  ( 11.45348876160960039, 3.114179898019400206, -8.421216112044099589 ) ) ;
#65734 = EDGE_CURVE ( 'NONE', #7968, #56428, #24984, .T. ) ;
#65735 = EDGE_CURVE ( 'NONE', #63935, #42844, #1350, .T. ) ;
#65736 = DIRECTION ( 'NONE',  ( 1.000000000000000000, 0.000000000000000000, 0.000000000000000000 ) ) ;
#65738 = DIRECTION ( 'NONE',  ( 0.4384236320213992233, -0.6355252626312997144, -0.6355252626312997144 ) ) ;
#65737 = CARTESIAN_POINT ( 'NONE',  ( 11.64444011870698148, -3.380850026685724430, 11.14878564716274667 ) ) ;
#65739 = CARTESIAN_POINT ( 'NONE',  ( 9.351468108405999402, -3.165798890946399879, 7.263744984161399465 ) ) ;
#65740 = CARTESIAN_POINT ( 'NONE',  ( 10.67826222744820086, -4.668580868411999596, -8.050725169876500331 ) ) ;
#65741 = ORIENTED_EDGE ( 'NONE', *, *, #15421, .T. ) ;
#65742 = CARTESIAN_POINT ( 'NONE',  ( 2.068384988122999868, -3.260690222378000325, 1.050103212221999982 ) ) ;
#65743 = CARTESIAN_POINT ( 'NONE',  ( 18.29983863915590803, -0.9627071483039522093, 12.32514597438827941 ) ) ;
#65744 = CARTESIAN_POINT ( 'NONE',  ( 16.40000000000000213, 14.76315775485999993, 50.50083396221000243 ) ) ;
#65745 = CARTESIAN_POINT ( 'NONE',  ( 18.02549019388837337, -2.911978589119716077, 13.57741733930972217 ) ) ;
#65746 = CARTESIAN_POINT ( 'NONE',  ( 10.47094409420000005, 5.100000000000000533, 6.571291218949999902 ) ) ;
#65747 = CARTESIAN_POINT ( 'NONE',  ( 12.11838997910887628, -2.753273141185784478, 13.72661716423429112 ) ) ;
#65748 = DIRECTION ( 'NONE',  ( 1.000000000000000000, 0.000000000000000000, 0.000000000000000000 ) ) ;
#65749 = CARTESIAN_POINT ( 'NONE',  ( 9.424850088744616272, -5.349972419855331118, 7.500009359253513530 ) ) ;
#65750 = CARTESIAN_POINT ( 'NONE',  ( 12.99165415090800124, -12.32813973498000060, -1.877091699536999947 ) ) ;
#65751 = VERTEX_POINT ( 'NONE', #15934 ) ;
#65752 = CARTESIAN_POINT ( 'NONE',  ( 8.807788144226000426, 4.090932644426789722, 6.546538158064899804 ) ) ;
#65753 = EDGE_CURVE ( 'NONE', #12380, #62494, #64736, .T. ) ;
#65754 = CARTESIAN_POINT ( 'NONE',  ( 12.38752622470988918, 11.20128320849600811, -3.203207420725545873 ) ) ;
#65755 = CARTESIAN_POINT ( 'NONE',  ( 17.87143624835593059, 1.954798354056923371, -13.77413458888036679 ) ) ;
#65756 = CARTESIAN_POINT ( 'NONE',  ( 10.65293113562639959, 5.100000000000000533, -6.444141223575878819 ) ) ;
#65757 = LINE ( 'NONE', #28719, #39946 ) ;
#65758 = ORIENTED_EDGE ( 'NONE', *, *, #40787, .F. ) ;
#65759 = FACE_OUTER_BOUND ( 'NONE', #22176, .T. ) ;
#65760 = FACE_OUTER_BOUND ( 'NONE', #27823, .T. ) ;
#65761 = CARTESIAN_POINT ( 'NONE',  ( 9.810585478579779917, -4.629544268302966614, 8.592274333092912997 ) ) ;
#65762 = CARTESIAN_POINT ( 'NONE',  ( 10.57980110216399972, 3.260758259645400337, 7.951464549725199227 ) ) ;
#65763 = CARTESIAN_POINT ( 'NONE',  ( 8.745593092018999926, -5.100000000000000533, 6.404090157675000228 ) ) ;
#65764 = CARTESIAN_POINT ( 'NONE',  ( 11.29595444038000096, -2.828863075736999910, -8.191124550002999882 ) ) ;
#65765 = CARTESIAN_POINT ( 'NONE',  ( 18.00096209670562786, -0.5835546240610994806, -13.98799446466780694 ) ) ;
#65766 = CARTESIAN_POINT ( 'NONE',  ( 9.631052653747600445, 5.349725748959462734, -7.768783048622874610 ) ) ;
#65767 = CARTESIAN_POINT ( 'NONE',  ( 9.470944094206000585, 5.100000000000000533, 6.571291218949999902 ) ) ;
#65768 = ORIENTED_EDGE ( 'NONE', *, *, #21703, .F. ) ;
#65769 = CARTESIAN_POINT ( 'NONE',  ( 7.371899607694904155, 3.032515528092295298, 8.944945008364053152 ) ) ;
#65770 = ORIENTED_EDGE ( 'NONE', *, *, #61365, .F. ) ;
#65771 = CARTESIAN_POINT ( 'NONE',  ( 18.12605992003771505, -2.245077608621426357, 13.72424617901693189 ) ) ;
#65772 = CARTESIAN_POINT ( 'NONE',  ( 7.760748336203000086, 3.157321061061999945, 6.445092363529999702 ) ) ;
#65773 = ORIENTED_EDGE ( 'NONE', *, *, #32996, .F. ) ;
#65774 = CARTESIAN_POINT ( 'NONE',  ( 10.60746886766490071, 3.501664543805500074, 8.405426684175299812 ) ) ;
#65775 = CARTESIAN_POINT ( 'NONE',  ( 6.067661678829444405, 1.119639795224268930, -0.1760443708165491672 ) ) ;
#65776 = CARTESIAN_POINT ( 'NONE',  ( 8.719914745407999490, -4.065337473341759988, -8.403568966271999230 ) ) ;
#65777 = CARTESIAN_POINT ( 'NONE',  ( 10.15403136780999915, 5.267988602993999514, 5.992335067371000079 ) ) ;
#65778 = DIRECTION ( 'NONE',  ( 0.000000000000000000, 1.000000000000000000, 0.000000000000000000 ) ) ;
#65779 = DIRECTION ( 'NONE',  ( -2.260144215113719931E-16, 0.3352635608502960163, -0.9421243786071880066 ) ) ;
#65780 = CARTESIAN_POINT ( 'NONE',  ( 23.66004879239100234, 13.39256445865000167, -3.813547382634999483 ) ) ;
#65781 = CIRCLE ( 'NONE', #51269, 13.10000000000000142 ) ;
#65782 = ADVANCED_FACE ( 'NONE', ( #22551 ), #38278, .F. ) ;
#65783 = CARTESIAN_POINT ( 'NONE',  ( 10.23643195768000069, -5.517145045299000294, -6.754127937316000363 ) ) ;
#65784 = CARTESIAN_POINT ( 'NONE',  ( 3.999971066382000284, -2.149963194831999935, 0.000000000000000000 ) ) ;
#65785 = PLANE ( 'NONE',  #62359 ) ;
#65786 = VERTEX_POINT ( 'NONE', #54369 ) ;
#65787 = CARTESIAN_POINT ( 'NONE',  ( 9.925810748568999031, 2.827416853083249304, 6.999756549658379789 ) ) ;
#65788 = FILL_AREA_STYLE ('',( #56349 ) ) ;
#65789 = CARTESIAN_POINT ( 'NONE',  ( 18.20500217910819885, -2.141655701387318977, -13.83591107703642997 ) ) ;
#65790 = CARTESIAN_POINT ( 'NONE',  ( 10.73278136149000161, -5.209917005081999619, 4.894959764772000455 ) ) ;
#65791 = CARTESIAN_POINT ( 'NONE',  ( 10.74207053302677828, -3.170338597610990128, -8.579608023176293230 ) ) ;
#65792 = CARTESIAN_POINT ( 'NONE',  ( 9.937659112603999034, 3.444147913214900214, -8.652134039551000910 ) ) ;
#65793 = CARTESIAN_POINT ( 'NONE',  ( 12.44718984625868430, 1.987489649616605236, 13.76884489496294961 ) ) ;
#65794 = B_SPLINE_SURFACE_WITH_KNOTS ( 'NONE', 1, 3, ( 
 ( #10444, #46831, #10106, #31784, #31440, #63583, #53102, #36336, #31106, #3818, #5202, #25156, #52411, #46489, #67795, #41240, #35990, #38748, #21965, #32137, #12179, #11473, #33161, #43304, #32473, #59373, #54478, #17063, #6924, #60075, #32813, #64264, #5884, #38395, #16718, #16379, #37709, #59037, #54130, #11138, #1000, #53788, #64611, #27225, #54825, #48895, #38047, #48548, #42956, #22312, #27919, #304, #65305, #43654, #59720, #652, #27567, #33509, #11822, #6579, #49229, #6227, #28258, #17420, #64948, #1338, #22653, #43998, #49576, #21283, #42615, #63923, #16034, #37364, #58686, #10790, #53448, #5545, #26885, #48200, #21621, #12874, #23358, #29658, #60757, #8652 ),
 ( #24043, #34200, #40460, #23699, #18118, #34890, #39093, #66338, #1686, #65653, #45034, #18462, #29306, #67028, #19139, #7972, #50618, #60418, #18809, #2038, #45378, #56205, #40136, #30000, #61450, #7273, #12523, #23003, #44352, #66688, #33854, #50959, #61790, #13906, #13568, #17775, #8312, #55170, #49927, #39787, #55519, #39437, #44697, #3057, #28613, #7621, #2719, #65993, #28967, #24390, #50274, #2376, #56546, #45719, #61107, #13227, #35234, #34554, #55864, #46060, #68743, #68393, #4425, #20860, #67705, #30668, #58262, #4767, #52330, #20169, #25416, #19488, #57570, #41497, #42198, #51976, #62129, #63498, #62810, #63148, #4080, #62469, #14927, #15275, #47093, #36948 ) ),
 .UNSPECIFIED., .F., .F., .F.,
 ( 2, 2 ),
 ( 4, 2, 2, 2, 2, 2, 2, 2, 2, 2, 2, 2, 2, 2, 2, 2, 2, 2, 2, 2, 2, 2, 2, 2, 2, 2, 2, 2, 2, 2, 2, 2, 2, 2, 2, 2, 2, 2, 2, 2, 2, 2, 4 ),
 ( 0.000000000000000000, 1.000000000000000000 ),
 ( 0.000000000000000000, 7.142680049747104757E-05, 0.0001428536009949420951, 0.0002142804014924131427, 0.0002857072019898841903, 0.0003571340024873552108, 0.0004285608029848262854, 0.0004999876034822973601, 0.0005357010037310328161, 0.0005714144039797683806, 0.0006071278042285039450, 0.0006428412044772394010, 0.0007142680049747104215, 0.0007856948054721815504, 0.0008214082057209171148, 0.0008571216059696525709, 0.0008928350062183880269, 0.0009285484064671235913, 0.0009999752069645947202, 0.001071402007462065632, 0.001142828807959536761, 0.001214255608457007890, 0.001285682408954478802, 0.001321395809203214367, 0.001357109209451949714, 0.001428536009949420843, 0.001499962810446891972, 0.001535676210695627536, 0.001571389610944363101, 0.001607103011193098665, 0.001642816411441834230, 0.001714243211939305142, 0.001785670012436776054, 0.001821383412685511618, 0.001857096812934247183, 0.001928523613431718312, 0.001964237013680454093, 0.001999950413929189440, 0.002035663814177924788, 0.002071377214426660569, 0.002142804014924131265, 0.002214230815421602393, 0.002285657615919073522 ),
 .UNSPECIFIED. ) ;
#65795 = CARTESIAN_POINT ( 'NONE',  ( 9.590594544025000445, -2.445960766574000189, 7.841185849078001091 ) ) ;
#65796 = ORIENTED_EDGE ( 'NONE', *, *, #17136, .T. ) ;
#65797 = CARTESIAN_POINT ( 'NONE',  ( 10.29353630808639863, 2.899999999999999911, 6.665341197380421079 ) ) ;
#65798 = CARTESIAN_POINT ( 'NONE',  ( 12.11827043973743301, 0.2342631834278612046, 13.99804438501501203 ) ) ;
#65799 = EDGE_LOOP ( 'NONE', ( #23680, #10891, #43443, #49349 ) ) ;
#65800 = CARTESIAN_POINT ( 'NONE',  ( 7.003728317543000514, 5.017953588770000195, -6.429833855306000601 ) ) ;
#65801 = CARTESIAN_POINT ( 'NONE',  ( 17.60531108750599927, 11.81466229355000053, -3.323436300174000380 ) ) ;
#65802 = CIRCLE ( 'NONE', #8915, 11.50000000000000178 ) ;
#65803 = CARTESIAN_POINT ( 'NONE',  ( 24.38452244591600149, -3.342920588330999809, -12.19242501195000017 ) ) ;
#65804 = CARTESIAN_POINT ( 'NONE',  ( 4.690459180880000467, -0.6685019426975999934, -1.486331215039000009 ) ) ;
#65805 = B_SPLINE_SURFACE_WITH_KNOTS ( 'NONE', 3, 3, ( 
 ( #34891, #56548, #30334, #24735, #23701, #8654, #46062, #29308, #29660, #14251, #35579, #24392, #50961, #51641, #3059, #34556, #50620, #54357, #23929, #54709, #22540, #43880, #27809, #65535, #28496, #49115, #18005, #34439, #60990, #39671, #44239, #55753, #49811, #1229, #65879, #7498, #12409, #59606, #55404, #11704, #28853, #33392, #39323, #6461, #23243, #18348, #1922, #6808, #38983, #50500, #33043, #22888, #17660, #16946, #50161, #2264, #23582, #44921, #49457, #12062, #45265, #13108, #7158, #7855, #60644, #66226, #55056 ),
 ( #2598, #12757, #38629, #29189, #38279, #65184, #28145, #60300, #17304, #59951, #1568, #33742, #44586, #34086, #36494, #60295, #22533, #44234, #49452, #60639, #55396, #64481, #34081, #28138, #27446, #65526, #55050, #59943, #37929, #33734, #59248, #7153, #11697, #17654, #54005, #1561, #65872, #22883, #33037, #17297, #28847, #11354, #1220, #43872, #16604, #28488, #49806, #1916, #23236, #27803, #59599, #2259, #17997, #54703, #39317, #38977, #44580, #33387, #12403, #65178, #38622, #54349, #32692, #6107, #7492, #12750, #12054 ),
 ( #878, #48770, #22193, #50155, #6801, #16939, #23573, #43530, #64829, #38272, #6453, #49109, #51188, #50492, #60985, #18683, #13100, #35792, #3284, #45937, #2937, #40686, #24953, #34771, #3957, #29881, #61330, #24614, #44916, #14128, #39662, #8878, #13450, #7848, #55748, #30213, #50840, #56080, #61669, #13784, #40016, #8189, #29183, #2593, #19363, #23924, #35455, #66220, #51518, #56429, #62015, #57107, #51861, #46285, #35117, #29539, #66564, #45259, #24266, #19713, #45603, #66907, #19022, #8533, #67248, #3618, #56780 ),
 ( #40348, #67589, #41033, #62356, #14474, #30547, #9205, #18343, #34432, #46971, #41720, #62688, #20739, #25296, #20053, #47315, #42067, #52900, #21417, #42752, #31582, #58825, #4997, #68274, #31927, #10934, #53240, #63021, #4647, #63720, #30893, #14811, #46631, #26335, #63375, #20394, #5339, #15499, #15833, #41381, #26684, #21086, #47658, #52206, #36130, #15151, #57444, #16176, #68973, #42413, #52550, #37163, #48000, #36472, #53587, #10244, #57792, #58484, #67937, #10588, #9552, #98, #9904, #4307, #25641, #64055, #31243 ) ),
 .UNSPECIFIED., .F., .F., .F.,
 ( 4, 4 ),
 ( 4, 1, 1, 1, 1, 1, 1, 1, 1, 1, 1, 1, 1, 1, 1, 1, 1, 1, 1, 1, 1, 1, 1, 1, 1, 1, 1, 1, 1, 1, 1, 1, 1, 1, 1, 1, 1, 1, 1, 1, 1, 1, 1, 1, 1, 1, 1, 1, 1, 1, 1, 1, 1, 1, 1, 1, 1, 1, 1, 1, 1, 1, 1, 1, 4 ),
 ( -0.02000000000000000042, 1.020000000000000018 ),
 ( -0.02000000000000000042, -0.003749999999999999861, 0.01250000000000000069, 0.02875000000000000125, 0.04499999999999999833, 0.06124999999999999889, 0.07749999999999999944, 0.09375000000000000000, 0.1100000000000000006, 0.1262500000000000011, 0.1424999999999999878, 0.1587500000000000022, 0.1749999999999999889, 0.1912500000000000033, 0.2074999999999999900, 0.2237500000000000044, 0.2399999999999999911, 0.2562499999999999778, 0.2725000000000000200, 0.2887500000000000067, 0.3049999999999999933, 0.3212499999999999800, 0.3375000000000000222, 0.3537500000000000089, 0.3699999999999999956, 0.3862499999999999822, 0.4025000000000000244, 0.4187500000000000111, 0.4349999999999999978, 0.4512499999999999845, 0.4675000000000000266, 0.4837500000000000133, 0.5000000000000000000, 0.5162499999999999867, 0.5324999999999999734, 0.5487499999999999600, 0.5649999999999999467, 0.5812500000000000444, 0.5975000000000000311, 0.6137500000000000178, 0.6300000000000000044, 0.6462499999999999911, 0.6624999999999999778, 0.6787499999999999645, 0.6949999999999999512, 0.7112500000000000488, 0.7275000000000000355, 0.7437500000000000222, 0.7600000000000000089, 0.7762499999999999956, 0.7924999999999999822, 0.8087499999999999689, 0.8249999999999999556, 0.8412500000000000533, 0.8575000000000000400, 0.8737500000000000266, 0.8900000000000000133, 0.9062500000000000000, 0.9224999999999999867, 0.9387499999999999734, 0.9549999999999999600, 0.9712499999999999467, 0.9875000000000000444, 1.003749999999999920, 1.020000000000000018 ),
 .UNSPECIFIED. ) ;
#65806 = CARTESIAN_POINT ( 'NONE',  ( 9.725595280412999699, 2.495531372253999791, -7.930944806125000746 ) ) ;
#65807 = CYLINDRICAL_SURFACE ( 'NONE', #7920, 1.350000000000000533 ) ;
#65808 = CARTESIAN_POINT ( 'NONE',  ( 9.922182479546000522, -3.489927462211000364, -9.111803974470001677 ) ) ;
#65809 = CARTESIAN_POINT ( 'NONE',  ( 8.169101745083519717, 4.353498524260636771, -8.815135294168911173 ) ) ;
#65810 = PLANE ( 'NONE',  #13669 ) ;
#65811 =( NAMED_UNIT ( * ) SI_UNIT ( $, .STERADIAN. ) SOLID_ANGLE_UNIT ( ) );
#65812 = CARTESIAN_POINT ( 'NONE',  ( 9.866664898013999263, -4.626219091573998909, -9.027249334595000008 ) ) ;
#65813 = CARTESIAN_POINT ( 'NONE',  ( 11.12133729122639991, 3.134101783108900197, -7.477221318588949117 ) ) ;
#65814 = CARTESIAN_POINT ( 'NONE',  ( 1.136390132542124398, -0.4581489286485235790, 3.499999999999998224 ) ) ;
#65815 = EDGE_CURVE ( 'NONE', #41592, #65121, #58071, .T. ) ;
#65816 = ADVANCED_FACE ( 'NONE', ( #32712 ), #12072, .F. ) ;
#65817 = CARTESIAN_POINT ( 'NONE',  ( 11.59603632436369125, 3.157359628034400068, -7.303218851299499548 ) ) ;
#65818 = CARTESIAN_POINT ( 'NONE',  ( 8.874784697134998623, 4.545051930576500254, -6.656340890368899643 ) ) ;
#65820 = CARTESIAN_POINT ( 'NONE',  ( 10.88463635395000040, -2.841787580345000119, 5.065370950741000300 ) ) ;
#65819 = CARTESIAN_POINT ( 'NONE',  ( 10.50760887879199856, -4.196341783741199372, 8.344486736701099971 ) ) ;
#65821 = CARTESIAN_POINT ( 'NONE',  ( 10.91620964606000044, 2.818413279081999789, -6.814156272943999504 ) ) ;
#65822 = ORIENTED_EDGE ( 'NONE', *, *, #45006, .T. ) ;
#65823 = CARTESIAN_POINT ( 'NONE',  ( 10.44999293566599974, 4.720032669050099550, 6.616719557880299085 ) ) ;
#65824 = CARTESIAN_POINT ( 'NONE',  ( 11.06924082387999952, -5.425685649895999774, 8.012912555523998392 ) ) ;
#65825 = CARTESIAN_POINT ( 'NONE',  ( 9.127126402770999292, 5.196937059091999878, 7.951360234587600218 ) ) ;
#65826 = CARTESIAN_POINT ( 'NONE',  ( 9.454862456499625978, 4.412447805680870694, -6.728365969834097626 ) ) ;
#65827 = CARTESIAN_POINT ( 'NONE',  ( 9.944325809452999820, -5.443013936195000291, 7.367349259341000156 ) ) ;
#65828 = DIRECTION ( 'NONE',  ( -1.000000000000000000, 0.000000000000000000, 0.000000000000000000 ) ) ;
#65830 = CARTESIAN_POINT ( 'NONE',  ( 10.44601354018326944, 3.000416447002273834, 6.731816600031359066 ) ) ;
#65829 = UNCERTAINTY_MEASURE_WITH_UNIT (LENGTH_MEASURE( 1.000000000000000082E-05 ), #52898, 'distance_accuracy_value', 'NONE');
#65831 = ORIENTED_EDGE ( 'NONE', *, *, #68408, .T. ) ;
#65832 = EDGE_CURVE ( 'NONE', #14332, #26661, #58693, .T. ) ;
#65833 = CARTESIAN_POINT ( 'NONE',  ( 9.356038493598999750, -3.273092657276900130, -6.806856425099999441 ) ) ;
#65834 = CARTESIAN_POINT ( 'NONE',  ( 9.771013540183334456, -4.768183399968641822, -6.500416447002272058 ) ) ;
#65835 = B_SPLINE_CURVE_WITH_KNOTS ( 'NONE', 3,
 ( #21387, #42720, #7732, #7039, #12290, #54589, #55286, #1451, #17172, #48995, #66108, #65761, #27681, #1107, #33272, #50040, #22419, #18225 ),
 .UNSPECIFIED., .F., .F.,
 ( 4, 2, 2, 2, 2, 2, 2, 2, 4 ),
 ( 0.1494581667962518179, 0.2557758959467203441, 0.3620936250971888981, 0.4684113542476573411, 0.5747290833981258951, 0.6810468125485944491, 0.7873645416990628920, 0.8936822708495314460, 1.000000000000000000 ),
 .UNSPECIFIED. ) ;
#65836 = LINE ( 'NONE', #55014, #33256 ) ;
#65837 = EDGE_CURVE ( 'NONE', #2005, #56175, #35807, .T. ) ;
#65838 = CARTESIAN_POINT ( 'NONE',  ( 6.999999999999999112, 10.24473655391737204, -4.324905599572709036 ) ) ;
#65839 = CARTESIAN_POINT ( 'NONE',  ( 24.46580263708699832, -3.340075003801000086, 12.12245366788000034 ) ) ;
#65840 = CARTESIAN_POINT ( 'NONE',  ( 11.71979841651039855, -4.304975143798100312, 6.689266534545799558 ) ) ;
#65841 = CARTESIAN_POINT ( 'NONE',  ( 10.30903300763299946, 4.597717337857299746, -8.126922218169600143 ) ) ;
#65842 = CARTESIAN_POINT ( 'NONE',  ( 12.20341915910182351, 2.330389505238763093, -13.70797212924216701 ) ) ;
#65843 = CARTESIAN_POINT ( 'NONE',  ( 25.18907852600200314, -8.466516726705998863, 8.230855237650001044 ) ) ;
#65844 = CARTESIAN_POINT ( 'NONE',  ( 12.15805955570366592, 2.854826764633444203, 12.27308055910813600 ) ) ;
#65845 = EDGE_LOOP ( 'NONE', ( #10566, #32901, #19308, #11251 ) ) ;
#65846 = CARTESIAN_POINT ( 'NONE',  ( 10.90000016885999834, 9.856474585920999232, -5.627825103726000755 ) ) ;
#65847 = CARTESIAN_POINT ( 'NONE',  ( 12.08004253349364454, -0.01140630886273803594, -14.00000041621361291 ) ) ;
#65848 = CARTESIAN_POINT ( 'NONE',  ( 13.73849254682300192, -8.874722368053999944, -7.906926164786999500 ) ) ;
#65849 = CARTESIAN_POINT ( 'NONE',  ( 11.58457173739308210, 4.937225096800481161, -8.361882233189918523 ) ) ;
#65850 = CIRCLE ( 'NONE', #35724, 9.250000000000000000 ) ;
#65851 = CARTESIAN_POINT ( 'NONE',  ( 4.599999999999999645, -3.199751711897561357, 12.18694338143115452 ) ) ;
#65852 = CYLINDRICAL_SURFACE ( 'NONE', #48550, 1.250000000000000222 ) ;
#65853 = LINE ( 'NONE', #43509, #66405 ) ;
#65854 = EDGE_LOOP ( 'NONE', ( #57437, #175, #9115, #16701 ) ) ;
#65855 = CARTESIAN_POINT ( 'NONE',  ( 23.56666365135700403, 8.694246338441999455, 8.392498551189996547 ) ) ;
#65856 = CARTESIAN_POINT ( 'NONE',  ( 18.07092639204458706, 2.147008627175521323, -13.74201915664823659 ) ) ;
#65857 = ORIENTED_EDGE ( 'NONE', *, *, #1401, .F. ) ;
#65858 = CARTESIAN_POINT ( 'NONE',  ( 8.434805295391889501, 5.349284795551519700, 7.676787393164572038 ) ) ;
#65859 = CARTESIAN_POINT ( 'NONE',  ( 24.77780384695583749, 8.621836997252826151, -8.548042839575236584 ) ) ;
#65860 = CARTESIAN_POINT ( 'NONE',  ( 8.506095280410999493, 2.305580295895999665, -7.860904109308999743 ) ) ;
#65861 = CARTESIAN_POINT ( 'NONE',  ( 24.30001694391200218, -12.21047201246000036, 3.271805662802000025 ) ) ;
#65862 = CARTESIAN_POINT ( 'NONE',  ( 11.09590547754519996, -2.684394667508000154, -7.541753805330609239 ) ) ;
#65863 = CARTESIAN_POINT ( 'NONE',  ( 18.02801395604344847, 0.4085932599149181832, -12.69115266610270254 ) ) ;
#65864 = CARTESIAN_POINT ( 'NONE',  ( 10.32101354018233152, -4.768183399968640934, 8.499583552997727054 ) ) ;
#65865 = VERTEX_POINT ( 'NONE', #66240 ) ;
#65866 = CARTESIAN_POINT ( 'NONE',  ( 9.137549407199999862, -2.995696424181999884, 8.544763501938000161 ) ) ;
#65867 = CARTESIAN_POINT ( 'NONE',  ( 18.06394506373647602, -2.862992422157873751, -13.58968849268030965 ) ) ;
#65868 = CARTESIAN_POINT ( 'NONE',  ( 7.100000000000000533, 12.50865771883999855, -2.924687089724999911 ) ) ;
#65869 = EDGE_LOOP ( 'NONE', ( #40805, #43947, #42830, #33870, #47564, #39463, #15290, #20224, #20884, #51273 ) ) ;
#65870 = CARTESIAN_POINT ( 'NONE',  ( 9.741003491525001223, 3.588532719919999892, -8.800216240366001585 ) ) ;
#65871 = ORIENTED_EDGE ( 'NONE', *, *, #59699, .T. ) ;
#65872 = CARTESIAN_POINT ( 'NONE',  ( 9.381367640780998940, 4.473477001189199775, 8.385811396220899994 ) ) ;
#65873 = CARTESIAN_POINT ( 'NONE',  ( 18.10980516112012495, -2.943705546998118816, -12.25131356140272132 ) ) ;
#65874 = CARTESIAN_POINT ( 'NONE',  ( 9.529346873515667227, 4.163624617374466652, 6.250000000000000000 ) ) ;
#65875 = EDGE_CURVE ( 'NONE', #19742, #12021, #54724, .T. ) ;
#65876 = CARTESIAN_POINT ( 'NONE',  ( 10.38314899745999931, -5.167567567567999731, 6.822293592207000934 ) ) ;
#65877 = CARTESIAN_POINT ( 'NONE',  ( 11.48831242699000121, -11.66400889920000061, -1.747256858593000173 ) ) ;
#65878 = EDGE_CURVE ( 'NONE', #2543, #65237, #43083, .T. ) ;
#65879 = CARTESIAN_POINT ( 'NONE',  ( 9.510025935145998588, 3.874109063559000088, 8.357822485499299958 ) ) ;
#65880 = CARTESIAN_POINT ( 'NONE',  ( 9.520528907821001141, -2.899999999999999911, 6.152188490330000370 ) ) ;
#65881 = ORIENTED_EDGE ( 'NONE', *, *, #62743, .T. ) ;
#65882 = DIRECTION ( 'NONE',  ( 0.000000000000000000, 0.000000000000000000, 1.000000000000000000 ) ) ;
#65883 = CARTESIAN_POINT ( 'NONE',  ( 10.78888278041000071, 2.675726696512000125, -6.748227692827999391 ) ) ;
#65884 = CARTESIAN_POINT ( 'NONE',  ( 10.86268281683999959, -5.065331559464999245, -5.170271095491000501 ) ) ;
#65885 = CARTESIAN_POINT ( 'NONE',  ( 12.44779487374910332, 3.012931620461074100, -13.55119122998581460 ) ) ;
#65886 = CARTESIAN_POINT ( 'NONE',  ( 10.52022949779799887, -3.290320231472799950, -8.564302809495998758 ) ) ;
#65887 = CARTESIAN_POINT ( 'NONE',  ( 24.74074867997300231, 3.240101435799000118, 11.83468233123000068 ) ) ;
#65888 = CARTESIAN_POINT ( 'NONE',  ( 17.72054635526678013, -0.7113363331415086810, 13.98191770012929780 ) ) ;
#65889 = CARTESIAN_POINT ( 'NONE',  ( 25.52469074519600056, -2.886190667329999737, 11.27615698518999920 ) ) ;
#65890 = ORIENTED_EDGE ( 'NONE', *, *, #39310, .T. ) ;
#65891 = ORIENTED_EDGE ( 'NONE', *, *, #39541, .F. ) ;
#65892 = CARTESIAN_POINT ( 'NONE',  ( 8.947714158774999760, 3.854507394315999758, -9.394302886912999639 ) ) ;
#65893 = CARTESIAN_POINT ( 'NONE',  ( 12.37275480852669318, -0.4515881961619166440, 13.89013012615365028 ) ) ;
#65894 = CARTESIAN_POINT ( 'NONE',  ( 12.61467092246319055, -0.5953860544347909789, -13.88283270324647845 ) ) ;
#65895 = LINE ( 'NONE', #28516, #31472 ) ;
#65896 = DIRECTION ( 'NONE',  ( -1.000000000000000000, 0.000000000000000000, 3.552713678967001067E-14 ) ) ;
#65897 = EDGE_CURVE ( 'NONE', #48158, #4266, #17198, .T. ) ;
#65898 = EDGE_CURVE ( 'NONE', #36822, #46708, #59798, .T. ) ;
#65899 = CARTESIAN_POINT ( 'NONE',  ( 8.385058059625000837, -4.977917894183000236, 6.416767031887000705 ) ) ;
#65901 = CIRCLE ( 'NONE', #6756, 14.00000000000000355 ) ;
#65900 = DIRECTION ( 'NONE',  ( 0.000000000000000000, 1.000000000000000000, 0.000000000000000000 ) ) ;
#65903 = FACE_OUTER_BOUND ( 'NONE', #2316, .T. ) ;
#65902 = CARTESIAN_POINT ( 'NONE',  ( 9.627126402771001068, -2.803062940908000122, 7.951360234587600218 ) ) ;
#65904 = CARTESIAN_POINT ( 'NONE',  ( 11.05964426047339799, 4.687693494822500639, -8.577215873335999774 ) ) ;
#65905 = ADVANCED_FACE ( 'NONE', ( #50858 ), #67263, .T. ) ;
#65906 = CARTESIAN_POINT ( 'NONE',  ( 12.71012435279160435, -0.7254930141058675286, 13.98119259374225365 ) ) ;
#65907 = CARTESIAN_POINT ( 'NONE',  ( 7.600000000000000533, 0.000000000000000000, 0.000000000000000000 ) ) ;
#65908 = CARTESIAN_POINT ( 'NONE',  ( 7.883148997456999929, 5.167567567567999731, 6.822293592207000934 ) ) ;
#65909 = CARTESIAN_POINT ( 'NONE',  ( 10.32891357011178179, -2.649873868443101355, -7.263327745081085141 ) ) ;
#65910 = CARTESIAN_POINT ( 'NONE',  ( 17.98440366585430539, -2.954302470114323675, -12.33403020158385743 ) ) ;
#65911 = EDGE_LOOP ( 'NONE', ( #23651, #54450, #17977, #9815, #55630, #51517, #23613, #5441, #1627, #39355 ) ) ;
#65913 = CARTESIAN_POINT ( 'NONE',  ( 12.43656315535333867, -1.853531805844372604, -12.46297683056140926 ) ) ;
#65912 = CARTESIAN_POINT ( 'NONE',  ( 8.289120559623999185, -4.310353212080000773, 9.459493062793997709 ) ) ;
#65914 = CARTESIAN_POINT ( 'NONE',  ( 9.509454719593000149, 3.116293075258000478, -6.208411413796000033 ) ) ;
#65915 = DIRECTION ( 'NONE',  ( 0.000000000000000000, 1.000000000000000000, 0.000000000000000000 ) ) ;
#65916 = CARTESIAN_POINT ( 'NONE',  ( 7.915155411429996235, -5.089315853099998677, 6.494606418034001294 ) ) ;
#65917 = FACE_OUTER_BOUND ( 'NONE', #58900, .T. ) ;
#65918 = EDGE_CURVE ( 'NONE', #53919, #63466, #42226, .T. ) ;
#65919 = CARTESIAN_POINT ( 'NONE',  ( 8.191498566858999908, 3.399962487441000381, 6.146646668338000552 ) ) ;
#65920 = CARTESIAN_POINT ( 'NONE',  ( 2.833702399587000098, -3.260318005001999975, 1.508036922365999954 ) ) ;
#65921 = VERTEX_POINT ( 'NONE', #14488 ) ;
#65922 = CARTESIAN_POINT ( 'NONE',  ( 12.08961557973414358, 0.1170514037749880998, -12.59946170170351465 ) ) ;
#65923 = DIRECTION ( 'NONE',  ( 0.000000000000000000, -1.000000000000000000, 0.000000000000000000 ) ) ;
#65924 = CARTESIAN_POINT ( 'NONE',  ( 8.751496707488000126, 4.081676005979390176, -8.356402621895700378 ) ) ;
#65925 = CARTESIAN_POINT ( 'NONE',  ( 7.101301658771000724, 3.554857159507999853, 8.889479859586000288 ) ) ;
#65926 = ORIENTED_EDGE ( 'NONE', *, *, #64062, .F. ) ;
#65927 = CARTESIAN_POINT ( 'NONE',  ( 6.882863159730999492, -1.197190821580000009, 0.3103650564550000102 ) ) ;
#65928 = CARTESIAN_POINT ( 'NONE',  ( 10.94699683900224230, 9.189629059784236276, 6.317109415722915067 ) ) ;
#65930 = CARTESIAN_POINT ( 'NONE',  ( 10.77332351902737528, 2.820285017511521719, -8.179908095962574066 ) ) ;
#65929 = CARTESIAN_POINT ( 'NONE',  ( 8.883148997460001084, 5.167567567567999731, 6.822293592207000934 ) ) ;
#65931 = CARTESIAN_POINT ( 'NONE',  ( 10.80502344389999791, 2.874741265256000489, -6.817099149379099110 ) ) ;
#65932 = ORIENTED_EDGE ( 'NONE', *, *, #63473, .T. ) ;
#65933 =( LENGTH_UNIT ( ) NAMED_UNIT ( * ) SI_UNIT ( .MILLI., .METRE. ) );
#65934 = ORIENTED_EDGE ( 'NONE', *, *, #27387, .F. ) ;
#65935 = DIRECTION ( 'NONE',  ( -0.9999999999996369571, -8.520359571663319094E-07, -4.194710005752155130E-09 ) ) ;
#65937 = CARTESIAN_POINT ( 'NONE',  ( -15.86200481174999943, 0.8000000000000000444, -3.149999999999999911 ) ) ;
#65936 = AXIS2_PLACEMENT_3D ( 'NONE', #2359, #30560, #24632 ) ;
#65938 = CARTESIAN_POINT ( 'NONE',  ( 17.86760510161943927, -0.5416168188285630514, -13.88579828294357554 ) ) ;
#65939 = ORIENTED_EDGE ( 'NONE', *, *, #62889, .T. ) ;
#65940 = CARTESIAN_POINT ( 'NONE',  ( 7.683884986463000111, -9.053566239910001201, 5.593786582504999494 ) ) ;
#65941 = CARTESIAN_POINT ( 'NONE',  ( 23.66004879239100234, -9.998910854163000295, -9.691527647852998584 ) ) ;
#65942 = CARTESIAN_POINT ( 'NONE',  ( 4.500000000000000000, -3.200000000000000178, 0.000000000000000000 ) ) ;
#65943 = CARTESIAN_POINT ( 'NONE',  ( 9.933536308084500277, 2.899999999999999911, -6.665341197412895546 ) ) ;
#65944 = CARTESIAN_POINT ( 'NONE',  ( 8.610875063856999745, -4.757997781751000410, 5.934102420827000124 ) ) ;
#65945 = ORIENTED_EDGE ( 'NONE', *, *, #49708, .F. ) ;
#65946 = DIRECTION ( 'NONE',  ( 1.000000000000000000, 0.000000000000000000, 0.000000000000000000 ) ) ;
#65947 = CARTESIAN_POINT ( 'NONE',  ( 24.13681598081500113, -12.33402671357999836, -3.394326608267999923 ) ) ;
#65948 = APPLICATION_CONTEXT ( 'automotive_design' ) ;
#65949 = CIRCLE ( 'NONE', #54781, 2.725000000000000089 ) ;
#65950 = CARTESIAN_POINT ( 'NONE',  ( 10.97360312464731713, 5.212835794440835002, 6.753664309372819474 ) ) ;
#65951 = CYLINDRICAL_SURFACE ( 'NONE', #14718, 1.250000000000000222 ) ;
#65952 = ORIENTED_EDGE ( 'NONE', *, *, #21140, .T. ) ;
#65953 = FACE_OUTER_BOUND ( 'NONE', #33006, .T. ) ;
#65954 = CARTESIAN_POINT ( 'NONE',  ( 0.1499942179679999987, -2.750000000000000000, 0.000000000000000000 ) ) ;
#65955 = CARTESIAN_POINT ( 'NONE',  ( 4.599999999999999645, 3.125000000000000000, -13.52084414783465682 ) ) ;
#65956 = ADVANCED_FACE ( 'NONE', ( #66925 ), #27687, .F. ) ;
#65957 = CARTESIAN_POINT ( 'NONE',  ( 5.000030787343000327, -2.045306479342562156, 0.5496608443529843457 ) ) ;
#65958 = CARTESIAN_POINT ( 'NONE',  ( 11.09999999999999964, 2.274006712557999688, -7.281956340829000673 ) ) ;
#65959 = EDGE_CURVE ( 'NONE', #33463, #21890, #3089, .T. ) ;
#65960 = CARTESIAN_POINT ( 'NONE',  ( 7.156776345353000224, 1.243223188895000053, 2.274921040069000118E-10 ) ) ;
#65961 = CARTESIAN_POINT ( 'NONE',  ( 17.55505043854147118, -3.125000000000000000, 12.28374638332999780 ) ) ;
#65962 = ORIENTED_EDGE ( 'NONE', *, *, #36133, .T. ) ;
#65963 = CARTESIAN_POINT ( 'NONE',  ( 10.89835090130999973, -3.121033016283800254, -8.043647632228999811 ) ) ;
#65964 = VERTEX_POINT ( 'NONE', #45194 ) ;
#65965 = DIRECTION ( 'NONE',  ( 1.000000000000000000, 0.000000000000000000, 0.000000000000000000 ) ) ;
#65966 = CARTESIAN_POINT ( 'NONE',  ( 9.743314158772999889, 5.149303692842000402, -5.987168472229000393 ) ) ;
#65967 = CARTESIAN_POINT ( 'NONE',  ( 2.586992650581000142, -3.369180291263000004, 0.2624141663141000280 ) ) ;
#65968 = B_SPLINE_CURVE_WITH_KNOTS ( 'NONE', 3,
 ( #30746, #31780, #36681, #41918, #47168, #9752, #52752, #10101, #31436, #4847, #68471, #25151, #52406, #58002, #21279, #4499, #25497, #53098, #47862, #26191, #42275, #31100, #52055, #9069, #30407, #4159 ),
 .UNSPECIFIED., .F., .F.,
 ( 4, 2, 2, 2, 2, 2, 2, 2, 2, 1, 1, 2, 2, 4 ),
 ( 0.000000000000000000, 0.1000754736140108403, 0.2001509472280216806, 0.4003018944560433612, 0.4503396312630491560, 0.5003773680700549509, 0.6004528416840660965, 0.7005283152980773531, 0.7255471837015801118, 0.7380566179033314356, 0.7443113350042072085, 0.7474386935546450950, 0.7505660521050829814, 0.8006037889120940498 ),
 .UNSPECIFIED. ) ;
#65969 = CARTESIAN_POINT ( 'NONE',  ( 10.82564972918999935, -5.331162346451000289, -8.542142527201001201 ) ) ;
#65970 = CARTESIAN_POINT ( 'NONE',  ( 6.850806999420246512, 1.515637746885903470, -0.07806395800591044154 ) ) ;
#65971 = CARTESIAN_POINT ( 'NONE',  ( 23.73948084457800078, 13.16333625243999883, 3.763513502666000043 ) ) ;
#65972 = CARTESIAN_POINT ( 'NONE',  ( 10.55478570706233299, 5.131706358131709500, -8.113400509224881318 ) ) ;
#65973 = ORIENTED_EDGE ( 'NONE', *, *, #39227, .F. ) ;
#65974 = CARTESIAN_POINT ( 'NONE',  ( 10.12821852033218128, -4.965567672101669494, -8.481131518971576355 ) ) ;
#65975 = AXIS2_PLACEMENT_3D ( 'NONE', #8908, #24650, #29914 ) ;
#65976 = CARTESIAN_POINT ( 'NONE',  ( 10.87872469555899890, -3.497841151814999883, 8.368784980615899372 ) ) ;
#65977 = CARTESIAN_POINT ( 'NONE',  ( 10.13049857835000012, 3.092060693447000297, 8.629378633793999498 ) ) ;
#65978 = CARTESIAN_POINT ( 'NONE',  ( 10.84419170916408426, -2.685373094371525937, -7.853312882625532509 ) ) ;
#65979 = CARTESIAN_POINT ( 'NONE',  ( 8.910378124222608776, -5.351542105685522799, 7.263808684111356939 ) ) ;
#65980 = CARTESIAN_POINT ( 'NONE',  ( 9.319055905798999007, 2.899999999999999911, -6.571291218949999902 ) ) ;
#65981 = CARTESIAN_POINT ( 'NONE',  ( 11.73256516821459883, 4.706297556651700020, -8.212808089543500500 ) ) ;
#65982 = ADVANCED_FACE ( 'NONE', ( #46820 ), #36395, .T. ) ;
#65983 = CIRCLE ( 'NONE', #5694, 11.84999999999999964 ) ;
#65984 = CARTESIAN_POINT ( 'NONE',  ( 7.100000000000113332, 4.265775746597376461, -8.859935407261559703 ) ) ;
#65985 = CARTESIAN_POINT ( 'NONE',  ( 10.13827973160999818, 4.102460098134500299, -6.362794488108000301 ) ) ;
#65986 = CARTESIAN_POINT ( 'NONE',  ( 24.13647503573200126, -9.107098899030999561, 8.984880450811999708 ) ) ;
#65987 = CIRCLE ( 'NONE', #67094, 13.98989063587000281 ) ;
#65988 = CARTESIAN_POINT ( 'NONE',  ( 0.8143050634219124451, -2.465875601137460293, -2.515512106780213308 ) ) ;
#65989 = CARTESIAN_POINT ( 'NONE',  ( 11.37168584123000059, 2.803494217761000495, -6.967881733280000489 ) ) ;
#65990 = ORIENTED_EDGE ( 'NONE', *, *, #24217, .T. ) ;
#65991 = CARTESIAN_POINT ( 'NONE',  ( 8.052730646792999991, -4.968144979409999884, 5.971795951526999602 ) ) ;
#65992 = B_SPLINE_CURVE_WITH_KNOTS ( 'NONE', 3,
 ( #39041, #12121, #44298, #11761 ),
 .UNSPECIFIED., .F., .F.,
 ( 4, 4 ),
 ( 0.6941764652077998532, 1.000000000000000000 ),
 .UNSPECIFIED. ) ;
#65993 = CARTESIAN_POINT ( 'NONE',  ( 18.25518009351764093, 2.707823354518788417, 13.73564093574334244 ) ) ;
#65994 = CARTESIAN_POINT ( 'NONE',  ( 25.29987261391899978, -8.756202924575998026, 7.455126447192999883 ) ) ;
#65995 = CARTESIAN_POINT ( 'NONE',  ( 10.51810807141099779, -3.940954591493389891, -8.776647962565998995 ) ) ;
#65996 = EDGE_LOOP ( 'NONE', ( #44241, #1894, #9848, #38976, #17623, #40667, #67149 ) ) ;
#65997 = CARTESIAN_POINT ( 'NONE',  ( 25.58980614432099898, 2.739981116774000025, -11.22452184305999978 ) ) ;
#65998 = CARTESIAN_POINT ( 'NONE',  ( 8.385051658773999606, 4.977909614887999545, 6.416776202806000029 ) ) ;
#65999 = EDGE_CURVE ( 'NONE', #2756, #45376, #8045, .T. ) ;
#66001 = CARTESIAN_POINT ( 'NONE',  ( 11.76077869730539938, 3.404661623424200201, 8.673950353177000139 ) ) ;
#66000 = CARTESIAN_POINT ( 'NONE',  ( 9.193385841233000733, 2.981992329588000423, -5.895876591910999664 ) ) ;
#66002 = AXIS2_PLACEMENT_3D ( 'NONE', #17023, #60027, #43958 ) ;
#66003 = CARTESIAN_POINT ( 'NONE',  ( 10.11548915876999999, 2.489190114737999782, -6.434635778494999236 ) ) ;
#66004 = ORIENTED_EDGE ( 'NONE', *, *, #21997, .T. ) ;
#66005 = CARTESIAN_POINT ( 'NONE',  ( 11.00366064676999933, 2.264078662261999941, 7.798351372501000078 ) ) ;
#66006 = CARTESIAN_POINT ( 'NONE',  ( 17.88835954937810158, -3.166508787604182196, -13.63720117115729558 ) ) ;
#66007 = CARTESIAN_POINT ( 'NONE',  ( 10.66995391537419913, 4.943675741382899780, 6.859089544950699668 ) ) ;
#66008 = CARTESIAN_POINT ( 'NONE',  ( 9.611390067472999732, -3.334847606888000193, 5.869121315726000709 ) ) ;
#66009 = CARTESIAN_POINT ( 'NONE',  ( 8.160036350658002036, 2.891230335795000883, 6.361714733157999291 ) ) ;
#66010 = ORIENTED_EDGE ( 'NONE', *, *, #63821, .F. ) ;
#66011 = CARTESIAN_POINT ( 'NONE',  ( 24.62769666374716238, 12.35739842157732937, 2.995926059509618877 ) ) ;
#66012 = CARTESIAN_POINT ( 'NONE',  ( 1.303056799208125005, -2.798833948393629978, -2.150913519912204031 ) ) ;
#66013 = CARTESIAN_POINT ( 'NONE',  ( 8.093556867701995117, -4.420942022140136984, 5.812522706633525438 ) ) ;
#66014 = CARTESIAN_POINT ( 'NONE',  ( 10.28315099603999982, -2.387772357283999725, 7.684266429524000408 ) ) ;
#66015 = CARTESIAN_POINT ( 'NONE',  ( 9.924988015501654104, -5.349815781278972615, 7.500001845592777272 ) ) ;
#66016 = CARTESIAN_POINT ( 'NONE',  ( 9.526759580228999269, -4.976892840331100132, 7.733500918284399894 ) ) ;
#66017 = ORIENTED_EDGE ( 'NONE', *, *, #7422, .F. ) ;
#66018 = CARTESIAN_POINT ( 'NONE',  ( 24.44496350777200178, -12.03536639536000052, -3.224849854974999985 ) ) ;
#66019 = B_SPLINE_CURVE_WITH_KNOTS ( 'NONE', 3,
 ( #37416, #52114, #58737, #31161, #63971, #68881, #10844, #31491, #63635, #4906, #58060, #63284, #32186, #62938, #21335, #15062, #4219, #30801, #42333, #31838, #53500, #57702, #26595, #53154, #68530, #52462 ),
 .UNSPECIFIED., .F., .F.,
 ( 4, 2, 2, 2, 2, 2, 2, 2, 2, 2, 2, 2, 4 ),
 ( 0.000000000000000000, 0.1761049413614339532, 0.2201311767017935517, 0.2421442943719733232, 0.2476475737895179607, 0.2531508532070625428, 0.2641574120421518179, 0.3522098827228736795, 0.4402623534035955410, 0.4842885887439561943, 0.5063017064141377421, 0.5283148240843194010, 0.7044197654457721169 ),
 .UNSPECIFIED. ) ;
#66020 = CARTESIAN_POINT ( 'NONE',  ( 11.63349010443640097, -2.725546193138000284, 7.404690636538299842 ) ) ;
#66021 = ORIENTED_EDGE ( 'NONE', *, *, #40584, .T. ) ;
#66022 = DIRECTION ( 'NONE',  ( 0.000000000000000000, 0.9617682669560660980, -0.2738645663029905530 ) ) ;
#66023 = ORIENTED_EDGE ( 'NONE', *, *, #6857, .F. ) ;
#66024 = B_SPLINE_CURVE_WITH_KNOTS ( 'NONE', 3,
 ( #58605, #16982, #5470, #58956 ),
 .UNSPECIFIED., .F., .F.,
 ( 4, 4 ),
 ( 0.000000000000000000, 1.000000000000000000 ),
 .UNSPECIFIED. ) ;
#66025 = CARTESIAN_POINT ( 'NONE',  ( 8.605545280412000508, 3.122811675949999977, -6.006064052396999919 ) ) ;
#66026 = CARTESIAN_POINT ( 'NONE',  ( 11.05435090131019926, 5.119447121461000449, -8.192386390235398608 ) ) ;
#66027 = CARTESIAN_POINT ( 'NONE',  ( 13.99999999231800096, 8.833253877201999060, 7.896562762484000686 ) ) ;
#66028 = CARTESIAN_POINT ( 'NONE',  ( 12.58267958641583739, 1.915804698272715489, -12.56868422206431113 ) ) ;
#66029 = CARTESIAN_POINT ( 'NONE',  ( 12.03148876160955005, -4.790673964186999534, 6.677731919207799294 ) ) ;
#66030 = CARTESIAN_POINT ( 'NONE',  ( 11.48146005378009882, -3.088328798999600000, 7.986817550794899745 ) ) ;
#66031 =( BOUNDED_SURFACE ( )  B_SPLINE_SURFACE ( 3, 3, ( 
 ( #34249, #42575, #4464, #25804, #62852, #9366, #15319, #57266, #63884, #20904 ),
 ( #15996, #25459, #62515, #14634, #56938, #9034, #10066, #46791, #31400, #63547 ),
 ( #47829, #30375, #19875, #9716, #57967, #21247, #68097, #51683, #41205, #41884 ),
 ( #3781, #25119, #14970, #69139, #46451, #67750, #52716, #15660, #36991, #4814 ) ),
 .UNSPECIFIED., .F., .F., .T. ) 
 B_SPLINE_SURFACE_WITH_KNOTS ( ( 4, 4 ),
 ( 4, 1, 1, 1, 1, 1, 1, 4 ),
 ( 0.000000000000000000, 1.000000000000000000 ),
 ( 0.6764685980817000122, 0.6779455865321999397, 0.6880926466457000235, 0.6995436293012999851, 0.7123096649787999946, 0.7264343954043999130, 0.7420586980075000172, 0.7441198533032000739 ),
 .UNSPECIFIED. ) 
 GEOMETRIC_REPRESENTATION_ITEM ( )  RATIONAL_B_SPLINE_SURFACE ( (
 ( 1.325324334266000159, 1.325324334266000159, 1.325324334266000159, 1.325324334266000159, 1.325324334266000159, 1.325324334266000159, 1.325324334266000159, 1.325324334266000159, 1.325324334266000159, 1.325324334266000159),
 ( 0.8915585552447999884, 0.8915585552447999884, 0.8915585552447999884, 0.8915585552447999884, 0.8915585552447999884, 0.8915585552447999884, 0.8915585552447999884, 0.8915585552447999884, 0.8915585552447999884, 0.8915585552447999884),
 ( 0.8915585552447999884, 0.8915585552447999884, 0.8915585552447999884, 0.8915585552447999884, 0.8915585552447999884, 0.8915585552447999884, 0.8915585552447999884, 0.8915585552447999884, 0.8915585552447999884, 0.8915585552447999884),
 ( 1.325324334266000159, 1.325324334266000159, 1.325324334266000159, 1.325324334266000159, 1.325324334266000159, 1.325324334266000159, 1.325324334266000159, 1.325324334266000159, 1.325324334266000159, 1.325324334266000159) ) ) 
 REPRESENTATION_ITEM ( '' )  SURFACE ( )  );
#66032 = ORIENTED_EDGE ( 'NONE', *, *, #54312, .F. ) ;
#66033 = CARTESIAN_POINT ( 'NONE',  ( 9.646013540183334456, 4.999583552997728830, 8.268183399968640046 ) ) ;
#66034 = VERTEX_POINT ( 'NONE', #55332 ) ;
#66035 = CARTESIAN_POINT ( 'NONE',  ( 7.994581853207999522, -2.263562268490999951, 8.007440964304000985 ) ) ;
#66036 = CARTESIAN_POINT ( 'NONE',  ( 29.91622776632000225, 7.451147316196999408E-09, -6.772075922106999712 ) ) ;
#66037 = ORIENTED_EDGE ( 'NONE', *, *, #62974, .T. ) ;
#66038 = CARTESIAN_POINT ( 'NONE',  ( 12.54683914358776597, -1.807964460291309861, -12.46961431371563300 ) ) ;
#66039 = CARTESIAN_POINT ( 'NONE',  ( 10.57149279008999798, 3.703313553258400059, 6.398515879103999993 ) ) ;
#66040 = CARTESIAN_POINT ( 'NONE',  ( 23.56666365135700403, 2.488348886664998538, -11.45224114467999499 ) ) ;
#66041 = CARTESIAN_POINT ( 'NONE',  ( 6.555026506349999948, -1.500000000000000000, 0.000000000000000000 ) ) ;
#66042 = CARTESIAN_POINT ( 'NONE',  ( 18.26683600807099950, -11.61819309989999915, 4.528402979683000318 ) ) ;
#66043 = EDGE_CURVE ( 'NONE', #48366, #53120, #57640, .T. ) ;
#66044 = CARTESIAN_POINT ( 'NONE',  ( 5.500000000000000000, -11.95749337870000062, -3.642574926947999892 ) ) ;
#66045 = CARTESIAN_POINT ( 'NONE',  ( 12.21287994455109605, -2.700912243963290660, -13.62875716402589887 ) ) ;
#66046 = EDGE_CURVE ( 'NONE', #47642, #63538, #29736, .T. ) ;
#66047 = CARTESIAN_POINT ( 'NONE',  ( 18.11564574962620000, 0.2765170649790828494, -12.69595318831094666 ) ) ;
#66048 = AXIS2_PLACEMENT_3D ( 'NONE', #40954, #46203, #7762 ) ;
#66049 = CARTESIAN_POINT ( 'NONE',  ( 11.49056651104150006, -3.914543207408039738, -6.638028001068500217 ) ) ;
#66050 = CARTESIAN_POINT ( 'NONE',  ( 11.26072066707849828, -3.023932655881500065, -6.909591111168198907 ) ) ;
#66051 = EDGE_CURVE ( 'NONE', #45933, #59889, #39750, .T. ) ;
#66052 = EDGE_CURVE ( 'NONE', #49024, #11162, #6233, .T. ) ;
#66053 = CARTESIAN_POINT ( 'NONE',  ( 7.326301658771000369, 3.394842219570000097, 9.388954446285000088 ) ) ;
#66054 = VERTEX_POINT ( 'NONE', #34015 ) ;
#66055 =( NAMED_UNIT ( * ) PLANE_ANGLE_UNIT ( ) SI_UNIT ( $, .RADIAN. ) );
#66056 = CARTESIAN_POINT ( 'NONE',  ( 23.60205915885299888, -11.88166580723999921, 3.967996863072999147 ) ) ;
#66057 = CARTESIAN_POINT ( 'NONE',  ( 8.142152878612547440, 3.293758513149187994, 8.705677052449509290 ) ) ;
#66058 = CARTESIAN_POINT ( 'NONE',  ( 10.33022126302999943, 2.650190549566000087, -7.694579890082000162 ) ) ;
#66059 = CARTESIAN_POINT ( 'NONE',  ( 18.09858302120873574, 2.191289104517298636, 12.51814558466706195 ) ) ;
#66060 = AXIS2_PLACEMENT_3D ( 'NONE', #54618, #33993, #29104 ) ;
#66061 = CARTESIAN_POINT ( 'NONE',  ( 11.01654498872999888, 5.423831355693000233, 4.991935587166999255 ) ) ;
#66062 = CARTESIAN_POINT ( 'NONE',  ( 9.939321360490000146, 2.638097915594000309, 6.328629954376999933 ) ) ;
#66063 = CARTESIAN_POINT ( 'NONE',  ( 10.81021345716900051, -3.363461959113699606, 6.921280946186199934 ) ) ;
#66064 = CARTESIAN_POINT ( 'NONE',  ( 8.748004441081999261, 3.610923974646400136, 6.658556819429599649 ) ) ;
#66065 = ORIENTED_EDGE ( 'NONE', *, *, #44843, .T. ) ;
#66066 = CARTESIAN_POINT ( 'NONE',  ( 12.20998423544387457, -2.691370015539682914, 12.40494896326797658 ) ) ;
#66067 = CARTESIAN_POINT ( 'NONE',  ( 9.249747021775998945, -4.754947163618299832, -8.162493079567200382 ) ) ;
#66068 = CARTESIAN_POINT ( 'NONE',  ( 9.736878146978000359, 2.742182981761000171, 6.839230404018000087 ) ) ;
#66069 = CARTESIAN_POINT ( 'NONE',  ( 9.140654977342494547, 5.049579698492543400, 8.197403194024859729 ) ) ;
#66070 = CARTESIAN_POINT ( 'NONE',  ( 10.59610807141099897, 4.052703327804870526, -8.639522915742999132 ) ) ;
#66071 = CARTESIAN_POINT ( 'NONE',  ( 12.75722706473759693, -0.7178228174669247785, 12.57953618971562548 ) ) ;
#66072 = CARTESIAN_POINT ( 'NONE',  ( 8.213545280409999094, 3.608525622520999843, 5.913376237674000002 ) ) ;
#66073 = CARTESIAN_POINT ( 'NONE',  ( 11.25041981190000051, 5.730782764036999488, 8.122675980938000251 ) ) ;
#66074 = CARTESIAN_POINT ( 'NONE',  ( 12.55381283423606043, 1.927626388171776783, 12.56664888159295934 ) ) ;
#66075 = VERTEX_POINT ( 'NONE', #52401 ) ;
#66076 = CARTESIAN_POINT ( 'NONE',  ( 9.983079719591000156, 5.002683760508999988, -8.912673867568997821 ) ) ;
#66077 = CARTESIAN_POINT ( 'NONE',  ( 11.47810404293059960, 3.436653965247300047, -8.647151967355000579 ) ) ;
#66078 = CARTESIAN_POINT ( 'NONE',  ( 10.71370252004577495, -5.723616352180168398, 7.813700803284126195 ) ) ;
#66080 = CARTESIAN_POINT ( 'NONE',  ( 24.53428993882599940, 8.855929947951999281, -9.286429770520999938 ) ) ;
#66079 = CARTESIAN_POINT ( 'NONE',  ( 7.700043146791999860, -3.346260729029000291, 6.002247316312999459 ) ) ;
#66081 = CARTESIAN_POINT ( 'NONE',  ( 10.74255864497999902, -3.209241371122599773, 6.880692865553299953 ) ) ;
#66082 = B_SPLINE_CURVE_WITH_KNOTS ( 'NONE', 3,
 ( #54234, #43764, #44807, #7734 ),
 .UNSPECIFIED., .F., .F.,
 ( 4, 4 ),
 ( 0.000000000000000000, 1.000000000000000000 ),
 .UNSPECIFIED. ) ;
#66083 = CARTESIAN_POINT ( 'NONE',  ( 11.07210672858429845, -4.692204557952299737, -6.979277962544199632 ) ) ;
#66084 = ORIENTED_EDGE ( 'NONE', *, *, #2401, .T. ) ;
#66085 = AXIS2_PLACEMENT_3D ( 'NONE', #47637, #54512, #68948 ) ;
#66086 = CARTESIAN_POINT ( 'NONE',  ( 0.9240182015432000240, 1.804890371571000074, 2.911542930280999641 ) ) ;
#66087 = CARTESIAN_POINT ( 'NONE',  ( 17.80428133516622680, -0.5732558493148650625, -12.68257967785424967 ) ) ;
#66088 = EDGE_CURVE ( 'NONE', #24517, #54370, #68964, .T. ) ;
#66089 = DIRECTION ( 'NONE',  ( 0.000000000000000000, -0.9624505444715647506, 0.2714570858282915333 ) ) ;
#66090 = CARTESIAN_POINT ( 'NONE',  ( 17.75978284916825345, -3.091857219538878709, 13.52996931830918825 ) ) ;
#66091 = CARTESIAN_POINT ( 'NONE',  ( 17.80000000001300009, 3.351264566333000072, 11.15757590352999884 ) ) ;
#66092 = ADVANCED_FACE ( 'NONE', ( #61268 ), #32698, .F. ) ;
#66093 = CARTESIAN_POINT ( 'NONE',  ( 4.900006121741999898, -1.947945353336633323, -0.5234957687185524122 ) ) ;
#66094 = CARTESIAN_POINT ( 'NONE',  ( 8.477766462057999775, 2.899999999999999911, -6.558719934578999933 ) ) ;
#66095 = DIRECTION ( 'NONE',  ( 1.000000000000000000, 0.000000000000000000, 0.000000000000000000 ) ) ;
#66096 = CARTESIAN_POINT ( 'NONE',  ( 13.15534550153200044, -12.11329499872000071, -2.052871598439000245 ) ) ;
#66097 = ORIENTED_EDGE ( 'NONE', *, *, #15560, .T. ) ;
#66098 = CARTESIAN_POINT ( 'NONE',  ( 6.666501733306198219, 5.101307144762445844, -8.327526203928272253 ) ) ;
#66099 = CARTESIAN_POINT ( 'NONE',  ( 10.96087378980999993, 5.155384868709999679, 5.099797507357000548 ) ) ;
#66100 = CARTESIAN_POINT ( 'NONE',  ( 7.424920563404769247, -2.344203440956357909, 8.033218592177277628 ) ) ;
#66101 = AXIS2_PLACEMENT_3D ( 'NONE', #27296, #44425, #60487 ) ;
#66102 = CARTESIAN_POINT ( 'NONE',  ( 17.59562484692321149, -0.6250000000000004441, 13.88107975066923494 ) ) ;
#66103 = CARTESIAN_POINT ( 'NONE',  ( 0.5559723532207999641, 2.401393137604999950, -2.383704365015999915 ) ) ;
#66104 = ORIENTED_EDGE ( 'NONE', *, *, #45887, .F. ) ;
#66105 = CARTESIAN_POINT ( 'NONE',  ( 10.78170625604383659, 3.320082702567634048, -8.679590637732799152 ) ) ;
#66106 = B_SPLINE_CURVE_WITH_KNOTS ( 'NONE', 3,
 ( #67683, #62449, #35886, #57201 ),
 .UNSPECIFIED., .F., .F.,
 ( 4, 4 ),
 ( 0.000000000000000000, 1.000000000000000000 ),
 .UNSPECIFIED. ) ;
#66107 = CARTESIAN_POINT ( 'NONE',  ( 11.30000285318000230, -11.76356368987999979, -1.428410073821000159 ) ) ;
#66108 = CARTESIAN_POINT ( 'NONE',  ( 9.789752973821551407, -4.327172861449236407, 8.717426404466646517 ) ) ;
#66109 = CARTESIAN_POINT ( 'NONE',  ( 11.41256651104150066, 4.098999650273559503, 8.498573944230598087 ) ) ;
#66110 = CARTESIAN_POINT ( 'NONE',  ( 18.49993212792200126, 2.908182645667999999, 12.18276646858999968 ) ) ;
#66111 = DIRECTION ( 'NONE',  ( 1.000000000000000000, 0.000000000000000000, 0.000000000000000000 ) ) ;
#66112 = CARTESIAN_POINT ( 'NONE',  ( 10.98768472633000037, -5.449702618601000026, 4.945212061625999134 ) ) ;
#66113 = CARTESIAN_POINT ( 'NONE',  ( 12.10000669845703847, -11.02846243759423039, 3.754394857303111621 ) ) ;
#66114 = CARTESIAN_POINT ( 'NONE',  ( 12.33505003437499958, -2.912475392678309571, 12.34587402705970405 ) ) ;
#66115 = ORIENTED_EDGE ( 'NONE', *, *, #7227, .F. ) ;
#66116 = B_SPLINE_CURVE_WITH_KNOTS ( 'NONE', 3,
 ( #46663, #41411, #15527, #41066, #47002, #62385 ),
 .UNSPECIFIED., .F., .F.,
 ( 4, 2, 4 ),
 ( 0.000000000000000000, 0.5000000000000000000, 1.000000000000000000 ),
 .UNSPECIFIED. ) ;
#66117 = CARTESIAN_POINT ( 'NONE',  ( 7.891027728344822023, 2.717852728070912605, 8.706984646977891984 ) ) ;
#66118 = ORIENTED_EDGE ( 'NONE', *, *, #63681, .T. ) ;
#66119 = CARTESIAN_POINT ( 'NONE',  ( 17.83374359992753000, -3.059519611938945172, 13.53873550554769878 ) ) ;
#66120 = CARTESIAN_POINT ( 'NONE',  ( 10.61656919669529842, -2.774362666861999838, -7.862118085997298778 ) ) ;
#66121 = ORIENTED_EDGE ( 'NONE', *, *, #66836, .F. ) ;
#66122 = ORIENTED_EDGE ( 'NONE', *, *, #50834, .F. ) ;
#66123 = FACE_OUTER_BOUND ( 'NONE', #41446, .T. ) ;
#66124 = CARTESIAN_POINT ( 'NONE',  ( 5.405159358444773687, -0.6598885925774604644, -0.9208617643536302078 ) ) ;
#66125 = CARTESIAN_POINT ( 'NONE',  ( 11.57299956498156845, -2.792989229543000107, -7.825000000000000178 ) ) ;
#66126 = DIRECTION ( 'NONE',  ( -0.1218403629891999795, 1.031102794712999922E-07, 0.9925497095595008368 ) ) ;
#66127 = CARTESIAN_POINT ( 'NONE',  ( 10.60518955639999916, 5.343965917319999370, -7.731522121091999544 ) ) ;
#66128 = CARTESIAN_POINT ( 'NONE',  ( 16.39999999347100257, -3.345256695718999751, -11.86066175541999890 ) ) ;
#66129 = EDGE_CURVE ( 'NONE', #15952, #8994, #15686, .T. ) ;
#66130 = CARTESIAN_POINT ( 'NONE',  ( 11.75766493321900086, 3.377423597792000187, -11.11036430104999972 ) ) ;
#66131 = CARTESIAN_POINT ( 'NONE',  ( 9.988720925027999797, -2.842024021884000273, -6.504330542082999322 ) ) ;
#66132 = CARTESIAN_POINT ( 'NONE',  ( 11.03977792509980915, 5.161925716702778111, -8.467638888446076706 ) ) ;
#66133 = ADVANCED_FACE ( 'NONE', ( #68814 ), #11469, .F. ) ;
#66134 = ADVANCED_FACE ( 'NONE', ( #49140 ), #1251, .T. ) ;
#66135 = CARTESIAN_POINT ( 'NONE',  ( 10.41272044195154223, -3.158844023651794952, -4.969917438239939145 ) ) ;
#66136 = ORIENTED_EDGE ( 'NONE', *, *, #7760, .T. ) ;
#66137 = DIRECTION ( 'NONE',  ( 1.000000000000000000, 0.000000000000000000, 0.000000000000000000 ) ) ;
#66138 =( LENGTH_UNIT ( ) NAMED_UNIT ( * ) SI_UNIT ( .MILLI., .METRE. ) );
#66139 = CARTESIAN_POINT ( 'NONE',  ( -0.2999999999999999889, -1.154700538379000108, 0.000000000000000000 ) ) ;
#66140 = B_SPLINE_CURVE_WITH_KNOTS ( 'NONE', 3,
 ( #47505, #36671, #3468, #14658, #15343, #57991, #19558, #62874 ),
 .UNSPECIFIED., .F., .F.,
 ( 4, 2, 2, 4 ),
 ( 0.000000000000000000, 0.2499999999999985567, 0.4999999999999971134, 1.000000000000000000 ),
 .UNSPECIFIED. ) ;
#66141 = DIRECTION ( 'NONE',  ( -0.7071068187612229439, 0.000000000000000000, -0.7071067436118699812 ) ) ;
#66142 = CARTESIAN_POINT ( 'NONE',  ( 10.81499708368651369, -2.650004840405617124, -7.499999822193714749 ) ) ;
#66143 = CARTESIAN_POINT ( 'NONE',  ( 9.164757945270769923, 5.217425660116052022, 7.827174490145248242 ) ) ;
#66144 = CARTESIAN_POINT ( 'NONE',  ( 12.78422741110790284, 1.875000586273901426, 13.78627160872174251 ) ) ;
#66145 = CARTESIAN_POINT ( 'NONE',  ( 9.332935524889000689, -5.100347267927999972, 8.693464469215999912 ) ) ;
#66146 = EDGE_LOOP ( 'NONE', ( #245, #44990, #68365, #60728, #52344 ) ) ;
#66147 = CARTESIAN_POINT ( 'NONE',  ( 9.970944094204998720, 5.100000000000000533, 6.571291218949999902 ) ) ;
#66148 = CARTESIAN_POINT ( 'NONE',  ( 12.17676779642100371, 0.3651687365794410445, 13.99525266148724256 ) ) ;
#66149 = EDGE_LOOP ( 'NONE', ( #56932, #25027 ) ) ;
#66150 = CARTESIAN_POINT ( 'NONE',  ( 6.769728317542999640, 2.788803157567000035, -8.345558963038001821 ) ) ;
#66151 = CARTESIAN_POINT ( 'NONE',  ( 0.7000000000000000666, -0.5773502691895999739, -1.000000000000000000 ) ) ;
#66152 = ADVANCED_FACE ( 'NONE', ( #28523 ), #44610, .F. ) ;
#66153 = CARTESIAN_POINT ( 'NONE',  ( 23.55066277914299988, -2.916948873479999982, -13.72949264782000078 ) ) ;
#66154 = CARTESIAN_POINT ( 'NONE',  ( 8.480233239714511484, 3.061143994416841263, 6.132506423769173765 ) ) ;
#66155 = VECTOR ( 'NONE', #54093, 999.9999999999998863 ) ;
#66156 = CARTESIAN_POINT ( 'NONE',  ( 10.07367028041000090, 4.905765359186999852, -8.776126235875999271 ) ) ;
#66157 = CARTESIAN_POINT ( 'NONE',  ( 10.02101354018262569, 4.768183399968643599, -8.499583552997725278 ) ) ;
#66158 = CARTESIAN_POINT ( 'NONE',  ( 10.94936583238000161, 8.462332231760997914, -6.519047867360999504 ) ) ;
#66159 = B_SPLINE_CURVE_WITH_KNOTS ( 'NONE', 3,
 ( #20030, #9877, #63000, #62333 ),
 .UNSPECIFIED., .F., .F.,
 ( 4, 4 ),
 ( 0.000000000000000000, 1.000000000000000000 ),
 .UNSPECIFIED. ) ;
#66160 = CARTESIAN_POINT ( 'NONE',  ( 7.881386639450599141, -5.152558780658690551, 6.796436122627368626 ) ) ;
#66161 = DIRECTION ( 'NONE',  ( 1.000000000000000000, 0.000000000000000000, 0.000000000000000000 ) ) ;
#66162 = PLANE ( 'NONE',  #42245 ) ;
#66163 = CARTESIAN_POINT ( 'NONE',  ( 9.705325322606999094, -5.130141620686999637, -6.219151643305999677 ) ) ;
#66164 = CARTESIAN_POINT ( 'NONE',  ( 10.89979975933730039, 4.819074589197400726, -7.218192605361100078 ) ) ;
#66165 = DIRECTION ( 'NONE',  ( 0.000000000000000000, 0.000000000000000000, -1.000000000000000000 ) ) ;
#66166 = CARTESIAN_POINT ( 'NONE',  ( 10.98146005378009882, 4.911671201000399556, -7.013182449205100255 ) ) ;
#66167 = CARTESIAN_POINT ( 'NONE',  ( 10.06324205624999912, 3.590523439766200031, -8.565862728991998409 ) ) ;
#66169 = CARTESIAN_POINT ( 'NONE',  ( 10.68683480410999920, -2.958852069189999767, 5.111032341795000100 ) ) ;
#66168 = CARTESIAN_POINT ( 'NONE',  ( 9.393126402770999306, -3.188752782784400441, 7.805918119494599239 ) ) ;
#66170 = CARTESIAN_POINT ( 'NONE',  ( 0.000000000000000000, -2.899999999999999911, -7.500000000000000000 ) ) ;
#66171 = EDGE_LOOP ( 'NONE', ( #63014, #34441, #27792, #59924, #33883 ) ) ;
#66172 = CARTESIAN_POINT ( 'NONE',  ( 11.51656039236534923, 5.173498198882000132, 7.442888368925779652 ) ) ;
#66173 = CARTESIAN_POINT ( 'NONE',  ( 9.124702828701000357, -4.778665285493000070, 8.799745834808000211 ) ) ;
#66174 = CARTESIAN_POINT ( 'NONE',  ( 8.998468108405997867, 5.098602956001000663, 7.188863445572599709 ) ) ;
#66175 = CARTESIAN_POINT ( 'NONE',  ( 9.986774547327625484, 4.078513067950353843, -6.628582782427464792 ) ) ;
#66176 = CARTESIAN_POINT ( 'NONE',  ( 10.77962878203999963, -2.397503436487000261, 7.755423856053000442 ) ) ;
#66177 = ADVANCED_FACE ( 'NONE', ( #28167 ), #25398, .F. ) ;
#66178 = CARTESIAN_POINT ( 'NONE',  ( 9.808181774614295634, -4.356028300593894897, 9.240976368499895344 ) ) ;
#66179 = EDGE_LOOP ( 'NONE', ( #46315, #11510, #18121, #23606 ) ) ;
#66180 = CARTESIAN_POINT ( 'NONE',  ( 9.176721904869998170, -3.004358235431599855, -8.058956102599799109 ) ) ;
#66181 = AXIS2_PLACEMENT_3D ( 'NONE', #14589, #31022, #3396 ) ;
#66182 = CARTESIAN_POINT ( 'NONE',  ( 9.646013540183332680, -3.000416447002271170, -6.731816600031360842 ) ) ;
#66183 = CARTESIAN_POINT ( 'NONE',  ( 5.397505169306999306, 1.361663118425000096, -0.5499102030850999689 ) ) ;
#66184 = CARTESIAN_POINT ( 'NONE',  ( 10.84999882987999875, 12.50000000000000000, 0.000000000000000000 ) ) ;
#66185 = DIRECTION ( 'NONE',  ( 0.000000000000000000, -1.000000000000000000, 0.000000000000000000 ) ) ;
#66186 = CARTESIAN_POINT ( 'NONE',  ( 11.60948876160955479, 3.304472173606900043, -8.223320049540498999 ) ) ;
#66187 = DIRECTION ( 'NONE',  ( 0.000000000000000000, -1.000000000000000000, 0.000000000000000000 ) ) ;
#66188 = CARTESIAN_POINT ( 'NONE',  ( 9.529318513071000751, -2.297586052318000061, -7.360088033824999876 ) ) ;
#66189 = DIRECTION ( 'NONE',  ( 0.7071068156326932863, 0.000000000000000000, -0.7071067467404001938 ) ) ;
#66190 = VERTEX_POINT ( 'NONE', #41063 ) ;
#66191 = CARTESIAN_POINT ( 'NONE',  ( 9.924988015501654104, -5.349815781278972615, 7.500001845592777272 ) ) ;
#66192 = CARTESIAN_POINT ( 'NONE',  ( 12.49249577546344625, 0.5416168188285649387, -13.88579828294357554 ) ) ;
#66193 = DIRECTION ( 'NONE',  ( -1.000000000000000000, -1.776356839400000238E-14, 0.000000000000000000 ) ) ;
#66194 = CARTESIAN_POINT ( 'NONE',  ( 25.08544203593700317, -8.543220285963998961, -8.155323815290000056 ) ) ;
#66195 = CARTESIAN_POINT ( 'NONE',  ( 10.47726354018323214, -4.629523725463626782, -8.592232985442821658 ) ) ;
#66196 = CARTESIAN_POINT ( 'NONE',  ( 7.000000000000000000, 9.903195496255079888, 4.550777181346948197 ) ) ;
#66197 = CARTESIAN_POINT ( 'NONE',  ( 5.563312991732289881, 12.16892724394992875, -3.760371626685871771 ) ) ;
#66198 = ORIENTED_EDGE ( 'NONE', *, *, #63909, .T. ) ;
#66199 = DIRECTION ( 'NONE',  ( -1.000000000000000000, 0.000000000000000000, 0.000000000000000000 ) ) ;
#66200 = CARTESIAN_POINT ( 'NONE',  ( 17.99219435089537811, 2.053195051521780723, -13.75813171417237868 ) ) ;
#66201 = EDGE_LOOP ( 'NONE', ( #4848, #51408, #61138, #3437, #51809 ) ) ;
#66202 = DIRECTION ( 'NONE',  ( 0.8660254037844288266, 0.000000000000000000, -0.5000000000000169864 ) ) ;
#66203 = CARTESIAN_POINT ( 'NONE',  ( 2.748890132544458353, -2.798833948393641080, 2.150913519912190708 ) ) ;
#66204 = CARTESIAN_POINT ( 'NONE',  ( 9.939260841229000221, 5.099602161831000124, -9.049221499261999924 ) ) ;
#66205 = CARTESIAN_POINT ( 'NONE',  ( 11.58482133862618468, -3.057020944820409092, 6.626386139742057146 ) ) ;
#66206 = CARTESIAN_POINT ( 'NONE',  ( 17.74403704562415740, 1.812651413143276713, -13.88215924362446074 ) ) ;
#66207 = LINE ( 'NONE', #28126, #37053 ) ;
#66208 = DIRECTION ( 'NONE',  ( 0.000000000000000000, -1.000000000000000000, 0.000000000000000000 ) ) ;
#66209 = EDGE_LOOP ( 'NONE', ( #17423, #4303, #58844, #9714, #3340 ) ) ;
#66210 = CARTESIAN_POINT ( 'NONE',  ( 9.571967469951999874, -4.084684048989999816, 8.946621592834999248 ) ) ;
#66211 = EDGE_CURVE ( 'NONE', #13672, #24349, #55601, .T. ) ;
#66212 = EDGE_CURVE ( 'NONE', #11605, #11483, #24763, .T. ) ;
#66213 = CARTESIAN_POINT ( 'NONE',  ( 18.08671416527213438, -2.828730077929408893, -13.59817001275034443 ) ) ;
#66214 = DIRECTION ( 'NONE',  ( -1.000000000000000000, 0.000000000000000000, 0.000000000000000000 ) ) ;
#66215 = ORIENTED_EDGE ( 'NONE', *, *, #45095, .F. ) ;
#66216 = B_SPLINE_CURVE_WITH_KNOTS ( 'NONE', 3,
 ( #7722, #21456, #50373, #49325 ),
 .UNSPECIFIED., .F., .F.,
 ( 4, 4 ),
 ( 0.000000000000000000, 1.000000000000000000 ),
 .UNSPECIFIED. ) ;
#66217 = CARTESIAN_POINT ( 'NONE',  ( 10.36950244779999863, 2.719131864236000062, -7.031786688683999920 ) ) ;
#66218 = CARTESIAN_POINT ( 'NONE',  ( 3.999999855301999752, 0.000000000000000000, -2.524999655449999825 ) ) ;
#66219 = VERTEX_POINT ( 'NONE', #8903 ) ;
#66220 = CARTESIAN_POINT ( 'NONE',  ( 9.024747021775999301, 3.141778309999299967, 6.746879837742599584 ) ) ;
#66221 = CARTESIAN_POINT ( 'NONE',  ( 18.13320831056635285, -2.045970293963736975, -12.43278322311362238 ) ) ;
#66222 = CARTESIAN_POINT ( 'NONE',  ( 11.66486084871730000, -2.792989229543000107, 7.825000000000000178 ) ) ;
#66223 = CARTESIAN_POINT ( 'NONE',  ( 21.60000000000000142, 0.000000000000000000, 0.000000000000000000 ) ) ;
#66224 = CARTESIAN_POINT ( 'NONE',  ( 11.84802180303800156, -11.72322844712000034, -1.964617572541000001 ) ) ;
#66225 = B_SPLINE_CURVE_WITH_KNOTS ( 'NONE', 3,
 ( #30613, #30281, #36896, #51586, #10314, #41787, #9618, #36197, #47037, #3680, #36542, #5067, #46353, #46699, #68003, #52276, #9971, #52618, #4371, #40756, #25022, #4712 ),
 .UNSPECIFIED., .F., .F.,
 ( 4, 2, 2, 1, 2, 2, 2, 2, 1, 2, 2, 4 ),
 ( 0.000000000000000000, 0.2499999999999695799, 0.3749999999999543698, 0.4374999999999433231, 0.4687499999999412137, 0.4999999999999390488, 0.5624999999999437117, 0.6249999999999484857, 0.6874999999999531486, 0.7187499999999569233, 0.7499999999999606981, 1.000000000000000000 ),
 .UNSPECIFIED. ) ;
#66226 = CARTESIAN_POINT ( 'NONE',  ( 8.733265421555000074, 3.837285628664199866, 6.658304367510099908 ) ) ;
#66227 = CARTESIAN_POINT ( 'NONE',  ( 9.354551302391419298, -3.358410772673184219, 9.116760870204894118 ) ) ;
#66228 = VERTEX_POINT ( 'NONE', #29213 ) ;
#66229 = DIRECTION ( 'NONE',  ( 1.000000000000000000, 0.000000000000000000, 0.000000000000000000 ) ) ;
#66230 = VECTOR ( 'NONE', #21321, 1000.000000000000000 ) ;
#66231 = CARTESIAN_POINT ( 'NONE',  ( 10.35752971959000135, 5.367812128871999988, -6.514736131541999598 ) ) ;
#66232 = ADVANCED_FACE ( 'NONE', ( #51887 ), #35819, .T. ) ;
#66233 = CARTESIAN_POINT ( 'NONE',  ( 11.05073074817000034, -5.235671266423000070, -5.012833499169000007 ) ) ;
#66234 = CARTESIAN_POINT ( 'NONE',  ( 12.27426597077010051, 3.015840035300827893, -13.67132055224443477 ) ) ;
#66235 = AXIS2_PLACEMENT_3D ( 'NONE', #50612, #66333, #2714 ) ;
#66236 = CARTESIAN_POINT ( 'NONE',  ( 9.051550650638001017, 2.899999999999999911, 6.227445478845999638 ) ) ;
#66237 = EDGE_CURVE ( 'NONE', #44976, #29684, #27237, .T. ) ;
#66238 = CARTESIAN_POINT ( 'NONE',  ( 10.84168850528999961, -2.681008214828000114, 6.554752254946000889 ) ) ;
#66239 = CARTESIAN_POINT ( 'NONE',  ( 17.87656099625190009, -0.6549277419692610680, 13.98467727287826889 ) ) ;
#66240 = CARTESIAN_POINT ( 'NONE',  ( 11.29998636608000062, 3.695122995756999984, -11.25914041192000070 ) ) ;
#66241 = VERTEX_POINT ( 'NONE', #62042 ) ;
#66242 = ORIENTED_EDGE ( 'NONE', *, *, #57603, .T. ) ;
#66243 = CARTESIAN_POINT ( 'NONE',  ( 9.585279719593998493, 2.928319778732999978, -8.861178115809998701 ) ) ;
#66244 = CARTESIAN_POINT ( 'NONE',  ( 12.64261640812602039, -0.6049408601398774676, 13.88227884472451557 ) ) ;
#66245 = CARTESIAN_POINT ( 'NONE',  ( 12.20071655346993111, -2.340273578591448356, 13.70604138523078142 ) ) ;
#66246 = LINE ( 'NONE', #28517, #59590 ) ;
#66247 = CARTESIAN_POINT ( 'NONE',  ( 7.962144353208000069, -4.874569256861000177, 6.119503992241999590 ) ) ;
#66248 = CARTESIAN_POINT ( 'NONE',  ( 24.53428988874600236, -8.855929874993998752, -9.286429786912000495 ) ) ;
#66250 = CARTESIAN_POINT ( 'NONE',  ( 11.12439163055999991, -5.544976217683999842, 5.163701761329000384 ) ) ;
#66249 = CARTESIAN_POINT ( 'NONE',  ( 10.61295058442699890, -3.546800160410199965, 8.548019252390998801 ) ) ;
#66251 = VECTOR ( 'NONE', #62064, 1000.000000000000114 ) ;
#66252 = ORIENTED_EDGE ( 'NONE', *, *, #68111, .F. ) ;
#66253 = CARTESIAN_POINT ( 'NONE',  ( 25.44993529014200107, -2.258942858049999725, 11.14410496443800014 ) ) ;
#66254 = VECTOR ( 'NONE', #51871, 1000.000000000000000 ) ;
#66255 = CARTESIAN_POINT ( 'NONE',  ( 11.03298400728999873, -2.754860951861000107, -5.027234841342000493 ) ) ;
#66256 = CARTESIAN_POINT ( 'NONE',  ( 11.09999999999999964, 5.299999999999999822, 6.469505845987999493 ) ) ;
#66257 = CARTESIAN_POINT ( 'NONE',  ( 12.29147016622806809, -0.3563519072604388049, 12.69327554148123660 ) ) ;
#66258 = CARTESIAN_POINT ( 'NONE',  ( 18.15919311585273377, -2.661142132628769641, -12.41257606618384557 ) ) ;
#66259 = EDGE_LOOP ( 'NONE', ( #58074, #20111, #53389 ) ) ;
#66261 = CARTESIAN_POINT ( 'NONE',  ( 7.956354808247001031, 3.389562910887999880, -6.282406754076000688 ) ) ;
#66260 = CARTESIAN_POINT ( 'NONE',  ( 9.123558059623999128, -5.558929022707999046, 6.272984818914999927 ) ) ;
#66262 = CARTESIAN_POINT ( 'NONE',  ( 9.053070280414001303, 2.391443348526999912, -6.856688371964000162 ) ) ;
#66263 = CARTESIAN_POINT ( 'NONE',  ( 8.573148997459998810, 5.167567567567999731, -6.822293592207000934 ) ) ;
#66264 = CARTESIAN_POINT ( 'NONE',  ( 10.05862282008599884, 4.666276081381299790, 6.425317846273999933 ) ) ;
#66265 = B_SPLINE_CURVE_WITH_KNOTS ( 'NONE', 3,
 ( #27985, #44762, #55589, #65719, #18529, #50342, #23425, #45101, #22721, #66410, #49997, #49294, #65370, #7336, #39856, #13296 ),
 .UNSPECIFIED., .F., .F.,
 ( 4, 2, 2, 2, 2, 2, 2, 4 ),
 ( 0.000000000000000000, 0.06249999999999904243, 0.1249999999999980849, 0.2499999999999983347, 0.4999999999999988898, 0.7499999999999993339, 0.8749999999999996669, 1.000000000000000000 ),
 .UNSPECIFIED. ) ;
#66266 = DIRECTION ( 'NONE',  ( 1.000000000000000000, 0.000000000000000000, 0.000000000000000000 ) ) ;
#66267 = CARTESIAN_POINT ( 'NONE',  ( 9.456592480104376364, 2.253870038478822391, 7.362952920305176008 ) ) ;
#66268 = CARTESIAN_POINT ( 'NONE',  ( 3.533037658052000207, 1.664759391734999872, -3.022254788923000035 ) ) ;
#66269 = EDGE_LOOP ( 'NONE', ( #62635, #52454, #13328, #43086 ) ) ;
#66270 = CARTESIAN_POINT ( 'NONE',  ( 12.22921692136009320, 0.4376617689587208315, -12.59240970319242514 ) ) ;
#66271 = CARTESIAN_POINT ( 'NONE',  ( 7.806992724014596874, -3.016426643082999792, 6.525734047976322394 ) ) ;
#66272 = CARTESIAN_POINT ( 'NONE',  ( 11.04230989604436530, -2.757690103955632743, 6.361542621298440281 ) ) ;
#66273 = CARTESIAN_POINT ( 'NONE',  ( 24.66122485234200212, 3.625879222137000202, -12.20767898207999913 ) ) ;
#66274 = EDGE_LOOP ( 'NONE', ( #31991, #58, #13550, #64112 ) ) ;
#66275 = CARTESIAN_POINT ( 'NONE',  ( 6.429134283178000508, -1.251891003439999928, -0.4257286625704000405 ) ) ;
#66276 = CARTESIAN_POINT ( 'NONE',  ( 7.888385841225999506, 2.869384229876999814, -6.678559560168999987 ) ) ;
#66278 = CARTESIAN_POINT ( 'NONE',  ( 24.67921321800200118, -8.727630028894999725, 9.158313644156001132 ) ) ;
#66277 = DIRECTION ( 'NONE',  ( 0.000000000000000000, -0.9659258262890756397, 0.2588190451024932059 ) ) ;
#66279 = CARTESIAN_POINT ( 'NONE',  ( 10.40299135172147693, -3.204747416617449218, -7.137146156348714854 ) ) ;
#66280 = ORIENTED_EDGE ( 'NONE', *, *, #25394, .T. ) ;
#66281 = VECTOR ( 'NONE', #34180, 1000.000000000000000 ) ;
#66282 = DIRECTION ( 'NONE',  ( 1.000000000000000000, 0.000000000000000000, 0.000000000000000000 ) ) ;
#66283 = ORIENTED_EDGE ( 'NONE', *, *, #35752, .T. ) ;
#66284 = CARTESIAN_POINT ( 'NONE',  ( 9.517712236484261012, -4.527663441039016412, 8.747762430587503246 ) ) ;
#66285 = CARTESIAN_POINT ( 'NONE',  ( 24.94502883495008305, -8.558261254986113897, -8.385775660771827233 ) ) ;
#66286 = CARTESIAN_POINT ( 'NONE',  ( 18.27393099755801487, -0.09542514088231193736, -13.99967976774382272 ) ) ;
#66287 = ORIENTED_EDGE ( 'NONE', *, *, #17260, .T. ) ;
#66288 = CARTESIAN_POINT ( 'NONE',  ( 7.643638571636000023, -9.072798860549999844, 5.701353631702000158 ) ) ;
#66289 = CARTESIAN_POINT ( 'NONE',  ( 10.15000066238999921, -1.714184350020999865E-13, 8.688602249551999193E-14 ) ) ;
#66290 = PLANE ( 'NONE',  #20325 ) ;
#66291 = DIRECTION ( 'NONE',  ( 0.000000000000000000, -1.000000000000000000, 0.000000000000000000 ) ) ;
#66292 = FACE_OUTER_BOUND ( 'NONE', #19355, .T. ) ;
#66293 = EDGE_LOOP ( 'NONE', ( #25711, #24539, #22735 ) ) ;
#66294 = CARTESIAN_POINT ( 'NONE',  ( 9.472537864290000442, 2.899999999999999911, -6.571291218949999902 ) ) ;
#66295 = EDGE_CURVE ( 'NONE', #11762, #33164, #51214, .T. ) ;
#66296 = EDGE_CURVE ( 'NONE', #43345, #5638, #39755, .T. ) ;
#66297 = CARTESIAN_POINT ( 'NONE',  ( 23.68315609214200279, -13.13569427494999964, -3.949142898887999742 ) ) ;
#66298 = CARTESIAN_POINT ( 'NONE',  ( 9.696013540182335078, 4.999583552997727054, 8.268183399968641822 ) ) ;
#66299 = CONICAL_SURFACE ( 'NONE', #29497, 12.49999584805000019, 0.7853981146832407223 ) ;
#66300 = CARTESIAN_POINT ( 'NONE',  ( 12.75598008708079512, -3.248071441111094693, 13.61800396221869391 ) ) ;
#66301 = ORIENTED_EDGE ( 'NONE', *, *, #39099, .F. ) ;
#66302 = CARTESIAN_POINT ( 'NONE',  ( 10.51293113580700123, -5.100000000000000533, 6.444141223116233164 ) ) ;
#66303 = CONICAL_SURFACE ( 'NONE', #59618, 13.94999927503000059, 0.7853981058017837080 ) ;
#66304 = CARTESIAN_POINT ( 'NONE',  ( 10.93870578215442713, -2.832454552556203708, -6.732216691000727060 ) ) ;
#66305 = DIRECTION ( 'NONE',  ( -1.000000000000000000, 5.085933197601780420E-15, -5.275114267344730344E-15 ) ) ;
#66306 = CARTESIAN_POINT ( 'NONE',  ( 10.02145237372899800, -3.956267952212241479, -8.774080944853649200 ) ) ;
#66307 = DIRECTION ( 'NONE',  ( 1.000000000000000000, 0.000000000000000000, 0.000000000000000000 ) ) ;
#66308 = CARTESIAN_POINT ( 'NONE',  ( 12.20981157025896735, -0.1908382484571562454, -13.89824168789394854 ) ) ;
#66309 = CARTESIAN_POINT ( 'NONE',  ( 17.96930180488791606, -2.968443477542578979, 12.33001868694671010 ) ) ;
#66310 = ORIENTED_EDGE ( 'NONE', *, *, #49735, .F. ) ;
#66311 = CARTESIAN_POINT ( 'NONE',  ( 10.37199293566600034, -3.366612813978900220, -8.276990458557699881 ) ) ;
#66312 = ORIENTED_EDGE ( 'NONE', *, *, #43168, .F. ) ;
#66313 = CARTESIAN_POINT ( 'NONE',  ( 17.72017830080754663, 1.875000000000000000, 13.78627079974493164 ) ) ;
#66314 = CARTESIAN_POINT ( 'NONE',  ( 9.775320280412000074, 2.527713920559999661, -6.969421869128999525 ) ) ;
#66315 = B_SPLINE_CURVE_WITH_KNOTS ( 'NONE', 3,
 ( #34821, #44968, #66272, #13157 ),
 .UNSPECIFIED., .F., .F.,
 ( 4, 4 ),
 ( 0.000000000000000000, 1.000000000000000000 ),
 .UNSPECIFIED. ) ;
#66316 = CARTESIAN_POINT ( 'NONE',  ( 2.964245321877999828, 0.1669473377653999946, 3.375257869341000028 ) ) ;
#66317 = EDGE_CURVE ( 'NONE', #23033, #34088, #35543, .T. ) ;
#66318 = CARTESIAN_POINT ( 'NONE',  ( 10.02800210979000184, -3.452027005875999865, -6.074520565702999697 ) ) ;
#66319 = CARTESIAN_POINT ( 'NONE',  ( 6.887676285888210792, 1.390704803993308092, 0.6075771062923210897 ) ) ;
#66320 = DIRECTION ( 'NONE',  ( -0.7071067811865150432, -0.1740570546198035029, -0.6853496492573148968 ) ) ;
#66321 = CARTESIAN_POINT ( 'NONE',  ( 10.34271159708237242, -5.100000000000000533, -6.305985890001590377 ) ) ;
#66322 = EDGE_LOOP ( 'NONE', ( #58997, #788, #27651, #45307 ) ) ;
#66323 = CARTESIAN_POINT ( 'NONE',  ( 12.13410404293056999, -4.442327784369100030, 6.599279737936000423 ) ) ;
#66324 = CARTESIAN_POINT ( 'NONE',  ( 10.09696969267000100, 5.253376380222999131, 8.530663119653999260 ) ) ;
#66325 = CARTESIAN_POINT ( 'NONE',  ( 10.63590686542660890, -5.314851119339436103, -7.853271763851031650 ) ) ;
#66326 = DIRECTION ( 'NONE',  ( -1.055605809059559446E-16, 0.9835354258236025382, -0.1807154286440004198 ) ) ;
#66327 = CARTESIAN_POINT ( 'NONE',  ( 9.217201318830829493, 2.656563516783068124, 7.632949642608349627 ) ) ;
#66328 = AXIS2_PLACEMENT_3D ( 'NONE', #18971, #8822, #62304 ) ;
#66329 = CARTESIAN_POINT ( 'NONE',  ( 11.51102763632551884, 3.088851714329700293, -7.079572058049399708 ) ) ;
#66330 = FACE_OUTER_BOUND ( 'NONE', #55196, .T. ) ;
#66331 = CARTESIAN_POINT ( 'NONE',  ( 9.705671671056999017, 3.009461603020800347, -7.666361006367900188 ) ) ;
#66332 = CARTESIAN_POINT ( 'NONE',  ( 18.13005353941770181, -0.4382646521645844340, 12.59237917444261434 ) ) ;
#66333 = DIRECTION ( 'NONE',  ( -1.000000000000000000, 0.000000000000000000, 0.000000000000000000 ) ) ;
#66334 = CARTESIAN_POINT ( 'NONE',  ( 8.100037824936533681, 5.084629185201427148, -6.579660631752214606 ) ) ;
#66335 = CARTESIAN_POINT ( 'NONE',  ( 10.75102028041000146, 2.478469530773999896, -7.438303846328000013 ) ) ;
#66336 = ORIENTED_EDGE ( 'NONE', *, *, #36928, .T. ) ;
#66337 = CARTESIAN_POINT ( 'NONE',  ( 7.539230646792000279, -4.696237245142999228, 5.830277424166999900 ) ) ;
#66338 = CARTESIAN_POINT ( 'NONE',  ( 17.79045811871160865, 1.826948899878884314, 13.88028486463507249 ) ) ;
#66339 = CARTESIAN_POINT ( 'NONE',  ( 23.89320776801300283, -1.894218448783000941, 11.32736289219000270 ) ) ;
#66340 = DIRECTION ( 'NONE',  ( 0.000000000000000000, 0.8648648648648720183, 0.5020047465136825426 ) ) ;
#66341 = VERTEX_POINT ( 'NONE', #18714 ) ;
#66342 = AXIS2_PLACEMENT_3D ( 'NONE', #36550, #51593, #62085 ) ;
#66343 = CARTESIAN_POINT ( 'NONE',  ( 17.79284288850699980, 3.413161633892000335, 11.89755489758000095 ) ) ;
#66344 = VECTOR ( 'NONE', #20540, 1000.000000000000000 ) ;
#66346 = CARTESIAN_POINT ( 'NONE',  ( 0.5294218405026995811, 3.414111695701551152, -0.9298589507122824172 ) ) ;
#66345 = CARTESIAN_POINT ( 'NONE',  ( 10.21924205624999971, -4.310927436352299580, -8.309340504471899536 ) ) ;
#66347 = CARTESIAN_POINT ( 'NONE',  ( 10.56983915876999980, 2.152856944368999770, -7.425100664021000441 ) ) ;
#66348 = EDGE_CURVE ( 'NONE', #25719, #6927, #56343, .T. ) ;
#66349 = EDGE_LOOP ( 'NONE', ( #2955, #65320, #48934, #44948 ) ) ;
#66350 = EDGE_CURVE ( 'NONE', #30029, #52567, #30920, .T. ) ;
#66351 = CARTESIAN_POINT ( 'NONE',  ( 11.11504246380000005, 3.456610836627000083, 5.970339330302000036 ) ) ;
#66353 = CARTESIAN_POINT ( 'NONE',  ( 9.393246442089999704, -5.100000000000000533, -6.421387671005999387 ) ) ;
#66352 = B_SPLINE_CURVE_WITH_KNOTS ( 'NONE', 3,
 ( #1510, #11997, #1859, #12693, #59888, #33680, #33334, #65472, #38924, #1166, #22481, #34030, #55343, #60245, #43823, #54998, #64776, #64427 ),
 .UNSPECIFIED., .F., .F.,
 ( 4, 2, 2, 2, 2, 2, 2, 2, 4 ),
 ( 0.000000000000000000, 0.1250000000000000000, 0.2500000000000000000, 0.3750000000000000000, 0.5000000000000000000, 0.6250000000000000000, 0.7500000000000000000, 0.8750000000000000000, 1.000000000000000000 ),
 .UNSPECIFIED. ) ;
#66354 = CARTESIAN_POINT ( 'NONE',  ( 11.23610538575739959, 5.109472165990999848, 7.765257665594799796 ) ) ;
#66355 = CARTESIAN_POINT ( 'NONE',  ( 9.465112865370999273, -2.290047720994000002, 6.601709978349000529 ) ) ;
#66356 = DIRECTION ( 'NONE',  ( 0.000000000000000000, -1.000000000000000000, 0.000000000000000000 ) ) ;
#66357 = EDGE_LOOP ( 'NONE', ( #23143, #21548, #50962, #67666 ) ) ;
#66358 = DIRECTION ( 'NONE',  ( 0.000000000000000000, -1.000000000000000000, 0.000000000000000000 ) ) ;
#66359 = CARTESIAN_POINT ( 'NONE',  ( 10.69015444038000062, -4.391267940138999570, -8.802346922965000431 ) ) ;
#66360 = CARTESIAN_POINT ( 'NONE',  ( 7.915661401038873279, -2.416848911730535399, 8.220850438606255750 ) ) ;
#66361 = CARTESIAN_POINT ( 'NONE',  ( 11.02786767503999954, -5.596230239120999705, 7.209501483790000442 ) ) ;
#66362 = CARTESIAN_POINT ( 'NONE',  ( 11.01279632507519857, -3.375091146194399983, -8.658468685623999406 ) ) ;
#66363 = CARTESIAN_POINT ( 'NONE',  ( 10.66455864497999961, -3.101067942814400347, 6.795973491698399371 ) ) ;
#66364 = ORIENTED_EDGE ( 'NONE', *, *, #41136, .F. ) ;
#66365 = CARTESIAN_POINT ( 'NONE',  ( 19.89999890908300273, 0.000000000000000000, 0.000000000000000000 ) ) ;
#66366 = CARTESIAN_POINT ( 'NONE',  ( 11.36687616594229944, -4.344946439135400240, 8.587337146608000182 ) ) ;
#66367 = ORIENTED_EDGE ( 'NONE', *, *, #6736, .T. ) ;
#66368 = DIRECTION ( 'NONE',  ( -3.667764737047155134E-10, 0.9466472399347399813, -0.3222716294121134584 ) ) ;
#66369 = ORIENTED_EDGE ( 'NONE', *, *, #38570, .F. ) ;
#66370 = CARTESIAN_POINT ( 'NONE',  ( 10.00107860442999907, -4.626219091573998909, -9.027249334595000008 ) ) ;
#66371 = CARTESIAN_POINT ( 'NONE',  ( 8.323770280408998801, 5.332332124071999857, -8.487089944253000340 ) ) ;
#66372 = CARTESIAN_POINT ( 'NONE',  ( 11.26212378248529866, 3.384904051819500381, -6.336291382830999908 ) ) ;
#66373 = CARTESIAN_POINT ( 'NONE',  ( -15.86200481174999943, 5.599999999999999645, 6.571291218949999902 ) ) ;
#66374 = CARTESIAN_POINT ( 'NONE',  ( 12.66183496498643635, 1.891282299343450379, -12.57277654391869071 ) ) ;
#66375 = CARTESIAN_POINT ( 'NONE',  ( 11.95764291764649911, -5.132124077409000229, 7.639947095788999221 ) ) ;
#66376 = CARTESIAN_POINT ( 'NONE',  ( 11.64767835872009982, -4.874341053673500568, 8.051056647135798272 ) ) ;
#66377 = EDGE_CURVE ( 'NONE', #7211, #60567, #58509, .T. ) ;
#66378 = ORIENTED_EDGE ( 'NONE', *, *, #54837, .F. ) ;
#66379 = FACE_OUTER_BOUND ( 'NONE', #36967, .T. ) ;
#66380 = AXIS2_PLACEMENT_3D ( 'NONE', #45480, #33955, #18909 ) ;
#66381 = ADVANCED_FACE ( 'NONE', ( #37190 ), #36500, .F. ) ;
#66382 = ORIENTED_EDGE ( 'NONE', *, *, #24482, .F. ) ;
#66383 = CARTESIAN_POINT ( 'NONE',  ( 9.112168146794999757, -2.368260286481999710, 7.410200011629000549 ) ) ;
#66384 = CARTESIAN_POINT ( 'NONE',  ( 17.64997652428802510, 0.7254930141063502536, 13.98119259374222700 ) ) ;
#66385 = VERTEX_POINT ( 'NONE', #16205 ) ;
#66386 = B_SPLINE_SURFACE_WITH_KNOTS ( 'NONE', 3, 3, ( 
 ( #38036, #21611, #6216, #64254 ),
 ( #32461, #60062, #54117, #64597 ),
 ( #37696, #64938, #33151, #5535 ),
 ( #17052, #47856, #27909, #38384 ),
 ( #59025, #65293, #17410, #11810 ),
 ( #54466, #58677, #11129, #32803 ),
 ( #1326, #22644, #53777, #38734 ),
 ( #69163, #16023, #12167, #5874 ),
 ( #10776, #33498, #54812, #26528 ),
 ( #27212, #21272, #53439, #63913 ) ),
 .UNSPECIFIED., .F., .F., .F.,
 ( 4, 1, 1, 1, 1, 1, 1, 4 ),
 ( 4, 4 ),
 ( 0.07063076901675000019, 0.1428571428570999946, 0.2857142857143000203, 0.4285714285713999594, 0.5714285714286000406, 0.7142857142856999797, 0.8571428571429000609, 0.9582423226859000387 ),
 ( -0.1917799910644999994, 1.191756862851000021 ),
 .UNSPECIFIED. ) ;
#66387 = CARTESIAN_POINT ( 'NONE',  ( 12.56929374240178987, -1.799893664886396349, -12.47078182885977604 ) ) ;
#66388 = CARTESIAN_POINT ( 'NONE',  ( 11.11302897915239818, 4.291996373817799970, 6.397263297997000109 ) ) ;
#66389 = CARTESIAN_POINT ( 'NONE',  ( 10.64557055961999943, -2.988935764546999607, -5.952339209104000162 ) ) ;
#66390 = CARTESIAN_POINT ( 'NONE',  ( 13.00000000000000178, 50.50083396221999976, 7.800765400072998901 ) ) ;
#66391 = CARTESIAN_POINT ( 'NONE',  ( 25.60000000000000142, 0.000000000000000000, 0.000000000000000000 ) ) ;
#66392 = CARTESIAN_POINT ( 'NONE',  ( 24.56046482358600258, -8.848342285144999764, 9.332993723418001153 ) ) ;
#66393 = CARTESIAN_POINT ( 'NONE',  ( 12.18091821863274049, -2.461361028094613435, -13.68154568029715179 ) ) ;
#66394 = CARTESIAN_POINT ( 'NONE',  ( 18.05145864173985260, -0.3802890292809140704, -12.69234946364261241 ) ) ;
#66395 = CYLINDRICAL_SURFACE ( 'NONE', #50871, 1.250000000000000222 ) ;
#66396 = CARTESIAN_POINT ( 'NONE',  ( 11.42887348028849992, -5.124210964533999935, -8.107837221875000111 ) ) ;
#66397 = CARTESIAN_POINT ( 'NONE',  ( 8.866801658774001282, 2.550580605805000012, 8.854682662413999594 ) ) ;
#66398 = ORIENTED_EDGE ( 'NONE', *, *, #24889, .T. ) ;
#66399 = AXIS2_PLACEMENT_3D ( 'NONE', #6117, #52996, #196 ) ;
#66400 = CARTESIAN_POINT ( 'NONE',  ( 10.98768472639999949, 5.139096889661000311, -4.945212061661000469 ) ) ;
#66401 = LINE ( 'NONE', #60131, #32778 ) ;
#66402 = CARTESIAN_POINT ( 'NONE',  ( 10.13381533919000077, 5.176445833090999926, -8.189798585019000043 ) ) ;
#66403 = B_SPLINE_CURVE_WITH_KNOTS ( 'NONE', 3,
 ( #31480, #52803, #10831, #32175, #32855, #17465, #6967, #1380, #33895, #342 ),
 .UNSPECIFIED., .F., .F.,
 ( 4, 2, 2, 2, 4 ),
 ( 0.1253320266324779719, 0.3126457153657128396, 0.4999594040989477906, 0.6872730928321826305, 0.8745867815654175814 ),
 .UNSPECIFIED. ) ;
#66404 = ADVANCED_FACE ( 'NONE', ( #473 ), #32554, .F. ) ;
#66405 = VECTOR ( 'NONE', #49427, 1000.000000000000000 ) ;
#66406 = CARTESIAN_POINT ( 'NONE',  ( 17.71825832218063468, 1.896331189961580455, 12.57190091395960607 ) ) ;
#66407 = CARTESIAN_POINT ( 'NONE',  ( 18.23590051321700400, 3.219096189435000088, -11.95421454054999977 ) ) ;
#66408 = CARTESIAN_POINT ( 'NONE',  ( 9.877261637240000169, 2.207988120125000009, 7.624813826992999921 ) ) ;
#66409 = CARTESIAN_POINT ( 'NONE',  ( 9.473608660036624940, -3.779042157900793786, 8.346587208109317757 ) ) ;
#66410 = CARTESIAN_POINT ( 'NONE',  ( 12.07990771228650750, 0.1878083608151937256, -12.60000737103648660 ) ) ;
#66411 = ORIENTED_EDGE ( 'NONE', *, *, #59364, .T. ) ;
#66412 = CARTESIAN_POINT ( 'NONE',  ( 12.22227632225713734, -2.273941840405719006, 12.50139599066422846 ) ) ;
#66413 = CARTESIAN_POINT ( 'NONE',  ( 9.906292290062998163, -3.250213325543700016, -7.064651992867799990 ) ) ;
#66414 = CARTESIAN_POINT ( 'NONE',  ( 10.70441484796999987, 3.444517850837000239, 6.009055070331999815 ) ) ;
#66415 = CARTESIAN_POINT ( 'NONE',  ( 12.34388784977539899, -5.255745690988000263, 7.571757098260779806 ) ) ;
#66416 = CARTESIAN_POINT ( 'NONE',  ( 10.79303032197930001, 4.663532080728800544, -6.572090902022299730 ) ) ;
#66417 = CARTESIAN_POINT ( 'NONE',  ( 12.39285676950935766, 0.4699213205053948128, 12.68829855189361844 ) ) ;
#66418 = CARTESIAN_POINT ( 'NONE',  ( 8.930989158774000458, 2.019067547072999957, 7.390982789861999969 ) ) ;
#66419 = B_SPLINE_CURVE_WITH_KNOTS ( 'NONE', 3,
 ( #909, #5108, #32385, #36937, #31690, #58942, #53698, #64511 ),
 .UNSPECIFIED., .F., .F.,
 ( 4, 2, 2, 4 ),
 ( 0.4992598756095557033, 0.7496299378047774908, 0.8748149689023887454, 1.000000000000000000 ),
 .UNSPECIFIED. ) ;
#66420 = DIRECTION ( 'NONE',  ( -1.000000000000000000, 2.664535259100999844E-14, -3.552713678802000396E-14 ) ) ;
#66421 = CARTESIAN_POINT ( 'NONE',  ( 12.18001225342674232, 2.492635468222105022, 12.45327835951381168 ) ) ;
#66422 = ORIENTED_EDGE ( 'NONE', *, *, #45423, .T. ) ;
#66423 = CARTESIAN_POINT ( 'NONE',  ( 8.798539158775000146, 5.851083642416999631, -7.072167224702999633 ) ) ;
#66424 = CARTESIAN_POINT ( 'NONE',  ( 10.78887616594230003, 3.613544262574699850, -6.281817606595999415 ) ) ;
#66425 = CARTESIAN_POINT ( 'NONE',  ( 10.79668711518602464, -4.601537912553735232, 9.136927527625404721 ) ) ;
#66427 = CARTESIAN_POINT ( 'NONE',  ( 25.12926878881309989, 11.33915774497326012, 3.290756510447234273 ) ) ;
#66426 = CARTESIAN_POINT ( 'NONE',  ( 8.020980646792999380, -3.245532552444000185, 8.949627348471000943 ) ) ;
#66428 = CARTESIAN_POINT ( 'NONE',  ( 10.05867167105700055, -4.990538396979200542, 7.333638993632098924 ) ) ;
#66429 = CARTESIAN_POINT ( 'NONE',  ( 10.70287750876920008, -4.469200303112399908, -8.228113772635300194 ) ) ;
#66430 = ORIENTED_EDGE ( 'NONE', *, *, #29372, .F. ) ;
#66431 = CARTESIAN_POINT ( 'NONE',  ( 0.9669268129214999563, 3.284885639805000146, 1.453889781857000019 ) ) ;
#66432 = CARTESIAN_POINT ( 'NONE',  ( 18.05193840052253407, -0.3791517837728508589, -12.69238281682625136 ) ) ;
#66433 = AXIS2_PLACEMENT_3D ( 'NONE', #29935, #31295, #67989 ) ;
#66434 = CARTESIAN_POINT ( 'NONE',  ( 24.67921321864300310, 12.29514728640000065, 2.979192498689000157 ) ) ;
#66435 = CARTESIAN_POINT ( 'NONE',  ( 17.93700172732586395, -2.995132885274008228, 13.55589876081949186 ) ) ;
#66436 = EDGE_CURVE ( 'NONE', #6658, #20386, #56462, .T. ) ;
#66437 = ADVANCED_FACE ( 'NONE', ( #6398 ), #27748, .F. ) ;
#66438 = CARTESIAN_POINT ( 'NONE',  ( 24.62774583285700203, -12.19917312477000060, 3.045379866084000131 ) ) ;
#66439 = CARTESIAN_POINT ( 'NONE',  ( 17.65854462812411185, -1.883284865257428775, -13.78503182716600683 ) ) ;
#66440 = CARTESIAN_POINT ( 'NONE',  ( 0.1499996298882999846, -2.250000000000000000, 0.000000000000000000 ) ) ;
#66441 = CARTESIAN_POINT ( 'NONE',  ( 1.700000000000000178, 0.000000000000000000, 0.000000000000000000 ) ) ;
#66442 = CARTESIAN_POINT ( 'NONE',  ( 23.71897700387453511, 13.13847632678408495, 3.829971267513319511 ) ) ;
#66443 = ORIENTED_EDGE ( 'NONE', *, *, #28518, .F. ) ;
#66444 = ADVANCED_FACE ( 'NONE', ( #12347 ), #49060, .T. ) ;
#66445 = CARTESIAN_POINT ( 'NONE',  ( 8.020982780409999791, 3.245534453799999941, 8.949623695221001540 ) ) ;
#66446 = CARTESIAN_POINT ( 'NONE',  ( 23.56665676678100141, -2.935523947847999970, 13.67844066972000050 ) ) ;
#66447 = CARTESIAN_POINT ( 'NONE',  ( 18.05387017991211707, 2.121311586892751677, -13.74657283404811992 ) ) ;
#66448 = LINE ( 'NONE', #24498, #59355 ) ;
#66449 = CARTESIAN_POINT ( 'NONE',  ( 1.938748887005000032, -2.269833785962000139, -2.784166953248000009 ) ) ;
#66450 = ORIENTED_EDGE ( 'NONE', *, *, #34465, .F. ) ;
#66451 = CARTESIAN_POINT ( 'NONE',  ( 10.75046352948212380, 3.823292445202991274, -8.850187295431105383 ) ) ;
#66452 = CARTESIAN_POINT ( 'NONE',  ( 10.65165493200484370, -5.052088798245987000, 5.056974862721875574 ) ) ;
#66453 = CARTESIAN_POINT ( 'NONE',  ( 10.55813337864000090, 2.466561068647000532, 6.633529813744000414 ) ) ;
#66454 = AXIS2_PLACEMENT_3D ( 'NONE', #31245, #52552, #27366 ) ;
#66455 = CARTESIAN_POINT ( 'NONE',  ( 10.87103032197929942, 4.583685623598699799, 8.316248703309600643 ) ) ;
#66456 = CARTESIAN_POINT ( 'NONE',  ( 7.921841810112000282, 2.875629839593000003, -6.725486766668000271 ) ) ;
#66457 = CARTESIAN_POINT ( 'NONE',  ( 10.84160444037999937, -2.641264320582999758, -7.444904971031999885 ) ) ;
#66458 = DIRECTION ( 'NONE',  ( -1.000000000000000000, 0.000000000000000000, 0.000000000000000000 ) ) ;
#66459 = CARTESIAN_POINT ( 'NONE',  ( 24.25375554908000097, 12.19812635653999955, 3.308082274583000526 ) ) ;
#66460 = CARTESIAN_POINT ( 'NONE',  ( 12.42339251327461369, -2.995356603774978144, 12.32227076303473368 ) ) ;
#66461 = CARTESIAN_POINT ( 'NONE',  ( 8.077529320371693800, 4.037993861317246136, 5.758221802075652818 ) ) ;
#66462 = EDGE_LOOP ( 'NONE', ( #34971, #25455, #41365, #40992 ) ) ;
#66463 = CARTESIAN_POINT ( 'NONE',  ( 18.27395862148971162, -2.614931059283422954, 13.75364391642198747 ) ) ;
#66464 = CARTESIAN_POINT ( 'NONE',  ( 10.41964694612699915, -5.186980343482999523, -7.973702485506099613 ) ) ;
#66465 = ORIENTED_EDGE ( 'NONE', *, *, #58412, .F. ) ;
#66466 = CARTESIAN_POINT ( 'NONE',  ( 8.784678295047998020, 4.000000000000000000, 7.500000000000000000 ) ) ;
#66467 = CARTESIAN_POINT ( 'NONE',  ( 10.28014141025500017, 4.417352327511700594, 6.756653759087999589 ) ) ;
#66468 = CARTESIAN_POINT ( 'NONE',  ( 9.739763540183334456, 3.672815144550903632, -6.282534154164605589 ) ) ;
#66469 = CARTESIAN_POINT ( 'NONE',  ( 20.75138802851920161, 0.000000000000000000, 0.000000000000000000 ) ) ;
#66470 = FACE_OUTER_BOUND ( 'NONE', #28294, .T. ) ;
#66471 = CARTESIAN_POINT ( 'NONE',  ( 10.90634530628000043, 3.089682683751000081, -6.534327427410000055 ) ) ;
#66472 = CARTESIAN_POINT ( 'NONE',  ( 8.060840674114759352, -9.103590313266881395, -5.835422151730319307 ) ) ;
#66473 = DIRECTION ( 'NONE',  ( 0.000000000000000000, 1.000000000000000000, 0.000000000000000000 ) ) ;
#66474 = CARTESIAN_POINT ( 'NONE',  ( 11.53971429488000133, 3.572666839320000065, -11.04878221693000029 ) ) ;
#66475 = CARTESIAN_POINT ( 'NONE',  ( 23.57777266354770873, -13.28347985581029356, -4.287254563653999817 ) ) ;
#66476 = CARTESIAN_POINT ( 'NONE',  ( 11.68333460557258796, -3.837988184179999873, -8.490304555719900392 ) ) ;
#66477 = AXIS2_PLACEMENT_3D ( 'NONE', #16953, #65540, #19030 ) ;
#66478 = CARTESIAN_POINT ( 'NONE',  ( 5.520886616771333522, -1.393043258182025346, 0.6426200619446648110 ) ) ;
#66479 = ORIENTED_EDGE ( 'NONE', *, *, #15779, .F. ) ;
#66480 = FACE_OUTER_BOUND ( 'NONE', #49346, .T. ) ;
#66481 = CARTESIAN_POINT ( 'NONE',  ( 10.90000668870999867, -1.199999999999999956, -11.27663029882999801 ) ) ;
#66482 = EDGE_CURVE ( 'NONE', #44634, #28703, #68820, .T. ) ;
#66483 = CARTESIAN_POINT ( 'NONE',  ( 10.76290585702731661, -2.920651757519954650, -8.329491109684262540 ) ) ;
#66484 = CARTESIAN_POINT ( 'NONE',  ( 10.41891290906799838, 3.190593056227700064, -8.490578012456198920 ) ) ;
#66485 = CARTESIAN_POINT ( 'NONE',  ( 12.56988000877536749, 3.209076157321550049, 13.62724777954567656 ) ) ;
#66486 = CARTESIAN_POINT ( 'NONE',  ( 10.48164908029000131, -4.022873587130999518, 9.090901241422999490 ) ) ;
#66487 = ORIENTED_EDGE ( 'NONE', *, *, #50582, .F. ) ;
#66488 = EDGE_CURVE ( 'NONE', #36042, #16713, #40471, .T. ) ;
#66489 = B_SPLINE_CURVE_WITH_KNOTS ( 'NONE', 3,
 ( #3459, #51701, #46122, #24797 ),
 .UNSPECIFIED., .F., .F.,
 ( 4, 4 ),
 ( 0.000000000000000000, 1.000000000000000000 ),
 .UNSPECIFIED. ) ;
#66490 = CARTESIAN_POINT ( 'NONE',  ( 12.38195926868453789, 0.4608195498121803735, -12.68876479732302265 ) ) ;
#66491 = CARTESIAN_POINT ( 'NONE',  ( 12.12622056954396221, 0.2566959043864855405, 13.99765098363215365 ) ) ;
#66492 = VERTEX_POINT ( 'NONE', #49399 ) ;
#66493 = DIRECTION ( 'NONE',  ( 0.8480635683783692702, 0.3746919961710865610, -0.3746919961710865610 ) ) ;
#66494 = CARTESIAN_POINT ( 'NONE',  ( 12.80505043854144276, -0.7192913403693027563, 12.57945229203838267 ) ) ;
#66495 = CARTESIAN_POINT ( 'NONE',  ( 24.32732080885899961, -3.577499572665000294, -12.48500538494000089 ) ) ;
#66496 = CARTESIAN_POINT ( 'NONE',  ( 8.510694764413049285, 3.299154217465439132, 5.962358501161194368 ) ) ;
#66497 = AXIS2_PLACEMENT_3D ( 'NONE', #44618, #27842, #43568 ) ;
#66498 = AXIS2_PLACEMENT_3D ( 'NONE', #40076, #18401, #10607 ) ;
#66499 = CARTESIAN_POINT ( 'NONE',  ( 6.799999999999999822, -10.75000000000000000, 0.000000000000000000 ) ) ;
#66500 = CARTESIAN_POINT ( 'NONE',  ( 11.12554667867999925, 8.127034475866000918, -6.768926555484000573 ) ) ;
#66501 = CARTESIAN_POINT ( 'NONE',  ( 0.4745747022587999409, -0.8195100712853999880, -3.441407140921999730 ) ) ;
#66502 = DIRECTION ( 'NONE',  ( 0.000000000000000000, -0.000000000000000000, 1.000000000000000000 ) ) ;
#66503 = CARTESIAN_POINT ( 'NONE',  ( 12.40985643288212614, 3.083578315866612574, 12.21685683184790783 ) ) ;
#66504 = CARTESIAN_POINT ( 'NONE',  ( 9.661323620223001285, -4.289037785427000316, -5.816478295321999781 ) ) ;
#66505 = CARTESIAN_POINT ( 'NONE',  ( 10.65364694612719809, 3.195501139158400061, -7.821061011719899980 ) ) ;
#66506 = CARTESIAN_POINT ( 'NONE',  ( 10.90000000000000036, 0.000000000000000000, 0.000000000000000000 ) ) ;
#66507 = CARTESIAN_POINT ( 'NONE',  ( 11.08729332543999924, 2.258658230726000138, -7.034579402814999938 ) ) ;
#66508 = CARTESIAN_POINT ( 'NONE',  ( 9.987254614702999689, 2.893436332050999926, -7.781516069110699263 ) ) ;
#66510 = CARTESIAN_POINT ( 'NONE',  ( 10.42861967375000098, -2.931274166824000105, 4.618461898129999632 ) ) ;
#66509 = CARTESIAN_POINT ( 'NONE',  ( 10.96226112747999970, 2.399999999999999911, -6.571291218949999902 ) ) ;
#66511 = CARTESIAN_POINT ( 'NONE',  ( 23.61842251754734079, -13.40083422037635863, 3.925480009447839702 ) ) ;
#66512 = ORIENTED_EDGE ( 'NONE', *, *, #9860, .F. ) ;
#66513 = CARTESIAN_POINT ( 'NONE',  ( 11.15278751119019773, 3.209519379020799867, 7.086443476450299706 ) ) ;
#66514 = CARTESIAN_POINT ( 'NONE',  ( 11.08992739829000129, -5.210546653347999602, 8.327600405525998895 ) ) ;
#66515 = CARTESIAN_POINT ( 'NONE',  ( 9.553696787962998371, 4.172481380750499902, 8.489491017455099708 ) ) ;
#66516 = CARTESIAN_POINT ( 'NONE',  ( 10.69601354018300832, -3.000416447002272058, -6.731816600031361730 ) ) ;
#66517 = EDGE_CURVE ( 'NONE', #60567, #64580, #2901, .T. ) ;
#66518 = CARTESIAN_POINT ( 'NONE',  ( 23.89320776801300283, 10.87822567731000234, -3.284864823438000236 ) ) ;
#66519 = CARTESIAN_POINT ( 'NONE',  ( 12.42368232297765829, 2.995580128734607328, 13.55572452362623714 ) ) ;
#66520 = UNCERTAINTY_MEASURE_WITH_UNIT (LENGTH_MEASURE( 1.000000000000000082E-05 ), #11964, 'distance_accuracy_value', 'NONE');
#66521 = ORIENTED_EDGE ( 'NONE', *, *, #42230, .F. ) ;
#66522 = EDGE_CURVE ( 'NONE', #24287, #67539, #66352, .T. ) ;
#66523 = EDGE_CURVE ( 'NONE', #64300, #43460, #8788, .T. ) ;
#66524 = CARTESIAN_POINT ( 'NONE',  ( 9.354025935145999782, -4.165792341207500193, -6.370288821165999593 ) ) ;
#66525 = CARTESIAN_POINT ( 'NONE',  ( 11.50029455687000102, -11.56505190006999939, -1.404305717648999918 ) ) ;
#66526 = CARTESIAN_POINT ( 'NONE',  ( 18.14791645918231566, 2.065340611094592216, -12.42959220787597197 ) ) ;
#66527 = CARTESIAN_POINT ( 'NONE',  ( 7.000000000000000888, 10.16543706753050635, -4.390894937880035265 ) ) ;
#66528 = VECTOR ( 'NONE', #50792, 1000.000000000000114 ) ;
#66529 = CARTESIAN_POINT ( 'NONE',  ( 24.53003472522700434, -3.319296498592000155, 12.04487452434999994 ) ) ;
#66530 = CARTESIAN_POINT ( 'NONE',  ( 11.51102763632551884, 3.088851714329700293, -7.079572058049399708 ) ) ;
#66531 = DIRECTION ( 'NONE',  ( 0.7071074108313172291, -0.7071061515412171428, 4.731348483750111872E-09 ) ) ;
#66532 = CARTESIAN_POINT ( 'NONE',  ( 9.265308298767999773, -5.700621988293000264, -7.339579610785999186 ) ) ;
#66533 = CARTESIAN_POINT ( 'NONE',  ( 25.31010666462800174, 11.20360457085999961, 3.315062111770000097 ) ) ;
#66534 = ORIENTED_EDGE ( 'NONE', *, *, #61621, .T. ) ;
#66535 = LINE ( 'NONE', #65846, #64526 ) ;
#66536 = CARTESIAN_POINT ( 'NONE',  ( 12.30894494036361309, -0.5330308249010426991, -13.98985951701901698 ) ) ;
#66537 = DIRECTION ( 'NONE',  ( 1.000000000000000000, 0.000000000000000000, 0.000000000000000000 ) ) ;
#66538 = CARTESIAN_POINT ( 'NONE',  ( 11.47657389914466464, 3.351225026288215947, -8.595592487855949315 ) ) ;
#66539 = EDGE_CURVE ( 'NONE', #38520, #23293, #2956, .T. ) ;
#66540 = CARTESIAN_POINT ( 'NONE',  ( 10.60226354018307937, -2.907767014557176566, -8.129523725463620565 ) ) ;
#66541 = CARTESIAN_POINT ( 'NONE',  ( 9.509454719593000149, 3.116293075258000478, -6.208411413796000033 ) ) ;
#66542 = CARTESIAN_POINT ( 'NONE',  ( 6.828376212599681416, 1.461404173720322053, 0.4338462895806718955 ) ) ;
#66543 = VERTEX_POINT ( 'NONE', #23177 ) ;
#66544 = CIRCLE ( 'NONE', #8512, 12.59999999999999964 ) ;
#66545 = FACE_OUTER_BOUND ( 'NONE', #12889, .T. ) ;
#66546 = CARTESIAN_POINT ( 'NONE',  ( 18.08776130068894972, 2.172968270232229937, -13.73740491327006552 ) ) ;
#66547 = ORIENTED_EDGE ( 'NONE', *, *, #34016, .T. ) ;
#66548 = CARTESIAN_POINT ( 'NONE',  ( 11.79999999771000141, 12.39026187696000036, 1.832249219479999969 ) ) ;
#66549 = CARTESIAN_POINT ( 'NONE',  ( 44.24148000000000280, 9.517611874540000017, 8.103398312166000039 ) ) ;
#66550 = VECTOR ( 'NONE', #19537, 1000.000000000000000 ) ;
#66551 = CARTESIAN_POINT ( 'NONE',  ( 9.351420280414000530, 4.953415418491999844, -8.946479654552000227 ) ) ;
#66552 = CARTESIAN_POINT ( 'NONE',  ( 24.11585382079778839, -12.52247569921947701, 3.380851800467152390 ) ) ;
#66553 = CARTESIAN_POINT ( 'NONE',  ( 11.64633327354034797, -4.864904118400500188, -6.934277916748599502 ) ) ;
#66554 = CYLINDRICAL_SURFACE ( 'NONE', #38181, 1.625000000000000000 ) ;
#66555 = DIRECTION ( 'NONE',  ( 1.000000000000000000, 0.000000000000000000, 0.000000000000000000 ) ) ;
#66556 = ORIENTED_EDGE ( 'NONE', *, *, #558, .T. ) ;
#66557 = CARTESIAN_POINT ( 'NONE',  ( 7.663649704783383143, 5.119381272888222867, -8.282547693636418629 ) ) ;
#66558 = CARTESIAN_POINT ( 'NONE',  ( 17.83309906208979001, -3.060119824108007425, -13.53852211359039792 ) ) ;
#66559 = CARTESIAN_POINT ( 'NONE',  ( 9.743314158772999889, 5.149303692842000402, -5.987168472229000393 ) ) ;
#66560 = VERTEX_POINT ( 'NONE', #17244 ) ;
#66561 = CARTESIAN_POINT ( 'NONE',  ( 10.40878363256000050, 3.093886843363999883, -6.480781753756000185 ) ) ;
#66562 = DIRECTION ( 'NONE',  ( 1.000000000000000000, 0.000000000000000000, 0.000000000000000000 ) ) ;
#66563 = ORIENTED_EDGE ( 'NONE', *, *, #39622, .T. ) ;
#66564 = CARTESIAN_POINT ( 'NONE',  ( 8.796784697134999220, 4.619613413415000203, 8.459069166353199165 ) ) ;
#66565 = CARTESIAN_POINT ( 'NONE',  ( 18.26132062505690712, -2.644858796842617821, -12.31930452622237127 ) ) ;
#66566 = ADVANCED_FACE ( 'NONE', ( #38565 ), #19662, .T. ) ;
#66567 = DIRECTION ( 'NONE',  ( -1.000000000000000000, 0.000000000000000000, 0.000000000000000000 ) ) ;
#66568 = CARTESIAN_POINT ( 'NONE',  ( 24.95271118850850556, 11.53329584871545599, -3.220779843859221891 ) ) ;
#66569 = CARTESIAN_POINT ( 'NONE',  ( 11.48394322905000031, -11.59615457572999908, -1.579582225534999829 ) ) ;
#66570 = EDGE_CURVE ( 'NONE', #4716, #30294, #26321, .T. ) ;
#66571 = CARTESIAN_POINT ( 'NONE',  ( 27.64127793187000037, 2.399999999999999911, 6.571291218949999902 ) ) ;
#66572 = CARTESIAN_POINT ( 'NONE',  ( 9.382584444952824398, -2.847231605938053356, 8.802921338423775666 ) ) ;
#66573 = EDGE_LOOP ( 'NONE', ( #4287, #19000, #5005, #56332 ) ) ;
#66574 = CARTESIAN_POINT ( 'NONE',  ( 11.59999999999999964, 3.116215992411100366, 7.174999999999999822 ) ) ;
#66575 = CARTESIAN_POINT ( 'NONE',  ( 10.31966721959000033, 4.764593388688000530, -5.997651217580999727 ) ) ;
#66576 = DIRECTION ( 'NONE',  ( 1.000000000000000000, 0.000000000000000000, 0.000000000000000000 ) ) ;
#66577 = CARTESIAN_POINT ( 'NONE',  ( 12.24916914324843376, 2.049138926831458818, -13.84922804760273607 ) ) ;
#66578 = CARTESIAN_POINT ( 'NONE',  ( 10.41891290906799838, -4.809406943772300380, -8.490578012456198920 ) ) ;
#66579 = B_SPLINE_CURVE_WITH_KNOTS ( 'NONE', 3,
 ( #4012, #29938, #68678, #51242 ),
 .UNSPECIFIED., .F., .F.,
 ( 4, 4 ),
 ( 0.000000000000000000, 1.000000000000000000 ),
 .UNSPECIFIED. ) ;
#66580 = CARTESIAN_POINT ( 'NONE',  ( 9.939319226872999735, -2.638101016021999978, 6.328632621050000573 ) ) ;
#66581 = CARTESIAN_POINT ( 'NONE',  ( 18.20553441509223802, -0.3226776716457260274, 13.99628514671256241 ) ) ;
#66582 = VECTOR ( 'NONE', #67654, 1000.000000000000000 ) ;
#66583 = CARTESIAN_POINT ( 'NONE',  ( 7.871384581343000342, 5.129340811002999878, 6.740051537885999977 ) ) ;
#66584 = VERTEX_POINT ( 'NONE', #14423 ) ;
#66585 = EDGE_LOOP ( 'NONE', ( #56775, #4357, #24598, #44186 ) ) ;
#66586 = CARTESIAN_POINT ( 'NONE',  ( 8.590779719591999708, 2.836879604150999601, -8.783908972046001296 ) ) ;
#66587 = DIRECTION ( 'NONE',  ( -1.000000000000000000, 0.000000000000000000, 0.000000000000000000 ) ) ;
#66588 = CARTESIAN_POINT ( 'NONE',  ( 12.33198418666045626, -2.089544947732335789, 13.75203186102260311 ) ) ;
#66589 = DIRECTION ( 'NONE',  ( 0.000000000000000000, 0.000000000000000000, 1.000000000000000000 ) ) ;
#66590 = CARTESIAN_POINT ( 'NONE',  ( 23.73801811364100089, 9.840518919942999432, -9.652166885300999866 ) ) ;
#66592 = B_SPLINE_CURVE_WITH_KNOTS ( 'NONE', 3,
 ( #60221, #59523, #28413, #17922, #44154, #22113, #39240, #43458, #34004, #43799, #49727, #16867, #33657, #28766 ),
 .UNSPECIFIED., .F., .F.,
 ( 4, 2, 2, 2, 2, 2, 4 ),
 ( 0.000000000000000000, 0.1250000000000019984, 0.1875000000000012768, 0.2187499999999998335, 0.2499999999999983902, 0.4999999999999975575, 1.000000000000000000 ),
 .UNSPECIFIED. ) ;
#66591 = CARTESIAN_POINT ( 'NONE',  ( 10.33744474310099903, 4.771257858050099721, -7.874284411628199365 ) ) ;
#66594 = CARTESIAN_POINT ( 'NONE',  ( 10.97044361512000066, -6.153378486422999671, 5.035908310043000213 ) ) ;
#66593 = CARTESIAN_POINT ( 'NONE',  ( 10.05570934641700021, -2.968569381205999669, 7.989780896525600085 ) ) ;
#66595 = CARTESIAN_POINT ( 'NONE',  ( 8.888847637062996299, -5.105690627519996028, -6.405231889100001297 ) ) ;
#66596 = ORIENTED_EDGE ( 'NONE', *, *, #26750, .T. ) ;
#66597 = AXIS2_PLACEMENT_3D ( 'NONE', #46587, #34812, #61371 ) ;
#66598 = FACE_OUTER_BOUND ( 'NONE', #29087, .T. ) ;
#66599 = CARTESIAN_POINT ( 'NONE',  ( 23.89320776801300283, -12.21745654481001075, -3.256241354617000816 ) ) ;
#66600 = CARTESIAN_POINT ( 'NONE',  ( 11.10000000000000142, 5.582294820874221131, 7.480015404794160716 ) ) ;
#66601 = CARTESIAN_POINT ( 'NONE',  ( 12.26182617418671938, -0.3097617571853261698, 12.69493148512415637 ) ) ;
#66602 = DIRECTION ( 'NONE',  ( -1.000000000000000000, 0.000000000000000000, 0.000000000000000000 ) ) ;
#66603 = ORIENTED_EDGE ( 'NONE', *, *, #65875, .F. ) ;
#66605 = DIRECTION ( 'NONE',  ( -1.000000000000000000, 0.000000000000000000, -3.164702532202999971E-14 ) ) ;
#66604 = LINE ( 'NONE', #18722, #9547 ) ;
#66606 = CARTESIAN_POINT ( 'NONE',  ( 8.605545280412000508, 3.122811675949999977, -6.006064052396999919 ) ) ;
#66607 = EDGE_CURVE ( 'NONE', #52724, #5164, #12129, .T. ) ;
#66608 = B_SPLINE_CURVE_WITH_KNOTS ( 'NONE', 3,
 ( #6888, #28224, #49539, #65270, #1651, #27886, #22969, #44319, #49198, #65615, #60382, #33822, #55137, #7240, #44664, #65957, #59001, #21929 ),
 .UNSPECIFIED., .F., .F.,
 ( 4, 2, 2, 2, 2, 2, 2, 2, 4 ),
 ( 0.000000000000000000, 0.1250000000000000555, 0.2500000000000001110, 0.3750000000000001665, 0.5000000000000001110, 0.6250000000000001110, 0.7500000000000001110, 0.8750000000000000000, 1.000000000000000000 ),
 .UNSPECIFIED. ) ;
#66609 = CYLINDRICAL_SURFACE ( 'NONE', #2553, 9.250000000000000000 ) ;
#66610 = CARTESIAN_POINT ( 'NONE',  ( 8.186778834302003816, -5.111320685747004156, 6.695945149192998436 ) ) ;
#66611 = DIRECTION ( 'NONE',  ( 0.000000000000000000, 0.2461538461537954858, -0.9692307692307821076 ) ) ;
#66612 = CARTESIAN_POINT ( 'NONE',  ( 9.429073750851015845, 2.311705066330824732, 7.962955877358613321 ) ) ;
#66613 = CARTESIAN_POINT ( 'NONE',  ( 2.971974909847999946, -3.378548644117000066, -0.5658866386176000240 ) ) ;
#66614 = ORIENTED_EDGE ( 'NONE', *, *, #22725, .T. ) ;
#66615 = CARTESIAN_POINT ( 'NONE',  ( 12.29127437512780219, -0.3560396104572045028, -12.69328656575056691 ) ) ;
#66616 = CARTESIAN_POINT ( 'NONE',  ( 12.00962052873067876, -4.169679534937900556, 8.360247930805771333 ) ) ;
#66617 = CARTESIAN_POINT ( 'NONE',  ( 24.23036330766939983, -12.32981272787003135, -3.306814091776679287 ) ) ;
#66618 = CARTESIAN_POINT ( 'NONE',  ( 24.60999195316300003, 3.467950226999999774, -12.10892777233999951 ) ) ;
#66619 =( NAMED_UNIT ( * ) PLANE_ANGLE_UNIT ( ) SI_UNIT ( $, .RADIAN. ) );
#66620 = VERTEX_POINT ( 'NONE', #60935 ) ;
#66621 = CARTESIAN_POINT ( 'NONE',  ( 6.787102968646999912, -1.006517980596000061, 0.5009083264753000364 ) ) ;
#66622 = CARTESIAN_POINT ( 'NONE',  ( 7.788935841227000445, 2.863733890340999899, -8.313606627241000524 ) ) ;
#66623 = EDGE_CURVE ( 'NONE', #28653, #58094, #43829, .T. ) ;
#66625 = CARTESIAN_POINT ( 'NONE',  ( 10.58580560302224782, 5.314991280552380459, -7.853445763305330729 ) ) ;
#66624 = CARTESIAN_POINT ( 'NONE',  ( 23.60000000000000142, 0.000000000000000000, 0.000000000000000000 ) ) ;
#66626 = CARTESIAN_POINT ( 'NONE',  ( 10.05862282008599884, 4.666276081381299790, 6.425317846273999933 ) ) ;
#66627 = CARTESIAN_POINT ( 'NONE',  ( 10.47683719568447636, -3.813711395361371714, -6.645958924689391090 ) ) ;
#66628 = ORIENTED_EDGE ( 'NONE', *, *, #22330, .T. ) ;
#66629 = VECTOR ( 'NONE', #7570, 1000.000000000000000 ) ;
#66630 = B_SPLINE_CURVE_WITH_KNOTS ( 'NONE', 3,
 ( #23745, #13615, #51007, #18854, #34601, #35280, #55569, #29706, #7319, #3107, #24439, #55914, #50323, #45765, #2421, #28660, #61835, #66041 ),
 .UNSPECIFIED., .F., .F.,
 ( 4, 2, 2, 2, 2, 2, 2, 2, 4 ),
 ( 0.000000000000000000, 0.1249999999999999722, 0.2499999999999999445, 0.3749999999999998890, 0.4999999999999998890, 0.6249999999999998890, 0.7499999999999997780, 0.8749999999999998890, 1.000000000000000000 ),
 .UNSPECIFIED. ) ;
#66631 = ORIENTED_EDGE ( 'NONE', *, *, #21052, .T. ) ;
#66632 = EDGE_CURVE ( 'NONE', #5657, #57674, #17426, .T. ) ;
#66633 = CARTESIAN_POINT ( 'NONE',  ( 3.400000000000000355, -1.500000000000000000, 0.000000000000000000 ) ) ;
#66634 = CARTESIAN_POINT ( 'NONE',  ( 8.470293146793999028, -4.255646685191999623, 9.114089645792999406 ) ) ;
#66635 = AXIS2_PLACEMENT_3D ( 'NONE', #31484, #42328, #63630 ) ;
#66636 = CARTESIAN_POINT ( 'NONE',  ( 18.08498662421418857, 0.4989076128645600350, -13.99111800451625243 ) ) ;
#66637 = ORIENTED_EDGE ( 'NONE', *, *, #9919, .F. ) ;
#66638 = CARTESIAN_POINT ( 'NONE',  ( 9.051363484269000281, -8.680251604461998838, 6.293370873935000276 ) ) ;
#66639 = FACE_OUTER_BOUND ( 'NONE', #69065, .T. ) ;
#66640 = DIRECTION ( 'NONE',  ( -1.000000000000000000, 0.000000000000000000, 0.000000000000000000 ) ) ;
#66641 = FACE_OUTER_BOUND ( 'NONE', #63638, .T. ) ;
#66642 = DIRECTION ( 'NONE',  ( 1.000000000000000000, 0.000000000000000000, 0.000000000000000000 ) ) ;
#66643 = VERTEX_POINT ( 'NONE', #29485 ) ;
#66644 = CARTESIAN_POINT ( 'NONE',  ( 9.843726350706999639, -4.115123626494000320, 9.466607949400000166 ) ) ;
#66645 = CARTESIAN_POINT ( 'NONE',  ( 12.64199182499459262, -3.104696382831371615, -13.52638422211150093 ) ) ;
#66646 = CARTESIAN_POINT ( 'NONE',  ( 5.594609839683376329, -1.500000000000000888, 0.1963495408493559080 ) ) ;
#66647 = CARTESIAN_POINT ( 'NONE',  ( 11.58810207955139937, -4.796537143354000499, 7.825000000000000178 ) ) ;
#66648 = AXIS2_PLACEMENT_3D ( 'NONE', #18817, #60425, #56212 ) ;
#66649 = CARTESIAN_POINT ( 'NONE',  ( 12.35713445931583010, -3.099811329677685467, 13.65268841750260620 ) ) ;
#66650 = ORIENTED_EDGE ( 'NONE', *, *, #57826, .T. ) ;
#66651 = CARTESIAN_POINT ( 'NONE',  ( 10.40685100253999984, -2.832432432432000269, -6.822293592207000934 ) ) ;
#66652 = CARTESIAN_POINT ( 'NONE',  ( 0.2066231058121046349, -2.618168328974044765E-06, -3.206444164765644977 ) ) ;
#66653 = CARTESIAN_POINT ( 'NONE',  ( 3.500000000000000444, 0.8984343939224210818, 3.199201382548016337 ) ) ;
#66654 = CARTESIAN_POINT ( 'NONE',  ( 24.08707381732377684, -3.338859752676834880, -12.58718648024971820 ) ) ;
#66655 = CARTESIAN_POINT ( 'NONE',  ( 9.020964430773000586, -2.907392932634000005, 6.146188468825999784 ) ) ;
#66656 = EDGE_CURVE ( 'NONE', #36346, #6237, #40631, .T. ) ;
#66657 = CARTESIAN_POINT ( 'NONE',  ( 12.24422661137779045, 0.2766185922798737873, -13.89631150889695732 ) ) ;
#66658 = CARTESIAN_POINT ( 'NONE',  ( 18.00740283128408947, -2.068595914410284120, 12.54170588102538275 ) ) ;
#66659 = ORIENTED_EDGE ( 'NONE', *, *, #43879, .F. ) ;
#66660 = CARTESIAN_POINT ( 'NONE',  ( 11.56833327354034857, -4.746587807672299597, -7.011667014989399149 ) ) ;
#66661 = EDGE_LOOP ( 'NONE', ( #34452, #29466, #34947, #31315, #3543 ) ) ;
#66662 = CYLINDRICAL_SURFACE ( 'NONE', #37809, 0.6999999999999992895 ) ;
#66663 = CARTESIAN_POINT ( 'NONE',  ( 10.21398584123000042, 3.990126737362999609, -8.809457313313998839 ) ) ;
#66664 = CARTESIAN_POINT ( 'NONE',  ( 2.999405651491000135, -3.212481615617999609, 0.1285223249498000098 ) ) ;
#66665 = CARTESIAN_POINT ( 'NONE',  ( 10.47211906628000122, -2.640759929160000130, -8.505246563374999624 ) ) ;
#66666 = FACE_OUTER_BOUND ( 'NONE', #39307, .T. ) ;
#66667 = CARTESIAN_POINT ( 'NONE',  ( 9.028522009144964500, -5.063507634687575809, 8.333874286671722587 ) ) ;
#66668 = ORIENTED_EDGE ( 'NONE', *, *, #35239, .T. ) ;
#66669 = CARTESIAN_POINT ( 'NONE',  ( 11.90841235500450068, -4.841138636481000290, 8.270568563129298667 ) ) ;
#66670 = CARTESIAN_POINT ( 'NONE',  ( 9.820199962102000413, 3.883325513302000154, 6.055618835924000187 ) ) ;
#66671 = CARTESIAN_POINT ( 'NONE',  ( 10.86501009699205866, -2.649983380499685737, -7.500000587580680111 ) ) ;
#66672 = CARTESIAN_POINT ( 'NONE',  ( 10.82169598649000086, -3.233475335853099875, 7.043598424555200133 ) ) ;
#66674 = CARTESIAN_POINT ( 'NONE',  ( 11.04166666666769103, 2.793604566010535528, 8.411630010704181259 ) ) ;
#66673 = CARTESIAN_POINT ( 'NONE',  ( 10.74609776273999984, 4.263105564403999459, 9.276980853981999786 ) ) ;
#66675 = CARTESIAN_POINT ( 'NONE',  ( 10.25564828895399927, 4.880669054351300495, -7.981013126389099099 ) ) ;
#66676 = VECTOR ( 'NONE', #67521, 1000.000000000000114 ) ;
#66677 = CARTESIAN_POINT ( 'NONE',  ( 10.95905699168409697, 2.826108491929388844, -6.684704321099483870 ) ) ;
#66678 = CARTESIAN_POINT ( 'NONE',  ( 9.199088727410998700, 2.999102593977000186, -7.583944523024719331 ) ) ;
#66679 = CARTESIAN_POINT ( 'NONE',  ( 18.01033200807250978, -0.5598083480993575334, 12.58755849294668394 ) ) ;
#66680 = CARTESIAN_POINT ( 'NONE',  ( 24.61098151538899970, 3.467630292425999627, 12.10773253045999986 ) ) ;
#66681 = CARTESIAN_POINT ( 'NONE',  ( 8.127093974303878809, 4.981402631029236083, -6.380819531419545498 ) ) ;
#66682 = CARTESIAN_POINT ( 'NONE',  ( 17.60000000024299993, 11.86189249994999884, -3.298671769835999967 ) ) ;
#66683 = VERTEX_POINT ( 'NONE', #24210 ) ;
#66684 = CARTESIAN_POINT ( 'NONE',  ( 7.603418146792000343, -5.687202994508999687, 6.847270485579000088 ) ) ;
#66685 = B_SPLINE_CURVE_WITH_KNOTS ( 'NONE', 3,
 ( #45899, #56392, #29499, #25606 ),
 .UNSPECIFIED., .F., .F.,
 ( 4, 4 ),
 ( 0.000000000000000000, 1.000000000000000000 ),
 .UNSPECIFIED. ) ;
#66686 = EDGE_CURVE ( 'NONE', #60348, #5919, #41986, .T. ) ;
#66687 = EDGE_CURVE ( 'NONE', #51766, #13783, #13732, .T. ) ;
#66688 = CARTESIAN_POINT ( 'NONE',  ( 18.21732822554148257, 2.220719680094977555, 13.82275391900495798 ) ) ;
#66689 = DIRECTION ( 'NONE',  ( 1.000000000000000000, -1.056835174927999956E-13, 0.000000000000000000 ) ) ;
#66690 = CARTESIAN_POINT ( 'NONE',  ( 10.47530200610849604, 5.350262918594154371, 7.499984559551275964 ) ) ;
#66691 = ORIENTED_EDGE ( 'NONE', *, *, #9463, .F. ) ;
#66692 = CARTESIAN_POINT ( 'NONE',  ( 7.935739158771999868, 5.430400319332999715, 7.210801214872999410 ) ) ;
#66694 = CARTESIAN_POINT ( 'NONE',  ( 0.7768612129559736568, -3.384277603090292352, 1.036914961361027343 ) ) ;
#66693 = CARTESIAN_POINT ( 'NONE',  ( 8.506095280410999493, 2.305580295895999665, -7.860904109308999743 ) ) ;
#66695 = CARTESIAN_POINT ( 'NONE',  ( 11.17788388625999829, 2.412139249855000056, -7.075601348558000048 ) ) ;
#66696 = ORIENTED_EDGE ( 'NONE', *, *, #62055, .T. ) ;
#66697 = CARTESIAN_POINT ( 'NONE',  ( 7.100000000000000533, 0.000000000000000000, 0.000000000000000000 ) ) ;
#66698 = AXIS2_PLACEMENT_3D ( 'NONE', #6275, #7673, #29358 ) ;
#66699 = CARTESIAN_POINT ( 'NONE',  ( 9.253736882039186540, -4.918551780227518933, -6.034027795051781773 ) ) ;
#66700 = CARTESIAN_POINT ( 'NONE',  ( 11.30995122972050027, 4.452766304612699955, 8.547040013405998948 ) ) ;
#66701 = CARTESIAN_POINT ( 'NONE',  ( 9.966331042021000286, -2.304002513595999613, 6.575636708208000059 ) ) ;
#66702 = FACE_BOUND ( 'NONE', #68989, .T. ) ;
#66703 = ORIENTED_EDGE ( 'NONE', *, *, #68293, .T. ) ;
#66704 = DIRECTION ( 'NONE',  ( -6.273181842718999770E-11, -6.273118898148000207E-11, -1.000000000000000000 ) ) ;
#66705 = CARTESIAN_POINT ( 'NONE',  ( 1.250973465874999802, -3.500000000000000000, 0.000000000000000000 ) ) ;
#66706 = EDGE_CURVE ( 'NONE', #49580, #50821, #19682, .T. ) ;
#66707 = CARTESIAN_POINT ( 'NONE',  ( 7.983375487919488478, -2.407341777098653157, 6.779802702655946867 ) ) ;
#66708 = CARTESIAN_POINT ( 'NONE',  ( 11.05639424537999993, -5.030223832177999732, 6.028291574375000295 ) ) ;
#66709 = CARTESIAN_POINT ( 'NONE',  ( 11.60477869730532774, -4.467447516829900600, -6.578238193496799724 ) ) ;
#66710 = CARTESIAN_POINT ( 'NONE',  ( 10.36060887879200010, -4.258572737033900601, 8.612148635591999835 ) ) ;
#66711 = ORIENTED_EDGE ( 'NONE', *, *, #63027, .T. ) ;
#66712 = CARTESIAN_POINT ( 'NONE',  ( 10.74001548714999998, -5.126947719599001196, -5.008168344353999935 ) ) ;
#66713 = B_SPLINE_CURVE_WITH_KNOTS ( 'NONE', 3,
 ( #38756, #44007, #16044, #53795 ),
 .UNSPECIFIED., .F., .F.,
 ( 4, 4 ),
 ( 0.000000000000000000, 1.000000000000000000 ),
 .UNSPECIFIED. ) ;
#66714 = CARTESIAN_POINT ( 'NONE',  ( 11.75656651104150008, -3.873914634362100262, 8.771777834828998976 ) ) ;
#66715 = VERTEX_POINT ( 'NONE', #56727 ) ;
#66716 = EDGE_CURVE ( 'NONE', #6955, #52670, #67885, .T. ) ;
#66717 = CARTESIAN_POINT ( 'NONE',  ( 18.43317799840268023, -2.892723637958458216, -12.11800683821374314 ) ) ;
#66718 = VERTEX_POINT ( 'NONE', #57736 ) ;
#66719 = CARTESIAN_POINT ( 'NONE',  ( 9.487725409950000355, -4.905858243509999106, -8.948175900338000588 ) ) ;
#66720 = CARTESIAN_POINT ( 'NONE',  ( 9.939260841229000221, 5.099602161831000124, -9.049221499261999924 ) ) ;
#66721 = CARTESIAN_POINT ( 'NONE',  ( 9.472537864290000442, -2.899999999999999911, -6.571291218949999902 ) ) ;
#66722 = CARTESIAN_POINT ( 'NONE',  ( 8.330224159023998709, 2.898680183691999979, -6.607597200868999820 ) ) ;
#66723 = CARTESIAN_POINT ( 'NONE',  ( 12.19628620791406348, 2.642962752853494024, -12.41715721841834608 ) ) ;
#66724 = CARTESIAN_POINT ( 'NONE',  ( 11.22333863405319931, -3.380905141010200232, 6.710270673950399889 ) ) ;
#66725 = CARTESIAN_POINT ( 'NONE',  ( 11.07102344389999971, -4.762665848028800220, 7.962849245488699879 ) ) ;
#66726 = ORIENTED_EDGE ( 'NONE', *, *, #489, .F. ) ;
#66727 = DIRECTION ( 'NONE',  ( 1.000000000000000000, 0.000000000000000000, 0.000000000000000000 ) ) ;
#66728 = VECTOR ( 'NONE', #15462, 1000.000000000000000 ) ;
#66729 = CARTESIAN_POINT ( 'NONE',  ( 9.304730646793998972, -5.284133759825000887, 6.489273023403000273 ) ) ;
#66730 = CARTESIAN_POINT ( 'NONE',  ( 12.80505043854146940, -3.125000000000000000, -13.52078605991414761 ) ) ;
#66731 = VERTEX_POINT ( 'NONE', #4595 ) ;
#66732 = CARTESIAN_POINT ( 'NONE',  ( 12.08558010717403164, -2.390021230702592092, -12.37125449870878846 ) ) ;
#66733 = CARTESIAN_POINT ( 'NONE',  ( 10.21462282008599942, 4.523146351753199568, 6.656181553372300108 ) ) ;
#66734 = CARTESIAN_POINT ( 'NONE',  ( 10.13035685320999946, -2.409329538444999752, -8.058042649154000259 ) ) ;
#66735 = CARTESIAN_POINT ( 'NONE',  ( 13.70005190196300227, -9.005348107749998832, -7.391036106496999381 ) ) ;
#66736 = LINE ( 'NONE', #69140, #11449 ) ;
#66737 = CARTESIAN_POINT ( 'NONE',  ( 9.907648723390195755, 5.170927832464149887, -8.821309888205709271 ) ) ;
#66738 = CARTESIAN_POINT ( 'NONE',  ( 5.200000000000000178, 0.8000000000000000444, 3.149999999999999911 ) ) ;
#66739 = FACE_OUTER_BOUND ( 'NONE', #34981, .T. ) ;
#66740 = AXIS2_PLACEMENT_3D ( 'NONE', #58099, #52854, #4953 ) ;
#66741 = CARTESIAN_POINT ( 'NONE',  ( 11.85979573085659844, -3.159987984332300215, -7.645349278262099979 ) ) ;
#66742 = CARTESIAN_POINT ( 'NONE',  ( 10.86272200990529946, -5.206705454565000224, -7.079074440652799893 ) ) ;
#66743 = CARTESIAN_POINT ( 'NONE',  ( 17.55505043854147118, -3.199751711897561801, 12.18694338143115452 ) ) ;
#66745 = VERTEX_POINT ( 'NONE', #41328 ) ;
#66744 = B_SPLINE_CURVE_WITH_KNOTS ( 'NONE', 3,
 ( #32863, #33555, #54529, #1051 ),
 .UNSPECIFIED., .F., .F.,
 ( 4, 4 ),
 ( 0.000000000000000000, 1.000000000000000000 ),
 .UNSPECIFIED. ) ;
#66746 = ORIENTED_EDGE ( 'NONE', *, *, #63821, .T. ) ;
#66747 = VECTOR ( 'NONE', #5308, 999.9999999999998863 ) ;
#66748 = FACE_OUTER_BOUND ( 'NONE', #51390, .T. ) ;
#66749 = CARTESIAN_POINT ( 'NONE',  ( 17.55505043854144276, -0.7302158263239199032, -13.98094363220830871 ) ) ;
#66750 = CARTESIAN_POINT ( 'NONE',  ( 24.22093787138100041, -3.188036788074999794, 12.21311288046000065 ) ) ;
#66751 = FACE_OUTER_BOUND ( 'NONE', #19857, .T. ) ;
#66752 = CARTESIAN_POINT ( 'NONE',  ( 17.81550493765275789, 1.931762299006052119, 12.56594712229140498 ) ) ;
#66753 = ADVANCED_FACE ( 'NONE', ( #32224 ), #15180, .F. ) ;
#66754 = FACE_OUTER_BOUND ( 'NONE', #51727, .T. ) ;
#66755 = EDGE_CURVE ( 'NONE', #12694, #20104, #10533, .T. ) ;
#66756 = CARTESIAN_POINT ( 'NONE',  ( 9.215291255903000689, 4.861981595026999337, 8.938817176893000038 ) ) ;
#66757 = CARTESIAN_POINT ( 'NONE',  ( 11.21022026213526601, 5.045753393512712570, 7.175001674908393134 ) ) ;
#66758 = ORIENTED_EDGE ( 'NONE', *, *, #38569, .T. ) ;
#66759 = CARTESIAN_POINT ( 'NONE',  ( 12.80505043854146940, -3.199751711897561801, 12.18694338143115452 ) ) ;
#66760 = CARTESIAN_POINT ( 'NONE',  ( 10.21024205624999937, -4.310927436352299580, -8.309340504471899536 ) ) ;
#66761 = CARTESIAN_POINT ( 'NONE',  ( 9.351497027444999333, 4.821940693094999730, 8.950154065657999425 ) ) ;
#66762 = CARTESIAN_POINT ( 'NONE',  ( 21.49999863197000138, 0.000000000000000000, 0.000000000000000000 ) ) ;
#66763 = B_SPLINE_CURVE_WITH_KNOTS ( 'NONE', 3,
 ( #18252, #56001, #50067, #13014 ),
 .UNSPECIFIED., .F., .F.,
 ( 4, 4 ),
 ( 0.000000000000000000, 1.000000000000000000 ),
 .UNSPECIFIED. ) ;
#66764 = PRODUCT_DEFINITION_SHAPE ( 'NONE', 'NONE',  #59017 ) ;
#66765 = CARTESIAN_POINT ( 'NONE',  ( 10.13662282008599824, 4.594711216567399781, -8.459250300176799797 ) ) ;
#66766 = CARTESIAN_POINT ( 'NONE',  ( 12.78440276244763041, 0.6249994333735301444, 12.67928921956170996 ) ) ;
#66767 = CARTESIAN_POINT ( 'NONE',  ( 9.342517219591000455, 5.057081813675999626, 8.967637988488998957 ) ) ;
#66768 = CARTESIAN_POINT ( 'NONE',  ( 9.261662452849000360, 2.944259351255000379, 6.507396354981000108 ) ) ;
#66769 = CARTESIAN_POINT ( 'NONE',  ( 12.54434846374635626, 1.931873423426545777, 12.56592826555434073 ) ) ;
#66770 = ORIENTED_EDGE ( 'NONE', *, *, #16717, .F. ) ;
#66771 = CARTESIAN_POINT ( 'NONE',  ( 9.643864158774000828, 2.927176851028000293, -5.932007155957999878 ) ) ;
#66772 = CARTESIAN_POINT ( 'NONE',  ( 10.83810672858429847, 2.978701842912999886, -6.731711997412900494 ) ) ;
#66773 = EDGE_CURVE ( 'NONE', #15877, #11716, #9847, .T. ) ;
#66774 = ADVANCED_FACE ( 'NONE', ( #36422 ), #36771, .T. ) ;
#66775 = CARTESIAN_POINT ( 'NONE',  ( 10.82122311210984478, -4.081721762518836449, 9.237771506523644760 ) ) ;
#66777 = CARTESIAN_POINT ( 'NONE',  ( 10.10434687351566474, 5.250000000000001776, 7.663624617374461323 ) ) ;
#66776 = CARTESIAN_POINT ( 'NONE',  ( 7.598066940377999678, -3.554853390786000045, 8.889491623367000273 ) ) ;
#66778 = CARTESIAN_POINT ( 'NONE',  ( 9.554101285864000204, -4.558267473659599389, 8.163359157892799089 ) ) ;
#66779 = CARTESIAN_POINT ( 'NONE',  ( 10.82179975933729921, -3.051121678931899783, -7.173532873542499466 ) ) ;
#66780 = ORIENTED_EDGE ( 'NONE', *, *, #37701, .T. ) ;
#66781 = EDGE_CURVE ( 'NONE', #21416, #43157, #15468, .T. ) ;
#66782 = CARTESIAN_POINT ( 'NONE',  ( 2.206657498381999982, -3.444624976169999631, -1.019033653642999804 ) ) ;
#66783 = CARTESIAN_POINT ( 'NONE',  ( 18.16417820190392618, -0.1413121815030540240, -12.69896133444535735 ) ) ;
#66784 = AXIS2_PLACEMENT_3D ( 'NONE', #40819, #30345, #13920 ) ;
#66785 = CARTESIAN_POINT ( 'NONE',  ( 12.68583900966313038, -11.53041019655163879, 4.891346001956513589 ) ) ;
#66786 = CARTESIAN_POINT ( 'NONE',  ( 11.59999999999999964, 5.207010770456999893, 7.174999999999999822 ) ) ;
#66787 = CARTESIAN_POINT ( 'NONE',  ( 9.996463691909600158, 5.100000000000000533, -6.665341197398679363 ) ) ;
#66789 = CARTESIAN_POINT ( 'NONE',  ( 17.71877800696621108, -1.896477791912290822, -13.78304299653506959 ) ) ;
#66788 = VECTOR ( 'NONE', #57048, 1000.000000000000000 ) ;
#66790 = CARTESIAN_POINT ( 'NONE',  ( 10.02314899745999988, -5.167567567567999731, -6.822293592207000934 ) ) ;
#66791 = LINE ( 'NONE', #33951, #34415 ) ;
#66792 = CARTESIAN_POINT ( 'NONE',  ( 9.362879440377000151, -3.677416446733000388, 9.250734868033999803 ) ) ;
#66793 = VERTEX_POINT ( 'NONE', #14759 ) ;
#66794 = CARTESIAN_POINT ( 'NONE',  ( 8.085170280410000743, 2.431401017850999935, 7.958393275880999873 ) ) ;
#66795 = CARTESIAN_POINT ( 'NONE',  ( 13.40279821320924114, -11.66091458874562470, -2.117181037223689888 ) ) ;
#66796 = CARTESIAN_POINT ( 'NONE',  ( 18.14066966380178769, 2.280775195392830579, -13.71753029190285389 ) ) ;
#66797 = AXIS2_PLACEMENT_3D ( 'NONE', #25346, #67988, #62740 ) ;
#66798 = CARTESIAN_POINT ( 'NONE',  ( 10.62120626704272475, -3.646797508062162851, 8.848526273074867277 ) ) ;
#66799 = CARTESIAN_POINT ( 'NONE',  ( 0.6465629140399999919, 2.290033430544000215, -2.273164938691999648 ) ) ;
#66800 = ORIENTED_EDGE ( 'NONE', *, *, #14161, .T. ) ;
#66801 = CARTESIAN_POINT ( 'NONE',  ( 13.99999999231800096, -8.833253877201999060, -7.896562762484000686 ) ) ;
#66802 = EDGE_CURVE ( 'NONE', #23870, #47396, #26631, .T. ) ;
#66803 = CARTESIAN_POINT ( 'NONE',  ( 10.96219100130544710, -4.057262373299075797, -9.264968071217497325 ) ) ;
#66804 = CARTESIAN_POINT ( 'NONE',  ( 9.778460659405999067, 5.743717947473999885, 7.748300625457000379 ) ) ;
#66805 = CARTESIAN_POINT ( 'NONE',  ( 10.28441772631199846, 4.372518460886800185, 6.733203680593099705 ) ) ;
#66806 = AXIS2_PLACEMENT_3D ( 'NONE', #11414, #11079, #32414 ) ;
#66807 = CARTESIAN_POINT ( 'NONE',  ( 5.000000000000000000, 0.000000000000000000, 0.000000000000000000 ) ) ;
#66808 = DIRECTION ( 'NONE',  ( -1.000000000000000000, 0.000000000000000000, 0.000000000000000000 ) ) ;
#66809 = CARTESIAN_POINT ( 'NONE',  ( 11.79999999771000141, 3.595163221087000149, -11.99793848941000007 ) ) ;
#66810 = CARTESIAN_POINT ( 'NONE',  ( 10.56498513754044311, 5.349957030113837497, -7.500000808964303545 ) ) ;
#66811 = CARTESIAN_POINT ( 'NONE',  ( 9.565773468336619345, 5.100000000000000533, 6.304440313901286785 ) ) ;
#66812 = CARTESIAN_POINT ( 'NONE',  ( 8.017695689388432356, 2.842496704177993827, 6.173521863453695246 ) ) ;
#66813 = ORIENTED_EDGE ( 'NONE', *, *, #53493, .T. ) ;
#66814 = CARTESIAN_POINT ( 'NONE',  ( 17.74765434492531213, -1.905326452124538550, 13.78174529102851587 ) ) ;
#66815 = DIRECTION ( 'NONE',  ( 0.000000000000000000, -1.000000000000000000, 0.000000000000000000 ) ) ;
#66816 = VERTEX_POINT ( 'NONE', #63318 ) ;
#66817 = ORIENTED_EDGE ( 'NONE', *, *, #6613, .F. ) ;
#66818 = CARTESIAN_POINT ( 'NONE',  ( 24.92848015187707844, -2.996103346371080001, -11.61747088698863806 ) ) ;
#66819 = CARTESIAN_POINT ( 'NONE',  ( 4.149992563291998948, 1.999946284944287722, -0.2617923565147984299 ) ) ;
#66820 = CARTESIAN_POINT ( 'NONE',  ( 6.999999691988000095, -12.89129024452999950, -1.677687644161999891 ) ) ;
#66821 = CARTESIAN_POINT ( 'NONE',  ( 11.09999999999999964, 4.000000000000000000, 7.500000000000000000 ) ) ;
#66822 = CARTESIAN_POINT ( 'NONE',  ( 10.36950244779999863, 2.719131864236000062, -7.031786688683999920 ) ) ;
#66823 = CARTESIAN_POINT ( 'NONE',  ( 8.691485517493021007, 3.974336348583935141, -8.874742188917888797 ) ) ;
#66824 = CARTESIAN_POINT ( 'NONE',  ( 10.20319453770999907, -3.421758889707999796, 6.017729046583999875 ) ) ;
#66825 = CARTESIAN_POINT ( 'NONE',  ( 18.08442823429788504, 0.4920215530101138546, -12.59040071882420797 ) ) ;
#66826 = CARTESIAN_POINT ( 'NONE',  ( 25.55279310973962126, 11.13093580945219685, 3.116563969436135118 ) ) ;
#66827 = CARTESIAN_POINT ( 'NONE',  ( 10.75210807141120029, -3.959980833595939664, -8.365272822098500427 ) ) ;
#66828 = CARTESIAN_POINT ( 'NONE',  ( 10.72510394928771227, -2.650147065043205519, 7.500007457243348163 ) ) ;
#66829 = ORIENTED_EDGE ( 'NONE', *, *, #49027, .T. ) ;
#66830 = CARTESIAN_POINT ( 'NONE',  ( 8.962753061708919944, 2.887246877270963186, -7.353476507976682619 ) ) ;
#66831 = CARTESIAN_POINT ( 'NONE',  ( 5.966666563206250551, -12.43894743589586405, -2.828924746354209763 ) ) ;
#66832 = CARTESIAN_POINT ( 'NONE',  ( 6.308784017580002512, 8.386574891157003719, 3.907856452066002184 ) ) ;
#66833 = CARTESIAN_POINT ( 'NONE',  ( 9.380417874594000338, 2.822750429186000165, -8.000467616829000761 ) ) ;
#66834 = EDGE_CURVE ( 'NONE', #14790, #30735, #481, .T. ) ;
#66835 = CARTESIAN_POINT ( 'NONE',  ( 12.17999522571488846, 2.481546339243234200, 13.67732359575999368 ) ) ;
#66836 = EDGE_CURVE ( 'NONE', #45160, #56759, #39617, .T. ) ;
#66837 = CARTESIAN_POINT ( 'NONE',  ( 9.757667269575000191, -4.489271889653999814, 5.986031004145000445 ) ) ;
#66838 = VERTEX_POINT ( 'NONE', #68220 ) ;
#66839 = CARTESIAN_POINT ( 'NONE',  ( 12.32623905011267240, 0.4017251370869492910, -12.69144801866011640 ) ) ;
#66840 = CARTESIAN_POINT ( 'NONE',  ( 12.54683519492311916, -0.5695321295966300212, 13.88429381145915720 ) ) ;
#66841 = ORIENTED_EDGE ( 'NONE', *, *, #18109, .F. ) ;
#66842 = DIRECTION ( 'NONE',  ( 1.000000000000000000, 0.000000000000000000, 0.000000000000000000 ) ) ;
#66843 = PLANE ( 'NONE',  #39608 ) ;
#66844 = CARTESIAN_POINT ( 'NONE',  ( 23.58457962933900376, -3.197576462624000193, -13.62102450554000121 ) ) ;
#66845 = CYLINDRICAL_SURFACE ( 'NONE', #29455, 0.5000000000000002220 ) ;
#66846 = B_SPLINE_CURVE_WITH_KNOTS ( 'NONE', 3,
 ( #27840, #1256, #60333, #28174, #18720, #55781, #7193, #39354, #33771, #65218, #28884, #12439, #40055, #65910, #59981, #33076, #54390, #6493, #7886, #1952, #60675, #55086, #44954, #34118, #28529, #54741, #34470, #49145, #23274, #55436, #12093, #18379, #49490, #22571, #50193, #2293, #66258, #39701, #43914, #17333, #38662, #1601, #19748, #41070, #9585, #29575, #20427, #35151, #40381, #62390, #56814, #62721, #66944 ),
 .UNSPECIFIED., .F., .F.,
 ( 4, 2, 2, 2, 2, 2, 2, 2, 2, 2, 2, 2, 2, 1, 2, 2, 2, 2, 2, 2, 2, 2, 2, 2, 1, 1, 2, 4 ),
 ( 0.000000000000000000, 0.06264497286387624153, 0.1252899457277524831, 0.1566124321596882862, 0.1879349185916240339, 0.2192574050235598371, 0.2349186482395275166, 0.2505798914554951962, 0.2819023778874309438, 0.2975636211033985679, 0.3132248643193661919, 0.3288861075353337604, 0.3445473507513013844, 0.3602085939672690640, 0.3680392155752531536, 0.3758698371832371876, 0.3915310803992061439, 0.3993617020071908441, 0.4071923236151755443, 0.4228535668311456663, 0.4306841884391316433, 0.4385148100471176202, 0.4541760532630899072, 0.4698372964790621942, 0.4854985396950344811, 0.4933291613030210687, 0.4972444721070140017, 0.5011597829110069346 ),
 .UNSPECIFIED. ) ;
#66847 = CARTESIAN_POINT ( 'NONE',  ( 8.844321844545273592, 2.684787752319955256, -7.853330290198121233 ) ) ;
#66848 = CARTESIAN_POINT ( 'NONE',  ( 4.599999999999999645, 0.000000000000000000, 0.000000000000000000 ) ) ;
#66849 = CARTESIAN_POINT ( 'NONE',  ( 7.966460921982568166, 5.180256874905277975, 8.180071673469157645 ) ) ;
#66850 = FACE_OUTER_BOUND ( 'NONE', #61756, .T. ) ;
#66851 = CARTESIAN_POINT ( 'NONE',  ( 9.441315108303999892, -3.111669560323000017, -8.958991988670002016 ) ) ;
#66852 = CARTESIAN_POINT ( 'NONE',  ( 11.14595257254739913, 3.168263696564200149, -7.741895249827200232 ) ) ;
#66853 = FACE_OUTER_BOUND ( 'NONE', #1003, .T. ) ;
#66854 = CARTESIAN_POINT ( 'NONE',  ( 10.57102344389999971, 3.237334151971200225, -7.037150754511299233 ) ) ;
#66855 = CARTESIAN_POINT ( 'NONE',  ( 8.923430433046998900, 3.028322657068899915, -6.900352112302299723 ) ) ;
#66857 = FACE_OUTER_BOUND ( 'NONE', #3311, .T. ) ;
#66856 = CARTESIAN_POINT ( 'NONE',  ( 15.76715644869600119, -8.722854347492999594, -8.080426068599999567 ) ) ;
#66858 = VECTOR ( 'NONE', #65965, 1000.000000000000000 ) ;
#66859 = DIRECTION ( 'NONE',  ( 1.000000000000000000, 0.000000000000000000, 0.000000000000000000 ) ) ;
#66860 = ORIENTED_EDGE ( 'NONE', *, *, #57372, .F. ) ;
#66861 = EDGE_CURVE ( 'NONE', #60220, #6314, #32200, .T. ) ;
#66862 = CARTESIAN_POINT ( 'NONE',  ( 10.94501463001509833, 4.472480213525599879, 8.256737112932800216 ) ) ;
#66863 = CARTESIAN_POINT ( 'NONE',  ( 10.22109127278999807, -2.983266195621000261, 8.764707262515999631 ) ) ;
#66864 = CARTESIAN_POINT ( 'NONE',  ( 10.16159632033899918, 3.070047649444500149, 7.879514065647800436 ) ) ;
#66865 = CARTESIAN_POINT ( 'NONE',  ( 10.90000000000000036, -2.778483479159999714, -6.925197956411000000 ) ) ;
#66866 = CARTESIAN_POINT ( 'NONE',  ( 24.52301462737445803, 12.12194122193224821, -3.142914130639136605 ) ) ;
#66867 = CARTESIAN_POINT ( 'NONE',  ( 6.949993407501000142, 13.87069231928999891, 4.225386915259999654 ) ) ;
#66868 = CARTESIAN_POINT ( 'NONE',  ( 23.57773640739606691, 2.928864175545800919, -13.64745269084981061 ) ) ;
#66869 = ORIENTED_EDGE ( 'NONE', *, *, #52792, .F. ) ;
#66870 = CARTESIAN_POINT ( 'NONE',  ( 9.759292290062999697, -3.012566816337000297, -6.926667499798199401 ) ) ;
#66871 = CARTESIAN_POINT ( 'NONE',  ( 8.654006363156080184, 3.802134689404237378, 5.879617511049012535 ) ) ;
#66872 = EDGE_CURVE ( 'NONE', #21901, #16690, #58796, .T. ) ;
#66873 = CARTESIAN_POINT ( 'NONE',  ( 18.11163387652230483, 2.018964330316874722, -12.43719698804479101 ) ) ;
#66874 = CARTESIAN_POINT ( 'NONE',  ( 11.13109956191000016, -2.679615677191000245, 4.997638975407999951 ) ) ;
#66875 = CARTESIAN_POINT ( 'NONE',  ( 5.399998984437000438, 12.98068687585000092, 1.765643277144999912 ) ) ;
#66876 = DIRECTION ( 'NONE',  ( 1.000000000000000000, 0.000000000000000000, 0.000000000000000000 ) ) ;
#66878 = CARTESIAN_POINT ( 'NONE',  ( 9.702742433789000032, -5.491975933468000726, -7.893788029530999673 ) ) ;
#66877 = AXIS2_PLACEMENT_3D ( 'NONE', #9225, #8896, #24973 ) ;
#66879 = CARTESIAN_POINT ( 'NONE',  ( 25.08240915828700324, 11.33760612088999942, 3.319396049943999838 ) ) ;
#66880 = ORIENTED_EDGE ( 'NONE', *, *, #66932, .T. ) ;
#66881 = CARTESIAN_POINT ( 'NONE',  ( 18.00383897971137515, 1.936685752045136821, -13.86556672038938309 ) ) ;
#66882 = CARTESIAN_POINT ( 'NONE',  ( 12.78109998040213213, 0.7302151644511238882, -13.98094363559787467 ) ) ;
#66883 = CARTESIAN_POINT ( 'NONE',  ( 8.392998836384890637, 2.713269406560838259, -7.026678396099404367 ) ) ;
#66884 = CARTESIAN_POINT ( 'NONE',  ( 18.17891100654625092, -2.457162529596722766, -13.68241659861169701 ) ) ;
#66885 = CARTESIAN_POINT ( 'NONE',  ( 2.978056799211333594, 2.150913519912206695, -2.798833948393626869 ) ) ;
#66886 = CARTESIAN_POINT ( 'NONE',  ( 9.468589158772999781, 4.034680274230000308, -6.102912434217000026 ) ) ;
#66887 = CARTESIAN_POINT ( 'NONE',  ( 15.95370777310256294, 3.574818104395620200, 11.79277689209176749 ) ) ;
#66888 = ORIENTED_EDGE ( 'NONE', *, *, #66237, .F. ) ;
#66889 = CARTESIAN_POINT ( 'NONE',  ( 4.000000000000000000, -0.5625597044909159683, 2.094005558844440174 ) ) ;
#66890 = CARTESIAN_POINT ( 'NONE',  ( 18.25550288558782341, 2.707593611552285395, -13.73570038168180218 ) ) ;
#66891 = ORIENTED_EDGE ( 'NONE', *, *, #18793, .F. ) ;
#66892 = CARTESIAN_POINT ( 'NONE',  ( 10.76990035061499995, -3.768906505327899836, 6.664354444139199529 ) ) ;
#66893 = CARTESIAN_POINT ( 'NONE',  ( 25.02476365129393088, 2.919224782832727794, 11.54271202783471750 ) ) ;
#66894 = CARTESIAN_POINT ( 'NONE',  ( 8.614404719593999005, 5.030502105212999453, -6.322203460290999999 ) ) ;
#66895 = CARTESIAN_POINT ( 'NONE',  ( 23.84021428159876521, -12.96267928454988727, 3.649536305042122120 ) ) ;
#66896 = B_SPLINE_CURVE_WITH_KNOTS ( 'NONE', 3,
 ( #62680, #57782, #9894, #67579, #20730, #9539 ),
 .UNSPECIFIED., .F., .F.,
 ( 4, 2, 4 ),
 ( 0.000000000000000000, 0.5000000000000000000, 1.000000000000000000 ),
 .UNSPECIFIED. ) ;
#66897 = CARTESIAN_POINT ( 'NONE',  ( 10.43614141025499897, -3.450366949021700158, -8.478951440767898973 ) ) ;
#66898 = DIRECTION ( 'NONE',  ( 0.000000000000000000, 1.000000000000000000, 0.000000000000000000 ) ) ;
#66899 = CARTESIAN_POINT ( 'NONE',  ( 5.399998535875000449, 6.217248937900999058E-14, 3.708144902247999495E-14 ) ) ;
#66900 = ORIENTED_EDGE ( 'NONE', *, *, #35927, .F. ) ;
#66901 = DIRECTION ( 'NONE',  ( -1.000000000000000000, 0.000000000000000000, 0.000000000000000000 ) ) ;
#66902 = DIRECTION ( 'NONE',  ( -1.000000000000000000, 0.000000000000000000, 0.000000000000000000 ) ) ;
#66903 = CARTESIAN_POINT ( 'NONE',  ( 25.59994555223700274, -10.55174472786000095, 3.754934689065000164 ) ) ;
#66904 = ORIENTED_EDGE ( 'NONE', *, *, #466, .F. ) ;
#66905 = CARTESIAN_POINT ( 'NONE',  ( 10.49937419337999955, 2.985313722448000195, -6.358656051156999389 ) ) ;
#66906 = EDGE_LOOP ( 'NONE', ( #42896, #52601, #14935, #39684 ) ) ;
#66907 = CARTESIAN_POINT ( 'NONE',  ( 8.670138961223999630, 4.946050868436800307, 6.860686042446299204 ) ) ;
#66908 = CARTESIAN_POINT ( 'NONE',  ( 17.72206310054082934, -3.180756431682054242, -12.19191584669666462 ) ) ;
#66909 = CARTESIAN_POINT ( 'NONE',  ( 11.83156678923300120, -11.57054462408999917, -1.756438942007999993 ) ) ;
#66910 = EDGE_CURVE ( 'NONE', #61746, #15326, #64606, .T. ) ;
#66911 = ADVANCED_FACE ( 'NONE', ( #37795 ), #11222, .F. ) ;
#66912 = CARTESIAN_POINT ( 'NONE',  ( 24.70869262301700076, -12.32777590421999925, -2.948351121266000074 ) ) ;
#66913 = EDGE_CURVE ( 'NONE', #45182, #47043, #23016, .T. ) ;
#66914 = EDGE_CURVE ( 'NONE', #52478, #18634, #48285, .T. ) ;
#66915 = CARTESIAN_POINT ( 'NONE',  ( 9.409553643212783314, -2.475290888679036794, 8.337164624878596442 ) ) ;
#66916 = ORIENTED_EDGE ( 'NONE', *, *, #38538, .F. ) ;
#66917 = CARTESIAN_POINT ( 'NONE',  ( 11.58457173739308210, 4.937225096800481161, 6.638117766810080589 ) ) ;
#66918 = CARTESIAN_POINT ( 'NONE',  ( 3.899999503719000060, 0.000000000000000000, 0.000000000000000000 ) ) ;
#66919 = FACE_OUTER_BOUND ( 'NONE', #52738, .T. ) ;
#66920 = CARTESIAN_POINT ( 'NONE',  ( 12.53658830138314784, 3.196304600777675642, -13.63024796167575126 ) ) ;
#66921 = B_SPLINE_CURVE_WITH_KNOTS ( 'NONE', 3,
 ( #10398, #3011, #50912, #55473, #33462, #50569 ),
 .UNSPECIFIED., .F., .F.,
 ( 4, 1, 1, 4 ),
 ( 0.000000000000000000, 0.2305484662882832936, 0.8346924768963898122, 1.000000000000000000 ),
 .UNSPECIFIED. ) ;
#66922 = CARTESIAN_POINT ( 'NONE',  ( 8.975151519677000422, -3.972335373863620234, -8.778912113473998247 ) ) ;
#66923 = CARTESIAN_POINT ( 'NONE',  ( 10.65550933554000146, -4.237674644795000667, 9.105223721671999115 ) ) ;
#66924 = CARTESIAN_POINT ( 'NONE',  ( 17.85458012075704559, 0.6654101994098620132, 13.98418081573739258 ) ) ;
#66925 = FACE_OUTER_BOUND ( 'NONE', #34933, .T. ) ;
#66926 = ORIENTED_EDGE ( 'NONE', *, *, #27025, .F. ) ;
#66927 = VERTEX_POINT ( 'NONE', #60164 ) ;
#66928 = CARTESIAN_POINT ( 'NONE',  ( 9.427245280414000561, 4.989193221215000307, -6.287302145481000082 ) ) ;
#66929 = CARTESIAN_POINT ( 'NONE',  ( 23.56664675778400309, 10.37811020278999941, -9.381454169592000625 ) ) ;
#66930 = CARTESIAN_POINT ( 'NONE',  ( 12.19673284948622793, -2.643529259147591404, 13.64196713071253164 ) ) ;
#66931 = CARTESIAN_POINT ( 'NONE',  ( 23.78804273620877652, 3.294425019659333653, 13.15453432728574867 ) ) ;
#66932 = EDGE_CURVE ( 'NONE', #10742, #13026, #62141, .T. ) ;
#66933 = CARTESIAN_POINT ( 'NONE',  ( 23.81982430084200075, 9.669052596895998164, -9.332375605283999676 ) ) ;
#66934 = CARTESIAN_POINT ( 'NONE',  ( 17.79325612864500172, -3.315492466914999881, -11.22361417850999921 ) ) ;
#66936 = CARTESIAN_POINT ( 'NONE',  ( 5.200000000000000178, 0.6646153846154000400, 2.616923076922999858 ) ) ;
#66935 = CARTESIAN_POINT ( 'NONE',  ( 10.81558376188599802, -4.962881317320600338, 6.886327436977599525 ) ) ;
#66937 = CARTESIAN_POINT ( 'NONE',  ( 12.80505043854143388, 3.149899482173124987, 12.25147293255931125 ) ) ;
#66938 = VERTEX_POINT ( 'NONE', #43042 ) ;
#66939 = CARTESIAN_POINT ( 'NONE',  ( 10.74718774421000056, -2.737610732962999727, 4.827894279797999566 ) ) ;
#66940 = CARTESIAN_POINT ( 'NONE',  ( 10.77666960233000104, -2.704364821029999977, -4.799376923177000265 ) ) ;
#66941 = CARTESIAN_POINT ( 'NONE',  ( 9.416972128128000108, -4.783349162191000481, -6.231236652334000148 ) ) ;
#66942 = CARTESIAN_POINT ( 'NONE',  ( 17.95964167607823470, 0.4764818960106712575, 12.68796903437992540 ) ) ;
#66943 = CARTESIAN_POINT ( 'NONE',  ( 12.34510720040652032, -0.4232991628857526445, 12.69050643263297573 ) ) ;
#66944 = CARTESIAN_POINT ( 'NONE',  ( 18.18005044388383240, -2.499999700414728743, -12.45156116530568902 ) ) ;
#66945 = ORIENTED_EDGE ( 'NONE', *, *, #61622, .T. ) ;
#66946 = CARTESIAN_POINT ( 'NONE',  ( 11.13494815609000099, -5.334103115335000034, 5.185088833845999723 ) ) ;
#66947 = DIRECTION ( 'NONE',  ( -1.000000000000000000, 0.000000000000000000, 0.000000000000000000 ) ) ;
#66948 = B_SPLINE_CURVE_WITH_KNOTS ( 'NONE', 3,
 ( #17015, #23311, #55124, #43951 ),
 .UNSPECIFIED., .F., .F.,
 ( 4, 4 ),
 ( 0.8746471354527770581, 1.000000000000000000 ),
 .UNSPECIFIED. ) ;
#66949 = AXIS2_PLACEMENT_3D ( 'NONE', #36626, #41865, #69120 ) ;
#66950 = CARTESIAN_POINT ( 'NONE',  ( 8.189586429382003985, -5.107684026525003418, 6.413118510302999731 ) ) ;
#66951 = SURFACE_SIDE_STYLE ('',( #18730 ) ) ;
#66952 = B_SPLINE_SURFACE_WITH_KNOTS ( 'NONE', 3, 3, ( 
 ( #6534, #9445, #52099, #4204 ),
 ( #25542, #46867, #20291, #2333 ),
 ( #65947, #44312, #17732, #65608 ),
 ( #39054, #50230, #60372, #1993 ),
 ( #34846, #28925, #18075, #7232 ),
 ( #23653, #7926, #49530, #45335 ),
 ( #2674, #50572, #18420, #55128 ),
 ( #66297, #39745, #34157, #43955 ),
 ( #61065, #13527, #44657, #60025 ),
 ( #39396, #13183, #29263, #22959 ),
 ( #17375, #23315, #55476, #38703 ),
 ( #8265, #12480, #33812, #24002 ) ),
 .UNSPECIFIED., .F., .F., .F.,
 ( 4, 1, 1, 1, 1, 1, 1, 1, 1, 4 ),
 ( 4, 4 ),
 ( 0.01098209966893000031, 0.05000000000000000278, 0.1000000000000000056, 0.1499999999999999944, 0.2000000000000000111, 0.2500000000000000000, 0.2999999999999999889, 0.3499999999999999778, 0.4000000000000000222, 0.4470359006038999716 ),
 ( -0.2706693970313999720, 1.270788585263999959 ),
 .UNSPECIFIED. ) ;
#66953 = ADVANCED_FACE ( 'NONE', ( #391 ), #14048, .T. ) ;
#66954 = CARTESIAN_POINT ( 'NONE',  ( 0.3408104211468100941, -2.670907248151955571, 2.053682415916353587 ) ) ;
#66955 = CARTESIAN_POINT ( 'NONE',  ( 9.884776718858692135, 2.675334876101736814, -7.165831161227206536 ) ) ;
#66956 = ORIENTED_EDGE ( 'NONE', *, *, #6207, .F. ) ;
#66957 = CARTESIAN_POINT ( 'NONE',  ( 12.64343166449435962, -0.6040886362899388073, -12.68065483099175417 ) ) ;
#66958 = CARTESIAN_POINT ( 'NONE',  ( 11.05853765099000086, -8.013864593771998557, -6.925175679306001086 ) ) ;
#66959 = ADVANCED_FACE ( 'NONE', ( #49315 ), #43078, .T. ) ;
#66960 = CARTESIAN_POINT ( 'NONE',  ( 24.52306328729269680, -8.782889800526138657, 8.926437641650338151 ) ) ;
#66961 = CARTESIAN_POINT ( 'NONE',  ( 7.935739158771999868, 5.430400319332999715, 7.210801214872999410 ) ) ;
#66962 = CARTESIAN_POINT ( 'NONE',  ( 18.28832092538753429, -2.855728056445002494, -11.50255606616314452 ) ) ;
#66963 = ORIENTED_EDGE ( 'NONE', *, *, #24475, .F. ) ;
#66964 = CARTESIAN_POINT ( 'NONE',  ( 5.975405406625999838, -0.8123280412348000690, -1.043359539020999982 ) ) ;
#66965 = CARTESIAN_POINT ( 'NONE',  ( 7.241960841228999968, 3.508889101792000087, -8.808374944720000599 ) ) ;
#66966 = CARTESIAN_POINT ( 'NONE',  ( 10.71081754702572120, 3.646708176540620183, -8.814774986206115770 ) ) ;
#66967 = CARTESIAN_POINT ( 'NONE',  ( 1.542640132540499254, 3.058252359239899132, 1.762666431298154146 ) ) ;
#66968 = CARTESIAN_POINT ( 'NONE',  ( 10.93479632507519916, 4.557787252275099732, -8.534037301706000278 ) ) ;
#66969 = ORIENTED_EDGE ( 'NONE', *, *, #6858, .F. ) ;
#66970 = CARTESIAN_POINT ( 'NONE',  ( 9.667080975990000269, -4.541622198376999542, 5.824041840233000755 ) ) ;
#66971 = ORIENTED_EDGE ( 'NONE', *, *, #52580, .T. ) ;
#66972 = CARTESIAN_POINT ( 'NONE',  ( 21.10000000000000142, 0.000000000000000000, 0.000000000000000000 ) ) ;
#66973 = CARTESIAN_POINT ( 'NONE',  ( 9.395316940379000670, -5.146736128384000075, 6.597417125647000447 ) ) ;
#66974 = CARTESIAN_POINT ( 'NONE',  ( 18.27048575441379796, 0.1188263301541416239, -13.99950072926553979 ) ) ;
#66975 = ORIENTED_EDGE ( 'NONE', *, *, #10142, .F. ) ;
#66976 = CARTESIAN_POINT ( 'NONE',  ( 10.95792420851827664, 8.961205178941138882, -6.431113706263509755 ) ) ;
#66977 = CARTESIAN_POINT ( 'NONE',  ( 7.605092582665629486, 3.121316641526586277, 8.549894104503566794 ) ) ;
#66978 = CARTESIAN_POINT ( 'NONE',  ( 7.924878289113923557, -5.349357204871147076, 7.500005630225521358 ) ) ;
#66979 = CARTESIAN_POINT ( 'NONE',  ( 25.59994555223599733, 2.024003533649000097, -11.01554633311000053 ) ) ;
#66980 = CARTESIAN_POINT ( 'NONE',  ( 18.01273579185514961, -2.926031893951825058, 12.34206213438603150 ) ) ;
#66981 = ORIENTED_EDGE ( 'NONE', *, *, #56121, .F. ) ;
#66982 = CARTESIAN_POINT ( 'NONE',  ( 9.781666627457001439, -5.464740618746000145, 8.817321229216000589 ) ) ;
#66983 = CARTESIAN_POINT ( 'NONE',  ( 12.18211070746583680, -2.551853945028482951, -13.66227842076493104 ) ) ;
#66984 = CARTESIAN_POINT ( 'NONE',  ( 10.41476354018330852, 2.782534154164605589, -7.827184855449099921 ) ) ;
#66985 = CARTESIAN_POINT ( 'NONE',  ( 11.00503223350061610, 5.210128592361205513, 6.635071905858886510 ) ) ;
#66986 = B_SPLINE_CURVE_WITH_KNOTS ( 'NONE', 3,
 ( #36827, #58144, #32276, #22105, #38893, #43095 ),
 .UNSPECIFIED., .F., .F.,
 ( 4, 2, 4 ),
 ( 0.000000000000000000, 0.5000000000000000000, 1.000000000000000000 ),
 .UNSPECIFIED. ) ;
#66987 = FACE_OUTER_BOUND ( 'NONE', #27771, .T. ) ;
#66988 = ORIENTED_EDGE ( 'NONE', *, *, #64935, .T. ) ;
#66989 = CARTESIAN_POINT ( 'NONE',  ( 23.61437394302592452, 13.25091963169895060, -4.104830024061406846 ) ) ;
#66990 = CARTESIAN_POINT ( 'NONE',  ( 8.810863317747999801, -3.039136629551499880, -7.500000000073117512 ) ) ;
#66991 = CARTESIAN_POINT ( 'NONE',  ( 7.143022165044063065, 2.536141393688100987, -6.357131192860917324 ) ) ;
#66992 = CARTESIAN_POINT ( 'NONE',  ( 3.400000000000000355, 0.000000000000000000, 0.000000000000000000 ) ) ;
#66993 = CARTESIAN_POINT ( 'NONE',  ( 7.925196951433999715, -5.124045536972000825, 6.724518905982000305 ) ) ;
#66994 = CARTESIAN_POINT ( 'NONE',  ( 12.72272221947698689, -0.6198980793944590673, -13.88138779565238501 ) ) ;
#66995 = EDGE_CURVE ( 'NONE', #42472, #62494, #17153, .T. ) ;
#66997 = EDGE_CURVE ( 'NONE', #49685, #15848, #59846, .T. ) ;
#66996 = CARTESIAN_POINT ( 'NONE',  ( 18.11762593468203875, -2.227530255644428525, 12.51091528569613409 ) ) ;
#66998 = ORIENTED_EDGE ( 'NONE', *, *, #63982, .T. ) ;
#66999 = CARTESIAN_POINT ( 'NONE',  ( 10.81013259637009938, -5.031671030421000168, -8.062151801142800167 ) ) ;
#67000 = B_SPLINE_CURVE_WITH_KNOTS ( 'NONE', 3,
 ( #32261, #36199, #57175, #66977, #9271, #68004, #57513, #67315, #46700, #25023 ),
 .UNSPECIFIED., .F., .F.,
 ( 4, 2, 2, 2, 4 ),
 ( 0.000000000000000000, 0.2500000000000000000, 0.5000000000000000000, 0.7500000000000000000, 1.000000000000000000 ),
 .UNSPECIFIED. ) ;
#67001 = ORIENTED_EDGE ( 'NONE', *, *, #64371, .F. ) ;
#67002 = CARTESIAN_POINT ( 'NONE',  ( 10.37026939687000038, 5.571553923009999743, 7.748385725654999945 ) ) ;
#67003 = AXIS2_PLACEMENT_3D ( 'NONE', #47907, #3, #62258 ) ;
#67004 = CARTESIAN_POINT ( 'NONE',  ( 0.1499942179680000265, -2.678379783547566895, 0.7197945678028326855 ) ) ;
#67005 = CARTESIAN_POINT ( 'NONE',  ( 9.965360841230999966, 4.034680274230000308, -6.102912434217000026 ) ) ;
#67006 = CARTESIAN_POINT ( 'NONE',  ( 3.061592516560999844, 3.309521440799999770, 1.672333154171000036 ) ) ;
#67007 = CARTESIAN_POINT ( 'NONE',  ( 10.11858840337999865, -3.393395892949000014, -5.921999462319999630 ) ) ;
#67008 = DIRECTION ( 'NONE',  ( 0.000000000000000000, 0.000000000000000000, -1.000000000000000000 ) ) ;
#67009 = CARTESIAN_POINT ( 'NONE',  ( 9.593325696102663613, -2.223596456112051811, -7.416212298303232586 ) ) ;
#67010 = VERTEX_POINT ( 'NONE', #28351 ) ;
#67011 = CARTESIAN_POINT ( 'NONE',  ( 12.05610404293055993, -4.502836909561000134, 6.476063885290000322 ) ) ;
#67012 = CARTESIAN_POINT ( 'NONE',  ( 10.99933470386000067, 5.081013421858999735, 8.239043921879998678 ) ) ;
#67013 = CARTESIAN_POINT ( 'NONE',  ( 10.81294898260481041, -2.920599542025066331, -8.329474447052662711 ) ) ;
#67014 = EDGE_CURVE ( 'NONE', #53328, #68916, #12268, .T. ) ;
#67015 = CARTESIAN_POINT ( 'NONE',  ( 7.000000000000000000, -6.255435840762999966, -3.000000000000000000 ) ) ;
#67017 = DIRECTION ( 'NONE',  ( 0.000000000000000000, 1.000000000000000000, 0.000000000000000000 ) ) ;
#67016 = CARTESIAN_POINT ( 'NONE',  ( 9.504903297738000134, 3.934733353759999552, 5.704831249548000471 ) ) ;
#67018 = CARTESIAN_POINT ( 'NONE',  ( 10.28026357027499849, 4.985299147223100746, -7.690095141806899903 ) ) ;
#67019 = CARTESIAN_POINT ( 'NONE',  ( 23.50387503050299998, 0.000000000000000000, 0.000000000000000000 ) ) ;
#67020 = CARTESIAN_POINT ( 'NONE',  ( 10.21225461470299933, 3.026595211686900377, -7.747639695388999215 ) ) ;
#67021 = B_SPLINE_CURVE_WITH_KNOTS ( 'NONE', 3,
 ( #66705, #23024, #7637, #49945, #66012, #17794, #50293, #12891, #50635, #18135, #24407, #29322, #2736, #39457, #34220, #2392, #23716, #13588 ),
 .UNSPECIFIED., .F., .F.,
 ( 4, 2, 2, 2, 2, 2, 2, 2, 4 ),
 ( 0.000000000000000000, 0.1250000000000000278, 0.2500000000000000555, 0.3749999999999999445, 0.4999999999999999445, 0.6249999999999998890, 0.7499999999999998890, 0.8750000000000000000, 1.000000000000000000 ),
 .UNSPECIFIED. ) ;
#67022 = CARTESIAN_POINT ( 'NONE',  ( 17.99148514253576892, -0.5743932053697962115, 12.58690132123599525 ) ) ;
#67023 = CARTESIAN_POINT ( 'NONE',  ( 25.59994555223700274, -10.55174472786000095, 3.754934689065000164 ) ) ;
#67024 = CARTESIAN_POINT ( 'NONE',  ( 8.112357311251360059, 5.053573198694982338, -6.503562400629845364 ) ) ;
#67025 = FACE_BOUND ( 'NONE', #64904, .T. ) ;
#67026 = ORIENTED_EDGE ( 'NONE', *, *, #13683, .F. ) ;
#67027 = CARTESIAN_POINT ( 'NONE',  ( 7.165495559622000243, -2.688354259407999880, 8.140021027181001401 ) ) ;
#67028 = CARTESIAN_POINT ( 'NONE',  ( 17.98066499537650742, 1.926393605117485919, 13.86683778668631462 ) ) ;
#67029 = CARTESIAN_POINT ( 'NONE',  ( 2.500973465876000112, 3.500000000000000000, 0.000000000000000000 ) ) ;
#67030 = CARTESIAN_POINT ( 'NONE',  ( 4.599999999999999645, 1.787816316115923509, -13.88537766212462898 ) ) ;
#67031 = ORIENTED_EDGE ( 'NONE', *, *, #58006, .F. ) ;
#67032 = CARTESIAN_POINT ( 'NONE',  ( 7.037114158771000660, 4.623631324973000112, 8.651459902566999816 ) ) ;
#67033 = AXIS2_PLACEMENT_3D ( 'NONE', #7377, #18569, #50035 ) ;
#67035 = CARTESIAN_POINT ( 'NONE',  ( 0.8009734658753000502, -3.500000000000000000, 0.000000000000000000 ) ) ;
#67034 = CARTESIAN_POINT ( 'NONE',  ( 9.408709346416998187, -3.216804796119200116, -7.128095150442700145 ) ) ;
#67036 = CARTESIAN_POINT ( 'NONE',  ( 10.34266415877000078, 5.750490533313000086, -8.094415907623000450 ) ) ;
#67037 = ORIENTED_EDGE ( 'NONE', *, *, #40361, .T. ) ;
#67038 = CARTESIAN_POINT ( 'NONE',  ( 1.498890132540667164, 2.798833948393634419, -2.150913519912196925 ) ) ;
#67039 = CARTESIAN_POINT ( 'NONE',  ( 18.12392562323104173, -2.970749524062575642, -13.68118179967287951 ) ) ;
#67040 = CARTESIAN_POINT ( 'NONE',  ( 10.42380110216399913, 3.026453990125600235, 8.094557215852098864 ) ) ;
#67041 = ADVANCED_FACE ( 'NONE', ( #5629 ), #28006, .T. ) ;
#67042 = CARTESIAN_POINT ( 'NONE',  ( 10.24478558459999888, -5.265199116477000452, 8.959495174640998982 ) ) ;
#67043 = CARTESIAN_POINT ( 'NONE',  ( 23.50387503050299998, -14.00000000000000000, 0.000000000000000000 ) ) ;
#67044 = ORIENTED_EDGE ( 'NONE', *, *, #6464, .F. ) ;
#67045 = CARTESIAN_POINT ( 'NONE',  ( 11.42397234076999979, -3.432581932914000156, 11.79497283202000091 ) ) ;
#67046 = CARTESIAN_POINT ( 'NONE',  ( 11.29595444038000096, -2.828863075736999910, -8.191124550002999882 ) ) ;
#67047 = AXIS2_PLACEMENT_3D ( 'NONE', #7093, #58849, #54645 ) ;
#67048 = CARTESIAN_POINT ( 'NONE',  ( 7.938552267647699168, -2.277490889987867639, 7.743639942309443747 ) ) ;
#67049 = CARTESIAN_POINT ( 'NONE',  ( 10.43579701286999928, -2.587605342384000195, 6.390039770907999461 ) ) ;
#67050 = CARTESIAN_POINT ( 'NONE',  ( 10.81013259637009938, -5.031671030421000168, -8.062151801142800167 ) ) ;
#67051 = CARTESIAN_POINT ( 'NONE',  ( 9.801355082327999568, -4.572497688003699601, 8.643954013369999245 ) ) ;
#67052 = ORIENTED_EDGE ( 'NONE', *, *, #40926, .F. ) ;
#67053 = DIRECTION ( 'NONE',  ( 1.000000000000000000, 0.000000000000000000, 0.000000000000000000 ) ) ;
#67054 = CARTESIAN_POINT ( 'NONE',  ( 0.5120809256593666925, 3.099336848560416247, -1.647554626188311167 ) ) ;
#67055 = VERTEX_POINT ( 'NONE', #1428 ) ;
#67056 = DIRECTION ( 'NONE',  ( -1.000000000000000000, -4.956352788505168356E-14, -1.734723475976808988E-14 ) ) ;
#67057 = VERTEX_POINT ( 'NONE', #17512 ) ;
#67058 = CARTESIAN_POINT ( 'NONE',  ( 9.531727112333999941, -4.010297355695000121, -9.208122400763999238 ) ) ;
#67059 = CARTESIAN_POINT ( 'NONE',  ( 9.152520280414000453, 4.102804347295999854, -5.770625657082999460 ) ) ;
#67060 = CARTESIAN_POINT ( 'NONE',  ( 19.89999890908300273, -12.52500000000000036, 0.000000000000000000 ) ) ;
#67061 = CARTESIAN_POINT ( 'NONE',  ( 8.228368194308000483, 4.806758213781000322, 6.177034601037000527 ) ) ;
#67062 = CARTESIAN_POINT ( 'NONE',  ( 12.23374516775628784, 2.245741837849041911, -12.50722324768529781 ) ) ;
#67063 = CARTESIAN_POINT ( 'NONE',  ( 12.17918044953561996, -2.988516238873000219, 6.972563939641199582 ) ) ;
#67064 = FACE_OUTER_BOUND ( 'NONE', #12189, .T. ) ;
#67065 = ORIENTED_EDGE ( 'NONE', *, *, #18232, .T. ) ;
#67066 = CARTESIAN_POINT ( 'NONE',  ( 9.099999931440999390, -4.000000000000000000, -7.500000000000000000 ) ) ;
#67067 = CARTESIAN_POINT ( 'NONE',  ( 8.764831853209999579, -5.808258301303999893, 7.446016267012000256 ) ) ;
#67068 = LINE ( 'NONE', #66730, #39113 ) ;
#67069 = ORIENTED_EDGE ( 'NONE', *, *, #46319, .T. ) ;
#67070 = CARTESIAN_POINT ( 'NONE',  ( 12.11312973616749034, -2.264845417406519346, -12.39478132878350358 ) ) ;
#67071 = CARTESIAN_POINT ( 'NONE',  ( 11.25656651104150008, 4.126085365637900182, 8.771777834828998976 ) ) ;
#67072 = CARTESIAN_POINT ( 'NONE',  ( 10.77401935321000082, -3.826867196099999813, -5.823197386290999589 ) ) ;
#67073 = CARTESIAN_POINT ( 'NONE',  ( 9.209122513651813335, 5.100000000000000533, 6.320295141290149132 ) ) ;
#67074 = CARTESIAN_POINT ( 'NONE',  ( 17.75870478550200104, -3.641518898264000548, -12.02435208579999859 ) ) ;
#67075 = CARTESIAN_POINT ( 'NONE',  ( 9.002376473208929752, 3.077871436655787996, -8.207577963560542145 ) ) ;
#67076 = CARTESIAN_POINT ( 'NONE',  ( 12.75679378108278961, -3.246933784478224450, -13.61827548339043403 ) ) ;
#67077 = DIRECTION ( 'NONE',  ( 1.000000000000000000, 0.000000000000000000, 0.000000000000000000 ) ) ;
#67078 = CARTESIAN_POINT ( 'NONE',  ( 10.59195391537400077, -2.942766577210000012, -8.218034727798299244 ) ) ;
#67079 = EDGE_CURVE ( 'NONE', #47667, #14966, #64270, .T. ) ;
#67081 = EDGE_CURVE ( 'NONE', #34904, #6782, #17953, .T. ) ;
#67080 = FACE_OUTER_BOUND ( 'NONE', #50081, .T. ) ;
#67082 = ORIENTED_EDGE ( 'NONE', *, *, #65643, .T. ) ;
#67083 = ORIENTED_EDGE ( 'NONE', *, *, #3647, .T. ) ;
#67084 = B_SPLINE_CURVE_WITH_KNOTS ( 'NONE', 3,
 ( #8407, #55956, #40226, #35328, #51397, #24487 ),
 .UNSPECIFIED., .F., .F.,
 ( 4, 2, 4 ),
 ( 0.000000000000000000, 0.5000000000000000000, 1.000000000000000000 ),
 .UNSPECIFIED. ) ;
#67085 =( NAMED_UNIT ( * ) SI_UNIT ( $, .STERADIAN. ) SOLID_ANGLE_UNIT ( ) );
#67086 = DIRECTION ( 'NONE',  ( -1.000000000000000000, 0.000000000000000000, 0.000000000000000000 ) ) ;
#67087 = CARTESIAN_POINT ( 'NONE',  ( 17.94485468269862238, 2.989306481654914194, 13.55738131293089666 ) ) ;
#67088 = CARTESIAN_POINT ( 'NONE',  ( 24.42400389426000373, -3.752283608186000041, 12.53632670480000044 ) ) ;
#67089 = CARTESIAN_POINT ( 'NONE',  ( 8.688561307509338860, 5.076530052485727751, 6.260338817618603002 ) ) ;
#67090 = CARTESIAN_POINT ( 'NONE',  ( 18.05338926791294440, 2.122656057830398790, 12.53150860927892296 ) ) ;
#67091 = CARTESIAN_POINT ( 'NONE',  ( 18.04816728597000264, 3.610133590554000182, -12.03375048192000207 ) ) ;
#67092 = CARTESIAN_POINT ( 'NONE',  ( 9.104014120666999332, 5.045862207587999748, 8.527865280865999154 ) ) ;
#67094 = AXIS2_PLACEMENT_3D ( 'NONE', #33154, #28248, #49568 ) ;
#67093 = B_SPLINE_CURVE_WITH_KNOTS ( 'NONE', 3,
 ( #48842, #42905, #948, #43601 ),
 .UNSPECIFIED., .F., .F.,
 ( 4, 4 ),
 ( 0.000000000000000000, 1.000000000000000000 ),
 .UNSPECIFIED. ) ;
#67095 = CARTESIAN_POINT ( 'NONE',  ( 9.448279512853625661, -3.525202972512352595, 8.234914996158446243 ) ) ;
#67096 = EDGE_LOOP ( 'NONE', ( #26897, #17778 ) ) ;
#67097 = CARTESIAN_POINT ( 'NONE',  ( 12.44669855353773080, -1.987833209345829300, 12.55628527126821226 ) ) ;
#67098 = CARTESIAN_POINT ( 'NONE',  ( 9.401721904869997815, -3.124169273628900179, -7.991693846894699860 ) ) ;
#67099 = CARTESIAN_POINT ( 'NONE',  ( 9.757669403192000601, 4.489270656625000022, 5.986034819543999852 ) ) ;
#67100 = EDGE_CURVE ( 'NONE', #9579, #33910, #33806, .T. ) ;
#67101 = CARTESIAN_POINT ( 'NONE',  ( 11.51790547754520055, -2.825704134258000266, 7.462730980357120458 ) ) ;
#67102 = EDGE_CURVE ( 'NONE', #19484, #21434, #22145, .T. ) ;
#67103 = CARTESIAN_POINT ( 'NONE',  ( 11.30579707368350029, 3.365167912142600137, -6.390809033205999690 ) ) ;
#67104 = CARTESIAN_POINT ( 'NONE',  ( 12.18532624936141673, 0.08167875237852871562, 12.69965198491186342 ) ) ;
#67105 = CARTESIAN_POINT ( 'NONE',  ( 8.122954719591000128, 3.566637212418000136, 5.743604853744000316 ) ) ;
#67106 = CARTESIAN_POINT ( 'NONE',  ( 9.972850246170999355, 5.044468801812000081, 6.258104779495000436 ) ) ;
#67107 = CARTESIAN_POINT ( 'NONE',  ( 12.20865459317944435, 2.312811904845647248, 12.49320495213146032 ) ) ;
#67108 = ORIENTED_EDGE ( 'NONE', *, *, #52390, .F. ) ;
#67109 = CARTESIAN_POINT ( 'NONE',  ( 25.37646820717300145, 8.494765293177998444, 7.922169669001000614 ) ) ;
#67110 = CARTESIAN_POINT ( 'NONE',  ( 10.44426222744799837, 3.013556901740999994, -8.312555471636301263 ) ) ;
#67111 = CARTESIAN_POINT ( 'NONE',  ( 10.77788359937968998, -4.967860659007850899, 8.954442448909505359 ) ) ;
#67113 = DIRECTION ( 'NONE',  ( 0.000000000000000000, 0.000000000000000000, -1.000000000000000000 ) ) ;
#67112 = CARTESIAN_POINT ( 'NONE',  ( 7.983191940377000861, -5.321924421352999701, 8.118250081378000971 ) ) ;
#67114 = CARTESIAN_POINT ( 'NONE',  ( 10.16684687351567007, 4.768183399968648040, -6.500416447002280051 ) ) ;
#67115 = CARTESIAN_POINT ( 'NONE',  ( 11.75718044953559804, -3.110233631466100324, -7.963966784336999005 ) ) ;
#67116 = ORIENTED_EDGE ( 'NONE', *, *, #54400, .F. ) ;
#67117 = CARTESIAN_POINT ( 'NONE',  ( 1.677382716469999924, -1.296472565164999979, 3.528106597684999901 ) ) ;
#67118 = CARTESIAN_POINT ( 'NONE',  ( 17.94287612687506694, -0.4902485962753033166, -12.68726381690838778 ) ) ;
#67120 = CARTESIAN_POINT ( 'NONE',  ( 11.48381255716000027, 3.703723199601000271, -11.90766076753999947 ) ) ;
#67119 = DIRECTION ( 'NONE',  ( 2.186536431443105034E-10, -0.8764392776392420092, 0.4815124013057229813 ) ) ;
#67121 = DIRECTION ( 'NONE',  ( 0.000000000000000000, 1.000000000000000000, 0.000000000000000000 ) ) ;
#67122 = CARTESIAN_POINT ( 'NONE',  ( 25.59997239626699894, -8.218962899087999929, 8.043524294852000267 ) ) ;
#67123 = CARTESIAN_POINT ( 'NONE',  ( 15.58179592144799486, 8.803826609192167751, 7.629963841725643903 ) ) ;
#67124 = DIRECTION ( 'NONE',  ( -1.000000000000000000, 0.000000000000000000, 0.000000000000000000 ) ) ;
#67125 = LINE ( 'NONE', #55274, #43336 ) ;
#67126 = CARTESIAN_POINT ( 'NONE',  ( 8.309480646794000336, -2.905864338704999827, 8.940687151810998046 ) ) ;
#67127 = ORIENTED_EDGE ( 'NONE', *, *, #39979, .T. ) ;
#67128 = CARTESIAN_POINT ( 'NONE',  ( 7.481079719589999399, 2.374037589774999901, 8.293392681990997772 ) ) ;
#67129 = CARTESIAN_POINT ( 'NONE',  ( 11.58810207955109917, 3.203462856645999945, -7.174999999999999822 ) ) ;
#67130 = CARTESIAN_POINT ( 'NONE',  ( 7.340118112958106344, -3.660443313038189928, 9.214377072997308460 ) ) ;
#67131 = CARTESIAN_POINT ( 'NONE',  ( 10.70440763477068558, -2.684940916868676641, 7.852706794445921901 ) ) ;
#67132 = CARTESIAN_POINT ( 'NONE',  ( 1.075700459007000065, -0.3467249428283000201, -3.408020022541999872 ) ) ;
#67133 = ORIENTED_EDGE ( 'NONE', *, *, #56460, .T. ) ;
#67134 = PLANE ( 'NONE',  #23242 ) ;
#67135 = CARTESIAN_POINT ( 'NONE',  ( 10.95672469555900008, -3.566534988568399900, 8.249937779480299938 ) ) ;
#67136 = CARTESIAN_POINT ( 'NONE',  ( 10.92087510617160540, -4.925384977304763545, -9.003857666150715033 ) ) ;
#67137 = CARTESIAN_POINT ( 'NONE',  ( 9.534905769125000319, 3.030948166328000237, 8.761984216465000586 ) ) ;
#67138 = CARTESIAN_POINT ( 'NONE',  ( 10.29262282008599882, 4.451581486939200083, 6.771613406921599854 ) ) ;
#67140 = CARTESIAN_POINT ( 'NONE',  ( 11.06049777433069892, 3.148547701490199913, -7.174999999999999822 ) ) ;
#67139 = CONICAL_SURFACE ( 'NONE', #45940, 1.900023899775999947, 0.7853981633972997312 ) ;
#67141 = CARTESIAN_POINT ( 'NONE',  ( 10.06949314679000018, -4.910373174915999783, -8.649593977693999847 ) ) ;
#67142 = CARTESIAN_POINT ( 'NONE',  ( 17.91964795130429877, 0.5080432161604431229, -13.88750743611951144 ) ) ;
#67143 = CARTESIAN_POINT ( 'NONE',  ( 11.49999672495000169, 3.632761979779000061, -11.06912554803999882 ) ) ;
#67144 = CARTESIAN_POINT ( 'NONE',  ( 11.23424042080529972, 4.544092497359197402, -6.342116603374311268 ) ) ;
#67145 = CARTESIAN_POINT ( 'NONE',  ( 8.550530719455091244, 3.458520770602964589, 5.843532653519790898 ) ) ;
#67146 = ORIENTED_EDGE ( 'NONE', *, *, #1611, .F. ) ;
#67147 = CARTESIAN_POINT ( 'NONE',  ( 17.77706283214427785, -1.915668542326107726, 13.78016448532189386 ) ) ;
#67148 = CARTESIAN_POINT ( 'NONE',  ( 17.59634971246090984, 3.125000000000000000, -13.52084437902332681 ) ) ;
#67149 = ORIENTED_EDGE ( 'NONE', *, *, #8276, .F. ) ;
#67150 = ORIENTED_EDGE ( 'NONE', *, *, #11731, .F. ) ;
#67151 = CARTESIAN_POINT ( 'NONE',  ( 17.55505043854143565, 2.500000000000000000, -25.00000000000000000 ) ) ;
#67152 = CARTESIAN_POINT ( 'NONE',  ( 9.760596873516666605, 3.370476274536378547, -6.407767014557177454 ) ) ;
#67153 = DIRECTION ( 'NONE',  ( -1.000000000000000000, 0.000000000000000000, 0.000000000000000000 ) ) ;
#67154 = AXIS2_PLACEMENT_3D ( 'NONE', #47395, #31316, #67325 ) ;
#67155 = CARTESIAN_POINT ( 'NONE',  ( 9.753142190738998352, 4.104977339646000090, 9.293283246364000050 ) ) ;
#67156 = DIRECTION ( 'NONE',  ( 0.9999999999999997780, -1.366939932386999783E-09, -2.239632587909999191E-08 ) ) ;
#67157 = CARTESIAN_POINT ( 'NONE',  ( 7.550000000000000711, 4.000000000000000000, 8.849999999999999645 ) ) ;
#67158 = CARTESIAN_POINT ( 'NONE',  ( 11.29621718459000057, -3.561654022787999807, 6.266039799355000106 ) ) ;
#67159 = CARTESIAN_POINT ( 'NONE',  ( 18.13088395572279765, -0.4376617689587271043, -12.59240970319242514 ) ) ;
#67160 = CARTESIAN_POINT ( 'NONE',  ( 10.56270535986999981, -2.509383044034000143, -8.602408326857998944 ) ) ;
#67161 = CARTESIAN_POINT ( 'NONE',  ( 11.39210538575740017, -3.157545584346100220, -7.298582155985900322 ) ) ;
#67162 = EDGE_CURVE ( 'NONE', #10085, #51086, #13007, .T. ) ;
#67164 = ADVANCED_FACE ( 'NONE', ( #10071 ), #68443, .F. ) ;
#67163 = FACE_BOUND ( 'NONE', #5061, .T. ) ;
#67165 = EDGE_LOOP ( 'NONE', ( #57634, #31362, #61916, #38477, #32105 ) ) ;
#67166 = CARTESIAN_POINT ( 'NONE',  ( 10.96256888877000080, -6.761399355091999297, -5.456120342596999073 ) ) ;
#67167 = SURFACE_STYLE_USAGE ( .BOTH. , #46550 ) ;
#67168 = DIRECTION ( 'NONE',  ( -0.7071065545305982303, 0.000000000000000000, -0.7071070078424241956 ) ) ;
#67169 = CARTESIAN_POINT ( 'NONE',  ( 8.832144816391009456, 4.216552416542988624, 6.534094574943864586 ) ) ;
#67170 = CARTESIAN_POINT ( 'NONE',  ( 9.456405316140999773, 3.728406863338599830, -8.750048621292000561 ) ) ;
#67171 = CARTESIAN_POINT ( 'NONE',  ( 12.33410680267662762, 3.073228032305981738, 13.65852590327789784 ) ) ;
#67172 = CARTESIAN_POINT ( 'NONE',  ( 10.30047649312000146, -4.027768368024999823, 9.431342508940000258 ) ) ;
#67173 = VERTEX_POINT ( 'NONE', #57973 ) ;
#67174 = CARTESIAN_POINT ( 'NONE',  ( 12.32512882958489797, 0.4004146478932060216, -12.69150435581204661 ) ) ;
#67175 = CARTESIAN_POINT ( 'NONE',  ( 12.18940025506974401, -0.3858260082455265971, 13.99468631105251859 ) ) ;
#67176 = ORIENTED_EDGE ( 'NONE', *, *, #37310, .F. ) ;
#67177 = CARTESIAN_POINT ( 'NONE',  ( 10.98768472639999949, 2.860903110339000133, 4.945212061661000469 ) ) ;
#67178 = CARTESIAN_POINT ( 'NONE',  ( 6.999999691988000095, -1.865174681369999698E-13, 1.040631529540999901E-13 ) ) ;
#67179 = CARTESIAN_POINT ( 'NONE',  ( 15.95676543642414025, 9.288185316739934194, 8.402783510542153778 ) ) ;
#67180 = CARTESIAN_POINT ( 'NONE',  ( 8.469851049286248212, 3.034069930634795575, 6.168783214997897169 ) ) ;
#67181 = TOROIDAL_SURFACE ( 'NONE', #48270, 7.720759220056000238, 1.000000000000000000 ) ;
#67182 = B_SPLINE_CURVE_WITH_KNOTS ( 'NONE', 3,
 ( #23976, #2647, #55797, #59999 ),
 .UNSPECIFIED., .F., .F.,
 ( 4, 4 ),
 ( 0.000000000000000000, 1.000000000000000000 ),
 .UNSPECIFIED. ) ;
#67183 = ADVANCED_FACE ( 'NONE', ( #21252 ), #10757, .T. ) ;
#67184 = CARTESIAN_POINT ( 'NONE',  ( 10.31905590579000176, 2.899999999999999911, -6.571291218949999902 ) ) ;
#67185 = CARTESIAN_POINT ( 'NONE',  ( 17.60000001947600268, -11.86186880240999919, 3.298627760718999991 ) ) ;
#67186 = CARTESIAN_POINT ( 'NONE',  ( 11.03681693200000069, 2.776621198269999979, 5.023845135586999966 ) ) ;
#67187 = CARTESIAN_POINT ( 'NONE',  ( 12.60431942020948526, 3.171686099353042909, 12.19427817519220092 ) ) ;
#67188 = DIRECTION ( 'NONE',  ( -1.000000000000000000, 0.000000000000000000, 0.000000000000000000 ) ) ;
#67189 = CARTESIAN_POINT ( 'NONE',  ( 10.48133997687999930, 4.184599793140999502, -6.653701289769800020 ) ) ;
#67190 = CARTESIAN_POINT ( 'NONE',  ( 6.899999691988000450, -12.20988339176000004, -3.111064831550000243 ) ) ;
#67191 = CARTESIAN_POINT ( 'NONE',  ( 11.15278751119019773, 3.209519379020799867, -7.913556523549700294 ) ) ;
#67192 = CARTESIAN_POINT ( 'NONE',  ( 10.13922949779699856, 4.633452903845899584, -8.449985803660998940 ) ) ;
#67194 = CARTESIAN_POINT ( 'NONE',  ( 12.41685245958457884, 2.003519757588521522, 12.55365090554869134 ) ) ;
#67193 = LINE ( 'NONE', #13730, #3997 ) ;
#67195 = CARTESIAN_POINT ( 'NONE',  ( 23.60440866767097745, -13.39487733609081843, 3.977422972493961595 ) ) ;
#67196 = ORIENTED_EDGE ( 'NONE', *, *, #26833, .F. ) ;
#67197 = AXIS2_PLACEMENT_3D ( 'NONE', #41998, #5273, #53171 ) ;
#67198 = CARTESIAN_POINT ( 'NONE',  ( 10.90346005378009941, 4.786957292481900161, 7.920222357891399945 ) ) ;
#67199 = AXIS2_PLACEMENT_3D ( 'NONE', #48438, #58239, #52648 ) ;
#67200 = CARTESIAN_POINT ( 'NONE',  ( 10.18755811987000115, -5.387486580809999204, 8.640943191857999750 ) ) ;
#67201 = CARTESIAN_POINT ( 'NONE',  ( 9.327747021775998348, 3.141778309999299967, 6.746879837742599584 ) ) ;
#67202 = DIRECTION ( 'NONE',  ( 1.000000000000000000, 0.000000000000000000, 0.000000000000000000 ) ) ;
#67203 = CARTESIAN_POINT ( 'NONE',  ( 10.87522165821000009, -4.831071966430999787, 6.312786525516999703 ) ) ;
#67204 = DIRECTION ( 'NONE',  ( -1.000000000000000000, 0.000000000000000000, 0.000000000000000000 ) ) ;
#67205 = CARTESIAN_POINT ( 'NONE',  ( 7.100000000000000533, 4.000000000000000000, 7.500000000000000000 ) ) ;
#67206 = EDGE_LOOP ( 'NONE', ( #36819, #52946, #9214, #36781 ) ) ;
#67207 = B_SPLINE_CURVE_WITH_KNOTS ( 'NONE', 3,
 ( #51678, #57261, #24773, #15655, #52016, #46786, #41534, #36289, #9713, #31058, #46100, #52368, #4461, #20901, #36988, #3436, #48854, #59333 ),
 .UNSPECIFIED., .F., .F.,
 ( 4, 2, 2, 2, 2, 2, 2, 2, 4 ),
 ( 0.000000000000000000, 0.1250000000000000000, 0.2500000000000000000, 0.3750000000000000000, 0.5000000000000000000, 0.6250000000000000000, 0.7500000000000000000, 0.8750000000000000000, 1.000000000000000000 ),
 .UNSPECIFIED. ) ;
#67208 = CARTESIAN_POINT ( 'NONE',  ( 8.847442991499999465, -4.071878040089889517, -6.360452723514999462 ) ) ;
#67209 = DIRECTION ( 'NONE',  ( 1.000000000000000000, 0.000000000000000000, 0.000000000000000000 ) ) ;
#67210 = CARTESIAN_POINT ( 'NONE',  ( 12.10988784977536525, -4.851105903694400645, 7.548634759728509280 ) ) ;
#67211 = CARTESIAN_POINT ( 'NONE',  ( 18.20249588168626786, 2.156032850912784404, -12.41417075669994219 ) ) ;
#67212 = CARTESIAN_POINT ( 'NONE',  ( 2.667640132542667963, -1.762666431298160141, 3.058252359239895579 ) ) ;
#67213 = PLANE ( 'NONE',  #13872 ) ;
#67214 = EDGE_CURVE ( 'NONE', #14991, #59582, #49821, .T. ) ;
#67215 = EDGE_CURVE ( 'NONE', #15615, #50564, #30462, .T. ) ;
#67216 = CARTESIAN_POINT ( 'NONE',  ( 12.33541982639859036, 2.912513636879463075, -13.57727066180432196 ) ) ;
#67217 = CARTESIAN_POINT ( 'NONE',  ( 9.881332132140999036, -4.333399685216000385, -9.088699530815999239 ) ) ;
#67218 = DIRECTION ( 'NONE',  ( 1.000000000000000000, 0.000000000000000000, 0.000000000000000000 ) ) ;
#67219 = ORIENTED_EDGE ( 'NONE', *, *, #18095, .F. ) ;
#67220 = CARTESIAN_POINT ( 'NONE',  ( -0.000000000000000000, -1.781870588985605464, -2.319407620233724820 ) ) ;
#67221 = CARTESIAN_POINT ( 'NONE',  ( 5.200000000963999724, 1.599999999036000098, -2.855877288059999651E-09 ) ) ;
#67222 = CARTESIAN_POINT ( 'NONE',  ( 13.46018463513500052, -9.195629459350000090, -7.535158378801000367 ) ) ;
#67223 = CARTESIAN_POINT ( 'NONE',  ( 17.80000000009400196, 3.216307036143000175, -11.40341376487999980 ) ) ;
#67224 = CARTESIAN_POINT ( 'NONE',  ( 18.17813554646084029, 2.450019327289897575, 12.46306814184580425 ) ) ;
#67225 = CARTESIAN_POINT ( 'NONE',  ( 8.971339158776000744, 4.082930418187999955, -6.104944817728999773 ) ) ;
#67226 = DIRECTION ( 'NONE',  ( 0.000000000000000000, 0.7071067811865474617, -0.7071067811865474617 ) ) ;
#67227 = ORIENTED_EDGE ( 'NONE', *, *, #36325, .T. ) ;
#67228 = CARTESIAN_POINT ( 'NONE',  ( 4.000000000000000000, 2.149963194831999935, 0.1424560705006994998 ) ) ;
#67229 = CARTESIAN_POINT ( 'NONE',  ( 18.03491643637239150, 3.065379368238251079, -13.66028979695642853 ) ) ;
#67230 = ORIENTED_EDGE ( 'NONE', *, *, #46883, .F. ) ;
#67231 = CARTESIAN_POINT ( 'NONE',  ( 10.64325461470300027, -4.840245908677600184, 7.286236678332599581 ) ) ;
#67232 = CARTESIAN_POINT ( 'NONE',  ( 11.14393020684970104, -2.750000000000000000, 7.500000000000000000 ) ) ;
#67233 = CARTESIAN_POINT ( 'NONE',  ( 8.555820280412000045, 2.414630869937000046, -6.801495146585999407 ) ) ;
#67234 = DIRECTION ( 'NONE',  ( 0.000000000000000000, -1.000000000000000000, 0.000000000000000000 ) ) ;
#67235 = CARTESIAN_POINT ( 'NONE',  ( 11.35545123989519922, -3.524778630617700248, -8.417769225118700405 ) ) ;
#67236 = CARTESIAN_POINT ( 'NONE',  ( 13.69992376746900042, -12.26631831379999937, -2.532779022035999805 ) ) ;
#67237 = DIRECTION ( 'NONE',  ( 1.000000000000000000, 0.000000000000000000, 0.000000000000000000 ) ) ;
#67238 = ORIENTED_EDGE ( 'NONE', *, *, #1524, .T. ) ;
#67239 = CARTESIAN_POINT ( 'NONE',  ( 3.452384183491000069, 1.140396268832999827, -3.309002319436000317 ) ) ;
#67240 = CARTESIAN_POINT ( 'NONE',  ( 10.60434687351566474, -2.749999999999998224, 7.663624617374462211 ) ) ;
#67242 = ADVANCED_FACE ( 'NONE', ( #36298 ), #42581, .T. ) ;
#67241 = CARTESIAN_POINT ( 'NONE',  ( 8.929995280412999392, 5.030502105212999453, -6.322203460290999999 ) ) ;
#67243 = ORIENTED_EDGE ( 'NONE', *, *, #11924, .F. ) ;
#67244 = AXIS2_PLACEMENT_3D ( 'NONE', #44884, #51491, #35087 ) ;
#67245 = CARTESIAN_POINT ( 'NONE',  ( 10.00074698269999907, 2.373893144840999891, -7.962435130300000274 ) ) ;
#67246 = EDGE_CURVE ( 'NONE', #1476, #33164, #37332, .T. ) ;
#67247 = ORIENTED_EDGE ( 'NONE', *, *, #24719, .T. ) ;
#67248 = CARTESIAN_POINT ( 'NONE',  ( 8.594151519676998419, 4.024693162376980382, 6.358456126310000123 ) ) ;
#67249 = CARTESIAN_POINT ( 'NONE',  ( 17.89634705932800074, -1.976313534945129291, -12.55826774113815425 ) ) ;
#67250 = AXIS2_PLACEMENT_3D ( 'NONE', #36924, #53000, #5096 ) ;
#67251 = CARTESIAN_POINT ( 'NONE',  ( 11.26443347348000046, -11.78677031080999882, -1.538950076482000107 ) ) ;
#67252 = DIRECTION ( 'NONE',  ( 0.000000000000000000, 0.8648648648648717963, 0.5020047465136829867 ) ) ;
#67253 = CARTESIAN_POINT ( 'NONE',  ( 9.370475807310532090, -3.052722418981052233, 8.962984445555635560 ) ) ;
#67254 = ORIENTED_EDGE ( 'NONE', *, *, #722, .F. ) ;
#67255 = CARTESIAN_POINT ( 'NONE',  ( 8.616995677562000466, 4.876077402042000131, 5.996974966532000018 ) ) ;
#67256 = CARTESIAN_POINT ( 'NONE',  ( 10.46298584122999920, 3.993164721578000176, -6.140176455708999725 ) ) ;
#67257 = CARTESIAN_POINT ( 'NONE',  ( 11.13092457518000167, -5.324127713801000361, -5.001427652733999807 ) ) ;
#67258 = CARTESIAN_POINT ( 'NONE',  ( 12.08891106753597633, 2.402099963521329595, -13.79240636836165201 ) ) ;
#67259 = CARTESIAN_POINT ( 'NONE',  ( 9.329759580229000093, -5.244164909883999748, -7.202614619576299226 ) ) ;
#67260 = EDGE_CURVE ( 'NONE', #41499, #49026, #34548, .T. ) ;
#67261 = CARTESIAN_POINT ( 'NONE',  ( 18.27048575441378375, -0.1188263301541328115, 13.99950072926553446 ) ) ;
#67262 = CARTESIAN_POINT ( 'NONE',  ( 17.71321509766717739, 11.53250522934357036, -4.886416279629735016 ) ) ;
#67263 = PLANE ( 'NONE',  #67618 ) ;
#67264 = EDGE_LOOP ( 'NONE', ( #48171, #40918, #24422, #58003 ) ) ;
#67265 = ORIENTED_EDGE ( 'NONE', *, *, #48129, .T. ) ;
#67266 = CARTESIAN_POINT ( 'NONE',  ( 9.228345280414000484, 2.481540185810000132, -7.878707153279001396 ) ) ;
#67267 = DIRECTION ( 'NONE',  ( 0.000000000000000000, -1.000000000000000000, 0.000000000000000000 ) ) ;
#67268 = CARTESIAN_POINT ( 'NONE',  ( 8.266851002545999805, -2.832432432432000269, 6.822293592207000934 ) ) ;
#67269 = CARTESIAN_POINT ( 'NONE',  ( 24.03569479623928018, 3.344478585231344780, 12.68125857544483637 ) ) ;
#67271 = CARTESIAN_POINT ( 'NONE',  ( 23.55064458304499908, 10.43113086418000002, -9.391476572615999885 ) ) ;
#67270 =( REPRESENTATION_RELATIONSHIP ('NONE','NONE', #10823, #12958 ) REPRESENTATION_RELATIONSHIP_WITH_TRANSFORMATION ( #49082 )SHAPE_REPRESENTATION_RELATIONSHIP( ) );
#67272 = DIRECTION ( 'NONE',  ( -3.827499907199999809E-10, -3.827498985732999890E-10, -1.000000000000000000 ) ) ;
#67274 = CARTESIAN_POINT ( 'NONE',  ( 8.785641572568696489, 4.855572132619596637, 9.057504313711934429 ) ) ;
#67273 = CARTESIAN_POINT ( 'NONE',  ( 10.15702593514599883, -4.165792341207500193, 8.629711178834000407 ) ) ;
#67275 = CARTESIAN_POINT ( 'NONE',  ( 8.755241167949000314, -5.090758519327002851, -6.463251571066001233 ) ) ;
#67276 = EDGE_LOOP ( 'NONE', ( #17844, #59070, #1544, #61111, #57194 ) ) ;
#67277 = CIRCLE ( 'NONE', #56111, 2.199999999999999734 ) ;
#67278 = CARTESIAN_POINT ( 'NONE',  ( 10.27381073070999840, -3.247454413448000121, 4.596980832202000045 ) ) ;
#67279 = CARTESIAN_POINT ( 'NONE',  ( 24.35365242081699932, -10.79182034090998776, -4.028979491970003934 ) ) ;
#67280 = CARTESIAN_POINT ( 'NONE',  ( 9.575728814717999526, -3.111669560323000017, -8.958991988670002016 ) ) ;
#67281 = CARTESIAN_POINT ( 'NONE',  ( 7.953506848056347778, 4.927760041869837515, 6.408859279631051287 ) ) ;
#67282 = B_SPLINE_CURVE_WITH_KNOTS ( 'NONE', 3,
 ( #11375, #43899, #59969, #33758, #1587, #44603, #23259, #65894, #55073, #64505, #38999, #16962, #54028, #16626, #49475, #49132, #54727, #7178, #22903, #27827, #11719, #37951, #32716, #6130, #27467, #48794, #28514, #44257, #65203, #903, #33061, #1244, #38295, #22216, #54375, #22557, #17320, #17676, #65553, #60318, #37836, #21748, #27010, #64734, #22094, #57781, #43081, #43439, #9893, #64387, #21074, #31233, #68609, #59158, #4637, #16850, #52540, #16508, #11262, #58473, #90, #63712, #58816, #58134, #47650, #25976, #32599, #47305, #53913, #10923, #26675, #31917, #64046, #20729, #5669, #42058, #32265, #63362, #15489, #42404, #48328, #36816, #53576, #21408, #5330, #6013, #27352, #53231, #433, #47988, #42742, #37491, #4988 ),
 .UNSPECIFIED., .F., .F.,
 ( 4, 2, 2, 2, 2, 2, 2, 2, 2, 1, 1, 2, 2, 2, 2, 2, 2, 2, 2, 2, 2, 2, 2, 2, 2, 2, 2, 2, 2, 2, 2, 2, 2, 1, 1, 2, 2, 2, 2, 1, 2, 2, 2, 2, 2, 2, 2, 2, 4 ),
 ( 0.000000000000000000, 0.03125000000000013878, 0.06250000000000027756, 0.09375000000000041633, 0.1093750000000004441, 0.1250000000000004718, 0.1562499999999978628, 0.1718749999999965583, 0.1874999999999952816, 0.2031249999999939770, 0.2109374999999943934, 0.2148437499999936162, 0.2187499999999929223, 0.2499999999999870659, 0.2656249999999834577, 0.2734374999999816258, 0.2812499999999797384, 0.2968749999999760192, 0.3124999999999722444, 0.3437499999999646949, 0.3593749999999609201, 0.3749999999999570899, 0.4062499999999493738, 0.4374999999999417133, 0.4999999999999258371, 0.5312499999999178435, 0.5624999999999098499, 0.5937499999999019673, 0.6093749999998983036, 0.6249999999998947509, 0.6562499999998887557, 0.6718749999998858691, 0.6874999999998828715, 0.7031249999998799849, 0.7109374999998784306, 0.7148437499998785416, 0.7187499999998785416, 0.7499999999998901989, 0.7656249999998960831, 0.7734374999998989697, 0.7773437499999016342, 0.7812499999999042988, 0.7968749999999096278, 0.8124999999999148459, 0.8437499999999256151, 0.8593749999999320544, 0.8749999999999386047, 0.9374999999999692468, 1.000000000000000000 ),
 .UNSPECIFIED. ) ;
#67283 = CARTESIAN_POINT ( 'NONE',  ( 25.49994615388218477, -2.042074746146404607, 11.11389836488523741 ) ) ;
#67284 = CARTESIAN_POINT ( 'NONE',  ( 10.88763167770999907, -5.057180698083000969, 5.046290572389999340 ) ) ;
#67285 = FACE_OUTER_BOUND ( 'NONE', #37646, .T. ) ;
#67286 = CARTESIAN_POINT ( 'NONE',  ( 23.58333993777100090, 3.286260152889999888E-13, -3.641531520771000148E-13 ) ) ;
#67287 = CONICAL_SURFACE ( 'NONE', #3655, 10.65000803020999953, 0.7853981633972997312 ) ;
#67288 = CARTESIAN_POINT ( 'NONE',  ( 11.05336220499919797, 3.034597079077000270, 7.174999999999999822 ) ) ;
#67289 = CARTESIAN_POINT ( 'NONE',  ( 9.216851002545999094, 2.832432432432000269, 6.822293592207000934 ) ) ;
#67290 = CARTESIAN_POINT ( 'NONE',  ( 3.448794404255000057, -3.398741721523000248, 0.4282444512000999626 ) ) ;
#67291 = ORIENTED_EDGE ( 'NONE', *, *, #60750, .T. ) ;
#67292 = ADVANCED_FACE ( 'NONE', ( #23326 ), #28579, .T. ) ;
#67293 = EDGE_CURVE ( 'NONE', #23956, #33463, #42086, .T. ) ;
#67294 = CARTESIAN_POINT ( 'NONE',  ( 12.39285676950935766, -0.4699213205053973663, -12.68829855189362732 ) ) ;
#67295 = CARTESIAN_POINT ( 'NONE',  ( 12.19705744667298575, -2.644897761314413565, -12.41662195506803634 ) ) ;
#67296 = CYLINDRICAL_SURFACE ( 'NONE', #64367, 0.5000000000000028866 ) ;
#67297 = CARTESIAN_POINT ( 'NONE',  ( 24.46580263708699832, 3.340075003801000086, -12.12245366788000034 ) ) ;
#67298 = DIRECTION ( 'NONE',  ( 0.000000000000000000, -0.7614089499631907509, 0.6482718649732928107 ) ) ;
#67299 = ORIENTED_EDGE ( 'NONE', *, *, #14802, .F. ) ;
#67300 = CARTESIAN_POINT ( 'NONE',  ( 6.630791561646000254, 1.270915225504000157, -0.3650349355777000038 ) ) ;
#67301 = EDGE_CURVE ( 'NONE', #54836, #58875, #22971, .T. ) ;
#67302 = APPLICATION_PROTOCOL_DEFINITION ( 'draft international standard', 'automotive_design', 1998, #47174 ) ;
#67303 = CARTESIAN_POINT ( 'NONE',  ( 17.91802421031557913, 0.5088992769509088632, 12.68627498207978377 ) ) ;
#67304 = CARTESIAN_POINT ( 'NONE',  ( 13.16012107570600342, -11.71981102724999957, -1.988987020038000209 ) ) ;
#67305 = CARTESIAN_POINT ( 'NONE',  ( 1.730140132539749853, -3.408904368339107815, 0.9161175952574674985 ) ) ;
#67306 = CARTESIAN_POINT ( 'NONE',  ( 11.27234208742519783, 3.445253572379500362, -8.372004648554700168 ) ) ;
#67307 = VERTEX_POINT ( 'NONE', #60384 ) ;
#67308 = CARTESIAN_POINT ( 'NONE',  ( 9.980430903642000473, -4.047223565251000466, 9.090364706348999846 ) ) ;
#67309 = ORIENTED_EDGE ( 'NONE', *, *, #27491, .T. ) ;
#67310 = CARTESIAN_POINT ( 'NONE',  ( 8.498279931254906217, -3.130208739192112954, 6.060545171114974927 ) ) ;
#67311 = CARTESIAN_POINT ( 'NONE',  ( 9.138566940380000503, -2.933824946949000090, 8.496487880080000110 ) ) ;
#67312 = CARTESIAN_POINT ( 'NONE',  ( 18.02418602114746093, -0.5568603909045894973, -13.98892293345219962 ) ) ;
#67313 = ORIENTED_EDGE ( 'NONE', *, *, #15618, .F. ) ;
#67314 = CARTESIAN_POINT ( 'NONE',  ( 23.56665676678700194, 0.000000000000000000, -3.819167204710999951E-13 ) ) ;
#67315 = CARTESIAN_POINT ( 'NONE',  ( 7.688669563556804754, 2.651071518674656513, 7.261053863064154790 ) ) ;
#67316 = CARTESIAN_POINT ( 'NONE',  ( 7.830279719588000731, 3.552539078410000162, -8.999639305067001160 ) ) ;
#67317 = LINE ( 'NONE', #34507, #20815 ) ;
#67318 = DIRECTION ( 'NONE',  ( 0.000000000000000000, 0.000000000000000000, 1.000000000000000000 ) ) ;
#67319 = ORIENTED_EDGE ( 'NONE', *, *, #1092, .T. ) ;
#67320 = CARTESIAN_POINT ( 'NONE',  ( 11.02286109245999945, -2.398753588646000079, 6.352476128646999065 ) ) ;
#67321 = CARTESIAN_POINT ( 'NONE',  ( 12.18817138783093768, -2.600938394370665208, -13.65148521156285533 ) ) ;
#67322 = CARTESIAN_POINT ( 'NONE',  ( 10.43559687351661758, 2.907767014557176566, -8.129523725463622341 ) ) ;
#67323 = CARTESIAN_POINT ( 'NONE',  ( 10.61721988130000049, -5.045606037229999785, -6.386907901056999570 ) ) ;
#67324 = CIRCLE ( 'NONE', #66181, 0.6999999999999992895 ) ;
#67325 = DIRECTION ( 'NONE',  ( 0.000000000000000000, -1.000000000000000000, 0.000000000000000000 ) ) ;
#67326 = VERTEX_POINT ( 'NONE', #33824 ) ;
#67327 = PRODUCT_DEFINITION_SHAPE ( 'NONE', 'NONE',  #49624 ) ;
#67328 = CARTESIAN_POINT ( 'NONE',  ( 24.12728270886359994, 12.50344094810666284, -3.372677501753305052 ) ) ;
#67329 = CARTESIAN_POINT ( 'NONE',  ( 21.72233714749290101, 0.000000000000000000, 0.000000000000000000 ) ) ;
#67330 = CARTESIAN_POINT ( 'NONE',  ( 10.08422653160753413, -2.899999999999999911, 6.304440313740826696 ) ) ;
#67331 = CARTESIAN_POINT ( 'NONE',  ( 3.105140132544083276, 0.9161175952574701631, 3.408904368339106927 ) ) ;
#67332 = CARTESIAN_POINT ( 'NONE',  ( 12.44045292577858142, -0.5080432161604421237, -13.88750743611951144 ) ) ;
#67333 = CARTESIAN_POINT ( 'NONE',  ( 18.17231130205940204, -2.401422691383821917, 12.47401593597049718 ) ) ;
#67334 = VERTEX_POINT ( 'NONE', #65617 ) ;
#67335 = CARTESIAN_POINT ( 'NONE',  ( 11.67403632436368888, -4.976178716761900489, -7.272033745815799755 ) ) ;
#67336 = EDGE_LOOP ( 'NONE', ( #59665, #1776 ) ) ;
#67337 = CARTESIAN_POINT ( 'NONE',  ( 9.701978494675000064, 3.399139198672999740, 6.026757051093999173 ) ) ;
#67338 = CARTESIAN_POINT ( 'NONE',  ( 11.83810207955129989, -3.203462856645999945, 7.174999999999999822 ) ) ;
#67339 = CARTESIAN_POINT ( 'NONE',  ( 9.874770280412001000, 4.038835765825999680, -5.935509327774999733 ) ) ;
#67340 = CARTESIAN_POINT ( 'NONE',  ( 3.515922480947999862, 1.817153928780999905, 3.042350142939999724 ) ) ;
#67341 = CARTESIAN_POINT ( 'NONE',  ( 9.947300131853999972, -4.892806669161000599, -9.067746434455999704 ) ) ;
#67342 = EDGE_CURVE ( 'NONE', #37649, #48127, #12841, .T. ) ;
#67343 = CARTESIAN_POINT ( 'NONE',  ( 15.39999999998900293, 9.471998555523999386, 8.194929586088999685 ) ) ;
#67344 = CIRCLE ( 'NONE', #53965, 0.6999999999999992895 ) ;
#67345 = CARTESIAN_POINT ( 'NONE',  ( 23.61807751515700105, 13.16786766521000196, 4.269890910948000773 ) ) ;
#67346 = ORIENTED_EDGE ( 'NONE', *, *, #9564, .T. ) ;
#67347 = EDGE_CURVE ( 'NONE', #34817, #25079, #27851, .T. ) ;
#67348 = CARTESIAN_POINT ( 'NONE',  ( 11.76072066707849828, -3.023932655881500065, 8.090408888831799317 ) ) ;
#67349 = CARTESIAN_POINT ( 'NONE',  ( 9.034110134264999203, 4.695345051283999815, 8.660667941667000491 ) ) ;
#67350 = CARTESIAN_POINT ( 'NONE',  ( 15.98069952315600162, 9.346107076637000688, 8.395568570714997847 ) ) ;
#67351 = CARTESIAN_POINT ( 'NONE',  ( 11.09999999999999964, 2.899999999999999911, 4.467422426380999845 ) ) ;
#67353 = CARTESIAN_POINT ( 'NONE',  ( 12.80505043854143388, 1.787816316115912185, -13.88537766212463254 ) ) ;
#67352 = CARTESIAN_POINT ( 'NONE',  ( 9.124700695083998170, 4.778663323155000420, 8.799742559280000265 ) ) ;
#67354 = CARTESIAN_POINT ( 'NONE',  ( 11.55610404293055993, 3.497163090439000310, -8.523936114709998790 ) ) ;
#67355 = CARTESIAN_POINT ( 'NONE',  ( 25.50764038565079161, -2.874079281045797796, -11.25426173516229511 ) ) ;
#67356 = CARTESIAN_POINT ( 'NONE',  ( 9.604355082327998616, 3.550486524676900402, -6.601790705997299114 ) ) ;
#67357 = CARTESIAN_POINT ( 'NONE',  ( 18.26845433917839756, 0.1286734328892390478, 12.59934825840596595 ) ) ;
#67358 = CARTESIAN_POINT ( 'NONE',  ( 24.35146665670700017, 3.377061749054000028, 12.26054704401999906 ) ) ;
#67359 = CARTESIAN_POINT ( 'NONE',  ( 10.76346886766499900, 3.365322927604099679, 8.653146038559000885 ) ) ;
#67360 = CARTESIAN_POINT ( 'NONE',  ( 0.4511054431563896183, 3.350439766384084361, -0.9395068199138416620 ) ) ;
#67361 = ORIENTED_EDGE ( 'NONE', *, *, #17313, .T. ) ;
#67362 = CARTESIAN_POINT ( 'NONE',  ( 7.769581853207999877, -2.431397064767999439, 7.958394431095000776 ) ) ;
#67363 = AXIS2_PLACEMENT_3D ( 'NONE', #35533, #42151, #9280 ) ;
#67364 = CARTESIAN_POINT ( 'NONE',  ( 4.000000000000000888, 1.719428477288966750, -1.321180510578594758 ) ) ;
#67365 = CARTESIAN_POINT ( 'NONE',  ( 5.700000000000000178, 12.03770622561999915, 3.722046322334000124 ) ) ;
#67366 = CARTESIAN_POINT ( 'NONE',  ( 10.22272469555899832, -3.360453478306600239, -6.393520617113999549 ) ) ;
#67367 = ORIENTED_EDGE ( 'NONE', *, *, #65918, .T. ) ;
#67368 = VECTOR ( 'NONE', #54558, 1000.000000000000114 ) ;
#67369 = CARTESIAN_POINT ( 'NONE',  ( 8.668204719592999652, 3.979464555644999901, 9.134076336209998814 ) ) ;
#67371 = CARTESIAN_POINT ( 'NONE',  ( 11.48011496860029901, 4.919769165942200040, 7.971338736265699332 ) ) ;
#67370 = CARTESIAN_POINT ( 'NONE',  ( 10.06726717315599906, -4.659895246859299789, -6.937642277832399174 ) ) ;
#67372 = CARTESIAN_POINT ( 'NONE',  ( 10.35752971959000135, 5.367812128871999988, -6.514736131541999598 ) ) ;
#67373 = ORIENTED_EDGE ( 'NONE', *, *, #65073, .F. ) ;
#67374 = EDGE_CURVE ( 'NONE', #44202, #53037, #18688, .T. ) ;
#67375 = FACE_OUTER_BOUND ( 'NONE', #58129, .T. ) ;
#67376 = CARTESIAN_POINT ( 'NONE',  ( 18.15197774836041589, -2.932501865601731428, -13.68943155935733991 ) ) ;
#67377 = CARTESIAN_POINT ( 'NONE',  ( 11.45764291764649911, 2.867875922590999771, 7.639947095788999221 ) ) ;
#67378 = CARTESIAN_POINT ( 'NONE',  ( 7.949305362820807019, -5.068892134240547520, 6.584878031929767950 ) ) ;
#67379 = CARTESIAN_POINT ( 'NONE',  ( 11.09999999999999964, -5.299524241844999928, -5.124965750789000296 ) ) ;
#67380 = ORIENTED_EDGE ( 'NONE', *, *, #618, .F. ) ;
#67381 = CARTESIAN_POINT ( 'NONE',  ( 11.82312259374200103, -3.643624473348999970, 12.02372562982000126 ) ) ;
#67382 = ADVANCED_FACE ( 'NONE', ( #65273 ), #6460, .T. ) ;
#67383 = EDGE_CURVE ( 'NONE', #27255, #49898, #37867, .T. ) ;
#67384 = DIRECTION ( 'NONE',  ( 0.000000000000000000, -1.000000000000000000, 0.000000000000000000 ) ) ;
#67385 = CARTESIAN_POINT ( 'NONE',  ( 8.222974175369182959, -5.661925504349325955, 8.013205229805864249 ) ) ;
#67386 = CARTESIAN_POINT ( 'NONE',  ( 11.26212378248529866, -4.615095948180499619, -6.336291382830999908 ) ) ;
#67387 = CARTESIAN_POINT ( 'NONE',  ( 9.826684229510000534, -4.901739481456999670, 8.407331414124799451 ) ) ;
#67388 = ORIENTED_EDGE ( 'NONE', *, *, #8830, .T. ) ;
#67389 = CARTESIAN_POINT ( 'NONE',  ( 11.07586359541999954, -5.334319426963999078, -4.951757428735000133 ) ) ;
#67390 = CARTESIAN_POINT ( 'NONE',  ( 10.89503166480599994, -5.274847857784000560, 7.410114961806599787 ) ) ;
#67391 = VERTEX_POINT ( 'NONE', #56403 ) ;
#67392 = CARTESIAN_POINT ( 'NONE',  ( 16.09997386696500143, -4.522001505202896787, -10.77728718286270215 ) ) ;
#67393 = VECTOR ( 'NONE', #63463, 1000.000000000000000 ) ;
#67394 = EDGE_LOOP ( 'NONE', ( #23741, #16669, #35933, #53797, #64261, #36304, #10817, #54371 ) ) ;
#67395 = CARTESIAN_POINT ( 'NONE',  ( 9.326385834542001874, -4.867164667115999599, -6.095483598963999938 ) ) ;
#67396 = CARTESIAN_POINT ( 'NONE',  ( 8.447510841229000533, 4.933589693325000525, -9.154576215408999573 ) ) ;
#67397 = CARTESIAN_POINT ( 'NONE',  ( 11.30367835872029936, 2.886444435522000251, -6.798177532456199934 ) ) ;
#67398 = CARTESIAN_POINT ( 'NONE',  ( 11.34657802013509986, -5.315911219205999849, 7.530633716161349689 ) ) ;
#67399 = CARTESIAN_POINT ( 'NONE',  ( 12.26151780194100382, 2.191289199348897654, -12.51818198400761517 ) ) ;
#67400 = CARTESIAN_POINT ( 'NONE',  ( 11.58841369783139896, -4.057552111898620417, 6.360711682373000109 ) ) ;
#67401 = CARTESIAN_POINT ( 'NONE',  ( 7.539232780409000689, 4.696238830159999544, 5.830273622963999536 ) ) ;
#67402 = EDGE_CURVE ( 'NONE', #12705, #58173, #47628, .T. ) ;
#67403 = ORIENTED_EDGE ( 'NONE', *, *, #29901, .T. ) ;
#67404 = CARTESIAN_POINT ( 'NONE',  ( 9.277969429786152133, 2.899999999999999911, -6.446868419509604209 ) ) ;
#67405 = CARTESIAN_POINT ( 'NONE',  ( 7.673644353206999114, -4.696237245142999228, 5.830277424166999900 ) ) ;
#67406 = CARTESIAN_POINT ( 'NONE',  ( 25.46373029971899982, -8.354610197568000274, -8.148451206582999262 ) ) ;
#67407 = VERTEX_POINT ( 'NONE', #67562 ) ;
#67408 = CARTESIAN_POINT ( 'NONE',  ( 12.80505043854146940, -3.125000000000000444, -12.28373071562070074 ) ) ;
#67409 = CARTESIAN_POINT ( 'NONE',  ( 11.08425954179440076, 4.982976321082899673, 6.683254058608399717 ) ) ;
#67410 = CARTESIAN_POINT ( 'NONE',  ( 10.52384314678999999, -5.441919393629000012, -7.989634081859001036 ) ) ;
#67411 = DIRECTION ( 'NONE',  ( 1.000000000000000000, 0.000000000000000000, 0.000000000000000000 ) ) ;
#67412 = CARTESIAN_POINT ( 'NONE',  ( 18.06944243593800081, -3.222040310929999762, -11.85748006108999952 ) ) ;
#67413 = DIRECTION ( 'NONE',  ( 0.000000000000000000, 1.000000000000000000, 0.000000000000000000 ) ) ;
#67414 = CARTESIAN_POINT ( 'NONE',  ( 12.30764200008710496, -3.049303773002894680, -13.66388724637008778 ) ) ;
#67415 = CARTESIAN_POINT ( 'NONE',  ( 11.31825954179440075, -3.333768806796900019, -8.053565341712399572 ) ) ;
#67416 = B_SPLINE_CURVE_WITH_KNOTS ( 'NONE', 3,
 ( #5653, #58456, #32584, #37821, #42041, #53895, #53214, #21732, #31553, #26994, #764, #16494, #47974, #27689, #52875, #15473, #5316, #26657, #27336, #22080, #43425, #72, #21393, #64719, #36799, #64031, #68591, #63347, #42727, #16151, #48311 ),
 .UNSPECIFIED., .F., .F.,
 ( 4, 2, 2, 1, 1, 2, 2, 2, 1, 2, 2, 2, 2, 2, 2, 2, 4 ),
 ( 0.000000000000000000, 0.06250000000001226796, 0.09375000000001840195, 0.1093750000000199701, 0.1171875000000205391, 0.1210937500000210665, 0.1250000000000215661, 0.1875000000000251188, 0.2187500000000255629, 0.2343750000000240641, 0.2500000000000225930, 0.3750000000000187628, 0.4375000000000192069, 0.4687500000000189848, 0.5000000000000187628, 0.7500000000000094369, 1.000000000000000000 ),
 .UNSPECIFIED. ) ;
#67417 = CARTESIAN_POINT ( 'NONE',  ( 10.14887885159599890, -2.730985436695000157, -7.348611220446799486 ) ) ;
#67418 = FACE_OUTER_BOUND ( 'NONE', #21399, .T. ) ;
#67419 = EDGE_LOOP ( 'NONE', ( #54275, #10534, #1045, #56012 ) ) ;
#67420 = VERTEX_POINT ( 'NONE', #51493 ) ;
#67421 = CARTESIAN_POINT ( 'NONE',  ( 10.26575685213000000, -4.574972855646000092, 4.689163863504999696 ) ) ;
#67422 = AXIS2_PLACEMENT_3D ( 'NONE', #47871, #310, #16383 ) ;
#67423 = FACE_OUTER_BOUND ( 'NONE', #66179, .T. ) ;
#67424 = CARTESIAN_POINT ( 'NONE',  ( 17.75984001012010438, 3.091833346853859688, 13.52991597407626223 ) ) ;
#67425 = CARTESIAN_POINT ( 'NONE',  ( 10.46009300862000124, 2.565654508827999614, -6.975684004278000394 ) ) ;
#67426 = FACE_BOUND ( 'NONE', #37947, .T. ) ;
#67427 = CARTESIAN_POINT ( 'NONE',  ( 17.55505043854143565, 3.125000000000000000, 12.28373071562070074 ) ) ;
#67428 = CARTESIAN_POINT ( 'NONE',  ( 23.61702328491799818, -13.18027949750999994, 4.241847907418000219 ) ) ;
#67429 = CARTESIAN_POINT ( 'NONE',  ( 10.62197831623999988, 5.779783227492000464, 7.256572995198999898 ) ) ;
#67430 = EDGE_CURVE ( 'NONE', #8552, #29897, #51160, .T. ) ;
#67431 = CARTESIAN_POINT ( 'NONE',  ( 11.91486084871699802, -5.207010770456999893, 7.174999999999999822 ) ) ;
#67432 = ORIENTED_EDGE ( 'NONE', *, *, #12968, .F. ) ;
#67433 = CARTESIAN_POINT ( 'NONE',  ( 12.54459593125683625, -1.931762302728656122, 12.56598641381995307 ) ) ;
#67434 = CARTESIAN_POINT ( 'NONE',  ( 9.146417874593998576, -4.797903641662700558, -7.839201596587598964 ) ) ;
#67435 = CARTESIAN_POINT ( 'NONE',  ( 10.76010575649000067, 4.535386075958999896, 6.001721352166000223 ) ) ;
#67436 = CARTESIAN_POINT ( 'NONE',  ( 12.18788784977535933, -4.985985832792199979, 7.556342205905759890 ) ) ;
#67437 = CARTESIAN_POINT ( 'NONE',  ( 11.59999999999999964, 2.500145227336000087, 7.174999999999999822 ) ) ;
#67438 = B_SPLINE_CURVE_WITH_KNOTS ( 'NONE', 3,
 ( #16380, #59721, #68828, #54479 ),
 .UNSPECIFIED., .F., .F.,
 ( 4, 4 ),
 ( 0.000000000000000000, 1.000000000000000000 ),
 .UNSPECIFIED. ) ;
#67439 = CARTESIAN_POINT ( 'NONE',  ( 10.34580110216399973, 2.909301855364999856, -6.833896451085399448 ) ) ;
#67440 = CARTESIAN_POINT ( 'NONE',  ( 12.37769715316224506, 0.4561785182478241829, 12.68897339690746762 ) ) ;
#67441 = AXIS2_PLACEMENT_3D ( 'NONE', #2578, #28473, #18666 ) ;
#67442 = CARTESIAN_POINT ( 'NONE',  ( 8.032364158772001161, 3.524748802314000340, 5.573833469815000718 ) ) ;
#67443 = CARTESIAN_POINT ( 'NONE',  ( 10.77962664842000073, 2.397507474987000009, 7.755423212350999407 ) ) ;
#67444 = CARTESIAN_POINT ( 'NONE',  ( 12.18947222198076652, 2.391413182808838744, 12.47619792628429636 ) ) ;
#67445 = ORIENTED_EDGE ( 'NONE', *, *, #40750, .T. ) ;
#67446 = VECTOR ( 'NONE', #44880, 1000.000000000000227 ) ;
#67447 = CARTESIAN_POINT ( 'NONE',  ( 8.640504719592000171, 2.305580295895999665, -7.860904109308999743 ) ) ;
#67448 = CARTESIAN_POINT ( 'NONE',  ( 11.09999999999999964, 4.000000000000000000, 7.500000000000000000 ) ) ;
#67449 = DIRECTION ( 'NONE',  ( 1.000000000000000000, 0.000000000000000000, 0.000000000000000000 ) ) ;
#67451 = CARTESIAN_POINT ( 'NONE',  ( 3.365110627350583083, -0.4777639219876382293, -3.497143207087723304 ) ) ;
#67450 = CARTESIAN_POINT ( 'NONE',  ( 8.983793146794999629, -3.979464503892999439, 9.134080454305001595 ) ) ;
#67452 = CARTESIAN_POINT ( 'NONE',  ( 12.09999999999999964, -4.755880058522735432, 8.017883087166149281 ) ) ;
#67453 = CARTESIAN_POINT ( 'NONE',  ( 10.35410941423799791, -3.257202320419700037, -6.825313060354999628 ) ) ;
#67454 = ORIENTED_EDGE ( 'NONE', *, *, #46319, .F. ) ;
#67455 = CARTESIAN_POINT ( 'NONE',  ( 2.201884160320000117, -2.304706330186000240, 2.969293668968000066 ) ) ;
#67456 = CARTESIAN_POINT ( 'NONE',  ( 17.55505043854144276, -0.6250000000000001110, -12.67928921589118474 ) ) ;
#67458 = CARTESIAN_POINT ( 'NONE',  ( 11.44731512799000228, 3.899625435828999898, -11.84583327264999930 ) ) ;
#67457 = CARTESIAN_POINT ( 'NONE',  ( 9.170239158775000732, 4.769103072373000352, -8.666849124598000387 ) ) ;
#67459 = CARTESIAN_POINT ( 'NONE',  ( 10.83253786428999987, 2.899999999999999911, 6.571291218949999902 ) ) ;
#67460 = CARTESIAN_POINT ( 'NONE',  ( 14.39999999806400055, -11.53037610505381494, 4.891426364203002919 ) ) ;
#67461 = CARTESIAN_POINT ( 'NONE',  ( 12.53658830138318159, -3.196304600777688076, 13.63024796167574948 ) ) ;
#67462 = CARTESIAN_POINT ( 'NONE',  ( 24.30000000000000071, -3.224868684338999980, -12.03537377768999939 ) ) ;
#67463 = CARTESIAN_POINT ( 'NONE',  ( 11.09806944063053891, -2.697063473153181068, 6.634103937395076755 ) ) ;
#67464 = CARTESIAN_POINT ( 'NONE',  ( 8.335879440378999305, -4.310353212080000773, 9.459493062793997709 ) ) ;
#67465 = ORIENTED_EDGE ( 'NONE', *, *, #33931, .F. ) ;
#67466 = CARTESIAN_POINT ( 'NONE',  ( 9.368920280410000245, 5.618384167307999277, 7.727742442702000503 ) ) ;
#67467 = ADVANCED_FACE ( 'NONE', ( #57419 ), #28619, .F. ) ;
#67469 = ADVANCED_FACE ( 'NONE', ( #30186 ), #3588, .F. ) ;
#67468 = B_SPLINE_CURVE_WITH_KNOTS ( 'NONE', 3,
 ( #59031, #53097, #15004, #62883 ),
 .UNSPECIFIED., .F., .F.,
 ( 4, 4 ),
 ( 0.000000000000000000, 1.000000000000000000 ),
 .UNSPECIFIED. ) ;
#67470 = B_SPLINE_CURVE_WITH_KNOTS ( 'NONE', 3,
 ( #6543, #54789, #38362, #59687 ),
 .UNSPECIFIED., .F., .F.,
 ( 4, 4 ),
 ( 0.000000000000000000, 1.000000000000000000 ),
 .UNSPECIFIED. ) ;
#67472 = DIRECTION ( 'NONE',  ( 4.468469752125040125E-09, 0.9867386997955089889, 0.1623167838699015042 ) ) ;
#67471 = CARTESIAN_POINT ( 'NONE',  ( 4.982454287316000929, -0.1571859003484000206, 1.535560374452000110 ) ) ;
#67473 = CARTESIAN_POINT ( 'NONE',  ( 7.643806538548957974, -5.335784186437363630, 6.386268904257039303 ) ) ;
#67474 = AXIS2_PLACEMENT_3D ( 'NONE', #34110, #23265, #39007 ) ;
#67475 = CARTESIAN_POINT ( 'NONE',  ( 7.702547272646715015, -2.712723599019214671, 7.026494385502345175 ) ) ;
#67476 = CARTESIAN_POINT ( 'NONE',  ( 0.9803365601255999984, -3.300563260077000294, -0.9171157435373999967 ) ) ;
#67477 = EDGE_LOOP ( 'NONE', ( #50194, #9338, #3679, #1407 ) ) ;
#67478 = CARTESIAN_POINT ( 'NONE',  ( 1.047957204161283018, -3.182233228816532922, -0.8842357997067202824 ) ) ;
#67479 = CARTESIAN_POINT ( 'NONE',  ( 12.01102763632551884, -4.911148285670300595, 7.920427941950599404 ) ) ;
#67480 = DIRECTION ( 'NONE',  ( 0.000000000000000000, 0.000000000000000000, 1.000000000000000000 ) ) ;
#67481 = CARTESIAN_POINT ( 'NONE',  ( 9.945533384955998812, 2.906048475816000121, 8.880389653997999844 ) ) ;
#67482 = CARTESIAN_POINT ( 'NONE',  ( 11.53564291764652872, 3.004110626587600308, 7.623106493640399606 ) ) ;
#67483 = PRODUCT_DEFINITION_SHAPE ( 'NONE', 'NONE',  #69201 ) ;
#67484 = CARTESIAN_POINT ( 'NONE',  ( 23.89491049328219319, -3.335473474314862852, 12.94526851323479910 ) ) ;
#67485 = CARTESIAN_POINT ( 'NONE',  ( 12.80505043854144276, 0.6600719421079733751, -13.91436771118225302 ) ) ;
#67486 = CARTESIAN_POINT ( 'NONE',  ( 12.13611496860034933, -2.828587461987000395, 8.100294210499798808 ) ) ;
#67487 = ADVANCED_FACE ( 'NONE', ( #11581 ), #38693, .F. ) ;
#67488 = CARTESIAN_POINT ( 'NONE',  ( 8.173029125821519969, 5.656335574181040826, 6.888602418924802961 ) ) ;
#67489 = AXIS2_PLACEMENT_3D ( 'NONE', #32257, #37147, #5661 ) ;
#67490 = ORIENTED_EDGE ( 'NONE', *, *, #64563, .F. ) ;
#67491 = B_SPLINE_CURVE_WITH_KNOTS ( 'NONE', 3,
 ( #6362, #58480, #15828, #26328, #43089, #48680, #1131, #10582, #32272, #26680 ),
 .UNSPECIFIED., .F., .F.,
 ( 4, 2, 2, 2, 4 ),
 ( 0.1254224513349476711, 0.3127176035874427718, 0.5000127558399378724, 0.6873079080924326956, 0.8746030603449276297 ),
 .UNSPECIFIED. ) ;
#67492 = CARTESIAN_POINT ( 'NONE',  ( 17.90989566141533018, -3.154773125069390449, 13.63992084652273817 ) ) ;
#67493 = CARTESIAN_POINT ( 'NONE',  ( 7.100000000000000533, -12.50865771883999855, -2.924687089723999822 ) ) ;
#67494 = ORIENTED_EDGE ( 'NONE', *, *, #37396, .F. ) ;
#67495 = FACE_OUTER_BOUND ( 'NONE', #61880, .T. ) ;
#67496 = EDGE_CURVE ( 'NONE', #21757, #16879, #51254, .T. ) ;
#67497 = CARTESIAN_POINT ( 'NONE',  ( 25.21376650222272531, -2.724979797188207264, -11.40630329634163331 ) ) ;
#67498 = DIRECTION ( 'NONE',  ( 0.000000000000000000, 0.9586353287342648244, -0.2846371488448895537 ) ) ;
#67499 = CARTESIAN_POINT ( 'NONE',  ( 11.04749144726329924, 3.499163784537000055, 8.206726025856399431 ) ) ;
#67500 = CARTESIAN_POINT ( 'NONE',  ( 11.15982925107999968, 5.578232410510000072, 8.067793621926998782 ) ) ;
#67501 = B_SPLINE_CURVE_WITH_KNOTS ( 'NONE', 3,
 ( #39026, #40064, #34479, #23285 ),
 .UNSPECIFIED., .F., .F.,
 ( 4, 4 ),
 ( 0.000000000000000000, 1.000000000000000000 ),
 .UNSPECIFIED. ) ;
#67502 = CARTESIAN_POINT ( 'NONE',  ( 10.93146722582000052, 2.472885155055999817, -7.514158739122999364 ) ) ;
#67503 = CARTESIAN_POINT ( 'NONE',  ( 10.06276198887462847, -4.665935521472182934, -6.932494801640175730 ) ) ;
#67504 = CARTESIAN_POINT ( 'NONE',  ( 10.62792628238999981, -3.100579357212000176, 8.599905962393000536 ) ) ;
#67505 = CARTESIAN_POINT ( 'NONE',  ( 18.22927867710215111, 0.2646961475753863979, -12.59722401988189588 ) ) ;
#67506 = CARTESIAN_POINT ( 'NONE',  ( 10.44486180556999955, -4.964082081645000422, -9.083599939499999110 ) ) ;
#67507 = CARTESIAN_POINT ( 'NONE',  ( 10.97364560330029981, -3.734560974198899874, -6.675475461903199736 ) ) ;
#67508 = CARTESIAN_POINT ( 'NONE',  ( 8.047385841228999581, 4.468366666325000125, 8.882140983065999862 ) ) ;
#67509 = ORIENTED_EDGE ( 'NONE', *, *, #49731, .T. ) ;
#67510 = AXIS2_PLACEMENT_3D ( 'NONE', #17462, #21656, #48932 ) ;
#67511 = CARTESIAN_POINT ( 'NONE',  ( 18.50001572531400029, 1.956586052127241571, -12.40985500457068547 ) ) ;
#67512 = CARTESIAN_POINT ( 'NONE',  ( 10.65729680854845540, 3.174840887412555546, -4.784047223682147632 ) ) ;
#67513 = CARTESIAN_POINT ( 'NONE',  ( 17.72120476622713880, 1.779652109340961408, 12.47368672373264076 ) ) ;
#67514 = CARTESIAN_POINT ( 'NONE',  ( 9.076468108405999047, 5.230803879475000251, -7.848577323721800170 ) ) ;
#67515 = CARTESIAN_POINT ( 'NONE',  ( 12.08136008892999591, 2.567386246332872712, 13.76259835127842024 ) ) ;
#67516 = CARTESIAN_POINT ( 'NONE',  ( 11.05935368890999904, -2.480241580537000168, 6.610077204591000566 ) ) ;
#67517 = EDGE_LOOP ( 'NONE', ( #15921, #40422, #42568, #64393 ) ) ;
#67518 = CARTESIAN_POINT ( 'NONE',  ( 12.31443506008844579, 0.3873604450494987361, -12.69205253629085028 ) ) ;
#67519 = CARTESIAN_POINT ( 'NONE',  ( 25.37957628771734875, 8.342521315683184113, 8.311489950699764151 ) ) ;
#67520 = ORIENTED_EDGE ( 'NONE', *, *, #34589, .F. ) ;
#67521 = DIRECTION ( 'NONE',  ( 2.887756364189944304E-10, 0.4812251768484908099, 0.8765970164032835799 ) ) ;
#67522 = LINE ( 'NONE', #67867, #51869 ) ;
#67523 = CYLINDRICAL_SURFACE ( 'NONE', #9523, 0.5000000000000000000 ) ;
#67524 = CARTESIAN_POINT ( 'NONE',  ( 10.98133997688000107, -3.815400206859000054, 8.346298710230199092 ) ) ;
#67525 = B_SPLINE_SURFACE_WITH_KNOTS ( 'NONE', 3, 3, ( 
 ( #105, #52558, #5006, #36833 ),
 ( #47668, #20749, #4654, #43104 ),
 ( #21769, #48345, #9910, #25994 ),
 ( #31936, #47325, #52213, #15839 ),
 ( #25649, #58150, #32287, #10253 ),
 ( #68980, #21422, #31249, #53594 ),
 ( #46978, #37171, #57450, #42759 ),
 ( #36478, #58490, #42073, #68282 ),
 ( #68628, #64066, #20402, #52909 ),
 ( #41726, #31588, #26342, #10594 ),
 ( #5690, #5352, #64406, #16184 ),
 ( #451, #37510, #15507, #27032 ),
 ( #15158, #57802, #9560, #16530 ),
 ( #21094, #42420, #28067, #28417 ),
 ( #39243, #33660, #44157, #43461 ),
 ( #11622, #6034, #28769, #65455 ) ),
 .UNSPECIFIED., .F., .F., .F.,
 ( 4, 1, 1, 1, 1, 1, 1, 1, 1, 1, 1, 1, 1, 4 ),
 ( 4, 4 ),
 ( 0.02931725585745999924, 0.07692307692307999434, 0.1538461538461999845, 0.2307692307692000011, 0.3076923076922999933, 0.3846153846154000133, 0.4615384615385000333, 0.5384615384614999112, 0.6153846153845999867, 0.6923076923076999512, 0.7692307692308000266, 0.8461538461537999600, 0.9230769230769000355, 0.9830414450855999853 ),
 ( -0.1835260008787999997, 1.183623993927000129 ),
 .UNSPECIFIED. ) ;
#67526 = CARTESIAN_POINT ( 'NONE',  ( 8.688131671361706054, 4.829518895119560895, -8.579743915872116489 ) ) ;
#67527 = AXIS2_PLACEMENT_3D ( 'NONE', #31412, #16010, #26508 ) ;
#67528 = CARTESIAN_POINT ( 'NONE',  ( 0.1455175461370999956, 3.330914467393999878, 1.191613524625000142 ) ) ;
#67529 = CARTESIAN_POINT ( 'NONE',  ( 11.28830977893787768, 3.023401864784706738, 8.326430086672806041 ) ) ;
#67530 = CARTESIAN_POINT ( 'NONE',  ( 12.63902032760542937, 3.180686373181415671, 12.19193352998605739 ) ) ;
#67531 = CARTESIAN_POINT ( 'NONE',  ( 17.55505043854144276, 0.6250000000000001110, 13.88107975066923316 ) ) ;
#67532 = CARTESIAN_POINT ( 'NONE',  ( 11.70794988689359961, 4.455786710255300598, -8.393984925606600811 ) ) ;
#67533 = CARTESIAN_POINT ( 'NONE',  ( 5.200000002520999587, 0.6646153838164000627, -2.616923079727000001 ) ) ;
#67534 = CARTESIAN_POINT ( 'NONE',  ( 10.49411415877000131, 2.866942652264999669, -8.960728730887002058 ) ) ;
#67535 = CARTESIAN_POINT ( 'NONE',  ( 9.961925467520998723, 2.860918852493000486, -7.421078600323300023 ) ) ;
#67537 = CARTESIAN_POINT ( 'NONE',  ( 12.19317846012505591, 2.372225799402258417, 12.48041235930111981 ) ) ;
#67536 = CARTESIAN_POINT ( 'NONE',  ( 15.86242637978999959, -8.523064092628001021, -8.288181269780999116 ) ) ;
#67538 = CARTESIAN_POINT ( 'NONE',  ( 23.63687345803960227, -13.40365592222601521, 3.866661307165411454 ) ) ;
#67539 = VERTEX_POINT ( 'NONE', #64030 ) ;
#67540 = CARTESIAN_POINT ( 'NONE',  ( 11.02812378248509795, 3.583106837161099900, 8.288725998710999576 ) ) ;
#67541 = AXIS2_PLACEMENT_3D ( 'NONE', #11227, #6317, #12274 ) ;
#67542 = CARTESIAN_POINT ( 'NONE',  ( 10.62698276521000196, -3.142914536759000121, 8.668455626664998803 ) ) ;
#67543 = CARTESIAN_POINT ( 'NONE',  ( 9.023797255587998833, 5.140789995332999851, 7.548297453605989027 ) ) ;
#67544 = CARTESIAN_POINT ( 'NONE',  ( 7.000000000000000000, -9.735955015381000166, -5.735955015381000166 ) ) ;
#67545 = LINE ( 'NONE', #30503, #9791 ) ;
#67546 = DIRECTION ( 'NONE',  ( 0.000000000000000000, 1.000000000000000000, 0.000000000000000000 ) ) ;
#67547 = DIRECTION ( 'NONE',  ( 0.000000000000000000, 1.000000000000000000, 0.000000000000000000 ) ) ;
#67548 = ORIENTED_EDGE ( 'NONE', *, *, #6858, .T. ) ;
#67549 = EDGE_CURVE ( 'NONE', #39743, #37501, #15338, .T. ) ;
#67550 = EDGE_CURVE ( 'NONE', #20205, #8257, #48659, .T. ) ;
#67551 = CARTESIAN_POINT ( 'NONE',  ( 9.050076168957998490, -4.579425901182000658, -8.483869947211399420 ) ) ;
#67552 = CARTESIAN_POINT ( 'NONE',  ( 10.64264450635444703, -5.032314077581211187, -5.044903346590539073 ) ) ;
#67553 = CARTESIAN_POINT ( 'NONE',  ( 11.14391429142989942, -3.977620450637519678, 8.674673860548999471 ) ) ;
#67554 = CARTESIAN_POINT ( 'NONE',  ( 17.79082714041176772, 1.799831594964171888, -12.47079078729191259 ) ) ;
#67555 = CARTESIAN_POINT ( 'NONE',  ( 7.000000000000000000, 10.80467225524999897, 3.475853594956999970 ) ) ;
#67556 = CARTESIAN_POINT ( 'NONE',  ( 5.500000000000000000, 0.000000000000000000, 0.000000000000000000 ) ) ;
#67557 = CARTESIAN_POINT ( 'NONE',  ( 12.18127175123626493, 2.459544125670197090, -13.68195797701648253 ) ) ;
#67558 = CARTESIAN_POINT ( 'NONE',  ( 9.399896294736999280, -5.679455740088000582, -8.329752476417999318 ) ) ;
#67559 = CARTESIAN_POINT ( 'NONE',  ( 25.37703561905400207, 11.10734551254999936, 3.396345752903999760 ) ) ;
#67560 = CARTESIAN_POINT ( 'NONE',  ( 9.496378438922418397, -5.350075508921414702, 7.852928877054440093 ) ) ;
#67561 = AXIS2_PLACEMENT_3D ( 'NONE', #59263, #33048, #53685 ) ;
#67562 = CARTESIAN_POINT ( 'NONE',  ( 2.435247277619000172, 2.372532593102000043, -2.573147701680999599 ) ) ;
#67563 = DIRECTION ( 'NONE',  ( 1.000000000000000000, 0.000000000000000000, 0.000000000000000000 ) ) ;
#67564 = CARTESIAN_POINT ( 'NONE',  ( 44.24148000000000280, -9.517611874540000017, 8.103398312166998352 ) ) ;
#67565 = LINE ( 'NONE', #35094, #8059 ) ;
#67566 = CARTESIAN_POINT ( 'NONE',  ( 17.91921746558519146, -11.21561494459223773, 3.152940210883220296 ) ) ;
#67567 = FACE_OUTER_BOUND ( 'NONE', #35924, .T. ) ;
#67568 = ORIENTED_EDGE ( 'NONE', *, *, #3605, .F. ) ;
#67569 = CARTESIAN_POINT ( 'NONE',  ( 8.653803059789179741, -2.648172424375523804, 7.852957271307993814 ) ) ;
#67570 = CARTESIAN_POINT ( 'NONE',  ( 18.27395862148967609, 2.614931059283417181, -13.75364391642199280 ) ) ;
#67571 = VERTEX_POINT ( 'NONE', #32925 ) ;
#67572 = EDGE_CURVE ( 'NONE', #67420, #15904, #21058, .T. ) ;
#67573 = CARTESIAN_POINT ( 'NONE',  ( 10.18732996542200020, -4.602191201513400109, 6.876242273533999416 ) ) ;
#67574 = CARTESIAN_POINT ( 'NONE',  ( 25.09888356831554290, 2.850926811815151840, 11.48730284164415494 ) ) ;
#67575 = CARTESIAN_POINT ( 'NONE',  ( 8.397785841227999981, 5.616457598545999907, -8.245813000738998255 ) ) ;
#67576 = CARTESIAN_POINT ( 'NONE',  ( 2.262975856965000254, 2.754481206214999922, -1.355138954038999977 ) ) ;
#67577 = CARTESIAN_POINT ( 'NONE',  ( 10.10733666362725991, 2.230327070931253264, -7.110663345345299646 ) ) ;
#67578 = CARTESIAN_POINT ( 'NONE',  ( 10.93479632507519916, -3.442212747724900268, -8.534037301706000278 ) ) ;
#67579 = CARTESIAN_POINT ( 'NONE',  ( 23.85395508732198167, 9.637287106755159982, -9.713125223865638702 ) ) ;
#67580 = CARTESIAN_POINT ( 'NONE',  ( 11.29997394663803867, -12.21464834820976897, -1.635338273580426494 ) ) ;
#67581 = ORIENTED_EDGE ( 'NONE', *, *, #16948, .F. ) ;
#67582 = DIRECTION ( 'NONE',  ( -0.000000000000000000, 0.9454292341245821296, 0.3258275053806940491 ) ) ;
#67583 = CARTESIAN_POINT ( 'NONE',  ( 10.59393020684899867, -2.750000000000000000, 7.500000000000000000 ) ) ;
#67584 = CARTESIAN_POINT ( 'NONE',  ( 8.889129719593999113, 5.687930027805999877, -7.109876198051000351 ) ) ;
#67585 = VERTEX_POINT ( 'NONE', #59484 ) ;
#67586 = CARTESIAN_POINT ( 'NONE',  ( 11.19121071698999970, 3.005389011699000079, -6.023544385387999966 ) ) ;
#67587 =( LENGTH_UNIT ( ) NAMED_UNIT ( * ) SI_UNIT ( .MILLI., .METRE. ) );
#67588 = ORIENTED_EDGE ( 'NONE', *, *, #870, .F. ) ;
#67589 = CARTESIAN_POINT ( 'NONE',  ( 10.10344474310099905, 5.137935629024000583, 6.947770206896899836 ) ) ;
#67590 = CARTESIAN_POINT ( 'NONE',  ( 17.79060029153385969, -3.161091907734806750, -12.19703033907565981 ) ) ;
#67591 = CARTESIAN_POINT ( 'NONE',  ( 11.35619132127000164, -11.69822877698999974, -1.509327410273999970 ) ) ;
#67592 = CARTESIAN_POINT ( 'NONE',  ( 24.53002386606100060, -12.09082868768999930, -3.147845687315999896 ) ) ;
#67593 = CARTESIAN_POINT ( 'NONE',  ( 13.50003721581400029, -9.159934378815998812, -7.517910889891000537 ) ) ;
#67594 = ORIENTED_EDGE ( 'NONE', *, *, #50189, .T. ) ;
#67595 = CARTESIAN_POINT ( 'NONE',  ( 10.09393020684899867, 5.250000000000000000, 7.500000000000000000 ) ) ;
#67596 = CARTESIAN_POINT ( 'NONE',  ( 10.19794834123000093, 4.262170647947000290, -8.834315641189999013 ) ) ;
#67597 = DIRECTION ( 'NONE',  ( 0.000000000000000000, 1.000000000000000000, 0.000000000000000000 ) ) ;
#67598 = CARTESIAN_POINT ( 'NONE',  ( 12.09915596617137723, 2.684647274610783452, -13.74018952919733394 ) ) ;
#67599 = CARTESIAN_POINT ( 'NONE',  ( 17.96742444759810908, 0.6007076874295131930, 13.98710814480368292 ) ) ;
#67600 = CARTESIAN_POINT ( 'NONE',  ( 18.38722619340700248, 3.117741388420999904, 11.18549237633000004 ) ) ;
#67601 = CARTESIAN_POINT ( 'NONE',  ( 7.851231298947399573, 5.072114957085871012, 6.622200184418144175 ) ) ;
#67602 = B_SPLINE_CURVE_WITH_KNOTS ( 'NONE', 3,
 ( #22942, #59664, #65593, #56054 ),
 .UNSPECIFIED., .F., .F.,
 ( 4, 4 ),
 ( 0.000000000000000000, 1.000000000000000000 ),
 .UNSPECIFIED. ) ;
#67603 = EDGE_CURVE ( 'NONE', #29053, #12282, #4558, .T. ) ;
#67604 = VERTEX_POINT ( 'NONE', #10560 ) ;
#67605 = ORIENTED_EDGE ( 'NONE', *, *, #61872, .F. ) ;
#67606 = CARTESIAN_POINT ( 'NONE',  ( 9.377520280414000098, 4.092867382745001059, -5.937785237406000505 ) ) ;
#67607 = CARTESIAN_POINT ( 'NONE',  ( 9.293683662962452630, 4.685540010276588063, 9.106439227925379853 ) ) ;
#67608 = CARTESIAN_POINT ( 'NONE',  ( 7.371537754583582291, -4.354055095920205787, 6.184131058409644943 ) ) ;
#67609 = CARTESIAN_POINT ( 'NONE',  ( 24.00507476546492569, 3.345682322440594714, 12.73790407563989469 ) ) ;
#67610 = CARTESIAN_POINT ( 'NONE',  ( 7.800894426331000275, 3.218815461055000160, 6.398977422524000147 ) ) ;
#67611 = CARTESIAN_POINT ( 'NONE',  ( 18.35296092448800209, -2.690559717027000364, -11.48481263514000084 ) ) ;
#67613 = CARTESIAN_POINT ( 'NONE',  ( 5.500000000000000000, 12.22293997673000021, -3.800173559029999648 ) ) ;
#67612 = CARTESIAN_POINT ( 'NONE',  ( 9.551138961223999857, -2.940105638081000006, 6.783753885003399375 ) ) ;
#67615 = VECTOR ( 'NONE', #20998, 1000.000000000000114 ) ;
#67614 = CARTESIAN_POINT ( 'NONE',  ( 8.908101985566998948, -4.557680047860001693, -6.178109778951999864 ) ) ;
#67616 = ORIENTED_EDGE ( 'NONE', *, *, #56324, .T. ) ;
#67617 = CARTESIAN_POINT ( 'NONE',  ( 10.08422653160753413, 2.899999999999999911, 6.304440313740826696 ) ) ;
#67618 = AXIS2_PLACEMENT_3D ( 'NONE', #2953, #45619, #19379 ) ;
#67619 = CARTESIAN_POINT ( 'NONE',  ( 9.319055905798999007, 2.899999999999999911, -6.571291218949999902 ) ) ;
#67620 = CARTESIAN_POINT ( 'NONE',  ( 9.622313405920001728, -4.009302068291999532, -9.043024413115999138 ) ) ;
#67621 = DIRECTION ( 'NONE',  ( -2.340984983634000236E-09, 1.000000000000000000, 1.141937478005999895E-09 ) ) ;
#67622 = CARTESIAN_POINT ( 'NONE',  ( 4.966698988835610784, 2.066632171653634664, -9.814801839911485045E-10 ) ) ;
#67623 = CARTESIAN_POINT ( 'NONE',  ( 10.98768521492000083, -5.299565686336999981, -4.945211137252000455 ) ) ;
#67624 = CARTESIAN_POINT ( 'NONE',  ( 24.34832118766533071, 12.03536993114527398, 3.224867653659703404 ) ) ;
#67625 = EDGE_CURVE ( 'NONE', #58126, #10880, #68691, .T. ) ;
#67626 = ADVANCED_FACE ( 'NONE', ( #21731 ), #58118, .F. ) ;
#67627 = CARTESIAN_POINT ( 'NONE',  ( 13.94806348789000161, 8.812672976752997656, 7.562028778248000016 ) ) ;
#67628 = CARTESIAN_POINT ( 'NONE',  ( 16.32020863168424185, -3.595521563589213265, -11.99782687963371153 ) ) ;
#67629 = VECTOR ( 'NONE', #41326, 1000.000000000000000 ) ;
#67630 = EDGE_CURVE ( 'NONE', #13225, #49271, #31552, .T. ) ;
#67631 = CARTESIAN_POINT ( 'NONE',  ( 11.10000057264999995, 0.4999994248636999705, 9.776630284457000997 ) ) ;
#67632 = FACE_BOUND ( 'NONE', #30366, .T. ) ;
#67633 = CARTESIAN_POINT ( 'NONE',  ( 9.906851002540999929, 2.832432432432000269, -6.822293592207000934 ) ) ;
#67634 = ORIENTED_EDGE ( 'NONE', *, *, #6309, .F. ) ;
#67635 = CARTESIAN_POINT ( 'NONE',  ( 12.54926746055851439, 0.6731412448965065076, -12.58200685883812930 ) ) ;
#67636 = CARTESIAN_POINT ( 'NONE',  ( 12.21194436379302317, -2.301855881702226991, -12.49553541603750695 ) ) ;
#67637 = DIRECTION ( 'NONE',  ( 0.000000000000000000, 0.6664713972123997854, -0.7455306007789026523 ) ) ;
#67638 = CARTESIAN_POINT ( 'NONE',  ( 8.834364158772999076, 4.141907758973999876, 6.047574021139999978 ) ) ;
#67639 = FACE_OUTER_BOUND ( 'NONE', #67917, .T. ) ;
#67640 = VERTEX_POINT ( 'NONE', #32250 ) ;
#67641 = DIRECTION ( 'NONE',  ( 1.000000000000000000, 0.000000000000000000, 0.000000000000000000 ) ) ;
#67642 = CARTESIAN_POINT ( 'NONE',  ( 17.59562594671659497, 0.6250000000000000000, 12.67928921589118119 ) ) ;
#67643 = CARTESIAN_POINT ( 'NONE',  ( 13.64720874474600087, -11.45913667646999912, -2.381478076492999918 ) ) ;
#67644 = CARTESIAN_POINT ( 'NONE',  ( 10.12426357027499790, 5.254871132332000094, 7.257895958275299542 ) ) ;
#67645 = CARTESIAN_POINT ( 'NONE',  ( 11.68788784977535933, 3.014014167207800465, -7.443657794094239222 ) ) ;
#67646 = ORIENTED_EDGE ( 'NONE', *, *, #67549, .T. ) ;
#67647 = CARTESIAN_POINT ( 'NONE',  ( 10.98286725694000054, -3.998514182530999772, 9.091066422484001208 ) ) ;
#67648 = VERTEX_POINT ( 'NONE', #68590 ) ;
#67649 = EDGE_CURVE ( 'NONE', #24123, #17996, #27335, .T. ) ;
#67650 = CARTESIAN_POINT ( 'NONE',  ( 7.622413825165171630, -2.920663668686906522, 8.329223781267950599 ) ) ;
#67651 = CARTESIAN_POINT ( 'NONE',  ( 8.239941940377999430, -2.735207418315000361, 6.771977475428999860 ) ) ;
#67652 = CARTESIAN_POINT ( 'NONE',  ( 18.27886422513981302, -0.04806343339260844838, -13.99993753789457962 ) ) ;
#67653 = ORIENTED_EDGE ( 'NONE', *, *, #3138, .F. ) ;
#67654 = DIRECTION ( 'NONE',  ( -1.000000000000000000, 0.000000000000000000, 0.000000000000000000 ) ) ;
#67655 = CARTESIAN_POINT ( 'NONE',  ( 9.050000000000000711, 0.000000000000000000, -4.000000000000000000 ) ) ;
#67656 = CARTESIAN_POINT ( 'NONE',  ( 7.929729719587999881, 2.435784185744999775, -7.548665584409000040 ) ) ;
#67657 = DIRECTION ( 'NONE',  ( 0.000000000000000000, 1.000000000000000000, 0.000000000000000000 ) ) ;
#67658 = CARTESIAN_POINT ( 'NONE',  ( 17.99289217961977627, -2.946103266178389024, 12.33638055411116241 ) ) ;
#67659 = ORIENTED_EDGE ( 'NONE', *, *, #46092, .T. ) ;
#67660 = CARTESIAN_POINT ( 'NONE',  ( 2.146806799206917304, -0.9161175952574931447, 3.408904368339100710 ) ) ;
#67661 = CARTESIAN_POINT ( 'NONE',  ( 12.20137260048311312, -2.663020829440327475, -13.63749600572422871 ) ) ;
#67662 = CARTESIAN_POINT ( 'NONE',  ( 12.79999999202000005, 11.41069016990000051, -4.623987642516999230 ) ) ;
#67663 = VERTEX_POINT ( 'NONE', #53559 ) ;
#67664 = CARTESIAN_POINT ( 'NONE',  ( 5.699996624164000103, -12.50864642754000045, -2.924703664565999617 ) ) ;
#67665 = CARTESIAN_POINT ( 'NONE',  ( 9.152446624286001864, 2.899999999999999911, -6.169193161299999950 ) ) ;
#67666 = ORIENTED_EDGE ( 'NONE', *, *, #40728, .T. ) ;
#67667 = CARTESIAN_POINT ( 'NONE',  ( 24.07540745826431916, 12.58941621619760021, -3.411518517344679147 ) ) ;
#67668 = TOROIDAL_SURFACE ( 'NONE', #2952, 12.20000000000000107, 0.6999999999999999556 ) ;
#67669 = DIRECTION ( 'NONE',  ( 0.000000000000000000, 1.000000000000000000, 0.000000000000000000 ) ) ;
#67670 = CARTESIAN_POINT ( 'NONE',  ( 10.06927318630900103, -3.243547362524661359, -8.526145288591964189 ) ) ;
#67671 = CARTESIAN_POINT ( 'NONE',  ( 10.93769853197999886, 5.063116524846000388, -4.920828787216999345 ) ) ;
#67672 = CARTESIAN_POINT ( 'NONE',  ( 12.18402495282434295, -0.07112389991331875827, -13.89976024287834910 ) ) ;
#67673 = CARTESIAN_POINT ( 'NONE',  ( 17.89701680218578517, -1.976751596789643850, 12.55823001632907499 ) ) ;
#67674 = VERTEX_POINT ( 'NONE', #16150 ) ;
#67675 = CARTESIAN_POINT ( 'NONE',  ( 7.895317210312003731, -5.140737874544996977, 6.778394131643998399 ) ) ;
#67676 = VERTEX_POINT ( 'NONE', #5652 ) ;
#67677 = CARTESIAN_POINT ( 'NONE',  ( 10.29378723213999969, 3.483632952461999999, 6.176337842045999338 ) ) ;
#67678 = B_SPLINE_CURVE_WITH_KNOTS ( 'NONE', 3,
 ( #54422, #60703, #33801, #22601 ),
 .UNSPECIFIED., .F., .F.,
 ( 4, 4 ),
 ( 0.000000000000000000, 1.000000000000000000 ),
 .UNSPECIFIED. ) ;
#67679 = CARTESIAN_POINT ( 'NONE',  ( 12.09999999999999964, -4.817420948848700313, 7.825000000000000178 ) ) ;
#67680 = AXIS2_PLACEMENT_3D ( 'NONE', #61208, #39537, #3160 ) ;
#67681 = CARTESIAN_POINT ( 'NONE',  ( 8.880270280412998929, 4.146787477634999775, -5.941926545671999627 ) ) ;
#67682 = CARTESIAN_POINT ( 'NONE',  ( 2.726256808742000270, -3.050987738140999994, 2.107392784704999578 ) ) ;
#67683 = CARTESIAN_POINT ( 'NONE',  ( 17.80000000009400196, -3.216307036143000175, -11.40341376487999980 ) ) ;
#67684 = LINE ( 'NONE', #16620, #64071 ) ;
#67685 = CARTESIAN_POINT ( 'NONE',  ( 9.004748037742926314, -5.259886971390435484, 7.984416769088259258 ) ) ;
#67686 = EDGE_CURVE ( 'NONE', #60256, #6863, #10374, .T. ) ;
#67687 = EDGE_CURVE ( 'NONE', #25573, #9331, #48775, .T. ) ;
#67688 = ORIENTED_EDGE ( 'NONE', *, *, #58887, .F. ) ;
#67689 = EDGE_CURVE ( 'NONE', #28055, #10085, #47973, .T. ) ;
#67690 = CARTESIAN_POINT ( 'NONE',  ( 12.00687348028854906, -5.003459210197000573, 6.957450711802899868 ) ) ;
#67691 = CARTESIAN_POINT ( 'NONE',  ( 3.290556799210374805, -3.500000000000002220, 0.4581489286484968781 ) ) ;
#67692 = CARTESIAN_POINT ( 'NONE',  ( 16.13682146000800088, 8.990085112443999549, 8.775549782916998609 ) ) ;
#67693 = CARTESIAN_POINT ( 'NONE',  ( 8.207504440379000954, -5.944572422272999646, 7.106845737860000511 ) ) ;
#67695 = CARTESIAN_POINT ( 'NONE',  ( 23.60205915885299888, -2.171992490544001786, -12.06370038613001228 ) ) ;
#67694 = CARTESIAN_POINT ( 'NONE',  ( 10.65050915380999896, 5.200037120669999346, 5.937706951697999891 ) ) ;
#67696 = CARTESIAN_POINT ( 'NONE',  ( 10.67410807141119911, 4.046361247106100123, -8.502397868920999358 ) ) ;
#67697 = CARTESIAN_POINT ( 'NONE',  ( 24.74447986542299915, -11.86527187233999925, 3.111026911665999872 ) ) ;
#67698 = CARTESIAN_POINT ( 'NONE',  ( 9.857646554150999663, 4.486270025758400060, -8.378853663802400931 ) ) ;
#67699 = CARTESIAN_POINT ( 'NONE',  ( 18.27044763842722830, -0.1172743548790616819, 12.59945959730644027 ) ) ;
#67700 = CARTESIAN_POINT ( 'NONE',  ( 25.39994675526091683, -10.74016667838613515, 3.821986401712638592 ) ) ;
#67701 = CARTESIAN_POINT ( 'NONE',  ( 5.000000000000000000, 0.8000000000000000444, -3.149999999999999911 ) ) ;
#67702 = CARTESIAN_POINT ( 'NONE',  ( 23.54908358533199930, 10.40234127004999998, 9.426912626873999557 ) ) ;
#67703 = ORIENTED_EDGE ( 'NONE', *, *, #57773, .T. ) ;
#67704 = CARTESIAN_POINT ( 'NONE',  ( 7.149102686541000118, -4.351670788182000038, 8.977200644264000218 ) ) ;
#67705 = CARTESIAN_POINT ( 'NONE',  ( 18.03520353647598995, 3.065561386738592020, 13.66025540057654553 ) ) ;
#67706 = FACE_BOUND ( 'NONE', #11735, .T. ) ;
#67707 = B_SPLINE_CURVE_WITH_KNOTS ( 'NONE', 3,
 ( #35713, #31499, #21006, #62944, #42341, #31845, #46890, #57031, #63641, #4226, #5262, #30469, #25213, #41301, #68194, #14732, #57364, #9469 ),
 .UNSPECIFIED., .F., .F.,
 ( 4, 2, 2, 2, 2, 2, 2, 2, 4 ),
 ( 0.000000000000000000, 0.1250000000000000000, 0.2500000000000000000, 0.3750000000000000000, 0.5000000000000000000, 0.6250000000000000000, 0.7500000000000000000, 0.8750000000000000000, 1.000000000000000000 ),
 .UNSPECIFIED. ) ;
#67708 = VERTEX_POINT ( 'NONE', #53894 ) ;
#67709 = EDGE_CURVE ( 'NONE', #56039, #27101, #352, .T. ) ;
#67710 = CARTESIAN_POINT ( 'NONE',  ( 18.01722669115800102, 3.499390932422000056, 11.96939125376999868 ) ) ;
#67711 =( GEOMETRIC_REPRESENTATION_CONTEXT ( 3 ) GLOBAL_UNCERTAINTY_ASSIGNED_CONTEXT ( ( #57658 ) ) GLOBAL_UNIT_ASSIGNED_CONTEXT ( ( #62354, #36825, #67935 ) ) REPRESENTATION_CONTEXT ( 'NONE', 'WORKASPACE' ) );
#67712 = CARTESIAN_POINT ( 'NONE',  ( 11.72433327354039889, 3.016779570871600313, 8.143111181492699302 ) ) ;
#67713 = CARTESIAN_POINT ( 'NONE',  ( 11.20537028040999949, 2.688545137295000220, -8.273930556758998023 ) ) ;
#67714 = ORIENTED_EDGE ( 'NONE', *, *, #67402, .T. ) ;
#67715 = CARTESIAN_POINT ( 'NONE',  ( 5.159193173016666911, -0.3926218265389189721, -1.460959015002473604 ) ) ;
#67716 = CARTESIAN_POINT ( 'NONE',  ( 17.92259505138777698, -3.107618780086669918, 12.21081961728240195 ) ) ;
#67717 = CARTESIAN_POINT ( 'NONE',  ( 11.08425954179440076, 4.982976321082899673, 6.683254058608399717 ) ) ;
#67718 = CARTESIAN_POINT ( 'NONE',  ( 11.09999999999999964, 5.350000000000000533, 7.500000000000000000 ) ) ;
#67720 = CARTESIAN_POINT ( 'NONE',  ( 9.884624721933931824, 2.899999999999999911, 6.445686799102332110 ) ) ;
#67719 = AXIS2_PLACEMENT_3D ( 'NONE', #68321, #63073, #57846 ) ;
#67721 = ORIENTED_EDGE ( 'NONE', *, *, #27450, .T. ) ;
#67722 = CARTESIAN_POINT ( 'NONE',  ( 11.25950692870000047, -3.811441498709999820, 11.68087307222999982 ) ) ;
#67723 = B_SPLINE_CURVE_WITH_KNOTS ( 'NONE', 3,
 ( #48086, #1226, #54355, #536, #16609, #43183, #15917, #6113, #59604, #190, #42839, #37934 ),
 .UNSPECIFIED., .F., .F.,
 ( 4, 2, 2, 2, 2, 4 ),
 ( 0.000000000000000000, 0.2500000000000000000, 0.5000000000000000000, 0.7500000000000000000, 0.8750000000000000000, 1.000000000000000000 ),
 .UNSPECIFIED. ) ;
#67724 = CARTESIAN_POINT ( 'NONE',  ( 15.90018573812399971, 8.493548356068000516, 8.263529029821000904 ) ) ;
#67725 = CARTESIAN_POINT ( 'NONE',  ( 8.258127245199675670, -5.292721928877631044, 8.664547103137167028 ) ) ;
#67726 = AXIS2_PLACEMENT_3D ( 'NONE', #3746, #52682, #25082 ) ;
#67727 = CARTESIAN_POINT ( 'NONE',  ( 9.296784697134999220, -3.380386586585000241, 8.459069166353199165 ) ) ;
#67728 = EDGE_LOOP ( 'NONE', ( #43021, #31024, #65962, #18485, #28403 ) ) ;
#67729 = CARTESIAN_POINT ( 'NONE',  ( 10.60379983616000032, -5.060307628864999963, -4.956681627023000303 ) ) ;
#67730 = CARTESIAN_POINT ( 'NONE',  ( 11.41195257254739914, -5.227167235646000165, 7.143100915737699452 ) ) ;
#67731 = ORIENTED_EDGE ( 'NONE', *, *, #22465, .T. ) ;
#67732 = EDGE_CURVE ( 'NONE', #42702, #44271, #54591, .T. ) ;
#67733 = CARTESIAN_POINT ( 'NONE',  ( 11.50029455687000102, -11.65000000000000036, 0.000000000000000000 ) ) ;
#67734 = ORIENTED_EDGE ( 'NONE', *, *, #13213, .F. ) ;
#67735 = CARTESIAN_POINT ( 'NONE',  ( 9.099999999999999645, 0.000000000000000000, 0.000000000000000000 ) ) ;
#67736 = CARTESIAN_POINT ( 'NONE',  ( 10.90000000000000036, -1.300000000000000044, 9.662944685757000940 ) ) ;
#67737 = CARTESIAN_POINT ( 'NONE',  ( 10.89835090130999973, 4.878966983716200190, -8.043647632228999811 ) ) ;
#67738 = CARTESIAN_POINT ( 'NONE',  ( 12.25203632436370071, -5.109717061557999429, 7.759151359668400083 ) ) ;
#67739 = CARTESIAN_POINT ( 'NONE',  ( 12.25653845796823482, 2.200227119461481529, -12.51640343681226142 ) ) ;
#67740 = CARTESIAN_POINT ( 'NONE',  ( 10.87457053952200070, -4.448306506338299826, 8.548957288282998945 ) ) ;
#67741 = CARTESIAN_POINT ( 'NONE',  ( 8.849385841230999361, 3.975069902178000270, 9.483774112875002160 ) ) ;
#67742 = VERTEX_POINT ( 'NONE', #61139 ) ;
#67743 = CARTESIAN_POINT ( 'NONE',  ( 4.649999478197480052, 2.033928581112999763E-13, -2.806643806251999915E-13 ) ) ;
#67744 = CARTESIAN_POINT ( 'NONE',  ( 9.294724726289000927, -4.148132978932999926, 9.337467253566000380 ) ) ;
#67745 = CARTESIAN_POINT ( 'NONE',  ( 11.09999999999999964, -5.299316147296000423, 5.124965750789000296 ) ) ;
#67746 = ORIENTED_EDGE ( 'NONE', *, *, #39146, .F. ) ;
#67747 = CARTESIAN_POINT ( 'NONE',  ( 12.42670498308437210, -2.997500030636913060, -12.32161918487003582 ) ) ;
#67748 = CARTESIAN_POINT ( 'NONE',  ( 10.15303300763299887, 4.787165141710600480, 6.674373427955200277 ) ) ;
#67749 = CARTESIAN_POINT ( 'NONE',  ( 11.16750564679000135, -3.188702545307000147, -8.788667016604001958 ) ) ;
#67750 = CARTESIAN_POINT ( 'NONE',  ( 9.600562361968000502, 10.31800062403999441, -4.698177885259996245 ) ) ;
#67751 = CARTESIAN_POINT ( 'NONE',  ( 17.86459523290600160, -11.80388957783000059, 3.369424016599000371 ) ) ;
#67752 = CARTESIAN_POINT ( 'NONE',  ( 9.333766445374624965, 2.750000000000000444, -7.340348008080749054 ) ) ;
#67753 = CARTESIAN_POINT ( 'NONE',  ( 12.80505043854146763, -3.248147246781389885, -13.61798588129780896 ) ) ;
#67754 = B_SPLINE_CURVE_WITH_KNOTS ( 'NONE', 3,
 ( #40561, #50718, #2812, #45473 ),
 .UNSPECIFIED., .F., .F.,
 ( 4, 4 ),
 ( 0.000000000000000000, 1.000000000000000000 ),
 .UNSPECIFIED. ) ;
#67755 = CARTESIAN_POINT ( 'NONE',  ( 10.97364560330029981, -3.734560974198899874, -6.675475461903199736 ) ) ;
#67756 = CARTESIAN_POINT ( 'NONE',  ( 10.81349144726329925, -4.738947899111299655, -6.457276458983999490 ) ) ;
#67757 = FACE_OUTER_BOUND ( 'NONE', #50463, .T. ) ;
#67758 = ORIENTED_EDGE ( 'NONE', *, *, #42574, .F. ) ;
#67759 = ORIENTED_EDGE ( 'NONE', *, *, #41039, .F. ) ;
#67760 = CARTESIAN_POINT ( 'NONE',  ( 12.71012435277331853, 0.7254930141035413893, -13.98119259374237444 ) ) ;
#67761 = AXIS2_PLACEMENT_3D ( 'NONE', #18953, #66842, #13030 ) ;
#67762 = PLANE ( 'NONE',  #110 ) ;
#67763 = CARTESIAN_POINT ( 'NONE',  ( 17.99248396117510751, 2.946503669282361404, 13.56850299727437736 ) ) ;
#67764 = CARTESIAN_POINT ( 'NONE',  ( 10.78637067803999905, 5.666041748529999644, -7.787005432561999285 ) ) ;
#67765 = DIRECTION ( 'NONE',  ( 0.000000000000000000, 1.000000000000000000, 0.000000000000000000 ) ) ;
#67766 =( GEOMETRIC_REPRESENTATION_CONTEXT ( 3 ) GLOBAL_UNCERTAINTY_ASSIGNED_CONTEXT ( ( #53457 ) ) GLOBAL_UNIT_ASSIGNED_CONTEXT ( ( #64053, #38182, #15831 ) ) REPRESENTATION_CONTEXT ( 'NONE', 'WORKASPACE' ) );
#67767 = CARTESIAN_POINT ( 'NONE',  ( 18.06437450929126243, 2.862796250983955737, 12.35961424106609208 ) ) ;
#67768 = DIRECTION ( 'NONE',  ( -0.000000000000000000, 0.008867170401640299751, 0.9999606858717338120 ) ) ;
#67769 = EDGE_CURVE ( 'NONE', #56890, #58925, #8646, .T. ) ;
#67771 = ADVANCED_FACE ( 'NONE', ( #3426 ), #58924, .F. ) ;
#67770 = CARTESIAN_POINT ( 'NONE',  ( 10.65550720192000078, 4.237674045823999869, 9.105219676299999065 ) ) ;
#67772 = VECTOR ( 'NONE', #33842, 1000.000000000000000 ) ;
#67773 = CARTESIAN_POINT ( 'NONE',  ( 8.716296636326459790, -4.700163249105822949, -6.344245921207472882 ) ) ;
#67774 = EDGE_CURVE ( 'NONE', #24046, #32256, #55416, .T. ) ;
#67775 = EDGE_CURVE ( 'NONE', #61078, #57180, #19858, .T. ) ;
#67776 = ORIENTED_EDGE ( 'NONE', *, *, #25273, .F. ) ;
#67777 = CARTESIAN_POINT ( 'NONE',  ( 12.09999999999999964, -2.820501972398000046, 7.825000000000000178 ) ) ;
#67778 = CARTESIAN_POINT ( 'NONE',  ( 8.893126402770997530, -3.188752782784400441, -7.194081880505399873 ) ) ;
#67779 = CARTESIAN_POINT ( 'NONE',  ( 10.59303303094000093, 2.436236667456999960, 7.793464546548000804 ) ) ;
#67780 = CARTESIAN_POINT ( 'NONE',  ( 11.05569598648999907, -2.869047858956000230, 6.826612223887499553 ) ) ;
#67781 = CARTESIAN_POINT ( 'NONE',  ( 9.865910841232000905, 2.685250982074999904, -7.026194612421999608 ) ) ;
#67782 = AXIS2_PLACEMENT_3D ( 'NONE', #13489, #66947, #50881 ) ;
#67783 = CARTESIAN_POINT ( 'NONE',  ( 11.01659413146999889, 7.354810577943000638, -6.171169745271000373 ) ) ;
#67784 = B_SPLINE_CURVE_WITH_KNOTS ( 'NONE', 3,
 ( #36892, #63441, #11680, #16239, #26747 ),
 .UNSPECIFIED., .F., .F.,
 ( 4, 1, 4 ),
 ( 0.000000000000000000, 0.5000000000000000000, 1.000000000000000000 ),
 .UNSPECIFIED. ) ;
#67785 = CARTESIAN_POINT ( 'NONE',  ( 25.09299597186400277, 8.442821527965000072, 8.583356320261000150 ) ) ;
#67786 = CARTESIAN_POINT ( 'NONE',  ( 12.29717897459458875, 0.3644117276601258060, 12.69296657371243953 ) ) ;
#67787 = CARTESIAN_POINT ( 'NONE',  ( 8.738426658774001154, 5.414918126383000185, 8.890678916765999418 ) ) ;
#67788 = CARTESIAN_POINT ( 'NONE',  ( 10.28314886242000092, 2.387776420306999992, 7.684265965147999644 ) ) ;
#67789 = AXIS2_PLACEMENT_3D ( 'NONE', #7925, #29262, #35865 ) ;
#67790 = CARTESIAN_POINT ( 'NONE',  ( 11.53713315544000118, -3.620704573398000115, 11.03277391605000091 ) ) ;
#67791 = VERTEX_POINT ( 'NONE', #9351 ) ;
#67792 = CARTESIAN_POINT ( 'NONE',  ( 9.924495280410999598, 4.946705552514000459, -6.253848946732999181 ) ) ;
#67793 = CARTESIAN_POINT ( 'NONE',  ( 6.994740308324000289, -1.394461760113000048, 0.5163436683935999083 ) ) ;
#67794 = ADVANCED_FACE ( 'NONE', ( #62836 ), #10393, .T. ) ;
#67795 = CARTESIAN_POINT ( 'NONE',  ( 17.93834580300581649, 2.005905130196157238, 13.76587868752632460 ) ) ;
#67796 = CARTESIAN_POINT ( 'NONE',  ( 11.45284386393252696, 4.902679577238613362, -7.175013233162909287 ) ) ;
#67797 = CARTESIAN_POINT ( 'NONE',  ( 10.34393020684899867, 2.750000000000000000, -7.500000000000000000 ) ) ;
#67798 = CARTESIAN_POINT ( 'NONE',  ( 11.04333729122639873, -5.003122373830000136, -7.473611442402849470 ) ) ;
#67799 = ORIENTED_EDGE ( 'NONE', *, *, #65528, .T. ) ;
#67800 = CARTESIAN_POINT ( 'NONE',  ( 2.254339447823000331, -2.269833785962000139, -2.784166953248000009 ) ) ;
#67801 = CARTESIAN_POINT ( 'NONE',  ( 10.13804496475983186, -5.254201105732013488, 6.278396282701761422 ) ) ;
#67803 = DIRECTION ( 'NONE',  ( 1.000000000000000000, 0.000000000000000000, 0.000000000000000000 ) ) ;
#67802 = CARTESIAN_POINT ( 'NONE',  ( 10.00464026716699806, 2.641193587372907103, 6.397822249176915221 ) ) ;
#67804 = LINE ( 'NONE', #46841, #22383 ) ;
#67805 = CARTESIAN_POINT ( 'NONE',  ( 13.50003721581400029, 9.159934378815998812, 7.517910889891000537 ) ) ;
#67806 = CARTESIAN_POINT ( 'NONE',  ( 18.13779378220194971, -2.273859756726421377, -13.71877938508614037 ) ) ;
#67807 = CARTESIAN_POINT ( 'NONE',  ( 10.60441638348510018, 3.158410350011299883, 7.705001100909899314 ) ) ;
#67808 = CARTESIAN_POINT ( 'NONE',  ( 24.76779883137896476, -11.72407962198572839, 3.191093704755281202 ) ) ;
#67809 = CARTESIAN_POINT ( 'NONE',  ( 8.400066940379998570, -2.800111029801999774, 9.079936276749000612 ) ) ;
#67810 = ORIENTED_EDGE ( 'NONE', *, *, #36707, .T. ) ;
#67811 = CARTESIAN_POINT ( 'NONE',  ( 9.304732780410999382, 5.284130523641000110, 6.489275570566000795 ) ) ;
#67813 = CARTESIAN_POINT ( 'NONE',  ( 10.79702055961999818, -5.792859009854000263, -7.049265738992000152 ) ) ;
#67812 = CARTESIAN_POINT ( 'NONE',  ( 5.195847890838999561, -1.431922326323000094, -0.3257311615064000243 ) ) ;
#67814 = CARTESIAN_POINT ( 'NONE',  ( 7.577752120373228095, -4.080750291709096089, 5.762678877088324825 ) ) ;
#67815 = AXIS2_PLACEMENT_3D ( 'NONE', #68249, #30187, #8850 ) ;
#67816 = DIRECTION ( 'NONE',  ( 0.000000000000000000, 0.7071067811865475727, -0.7071067811865475727 ) ) ;
#67817 = CARTESIAN_POINT ( 'NONE',  ( 1.790929700619999787, 1.756325177964999984, 2.941112093452000309 ) ) ;
#67818 = ORIENTED_EDGE ( 'NONE', *, *, #24618, .F. ) ;
#67819 = DIRECTION ( 'NONE',  ( 0.000000000000000000, 0.9516627710998093459, 0.3071448682668031505 ) ) ;
#67820 = CARTESIAN_POINT ( 'NONE',  ( 11.12903166480609940, -4.864052766304100217, 7.439078678739090122 ) ) ;
#67821 = CARTESIAN_POINT ( 'NONE',  ( 10.90710314112699564, -5.175205309304410584, -8.818007615062088078 ) ) ;
#67822 = CARTESIAN_POINT ( 'NONE',  ( 10.81579666500999970, 5.374569445151000657, 6.698728322222000209 ) ) ;
#67823 = ADVANCED_FACE ( 'NONE', ( #5149 ), #30694, .F. ) ;
#67824 =( GEOMETRIC_REPRESENTATION_CONTEXT ( 3 ) GLOBAL_UNCERTAINTY_ASSIGNED_CONTEXT ( ( #13405 ) ) GLOBAL_UNIT_ASSIGNED_CONTEXT ( ( #59088, #11190, #38455 ) ) REPRESENTATION_CONTEXT ( 'NONE', 'WORKASPACE' ) );
#67825 = CARTESIAN_POINT ( 'NONE',  ( 11.26072066707849828, 4.976067344118500380, 8.090408888831799317 ) ) ;
#67826 = B_SPLINE_CURVE_WITH_KNOTS ( 'NONE', 3,
 ( #49437, #12387, #55038, #12737, #24252, #65513, #50479, #34418, #17641, #7836, #7478, #34757, #44902, #35104 ),
 .UNSPECIFIED., .F., .F.,
 ( 4, 2, 2, 2, 2, 2, 4 ),
 ( 0.000000000000000000, 0.2500000000000002220, 0.3749999999999998890, 0.4999999999999995559, 0.6249999999999992228, 0.7499999999999988898, 1.000000000000000000 ),
 .UNSPECIFIED. ) ;
#67827 = DIRECTION ( 'NONE',  ( -1.000000000000000000, 0.000000000000000000, 0.000000000000000000 ) ) ;
#67828 = EDGE_CURVE ( 'NONE', #22792, #68105, #63175, .T. ) ;
#67829 = AXIS2_PLACEMENT_3D ( 'NONE', #4668, #27048, #21108 ) ;
#67830 = CARTESIAN_POINT ( 'NONE',  ( 8.599999952505998024, 4.749999993641800700, 7.500000000000000000 ) ) ;
#67831 = CARTESIAN_POINT ( 'NONE',  ( 23.85399112845500369, -3.593188128842942586, -13.20264652469179545 ) ) ;
#67832 = CARTESIAN_POINT ( 'NONE',  ( 8.356851002541000994, 2.832432432432000269, -6.822293592207000934 ) ) ;
#67833 = VECTOR ( 'NONE', #49246, 1000.000000000000000 ) ;
#67834 = CARTESIAN_POINT ( 'NONE',  ( 18.13175260058829963, -2.961013189755323349, 13.68330200419956988 ) ) ;
#67835 = CARTESIAN_POINT ( 'NONE',  ( 17.81487012556099359, 3.068783844977785336, -13.53623303301527159 ) ) ;
#67836 = ORIENTED_EDGE ( 'NONE', *, *, #46405, .T. ) ;
#67837 = CARTESIAN_POINT ( 'NONE',  ( 8.616332388160998335, -5.167567399848000065, -6.822293593032000558 ) ) ;
#67838 = CARTESIAN_POINT ( 'NONE',  ( 9.140654977342494547, -2.950420301507454379, -6.802596805975135830 ) ) ;
#67839 = EDGE_LOOP ( 'NONE', ( #45955, #53973, #10368, #48760 ) ) ;
#67840 = CARTESIAN_POINT ( 'NONE',  ( 9.343930206849998754, 2.750000000000000000, 7.500000000000000000 ) ) ;
#67841 = CARTESIAN_POINT ( 'NONE',  ( 15.90018573812399971, 8.493548356068000516, 8.263529029821000904 ) ) ;
#67842 = CARTESIAN_POINT ( 'NONE',  ( 10.77962664842000073, 2.397507474987000009, 7.755423212350999407 ) ) ;
#67843 = CARTESIAN_POINT ( 'NONE',  ( 9.831594052344000190, 3.539229510464000139, -8.956011942092999334 ) ) ;
#67844 = CARTESIAN_POINT ( 'NONE',  ( 10.03743284169262573, -4.454886069780877200, -6.752597208702827203 ) ) ;
#67845 = CARTESIAN_POINT ( 'NONE',  ( 9.590594544025000445, -2.445960766574000189, 7.841185849078001091 ) ) ;
#67846 = CARTESIAN_POINT ( 'NONE',  ( 18.27886405737313069, 0.04734719685816928675, -12.59993264914401401 ) ) ;
#67847 = AXIS2_PLACEMENT_3D ( 'NONE', #2424, #56256, #3110 ) ;
#67848 = CARTESIAN_POINT ( 'NONE',  ( 23.58888758076617265, -13.25332336394347621, -4.277527736586637097 ) ) ;
#67849 = CARTESIAN_POINT ( 'NONE',  ( 10.85056919669530018, -3.169300617545700138, -7.745432529082900253 ) ) ;
#67850 = FACE_OUTER_BOUND ( 'NONE', #23217, .T. ) ;
#67851 = ORIENTED_EDGE ( 'NONE', *, *, #53523, .F. ) ;
#67852 = CARTESIAN_POINT ( 'NONE',  ( 10.96873203361999849, -5.814970961921999582, -4.932337198421000046 ) ) ;
#67853 = CARTESIAN_POINT ( 'NONE',  ( 9.466846873515667227, 3.231816600031355069, 6.500416447002276499 ) ) ;
#67854 = CARTESIAN_POINT ( 'NONE',  ( 8.996463691919831973, 5.100000000000000533, -6.665341197420957542 ) ) ;
#67855 = CARTESIAN_POINT ( 'NONE',  ( 8.688612068284333745, 2.650857310365788422, 7.263856826349759821 ) ) ;
#67856 = CYLINDRICAL_SURFACE ( 'NONE', #18291, 11.79499999999999993 ) ;
#67857 = CARTESIAN_POINT ( 'NONE',  ( 12.33310466175876741, 1.963577280744727149, 13.86161695422964435 ) ) ;
#67858 = CARTESIAN_POINT ( 'NONE',  ( 11.02445830383999947, -3.404091099119999519, 5.822494319281999786 ) ) ;
#67859 = ORIENTED_EDGE ( 'NONE', *, *, #36784, .T. ) ;
#67860 = CARTESIAN_POINT ( 'NONE',  ( 12.23148815955158142, 0.2485241243229640573, -12.69673260777818946 ) ) ;
#67862 = EDGE_CURVE ( 'NONE', #32077, #23499, #3763, .T. ) ;
#67861 = AXIS2_PLACEMENT_3D ( 'NONE', #50062, #22439, #17555 ) ;
#67863 = CARTESIAN_POINT ( 'NONE',  ( 12.53842061970401822, -0.6791475903684007775, 13.98351814429473094 ) ) ;
#67864 = ADVANCED_FACE ( 'NONE', ( #52004 ), #4040, .T. ) ;
#67865 = VERTEX_POINT ( 'NONE', #25443 ) ;
#67866 = CARTESIAN_POINT ( 'NONE',  ( 12.19289742234822072, -2.094552964378148641, 12.42468808284045245 ) ) ;
#67867 = CARTESIAN_POINT ( 'NONE',  ( 7.199141827028999963, 0.000000000000000000, -1.200857723089999940 ) ) ;
#67868 = CARTESIAN_POINT ( 'NONE',  ( 10.79184687351629890, -4.999583552997724389, -6.731816600031356401 ) ) ;
#67869 = CARTESIAN_POINT ( 'NONE',  ( 11.96595122972050085, -3.656201404350900130, 8.295047870239098842 ) ) ;
#67870 = B_SPLINE_CURVE_WITH_KNOTS ( 'NONE', 3,
 ( #23683, #54810, #40121, #1673 ),
 .UNSPECIFIED., .F., .F.,
 ( 4, 4 ),
 ( 0.4999999997918080918, 1.000000000000000000 ),
 .UNSPECIFIED. ) ;
#67871 = VECTOR ( 'NONE', #27320, 1000.000000000000000 ) ;
#67872 = CARTESIAN_POINT ( 'NONE',  ( 8.729782384210551527, 4.176498446805472220, -8.849932004427472521 ) ) ;
#67873 = CYLINDRICAL_SURFACE ( 'NONE', #47673, 13.17499999999999893 ) ;
#67874 = CARTESIAN_POINT ( 'NONE',  ( 11.23052404082913291, 2.954319127720149041, -7.175009054135016662 ) ) ;
#67875 = AXIS2_PLACEMENT_3D ( 'NONE', #68294, #68639, #9923 ) ;
#67876 = CARTESIAN_POINT ( 'NONE',  ( 12.24851426484563177, 2.019008278824861335, 12.43718985311489966 ) ) ;
#67877 = CARTESIAN_POINT ( 'NONE',  ( 9.309310001151999359, -5.531435376468999188, -8.256621485025000595 ) ) ;
#67878 = CARTESIAN_POINT ( 'NONE',  ( 11.06795257254739973, 3.036453385827900142, -7.780229861306499295 ) ) ;
#67879 = CARTESIAN_POINT ( 'NONE',  ( 10.62947109217999930, 5.100000000000000533, 6.152188490330000370 ) ) ;
#67880 = CARTESIAN_POINT ( 'NONE',  ( 12.80505043854144276, 0.6249999999999994449, -12.67928921589118652 ) ) ;
#67881 = EDGE_CURVE ( 'NONE', #36489, #31711, #46775, .T. ) ;
#67882 = CARTESIAN_POINT ( 'NONE',  ( 9.503988259786000370, 3.832626376493700082, -8.768215461831999846 ) ) ;
#67884 = CARTESIAN_POINT ( 'NONE',  ( 9.283078676347997771, -4.247267730859300094, 6.553315803938899897 ) ) ;
#67883 = CARTESIAN_POINT ( 'NONE',  ( 10.99999648468999958, -1.199999999999999956, -9.776630298829998011 ) ) ;
#67885 = LINE ( 'NONE', #46577, #47530 ) ;
#67886 = ORIENTED_EDGE ( 'NONE', *, *, #68106, .F. ) ;
#67887 = AXIS2_PLACEMENT_3D ( 'NONE', #30265, #31294, #20446 ) ;
#67888 = DIRECTION ( 'NONE',  ( 0.000000000000000000, -0.3222656952305000266, -0.9466492601157001641 ) ) ;
#67889 = CARTESIAN_POINT ( 'NONE',  ( 9.546517828664185856, 2.481203689726812822, -8.418993938519275133 ) ) ;
#67890 = CARTESIAN_POINT ( 'NONE',  ( 10.31155864497999808, 4.682585200569199912, 6.965412239408199646 ) ) ;
#67891 = CARTESIAN_POINT ( 'NONE',  ( 23.54905757042499914, -2.963884539164999943, 13.72195237095000131 ) ) ;
#67892 = CONICAL_SURFACE ( 'NONE', #53378, 13.94234658587000197, 1.233427434088239627 ) ;
#67893 = CARTESIAN_POINT ( 'NONE',  ( 24.60109515015806281, 12.20853554534348007, -3.061026489875391388 ) ) ;
#67894 = DIRECTION ( 'NONE',  ( 1.000000000000000000, 0.000000000000000000, 0.000000000000000000 ) ) ;
#67895 = CARTESIAN_POINT ( 'NONE',  ( 12.25784352200408200, 2.802116367125526253, 13.60467368965351120 ) ) ;
#67896 = CARTESIAN_POINT ( 'NONE',  ( 23.64710177088100096, 3.329564310917000114, -13.50251062865999963 ) ) ;
#67897 = ORIENTED_EDGE ( 'NONE', *, *, #12080, .F. ) ;
#67898 = CARTESIAN_POINT ( 'NONE',  ( 4.238373395050000880, 0.5984951807791000222, 1.096724531692999882 ) ) ;
#67899 = CARTESIAN_POINT ( 'NONE',  ( 9.225367640781000134, -3.396982508013000501, -6.371835875489000323 ) ) ;
#67900 = CIRCLE ( 'NONE', #55644, 2.149999999999999911 ) ;
#67901 = CARTESIAN_POINT ( 'NONE',  ( 10.36409410702807143, -4.658690586846539361, -4.954046122677381980 ) ) ;
#67902 = CARTESIAN_POINT ( 'NONE',  ( 11.68923293495519999, -5.032672437899000428, 7.541513160549049744 ) ) ;
#67903 = CARTESIAN_POINT ( 'NONE',  ( 18.26259847173841422, 2.320949922530730181, -12.38441499264346390 ) ) ;
#67904 = CARTESIAN_POINT ( 'NONE',  ( 2.730140132542667963, -3.408904368339107815, 0.9161175952574674985 ) ) ;
#67905 = CARTESIAN_POINT ( 'NONE',  ( 18.01268549161953914, 2.926083040867999863, 12.34202569327310250 ) ) ;
#67906 = CARTESIAN_POINT ( 'NONE',  ( 12.42225203016886148, 3.001455243200948253, -13.55441486462863665 ) ) ;
#67907 = CARTESIAN_POINT ( 'NONE',  ( 11.09999999999999964, -4.000000000000000000, -7.500000000000000000 ) ) ;
#67908 = CARTESIAN_POINT ( 'NONE',  ( 10.00190805961999807, -2.729654112791000120, -8.843024969850999284 ) ) ;
#67909 = EDGE_CURVE ( 'NONE', #33561, #65121, #20411, .T. ) ;
#67910 = CARTESIAN_POINT ( 'NONE',  ( 8.906851002547000462, 2.832432432432000269, -6.822293592207000934 ) ) ;
#67911 = CARTESIAN_POINT ( 'NONE',  ( 12.12629894760562621, 0.2577288767859165497, -13.99764474128114777 ) ) ;
#67912 = CARTESIAN_POINT ( 'NONE',  ( 8.969356963619999235, 2.880642974985999860, -7.499999999914821025 ) ) ;
#67913 = FACE_OUTER_BOUND ( 'NONE', #68434, .T. ) ;
#67914 = FACE_OUTER_BOUND ( 'NONE', #27004, .T. ) ;
#67915 = CARTESIAN_POINT ( 'NONE',  ( 8.772439158776000667, 3.098073081301000009, -8.567513114264999174 ) ) ;
#67916 = CARTESIAN_POINT ( 'NONE',  ( 12.06441235500451015, -4.638700978900200056, 8.085115074060599483 ) ) ;
#67917 = EDGE_LOOP ( 'NONE', ( #53906, #55447, #26148, #10915, #46376 ) ) ;
#67918 = CARTESIAN_POINT ( 'NONE',  ( 8.466090690305595245, -5.179931350395992062, 8.180989497825457590 ) ) ;
#67919 = CARTESIAN_POINT ( 'NONE',  ( 18.03598133453868968, 1.971494603937298917, -13.86049335245054159 ) ) ;
#67920 = VERTEX_POINT ( 'NONE', #14954 ) ;
#67921 = CARTESIAN_POINT ( 'NONE',  ( 9.934038493598999153, -3.372531419565699906, 8.098323595618600379 ) ) ;
#67922 = CARTESIAN_POINT ( 'NONE',  ( 12.79999999202000005, -11.41069016990000051, 4.623987642516999230 ) ) ;
#67923 = CARTESIAN_POINT ( 'NONE',  ( 11.09999999999999964, -4.000000000000000000, 7.500000000000000000 ) ) ;
#67924 = CARTESIAN_POINT ( 'NONE',  ( 13.99999999347100044, 9.187456302440001110, 8.213201953411001455 ) ) ;
#67925 = CARTESIAN_POINT ( 'NONE',  ( 10.85679632507500081, -3.509334349252600127, -8.409605917786398877 ) ) ;
#67926 = CARTESIAN_POINT ( 'NONE',  ( 11.60000000000000142, -3.752125624359933909, -6.451199048602688002 ) ) ;
#67927 = AXIS2_PLACEMENT_3D ( 'NONE', #2889, #24213, #45556 ) ;
#67928 = CYLINDRICAL_SURFACE ( 'NONE', #38504, 1.449999999999999734 ) ;
#67929 = ORIENTED_EDGE ( 'NONE', *, *, #1799, .F. ) ;
#67930 = CARTESIAN_POINT ( 'NONE',  ( 7.627164364716389144, 5.349908229800731441, -7.706112628381206697 ) ) ;
#67931 = CARTESIAN_POINT ( 'NONE',  ( 8.988579719593998263, 4.902869380824999901, -8.978557145469999057 ) ) ;
#67932 = VERTEX_POINT ( 'NONE', #36977 ) ;
#67933 = AXIS2_PLACEMENT_3D ( 'NONE', #32262, #21745, #59155 ) ;
#67934 = CARTESIAN_POINT ( 'NONE',  ( 10.60199294549000193, 2.164976235211999889, -7.764525279724000306 ) ) ;
#67935 =( NAMED_UNIT ( * ) SI_UNIT ( $, .STERADIAN. ) SOLID_ANGLE_UNIT ( ) );
#67936 = ORIENTED_EDGE ( 'NONE', *, *, #48446, .T. ) ;
#67937 = CARTESIAN_POINT ( 'NONE',  ( 8.668126402770999661, 5.196937059091999878, 7.951360234587600218 ) ) ;
#67938 = CARTESIAN_POINT ( 'NONE',  ( 17.77742128654740839, -1.915804696728240941, -12.56864479336926088 ) ) ;
#67939 = CARTESIAN_POINT ( 'NONE',  ( 11.40156680346000151, -11.68030187645999973, -1.636056047313999784 ) ) ;
#67940 = COLOUR_RGB ( '', 0.40784314, 0.44705882, 0.49803922) ;
#67941 = CARTESIAN_POINT ( 'NONE',  ( 27.64127793187000037, -5.599999999999999645, 6.571291218949999902 ) ) ;
#67942 = EDGE_CURVE ( 'NONE', #24760, #63789, #61287, .T. ) ;
#67943 = CARTESIAN_POINT ( 'NONE',  ( 24.44496483130000186, -3.224879855413000040, 12.03535978074999946 ) ) ;
#67944 = EDGE_CURVE ( 'NONE', #3150, #36346, #53398, .T. ) ;
#67945 = VERTEX_POINT ( 'NONE', #21912 ) ;
#67946 = DIRECTION ( 'NONE',  ( 1.000000000000000000, 0.000000000000000000, 0.000000000000000000 ) ) ;
#67947 = CARTESIAN_POINT ( 'NONE',  ( 11.37168584123000059, 2.803494217761000495, -6.967881733280000489 ) ) ;
#67948 = CIRCLE ( 'NONE', #13286, 1.250000000000000000 ) ;
#67949 = CARTESIAN_POINT ( 'NONE',  ( 25.46371819568200223, 2.879482785682999868, 11.30954024936000124 ) ) ;
#67950 = CARTESIAN_POINT ( 'NONE',  ( 12.75695158412489150, 3.246897126047498361, -13.61828421767944164 ) ) ;
#67951 = CARTESIAN_POINT ( 'NONE',  ( 18.25212991285166808, 0.2010519787742756082, 13.99856097495847607 ) ) ;
#67952 = CARTESIAN_POINT ( 'NONE',  ( 17.76427412810700091, 3.313981393620000215, 11.22406656470000108 ) ) ;
#67953 = CARTESIAN_POINT ( 'NONE',  ( 9.753033816428001046, -4.922930220739999641, -8.639537379291999386 ) ) ;
#67954 = ORIENTED_EDGE ( 'NONE', *, *, #24704, .F. ) ;
#67955 = VERTEX_POINT ( 'NONE', #16670 ) ;
#67956 = CARTESIAN_POINT ( 'NONE',  ( 9.169760841232999837, 4.728328492779000136, -8.692725459657999920 ) ) ;
#67957 = CARTESIAN_POINT ( 'NONE',  ( 10.99999999997000089, 4.000000000000000000, -8.949999999967999997 ) ) ;
#67958 = CARTESIAN_POINT ( 'NONE',  ( 2.716661701819526709, -2.750000000000000000, -3.881553357679799511E-10 ) ) ;
#67959 = CARTESIAN_POINT ( 'NONE',  ( 23.80948464333900816, 3.305733230510045750, 13.11180694039508943 ) ) ;
#67960 = CARTESIAN_POINT ( 'NONE',  ( 7.875706921239332914, 4.438897210574712204, 6.198347075216069868 ) ) ;
#67961 = ADVANCED_FACE ( 'NONE', ( #11768 ), #5146, .F. ) ;
#67962 = CARTESIAN_POINT ( 'NONE',  ( 17.86873602477000134, -3.252323392204000019, -11.33729809900999896 ) ) ;
#67964 = CARTESIAN_POINT ( 'NONE',  ( 25.46375152665800101, -2.879425814940999917, -11.30951176145000048 ) ) ;
#67963 = CARTESIAN_POINT ( 'NONE',  ( 9.977709346417000802, -3.092687088662700035, 7.930842873041400232 ) ) ;
#67965 = CARTESIAN_POINT ( 'NONE',  ( 9.041579158320997678, -5.131952024793004163, -6.343693428288000646 ) ) ;
#67966 = ORIENTED_EDGE ( 'NONE', *, *, #24474, .T. ) ;
#67967 = EDGE_CURVE ( 'NONE', #51438, #55718, #26247, .T. ) ;
#67968 = FACE_OUTER_BOUND ( 'NONE', #2266, .T. ) ;
#67969 = CARTESIAN_POINT ( 'NONE',  ( 10.34549887484000052, -3.253839642723999948, -4.718279307348000273 ) ) ;
#67970 = CARTESIAN_POINT ( 'NONE',  ( 10.56244474310100045, 5.137935629024000583, 6.947770206896899836 ) ) ;
#67971 = CARTESIAN_POINT ( 'NONE',  ( 18.18005043799237086, -2.500000011518549670, 12.45159158845318359 ) ) ;
#67972 = VECTOR ( 'NONE', #61451, 1000.000000000000000 ) ;
#67973 = FACE_OUTER_BOUND ( 'NONE', #35425, .T. ) ;
#67974 = CARTESIAN_POINT ( 'NONE',  ( 10.64393020684899938, -2.750000000000000000, 7.500000000000000000 ) ) ;
#67975 = CARTESIAN_POINT ( 'NONE',  ( 24.39664237533066427, 12.03536608459189772, 3.224866623003459498 ) ) ;
#67976 = CARTESIAN_POINT ( 'NONE',  ( 25.49994615402906106, 10.64595569529905816, -3.788460566544836094 ) ) ;
#67977 = CARTESIAN_POINT ( 'NONE',  ( 7.967646874132946699, 2.971274813974494222, -6.517255511639618248 ) ) ;
#67978 = CARTESIAN_POINT ( 'NONE',  ( 6.815773995485999492, -1.064812127159999955, 0.2760466167989999997 ) ) ;
#67979 = CARTESIAN_POINT ( 'NONE',  ( 0.1426929024220463249, 0.4105104488565842202, -3.142673126269484030 ) ) ;
#67980 = CARTESIAN_POINT ( 'NONE',  ( 3.491703015634000096, -2.440397167367000186, 2.160034081118999971 ) ) ;
#67981 = ORIENTED_EDGE ( 'NONE', *, *, #53978, .F. ) ;
#67982 = CARTESIAN_POINT ( 'NONE',  ( 12.60420289721210985, -0.5919389804100259056, -12.68142457171642690 ) ) ;
#67983 = CARTESIAN_POINT ( 'NONE',  ( 12.21947784592275354, -2.718529665895031311, -12.39796232698949652 ) ) ;
#67984 = CARTESIAN_POINT ( 'NONE',  ( 11.50000000000000000, -4.000000000000000000, 7.500000000000000000 ) ) ;
#67985 = CARTESIAN_POINT ( 'NONE',  ( 11.09999999999999964, 0.000000000000000000, -2.784439345760000141E-13 ) ) ;
#67986 = CARTESIAN_POINT ( 'NONE',  ( 3.500000000000000888, 0.002369752946726449983, 3.285293661413511312 ) ) ;
#67987 = VERTEX_POINT ( 'NONE', #16326 ) ;
#67988 = DIRECTION ( 'NONE',  ( -0.8660254037844296038, 7.899625398266597896E-12, 0.5000000000000157652 ) ) ;
#67989 = DIRECTION ( 'NONE',  ( 1.000000000000000000, 0.000000000000000000, 0.000000000000000000 ) ) ;
#67990 = B_SPLINE_CURVE_WITH_KNOTS ( 'NONE', 3,
 ( #12022, #38590, #43846, #48051 ),
 .UNSPECIFIED., .F., .F.,
 ( 4, 4 ),
 ( 0.000000000000000000, 1.000000000000000000 ),
 .UNSPECIFIED. ) ;
#67991 = CARTESIAN_POINT ( 'NONE',  ( 0.5734567831477479505, 2.175120696137909260, 2.781256206680508658 ) ) ;
#67992 = CARTESIAN_POINT ( 'NONE',  ( 10.93769906950999982, 5.063122007744000008, 4.920829195600999739 ) ) ;
#67993 = CARTESIAN_POINT ( 'NONE',  ( 1.678056799206624872, -2.150913519912214245, 2.798833948393621984 ) ) ;
#67994 = CARTESIAN_POINT ( 'NONE',  ( 11.18412378248529926, 3.450971646934100079, -6.461285588983000316 ) ) ;
#67995 = VERTEX_POINT ( 'NONE', #60017 ) ;
#67996 = CARTESIAN_POINT ( 'NONE',  ( 11.03855816545999957, -2.974093234901999949, 8.716125417860000724 ) ) ;
#67997 = EDGE_LOOP ( 'NONE', ( #51061, #3188, #62355 ) ) ;
#67998 = CARTESIAN_POINT ( 'NONE',  ( 9.225036374688860619, -2.649952446100997339, 7.500002253091946791 ) ) ;
#67999 = CARTESIAN_POINT ( 'NONE',  ( 9.331129440379999807, -4.141908960411000429, 6.047561724438000219 ) ) ;
#68000 = FACE_OUTER_BOUND ( 'NONE', #21280, .T. ) ;
#68001 = EDGE_CURVE ( 'NONE', #66715, #59809, #44305, .T. ) ;
#68002 = ORIENTED_EDGE ( 'NONE', *, *, #7796, .F. ) ;
#68003 = CARTESIAN_POINT ( 'NONE',  ( 23.60091554815658554, 10.15345215840743087, 9.602364516840143693 ) ) ;
#68004 = CARTESIAN_POINT ( 'NONE',  ( 7.646881073111088334, 2.711253299328941768, 7.970042138743662186 ) ) ;
#68005 = CARTESIAN_POINT ( 'NONE',  ( 7.043539158770000697, 5.150153908582999485, -6.706147112165000479 ) ) ;
#68006 = DIRECTION ( 'NONE',  ( -9.754664239791915610E-08, 0.7071067475397934121, -0.7071068148332932957 ) ) ;
#68007 = CARTESIAN_POINT ( 'NONE',  ( 10.21613001987144465, -2.826347940569525097, 6.832757752125532491 ) ) ;
#68008 = ORIENTED_EDGE ( 'NONE', *, *, #23599, .F. ) ;
#68009 = CARTESIAN_POINT ( 'NONE',  ( 2.000973465872999846, 3.500000000000000000, 0.000000000000000000 ) ) ;
#68010 = CARTESIAN_POINT ( 'NONE',  ( 12.25784352200452787, -2.802116367126311403, -13.60467368965330337 ) ) ;
#68011 = CARTESIAN_POINT ( 'NONE',  ( 23.59999172348799945, -10.30759808834999980, 9.317726582648999667 ) ) ;
#68012 = ORIENTED_EDGE ( 'NONE', *, *, #63736, .T. ) ;
#68013 = CARTESIAN_POINT ( 'NONE',  ( 9.741009892375998902, -3.588529236307000048, -8.800227248412999970 ) ) ;
#68014 = CARTESIAN_POINT ( 'NONE',  ( 10.81772273141334750, -5.100000000000000533, -6.253511885790826952 ) ) ;
#68015 = ORIENTED_EDGE ( 'NONE', *, *, #58981, .F. ) ;
#68016 = CARTESIAN_POINT ( 'NONE',  ( 10.94990783606475837, 2.251524537340385379, 7.510583322451364729 ) ) ;
#68017 = CARTESIAN_POINT ( 'NONE',  ( 5.125859839683417185, -1.460959015002473382, -0.3926218265389205819 ) ) ;
#68018 = CARTESIAN_POINT ( 'NONE',  ( 11.59999999999999964, 5.386831235742000068, 7.825000000000000178 ) ) ;
#68019 = CARTESIAN_POINT ( 'NONE',  ( 3.115556799210791539, 0.4581489286485002088, 3.500000000000001776 ) ) ;
#68020 = B_SPLINE_CURVE_WITH_KNOTS ( 'NONE', 3,
 ( #1858, #13046, #60244, #12346 ),
 .UNSPECIFIED., .F., .F.,
 ( 4, 4 ),
 ( 0.000000000000000000, 1.000000000000000000 ),
 .UNSPECIFIED. ) ;
#68021 = B_SPLINE_CURVE_WITH_KNOTS ( 'NONE', 3,
 ( #24939, #52537, #63009, #14798, #36813, #26320, #58131, #35779, #47647, #46272, #57094, #9193, #41368, #30534 ),
 .UNSPECIFIED., .F., .F.,
 ( 4, 2, 2, 2, 2, 2, 4 ),
 ( 0.000000000000000000, 0.1250000000000022204, 0.2500000000000044409, 0.5000000000000093259, 0.6250000000000076605, 0.7500000000000059952, 1.000000000000000000 ),
 .UNSPECIFIED. ) ;
#68022 = CARTESIAN_POINT ( 'NONE',  ( 10.90000000000000036, 0.2500000000000000000, 4.902439024389999567 ) ) ;
#68023 = CARTESIAN_POINT ( 'NONE',  ( 18.18008862603428710, -2.492635669256735298, 12.45330984115723361 ) ) ;
#68024 = ORIENTED_EDGE ( 'NONE', *, *, #11203, .T. ) ;
#68025 = ADVANCED_FACE ( 'NONE', ( #49522 ), #6173, .F. ) ;
#68026 = CARTESIAN_POINT ( 'NONE',  ( 10.61257802013489737, -4.891884252872400474, -7.479237407015119743 ) ) ;
#68027 = EDGE_CURVE ( 'NONE', #59240, #44124, #17057, .T. ) ;
#68028 = ORIENTED_EDGE ( 'NONE', *, *, #67881, .T. ) ;
#68029 = CARTESIAN_POINT ( 'NONE',  ( 9.646287586158999616, 2.591467678478000192, 6.760055064032999717 ) ) ;
#68030 = CARTESIAN_POINT ( 'NONE',  ( 11.21253483539785201, -4.338990010211682069, -8.308639362931229400 ) ) ;
#68031 = CARTESIAN_POINT ( 'NONE',  ( 27.64127793187000037, 2.399999999999999911, 6.571291218949999902 ) ) ;
#68032 = EDGE_CURVE ( 'NONE', #36772, #31317, #67093, .T. ) ;
#68033 = CARTESIAN_POINT ( 'NONE',  ( 2.384164467059000092, 2.877138355028999506, -2.068711953730999920 ) ) ;
#68034 = CARTESIAN_POINT ( 'NONE',  ( 10.52342417510000061, -3.209670667763000029, -9.177087527572998837 ) ) ;
#68035 = CARTESIAN_POINT ( 'NONE',  ( 10.98768472569999943, 6.720753179915999631, -5.471698458723999181 ) ) ;
#68036 = CARTESIAN_POINT ( 'NONE',  ( 8.975133088423635996, -5.349981448246158955, 7.499992563499107590 ) ) ;
#68037 = ORIENTED_EDGE ( 'NONE', *, *, #2057, .F. ) ;
#68038 = CARTESIAN_POINT ( 'NONE',  ( 11.04687750876899877, -4.617914354660699772, 6.541108991297599928 ) ) ;
#68039 = LINE ( 'NONE', #20155, #4134 ) ;
#68040 = CARTESIAN_POINT ( 'NONE',  ( 15.48701341325400094, 9.525963125313998248, 8.191611664426000416 ) ) ;
#68041 = CARTESIAN_POINT ( 'NONE',  ( 23.73953457051037930, 9.827638729800828088, 9.725490280229180939 ) ) ;
#68042 = AXIS2_PLACEMENT_3D ( 'NONE', #67907, #47631, #20364 ) ;
#68044 = FACE_OUTER_BOUND ( 'NONE', #20486, .T. ) ;
#68043 = CARTESIAN_POINT ( 'NONE',  ( 11.27110638630999873, 5.469603964121000139, 8.504707115835000053 ) ) ;
#68045 = CARTESIAN_POINT ( 'NONE',  ( 10.57564694612699974, 3.068007311611700150, -7.871941502982999772 ) ) ;
#68046 = ADVANCED_FACE ( 'NONE', ( #6872 ), #22076, .F. ) ;
#68047 = CARTESIAN_POINT ( 'NONE',  ( 12.80505043854146940, -3.174834474598374090, 12.21921104873077013 ) ) ;
#68048 = CARTESIAN_POINT ( 'NONE',  ( 10.21024205624999937, 3.689072563647699976, -8.309340504471899536 ) ) ;
#68049 = CARTESIAN_POINT ( 'NONE',  ( 18.20545956023470779, 0.3178346465811124899, 12.59599179195193663 ) ) ;
#68050 = CARTESIAN_POINT ( 'NONE',  ( 6.869746981740999736, 1.502678685822000038, 0.3990061803045000244 ) ) ;
#68051 = CARTESIAN_POINT ( 'NONE',  ( 11.80233327354039830, 2.898463260143000042, 8.220500279733599314 ) ) ;
#68052 = CARTESIAN_POINT ( 'NONE',  ( 23.55340455206400208, 10.33190633022999982, 9.496206588478999677 ) ) ;
#68053 = ORIENTED_EDGE ( 'NONE', *, *, #63516, .F. ) ;
#68054 = CARTESIAN_POINT ( 'NONE',  ( 8.732394353210001015, -2.806079842068999852, 8.615883328687999665 ) ) ;
#68055 = CARTESIAN_POINT ( 'NONE',  ( 4.000000000000000000, 1.878475312369307426, -1.082895748632574984 ) ) ;
#68056 = CARTESIAN_POINT ( 'NONE',  ( 7.811250121011001468, -4.190252858842606010, 6.133645552891420216 ) ) ;
#68057 = ORIENTED_EDGE ( 'NONE', *, *, #44809, .T. ) ;
#68058 = CARTESIAN_POINT ( 'NONE',  ( 18.38069952315600020, 3.381269036354999979, 12.09968217836000015 ) ) ;
#68059 = CARTESIAN_POINT ( 'NONE',  ( 11.18412378248529926, 3.450971646934100079, 8.538714411016998795 ) ) ;
#68060 = CARTESIAN_POINT ( 'NONE',  ( 10.28180471959000108, 3.991526675591000384, -5.814300410279999554 ) ) ;
#68061 = EDGE_LOOP ( 'NONE', ( #8847, #58804, #54168, #45238 ) ) ;
#68062 = LINE ( 'NONE', #57232, #41748 ) ;
#68063 = LINE ( 'NONE', #57233, #49886 ) ;
#68064 = CARTESIAN_POINT ( 'NONE',  ( 10.78887616594230003, 3.613544262574699850, 8.718182393403999697 ) ) ;
#68065 = CARTESIAN_POINT ( 'NONE',  ( 10.74600376124999990, -5.242711034443999552, 8.978690688221998784 ) ) ;
#68066 = DIRECTION ( 'NONE',  ( 0.9999999999999987788, -4.835300858369983927E-08, -1.472962857897996183E-08 ) ) ;
#68067 = VERTEX_POINT ( 'NONE', #18756 ) ;
#68068 = CARTESIAN_POINT ( 'NONE',  ( 7.861428251418627333, -5.109570395020106126, 6.686999168342897981 ) ) ;
#68069 = CARTESIAN_POINT ( 'NONE',  ( 4.000000000000000000, 0.000000000000000000, 0.000000000000000000 ) ) ;
#68070 = CARTESIAN_POINT ( 'NONE',  ( 8.214066216216412641, -5.709958105020243480, 7.828137529621371549 ) ) ;
#68071 = CARTESIAN_POINT ( 'NONE',  ( 9.195468108405998819, -2.901397043998999781, 7.188863445572599709 ) ) ;
#68072 = ORIENTED_EDGE ( 'NONE', *, *, #56098, .F. ) ;
#68073 = CARTESIAN_POINT ( 'NONE',  ( 2.792640132542833165, -3.058252359239901796, -1.762666431298149039 ) ) ;
#68074 = CARTESIAN_POINT ( 'NONE',  ( 10.69810941423799910, -3.053977294209000437, 8.359277272599898723 ) ) ;
#68075 = ORIENTED_EDGE ( 'NONE', *, *, #19973, .F. ) ;
#68076 = CARTESIAN_POINT ( 'NONE',  ( 9.496463691920835615, 5.100000000000000533, -6.665341197420965536 ) ) ;
#68077 = VERTEX_POINT ( 'NONE', #61398 ) ;
#68078 = EDGE_CURVE ( 'NONE', #53328, #7557, #57934, .T. ) ;
#68079 = EDGE_CURVE ( 'NONE', #8953, #60567, #19679, .T. ) ;
#68080 = DIRECTION ( 'NONE',  ( -1.000000000000000000, 0.000000000000000000, 0.000000000000000000 ) ) ;
#68081 = CARTESIAN_POINT ( 'NONE',  ( 10.61171207387999971, -2.821101057508000221, -4.761811341319999613 ) ) ;
#68082 = CARTESIAN_POINT ( 'NONE',  ( 11.43345123989529810, 4.540230239159599890, -8.543317325199000223 ) ) ;
#68083 = CARTESIAN_POINT ( 'NONE',  ( 11.80878751119029957, -5.041025164610000608, 6.955365841266999638 ) ) ;
#68084 = CARTESIAN_POINT ( 'NONE',  ( 12.20882029558151949, 2.312280790556523247, -12.49335225873939770 ) ) ;
#68085 = CARTESIAN_POINT ( 'NONE',  ( 10.80072469555900128, -3.429147315060100176, 8.487632181750699445 ) ) ;
#68086 = CARTESIAN_POINT ( 'NONE',  ( 8.271698341229999585, 5.629399530851999955, 8.631829656822000985 ) ) ;
#68087 = VERTEX_POINT ( 'NONE', #14875 ) ;
#68088 = VECTOR ( 'NONE', #4117, 1000.000000000000000 ) ;
#68089 = CARTESIAN_POINT ( 'NONE',  ( 3.500000000000000000, -2.946081722130999836, 0.9972449351501998516 ) ) ;
#68090 = CARTESIAN_POINT ( 'NONE',  ( 8.481683059623998489, -2.472358291268000219, 6.234202627038999189 ) ) ;
#68091 = LINE ( 'NONE', #35947, #37957 ) ;
#68092 = ORIENTED_EDGE ( 'NONE', *, *, #43046, .F. ) ;
#68093 = B_SPLINE_SURFACE_WITH_KNOTS ( 'NONE', 3, 3, ( 
 ( #19373, #24279, #2606, #56091 ),
 ( #13115, #34444, #50167, #65884 ),
 ( #49816, #51199, #35126, #44928 ),
 ( #18012, #50506, #61341, #61679 ),
 ( #67257, #66233, #39329, #34091 ) ),
 .UNSPECIFIED., .F., .F., .F.,
 ( 4, 1, 4 ),
 ( 4, 4 ),
 ( -0.006081020443020000374, 0.000000000000000000, 0.03678947617080999960 ),
 ( -0.1730217193418999988, 1.173021718456999984 ),
 .UNSPECIFIED. ) ;
#68094 = CARTESIAN_POINT ( 'NONE',  ( 12.75673482301077932, -1.762409409947525374, -12.47613375359912524 ) ) ;
#68095 = CARTESIAN_POINT ( 'NONE',  ( 11.28118179236249929, 3.732952383914999839, 8.749800764654999341 ) ) ;
#68096 = CARTESIAN_POINT ( 'NONE',  ( 11.00119435320999983, -4.640445114785999969, -9.059317673956000405 ) ) ;
#68097 = CARTESIAN_POINT ( 'NONE',  ( 10.06162737365999682, 9.774413574170004892, -6.274226718126997504 ) ) ;
#68098 = CARTESIAN_POINT ( 'NONE',  ( 2.446201642328499570, 2.726743374470192993, -2.246552915429936181 ) ) ;
#68099 = CARTESIAN_POINT ( 'NONE',  ( 10.68559687351635112, 5.092232985442825210, 8.129523725463618788 ) ) ;
#68100 = CARTESIAN_POINT ( 'NONE',  ( 12.27233953995990134, -2.172968329541576704, -13.73735571485410745 ) ) ;
#68101 = CARTESIAN_POINT ( 'NONE',  ( 10.92441504065829960, -3.305585767322499979, -6.982228367137699898 ) ) ;
#68102 = CARTESIAN_POINT ( 'NONE',  ( 10.49316089255587414, 4.959455279339148426, 8.606798394218628800 ) ) ;
#68103 = CARTESIAN_POINT ( 'NONE',  ( 11.57240408529958842, 3.267527001822357224, -7.017887023514778555 ) ) ;
#68104 = LINE ( 'NONE', #30053, #53430 ) ;
#68105 = VERTEX_POINT ( 'NONE', #19432 ) ;
#68106 = EDGE_CURVE ( 'NONE', #1011, #24471, #44585, .T. ) ;
#68107 = EDGE_LOOP ( 'NONE', ( #67616, #8764, #22379, #41965 ) ) ;
#68108 = DIRECTION ( 'NONE',  ( -1.000000000000000000, 0.000000000000000000, 0.000000000000000000 ) ) ;
#68109 = DIRECTION ( 'NONE',  ( 1.000000000000000000, 0.000000000000000000, 0.000000000000000000 ) ) ;
#68110 = CARTESIAN_POINT ( 'NONE',  ( 18.17514039568614237, 2.578830838032381223, 13.65637626280583561 ) ) ;
#68111 = EDGE_CURVE ( 'NONE', #26364, #49024, #66225, .T. ) ;
#68112 = CARTESIAN_POINT ( 'NONE',  ( 9.976690600124999975, 4.172224310749999887, -6.147156451669999910 ) ) ;
#68113 = FACE_BOUND ( 'NONE', #53075, .T. ) ;
#68114 = CARTESIAN_POINT ( 'NONE',  ( 17.88765289689606064, 3.029249243711964468, 12.31236272700674839 ) ) ;
#68115 = CARTESIAN_POINT ( 'NONE',  ( 23.61278986222799858, -13.29111433880999904, 4.056100357100000942 ) ) ;
#68116 = CARTESIAN_POINT ( 'NONE',  ( 9.571961069101000419, 4.084683332033999470, 8.946609345378000455 ) ) ;
#68117 = ORIENTED_EDGE ( 'NONE', *, *, #18312, .T. ) ;
#68118 = CARTESIAN_POINT ( 'NONE',  ( 8.767881343006999728, -4.605543323398999966, -6.293427432547999523 ) ) ;
#68119 = EDGE_LOOP ( 'NONE', ( #32470, #22900, #20738, #52899 ) ) ;
#68120 = CARTESIAN_POINT ( 'NONE',  ( 12.23541831425122872, -2.757387829712826033, 12.38789221355391312 ) ) ;
#68121 = CARTESIAN_POINT ( 'NONE',  ( 8.618968789468430813, 5.058209485103853709, -8.358329603623534609 ) ) ;
#68122 = CARTESIAN_POINT ( 'NONE',  ( 9.353724647487000610, 2.823567847429000022, 9.032053040610000139 ) ) ;
#68123 = CARTESIAN_POINT ( 'NONE',  ( 11.06080513895999928, -2.973119161490000106, 8.070849345005600028 ) ) ;
#68124 = CARTESIAN_POINT ( 'NONE',  ( 7.289711015751999312, -0.9708250560305000665, 0.5387387265405000347 ) ) ;
#68125 = CARTESIAN_POINT ( 'NONE',  ( 25.59994555223600088, 9.407310119913397273, 6.227539428019859713 ) ) ;
#68126 = CYLINDRICAL_SURFACE ( 'NONE', #53222, 1.350000000000000533 ) ;
#68127 = EDGE_CURVE ( 'NONE', #55894, #34052, #12867, .T. ) ;
#68128 = AXIS2_PLACEMENT_3D ( 'NONE', #30773, #26218, #36711 ) ;
#68129 = CARTESIAN_POINT ( 'NONE',  ( 12.42410782380136780, -0.4959072410923938690, 12.68697406334525368 ) ) ;
#68130 = CARTESIAN_POINT ( 'NONE',  ( 18.29983863916000075, -2.861762957209999847, 11.98830831200999825 ) ) ;
#68131 = CARTESIAN_POINT ( 'NONE',  ( 10.97534709859457003, 5.193992591246429313, -6.717726803886520770 ) ) ;
#68132 = CARTESIAN_POINT ( 'NONE',  ( 11.56631965465000178, -3.502676170607000206, 11.07146920481999963 ) ) ;
#68133 = ORIENTED_EDGE ( 'NONE', *, *, #59561, .T. ) ;
#68134 = CARTESIAN_POINT ( 'NONE',  ( 9.187479719595000205, 2.391443348526999912, -6.856688371964000162 ) ) ;
#68135 = CARTESIAN_POINT ( 'NONE',  ( -0.000000000000000000, -0.3800960799355100894, 2.900041633271500441 ) ) ;
#68136 = CARTESIAN_POINT ( 'NONE',  ( 5.500000000000000000, -13.87069231928999891, -4.225386915259999654 ) ) ;
#68137 = CARTESIAN_POINT ( 'NONE',  ( 12.79999999202000005, 11.41069016990000051, -4.623987642516999230 ) ) ;
#68138 = CARTESIAN_POINT ( 'NONE',  ( 12.09999999999999964, -3.011522968892934138, 8.147838400233645473 ) ) ;
#68139 = AXIS2_PLACEMENT_3D ( 'NONE', #37457, #26975, #44099 ) ;
#68140 = CARTESIAN_POINT ( 'NONE',  ( 11.38795122972049967, -3.601717549869600354, -6.578956058177199751 ) ) ;
#68141 = ORIENTED_EDGE ( 'NONE', *, *, #38569, .F. ) ;
#68142 = CARTESIAN_POINT ( 'NONE',  ( 2.063611650058999825, -0.2184777168079999887, 3.585542759708000293 ) ) ;
#68143 = CARTESIAN_POINT ( 'NONE',  ( 7.308885841229000313, 4.847807297114000491, 9.065373753110998578 ) ) ;
#68146 = CARTESIAN_POINT ( 'NONE',  ( 13.73899430609700190, -9.712898924749000074, -7.967785796560000300 ) ) ;
#68145 = CARTESIAN_POINT ( 'NONE',  ( 9.120514158775000269, 5.306366356490000769, -7.996450761531000317 ) ) ;
#68144 = PRODUCT_DEFINITION_CONTEXT ( 'detailed design', #28926, 'design' ) ;
#68147 = CARTESIAN_POINT ( 'NONE',  ( 15.89979320884932967, 8.154023814690251726, 9.295983641917246132 ) ) ;
#68148 = ORIENTED_EDGE ( 'NONE', *, *, #17808, .T. ) ;
#68149 = CARTESIAN_POINT ( 'NONE',  ( 18.18012160401611155, -2.482106737233723326, -13.67720576235794816 ) ) ;
#68150 = CARTESIAN_POINT ( 'NONE',  ( 11.17056785386839834, 3.281375110759499947, 7.016391833292499491 ) ) ;
#68151 = CARTESIAN_POINT ( 'NONE',  ( 24.51106630233162065, -11.97393966168535862, 3.208408158990909698 ) ) ;
#68152 = CARTESIAN_POINT ( 'NONE',  ( 8.721004440379999778, -5.983034890242000081, 7.440798487724999966 ) ) ;
#68153 = ORIENTED_EDGE ( 'NONE', *, *, #61702, .T. ) ;
#68154 = CARTESIAN_POINT ( 'NONE',  ( 9.646790723601728956, -5.267286625425933622, -8.036436072827047639 ) ) ;
#68156 = CARTESIAN_POINT ( 'NONE',  ( 11.02419555961999897, -2.407899345275000158, -8.439548421502999886 ) ) ;
#68155 = CARTESIAN_POINT ( 'NONE',  ( 11.08810207955139937, 3.203462856645999945, -7.174999999999999822 ) ) ;
#68157 = CARTESIAN_POINT ( 'NONE',  ( 7.479299064383798878, -2.376666221062909035, 6.873252664167585735 ) ) ;
#68158 = CARTESIAN_POINT ( 'NONE',  ( 7.000000000000000000, 0.8000000000000000444, -3.149999999999999911 ) ) ;
#68159 = CARTESIAN_POINT ( 'NONE',  ( 1.833838311998000181, 2.957881470139000157, 1.368292308076999975 ) ) ;
#68160 = ORIENTED_EDGE ( 'NONE', *, *, #29507, .T. ) ;
#68161 = LINE ( 'NONE', #36361, #12061 ) ;
#68162 = CARTESIAN_POINT ( 'NONE',  ( 10.90749413291699987, -3.211956830789300277, 7.859564368461399830 ) ) ;
#68163 = CARTESIAN_POINT ( 'NONE',  ( 10.52638970730999901, 2.451081172664000274, 6.282749363171999946 ) ) ;
#68164 = CARTESIAN_POINT ( 'NONE',  ( 10.74599736040000053, 5.242718773683000322, 8.978699897073999736 ) ) ;
#68165 = CARTESIAN_POINT ( 'NONE',  ( 10.62072335273219892, 4.397090433355999473, 6.430603299050000388 ) ) ;
#68166 = EDGE_CURVE ( 'NONE', #58906, #32433, #14478, .T. ) ;
#68167 = EDGE_CURVE ( 'NONE', #7389, #32586, #47731, .T. ) ;
#68168 = CARTESIAN_POINT ( 'NONE',  ( 23.80818223285949742, -3.306687018882327855, 13.11409922197318956 ) ) ;
#68169 = EDGE_CURVE ( 'NONE', #38774, #9042, #10247, .T. ) ;
#68170 = EDGE_CURVE ( 'NONE', #44713, #21934, #38608, .T. ) ;
#68171 = FACE_OUTER_BOUND ( 'NONE', #32509, .T. ) ;
#68172 = CARTESIAN_POINT ( 'NONE',  ( 11.35565467195930189, 2.863826994586553987, -6.911917091190551865 ) ) ;
#68173 = CARTESIAN_POINT ( 'NONE',  ( 11.09999999999999964, 2.700688487044999864, -5.124965750789000296 ) ) ;
#68174 = CARTESIAN_POINT ( 'NONE',  ( 18.06209397514829718, -1.995989992690351933, 13.85698731868970413 ) ) ;
#68175 = CYLINDRICAL_SURFACE ( 'NONE', #26062, 2.000000000000001332 ) ;
#68176 = VERTEX_POINT ( 'NONE', #15900 ) ;
#68177 = CARTESIAN_POINT ( 'NONE',  ( 16.09992084546400193, -8.991497430826001391, -8.719551690569000257 ) ) ;
#68178 = CARTESIAN_POINT ( 'NONE',  ( 9.171146261768624797, -3.287258916643901241, -6.460774852777244170 ) ) ;
#68179 = EDGE_LOOP ( 'NONE', ( #12176, #22457, #68075, #53468 ) ) ;
#68180 = FILL_AREA_STYLE ('',( #52106 ) ) ;
#68181 = AXIS2_PLACEMENT_3D ( 'NONE', #36316, #20237, #52042 ) ;
#68182 = CARTESIAN_POINT ( 'NONE',  ( 11.85979573085659844, 4.840012015667699785, 7.354650721737899133 ) ) ;
#68183 = CARTESIAN_POINT ( 'NONE',  ( 10.28314886242000092, 2.387776420306999992, 7.684265965147999644 ) ) ;
#68184 = CARTESIAN_POINT ( 'NONE',  ( 10.18512471524999974, 5.526143977810000329, -7.556025088797999167 ) ) ;
#68185 = CARTESIAN_POINT ( 'NONE',  ( 9.328216720588626387, -3.237060173287368503, -7.928316576537355331 ) ) ;
#68186 = CARTESIAN_POINT ( 'NONE',  ( 9.576494682405000347, -4.593972507100000158, 5.662052676321000177 ) ) ;
#68187 = CARTESIAN_POINT ( 'NONE',  ( 18.18883553772844763, 0.3494793053307434505, -12.59515668824706580 ) ) ;
#68188 = CARTESIAN_POINT ( 'NONE',  ( 12.60033281150904472, 3.091857377016624220, -12.29379371307818225 ) ) ;
#68189 = CARTESIAN_POINT ( 'NONE',  ( 11.67918044953561996, -2.988516238873000219, -8.027436060358800418 ) ) ;
#68190 = LINE ( 'NONE', #25557, #38911 ) ;
#68191 = ORIENTED_EDGE ( 'NONE', *, *, #44372, .T. ) ;
#68192 = LINE ( 'NONE', #26252, #21325 ) ;
#68193 = CARTESIAN_POINT ( 'NONE',  ( 25.44995096658100309, 2.258942858049999725, -12.29419282279000036 ) ) ;
#68194 = CARTESIAN_POINT ( 'NONE',  ( 10.18559687351583243, -2.907767014557174790, -6.870476274536379435 ) ) ;
#68195 = CARTESIAN_POINT ( 'NONE',  ( 7.156203327080998378, 10.79836147658999757, 3.492272478327004492 ) ) ;
#68196 = CARTESIAN_POINT ( 'NONE',  ( 12.36102515544322600, 1.940652449090402021, 13.86484480881333070 ) ) ;
#68197 = CARTESIAN_POINT ( 'NONE',  ( 10.85738557828999973, -2.754556666341999804, 8.976367391363998749 ) ) ;
#68198 = CARTESIAN_POINT ( 'NONE',  ( 24.30000000000000071, 0.000000000000000000, 0.000000000000000000 ) ) ;
#68199 = CARTESIAN_POINT ( 'NONE',  ( 12.15449479986287251, -0.3231860383015694449, 13.99628497142876249 ) ) ;
#68200 = VERTEX_POINT ( 'NONE', #17282 ) ;
#68201 = CARTESIAN_POINT ( 'NONE',  ( 12.70926349491446672, -1.766754859226808305, 12.47551934520473260 ) ) ;
#68202 = LINE ( 'NONE', #36757, #38200 ) ;
#68203 = CARTESIAN_POINT ( 'NONE',  ( 10.55991645936999923, -5.094263939633999705, 6.075409946530999861 ) ) ;
#68204 = CARTESIAN_POINT ( 'NONE',  ( 15.44552286930765383, 9.471974105402711785, 8.194957690431849073 ) ) ;
#68205 = CARTESIAN_POINT ( 'NONE',  ( 11.12903166480609940, -4.864052766304100217, 7.439078678739090122 ) ) ;
#68206 = EDGE_CURVE ( 'NONE', #48764, #38102, #51121, .T. ) ;
#68207 = CARTESIAN_POINT ( 'NONE',  ( 8.719369705998316178, 4.353260231620209808, -8.814526689006324744 ) ) ;
#68208 = LINE ( 'NONE', #46906, #45482 ) ;
#68209 = DIRECTION ( 'NONE',  ( 0.000000000000000000, -0.6482718649732923666, 0.7614089499631913061 ) ) ;
#68210 = EDGE_CURVE ( 'NONE', #66543, #2854, #32000, .T. ) ;
#68211 = CARTESIAN_POINT ( 'NONE',  ( 12.32336322858527744, 1.942450600934330085, 12.44937554728605100 ) ) ;
#68212 = CARTESIAN_POINT ( 'NONE',  ( 9.353311703536000721, -4.905858243509999106, -8.948175900338000588 ) ) ;
#68213 = AXIS2_PLACEMENT_3D ( 'NONE', #40637, #56386, #3573 ) ;
#68214 = CARTESIAN_POINT ( 'NONE',  ( 10.21462282008599942, 4.523146351753199568, -8.343818446627699004 ) ) ;
#68215 = LINE ( 'NONE', #41323, #42533 ) ;
#68216 = CARTESIAN_POINT ( 'NONE',  ( 9.926176658771000305, 4.356412802752999802, -9.313960415320000408 ) ) ;
#68217 = CARTESIAN_POINT ( 'NONE',  ( 8.744113844317999096, 4.323050436788100193, -6.262250912840999106 ) ) ;
#68219 = CARTESIAN_POINT ( 'NONE',  ( 12.30490414476351013, 2.123060221900641587, 12.53148904350137016 ) ) ;
#68218 = DIRECTION ( 'NONE',  ( 4.468466013035040012E-09, -0.9867386997955089889, -0.1623167838699015042 ) ) ;
#68220 = CARTESIAN_POINT ( 'NONE',  ( 11.29998636608000062, -3.695122995756999984, 11.25914041192000070 ) ) ;
#68221 = ORIENTED_EDGE ( 'NONE', *, *, #17175, .F. ) ;
#68222 = B_SPLINE_CURVE_WITH_KNOTS ( 'NONE', 3,
 ( #33208, #43699, #64995, #59767, #54526, #6628, #61497, #62174, #24093, #45426, #13274, #29016, #34938, #7669, #14297, #40509, #44743, #35625 ),
 .UNSPECIFIED., .F., .F.,
 ( 4, 2, 2, 2, 2, 2, 2, 2, 4 ),
 ( 0.000000000000000000, 0.1249999999999996669, 0.2499999999999993339, 0.3749999999999990008, 0.4999999999999986677, 0.6249999999999990008, 0.7499999999999993339, 0.8749999999999996669, 1.000000000000000000 ),
 .UNSPECIFIED. ) ;
#68223 = CARTESIAN_POINT ( 'NONE',  ( 12.43800415128889725, -0.5060493095660281160, 12.68643001347753518 ) ) ;
#68224 = CARTESIAN_POINT ( 'NONE',  ( 11.59999999999999964, 5.386831235742000068, -7.174999999999999822 ) ) ;
#68225 = CARTESIAN_POINT ( 'NONE',  ( 9.644299024500105233, 2.624632560452479169, -6.377853817079278897 ) ) ;
#68226 = CARTESIAN_POINT ( 'NONE',  ( 9.123101285863999266, 3.353260484332500013, 8.268485718282699182 ) ) ;
#68227 = CARTESIAN_POINT ( 'NONE',  ( 8.757986382567201744, 4.151567127026601689, -8.349715092260979077 ) ) ;
#68228 = CIRCLE ( 'NONE', #31421, 0.4999999999999997224 ) ;
#68229 = CARTESIAN_POINT ( 'NONE',  ( 23.58134502776777097, -3.140546043133733978, -13.62725458207014917 ) ) ;
#68230 = CARTESIAN_POINT ( 'NONE',  ( 12.72264977853956580, -3.119885623323980894, 13.52225790872755873 ) ) ;
#68231 = CARTESIAN_POINT ( 'NONE',  ( 13.00000000001300116, -11.52577654661000039, -1.696746661728000038 ) ) ;
#68232 = CARTESIAN_POINT ( 'NONE',  ( 8.156123186758179600, 2.990802688239547535, 6.388664891360845033 ) ) ;
#68233 = EDGE_LOOP ( 'NONE', ( #16979, #25690, #61423, #63495 ) ) ;
#68234 = CARTESIAN_POINT ( 'NONE',  ( 5.208516125328000790, -0.1340246339512000118, 1.126467857079999968 ) ) ;
#68235 = CARTESIAN_POINT ( 'NONE',  ( 9.934583761885999564, -5.078750111091999919, -8.187519150726398465 ) ) ;
#68236 = LINE ( 'NONE', #2898, #35451 ) ;
#68237 = CARTESIAN_POINT ( 'NONE',  ( 11.89700581613019992, -3.130347327833300053, 6.941573685175900010 ) ) ;
#68238 = CARTESIAN_POINT ( 'NONE',  ( 17.91266776300914643, 3.012678901972745571, -12.31722829471395997 ) ) ;
#68239 = CARTESIAN_POINT ( 'NONE',  ( 11.04420485398999929, -2.755310155137999484, 5.177028922958999857 ) ) ;
#68240 = CARTESIAN_POINT ( 'NONE',  ( 18.04518119037968660, 2.887943935962514086, 12.35267345330769473 ) ) ;
#68241 = ADVANCED_FACE ( 'NONE', ( #16244 ), #67668, .F. ) ;
#68242 = CARTESIAN_POINT ( 'NONE',  ( 12.64149076269671923, 3.109019952263742947, -13.52530492583441024 ) ) ;
#68243 = CARTESIAN_POINT ( 'NONE',  ( 9.355894592352999695, -5.864995026133001055, -7.324074232821000230 ) ) ;
#68244 = CARTESIAN_POINT ( 'NONE',  ( 10.22908305962000064, -4.838492992840000007, -5.852445959518000507 ) ) ;
#68245 = CARTESIAN_POINT ( 'NONE',  ( 11.59999999999999964, 5.250000000000000000, -7.500000000000000000 ) ) ;
#68246 = ADVANCED_FACE ( 'NONE', ( #170 ), #23010, .F. ) ;
#68247 = CARTESIAN_POINT ( 'NONE',  ( 10.95037914754042419, -5.141203310087995249, -5.102208348236233704 ) ) ;
#68248 = ADVANCED_FACE ( 'NONE', ( #49096 ), #33373, .T. ) ;
#68249 = CARTESIAN_POINT ( 'NONE',  ( 5.100000004521000108, 0.8000000000000000444, 3.149999999999999911 ) ) ;
#68250 = CARTESIAN_POINT ( 'NONE',  ( 11.09999999999999964, 7.281355457699000056, 6.286510842043999681 ) ) ;
#68251 = CARTESIAN_POINT ( 'NONE',  ( 17.72046959774372965, 1.875000000000000444, 12.57541560742027364 ) ) ;
#68252 = ORIENTED_EDGE ( 'NONE', *, *, #34615, .F. ) ;
#68253 = CARTESIAN_POINT ( 'NONE',  ( 9.152520280414000453, 4.102804347295999854, -5.770625657082999460 ) ) ;
#68254 = CARTESIAN_POINT ( 'NONE',  ( 12.28179573085659904, -3.026866171144600326, 7.331616337578100051 ) ) ;
#68255 = ORIENTED_EDGE ( 'NONE', *, *, #21052, .F. ) ;
#68256 = CARTESIAN_POINT ( 'NONE',  ( -15.86200481174999943, -2.399999999999999911, 6.571291218949999902 ) ) ;
#68257 = CARTESIAN_POINT ( 'NONE',  ( 17.94049251029957048, 1.899108762321197963, -13.87060088084272813 ) ) ;
#68258 = ORIENTED_EDGE ( 'NONE', *, *, #6207, .T. ) ;
#68259 = CARTESIAN_POINT ( 'NONE',  ( 11.51656039236534923, 5.173498198882000132, 7.442888368925779652 ) ) ;
#68260 = CARTESIAN_POINT ( 'NONE',  ( 8.414360841228999632, 5.461114003844000031, -8.582501063019000398 ) ) ;
#68261 = CARTESIAN_POINT ( 'NONE',  ( 18.06247470497382324, 3.164801830445714614, -11.41978211466257243 ) ) ;
#68262 = CARTESIAN_POINT ( 'NONE',  ( 11.40211496860029783, -3.206052520092899982, -7.093139000852099585 ) ) ;
#68263 = DIRECTION ( 'NONE',  ( 0.000000000000000000, 1.000000000000000000, 0.000000000000000000 ) ) ;
#68264 = DIRECTION ( 'NONE',  ( 0.000000000000000000, 1.000000000000000000, 0.000000000000000000 ) ) ;
#68265 = EDGE_LOOP ( 'NONE', ( #47344, #10102, #43094, #27167 ) ) ;
#68266 = CARTESIAN_POINT ( 'NONE',  ( 43.76123417800000226, -11.06886219213000011, 1.536526853569999851 ) ) ;
#68267 =( BOUNDED_CURVE ( )  B_SPLINE_CURVE ( 3, ( #5048, #52600, #48049, #57494, #9602, #30944, #52261 ),
 .UNSPECIFIED., .F., .T. ) 
 B_SPLINE_CURVE_WITH_KNOTS ( ( 4, 1, 1, 1, 4 ),
 ( 0.000000000000000000, 0.1584901274852722752, 0.4217256158758324047, 0.6948883626783448619, 1.000000000000000000 ),
 .UNSPECIFIED. ) 
 CURVE ( )  GEOMETRIC_REPRESENTATION_ITEM ( )  RATIONAL_B_SPLINE_CURVE ( ( 1.171572587279782862, 1.171572587279782862, 1.171572587279782862, 1.171572587279782862, 1.171572587279782862, 1.171572587279782862, 1.171572587279782862 ) ) 
 REPRESENTATION_ITEM ( '' )  );
#68268 = CARTESIAN_POINT ( 'NONE',  ( 9.278070280414000948, 2.546924812613000189, -6.918870225297999887 ) ) ;
#68269 = VERTEX_POINT ( 'NONE', #63790 ) ;
#68270 = EDGE_CURVE ( 'NONE', #37115, #17632, #63616, .T. ) ;
#68271 = CARTESIAN_POINT ( 'NONE',  ( 9.831594052344000190, 3.539229510464000139, -8.956011942092999334 ) ) ;
#68272 =( NAMED_UNIT ( * ) SI_UNIT ( $, .STERADIAN. ) SOLID_ANGLE_UNIT ( ) );
#68273 = ORIENTED_EDGE ( 'NONE', *, *, #15665, .T. ) ;
#68274 = CARTESIAN_POINT ( 'NONE',  ( 9.554646554150998838, 4.619310611972400338, 6.380697202105999999 ) ) ;
#68275 = CARTESIAN_POINT ( 'NONE',  ( 18.11779302252799440, -2.227307244339886250, -12.51093773244153873 ) ) ;
#68276 = CARTESIAN_POINT ( 'NONE',  ( 16.32020863168370894, 3.595521563589540559, 11.99782687963361205 ) ) ;
#68277 = B_SPLINE_CURVE_WITH_KNOTS ( 'NONE', 3,
 ( #58013, #63238, #31111, #10450 ),
 .UNSPECIFIED., .F., .F.,
 ( 4, 4 ),
 ( 0.000000000000000000, 1.000000000000000000 ),
 .UNSPECIFIED. ) ;
#68278 = CIRCLE ( 'NONE', #1168, 0.5000000000000004441 ) ;
#68279 = CARTESIAN_POINT ( 'NONE',  ( 18.16429560770317408, -2.358968865818011018, -12.48332026670070860 ) ) ;
#68280 = CARTESIAN_POINT ( 'NONE',  ( 11.71253483539785734, -4.338990010211682069, 6.691360637068767936 ) ) ;
#68281 = VERTEX_POINT ( 'NONE', #65161 ) ;
#68282 = CARTESIAN_POINT ( 'NONE',  ( 12.13642952379600004, 11.66478987891999886, -3.865847705614000152 ) ) ;
#68283 = CARTESIAN_POINT ( 'NONE',  ( 7.325000000000000178, 4.000000000000000000, 9.239711431703000244 ) ) ;
#68284 = CARTESIAN_POINT ( 'NONE',  ( 11.07184579812000003, -5.268087732220000596, -5.079906681876000363 ) ) ;
#68285 = CARTESIAN_POINT ( 'NONE',  ( 8.810863317747999801, 4.960863370448500120, 7.499999999926881600 ) ) ;
#68286 = CARTESIAN_POINT ( 'NONE',  ( 17.60274960888721552, 0.7290235424212095916, 13.98100605002522734 ) ) ;
#68287 = CARTESIAN_POINT ( 'NONE',  ( 18.16715644869600155, 3.024463723863999753, 11.49930835314999911 ) ) ;
#68288 = CIRCLE ( 'NONE', #33683, 2.750000000000000000 ) ;
#68289 = CARTESIAN_POINT ( 'NONE',  ( 9.701728707608999969, -4.253751259212999791, -8.839942087209999855 ) ) ;
#68290 = ORIENTED_EDGE ( 'NONE', *, *, #8279, .F. ) ;
#68291 = ORIENTED_EDGE ( 'NONE', *, *, #37341, .F. ) ;
#68292 = CARTESIAN_POINT ( 'NONE',  ( 10.12339528040999959, 3.988943694240999704, -8.966360307350999648 ) ) ;
#68293 = EDGE_CURVE ( 'NONE', #49843, #64580, #23627, .T. ) ;
#68294 = CARTESIAN_POINT ( 'NONE',  ( 11.59999999999999964, -4.000000000000000000, -7.500000000000000000 ) ) ;
#68295 = CARTESIAN_POINT ( 'NONE',  ( 8.470944094208999076, 5.100000000000000533, 6.571291218949999902 ) ) ;
#68296 = CARTESIAN_POINT ( 'NONE',  ( 24.14324463483463390, 3.327227329398946942, 12.48606449362839754 ) ) ;
#68297 = CARTESIAN_POINT ( 'NONE',  ( 10.72191429142990060, 4.025072603369280522, -6.183971186511000084 ) ) ;
#68298 = CARTESIAN_POINT ( 'NONE',  ( 10.01660887879199890, 3.803658216258800184, -6.655513263298900029 ) ) ;
#68300 = CARTESIAN_POINT ( 'NONE',  ( 7.883148997456999929, -5.167567567567999731, 6.822293592207000934 ) ) ;
#68299 = CARTESIAN_POINT ( 'NONE',  ( 9.473138961223998677, -3.053949131563199693, 6.860686042446299204 ) ) ;
#68301 = CARTESIAN_POINT ( 'NONE',  ( 7.426677373658002956, -3.232655724474999381, 6.473459691208998557 ) ) ;
#68302 = ORIENTED_EDGE ( 'NONE', *, *, #26833, .T. ) ;
#68303 = B_SPLINE_CURVE_WITH_KNOTS ( 'NONE', 3,
 ( #33945, #5975, #44786, #59463, #64699, #17515, #11914, #17867, #22053, #33254, #38136, #11226, #32562, #16810, #11560, #54917, #32904, #1089, #33599, #22403, #7361, #6316, #49318, #39182, #7020, #2129, #28355, #23449, #22747, #49671, #50021, #1779 ),
 .UNSPECIFIED., .F., .F.,
 ( 4, 2, 2, 2, 2, 2, 2, 2, 1, 2, 2, 2, 1, 1, 1, 2, 2, 4 ),
 ( 0.000000000000000000, 0.2500000000000237033, 0.3750000000000346945, 0.4375000000000415779, 0.4687500000000449085, 0.5000000000000481837, 0.6250000000000585088, 0.6875000000000665024, 0.7187500000000688338, 0.7343750000000688338, 0.7500000000000688338, 0.8125000000000668354, 0.8437500000000682787, 0.8593750000000691669, 0.8671875000000695000, 0.8710937500000708322, 0.8750000000000721645, 1.000000000000000000 ),
 .UNSPECIFIED. ) ;
#68304 = CARTESIAN_POINT ( 'NONE',  ( 0.1499942179679999987, 2.750000000000000000, 0.000000000000000000 ) ) ;
#68305 = CARTESIAN_POINT ( 'NONE',  ( 18.90826270587400160, 0.000000000000000000, 0.000000000000000000 ) ) ;
#68306 = CARTESIAN_POINT ( 'NONE',  ( 9.735025935145998233, 3.814256956409300070, 8.765655525501999890 ) ) ;
#68307 = CARTESIAN_POINT ( 'NONE',  ( 4.599999999999999645, 3.125000000000000000, 13.52078605991414939 ) ) ;
#68308 = DIRECTION ( 'NONE',  ( 0.000000000000000000, -1.000000000000000000, 0.000000000000000000 ) ) ;
#68309 = CARTESIAN_POINT ( 'NONE',  ( 9.856463691916330205, -5.100000000000000533, 6.665341197412375962 ) ) ;
#68310 = CARTESIAN_POINT ( 'NONE',  ( 9.044210841233001119, 2.773858540272000184, -8.951250717848999727 ) ) ;
#68311 = CARTESIAN_POINT ( 'NONE',  ( 14.02348875342600110, 8.812421938351000961, 7.562304860556999131 ) ) ;
#68312 = CARTESIAN_POINT ( 'NONE',  ( 7.612571400991003046, -4.588494467460999537, 6.486759529251004075 ) ) ;
#68313 = VECTOR ( 'NONE', #29609, 1000.000000000000000 ) ;
#68314 = CARTESIAN_POINT ( 'NONE',  ( 10.87668353155522638, -2.650012393097451291, -7.302148410131374945 ) ) ;
#68315 = CARTESIAN_POINT ( 'NONE',  ( 11.58126742035590695, -4.768619073576777723, 7.893373809886144343 ) ) ;
#68316 = CARTESIAN_POINT ( 'NONE',  ( 8.736413463905998711, 4.084156314540369870, -8.382409559052598880 ) ) ;
#68317 = CARTESIAN_POINT ( 'NONE',  ( 9.865041550948095761, 2.650034642413356512, -7.500002425457249267 ) ) ;
#68318 = ORIENTED_EDGE ( 'NONE', *, *, #23600, .F. ) ;
#68319 = CARTESIAN_POINT ( 'NONE',  ( 12.50079267818768258, 0.5460377805369034387, -12.68419612078312042 ) ) ;
#68320 = CARTESIAN_POINT ( 'NONE',  ( 12.25843860534618202, -2.803243370077761476, -12.37572767902445925 ) ) ;
#68321 = CARTESIAN_POINT ( 'NONE',  ( 11.09999999999999964, 5.599999999999999645, -6.571291218949999902 ) ) ;
#68322 = DIRECTION ( 'NONE',  ( -1.000000000000000000, 0.000000000000000000, 0.000000000000000000 ) ) ;
#68323 = CARTESIAN_POINT ( 'NONE',  ( 1.603056799207541738, 2.798833948393625981, 2.150913519912208471 ) ) ;
#68324 = VERTEX_POINT ( 'NONE', #48755 ) ;
#68325 = PLANE ( 'NONE',  #44461 ) ;
#68326 = EDGE_CURVE ( 'NONE', #59469, #51368, #39792, .T. ) ;
#68327 = PRODUCT_CONTEXT ( 'NONE', #50760, 'mechanical' ) ;
#68328 = EDGE_CURVE ( 'NONE', #20140, #40405, #26976, .T. ) ;
#68329 = CARTESIAN_POINT ( 'NONE',  ( 10.98611853005698968, 8.045559802946883110, 6.520188272055316148 ) ) ;
#68330 = CARTESIAN_POINT ( 'NONE',  ( 13.55296092448800138, -11.54193659611999934, -2.433871908353000268 ) ) ;
#68331 = CARTESIAN_POINT ( 'NONE',  ( 10.72510394928502286, 2.650147065043140238, 7.500007457243191844 ) ) ;
#68332 = CARTESIAN_POINT ( 'NONE',  ( 11.55811496860034815, 5.045590851977999947, -6.964183526617899744 ) ) ;
#68333 = ORIENTED_EDGE ( 'NONE', *, *, #66317, .T. ) ;
#68334 = CARTESIAN_POINT ( 'NONE',  ( 10.39106278671000005, -4.025320977579999848, 9.261121875182000807 ) ) ;
#68335 = ORIENTED_EDGE ( 'NONE', *, *, #10835, .T. ) ;
#68336 = CARTESIAN_POINT ( 'NONE',  ( 9.525000000000000355, 4.417172942406000224, 8.783926296998000538 ) ) ;
#68337 = CARTESIAN_POINT ( 'NONE',  ( 8.893206853209999707, -3.977267280662000193, 9.308921106447000327 ) ) ;
#68338 = CIRCLE ( 'NONE', #53831, 1.049999999999999822 ) ;
#68339 = CARTESIAN_POINT ( 'NONE',  ( 16.13573769406199787, 8.400696156758000299, 8.016340154447000543 ) ) ;
#68340 = ORIENTED_EDGE ( 'NONE', *, *, #11422, .T. ) ;
#68341 = CARTESIAN_POINT ( 'NONE',  ( 16.39999999485600313, 3.595156957901000094, 11.99794989424000136 ) ) ;
#68342 = DIRECTION ( 'NONE',  ( 0.000000000000000000, 0.6460229165592984435, -0.7633180145130977756 ) ) ;
#68343 = CARTESIAN_POINT ( 'NONE',  ( 7.192714158770000310, 4.413443707129999893, -8.834960942136000028 ) ) ;
#68344 = LINE ( 'NONE', #42824, #40931 ) ;
#68345 = DIRECTION ( 'NONE',  ( -1.000000000000000000, -2.360367262211999706E-11, -1.096475580870000113E-09 ) ) ;
#68346 = ORIENTED_EDGE ( 'NONE', *, *, #54778, .F. ) ;
#68347 = CARTESIAN_POINT ( 'NONE',  ( 10.31167756636999933, -2.874479384703000129, 8.900026329558999194 ) ) ;
#68348 = CARTESIAN_POINT ( 'NONE',  ( 12.19231142703039339, -2.623190749633721897, -13.64650702417935157 ) ) ;
#68349 = DIRECTION ( 'NONE',  ( 1.000000000000000000, 0.000000000000000000, 0.000000000000000000 ) ) ;
#68350 = ORIENTED_EDGE ( 'NONE', *, *, #57375, .F. ) ;
#68351 = EDGE_CURVE ( 'NONE', #44271, #37125, #22750, .T. ) ;
#68352 = CARTESIAN_POINT ( 'NONE',  ( 29.91622776601699840, 0.000000000000000000, 0.000000000000000000 ) ) ;
#68353 = CARTESIAN_POINT ( 'NONE',  ( 10.90000000000000036, -5.100000000000000533, -6.436740704805999691 ) ) ;
#68354 = ORIENTED_EDGE ( 'NONE', *, *, #21180, .T. ) ;
#68355 = CARTESIAN_POINT ( 'NONE',  ( 23.59536289310526413, -10.17255618909020498, 9.586547987916594238 ) ) ;
#68356 = CARTESIAN_POINT ( 'NONE',  ( 10.93388704970945824, 2.287708072853963159, 7.858003405079239556 ) ) ;
#68357 = EDGE_CURVE ( 'NONE', #67055, #60176, #1094, .T. ) ;
#68358 = CARTESIAN_POINT ( 'NONE',  ( 11.30000000000000071, -6.616929226765999876E-14, -1.143529715363999905E-14 ) ) ;
#68359 = CARTESIAN_POINT ( 'NONE',  ( 10.16052890781999984, 2.899999999999999911, -6.152188490330000370 ) ) ;
#68360 = PLANE ( 'NONE',  #37504 ) ;
#68361 = DIRECTION ( 'NONE',  ( 0.7071067617951957152, 0.000000000000000000, -0.7071068005778986532 ) ) ;
#68362 = B_SPLINE_CURVE_WITH_KNOTS ( 'NONE', 3,
 ( #1270, #38676, #27496, #49504, #59997 ),
 .UNSPECIFIED., .F., .F.,
 ( 4, 1, 4 ),
 ( 0.000000000000000000, 0.5000000000000000000, 1.000000000000000000 ),
 .UNSPECIFIED. ) ;
#68363 = CARTESIAN_POINT ( 'NONE',  ( 9.560596873515667227, -3.370476274536376771, -8.592232985442823434 ) ) ;
#68364 = CARTESIAN_POINT ( 'NONE',  ( 10.01532628870999986, -4.946995631616999844, 8.559221361189001342 ) ) ;
#68365 = ORIENTED_EDGE ( 'NONE', *, *, #18959, .T. ) ;
#68366 = CARTESIAN_POINT ( 'NONE',  ( 7.780759508074995168, -4.599947829706001912, 6.384407252255998699 ) ) ;
#68367 = ORIENTED_EDGE ( 'NONE', *, *, #4218, .F. ) ;
#68368 = CARTESIAN_POINT ( 'NONE',  ( 9.632179190069999564, 5.638172764974000550, 6.476627236431999890 ) ) ;
#68369 = CARTESIAN_POINT ( 'NONE',  ( 10.99845801742999996, -5.289427263538000190, 4.962451247354000117 ) ) ;
#68370 = CARTESIAN_POINT ( 'NONE',  ( 9.567560841232999991, 5.349936549139000519, -7.138437102151999447 ) ) ;
#68371 = CARTESIAN_POINT ( 'NONE',  ( 3.390171590515999700, 3.025066006789999928, -1.845780140648000112 ) ) ;
#68372 = CARTESIAN_POINT ( 'NONE',  ( 25.59994555223600088, -9.407310119913413260, -6.227539428019629675 ) ) ;
#68373 = CYLINDRICAL_SURFACE ( 'NONE', #65174, 0.4999999999999998335 ) ;
#68374 = CARTESIAN_POINT ( 'NONE',  ( 18.02801947735587618, 0.4085868565813729480, 13.89191718360218353 ) ) ;
#68375 = ORIENTED_EDGE ( 'NONE', *, *, #68827, .F. ) ;
#68376 = CARTESIAN_POINT ( 'NONE',  ( 12.80505043854144276, 0.6249999999999994449, 13.88107975066923316 ) ) ;
#68377 = CARTESIAN_POINT ( 'NONE',  ( 11.16579975933730040, -2.791514215189000225, 7.915786590091300035 ) ) ;
#68378 = CARTESIAN_POINT ( 'NONE',  ( 10.57907406728876865, 2.241676822008003889, -7.748197378945968161 ) ) ;
#68379 = DIRECTION ( 'NONE',  ( 0.000000000000000000, 0.4739929102870218958, -0.8805286599524397850 ) ) ;
#68380 = CARTESIAN_POINT ( 'NONE',  ( 7.320269353207000229, -2.466384407480000096, 6.935560677555000275 ) ) ;
#68382 = CARTESIAN_POINT ( 'NONE',  ( 12.07940096941472241, 2.330761819168849502, -13.80597083265678826 ) ) ;
#68381 = CARTESIAN_POINT ( 'NONE',  ( 10.50285691784999997, 5.158890929072000198, 8.369954994793999958 ) ) ;
#68383 = VECTOR ( 'NONE', #57849, 1000.000000000000000 ) ;
#68384 = CARTESIAN_POINT ( 'NONE',  ( 11.30579707368350029, 3.365167912142600137, -6.390809033205999690 ) ) ;
#68385 = CARTESIAN_POINT ( 'NONE',  ( 11.25740844561608611, -2.954218652640771214, -7.175000373111195984 ) ) ;
#68386 = CARTESIAN_POINT ( 'NONE',  ( 10.31155864497999808, 4.682585200569199912, -8.034587760591801242 ) ) ;
#68387 = CARTESIAN_POINT ( 'NONE',  ( 18.22055608408778937, 0.2856017019952105662, 12.59676745213710625 ) ) ;
#68388 = CARTESIAN_POINT ( 'NONE',  ( 7.114743061344000807, -0.9896579195269999962, 1.009884616012000080 ) ) ;
#68389 = CARTESIAN_POINT ( 'NONE',  ( 11.09590547754519996, 5.315605332491999846, 7.458246194669389872 ) ) ;
#68390 = CARTESIAN_POINT ( 'NONE',  ( 9.298455008774132224, -3.051544939223430397, 7.263673592043552674 ) ) ;
#68391 = ORIENTED_EDGE ( 'NONE', *, *, #23539, .F. ) ;
#68392 = CARTESIAN_POINT ( 'NONE',  ( 8.989144353209001181, -5.284133759825000887, 6.489273023403000273 ) ) ;
#68393 = CARTESIAN_POINT ( 'NONE',  ( 18.10159474502872357, 2.998280829653924506, 13.67518427740799680 ) ) ;
#68394 = CARTESIAN_POINT ( 'NONE',  ( 6.899999438051000133, 0.5526611926744998682, 1.394476821647000042 ) ) ;
#68395 = ORIENTED_EDGE ( 'NONE', *, *, #52164, .T. ) ;
#68396 = CARTESIAN_POINT ( 'NONE',  ( 0.07426626274182999976, -1.906427021235999941, -2.406055758466000061 ) ) ;
#68397 = CARTESIAN_POINT ( 'NONE',  ( 11.43345123989529810, 4.540230239159599890, 6.456682674800999777 ) ) ;
#68398 = CARTESIAN_POINT ( 'NONE',  ( 10.43325471958999984, 5.596203146559000530, -8.042024377770999877 ) ) ;
#68399 = ORIENTED_EDGE ( 'NONE', *, *, #14023, .F. ) ;
#68400 = CARTESIAN_POINT ( 'NONE',  ( 9.279336721442293268, 3.836368765436817263, -6.250006800841096499 ) ) ;
#68401 = CARTESIAN_POINT ( 'NONE',  ( 8.620740978634000129, 4.599999999999999645, 5.898823289756999877 ) ) ;
#68402 = CARTESIAN_POINT ( 'NONE',  ( 10.20226357027499908, 5.120085139777000194, 7.283900408233900059 ) ) ;
#68403 = CARTESIAN_POINT ( 'NONE',  ( 10.52324012719000024, -3.325647021086999722, 5.689999163383999026 ) ) ;
#68404 = CARTESIAN_POINT ( 'NONE',  ( 7.308885841229000313, 4.847807297114000491, 9.065373753110998578 ) ) ;
#68405 = ORIENTED_EDGE ( 'NONE', *, *, #37473, .F. ) ;
#68406 = CARTESIAN_POINT ( 'NONE',  ( 8.724024145839393896, 3.782477278638352036, 6.654559194835224289 ) ) ;
#68407 = EDGE_CURVE ( 'NONE', #31626, #37115, #46175, .T. ) ;
#68408 = EDGE_CURVE ( 'NONE', #60390, #51100, #12739, .T. ) ;
#68409 = CARTESIAN_POINT ( 'NONE',  ( 8.213314158768998396, 4.511685119297999869, -5.670317910541000650 ) ) ;
#68410 = CARTESIAN_POINT ( 'NONE',  ( 8.287884602529770106, -4.765396756871579598, 9.061745085214184314 ) ) ;
#68411 = CARTESIAN_POINT ( 'NONE',  ( 9.877342523874999003, -5.264483068122999931, 7.693563834190999984 ) ) ;
#68412 = VERTEX_POINT ( 'NONE', #50828 ) ;
#68414 = CARTESIAN_POINT ( 'NONE',  ( 16.00261247405899923, -3.453035413593999792, -11.78892418867000025 ) ) ;
#68413 = AXIS2_PLACEMENT_3D ( 'NONE', #48120, #49151, #6498 ) ;
#68415 = CARTESIAN_POINT ( 'NONE',  ( 7.102397164862999546, -0.2464401224313000349, -3.049949836518000001 ) ) ;
#68416 = VERTEX_POINT ( 'NONE', #2924 ) ;
#68417 = CARTESIAN_POINT ( 'NONE',  ( 9.523148997461001741, 5.167567567567999731, -6.822293592207000934 ) ) ;
#68418 = CYLINDRICAL_SURFACE ( 'NONE', #12266, 1.250000000000000000 ) ;
#68419 = VERTEX_POINT ( 'NONE', #13771 ) ;
#68420 = AXIS2_PLACEMENT_3D ( 'NONE', #18628, #44171, #66165 ) ;
#68421 = CARTESIAN_POINT ( 'NONE',  ( 18.08617702649035763, 0.3300666952397346421, -13.89473968862477449 ) ) ;
#68422 = CARTESIAN_POINT ( 'NONE',  ( 9.402304893999998470, -4.531444417037000072, -6.133284059228000018 ) ) ;
#68423 = CARTESIAN_POINT ( 'NONE',  ( 10.42499241036559532, -5.349775919985432004, 7.500001834605715345 ) ) ;
#68424 = CARTESIAN_POINT ( 'NONE',  ( 11.27234208742519783, 3.445253572379500362, -8.372004648554700168 ) ) ;
#68425 = CARTESIAN_POINT ( 'NONE',  ( 11.09725056272499977, -2.683866746800999792, 7.480494252843770120 ) ) ;
#68426 = CARTESIAN_POINT ( 'NONE',  ( 8.666985328329976923, -5.621196112576180681, 6.797938611047623425 ) ) ;
#68427 = CARTESIAN_POINT ( 'NONE',  ( 10.82533997688000049, -3.756890902898200046, 8.614534918052999757 ) ) ;
#68428 = CARTESIAN_POINT ( 'NONE',  ( 9.362885841227999606, 3.677414437776999723, 9.250745771096999803 ) ) ;
#68429 = ORIENTED_EDGE ( 'NONE', *, *, #54208, .T. ) ;
#68430 = CARTESIAN_POINT ( 'NONE',  ( 9.143927823787141307, -2.750011555256801188, -7.499999844943244121 ) ) ;
#68431 = CONICAL_SURFACE ( 'NONE', #20434, 13.22499948080999843, 0.7853981240402999608 ) ;
#68432 = CARTESIAN_POINT ( 'NONE',  ( 11.59999999999999964, -2.935681553670999921, -8.155535082817699788 ) ) ;
#68433 = CARTESIAN_POINT ( 'NONE',  ( 11.79999999684100054, 3.345264396959000130, -11.86064773189999855 ) ) ;
#68434 = EDGE_LOOP ( 'NONE', ( #21500, #46872, #14424, #13099, #3163 ) ) ;
#68435 = CARTESIAN_POINT ( 'NONE',  ( 12.37577160951054367, -2.954704321271699907, -12.33392404961604072 ) ) ;
#68436 = EDGE_CURVE ( 'NONE', #2498, #19018, #67826, .T. ) ;
#68437 = CIRCLE ( 'NONE', #61766, 1.500000000000000000 ) ;
#68438 = CARTESIAN_POINT ( 'NONE',  ( 18.36457177586446221, 3.090900475971610550, 11.23268385208956488 ) ) ;
#68439 = CARTESIAN_POINT ( 'NONE',  ( 24.35365242081700288, -8.326148686863003689, 7.789520173261992753 ) ) ;
#68440 = CARTESIAN_POINT ( 'NONE',  ( 11.09999999999999964, -5.350000000000000533, 7.500000000000000000 ) ) ;
#68441 = CARTESIAN_POINT ( 'NONE',  ( 12.52647507922624115, -1.940423270478297768, -13.77628945559398588 ) ) ;
#68442 = CARTESIAN_POINT ( 'NONE',  ( 11.48641235500450009, -4.739919807690899489, -6.822158181405299615 ) ) ;
#68443 = PLANE ( 'NONE',  #59893 ) ;
#68444 = CARTESIAN_POINT ( 'NONE',  ( 17.88886072129112748, -3.119102935781168817, 12.20783478086260487 ) ) ;
#68445 = EDGE_LOOP ( 'NONE', ( #42152, #51921, #67653, #52395 ) ) ;
#68446 = VERTEX_POINT ( 'NONE', #33721 ) ;
#68447 = CARTESIAN_POINT ( 'NONE',  ( 11.30000000000000071, 0.000000000000000000, 0.000000000000000000 ) ) ;
#68448 = CARTESIAN_POINT ( 'NONE',  ( -0.2999999999999999889, -0.5773502691895999739, -1.000000000000000000 ) ) ;
#68449 = CARTESIAN_POINT ( 'NONE',  ( 10.58996475420000039, 2.876740601533999797, -6.236530348556999392 ) ) ;
#68450 = CARTESIAN_POINT ( 'NONE',  ( 10.84088306584999906, -2.636277440143000472, -7.512643837511999934 ) ) ;
#68451 = CARTESIAN_POINT ( 'NONE',  ( 17.96133816917716786, 2.975035784927402727, 12.32810058309831014 ) ) ;
#68452 = CARTESIAN_POINT ( 'NONE',  ( 23.95125525613000050, -12.88154415998999980, 3.488952313995000054 ) ) ;
#68453 = CARTESIAN_POINT ( 'NONE',  ( 9.228133567168001150, 2.875367362387999837, 8.669940206484001877 ) ) ;
#68454 = EDGE_LOOP ( 'NONE', ( #41339, #44965, #47534, #16677 ) ) ;
#68455 = CARTESIAN_POINT ( 'NONE',  ( 8.686257345956043707, -4.773936950834467119, -6.393475887002888491 ) ) ;
#68456 = EDGE_LOOP ( 'NONE', ( #7542, #47299, #36719, #59506 ) ) ;
#68457 = CARTESIAN_POINT ( 'NONE',  ( 12.36494524852001398, -2.943800415886788979, 12.33703218264930079 ) ) ;
#68458 = CARTESIAN_POINT ( 'NONE',  ( 9.222405316139999698, -4.184077495686000958, -8.347244604637999998 ) ) ;
#68459 = AXIS2_PLACEMENT_3D ( 'NONE', #14030, #3187, #61572 ) ;
#68460 = CARTESIAN_POINT ( 'NONE',  ( 11.05935155529000014, 2.480238120735000162, 6.610075178640000715 ) ) ;
#68461 = CARTESIAN_POINT ( 'NONE',  ( 12.18277869730536977, -4.531392946702499813, 8.547856079839998955 ) ) ;
#68462 = CARTESIAN_POINT ( 'NONE',  ( 11.66889198508051884, -11.69116221025809921, -1.923144176179720555 ) ) ;
#68463 = CIRCLE ( 'NONE', #58446, 2.200000000000001954 ) ;
#68464 = CARTESIAN_POINT ( 'NONE',  ( 11.12454631916000025, 7.322342417344000154, -6.385060111035000041 ) ) ;
#68465 = CARTESIAN_POINT ( 'NONE',  ( 10.39503166480599994, 2.725152142215999884, -7.589885038193400213 ) ) ;
#68466 = CARTESIAN_POINT ( 'NONE',  ( 12.46581852961811698, -0.5250240499537052186, 12.68539034781188413 ) ) ;
#68467 = EDGE_CURVE ( 'NONE', #44304, #4423, #21880, .T. ) ;
#68468 = EDGE_CURVE ( 'NONE', #7379, #43730, #41083, .T. ) ;
#68469 = CARTESIAN_POINT ( 'NONE',  ( 8.288068612932629975, 3.223876500227366382, -8.634712533562288073 ) ) ;
#68470 = CARTESIAN_POINT ( 'NONE',  ( 10.31667774810000004, 3.819530253758000260, 6.062195927068000145 ) ) ;
#68471 = CARTESIAN_POINT ( 'NONE',  ( 9.169137439642966569, -2.970390391148245435, 8.373688857599031365 ) ) ;
#68472 = ORIENTED_EDGE ( 'NONE', *, *, #14055, .F. ) ;
#68473 = CARTESIAN_POINT ( 'NONE',  ( 8.731095280410999138, 2.469361196073999842, -7.826019481986000059 ) ) ;
#68474 = CARTESIAN_POINT ( 'NONE',  ( 10.14887885159599890, 5.269014563305000287, -7.348611220446799486 ) ) ;
#68475 = CARTESIAN_POINT ( 'NONE',  ( 10.97892463630881110, -2.365042658448092361, 6.878289458889421226 ) ) ;
#68476 = CARTESIAN_POINT ( 'NONE',  ( 12.43753697068043884, -3.107573092003766746, -12.21083123506395118 ) ) ;
#68477 = CARTESIAN_POINT ( 'NONE',  ( 12.10000000000000497, -4.447112190091931261, 8.372281669763946610 ) ) ;
#68478 = CARTESIAN_POINT ( 'NONE',  ( 10.79303032197930001, -3.336467919271199900, -6.572090902022299730 ) ) ;
#68479 = ORIENTED_EDGE ( 'NONE', *, *, #13361, .T. ) ;
#68480 = STYLED_ITEM ( 'NONE', ( #58145 ), #30727 ) ;
#68481 = B_SPLINE_CURVE_WITH_KNOTS ( 'NONE', 3,
 ( #34673, #44480, #29086, #65772, #49701, #7051 ),
 .UNSPECIFIED., .F., .F.,
 ( 4, 1, 1, 4 ),
 ( 0.000000000000000000, 0.3333333333333000081, 0.6666666666667000474, 1.000000000000000000 ),
 .UNSPECIFIED. ) ;
#68482 = CARTESIAN_POINT ( 'NONE',  ( 5.655092287087765790, -12.08052032219203831, 3.735600122826553182 ) ) ;
#68483 = CARTESIAN_POINT ( 'NONE',  ( 8.207510841230000409, 5.944584532500000407, 7.106843289410999631 ) ) ;
#68484 = CIRCLE ( 'NONE', #42853, 2.725000000000000089 ) ;
#68486 = CARTESIAN_POINT ( 'NONE',  ( 13.80650642310300036, -9.578547012936001082, -8.130125899688998459 ) ) ;
#68485 = CARTESIAN_POINT ( 'NONE',  ( 9.418864158773999407, 3.210851187372000037, -6.346613542714999667 ) ) ;
#68487 = DIRECTION ( 'NONE',  ( 0.000000000000000000, 0.000000000000000000, -1.000000000000000000 ) ) ;
#68488 = ORIENTED_EDGE ( 'NONE', *, *, #64295, .F. ) ;
#68489 = CARTESIAN_POINT ( 'NONE',  ( 9.736878146978000359, 2.742182981761000171, 6.839230404018000087 ) ) ;
#68490 = CARTESIAN_POINT ( 'NONE',  ( 18.16473232272958427, -2.360987313248031683, -13.70192779769509528 ) ) ;
#68491 = CARTESIAN_POINT ( 'NONE',  ( 10.40749413291699987, 4.788043169210699723, 7.859564368461399830 ) ) ;
#68492 = CARTESIAN_POINT ( 'NONE',  ( 4.599999999999999645, 0.7192913403693006469, 12.57945229203838444 ) ) ;
#68493 = CARTESIAN_POINT ( 'NONE',  ( 7.897956853208000005, -3.608524635952000459, 5.913372239166000632 ) ) ;
#68494 = ORIENTED_EDGE ( 'NONE', *, *, #36137, .F. ) ;
#68495 = CARTESIAN_POINT ( 'NONE',  ( 7.711426658771000753, 5.797099724369999763, 8.340484548805999765 ) ) ;
#68496 = EDGE_CURVE ( 'NONE', #16603, #24287, #30325, .T. ) ;
#68498 = CARTESIAN_POINT ( 'NONE',  ( 10.19122055961999962, -3.990707710465999813, -5.651373900265999950 ) ) ;
#68497 = CARTESIAN_POINT ( 'NONE',  ( 10.18367854428777974, -2.796579479970164872, 8.204151721975753375 ) ) ;
#68499 = CARTESIAN_POINT ( 'NONE',  ( 7.507604010646850234, -2.694814696844040736, 6.316660876498477073 ) ) ;
#68500 = DIRECTION ( 'NONE',  ( -1.000000000000000000, 0.000000000000000000, 0.000000000000000000 ) ) ;
#68501 = CARTESIAN_POINT ( 'NONE',  ( 1.404700767030999886, 0.7969358895047999880, 3.160091737778000009 ) ) ;
#68502 = ORIENTED_EDGE ( 'NONE', *, *, #66607, .F. ) ;
#68503 = CARTESIAN_POINT ( 'NONE',  ( 1.238685001925042384, 2.938954507330893140, -1.506992772821682314 ) ) ;
#68504 = EDGE_CURVE ( 'NONE', #39994, #37746, #52538, .T. ) ;
#68505 = CARTESIAN_POINT ( 'NONE',  ( 11.17826222744820086, -4.668580868411999596, 6.949274830123499669 ) ) ;
#68506 = CARTESIAN_POINT ( 'NONE',  ( 9.719613305057999142, 5.967773797872000685, 7.406643507784999692 ) ) ;
#68507 = CARTESIAN_POINT ( 'NONE',  ( 9.353724647487000610, 2.823567847429000022, 9.032053040610000139 ) ) ;
#68508 = CARTESIAN_POINT ( 'NONE',  ( 10.52226222744799955, 3.119510978356100139, 6.774721295617600170 ) ) ;
#68509 = ORIENTED_EDGE ( 'NONE', *, *, #20125, .F. ) ;
#68510 = CARTESIAN_POINT ( 'NONE',  ( 10.98768472569999943, 6.720753179915999631, -5.471698458723999181 ) ) ;
#68511 = CARTESIAN_POINT ( 'NONE',  ( 12.40905465428145504, 1.877469967418645247, -12.45933993000109119 ) ) ;
#68512 = VECTOR ( 'NONE', #51209, 1000.000000000000000 ) ;
#68513 = DIRECTION ( 'NONE',  ( 0.000000000000000000, -1.000000000000000000, 0.000000000000000000 ) ) ;
#68514 = CARTESIAN_POINT ( 'NONE',  ( 25.25777475496700220, -2.569644838348999816, -11.37092172327999862 ) ) ;
#68515 = AXIS2_PLACEMENT_3D ( 'NONE', #657, #21970, #26890 ) ;
#68516 = CARTESIAN_POINT ( 'NONE',  ( 18.27122651615335158, -2.402315819361985572, 13.79236889726217186 ) ) ;
#68517 = CARTESIAN_POINT ( 'NONE',  ( 11.30000285318000230, 11.76356368987999979, 1.428410073821000159 ) ) ;
#68518 = VERTEX_POINT ( 'NONE', #24602 ) ;
#68519 = DIRECTION ( 'NONE',  ( 0.000000000000000000, 0.000000000000000000, -1.000000000000000000 ) ) ;
#68520 = CARTESIAN_POINT ( 'NONE',  ( 9.242292592096250203, -4.365494583328262124, -6.294013902202234334 ) ) ;
#68521 = ORIENTED_EDGE ( 'NONE', *, *, #50106, .T. ) ;
#68522 = CARTESIAN_POINT ( 'NONE',  ( 8.216851002544000693, 2.832432432432000269, 6.822293592207000934 ) ) ;
#68523 = ADVANCED_FACE ( 'NONE', ( #68607 ), #15487, .F. ) ;
#68524 = CARTESIAN_POINT ( 'NONE',  ( 11.09672200990539892, 3.182132064022000328, 7.785290430335599865 ) ) ;
#68525 = CARTESIAN_POINT ( 'NONE',  ( 11.18051582549000145, 5.340073783367000892, 8.416152717850000187 ) ) ;
#68526 = CARTESIAN_POINT ( 'NONE',  ( 9.922184613163000932, 3.489926301007000298, -9.111807643819000546 ) ) ;
#68527 = CARTESIAN_POINT ( 'NONE',  ( 10.18940772478662637, -4.553612660159668479, -8.177528816364860731 ) ) ;
#68528 = CARTESIAN_POINT ( 'NONE',  ( 10.30047649312000146, -4.027768368024999823, 9.431342508940000258 ) ) ;
#68529 = CARTESIAN_POINT ( 'NONE',  ( 17.55505043854144276, 0.6250000000000001110, -12.67928921589118652 ) ) ;
#68530 = CARTESIAN_POINT ( 'NONE',  ( 8.983360123997224278, 5.350320840654694265, 7.640098978919741768 ) ) ;
#68531 = CARTESIAN_POINT ( 'NONE',  ( 11.28949010443639978, -2.999324937259999935, -7.574834962826040297 ) ) ;
#68532 = CARTESIAN_POINT ( 'NONE',  ( 7.127331191709949998, -0.2622596576204692664, 1.265536610600155099 ) ) ;
#68533 = ORIENTED_EDGE ( 'NONE', *, *, #31344, .T. ) ;
#68534 = AXIS2_PLACEMENT_3D ( 'NONE', #11068, #32402, #47103 ) ;
#68535 = CARTESIAN_POINT ( 'NONE',  ( 7.474999999999996980, 4.000000000000000000, 8.979903810567666511 ) ) ;
#68536 = CARTESIAN_POINT ( 'NONE',  ( 12.03192018828833731, -4.908970299435360118, 7.824998071251875409 ) ) ;
#68537 = CARTESIAN_POINT ( 'NONE',  ( 8.674830025576062198, 2.649890579813255709, 7.499988935010339475 ) ) ;
#68538 = AXIS2_PLACEMENT_3D ( 'NONE', #58747, #63980, #366 ) ;
#68539 = CARTESIAN_POINT ( 'NONE',  ( 11.32763480027999137, 9.448540156737001539, 6.821721532523001841 ) ) ;
#68540 = CARTESIAN_POINT ( 'NONE',  ( 12.09886375431303485, 2.684759089869686477, 13.74018286504951192 ) ) ;
#68541 = CARTESIAN_POINT ( 'NONE',  ( 10.96876739532000045, -2.333349849211999949, 6.524062020538999640 ) ) ;
#68542 = CARTESIAN_POINT ( 'NONE',  ( 12.40638932695447672, -0.4813547430241597036, -12.68771948605803424 ) ) ;
#68543 = AXIS2_PLACEMENT_3D ( 'NONE', #51154, #45223, #30181 ) ;
#68544 = CARTESIAN_POINT ( 'NONE',  ( 12.71024384884961833, -0.7243378955761884397, 13.98124959093732400 ) ) ;
#68545 = VERTEX_POINT ( 'NONE', #4635 ) ;
#68546 = CARTESIAN_POINT ( 'NONE',  ( 24.53003472522700434, 8.771519074185000875, 8.897032352648000852 ) ) ;
#68547 = CARTESIAN_POINT ( 'NONE',  ( 10.13827973160999818, -3.897539901865500145, -6.362794488108000301 ) ) ;
#68548 = CARTESIAN_POINT ( 'NONE',  ( 13.70005190196300227, -9.005348107749998832, -7.391036106496999381 ) ) ;
#68549 = CARTESIAN_POINT ( 'NONE',  ( 9.600494040286998043, -5.206548117663999165, 8.585114612872999373 ) ) ;
#68550 = CARTESIAN_POINT ( 'NONE',  ( 11.84287482311539996, -3.196874704906699893, 7.175518335304800210 ) ) ;
#68551 = CARTESIAN_POINT ( 'NONE',  ( 8.705629240797998492, 3.771058080785100408, 6.623477632995699693 ) ) ;
#68552 = EDGE_CURVE ( 'NONE', #57647, #20309, #36118, .T. ) ;
#68553 = EDGE_CURVE ( 'NONE', #10113, #27484, #19411, .T. ) ;
#68554 = CARTESIAN_POINT ( 'NONE',  ( 9.112942518363999156, 5.100000000000000533, 6.192000867487999827 ) ) ;
#68555 = CARTESIAN_POINT ( 'NONE',  ( 9.731470621293439649, 3.294701422184862949, -8.705110408592389604 ) ) ;
#68556 = CARTESIAN_POINT ( 'NONE',  ( 12.07989974639899167, 2.471827770301481042, 12.35516928474874554 ) ) ;
#68557 = CARTESIAN_POINT ( 'NONE',  ( 9.221306596384000187, -5.362859773739999447, -6.470306978669999154 ) ) ;
#68558 = EDGE_CURVE ( 'NONE', #68596, #51514, #36486, .T. ) ;
#68559 = CARTESIAN_POINT ( 'NONE',  ( 11.60948876160955479, 3.304472173606900043, -8.223320049540498999 ) ) ;
#68560 = CARTESIAN_POINT ( 'NONE',  ( 8.283628111110997949, 2.878995628920999916, -6.357604486408997779 ) ) ;
#68561 = CARTESIAN_POINT ( 'NONE',  ( 10.01676721958999927, 4.324998751150999965, -9.154078823942999321 ) ) ;
#68562 = CARTESIAN_POINT ( 'NONE',  ( 8.718784697134999817, 4.694174896253500151, -6.425520776924999566 ) ) ;
#68564 = CARTESIAN_POINT ( 'NONE',  ( 12.72293129229312747, 3.125000000000000444, 12.28373127578716328 ) ) ;
#68563 = CARTESIAN_POINT ( 'NONE',  ( 9.057169810767971896, -3.796486612318636933, -8.707169876682314680 ) ) ;
#68565 = DIRECTION ( 'NONE',  ( -1.000000000000000000, 0.000000000000000000, 0.000000000000000000 ) ) ;
#68566 = EDGE_LOOP ( 'NONE', ( #22230, #15656, #66726, #29179 ) ) ;
#68567 = VECTOR ( 'NONE', #22222, 1000.000000000000000 ) ;
#68568 = CYLINDRICAL_SURFACE ( 'NONE', #16024, 1.250000000000000222 ) ;
#68569 = CARTESIAN_POINT ( 'NONE',  ( 10.24809687351608289, 4.327184855449106138, 8.717465845835393523 ) ) ;
#68570 = CARTESIAN_POINT ( 'NONE',  ( 10.81316193496000011, -3.756072284922999938, 6.071597915422999314 ) ) ;
#68571 = CARTESIAN_POINT ( 'NONE',  ( 8.971126402771000485, 4.939810497841199854, 7.854398824525599565 ) ) ;
#68572 = CARTESIAN_POINT ( 'NONE',  ( 29.91622776601699840, -7.448824697892998696E-09, 6.772075922005999615 ) ) ;
#68573 = CARTESIAN_POINT ( 'NONE',  ( 12.23409240334736658, -2.245563803222850652, 13.72414218390522223 ) ) ;
#68574 = CARTESIAN_POINT ( 'NONE',  ( 5.500000000000000000, 13.17499999999999893, 0.000000000000000000 ) ) ;
#68575 = DIRECTION ( 'NONE',  ( 0.000000000000000000, 0.2588190451024932059, -0.9659258262890756397 ) ) ;
#68576 = VERTEX_POINT ( 'NONE', #25630 ) ;
#68577 = CARTESIAN_POINT ( 'NONE',  ( 5.184842376537999620, 1.175001787988000146, 0.4961318581031999297 ) ) ;
#68578 = AXIS2_PLACEMENT_3D ( 'NONE', #50822, #57774, #31563 ) ;
#68579 = CARTESIAN_POINT ( 'NONE',  ( 8.769442991499998286, -4.080527519162810535, -6.223324745230999433 ) ) ;
#68580 = CARTESIAN_POINT ( 'NONE',  ( 10.98768577056000062, -2.700436730051000378, -4.945210085382000464 ) ) ;
#68581 = CARTESIAN_POINT ( 'NONE',  ( 12.06833327354034857, -4.746587807672299597, 7.988332985010599963 ) ) ;
#68582 = CARTESIAN_POINT ( 'NONE',  ( 18.05208962242102189, 2.879457400869559702, -12.35505085550156323 ) ) ;
#68583 = CARTESIAN_POINT ( 'NONE',  ( 9.099999931440999390, -2.935682118448999844, -8.155535999783198875 ) ) ;
#68584 = AXIS2_PLACEMENT_3D ( 'NONE', #3675, #8938, #9967 ) ;
#68585 = CARTESIAN_POINT ( 'NONE',  ( 17.59643454745089386, 3.125000000000000444, 12.28373095898682621 ) ) ;
#68586 = CARTESIAN_POINT ( 'NONE',  ( 7.764631182151003230, 2.924915923740001311, 6.482382710726004582 ) ) ;
#68587 = CARTESIAN_POINT ( 'NONE',  ( 10.90000000000000036, 0.2500000000000000000, -4.902439024389999567 ) ) ;
#68588 = CARTESIAN_POINT ( 'NONE',  ( 24.44496487975900223, 3.224879802562000464, -12.03535984693000138 ) ) ;
#68589 = DIRECTION ( 'NONE',  ( -1.000000000000000000, 0.000000000000000000, 0.000000000000000000 ) ) ;
#68590 = CARTESIAN_POINT ( 'NONE',  ( 17.55505043854143565, 3.125000000000000000, 12.28373071562070074 ) ) ;
#68591 = CARTESIAN_POINT ( 'NONE',  ( 23.71888924647654306, 9.886276567970025297, -9.463295795964285162 ) ) ;
#68592 = FACE_BOUND ( 'NONE', #51608, .T. ) ;
#68593 = B_SPLINE_CURVE_WITH_KNOTS ( 'NONE', 3,
 ( #68751, #15284, #53032, #5478 ),
 .UNSPECIFIED., .F., .F.,
 ( 4, 4 ),
 ( 0.000000000000000000, 1.000000000000000000 ),
 .UNSPECIFIED. ) ;
#68594 = CARTESIAN_POINT ( 'NONE',  ( 24.63808311177700361, 12.49523003131000110, -2.948547624863999683 ) ) ;
#68595 =( REPRESENTATION_RELATIONSHIP ('NONE','NONE', #10823, #53976 ) REPRESENTATION_RELATIONSHIP_WITH_TRANSFORMATION ( #22503 )SHAPE_REPRESENTATION_RELATIONSHIP( ) );
#68596 = VERTEX_POINT ( 'NONE', #58132 ) ;
#68597 = CARTESIAN_POINT ( 'NONE',  ( 9.600045280412000892, 3.021734963141999852, -6.070209284876999511 ) ) ;
#68598 = CARTESIAN_POINT ( 'NONE',  ( 12.10948876160955479, -4.695527826393099957, 6.776679950459500112 ) ) ;
#68599 = ORIENTED_EDGE ( 'NONE', *, *, #65832, .F. ) ;
#68600 = B_SPLINE_CURVE_WITH_KNOTS ( 'NONE', 3,
 ( #37108, #16799, #65031, #56540 ),
 .UNSPECIFIED., .F., .F.,
 ( 4, 4 ),
 ( 0.000000000000000000, 1.000000000000000000 ),
 .UNSPECIFIED. ) ;
#68601 = DIRECTION ( 'NONE',  ( 0.000000000000000000, 0.000000000000000000, -1.000000000000000000 ) ) ;
#68602 = CARTESIAN_POINT ( 'NONE',  ( 11.33041235500449950, -4.942357465271699724, -6.636704692336500067 ) ) ;
#68603 = ORIENTED_EDGE ( 'NONE', *, *, #7036, .T. ) ;
#68604 = CARTESIAN_POINT ( 'NONE',  ( 11.26723293495529887, 2.826061044294000180, 7.547192037433419820 ) ) ;
#68605 = EDGE_CURVE ( 'NONE', #13517, #12282, #6904, .T. ) ;
#68606 = CARTESIAN_POINT ( 'NONE',  ( 9.591185841232000797, 2.173570076733999823, -8.023168429484000441 ) ) ;
#68607 = FACE_OUTER_BOUND ( 'NONE', #29783, .T. ) ;
#68608 = CARTESIAN_POINT ( 'NONE',  ( 10.57102344389999971, -4.762665848028800220, -7.037150754511299233 ) ) ;
#68609 = CARTESIAN_POINT ( 'NONE',  ( 12.20071588509496863, 0.1606973242730105611, -13.89876784138466626 ) ) ;
#68610 = DIRECTION ( 'NONE',  ( 1.000000000000000000, 0.000000000000000000, 0.000000000000000000 ) ) ;
#68611 = EDGE_CURVE ( 'NONE', #19003, #26690, #58671, .T. ) ;
#68612 = CARTESIAN_POINT ( 'NONE',  ( 11.09999999999999964, 5.553261372860998968, 5.124965741905999295 ) ) ;
#68613 = VERTEX_POINT ( 'NONE', #20382 ) ;
#68614 = CARTESIAN_POINT ( 'NONE',  ( 13.80650642310300036, 9.578547012936001082, 8.130125899688998459 ) ) ;
#68615 = CARTESIAN_POINT ( 'NONE',  ( 8.351014158771000950, 5.616457598545999907, -8.245813000738998255 ) ) ;
#68616 = ORIENTED_EDGE ( 'NONE', *, *, #4429, .T. ) ;
#68617 = AXIS2_PLACEMENT_3D ( 'NONE', #56636, #62217, #67113 ) ;
#68618 = CARTESIAN_POINT ( 'NONE',  ( 9.882903428397000312, 4.314559027837000293, -9.161039561412001930 ) ) ;
#68619 = VERTEX_POINT ( 'NONE', #62343 ) ;
#68620 = DIRECTION ( 'NONE',  ( 0.000000000000000000, 0.000000000000000000, 1.000000000000000000 ) ) ;
#68621 = CARTESIAN_POINT ( 'NONE',  ( 18.02661896923965656, -2.910306870311579974, -12.34644497411517250 ) ) ;
#68622 = AXIS2_PLACEMENT_3D ( 'NONE', #69150, #63556, #53076 ) ;
#68623 = CARTESIAN_POINT ( 'NONE',  ( 9.610944094206999466, -5.100000000000000533, -6.571291218949999902 ) ) ;
#68624 = B_SPLINE_CURVE_WITH_KNOTS ( 'NONE', 3,
 ( #54579, #64353, #37805, #54222, #38141, #60512, #23101, #43750, #22753, #1096 ),
 .UNSPECIFIED., .F., .F.,
 ( 4, 2, 2, 2, 4 ),
 ( 0.000000000000000000, 0.2500000000000000000, 0.5000000000000000000, 0.7500000000000000000, 1.000000000000000000 ),
 .UNSPECIFIED. ) ;
#68625 = DIRECTION ( 'NONE',  ( 1.000000000000000000, 0.000000000000000000, 0.000000000000000000 ) ) ;
#68626 = CARTESIAN_POINT ( 'NONE',  ( 8.969027209994999694, -8.708546445325000107, -6.388758794122999518 ) ) ;
#68627 = ORIENTED_EDGE ( 'NONE', *, *, #53652, .F. ) ;
#68628 = CARTESIAN_POINT ( 'NONE',  ( 11.85864217039400259, 11.85700164854999983, -4.150661879143999755 ) ) ;
#68629 = CARTESIAN_POINT ( 'NONE',  ( 17.71037843287399838, 11.39032026920000007, -4.571464210656999150 ) ) ;
#68630 = CARTESIAN_POINT ( 'NONE',  ( 8.440795537699431250, -5.100000000000000533, 6.662590550605512973 ) ) ;
#68631 = CARTESIAN_POINT ( 'NONE',  ( 8.824071121570657539, 4.974071175014779911, 7.751553442067931954 ) ) ;
#68632 = CARTESIAN_POINT ( 'NONE',  ( 11.54684497800060150, 3.023157657667436826, 7.175001354288133015 ) ) ;
#68633 = CARTESIAN_POINT ( 'NONE',  ( 18.23043922992600230, -3.518658233831999826, 12.06062508533999988 ) ) ;
#68634 = CARTESIAN_POINT ( 'NONE',  ( 10.01597818573999987, -4.792673671522000411, -6.390249203106999509 ) ) ;
#68635 = EDGE_CURVE ( 'NONE', #34076, #26471, #25231, .T. ) ;
#68636 = ORIENTED_EDGE ( 'NONE', *, *, #68436, .T. ) ;
#68637 = ORIENTED_EDGE ( 'NONE', *, *, #64336, .F. ) ;
#68638 = CARTESIAN_POINT ( 'NONE',  ( 11.13509627103000099, 5.337904119774999678, -5.086083210688999934 ) ) ;
#68639 = DIRECTION ( 'NONE',  ( -1.000000000000000000, 0.000000000000000000, 0.000000000000000000 ) ) ;
#68640 = EDGE_CURVE ( 'NONE', #24760, #45907, #41958, .T. ) ;
#68641 = EDGE_CURVE ( 'NONE', #9679, #65751, #42822, .T. ) ;
#68642 = CARTESIAN_POINT ( 'NONE',  ( 12.72306420252713544, -3.125000000000000888, 13.52084465375506461 ) ) ;
#68643 = CARTESIAN_POINT ( 'NONE',  ( 0.1499942179679999710, 2.199046806507071405, -1.689975037551097348 ) ) ;
#68644 = CARTESIAN_POINT ( 'NONE',  ( 11.71922412107039868, 4.069539071394910223, -6.185573549454999487 ) ) ;
#68645 = CARTESIAN_POINT ( 'NONE',  ( 9.560684229509998744, 3.388828644390000200, -6.885038603985500494 ) ) ;
#68647 = CARTESIAN_POINT ( 'NONE',  ( 4.400000000000000355, 1.266759534686000110, 0.8033182938792000627 ) ) ;
#68646 = CARTESIAN_POINT ( 'NONE',  ( 10.50962143724499853, -3.332852462363599777, 8.250837174995698575 ) ) ;
#68648 = CARTESIAN_POINT ( 'NONE',  ( 4.607109839683332986, -1.199500263597270244, -0.9218200799623728070 ) ) ;
#68649 = ORIENTED_EDGE ( 'NONE', *, *, #54535, .T. ) ;
#68650 = B_SPLINE_CURVE_WITH_KNOTS ( 'NONE', 3,
 ( #49788, #65858, #60623, #2245, #28828, #39998, #8174, #29523, #50825, #20037, #40669, #52192, #36114, #4291 ),
 .UNSPECIFIED., .F., .F.,
 ( 4, 2, 2, 2, 2, 2, 4 ),
 ( 0.1255288371561983085, 0.2191765140581366789, 0.3128241909600750770, 0.4064718678620133918, 0.5001195447639518177, 0.6874148985678291135, 0.8747102523717062983 ),
 .UNSPECIFIED. ) ;
#68651 = CARTESIAN_POINT ( 'NONE',  ( 1.000973465875999890, 3.500000000000000000, 0.000000000000000000 ) ) ;
#68652 = CARTESIAN_POINT ( 'NONE',  ( 10.35355256951999969, -3.429327234421000181, -4.862083573089999611 ) ) ;
#68653 = CARTESIAN_POINT ( 'NONE',  ( 10.24160887879199855, 3.710311786319799854, 8.745979585038000437 ) ) ;
#68654 = LINE ( 'NONE', #63409, #7949 ) ;
#68655 = CARTESIAN_POINT ( 'NONE',  ( 10.74609562913000005, -4.263104965433000437, 9.276976808608999647 ) ) ;
#68656 = CARTESIAN_POINT ( 'NONE',  ( 18.16752965492863936, 2.624502287304359527, -12.42171427742621859 ) ) ;
#68657 = CARTESIAN_POINT ( 'NONE',  ( 10.66052890781999984, -2.899999999999999911, -6.152188490330000370 ) ) ;
#68658 = EDGE_CURVE ( 'NONE', #49429, #1971, #60284, .T. ) ;
#68659 = CARTESIAN_POINT ( 'NONE',  ( 13.55266668291200105, 9.123246021508000680, 7.477861434740999513 ) ) ;
#68660 = CARTESIAN_POINT ( 'NONE',  ( 11.91486084871699802, -5.207010770456999893, 7.174999999999999822 ) ) ;
#68661 = CARTESIAN_POINT ( 'NONE',  ( 9.712659112603999390, -4.376739491155700712, -8.280881105104999307 ) ) ;
#68662 = CARTESIAN_POINT ( 'NONE',  ( 6.412459438551000090, -0.6732323296109999911, -0.9643333493903999409 ) ) ;
#68663 = CARTESIAN_POINT ( 'NONE',  ( 10.87837607040048127, -3.132032243413395367, 7.603545367532808186 ) ) ;
#68664 = AXIS2_PLACEMENT_3D ( 'NONE', #36657, #10075, #9958 ) ;
#68665 = CARTESIAN_POINT ( 'NONE',  ( 6.899999691988000450, -11.00717859340000082, 1.432487142323000118 ) ) ;
#68666 = DIRECTION ( 'NONE',  ( 0.000000000000000000, -1.000000000000000000, 0.000000000000000000 ) ) ;
#68667 = ORIENTED_EDGE ( 'NONE', *, *, #28754, .T. ) ;
#68668 = CARTESIAN_POINT ( 'NONE',  ( 12.24904276456879160, -0.2856309244984034379, -12.69568149856438311 ) ) ;
#68669 = CARTESIAN_POINT ( 'NONE',  ( 12.80505043854146940, -3.125000000000000000, -12.28373071562070074 ) ) ;
#68670 = DIRECTION ( 'NONE',  ( 0.000000000000000000, -0.8615889394142682844, 0.5076066385292812289 ) ) ;
#68671 = CARTESIAN_POINT ( 'NONE',  ( 24.52301487032427829, 3.339126876001507593, -12.06936641334276672 ) ) ;
#68672 = CARTESIAN_POINT ( 'NONE',  ( 1.728056799208041561, -2.150913519912213800, 2.798833948393621540 ) ) ;
#68673 = ORIENTED_EDGE ( 'NONE', *, *, #48403, .T. ) ;
#68674 = CARTESIAN_POINT ( 'NONE',  ( 18.30008632280270930, 2.887848135250621385E-14, -11.85014035451981762 ) ) ;
#68675 = APPLICATION_PROTOCOL_DEFINITION ( 'draft international standard', 'automotive_design', 1998, #39623 ) ;
#68676 = CARTESIAN_POINT ( 'NONE',  ( 11.14256920625030034, -3.957769094421040190, -6.325872106312999676 ) ) ;
#68677 = CARTESIAN_POINT ( 'NONE',  ( 10.98395291507793381, 8.151105813983006598, 6.540856040902778723 ) ) ;
#68678 = CARTESIAN_POINT ( 'NONE',  ( 9.568197172114265570, -5.125396288426561142, -6.749639981083131346 ) ) ;
#68679 = CARTESIAN_POINT ( 'NONE',  ( 11.49999672495000347, -8.721203281753666658, 7.819494091976963546 ) ) ;
#68680 = CARTESIAN_POINT ( 'NONE',  ( 10.37199293566600034, 4.633387186021100668, -8.276990458557699881 ) ) ;
#68681 = VERTEX_POINT ( 'NONE', #5667 ) ;
#68682 = CARTESIAN_POINT ( 'NONE',  ( 9.889844610056000462, -4.052276314598000084, 9.260527932809999641 ) ) ;
#68683 = ORIENTED_EDGE ( 'NONE', *, *, #14666, .F. ) ;
#68684 = CARTESIAN_POINT ( 'NONE',  ( 9.441293086742424734, -5.329066508289010962, 7.778880124525636930 ) ) ;
#68685 = CARTESIAN_POINT ( 'NONE',  ( 7.647245559622000144, -5.850279024084999335, 6.784181137144999596 ) ) ;
#68686 = CIRCLE ( 'NONE', #11743, 2.000000000000001332 ) ;
#68687 = EDGE_CURVE ( 'NONE', #37266, #2854, #51971, .T. ) ;
#68688 = CARTESIAN_POINT ( 'NONE',  ( 17.60274960888721552, -0.7290235424212396786, -13.98100605002522734 ) ) ;
#68689 = VERTEX_POINT ( 'NONE', #43079 ) ;
#68690 = CARTESIAN_POINT ( 'NONE',  ( 0.000000000000000000, 0.3800960799355100894, -2.900041633271500441 ) ) ;
#68691 = B_SPLINE_CURVE_WITH_KNOTS ( 'NONE', 3,
 ( #63693, #15808, #43424, #16832 ),
 .UNSPECIFIED., .F., .F.,
 ( 4, 4 ),
 ( 0.000000000000000000, 1.000000000000000000 ),
 .UNSPECIFIED. ) ;
#68692 = CARTESIAN_POINT ( 'NONE',  ( 6.703179719589999586, 5.447281585506000390, -7.886005609586001164 ) ) ;
#68693 = ADVANCED_FACE ( 'NONE', ( #59500 ), #39848, .F. ) ;
#68694 = CARTESIAN_POINT ( 'NONE',  ( 9.541846873516668381, -3.000416447002275611, -8.268183399968640046 ) ) ;
#68695 = CARTESIAN_POINT ( 'NONE',  ( 9.487498405967778936, 4.950355006253724710, 8.458582407359203970 ) ) ;
#68696 = ORIENTED_EDGE ( 'NONE', *, *, #52985, .T. ) ;
#68697 = CARTESIAN_POINT ( 'NONE',  ( 10.06343867337000120, -5.156226070197000411, 6.125223053176999777 ) ) ;
#68698 = CARTESIAN_POINT ( 'NONE',  ( 11.60000000000000497, 3.552887809908070960, 8.372281669763946610 ) ) ;
#68699 = CARTESIAN_POINT ( 'NONE',  ( 9.478248830702476369, -3.044910121894152333, 6.882626671536596241 ) ) ;
#68700 = ORIENTED_EDGE ( 'NONE', *, *, #14872, .F. ) ;
#68701 = CARTESIAN_POINT ( 'NONE',  ( 10.99385884816394388, -6.143977714627776976, -5.074464171073912233 ) ) ;
#68702 = ORIENTED_EDGE ( 'NONE', *, *, #52731, .F. ) ;
#68703 = CARTESIAN_POINT ( 'NONE',  ( 11.79999999742035044, 12.31348763297674331, 1.888274624276562896 ) ) ;
#68704 = CARTESIAN_POINT ( 'NONE',  ( 17.88386803568321426, 0.5319881936868626759, -13.88630234897434690 ) ) ;
#68705 = CARTESIAN_POINT ( 'NONE',  ( 8.745593092018999926, -5.100000000000000533, 6.404090157675000228 ) ) ;
#68706 = CARTESIAN_POINT ( 'NONE',  ( 5.000000000000000000, -0.2999999999999999889, 11.34603454956999791 ) ) ;
#68707 = CARTESIAN_POINT ( 'NONE',  ( 6.899999691988000450, 13.10000000000000142, -1.604287306883032847E-15 ) ) ;
#68708 = CARTESIAN_POINT ( 'NONE',  ( 9.224024145839393896, -4.217522721361648408, 6.654559194835224289 ) ) ;
#68709 = CARTESIAN_POINT ( 'NONE',  ( 12.23542143184359965, 2.757395375068925514, 13.61543998564091140 ) ) ;
#68710 = AXIS2_PLACEMENT_3D ( 'NONE', #54017, #28150, #21515 ) ;
#68711 = VERTEX_POINT ( 'NONE', #11598 ) ;
#68712 = EDGE_LOOP ( 'NONE', ( #6153, #38958, #59608, #48503 ) ) ;
#68713 = CARTESIAN_POINT ( 'NONE',  ( 9.722769750889000306, 5.493785011855999656, 6.566826815556000341 ) ) ;
#68714 = CARTESIAN_POINT ( 'NONE',  ( 9.926176658771000305, 4.356412802752999802, -9.313960415320000408 ) ) ;
#68715 = CIRCLE ( 'NONE', #29677, 0.4999999999999998335 ) ;
#68716 = FACE_OUTER_BOUND ( 'NONE', #4457, .T. ) ;
#68717 = CARTESIAN_POINT ( 'NONE',  ( 12.42175510762288404, 2.005905104281934914, -13.76592701692033138 ) ) ;
#68718 = CARTESIAN_POINT ( 'NONE',  ( 10.16052890781999984, 2.899999999999999911, -6.152188490330000370 ) ) ;
#68719 = CARTESIAN_POINT ( 'NONE',  ( 18.14710216240463581, -0.2005085131878108218, 13.89805835524349931 ) ) ;
#68720 = DIRECTION ( 'NONE',  ( -1.000000000000000000, 0.000000000000000000, 0.000000000000000000 ) ) ;
#68721 = CARTESIAN_POINT ( 'NONE',  ( 9.543013888829964486, -2.517265190286118948, -8.482290249887922684 ) ) ;
#68722 = ORIENTED_EDGE ( 'NONE', *, *, #4247, .F. ) ;
#68723 = CARTESIAN_POINT ( 'NONE',  ( 12.43800705108280802, 0.5060514261277413439, 13.88760251447654781 ) ) ;
#68724 = ADVANCED_FACE ( 'NONE', ( #10233 ), #58337, .F. ) ;
#68725 = CARTESIAN_POINT ( 'NONE',  ( 11.51041369783139956, -4.064477673403060543, 6.223614866029000048 ) ) ;
#68726 = CARTESIAN_POINT ( 'NONE',  ( 3.165556799210874406, 0.4581489286485003198, 3.500000000000000444 ) ) ;
#68727 = ADVANCED_FACE ( 'NONE', ( #777 ), #45509, .F. ) ;
#68728 = CARTESIAN_POINT ( 'NONE',  ( 15.83590051321700010, 9.131200976137998637, 8.359844154751998602 ) ) ;
#68729 = CARTESIAN_POINT ( 'NONE',  ( 7.924355646793000751, -2.432121990576000314, 6.597519606637999523 ) ) ;
#68731 = CARTESIAN_POINT ( 'NONE',  ( 23.60205915885299888, -2.489696159930001595, -12.09604418630999945 ) ) ;
#68730 = CARTESIAN_POINT ( 'NONE',  ( 9.696080515601000371, 2.554416243104999928, 7.600685069647000525 ) ) ;
#68732 = CARTESIAN_POINT ( 'NONE',  ( 10.13662282008599824, 4.594711216567399781, -8.459250300176799797 ) ) ;
#68733 = AXIS2_PLACEMENT_3D ( 'NONE', #57143, #7888, #9241 ) ;
#68734 = B_SPLINE_CURVE_WITH_KNOTS ( 'NONE', 3,
 ( #51527, #15505, #56785, #36831, #3623, #67593 ),
 .UNSPECIFIED., .F., .F.,
 ( 4, 2, 4 ),
 ( 0.000000000000000000, 0.5000000000000000000, 1.000000000000000000 ),
 .UNSPECIFIED. ) ;
#68735 = FACE_OUTER_BOUND ( 'NONE', #17609, .T. ) ;
#68736 = CARTESIAN_POINT ( 'NONE',  ( 9.045101285863999863, 3.441732526340400167, -6.836640842107200022 ) ) ;
#68737 = CARTESIAN_POINT ( 'NONE',  ( 18.27538032657185951, -0.08234928811777071644, 12.59973629603894096 ) ) ;
#68738 = CARTESIAN_POINT ( 'NONE',  ( 6.803330717051000676, 1.304674974472000093, -0.8456194954836000477 ) ) ;
#68739 = CARTESIAN_POINT ( 'NONE',  ( 18.10505187282240058, -3.528432543146287070, 12.01774066417138087 ) ) ;
#68740 = VERTEX_POINT ( 'NONE', #49707 ) ;
#68741 = CARTESIAN_POINT ( 'NONE',  ( 8.508081853209001011, -2.202816532622999812, 7.706987678916999762 ) ) ;
#68742 = CARTESIAN_POINT ( 'NONE',  ( 9.791229719590001324, 4.294368353031000396, -8.968663198664000191 ) ) ;
#68743 = CARTESIAN_POINT ( 'NONE',  ( 18.12392562323100265, 2.970749524062570313, 13.68118179967288128 ) ) ;
#68744 = EDGE_CURVE ( 'NONE', #42399, #21322, #28745, .T. ) ;
#68745 = CARTESIAN_POINT ( 'NONE',  ( 25.50731686952359212, -11.18389986068883601, -3.138234620650206086 ) ) ;
#68746 = ORIENTED_EDGE ( 'NONE', *, *, #7760, .F. ) ;
#68747 = CARTESIAN_POINT ( 'NONE',  ( 0.2882532571067000227, 2.601420761213999899, -2.147952162500999851 ) ) ;
#68748 = CARTESIAN_POINT ( 'NONE',  ( 11.67403632436368888, 3.023821283238099955, 7.727966254184200245 ) ) ;
#68749 = CARTESIAN_POINT ( 'NONE',  ( 10.25880778041000063, 2.491777456852000139, -7.289938575364999451 ) ) ;
#68750 = EDGE_LOOP ( 'NONE', ( #45173, #47155, #15459, #52349 ) ) ;
#68751 = CARTESIAN_POINT ( 'NONE',  ( 8.832537864289999874, 2.899999999999999911, 6.571291218949999902 ) ) ;
#68752 = DIRECTION ( 'NONE',  ( 1.000000000000000000, 0.000000000000000000, 4.050801148937999854E-14 ) ) ;
#68753 = CARTESIAN_POINT ( 'NONE',  ( 10.46887750876899936, 3.307728619566300043, 6.425720373262999274 ) ) ;
#68754 = CARTESIAN_POINT ( 'NONE',  ( 10.96876739532000045, -2.333349849211999949, 6.524062020538999640 ) ) ;
#68755 = CARTESIAN_POINT ( 'NONE',  ( 7.950760841228999176, 2.095715612964000218, 8.056490963156001328 ) ) ;
#68756 = ORIENTED_EDGE ( 'NONE', *, *, #31576, .F. ) ;
#68757 = DIRECTION ( 'NONE',  ( 0.000000000000000000, 1.000000000000000000, 0.000000000000000000 ) ) ;
#68758 = CARTESIAN_POINT ( 'NONE',  ( 7.367989158767000113, 5.517512745430000365, -8.643112676966000052 ) ) ;
#68759 = CARTESIAN_POINT ( 'NONE',  ( 8.288478674082428554, -4.754023060363307351, 9.067272220935310045 ) ) ;
#68760 = CARTESIAN_POINT ( 'NONE',  ( 10.89529697814178100, -3.173432105636238454, -7.215614489968412926 ) ) ;
#68761 = ORIENTED_EDGE ( 'NONE', *, *, #38171, .F. ) ;
#68762 = CARTESIAN_POINT ( 'NONE',  ( 11.35400411985998304, 11.72677417300536362, 1.687001524046905399 ) ) ;
#68763 = CARTESIAN_POINT ( 'NONE',  ( 6.219609839683335473, -0.1963495408493605987, -1.500000000000000444 ) ) ;
#68764 = ORIENTED_EDGE ( 'NONE', *, *, #49497, .F. ) ;
#68765 = CARTESIAN_POINT ( 'NONE',  ( 17.55505043854144276, 0.6250000000000001110, -12.67928921589118474 ) ) ;
#68766 = CARTESIAN_POINT ( 'NONE',  ( 18.43329252113700534, -2.892698357136523235, 12.11790064375147047 ) ) ;
#68767 = AXIS2_PLACEMENT_3D ( 'NONE', #32640, #28437, #54651 ) ;
#68768 = ORIENTED_EDGE ( 'NONE', *, *, #38391, .T. ) ;
#68769 = CARTESIAN_POINT ( 'NONE',  ( 17.86832607310548582, 0.5412024733746048089, -13.88582008197801976 ) ) ;
#68770 = DIRECTION ( 'NONE',  ( -0.4999999999999719669, 0.6407827956774649891, -0.5825782426110679424 ) ) ;
#68771 = CARTESIAN_POINT ( 'NONE',  ( 2.540556799210292205, 3.500000000000000888, -0.4581489286485045387 ) ) ;
#68772 = CARTESIAN_POINT ( 'NONE',  ( 11.18923293495519822, 2.967327562101000016, -7.458486839450950256 ) ) ;
#68773 = ADVANCED_FACE ( 'NONE', ( #55303 ), #12306, .F. ) ;
#68774 = CARTESIAN_POINT ( 'NONE',  ( 12.09966954483535773, -3.361010663344000005, 8.485927942460499196 ) ) ;
#68775 = LINE ( 'NONE', #4800, #56550 ) ;
#68776 = CARTESIAN_POINT ( 'NONE',  ( 11.87964291764649971, -5.268358781405000357, 7.656787697937099679 ) ) ;
#68777 = EDGE_LOOP ( 'NONE', ( #36192, #64884, #1630 ) ) ;
#68778 = CARTESIAN_POINT ( 'NONE',  ( 9.181704719590001673, 3.734279507827999556, 8.942126004519000304 ) ) ;
#68779 = EDGE_LOOP ( 'NONE', ( #11477, #3283, #55612, #17186 ) ) ;
#68780 = CARTESIAN_POINT ( 'NONE',  ( 7.773264469372000107, 2.859518616742000141, 6.768376720750000075 ) ) ;
#68781 = AXIS2_PLACEMENT_3D ( 'NONE', #36936, #31689, #53010 ) ;
#68782 = B_SPLINE_CURVE_WITH_KNOTS ( 'NONE', 3,
 ( #50121, #54669, #44199, #7459 ),
 .UNSPECIFIED., .F., .F.,
 ( 4, 4 ),
 ( 0.000000000000000000, 1.000000000000000000 ),
 .UNSPECIFIED. ) ;
#68783 = CARTESIAN_POINT ( 'NONE',  ( 7.647245559622000144, -5.850279024084999335, 6.784181137144999596 ) ) ;
#68784 = CARTESIAN_POINT ( 'NONE',  ( 11.07232916052000071, -5.267955070953999730, 5.080680273674000880 ) ) ;
#68785 = ORIENTED_EDGE ( 'NONE', *, *, #18191, .T. ) ;
#68786 = CARTESIAN_POINT ( 'NONE',  ( 12.67197039647513535, -3.110753821461599067, -12.28805851341190980 ) ) ;
#68787 = CARTESIAN_POINT ( 'NONE',  ( 18.15262501848119925, 3.263149105983724763, 11.18369374219401635 ) ) ;
#68788 = CARTESIAN_POINT ( 'NONE',  ( 23.60000000000000497, -1.954456612737695442, 13.79170061782608414 ) ) ;
#68789 = DIRECTION ( 'NONE',  ( 1.000000000000000000, 0.000000000000000000, 0.000000000000000000 ) ) ;
#68790 = CARTESIAN_POINT ( 'NONE',  ( 12.15975302296895499, -2.850959433913118346, -13.70664605376239287 ) ) ;
#68791 = CARTESIAN_POINT ( 'NONE',  ( 10.60441638348510018, -4.841589649988700117, -7.294998899090099798 ) ) ;
#68792 = CARTESIAN_POINT ( 'NONE',  ( 11.50962052873067520, 3.830320465062102109, -6.639752069194234885 ) ) ;
#68793 = CARTESIAN_POINT ( 'NONE',  ( 18.28026264019201363, -2.471821293434737665, 12.35517058147370761 ) ) ;
#68794 = ORIENTED_EDGE ( 'NONE', *, *, #48870, .F. ) ;
#68795 = VERTEX_POINT ( 'NONE', #18933 ) ;
#68796 = DIRECTION ( 'NONE',  ( 0.000000000000000000, 0.000000000000000000, 1.000000000000000000 ) ) ;
#68797 = LINE ( 'NONE', #41215, #40299 ) ;
#68798 = CARTESIAN_POINT ( 'NONE',  ( 4.900006121741999010, 1.599333684796362398, 1.229093439949826561 ) ) ;
#68799 = CARTESIAN_POINT ( 'NONE',  ( 10.18512471524999974, 5.526143977810000329, -7.556025088797999167 ) ) ;
#68800 = DIRECTION ( 'NONE',  ( -0.7071067811866525998, 0.000000000000000000, -0.7071067811864425456 ) ) ;
#68801 = CARTESIAN_POINT ( 'NONE',  ( 18.15889616939339035, 2.662482328103963791, 12.41224410776442966 ) ) ;
#68802 = CARTESIAN_POINT ( 'NONE',  ( 8.493376396436000064, 2.902501347630999984, -6.607668289109998483 ) ) ;
#68803 = CARTESIAN_POINT ( 'NONE',  ( 9.882259685352000389, 4.932708901218999742, 6.390989635557000170 ) ) ;
#68804 = ORIENTED_EDGE ( 'NONE', *, *, #13110, .F. ) ;
#68805 = CARTESIAN_POINT ( 'NONE',  ( 8.897208772779700681, 5.334183864695357435, -8.671862932165968374 ) ) ;
#68806 = ADVANCED_FACE ( 'NONE', ( #66470 ), #33984, .F. ) ;
#68807 = ORIENTED_EDGE ( 'NONE', *, *, #11583, .F. ) ;
#68808 = CARTESIAN_POINT ( 'NONE',  ( 12.52601681438820869, -3.059349880828010626, 12.30349483713085057 ) ) ;
#68809 = ADVANCED_FACE ( 'NONE', ( #18594 ), #15920, .F. ) ;
#68810 = CARTESIAN_POINT ( 'NONE',  ( 9.602342523874998648, -4.857027829858100887, -7.368808371628100318 ) ) ;
#68811 = CARTESIAN_POINT ( 'NONE',  ( 9.743561007103998861, 5.287400066955999733, 8.939966147452000911 ) ) ;
#68812 = CARTESIAN_POINT ( 'NONE',  ( 11.31524174883999834, -4.028418853626810403, 6.466884287543999577 ) ) ;
#68813 = CARTESIAN_POINT ( 'NONE',  ( 8.871410841230998656, 2.721111233225000259, -6.936528696292000085 ) ) ;
#68814 = FACE_OUTER_BOUND ( 'NONE', #34913, .T. ) ;
#68815 = CONICAL_SURFACE ( 'NONE', #38688, 13.94234652582999878, 1.233427434088239627 ) ;
#68816 = CARTESIAN_POINT ( 'NONE',  ( 10.51810807141099779, 4.059045408506610109, -8.776647962565998995 ) ) ;
#68817 = CARTESIAN_POINT ( 'NONE',  ( 10.82459575937373586, 5.732063870690240925, -7.156463326781315359 ) ) ;
#68818 = CARTESIAN_POINT ( 'NONE',  ( 11.59999999999999787, 3.125502297258556439, -7.869208573981370414 ) ) ;
#68819 = CARTESIAN_POINT ( 'NONE',  ( 9.383148997457999130, 5.167567567567999731, 6.822293592207000934 ) ) ;
#68820 = B_SPLINE_CURVE_WITH_KNOTS ( 'NONE', 3,
 ( #53950, #49750, #6745, #32982 ),
 .UNSPECIFIED., .F., .F.,
 ( 4, 4 ),
 ( 0.000000000000000000, 1.000000000000000000 ),
 .UNSPECIFIED. ) ;
#68821 = CARTESIAN_POINT ( 'NONE',  ( 11.53937265905000054, -3.642773248484000082, 11.02530338024999956 ) ) ;
#68822 = EDGE_LOOP ( 'NONE', ( #12424, #2968, #40716, #20195 ) ) ;
#68823 = DIRECTION ( 'NONE',  ( -1.000000000000000000, 0.000000000000000000, 0.000000000000000000 ) ) ;
#68824 = CARTESIAN_POINT ( 'NONE',  ( 0.000000000000000000, -2.533699434757234137, 1.460905701136922197 ) ) ;
#68825 = CARTESIAN_POINT ( 'NONE',  ( 11.50001496185000249, 12.52500000000000036, 0.000000000000000000 ) ) ;
#68826 = DIRECTION ( 'NONE',  ( 0.000000000000000000, 0.3146293386371170064, -0.9492146118074512584 ) ) ;
#68827 = EDGE_CURVE ( 'NONE', #31041, #51438, #45309, .T. ) ;
#68828 = CARTESIAN_POINT ( 'NONE',  ( 11.09999999999999964, 5.299999998610999796, -5.148506132424000015 ) ) ;
#68829 = CARTESIAN_POINT ( 'NONE',  ( 10.42380110216399913, -4.973546009874400653, -6.905442784147899360 ) ) ;
#68830 = VERTEX_POINT ( 'NONE', #47910 ) ;
#68831 = VECTOR ( 'NONE', #46070, 1000.000000000000000 ) ;
#68832 = CARTESIAN_POINT ( 'NONE',  ( 11.27769289846838241, 2.954326301843319680, -7.824982657629016458 ) ) ;
#68833 = EDGE_CURVE ( 'NONE', #42930, #4322, #61053, .T. ) ;
#68834 = CARTESIAN_POINT ( 'NONE',  ( 8.592635841230999105, 3.856772556595000179, 5.521246073317000125 ) ) ;
#68837 = CARTESIAN_POINT ( 'NONE',  ( 13.64506009312500190, -9.630614656729999723, -7.923290881757000470 ) ) ;
#68836 = CARTESIAN_POINT ( 'NONE',  ( 9.269689158774999882, 3.135494838036999798, -8.598037907310999373 ) ) ;
#68835 = UNCERTAINTY_MEASURE_WITH_UNIT (LENGTH_MEASURE( 1.000000000000000082E-05 ), #360, 'distance_accuracy_value', 'NONE');
#68838 = CARTESIAN_POINT ( 'NONE',  ( 18.14470825305572532, -2.707255376881378961, 13.62731588230026070 ) ) ;
#68839 = EDGE_LOOP ( 'NONE', ( #25657, #2348, #55528, #940 ) ) ;
#68840 = CARTESIAN_POINT ( 'NONE',  ( 9.442087588264000075, 4.742492734433000123, 8.809983635807000724 ) ) ;
#68841 = CARTESIAN_POINT ( 'NONE',  ( 18.17891560871130707, -2.542711950176887559, -13.66427582110434713 ) ) ;
#68842 = CARTESIAN_POINT ( 'NONE',  ( 10.57980110216399972, 3.260758259645400337, 7.951464549725199227 ) ) ;
#68843 = FACE_OUTER_BOUND ( 'NONE', #59703, .T. ) ;
#68844 = CARTESIAN_POINT ( 'NONE',  ( 9.160311019873999427, -4.122021308488999836, 9.013573548576999883 ) ) ;
#68845 = EDGE_LOOP ( 'NONE', ( #36689, #5561, #38758, #42911, #21624, #32088, #49010, #5390, #14573, #49968 ) ) ;
#68846 = CARTESIAN_POINT ( 'NONE',  ( 8.674239158774001979, 5.983047240001000411, 7.440798119034999658 ) ) ;
#68848 = CARTESIAN_POINT ( 'NONE',  ( 10.37902717885803483, 2.650237472150223095, -7.263327126957213054 ) ) ;
#68847 = CARTESIAN_POINT ( 'NONE',  ( 13.70003001321900449, 10.31266399190333516, 7.179884396236115407 ) ) ;
#68849 = CARTESIAN_POINT ( 'NONE',  ( 7.611539800697518565, -4.772443708916318528, 5.941223257842239036 ) ) ;
#68850 = DIRECTION ( 'NONE',  ( 0.000000000000000000, 0.9553735099700838562, -0.2954005017724949944 ) ) ;
#68851 = CARTESIAN_POINT ( 'NONE',  ( 1.023245171504000073, -3.085119672805999524, 1.050391531144999835 ) ) ;
#68852 = ORIENTED_EDGE ( 'NONE', *, *, #5864, .F. ) ;
#68853 = CARTESIAN_POINT ( 'NONE',  ( 5.771693173016667622, 0.7554284705563509839, -1.310679582531385945 ) ) ;
#68854 = CARTESIAN_POINT ( 'NONE',  ( 10.92795525820100089, -4.094749303624469761, 8.498986197235801399 ) ) ;
#68855 = CARTESIAN_POINT ( 'NONE',  ( 9.298033738970000073, 4.087077023028999001, 9.429414864145000408 ) ) ;
#68856 = CARTESIAN_POINT ( 'NONE',  ( 10.32949413291699869, 4.912929163218899831, 7.916546720849799712 ) ) ;
#68857 = ORIENTED_EDGE ( 'NONE', *, *, #47267, .T. ) ;
#68858 = DIRECTION ( 'NONE',  ( 0.7660444431251208774, 4.730414054088128888E-08, 0.6427876096792169980 ) ) ;
#68859 = CARTESIAN_POINT ( 'NONE',  ( 12.70926349491442764, 1.766754859226804086, -12.47551934520473083 ) ) ;
#68860 = CARTESIAN_POINT ( 'NONE',  ( 11.96989666366029859, -4.058428102321880004, 6.185029684353999357 ) ) ;
#68861 = B_SPLINE_CURVE_WITH_KNOTS ( 'NONE', 3,
 ( #62329, #67560, #20366, #14783, #20711, #46255, #36102, #14444, #30185, #51492 ),
 .UNSPECIFIED., .F., .F.,
 ( 4, 2, 2, 2, 4 ),
 ( 0.1254132184345819190, 0.3127269071678268619, 0.5000405959010718604, 0.6873542846343168033, 0.8746679733675617463 ),
 .UNSPECIFIED. ) ;
#68862 = CARTESIAN_POINT ( 'NONE',  ( 24.67921310950000091, -12.29514723793999842, -2.979192343402000009 ) ) ;
#68863 = AXIS2_PLACEMENT_3D ( 'NONE', #50453, #34390, #7113 ) ;
#68864 = CARTESIAN_POINT ( 'NONE',  ( 18.15341532599041230, -2.105586285009643177, 13.84075898842494468 ) ) ;
#68865 = CARTESIAN_POINT ( 'NONE',  ( 10.90000037895999796, 0.2999996193951000034, 9.776630289319001577 ) ) ;
#68866 = ORIENTED_EDGE ( 'NONE', *, *, #56041, .T. ) ;
#68867 = CARTESIAN_POINT ( 'NONE',  ( 10.97755399909358154, 4.133346405062088280, 6.221473734489901375 ) ) ;
#68868 = B_SPLINE_CURVE_WITH_KNOTS ( 'NONE', 3,
 ( #48419, #27443, #59940, #69056, #16936, #53326 ),
 .UNSPECIFIED., .F., .F.,
 ( 4, 2, 4 ),
 ( 0.000000000000000000, 0.5000000000000000000, 1.000000000000000000 ),
 .UNSPECIFIED. ) ;
#68869 = FACE_OUTER_BOUND ( 'NONE', #40586, .T. ) ;
#68870 = ORIENTED_EDGE ( 'NONE', *, *, #14134, .F. ) ;
#68871 = SURFACE_STYLE_FILL_AREA ( #68180 ) ;
#68872 = CARTESIAN_POINT ( 'NONE',  ( 11.78594988689359901, 4.393436444036099786, 6.728309553046099012 ) ) ;
#68873 = MECHANICAL_DESIGN_GEOMETRIC_PRESENTATION_REPRESENTATION (  '', ( #10781 ), #67711 ) ;
#68874 = CARTESIAN_POINT ( 'NONE',  ( 6.166666667118732015, -12.50864712907674381, 2.924698073458500414 ) ) ;
#68875 = EDGE_CURVE ( 'NONE', #55008, #10995, #38610, .T. ) ;
#68876 = CARTESIAN_POINT ( 'NONE',  ( 10.22440590001000160, 5.317411003666999925, -8.272452263128000638 ) ) ;
#68877 = CARTESIAN_POINT ( 'NONE',  ( 8.166615904750996080, 4.665939084510003276, 6.165875187757999143 ) ) ;
#68878 = CARTESIAN_POINT ( 'NONE',  ( 9.632185590920999019, -5.638162562978999759, 6.476633609657000079 ) ) ;
#68879 = CARTESIAN_POINT ( 'NONE',  ( 18.10066919781365513, -0.4738025322793328886, -12.59109159930368627 ) ) ;
#68880 = AXIS2_PLACEMENT_3D ( 'NONE', #34134, #44285, #50547 ) ;
#68881 = CARTESIAN_POINT ( 'NONE',  ( 9.041114868689660966, 4.912818212989734867, 8.494533580134559614 ) ) ;
#68882 = CARTESIAN_POINT ( 'NONE',  ( 10.74795391537419853, -3.169881940022800215, -8.063786182297898009 ) ) ;
#68883 = CARTESIAN_POINT ( 'NONE',  ( 8.149357780409999918, 2.583668273793999770, 6.684750595573999199 ) ) ;
#68884 = EDGE_LOOP ( 'NONE', ( #9187, #66547, #5398, #6792 ) ) ;
#68885 = CARTESIAN_POINT ( 'NONE',  ( 11.10000000000000320, 2.503699319922003674, -6.700110939026191481 ) ) ;
#68886 = DIRECTION ( 'NONE',  ( 1.000000000000000000, 0.000000000000000000, 0.000000000000000000 ) ) ;
#68887 = CARTESIAN_POINT ( 'NONE',  ( 8.561977803070984550, 2.916400247641351751, -6.350095013862320670 ) ) ;
#68888 = CARTESIAN_POINT ( 'NONE',  ( 11.09999999999999964, -2.700000000000000178, -5.157071250680000496 ) ) ;
#68889 = DIRECTION ( 'NONE',  ( 0.000000000000000000, 0.000000000000000000, 1.000000000000000000 ) ) ;
#68891 = CARTESIAN_POINT ( 'NONE',  ( 10.93665077113000095, 8.761693334770001229, 6.467187816040000037 ) ) ;
#68890 = B_SPLINE_CURVE_WITH_KNOTS ( 'NONE', 3,
 ( #19125, #40449, #34191, #61775 ),
 .UNSPECIFIED., .F., .F.,
 ( 4, 4 ),
 ( 0.000000000000000000, 1.000000000000000000 ),
 .UNSPECIFIED. ) ;
#68892 = CIRCLE ( 'NONE', #61075, 0.4999999999999997224 ) ;
#68893 = CARTESIAN_POINT ( 'NONE',  ( 12.37275785088829316, -0.4515912411692236117, -12.68919663782859963 ) ) ;
#68894 = DIRECTION ( 'NONE',  ( 0.000000000000000000, 1.000000000000000000, 0.000000000000000000 ) ) ;
#68895 = EDGE_CURVE ( 'NONE', #11014, #43802, #1863, .T. ) ;
#68896 = ORIENTED_EDGE ( 'NONE', *, *, #35553, .F. ) ;
#68897 = CARTESIAN_POINT ( 'NONE',  ( 24.62774583285499830, 8.736962890587999908, 9.042103898172999976 ) ) ;
#68898 = EDGE_CURVE ( 'NONE', #59588, #7219, #57797, .T. ) ;
#68899 = CARTESIAN_POINT ( 'NONE',  ( 10.41690035061499842, -3.695660922043800145, -8.600505223349999895 ) ) ;
#68900 = DIRECTION ( 'NONE',  ( 1.000000000000000000, 0.000000000000000000, 0.000000000000000000 ) ) ;
#68901 = CARTESIAN_POINT ( 'NONE',  ( 9.075489683949001574, -4.020837068201999820, 8.948702918089999514 ) ) ;
#68902 = CARTESIAN_POINT ( 'NONE',  ( 11.76902897915239876, -3.778278678798900447, 6.662660017635100296 ) ) ;
#68903 = EDGE_CURVE ( 'NONE', #7230, #3060, #52108, .T. ) ;
#68904 = CARTESIAN_POINT ( 'NONE',  ( 12.17712767754846759, 0.3597466176220713852, 12.59486741915706531 ) ) ;
#68905 = CARTESIAN_POINT ( 'NONE',  ( 0.4006366850170999805, -2.512770725774000180, 2.251027108384000108 ) ) ;
#68906 = CARTESIAN_POINT ( 'NONE',  ( 4.921193962081806816, -0.4916051705834446062, -1.093023166939333990 ) ) ;
#68907 = CARTESIAN_POINT ( 'NONE',  ( 12.08117318674009688, 2.436835578774657396, 12.36211850556986569 ) ) ;
#68908 = DIRECTION ( 'NONE',  ( 1.000000000000000000, 0.000000000000000000, 0.000000000000000000 ) ) ;
#68909 = CARTESIAN_POINT ( 'NONE',  ( 10.45257053952200010, 3.605640676136899980, -6.577269499510100204 ) ) ;
#68910 = CARTESIAN_POINT ( 'NONE',  ( 11.90028836426310122, 11.81686663804764770, -4.153560932554616336 ) ) ;
#68911 = CARTESIAN_POINT ( 'NONE',  ( 10.11548915876999999, 2.489190114737999782, -6.434635778494999236 ) ) ;
#68912 = CARTESIAN_POINT ( 'NONE',  ( 9.225367640781000134, 4.603017491986999943, -6.371835875489000323 ) ) ;
#68914 = CARTESIAN_POINT ( 'NONE',  ( 1.700000000000000178, 0.000000000000000000, 0.000000000000000000 ) ) ;
#68913 = LINE ( 'NONE', #51806, #67629 ) ;
#68915 = CARTESIAN_POINT ( 'NONE',  ( 11.28830977893788123, -4.976598135215292373, -6.673569913327194847 ) ) ;
#68916 = VERTEX_POINT ( 'NONE', #15747 ) ;
#68917 = AXIS2_PLACEMENT_3D ( 'NONE', #59059, #10468, #37389 ) ;
#68918 = B_SPLINE_CURVE_WITH_KNOTS ( 'NONE', 3,
 ( #54747, #35412, #6846, #28181, #24221, #65574, #17697, #8492, #39021, #60339 ),
 .UNSPECIFIED., .F., .F.,
 ( 4, 2, 2, 2, 4 ),
 ( 0.000000000000000000, 0.1968496138483742108, 0.3936992276967484217, 0.5905488415451226603, 0.7873984553934968433 ),
 .UNSPECIFIED. ) ;
#68919 = CARTESIAN_POINT ( 'NONE',  ( 12.40293124239839173, 0.4784650741312070354, 12.68786664693105593 ) ) ;
#68920 = EDGE_CURVE ( 'NONE', #2068, #38985, #42658, .T. ) ;
#68921 = DIRECTION ( 'NONE',  ( 0.000000000000000000, -1.000000000000000000, 0.000000000000000000 ) ) ;
#68922 = MECHANICAL_DESIGN_GEOMETRIC_PRESENTATION_REPRESENTATION (  '', ( #5250 ), #14192 ) ;
#68923 = CARTESIAN_POINT ( 'NONE',  ( 10.37874387220000116, -4.882732524430000609, 6.350796477317000921 ) ) ;
#68924 = CARTESIAN_POINT ( 'NONE',  ( 10.23557120343299864, 3.957971921952620598, 6.634008278083699750 ) ) ;
#68925 = FACE_OUTER_BOUND ( 'NONE', #51692, .T. ) ;
#68927 = CARTESIAN_POINT ( 'NONE',  ( 12.22230712497533034, -2.273859679217654861, 13.71882920742291745 ) ) ;
#68926 = VECTOR ( 'NONE', #2025, 1000.000000000000114 ) ;
#68928 = CARTESIAN_POINT ( 'NONE',  ( 12.18211070746967728, 2.551853945066973939, 13.66227842075671184 ) ) ;
#68929 = CARTESIAN_POINT ( 'NONE',  ( 8.155024894413680059, 3.133330062225388346, 6.255279687528450872 ) ) ;
#68930 = EDGE_LOOP ( 'NONE', ( #9963, #43112, #64798 ) ) ;
#68931 = CARTESIAN_POINT ( 'NONE',  ( 4.911164598758000821, -1.268823648606999921, -0.1298529817190000046 ) ) ;
#68932 = CARTESIAN_POINT ( 'NONE',  ( 9.883925467520999320, -5.276153033933000280, -7.411581555133209598 ) ) ;
#68933 = AXIS2_PLACEMENT_3D ( 'NONE', #30180, #56045, #13411 ) ;
#68934 = FACE_OUTER_BOUND ( 'NONE', #67206, .T. ) ;
#68935 = CARTESIAN_POINT ( 'NONE',  ( 10.86325056272499978, -3.107965259299500183, 7.486779603004729111 ) ) ;
#68936 = CARTESIAN_POINT ( 'NONE',  ( 18.17829451895831738, 2.452078260301032042, -12.46263202712694707 ) ) ;
#68937 = DIRECTION ( 'NONE',  ( -3.751129491691894952E-06, -0.2588385419140925015, 0.9659206019159729539 ) ) ;
#68938 = CARTESIAN_POINT ( 'NONE',  ( 18.13624051175171203, 2.730018211965808295, 12.39499564928988207 ) ) ;
#68940 = CIRCLE ( 'NONE', #10901, 1.775000326287000219 ) ;
#68939 = CARTESIAN_POINT ( 'NONE',  ( 7.778861800931997195, 3.520498707107000858, 6.411393241748998051 ) ) ;
#68941 = CARTESIAN_POINT ( 'NONE',  ( 11.63459739833729856, -4.823158118387800286, 7.174999999999999822 ) ) ;
#68942 = CARTESIAN_POINT ( 'NONE',  ( 24.78000005981499854, 12.27029765734999955, 2.912405417372000205 ) ) ;
#68943 = CARTESIAN_POINT ( 'NONE',  ( 12.43745875767134734, 1.881346041122103907, 13.87306493545927033 ) ) ;
#68944 = B_SPLINE_SURFACE_WITH_KNOTS ( 'NONE', 3, 3, ( 
 ( #39322, #66909, #55400, #66224 ),
 ( #49456, #28851, #23579, #49810 ),
 ( #18347, #65532, #60989, #7496 ),
 ( #7157, #28493, #44584, #13104 ),
 ( #29187, #23928, #65877, #50498 ),
 ( #45264, #66569, #67939, #35458 ),
 ( #41722, #45939, #67591, #67251 ),
 ( #61673, #19024, #36474, #46288 ),
 ( #56432, #52208, #9207, #56782 ) ),
 .UNSPECIFIED., .F., .F., .F.,
 ( 4, 1, 1, 1, 1, 1, 4 ),
 ( 4, 4 ),
 ( 0.05136528901823000232, 0.1666666666667000196, 0.3333333333333000081, 0.5000000000000000000, 0.6666666666667000474, 0.8333333333333000637, 0.9784615765758000183 ),
 ( -0.1917159053268999991, 1.191863452461999984 ),
 .UNSPECIFIED. ) ;
#68945 = CARTESIAN_POINT ( 'NONE',  ( 7.924878289113923557, -5.349357204871147076, 7.500005630225521358 ) ) ;
#68946 = FACE_OUTER_BOUND ( 'NONE', #40949, .T. ) ;
#68947 = CARTESIAN_POINT ( 'NONE',  ( 11.08810207955139937, -4.796537143354000499, -7.174999999999999822 ) ) ;
#68948 = DIRECTION ( 'NONE',  ( 0.000000000000000000, -1.000000000000000000, 0.000000000000000000 ) ) ;
#68949 = ORIENTED_EDGE ( 'NONE', *, *, #56776, .F. ) ;
#68950 = CARTESIAN_POINT ( 'NONE',  ( 8.406645280410000254, 3.807713920470999991, -9.221758713517999695 ) ) ;
#68951 = CARTESIAN_POINT ( 'NONE',  ( 10.93210941423800087, -3.358814833524500276, 8.082391773166900606 ) ) ;
#68952 = EDGE_LOOP ( 'NONE', ( #52379, #22030, #6399, #40073, #39790 ) ) ;
#68953 = CARTESIAN_POINT ( 'NONE',  ( 13.09019624054850617, 12.38961571551778640, 1.836606440307306354 ) ) ;
#68954 = CARTESIAN_POINT ( 'NONE',  ( 10.27610941423800028, -3.155589807313900153, -6.733017893878099791 ) ) ;
#68955 = EDGE_LOOP ( 'NONE', ( #30648, #29606, #17088, #63920 ) ) ;
#68956 = FACE_OUTER_BOUND ( 'NONE', #28585, .T. ) ;
#68957 = CARTESIAN_POINT ( 'NONE',  ( 8.845310841232000953, 5.851083642416999631, -7.072167224702999633 ) ) ;
#68958 = EDGE_CURVE ( 'NONE', #64347, #45997, #219, .T. ) ;
#68959 = CARTESIAN_POINT ( 'NONE',  ( 17.85726930274100255, -3.190143309604999811, 11.45065656613999927 ) ) ;
#68960 = ADVANCED_FACE ( 'NONE', ( #29354 ), #39708, .F. ) ;
#68961 = CARTESIAN_POINT ( 'NONE',  ( 9.317462135714000837, -5.100000000000000533, 6.571291218949999902 ) ) ;
#68962 = CARTESIAN_POINT ( 'NONE',  ( 9.789763540182331525, -4.327184855449096368, -6.282534154164603812 ) ) ;
#68963 = CARTESIAN_POINT ( 'NONE',  ( 9.557169810767971896, -3.796486612318636933, 6.292830123317686208 ) ) ;
#68964 = B_SPLINE_CURVE_WITH_KNOTS ( 'NONE', 3,
 ( #19905, #23858, #34364, #14999 ),
 .UNSPECIFIED., .F., .F.,
 ( 4, 4 ),
 ( 0.000000000000000000, 1.000000000000000000 ),
 .UNSPECIFIED. ) ;
#68965 = CARTESIAN_POINT ( 'NONE',  ( 11.09999999999999964, 6.593648131501000265, 5.598803515845999890 ) ) ;
#68966 = ORIENTED_EDGE ( 'NONE', *, *, #62917, .F. ) ;
#68967 = AXIS2_PLACEMENT_3D ( 'NONE', #54092, #21927, #43265 ) ;
#68968 = CARTESIAN_POINT ( 'NONE',  ( 8.880270280412998929, 4.146787477634999775, -5.941926545671999627 ) ) ;
#68969 = EDGE_LOOP ( 'NONE', ( #21102, #16320, #46612, #23131, #64009, #64666, #48662 ) ) ;
#68970 = AXIS2_PLACEMENT_3D ( 'NONE', #15809, #417, #58119 ) ;
#68971 = CARTESIAN_POINT ( 'NONE',  ( 10.89393020684959978, 2.750000000000000000, -7.500000000000000000 ) ) ;
#68972 = ORIENTED_EDGE ( 'NONE', *, *, #52834, .T. ) ;
#68973 = CARTESIAN_POINT ( 'NONE',  ( 8.921417874593998931, 2.822750429186000165, 6.999532383170999239 ) ) ;
#68974 = CARTESIAN_POINT ( 'NONE',  ( 18.12879050829621619, -2.748092781515380167, -12.39029782533441804 ) ) ;
#68975 = CARTESIAN_POINT ( 'NONE',  ( 10.22726354018266370, 4.629523725463627670, -6.407767014557179230 ) ) ;
#68976 = CIRCLE ( 'NONE', #31017, 13.17499999999999538 ) ;
#68977 = CARTESIAN_POINT ( 'NONE',  ( 18.14750831225986261, -2.299919533022120710, -12.49594326303513370 ) ) ;
#68978 = CARTESIAN_POINT ( 'NONE',  ( 8.576923877145999242, 3.399999999999999911, 5.924121105096999962 ) ) ;
#68979 = ORIENTED_EDGE ( 'NONE', *, *, #1062, .T. ) ;
#68980 = CARTESIAN_POINT ( 'NONE',  ( 12.05989062672900047, 12.07342271643000053, -3.473919584753000223 ) ) ;
#68981 = CARTESIAN_POINT ( 'NONE',  ( 18.01587601577499953, 11.44428158143999852, -4.450268217599000486 ) ) ;
#68982 = DIRECTION ( 'NONE',  ( -1.000000000000000000, 0.000000000000000000, 0.000000000000000000 ) ) ;
#68983 = CIRCLE ( 'NONE', #32172, 13.89999852641999922 ) ;
#68984 = CARTESIAN_POINT ( 'NONE',  ( -15.86200481174999943, 11.00717859340000082, 1.432487142323000118 ) ) ;
#68985 = EDGE_CURVE ( 'NONE', #11689, #59582, #22702, .T. ) ;
#68986 = CARTESIAN_POINT ( 'NONE',  ( 9.146614158775999925, 2.981992329588000423, -5.895876591910999664 ) ) ;
#68987 = CARTESIAN_POINT ( 'NONE',  ( 16.00000001290300133, -11.86188960208913912, 3.298666395463871304 ) ) ;
#68988 = CARTESIAN_POINT ( 'NONE',  ( 9.858853446676000942, -2.668079545448999834, -7.206971019603000350 ) ) ;
#68989 = EDGE_LOOP ( 'NONE', ( #31451, #14108 ) ) ;
#68990 = VERTEX_POINT ( 'NONE', #23405 ) ;
#68991 = AXIS2_PLACEMENT_3D ( 'NONE', #44730, #3091, #65687 ) ;
#68992 = CYLINDRICAL_SURFACE ( 'NONE', #63844, 1.250000000000000222 ) ;
#68993 = CARTESIAN_POINT ( 'NONE',  ( 10.99999999997000089, 4.000000000000000000, -7.500000000000000000 ) ) ;
#68994 = CARTESIAN_POINT ( 'NONE',  ( 1.155140132541250031, 0.9161175952574702741, 3.408904368339106927 ) ) ;
#68995 = FACE_OUTER_BOUND ( 'NONE', #22296, .T. ) ;
#68996 = CARTESIAN_POINT ( 'NONE',  ( 10.51414141025500015, 4.615773412711500434, -8.596754040696000132 ) ) ;
#68997 = CARTESIAN_POINT ( 'NONE',  ( 10.04193802597399987, 3.549239910423600097, -6.759376420744099612 ) ) ;
#68999 = CARTESIAN_POINT ( 'NONE',  ( 4.399663372146739526, 1.348965324306665048, -0.3595321560971826425 ) ) ;
#68998 = CARTESIAN_POINT ( 'NONE',  ( 9.623101285863999266, -4.646739515667500875, 8.268485718282699182 ) ) ;
#69000 = CARTESIAN_POINT ( 'NONE',  ( 8.493436541922999794, -2.902501512378997894, 6.607638123744003167 ) ) ;
#69001 = ORIENTED_EDGE ( 'NONE', *, *, #68744, .T. ) ;
#69002 = CARTESIAN_POINT ( 'NONE',  ( 9.810596873515665450, 3.370476274536378103, -6.407767014557176566 ) ) ;
#69003 = ADVANCED_FACE ( 'NONE', ( #23744 ), #34964, .F. ) ;
#69004 = CARTESIAN_POINT ( 'NONE',  ( 8.030239402831002238, -2.905307396403002507, 6.399703979581998325 ) ) ;
#69005 = CARTESIAN_POINT ( 'NONE',  ( 9.507063610504999929, 4.524705472883399970, 6.333351572150998976 ) ) ;
#69006 = DIRECTION ( 'NONE',  ( 1.000000000000000000, 0.000000000000000000, 0.000000000000000000 ) ) ;
#69007 = CARTESIAN_POINT ( 'NONE',  ( 9.347248564704999652, -4.028326926800000152, 9.469437404464001062 ) ) ;
#69008 = LINE ( 'NONE', #5381, #48638 ) ;
#69009 = CARTESIAN_POINT ( 'NONE',  ( 16.04750315638899849, -3.679714098878999806, -11.11063745184000062 ) ) ;
#69010 = CARTESIAN_POINT ( 'NONE',  ( 13.75961700471900073, 8.905065757320999253, 7.452879173751000508 ) ) ;
#69011 = CARTESIAN_POINT ( 'NONE',  ( 11.09999999999999964, 4.000000000000000000, -7.500000000000000000 ) ) ;
#69012 = CARTESIAN_POINT ( 'NONE',  ( 9.586013376692998023, -4.772923352651200268, -7.107192877568799361 ) ) ;
#69013 = CARTESIAN_POINT ( 'NONE',  ( 6.355377242029001117, 0.8975578082598999474, -1.162289642979999815 ) ) ;
#69014 = CARTESIAN_POINT ( 'NONE',  ( 6.999999999999999112, 8.814407058729466726, -4.633674960078741023 ) ) ;
#69015 = CARTESIAN_POINT ( 'NONE',  ( 18.28081516007887330, 2.296096720429526616, 12.39048987307994842 ) ) ;
#69016 = CARTESIAN_POINT ( 'NONE',  ( 7.760743125788000185, -3.157312404059000155, 6.445099350801999805 ) ) ;
#69017 = VERTEX_POINT ( 'NONE', #6451 ) ;
#69018 = CARTESIAN_POINT ( 'NONE',  ( 12.26342954938197316, 0.3125562302819458460, -12.69484091569604089 ) ) ;
#69019 = B_SPLINE_CURVE_WITH_KNOTS ( 'NONE', 3,
 ( #7598, #65284, #33489, #28237, #49553, #1665, #28947, #28593, #50251, #2353, #49904, #23335, #44676, #23676, #65970, #45014, #66319, #18442 ),
 .UNSPECIFIED., .F., .F.,
 ( 4, 2, 2, 2, 2, 2, 2, 2, 4 ),
 ( 0.000000000000000000, 0.1250000000000000000, 0.2500000000000000000, 0.3750000000000000000, 0.5000000000000000000, 0.6250000000000000000, 0.7500000000000000000, 0.8750000000000000000, 1.000000000000000000 ),
 .UNSPECIFIED. ) ;
#69020 = CARTESIAN_POINT ( 'NONE',  ( 10.85056919669530018, 4.830699382454300306, -7.745432529082900253 ) ) ;
#69021 = CARTESIAN_POINT ( 'NONE',  ( 11.09999999999999964, -4.000000000000000000, -7.500000000000000000 ) ) ;
#69023 = CARTESIAN_POINT ( 'NONE',  ( 11.59999999999999964, 4.000000000000000000, -7.500000000000000000 ) ) ;
#69022 = AXIS2_PLACEMENT_3D ( 'NONE', #15518, #31946, #53261 ) ;
#69024 = CARTESIAN_POINT ( 'NONE',  ( 10.26088874562948128, 3.646602187524448535, -8.814783671671067466 ) ) ;
#69025 = VERTEX_POINT ( 'NONE', #32353 ) ;
#69026 = CARTESIAN_POINT ( 'NONE',  ( 10.09393020684899867, 5.250000000000000000, -7.500000000000000000 ) ) ;
#69027 = CONTEXT_DEPENDENT_SHAPE_REPRESENTATION ( #44539, #364 ) ;
#69028 = CARTESIAN_POINT ( 'NONE',  ( 11.35545123989519922, -3.524778630617700248, -8.417769225118700405 ) ) ;
#69029 = CARTESIAN_POINT ( 'NONE',  ( 24.48564577462000003, -8.805068883974998428, -8.922048782936000677 ) ) ;
#69030 = CARTESIAN_POINT ( 'NONE',  ( 10.51059687351600225, -3.370476274536376771, 6.407767014557176566 ) ) ;
#69031 = CARTESIAN_POINT ( 'NONE',  ( 7.589309517775307157, 5.301171624786114478, -7.912166694486026053 ) ) ;
#69032 = AXIS2_PLACEMENT_3D ( 'NONE', #19266, #67153, #2501 ) ;
#69033 = CARTESIAN_POINT ( 'NONE',  ( 12.99165415090800124, 12.32813973498000060, 1.877091699536999947 ) ) ;
#69034 = VERTEX_POINT ( 'NONE', #6799 ) ;
#69035 = CARTESIAN_POINT ( 'NONE',  ( 9.854949224988001077, -2.800315695760000168, 9.013807298610000629 ) ) ;
#69036 = CARTESIAN_POINT ( 'NONE',  ( 17.69878333211497434, 3.108595074582393369, -13.52536937155546504 ) ) ;
#69037 = ORIENTED_EDGE ( 'NONE', *, *, #64955, .F. ) ;
#69038 = CARTESIAN_POINT ( 'NONE',  ( 7.000000000000000000, 0.3230303992915000144, -3.000000000000000000 ) ) ;
#69039 = CARTESIAN_POINT ( 'NONE',  ( 9.112168146794999757, -2.368260286481999710, 7.410200011629000549 ) ) ;
#69040 = CARTESIAN_POINT ( 'NONE',  ( 18.39984528086700166, -1.003641614260999896E-13, 7.549516567450998842E-14 ) ) ;
#69041 = AXIS2_PLACEMENT_3D ( 'NONE', #8106, #2853, #44830 ) ;
#69042 = EDGE_CURVE ( 'NONE', #63477, #52918, #1836, .T. ) ;
#69043 = ORIENTED_EDGE ( 'NONE', *, *, #3351, .F. ) ;
#69044 = CARTESIAN_POINT ( 'NONE',  ( 27.64127793187000037, -5.599999999999999645, 6.571291218949999902 ) ) ;
#69045 = EDGE_CURVE ( 'NONE', #54862, #15717, #28136, .T. ) ;
#69046 = CARTESIAN_POINT ( 'NONE',  ( 18.14887404798968618, 0.1995702674084748607, -12.69797248607429374 ) ) ;
#69047 = CARTESIAN_POINT ( 'NONE',  ( 9.552263540183332680, -2.907767014557177898, -8.129523725463625894 ) ) ;
#69048 = EDGE_CURVE ( 'NONE', #62522, #7389, #40939, .T. ) ;
#69049 = CARTESIAN_POINT ( 'NONE',  ( 7.219277519215202332, 4.353512721038384825, -8.815217796131234351 ) ) ;
#69050 = ORIENTED_EDGE ( 'NONE', *, *, #16478, .T. ) ;
#69051 = CARTESIAN_POINT ( 'NONE',  ( 10.46933016578999975, -4.988498232033999891, 6.213103211926000569 ) ) ;
#69052 = EDGE_CURVE ( 'NONE', #26809, #8503, #43175, .T. ) ;
#69053 = CARTESIAN_POINT ( 'NONE',  ( 11.59999999999999964, 3.850275034462829815, 8.514310854298580367 ) ) ;
#69054 = LINE ( 'NONE', #11692, #60121 ) ;
#69055 = EDGE_LOOP ( 'NONE', ( #18133, #44254 ) ) ;
#69056 = CARTESIAN_POINT ( 'NONE',  ( 11.53935385204243147, -3.267863779230331112, 11.38835623221634386 ) ) ;
#69057 = B_SPLINE_CURVE_WITH_KNOTS ( 'NONE', 3,
 ( #25846, #9077, #26197, #25504, #46833, #15361 ),
 .UNSPECIFIED., .F., .F.,
 ( 4, 1, 1, 4 ),
 ( 0.000000000000000000, 0.1550125193756538011, 0.7488612380692285520, 1.000000000000000000 ),
 .UNSPECIFIED. ) ;
#69058 = ORIENTED_EDGE ( 'NONE', *, *, #18274, .T. ) ;
#69059 = CARTESIAN_POINT ( 'NONE',  ( 9.842836772853271299, -2.713977296312396259, -7.027125797468761981 ) ) ;
#69060 = CARTESIAN_POINT ( 'NONE',  ( 17.91028475965239153, -1.853043856158717029, -12.46299565389693242 ) ) ;
#69061 = CARTESIAN_POINT ( 'NONE',  ( 17.60655599801540561, -0.6229596466635308749, -12.67942438339646749 ) ) ;
#69062 = CARTESIAN_POINT ( 'NONE',  ( 7.801679552337999368, 4.516824445382995989, -6.385720355065998000 ) ) ;
#69063 = CARTESIAN_POINT ( 'NONE',  ( 5.700000000000000178, 13.94845324556000143, -4.312847325879000770 ) ) ;
#69064 = CARTESIAN_POINT ( 'NONE',  ( 24.00507812729757973, 12.70419977581086712, 3.471507264481290989 ) ) ;
#69065 = EDGE_LOOP ( 'NONE', ( #31110, #82, #59515, #3450, #42928 ) ) ;
#69066 = CARTESIAN_POINT ( 'NONE',  ( 8.500365452454994752, -5.097361224984004124, 6.605627025648004746 ) ) ;
#69067 = ORIENTED_EDGE ( 'NONE', *, *, #37865, .F. ) ;
#69068 = CARTESIAN_POINT ( 'NONE',  ( 9.260906466624998501, 4.901388651757999426, 9.090324495507999814 ) ) ;
#69069 = CARTESIAN_POINT ( 'NONE',  ( 10.79701415876999882, 5.792870175253000298, -7.049262931951000510 ) ) ;
#69070 = CARTESIAN_POINT ( 'NONE',  ( 20.10000000000000142, 0.000000000000000000, 0.000000000000000000 ) ) ;
#69071 = CARTESIAN_POINT ( 'NONE',  ( 12.60210251410535420, 1.908512130997219725, -13.78126077419328332 ) ) ;
#69072 = LINE ( 'NONE', #63471, #60527 ) ;
#69073 = CARTESIAN_POINT ( 'NONE',  ( 1.699999999999999956, 2.250000000000000000, 0.000000000000000000 ) ) ;
#69074 = CIRCLE ( 'NONE', #34466, 1.350000000000000311 ) ;
#69075 = CARTESIAN_POINT ( 'NONE',  ( 6.949999692073999924, 11.00717859340000082, -1.432487142323000118 ) ) ;
#69076 = EDGE_LOOP ( 'NONE', ( #13513, #19380, #45037, #10713, #36548, #48681, #52969, #10379, #36641, #22274 ) ) ;
#69077 = AXIS2_PLACEMENT_3D ( 'NONE', #24825, #46151, #8061 ) ;
#69078 = CARTESIAN_POINT ( 'NONE',  ( 12.66331021901985032, 0.6090267839138837624, 13.88203573366629762 ) ) ;
#69079 = CARTESIAN_POINT ( 'NONE',  ( 10.94426222744800015, -4.986443098259000450, 6.687444528363699625 ) ) ;
#69080 = B_SPLINE_CURVE_WITH_KNOTS ( 'NONE', 3,
 ( #3557, #14413, #25581, #30486, #46908, #19298, #51799, #67529, #24201, #62296 ),
 .UNSPECIFIED., .F., .F.,
 ( 4, 2, 2, 2, 4 ),
 ( 0.000000000000000000, 0.2499999999999997780, 0.4999999999999995559, 0.7499999999999997780, 1.000000000000000000 ),
 .UNSPECIFIED. ) ;
#69081 = CARTESIAN_POINT ( 'NONE',  ( 21.72233714749290101, 0.000000000000000000, 0.000000000000000000 ) ) ;
#69082 = CARTESIAN_POINT ( 'NONE',  ( 8.116918146793999256, -5.773185758034999893, 7.141496747382000798 ) ) ;
#69084 = CARTESIAN_POINT ( 'NONE',  ( 13.63328756540911790, 11.47070279790940717, 2.387969831734693127 ) ) ;
#69083 = CARTESIAN_POINT ( 'NONE',  ( 13.99999999393279104, 9.282302710986076733, 8.207095416277889299 ) ) ;
#69085 = CARTESIAN_POINT ( 'NONE',  ( 11.35502763632549872, 2.839566963815999934, -6.964545474268299508 ) ) ;
#69086 = CARTESIAN_POINT ( 'NONE',  ( 10.65293113562639959, -5.100000000000000533, -6.444141223575878819 ) ) ;
#69087 = ADVANCED_FACE ( 'NONE', ( #876 ), #64826, .T. ) ;
#69088 = CARTESIAN_POINT ( 'NONE',  ( 10.03293802597399953, 3.549239910423600097, -6.759376420744099612 ) ) ;
#69089 = CARTESIAN_POINT ( 'NONE',  ( 17.81315952985430684, -0.5693054069933379813, 12.68281928773556366 ) ) ;
#69090 = B_SPLINE_SURFACE_WITH_KNOTS ( 'NONE', 1, 3, ( 
 ( #55687, #50784, #51124, #45198, #3558, #2533, #67530, #45877, #67187, #8475, #18964, #14069, #19299, #35393, #56719, #8814, #7784, #13724, #46222, #50430, #35053, #34710, #66503, #18624, #19652, #39953, #61271, #13388, #2879, #24202, #45544, #40290, #5279, #10187, #36068, #58084, #37105, #57383, #36763, #52140, #31517, #53181, #21024, #58763, #42358, #10869, #52839, #15775, #42690, #63659, #58419, #9488, #10524, #68556, #3898, #68907, #14750, #31864, #26621, #42009, #4934, #46909, #47940, #30830, #4243, #47253, #15438, #25582, #25233, #25923, #32214, #46567, #21360, #62625, #26273, #67876, #19996, #63310, #41320, #40, #4585, #68211, #47599, #20330, #41658, #9839, #62962, #63998, #16116, #20678, #37442, #15090, #36414, #57728, #31184, #52489, #381, #22392, #65730, #5620, #60494, #28339, #43729, #59799, #59451, #17853, #26961, #53528 ),
 ( #38124, #11901, #53863, #60154, #32550, #49658, #54560, #33239, #17144, #48971, #22734, #49307, #1419, #44083, #38476, #64337, #65027, #6657, #12603, #27998, #64688, #23085, #44432, #65382, #12258, #5964, #39171, #17503, #16455, #38826, #27650, #54904, #33587, #37787, #7007, #1767, #59108, #48275, #27302, #21697, #43033, #11214, #48626, #729, #22041, #43388, #16796, #11549, #32892, #54202, #6303, #1077, #8046, #66421, #7349, #2796, #34970, #13309, #29389, #55253, #67444, #56630, #13986, #67107, #23435, #2453, #55602, #44774, #61188, #62211, #19215, #39517, #51040, #51378, #33934, #45113, #39869, #56287, #34281, #23778, #28694, #8733, #2118, #30078, #8392, #24122, #50699, #34630, #55943, #40542, #45457, #66769, #66074, #24813, #18887, #45794, #40212, #18542, #61528, #61866, #29737, #19567, #3477, #13643, #7703, #35312, #3141, #24470 ) ),
 .UNSPECIFIED., .F., .F., .F.,
 ( 2, 2 ),
 ( 4, 2, 2, 2, 2, 2, 2, 2, 2, 2, 2, 2, 2, 2, 2, 2, 2, 2, 2, 2, 2, 2, 2, 2, 2, 2, 2, 2, 2, 2, 2, 2, 2, 2, 2, 2, 2, 2, 2, 2, 2, 2, 2, 2, 2, 2, 2, 2, 2, 2, 2, 2, 2, 4 ),
 ( 0.000000000000000000, 1.000000000000000000 ),
 ( 0.000000000000000000, 7.156607294609336489E-05, 0.0001431321458921867298, 0.0001789151823652334054, 0.0002146982188382801082, 0.0002325897370748034325, 0.0002504812553113267568, 0.0002862642917843734596, 0.0003220473282574201623, 0.0003578303647304668109, 0.0003936134012035135137, 0.0004293964376765602164, 0.0004651794741496068650, 0.0004830709923861301893, 0.0005009625106226535136, 0.0005725285835687469191, 0.0006440946565148403247, 0.0007156607294609336218, 0.0007872268024070270273, 0.0008587928753531204329, 0.0008945759118261670815, 0.0009303589482992137300, 0.0009661419847722603786, 0.001001925021245307027, 0.001037708057718353784, 0.001073491094191400541, 0.001145057167137493838, 0.001180840203610540595, 0.001216623240083587135, 0.001252406276556633892, 0.001288189313029680649, 0.001359755385975773946, 0.001395538422448820703, 0.001431321458921867244, 0.001467104495394914001, 0.001502887531867960758, 0.001574453604814054055, 0.001646019677760147352, 0.001681802714233194109, 0.001717585750706240866, 0.001753368787179287406, 0.001789151823652334163, 0.001860717896598427460, 0.001896500933071474000, 0.001932283969544520757, 0.001968067006017567514, 0.002003850042490614054, 0.002039633078963661028, 0.002075416115436707568, 0.002146982188382801082, 0.002182765224855847622, 0.002218548261328894163, 0.002254331297801941136, 0.002290114334274987676 ),
 .UNSPECIFIED. ) ;
#69091 = CARTESIAN_POINT ( 'NONE',  ( 6.807740044269000812, -1.061937232448999957, 0.3932159216488000375 ) ) ;
#69092 = ADVANCED_FACE ( 'NONE', ( #49450 ), #47675, .T. ) ;
#69093 = CARTESIAN_POINT ( 'NONE',  ( 23.91178178635799867, 9.488588060152000736, 9.248841913497999556 ) ) ;
#69094 = EDGE_LOOP ( 'NONE', ( #33935, #13804, #10709 ) ) ;
#69095 = CARTESIAN_POINT ( 'NONE',  ( 8.470293146793999028, -4.255646685191999623, 9.114089645792999406 ) ) ;
#69096 = CARTESIAN_POINT ( 'NONE',  ( 9.319414158774000256, 2.656512020013999997, -7.884832994446999699 ) ) ;
#69097 = CYLINDRICAL_SURFACE ( 'NONE', #46081, 2.200000000000000178 ) ;
#69098 = DIRECTION ( 'NONE',  ( 0.000000000000000000, 0.2714570858282905341, -0.9624505444715651947 ) ) ;
#69099 = ORIENTED_EDGE ( 'NONE', *, *, #44683, .F. ) ;
#69100 = B_SPLINE_CURVE_WITH_KNOTS ( 'NONE', 3,
 ( #28394, #44825, #1817, #28046, #12307, #27351, #38526, #59848, #54253, #48674, #39221, #6012, #12654, #55304, #1125, #43438 ),
 .UNSPECIFIED., .F., .F.,
 ( 4, 2, 2, 2, 2, 2, 2, 4 ),
 ( 0.000000000000000000, 0.06249999999999879263, 0.1249999999999975853, 0.2499999999999972800, 0.4999999999999981126, 0.7499999999999987788, 0.8749999999999994449, 1.000000000000000000 ),
 .UNSPECIFIED. ) ;
#69101 = CARTESIAN_POINT ( 'NONE',  ( 0.2799269853179000012, 3.021985743044000028, 1.081096232840000004 ) ) ;
#69102 = CARTESIAN_POINT ( 'NONE',  ( 7.000000000000000000, 0.2708497377871000311, -3.000000000000000000 ) ) ;
#69103 = CARTESIAN_POINT ( 'NONE',  ( 2.981521585972999766, 3.146372654723999851, -2.056384300341000060 ) ) ;
#69104 = VERTEX_POINT ( 'NONE', #34768 ) ;
#69105 = CARTESIAN_POINT ( 'NONE',  ( 12.51647491292534120, -0.6599616342124140500, -12.58270523616455350 ) ) ;
#69106 = CARTESIAN_POINT ( 'NONE',  ( 9.218291396515251535, -5.004075074800184986, -6.183516294244955525 ) ) ;
#69107 = CARTESIAN_POINT ( 'NONE',  ( 18.13174941159750730, 2.917101476509660785, -12.25768593326185574 ) ) ;
#69108 = CARTESIAN_POINT ( 'NONE',  ( 15.88832047282410720, -8.582214862760457308, -8.173711952084849131 ) ) ;
#69109 = DIRECTION ( 'NONE',  ( 0.000000000000000000, -0.9421243786071877846, -0.3352635608502960718 ) ) ;
#69110 = EDGE_LOOP ( 'NONE', ( #5582, #53234, #28286, #3360, #62733, #43925, #8633, #5677, #30531, #8414 ) ) ;
#69111 = DIRECTION ( 'NONE',  ( 0.000000000000000000, 1.000000000000000000, 0.000000000000000000 ) ) ;
#69112 = CARTESIAN_POINT ( 'NONE',  ( 7.856379719586000121, 5.390931070480998955, -6.467229401624000396 ) ) ;
#69113 = CARTESIAN_POINT ( 'NONE',  ( 8.539901661839698122, -3.276467725318618296, 5.918453690889198704 ) ) ;
#69114 = CARTESIAN_POINT ( 'NONE',  ( 10.96954340945999995, -8.070525344816001478, 6.995684484348000609 ) ) ;
#69115 = EDGE_LOOP ( 'NONE', ( #32367, #59228, #50491, #64592 ) ) ;
#69116 = CARTESIAN_POINT ( 'NONE',  ( 16.13837349797499954, -3.856691945087999951, -11.95672051617999898 ) ) ;
#69117 = CARTESIAN_POINT ( 'NONE',  ( 11.83979429613600232, 11.64688653560999931, 1.860528257274000064 ) ) ;
#69118 = ORIENTED_EDGE ( 'NONE', *, *, #2057, .T. ) ;
#69119 = CARTESIAN_POINT ( 'NONE',  ( 24.71803605778425705, 3.123403878897051289, -11.79148459578962971 ) ) ;
#69120 = DIRECTION ( 'NONE',  ( 0.000000000000000000, 0.2588190451024934280, -0.9659258262890756397 ) ) ;
#69121 = CARTESIAN_POINT ( 'NONE',  ( 7.861016604981150735, -4.181402732447497606, 6.140015153376770840 ) ) ;
#69122 = ORIENTED_EDGE ( 'NONE', *, *, #7617, .F. ) ;
#69123 = DIRECTION ( 'NONE',  ( 1.000000000000000000, 0.000000000000000000, 0.000000000000000000 ) ) ;
#69124 = CARTESIAN_POINT ( 'NONE',  ( 6.999999691988000095, 12.49999909016000110, -4.772673758002000880E-10 ) ) ;
#69125 = CIRCLE ( 'NONE', #12038, 1.500000000000000444 ) ;
#69126 = CARTESIAN_POINT ( 'NONE',  ( 11.39189666366029918, 3.947847673382490541, -8.673729056199000809 ) ) ;
#69127 = CARTESIAN_POINT ( 'NONE',  ( 8.877678275024724286, -2.921484010191843339, 8.876657601656255281 ) ) ;
#69128 = EDGE_CURVE ( 'NONE', #1971, #62373, #12401, .T. ) ;
#69129 = CARTESIAN_POINT ( 'NONE',  ( 11.58425954179440076, -3.017023678917100327, 6.683254058608399717 ) ) ;
#69130 = VERTEX_POINT ( 'NONE', #55048 ) ;
#69131 = CARTESIAN_POINT ( 'NONE',  ( 7.550614158771000284, 4.468366666325000125, 8.882140983065999862 ) ) ;
#69132 = EDGE_CURVE ( 'NONE', #1201, #63599, #59946, .T. ) ;
#69133 = ORIENTED_EDGE ( 'NONE', *, *, #60188, .T. ) ;
#69134 = CARTESIAN_POINT ( 'NONE',  ( 9.416846873516664829, 3.231816600031355069, -8.499583552997725278 ) ) ;
#69135 = CARTESIAN_POINT ( 'NONE',  ( 7.283516392955999841, -4.426925773067000414, 9.293310812901001583 ) ) ;
#69136 = CARTESIAN_POINT ( 'NONE',  ( 11.12376201898999994, 6.339186361347000087, -5.425853403269999653 ) ) ;
#69137 = VERTEX_POINT ( 'NONE', #33732 ) ;
#69138 = CARTESIAN_POINT ( 'NONE',  ( 12.18370898482675280, -2.431702807279748413, -12.46721300078355554 ) ) ;
#69139 = CARTESIAN_POINT ( 'NONE',  ( 7.848356335646994530, 10.67649265946998938, -3.847892590697003623 ) ) ;
#69140 = CARTESIAN_POINT ( 'NONE',  ( 17.55505043854147118, -1.875000000000000000, -12.57541666120755863 ) ) ;
#69141 = DIRECTION ( 'NONE',  ( -0.7071060865237062121, 0.7071074758487063683, 8.141784862113073118E-10 ) ) ;
#69142 = CARTESIAN_POINT ( 'NONE',  ( 12.25717089523538483, -2.039201503940136551, -13.85070424198620742 ) ) ;
#69143 = CARTESIAN_POINT ( 'NONE',  ( 10.67826222744820086, -4.668580868411999596, -8.050725169876500331 ) ) ;
#69144 = CARTESIAN_POINT ( 'NONE',  ( 11.47822875044625945, 4.169680329100683203, -6.639682804525812720 ) ) ;
#69145 = CARTESIAN_POINT ( 'NONE',  ( 18.18591139755470820, -2.124730565513616831, 12.41957995629783440 ) ) ;
#69146 = ORIENTED_EDGE ( 'NONE', *, *, #29201, .T. ) ;
#69147 = FACE_OUTER_BOUND ( 'NONE', #37256, .T. ) ;
#69148 = ORIENTED_EDGE ( 'NONE', *, *, #63339, .F. ) ;
#69149 = EDGE_CURVE ( 'NONE', #18837, #518, #52720, .T. ) ;
#69150 = CARTESIAN_POINT ( 'NONE',  ( 0.000000000000000000, 0.000000000000000000, 0.000000000000000000 ) ) ;
#69151 = FACE_OUTER_BOUND ( 'NONE', #60964, .T. ) ;
#69152 = CARTESIAN_POINT ( 'NONE',  ( 4.900006121741998122, 1.747572776708516740, 1.007237960741796057 ) ) ;
#69153 = CARTESIAN_POINT ( 'NONE',  ( 10.71983649979000042, 3.571741329336999726, -5.696148467328000287 ) ) ;
#69154 = DIRECTION ( 'NONE',  ( 0.000000000000000000, -1.000000000000000000, 0.000000000000000000 ) ) ;
#69155 = CARTESIAN_POINT ( 'NONE',  ( 8.787837227906001303, -4.603772362336000512, -6.276682186892999837 ) ) ;
#69156 = CARTESIAN_POINT ( 'NONE',  ( 9.099999952505998024, -3.250000006358199744, 7.500000000000000000 ) ) ;
#69157 = CARTESIAN_POINT ( 'NONE',  ( 18.20346453091165273, -2.853274009397274380, -12.27345743255177446 ) ) ;
#69158 = ORIENTED_EDGE ( 'NONE', *, *, #62743, .F. ) ;
#69159 = CARTESIAN_POINT ( 'NONE',  ( 10.48496058254999852, -5.061587542142000018, -4.699980696949000780 ) ) ;
#69160 = CARTESIAN_POINT ( 'NONE',  ( 12.33348197901556276, -2.910306952023486549, 12.34646687328217141 ) ) ;
#69161 = DIRECTION ( 'NONE',  ( 0.000000000000000000, 1.000000000000000000, 0.000000000000000000 ) ) ;
#69162 = CARTESIAN_POINT ( 'NONE',  ( 12.02166954483529970, -3.437903757373499847, 8.367285821793199574 ) ) ;
#69163 = CARTESIAN_POINT ( 'NONE',  ( 18.53574650668400281, 2.786976374009999535, -11.27236326136999978 ) ) ;
#69164 = CARTESIAN_POINT ( 'NONE',  ( 11.36749010443639918, 4.863785690678500195, -7.564597762509089662 ) ) ;
#69165 = CARTESIAN_POINT ( 'NONE',  ( 12.21985383964851657, -0.2197131112048753554, 12.69744725510431493 ) ) ;
#69166 = CARTESIAN_POINT ( 'NONE',  ( 5.648274849241648354, -12.08704511044963326, -3.737576519652977769 ) ) ;
#69167 = CARTESIAN_POINT ( 'NONE',  ( 9.634020792350998619, 3.042978295541999945, 8.588098960242001922 ) ) ;
#69168 = CARTESIAN_POINT ( 'NONE',  ( 11.26374551471000274, -3.753781600817000186, 11.28122097457000095 ) ) ;
#69169 = EDGE_CURVE ( 'NONE', #36015, #45376, #65295, .T. ) ;
#69170 = ORIENTED_EDGE ( 'NONE', *, *, #741, .T. ) ;
#69171 = DIRECTION ( 'NONE',  ( 0.000000000000000000, 1.000000000000000000, 0.000000000000000000 ) ) ;
#69172 = CARTESIAN_POINT ( 'NONE',  ( 7.393365321925000622, -0.9580424575664999720, 0.9776229950699999449 ) ) ;
#69173 = DIRECTION ( 'NONE',  ( 0.000000000000000000, 0.9565994702956990281, 0.2914059941558995726 ) ) ;
#69174 = CARTESIAN_POINT ( 'NONE',  ( 3.448119472057917800, 2.777709467148614664, -2.177750925185379050 ) ) ;
#69175 = DIRECTION ( 'NONE',  ( 2.186552006505938554E-10, 0.8077514394224775129, -0.5895232074404836986 ) ) ;
#69176 = CARTESIAN_POINT ( 'NONE',  ( 11.55610404293055993, -4.502836909561000134, -8.523936114709998790 ) ) ;
#69177 = ORIENTED_EDGE ( 'NONE', *, *, #68641, .T. ) ;
#69178 = CARTESIAN_POINT ( 'NONE',  ( 6.976638848880287291, -1.323261473620580553, 0.6079296519753562000 ) ) ;
#69179 = CARTESIAN_POINT ( 'NONE',  ( 8.785198341231000185, 5.414918126383000185, 8.890678916765999418 ) ) ;
#69181 = CARTESIAN_POINT ( 'NONE',  ( 4.900006121741999010, -2.000000000000000000, 0.000000000000000000 ) ) ;
#69180 = CARTESIAN_POINT ( 'NONE',  ( 8.266329719591000824, 4.769017407621999993, -8.862909124839001507 ) ) ;
#69182 = CARTESIAN_POINT ( 'NONE',  ( 2.210247277619000084, 2.108360286353999413, -2.286637680308000409 ) ) ;
#69183 = EDGE_LOOP ( 'NONE', ( #20655, #9909, #50135, #23235 ) ) ;
#69184 = CARTESIAN_POINT ( 'NONE',  ( 11.07345995138000028, 3.998673170817999889, 8.920816085870999501 ) ) ;
#69185 = CARTESIAN_POINT ( 'NONE',  ( 18.10189407302238607, -2.802802817710309480, -13.60450747121971204 ) ) ;
#69186 = CARTESIAN_POINT ( 'NONE',  ( 10.92441504065829960, 4.694414232677499577, 8.017771632862299214 ) ) ;
#69187 = CARTESIAN_POINT ( 'NONE',  ( 10.53733998880999856, -2.992814141720000265, 8.731692578598000409 ) ) ;
#69188 = CARTESIAN_POINT ( 'NONE',  ( 7.807370559623000084, -3.650411072918999800, 6.083135626079000602 ) ) ;
#69189 = ORIENTED_EDGE ( 'NONE', *, *, #57128, .T. ) ;
#69190 = CARTESIAN_POINT ( 'NONE',  ( 8.802614158774000330, 3.975069902178000270, 9.483774112875002160 ) ) ;
#69192 = FACE_OUTER_BOUND ( 'NONE', #58713, .T. ) ;
#69191 = CARTESIAN_POINT ( 'NONE',  ( 10.77222057153667656, 4.304280767886410786, -8.319452754344771606 ) ) ;
#69193 = VECTOR ( 'NONE', #14442, 1000.000000000000000 ) ;
#69194 = CARTESIAN_POINT ( 'NONE',  ( 7.742012705865137789, -5.501263588994199871, 8.379108557587658268 ) ) ;
#69195 = CARTESIAN_POINT ( 'NONE',  ( 11.09999999999999964, -0.5000000000000000000, 5.124965750789000296 ) ) ;
#69196 = NEXT_ASSEMBLY_USAGE_OCCURRENCE ( 'NAUO1', ' ', ' ', #7317, #43225, $ ) ;
#69197 = NEXT_ASSEMBLY_USAGE_OCCURRENCE ( 'NAUO2', ' ', ' ', #7317, #35119, $ ) ;
#69198 = NEXT_ASSEMBLY_USAGE_OCCURRENCE ( 'NAUO3', ' ', ' ', #7317, #46633, $ ) ;
#69199 = NEXT_ASSEMBLY_USAGE_OCCURRENCE ( 'NAUO4', ' ', ' ', #7317, #39365, $ ) ;
#69200 = NEXT_ASSEMBLY_USAGE_OCCURRENCE ( 'NAUO5', ' ', ' ', #7317, #57742, $ ) ;
#69201 = NEXT_ASSEMBLY_USAGE_OCCURRENCE ( 'NAUO6', ' ', ' ', #7317, #51754, $ ) ;
#69202 = NEXT_ASSEMBLY_USAGE_OCCURRENCE ( 'NAUO7', ' ', ' ', #7317, #38090, $ ) ;
#69203 = NEXT_ASSEMBLY_USAGE_OCCURRENCE ( 'NAUO8', ' ', ' ', #7317, #59017, $ ) ;
#69204 = NEXT_ASSEMBLY_USAGE_OCCURRENCE ( 'NAUO9', ' ', ' ', #7317, #50496, $ ) ;
#69205 = NEXT_ASSEMBLY_USAGE_OCCURRENCE ( 'NAUO10', ' ', ' ', #7317, #2199, $ ) ;
#69206 = NEXT_ASSEMBLY_USAGE_OCCURRENCE ( 'NAUO11', ' ', ' ', #7317, #49624, $ ) ;
#69207 = NEXT_ASSEMBLY_USAGE_OCCURRENCE ( 'NAUO12', ' ', ' ', #7317, #44514, $ ) ;
#69208 = NEXT_ASSEMBLY_USAGE_OCCURRENCE ( 'NAUO13', ' ', ' ', #7317, #16698, $ ) ;
#69209 = NEXT_ASSEMBLY_USAGE_OCCURRENCE ( 'NAUO14', ' ', ' ', #7317, #29121, $ ) ;
ENDSEC;
END-ISO-10303-21;
